#274381=CARTESIAN_POINT('Ctrl Pts',(-10.0160238186115,12.2,-5.24415555162838));
#274382=CARTESIAN_POINT('Ctrl Pts',(-10.0182388956476,12.2,-5.24694578014271));
#274383=CARTESIAN_POINT('Ctrl Pts',(-10.0204550622336,12.2,-5.24974408087327));
#274384=CARTESIAN_POINT('Ctrl Pts',(-10.0226712292222,12.2,-5.25254238211218));
#274385=CARTESIAN_POINT('Ctrl Pts',(-10.0248884846278,12.2,-5.25534875565338));
#274386=CARTESIAN_POINT('Ctrl Pts',(-10.027106784742,12.2,-5.25816319135518));
#274387=CARTESIAN_POINT('Ctrl Pts',(-10.0293250844532,12.2,-5.26097762654569));
#274388=CARTESIAN_POINT('Ctrl Pts',(-10.031544430856,12.2,-5.26380012362741));
#274389=CARTESIAN_POINT('Ctrl Pts',(-10.0337647804838,12.2,-5.26663067331696));
#274390=CARTESIAN_POINT('Ctrl Pts',(-10.0359851301115,12.2,-5.26946122300651));
#274391=CARTESIAN_POINT('Ctrl Pts',(-10.0382064823394,12.2,-5.27229982469302));
#274392=CARTESIAN_POINT('Ctrl Pts',(-10.0404287964771,12.2,-5.27514646747755));
#274393=CARTESIAN_POINT('Ctrl Pts',(-10.0433918818594,12.2,-5.27894199101787));
#274394=CARTESIAN_POINT('Ctrl Pts',(-10.046356677641,12.2,-5.28275181269434));
#274395=CARTESIAN_POINT('Ctrl Pts',(-10.0493230837317,12.2,-5.28657590615806));
#274396=CARTESIAN_POINT('Ctrl Pts',(-10.0515478888049,12.2,-5.28944397690714));
#274397=CARTESIAN_POINT('Ctrl Pts',(-10.0537735996117,12.2,-5.29232007617512));
#274398=CARTESIAN_POINT('Ctrl Pts',(-10.0560001747271,12.2,-5.29520419388704));
#274399=CARTESIAN_POINT('Ctrl Pts',(-10.058226749438,12.2,-5.29808831107501));
#274400=CARTESIAN_POINT('Ctrl Pts',(-10.0604541895072,12.2,-5.30098044610422));
#274401=CARTESIAN_POINT('Ctrl Pts',(-10.0626824527179,12.2,-5.30388058883287));
#274402=CARTESIAN_POINT('Ctrl Pts',(-10.0649107159287,12.2,-5.30678073156153));
#274403=CARTESIAN_POINT('Ctrl Pts',(-10.0671398030063,12.2,-5.30968888177863));
#274404=CARTESIAN_POINT('Ctrl Pts',(-10.0693696727271,12.2,-5.31260503043594));
#274405=CARTESIAN_POINT('Ctrl Pts',(-10.0715995424479,12.2,-5.31552117909327));
#274406=CARTESIAN_POINT('Ctrl Pts',(-10.073830195969,12.2,-5.31844532509055));
#274407=CARTESIAN_POINT('Ctrl Pts',(-10.0760615897314,12.2,-5.3213774582473));
#274408=CARTESIAN_POINT('Ctrl Pts',(-10.0782929834937,12.2,-5.32430959140405));
#274409=CARTESIAN_POINT('Ctrl Pts',(-10.0805251200545,12.2,-5.32724971180322));
#274410=CARTESIAN_POINT('Ctrl Pts',(-10.0827579573067,12.2,-5.33019780894542));
#274411=CARTESIAN_POINT('Ctrl Pts',(-10.0849907945588,12.2,-5.33314590608762));
#274412=CARTESIAN_POINT('Ctrl Pts',(-10.0872243338109,12.2,-5.33610197912926));
#274413=CARTESIAN_POINT('Ctrl Pts',(-10.0894585349797,12.2,-5.33906601889547));
#274414=CARTESIAN_POINT('Ctrl Pts',(-10.0916927365543,12.2,-5.34203005920015));
#274415=CARTESIAN_POINT('Ctrl Pts',(-10.0939276000624,12.2,-5.34500206704876));
#274416=CARTESIAN_POINT('Ctrl Pts',(-10.0961630855541,12.2,-5.34798202985793));
#274417=CARTESIAN_POINT('Ctrl Pts',(-10.0991437321994,12.2,-5.35195531270122));
#274418=CARTESIAN_POINT('Ctrl Pts',(-10.1021254821311,12.2,-5.355942739759));
#274419=CARTESIAN_POINT('Ctrl Pts',(-10.1051082402897,12.2,-5.35994428450557));
#274420=CARTESIAN_POINT('Ctrl Pts',(-10.1073453090102,12.2,-5.3629454432018));
#274421=CARTESIAN_POINT('Ctrl Pts',(-10.1095829447208,12.2,-5.36595454263154));
#274422=CARTESIAN_POINT('Ctrl Pts',(-10.1118211114728,12.2,-5.36897157389624));
#274423=CARTESIAN_POINT('Ctrl Pts',(-10.1140592782247,12.2,-5.37198860516093));
#274424=CARTESIAN_POINT('Ctrl Pts',(-10.1162979764433,12.2,-5.37501356935007));
#274425=CARTESIAN_POINT('Ctrl Pts',(-10.1185371685286,12.2,-5.37804645357213));
#274426=CARTESIAN_POINT('Ctrl Pts',(-10.1207763610206,12.2,-5.38107933834517));
#274427=CARTESIAN_POINT('Ctrl Pts',(-10.1230160464794,12.2,-5.3841201444871));
#274428=CARTESIAN_POINT('Ctrl Pts',(-10.1252561779717,12.2,-5.38716885968126));
#274429=CARTESIAN_POINT('Ctrl Pts',(-10.1274963090571,12.2,-5.39021757432157));
#274430=CARTESIAN_POINT('Ctrl Pts',(-10.1297368853697,12.2,-5.3932741973836));
#274431=CARTESIAN_POINT('Ctrl Pts',(-10.131977863942,12.2,-5.39633871684295));
#274432=CARTESIAN_POINT('Ctrl Pts',(-10.1342188425142,12.2,-5.3994032363023));
#274433=CARTESIAN_POINT('Ctrl Pts',(-10.1364602251632,12.2,-5.40247565238601));
#274434=CARTESIAN_POINT('Ctrl Pts',(-10.1387019915142,12.2,-5.40555595924693));
#274435=CARTESIAN_POINT('Ctrl Pts',(-10.1409437578652,12.2,-5.40863626610785));
#274436=CARTESIAN_POINT('Ctrl Pts',(-10.1431859115927,12.2,-5.41172446343756));
#274437=CARTESIAN_POINT('Ctrl Pts',(-10.1454284470001,12.2,-5.41482055400001));
#274438=CARTESIAN_POINT('Ctrl Pts',(-9.95917514600006,15.2,-5.75020264100001));
#274439=CARTESIAN_POINT('Ctrl Pts',(-9.95917514600006,11.6,-5.75020264100001));
#274440=CARTESIAN_POINT('Ctrl Pts',(-9.95841243100006,15.2,-5.75014921000002));
#274441=CARTESIAN_POINT('Ctrl Pts',(-9.95841243100006,11.6,-5.75014921000002));
#274442=CARTESIAN_POINT('Ctrl Pts',(-9.95688746000006,15.2,-5.75004209300002));
#274443=CARTESIAN_POINT('Ctrl Pts',(-9.95688746000006,11.6,-5.75004209300002));
#274444=CARTESIAN_POINT('Ctrl Pts',(-9.95460138500006,15.2,-5.74988064700002));
#274445=CARTESIAN_POINT('Ctrl Pts',(-9.95460138500006,11.6,-5.74988064700002));
#274446=CARTESIAN_POINT('Ctrl Pts',(-9.95155604400006,15.2,-5.74966384900002));
#274447=CARTESIAN_POINT('Ctrl Pts',(-9.95155604400006,11.6,-5.74966384900002));
#274448=CARTESIAN_POINT('Ctrl Pts',(-9.94775397000006,15.2,-5.74939029000002));
#274449=CARTESIAN_POINT('Ctrl Pts',(-9.94775397000006,11.6,-5.74939029000002));
#274450=CARTESIAN_POINT('Ctrl Pts',(-9.94395649900006,15.2,-5.74911416700001));
#274451=CARTESIAN_POINT('Ctrl Pts',(-9.94395649900006,11.6,-5.74911416700001));
#274452=CARTESIAN_POINT('Ctrl Pts',(-9.94016363100006,15.2,-5.74883548400001));
#274453=CARTESIAN_POINT('Ctrl Pts',(-9.94016363100006,11.6,-5.74883548400001));
#274454=CARTESIAN_POINT('Ctrl Pts',(-9.93637537100006,15.2,-5.74855424400001));
#274455=CARTESIAN_POINT('Ctrl Pts',(-9.93637537100006,11.6,-5.74855424400001));
#274456=CARTESIAN_POINT('Ctrl Pts',(-9.93259172200006,15.2,-5.74827044900001));
#274457=CARTESIAN_POINT('Ctrl Pts',(-9.93259172200006,11.6,-5.74827044900001));
#274458=CARTESIAN_POINT('Ctrl Pts',(-9.92881269100006,15.2,-5.74798410500001));
#274459=CARTESIAN_POINT('Ctrl Pts',(-9.92881269100006,11.6,-5.74798410500001));
#274460=CARTESIAN_POINT('Ctrl Pts',(-9.92503828400006,15.2,-5.74769522000001));
#274461=CARTESIAN_POINT('Ctrl Pts',(-9.92503828400006,11.6,-5.74769522000001));
#274462=CARTESIAN_POINT('Ctrl Pts',(-9.92126851000006,15.2,-5.74740380100002));
#274463=CARTESIAN_POINT('Ctrl Pts',(-9.92126851000006,11.6,-5.74740380100002));
#274464=CARTESIAN_POINT('Ctrl Pts',(-9.91750337600006,15.2,-5.74710985300002));
#274465=CARTESIAN_POINT('Ctrl Pts',(-9.91750337600006,11.6,-5.74710985300002));
#274466=CARTESIAN_POINT('Ctrl Pts',(-9.91374289200006,15.2,-5.74681338700002));
#274467=CARTESIAN_POINT('Ctrl Pts',(-9.91374289200006,11.6,-5.74681338700002));
#274468=CARTESIAN_POINT('Ctrl Pts',(-9.90998706400006,15.2,-5.74651440900002));
#274469=CARTESIAN_POINT('Ctrl Pts',(-9.90998706400006,11.6,-5.74651440900002));
#274470=CARTESIAN_POINT('Ctrl Pts',(-9.90623590000006,15.2,-5.74621292500002));
#274471=CARTESIAN_POINT('Ctrl Pts',(-9.90623590000006,11.6,-5.74621292500002));
#274472=CARTESIAN_POINT('Ctrl Pts',(-9.90248940500006,15.2,-5.74590894100002));
#274473=CARTESIAN_POINT('Ctrl Pts',(-9.90248940500006,11.6,-5.74590894100002));
#274474=CARTESIAN_POINT('Ctrl Pts',(-9.89874758700006,15.2,-5.74560246200001));
#274475=CARTESIAN_POINT('Ctrl Pts',(-9.89874758700006,11.6,-5.74560246200001));
#274476=CARTESIAN_POINT('Ctrl Pts',(-9.89501045000006,15.2,-5.74529349400001));
#274477=CARTESIAN_POINT('Ctrl Pts',(-9.89501045000006,11.6,-5.74529349400001));
#274478=CARTESIAN_POINT('Ctrl Pts',(-9.89127800100006,15.2,-5.74498204400002));
#274479=CARTESIAN_POINT('Ctrl Pts',(-9.89127800100006,11.6,-5.74498204400002));
#274480=CARTESIAN_POINT('Ctrl Pts',(-9.88755024700006,15.2,-5.74466811600002));
#274481=CARTESIAN_POINT('Ctrl Pts',(-9.88755024700006,11.6,-5.74466811600002));
#274482=CARTESIAN_POINT('Ctrl Pts',(-9.88382719300006,15.2,-5.74435171600002));
#274483=CARTESIAN_POINT('Ctrl Pts',(-9.88382719300006,11.6,-5.74435171600002));
#274484=CARTESIAN_POINT('Ctrl Pts',(-9.88010884700006,15.2,-5.74403285200002));
#274485=CARTESIAN_POINT('Ctrl Pts',(-9.88010884700006,11.6,-5.74403285200002));
#274486=CARTESIAN_POINT('Ctrl Pts',(-9.87639521400006,15.2,-5.74371152900002));
#274487=CARTESIAN_POINT('Ctrl Pts',(-9.87639521400006,11.6,-5.74371152900002));
#274488=CARTESIAN_POINT('Ctrl Pts',(-9.87268630300006,15.2,-5.74338775400002));
#274489=CARTESIAN_POINT('Ctrl Pts',(-9.87268630300006,11.6,-5.74338775400002));
#274490=CARTESIAN_POINT('Ctrl Pts',(-9.86898212000006,15.2,-5.74306153500002));
#274491=CARTESIAN_POINT('Ctrl Pts',(-9.86898212000006,11.6,-5.74306153500002));
#274492=CARTESIAN_POINT('Ctrl Pts',(-9.86528267300006,15.2,-5.74273287600001));
#274493=CARTESIAN_POINT('Ctrl Pts',(-9.86528267300006,11.6,-5.74273287600001));
#274494=CARTESIAN_POINT('Ctrl Pts',(-9.86158796700006,15.2,-5.74240178400002));
#274495=CARTESIAN_POINT('Ctrl Pts',(-9.86158796700006,11.6,-5.74240178400002));
#274496=CARTESIAN_POINT('Ctrl Pts',(-9.85789800900006,15.2,-5.74206826700002));
#274497=CARTESIAN_POINT('Ctrl Pts',(-9.85789800900006,11.6,-5.74206826700002));
#274498=CARTESIAN_POINT('Ctrl Pts',(-9.85421280700006,15.2,-5.74173232900002));
#274499=CARTESIAN_POINT('Ctrl Pts',(-9.85421280700006,11.6,-5.74173232900002));
#274500=CARTESIAN_POINT('Ctrl Pts',(-9.85053236600006,15.2,-5.74139397800002));
#274501=CARTESIAN_POINT('Ctrl Pts',(-9.85053236600006,11.6,-5.74139397800002));
#274502=CARTESIAN_POINT('Ctrl Pts',(-9.84685669200006,15.2,-5.74105321800002));
#274503=CARTESIAN_POINT('Ctrl Pts',(-9.84685669200006,11.6,-5.74105321800002));
#274504=CARTESIAN_POINT('Ctrl Pts',(-9.84318579500006,15.2,-5.74071005800001));
#274505=CARTESIAN_POINT('Ctrl Pts',(-9.84318579500006,11.6,-5.74071005800001));
#274506=CARTESIAN_POINT('Ctrl Pts',(-9.83951967700006,15.2,-5.74036450400002));
#274507=CARTESIAN_POINT('Ctrl Pts',(-9.83951967700006,11.6,-5.74036450400002));
#274508=CARTESIAN_POINT('Ctrl Pts',(-9.83585834900006,15.2,-5.74001656000001));
#274509=CARTESIAN_POINT('Ctrl Pts',(-9.83585834900006,11.6,-5.74001656000001));
#274510=CARTESIAN_POINT('Ctrl Pts',(-9.83220181500006,15.2,-5.73966623600001));
#274511=CARTESIAN_POINT('Ctrl Pts',(-9.83220181500006,11.6,-5.73966623600001));
#274512=CARTESIAN_POINT('Ctrl Pts',(-9.82855008400006,15.2,-5.73931353600001));
#274513=CARTESIAN_POINT('Ctrl Pts',(-9.82855008400006,11.6,-5.73931353600001));
#274514=CARTESIAN_POINT('Ctrl Pts',(-9.82490316100006,15.2,-5.73895846600001));
#274515=CARTESIAN_POINT('Ctrl Pts',(-9.82490316100006,11.6,-5.73895846600001));
#274516=CARTESIAN_POINT('Ctrl Pts',(-9.82126105300006,15.2,-5.73860103500002));
#274517=CARTESIAN_POINT('Ctrl Pts',(-9.82126105300006,11.6,-5.73860103500002));
#274518=CARTESIAN_POINT('Ctrl Pts',(-9.81762376700006,15.2,-5.73824124900002));
#274519=CARTESIAN_POINT('Ctrl Pts',(-9.81762376700006,11.6,-5.73824124900002));
#274520=CARTESIAN_POINT('Ctrl Pts',(-9.81399131100006,15.2,-5.73787911300002));
#274521=CARTESIAN_POINT('Ctrl Pts',(-9.81399131100006,11.6,-5.73787911300002));
#274522=CARTESIAN_POINT('Ctrl Pts',(-9.81036369000006,15.2,-5.73751463500002));
#274523=CARTESIAN_POINT('Ctrl Pts',(-9.81036369000006,11.6,-5.73751463500002));
#274524=CARTESIAN_POINT('Ctrl Pts',(-9.80674091100006,15.2,-5.73714781900001));
#274525=CARTESIAN_POINT('Ctrl Pts',(-9.80674091100006,11.6,-5.73714781900001));
#274526=CARTESIAN_POINT('Ctrl Pts',(-9.80312298100005,15.2,-5.73677867600002));
#274527=CARTESIAN_POINT('Ctrl Pts',(-9.80312298100005,11.6,-5.73677867600002));
#274528=CARTESIAN_POINT('Ctrl Pts',(-9.79950990800005,15.2,-5.73640720800002));
#274529=CARTESIAN_POINT('Ctrl Pts',(-9.79950990800005,11.6,-5.73640720800002));
#274530=CARTESIAN_POINT('Ctrl Pts',(-9.79590169600005,15.2,-5.73603342500002));
#274531=CARTESIAN_POINT('Ctrl Pts',(-9.79590169600005,11.6,-5.73603342500002));
#274532=CARTESIAN_POINT('Ctrl Pts',(-9.79229835500006,15.2,-5.73565733100001));
#274533=CARTESIAN_POINT('Ctrl Pts',(-9.79229835500006,11.6,-5.73565733100001));
#274534=CARTESIAN_POINT('Ctrl Pts',(-9.78869989000006,15.2,-5.73527893500002));
#274535=CARTESIAN_POINT('Ctrl Pts',(-9.78869989000006,11.6,-5.73527893500002));
#274536=CARTESIAN_POINT('Ctrl Pts',(-9.78510630800006,15.2,-5.73489824300002));
#274537=CARTESIAN_POINT('Ctrl Pts',(-9.78510630800006,11.6,-5.73489824300002));
#274538=CARTESIAN_POINT('Ctrl Pts',(-9.78151761600006,15.2,-5.73451526100002));
#274539=CARTESIAN_POINT('Ctrl Pts',(-9.78151761600006,11.6,-5.73451526100002));
#274540=CARTESIAN_POINT('Ctrl Pts',(-9.77793382100005,15.2,-5.73412999600002));
#274541=CARTESIAN_POINT('Ctrl Pts',(-9.77793382100005,11.6,-5.73412999600002));
#274542=CARTESIAN_POINT('Ctrl Pts',(-9.77435492900005,15.2,-5.73374245400001));
#274543=CARTESIAN_POINT('Ctrl Pts',(-9.77435492900005,11.6,-5.73374245400001));
#274544=CARTESIAN_POINT('Ctrl Pts',(-9.77078094800006,15.2,-5.73335264400002));
#274545=CARTESIAN_POINT('Ctrl Pts',(-9.77078094800006,11.6,-5.73335264400002));
#274546=CARTESIAN_POINT('Ctrl Pts',(-9.76721188400006,15.2,-5.73296057000002));
#274547=CARTESIAN_POINT('Ctrl Pts',(-9.76721188400006,11.6,-5.73296057000002));
#274548=CARTESIAN_POINT('Ctrl Pts',(-9.76364774500006,15.2,-5.73256624100001));
#274549=CARTESIAN_POINT('Ctrl Pts',(-9.76364774500006,11.6,-5.73256624100001));
#274550=CARTESIAN_POINT('Ctrl Pts',(-9.76008853600005,15.2,-5.73216966200001));
#274551=CARTESIAN_POINT('Ctrl Pts',(-9.76008853600005,11.6,-5.73216966200001));
#274552=CARTESIAN_POINT('Ctrl Pts',(-9.75653426500006,15.2,-5.73177084100001));
#274553=CARTESIAN_POINT('Ctrl Pts',(-9.75653426500006,11.6,-5.73177084100001));
#274554=CARTESIAN_POINT('Ctrl Pts',(-9.75298493900006,15.2,-5.73136978400001));
#274555=CARTESIAN_POINT('Ctrl Pts',(-9.75298493900006,11.6,-5.73136978400001));
#274556=CARTESIAN_POINT('Ctrl Pts',(-9.74944056500006,15.2,-5.73096650000001));
#274557=CARTESIAN_POINT('Ctrl Pts',(-9.74944056500006,11.6,-5.73096650000001));
#274558=CARTESIAN_POINT('Ctrl Pts',(-9.74590115000005,15.2,-5.73056099200001));
#274559=CARTESIAN_POINT('Ctrl Pts',(-9.74590115000005,11.6,-5.73056099200001));
#274560=CARTESIAN_POINT('Ctrl Pts',(-9.74236669900005,15.2,-5.73015327100002));
#274561=CARTESIAN_POINT('Ctrl Pts',(-9.74236669900005,11.6,-5.73015327100002));
#274562=CARTESIAN_POINT('Ctrl Pts',(-9.73883722100006,15.2,-5.72974334100002));
#274563=CARTESIAN_POINT('Ctrl Pts',(-9.73883722100006,11.6,-5.72974334100002));
#274564=CARTESIAN_POINT('Ctrl Pts',(-9.73531272200006,15.2,-5.72933121000001));
#274565=CARTESIAN_POINT('Ctrl Pts',(-9.73531272200006,11.6,-5.72933121000001));
#274566=CARTESIAN_POINT('Ctrl Pts',(-9.73179320900006,15.2,-5.72891688500002));
#274567=CARTESIAN_POINT('Ctrl Pts',(-9.73179320900006,11.6,-5.72891688500002));
#274568=CARTESIAN_POINT('Ctrl Pts',(-9.72827869000006,15.2,-5.72850037300002));
#274569=CARTESIAN_POINT('Ctrl Pts',(-9.72827869000006,11.6,-5.72850037300002));
#274570=CARTESIAN_POINT('Ctrl Pts',(-9.72476917000006,15.2,-5.72808168000002));
#274571=CARTESIAN_POINT('Ctrl Pts',(-9.72476917000006,11.6,-5.72808168000002));
#274572=CARTESIAN_POINT('Ctrl Pts',(-9.72126465700006,15.2,-5.72766081300002));
#274573=CARTESIAN_POINT('Ctrl Pts',(-9.72126465700006,11.6,-5.72766081300002));
#274574=CARTESIAN_POINT('Ctrl Pts',(-9.71776515900006,15.2,-5.72723778200002));
#274575=CARTESIAN_POINT('Ctrl Pts',(-9.71776515900006,11.6,-5.72723778200002));
#274576=CARTESIAN_POINT('Ctrl Pts',(-9.71427068100006,15.2,-5.72681259100002));
#274577=CARTESIAN_POINT('Ctrl Pts',(-9.71427068100006,11.6,-5.72681259100002));
#274578=CARTESIAN_POINT('Ctrl Pts',(-9.71078123000006,15.2,-5.72638524700002));
#274579=CARTESIAN_POINT('Ctrl Pts',(-9.71078123000006,11.6,-5.72638524700002));
#274580=CARTESIAN_POINT('Ctrl Pts',(-9.70729681500006,15.2,-5.72595575900002));
#274581=CARTESIAN_POINT('Ctrl Pts',(-9.70729681500006,11.6,-5.72595575900002));
#274582=CARTESIAN_POINT('Ctrl Pts',(-9.70381744100006,15.2,-5.72552413200001));
#274583=CARTESIAN_POINT('Ctrl Pts',(-9.70381744100006,11.6,-5.72552413200001));
#274584=CARTESIAN_POINT('Ctrl Pts',(-9.70034311500006,15.2,-5.72509037400001));
#274585=CARTESIAN_POINT('Ctrl Pts',(-9.70034311500006,11.6,-5.72509037400001));
#274586=CARTESIAN_POINT('Ctrl Pts',(-9.69687384600006,15.2,-5.72465449300001));
#274587=CARTESIAN_POINT('Ctrl Pts',(-9.69687384600006,11.6,-5.72465449300001));
#274588=CARTESIAN_POINT('Ctrl Pts',(-9.69340963900006,15.2,-5.72421649500002));
#274589=CARTESIAN_POINT('Ctrl Pts',(-9.69340963900006,11.6,-5.72421649500002));
#274590=CARTESIAN_POINT('Ctrl Pts',(-9.68995050200006,15.2,-5.72377638700001));
#274591=CARTESIAN_POINT('Ctrl Pts',(-9.68995050200006,11.6,-5.72377638700001));
#274592=CARTESIAN_POINT('Ctrl Pts',(-9.68649644100006,15.2,-5.72333417800002));
#274593=CARTESIAN_POINT('Ctrl Pts',(-9.68649644100006,11.6,-5.72333417800002));
#274594=CARTESIAN_POINT('Ctrl Pts',(-9.68304746500005,15.2,-5.72288987300002));
#274595=CARTESIAN_POINT('Ctrl Pts',(-9.68304746500005,11.6,-5.72288987300002));
#274596=CARTESIAN_POINT('Ctrl Pts',(-9.67960357800006,15.2,-5.72244348100002));
#274597=CARTESIAN_POINT('Ctrl Pts',(-9.67960357800006,11.6,-5.72244348100002));
#274598=CARTESIAN_POINT('Ctrl Pts',(-9.67616479000006,15.2,-5.72199500700002));
#274599=CARTESIAN_POINT('Ctrl Pts',(-9.67616479000006,11.6,-5.72199500700002));
#274600=CARTESIAN_POINT('Ctrl Pts',(-9.67273110700006,15.2,-5.72154446000001));
#274601=CARTESIAN_POINT('Ctrl Pts',(-9.67273110700006,11.6,-5.72154446000001));
#274602=CARTESIAN_POINT('Ctrl Pts',(-9.66930253400006,15.2,-5.72109184700002));
#274603=CARTESIAN_POINT('Ctrl Pts',(-9.66930253400006,11.6,-5.72109184700002));
#274604=CARTESIAN_POINT('Ctrl Pts',(-9.66587908100006,15.2,-5.72063717600001));
#274605=CARTESIAN_POINT('Ctrl Pts',(-9.66587908100006,11.6,-5.72063717600001));
#274606=CARTESIAN_POINT('Ctrl Pts',(-9.66246075400005,15.2,-5.72018045200001));
#274607=CARTESIAN_POINT('Ctrl Pts',(-9.66246075400005,11.6,-5.72018045200001));
#274608=CARTESIAN_POINT('Ctrl Pts',(-9.65904756000005,15.2,-5.71972168500002));
#274609=CARTESIAN_POINT('Ctrl Pts',(-9.65904756000005,11.6,-5.71972168500002));
#274610=CARTESIAN_POINT('Ctrl Pts',(-9.65563950500006,15.2,-5.71926088000002));
#274611=CARTESIAN_POINT('Ctrl Pts',(-9.65563950500006,11.6,-5.71926088000002));
#274612=CARTESIAN_POINT('Ctrl Pts',(-9.65223659800006,15.2,-5.71879804700002));
#274613=CARTESIAN_POINT('Ctrl Pts',(-9.65223659800006,11.6,-5.71879804700002));
#274614=CARTESIAN_POINT('Ctrl Pts',(-9.64883884500006,15.2,-5.71833319000002));
#274615=CARTESIAN_POINT('Ctrl Pts',(-9.64883884500006,11.6,-5.71833319000002));
#274616=CARTESIAN_POINT('Ctrl Pts',(-9.64544625400006,15.2,-5.71786632000002));
#274617=CARTESIAN_POINT('Ctrl Pts',(-9.64544625400006,11.6,-5.71786632000002));
#274618=CARTESIAN_POINT('Ctrl Pts',(-9.64205883100006,15.2,-5.71739744100002));
#274619=CARTESIAN_POINT('Ctrl Pts',(-9.64205883100006,11.6,-5.71739744100002));
#274620=CARTESIAN_POINT('Ctrl Pts',(-9.63867658300006,15.2,-5.71692656400002));
#274621=CARTESIAN_POINT('Ctrl Pts',(-9.63867658300006,11.6,-5.71692656400002));
#274622=CARTESIAN_POINT('Ctrl Pts',(-9.63529951700006,15.2,-5.71645369400001));
#274623=CARTESIAN_POINT('Ctrl Pts',(-9.63529951700006,11.6,-5.71645369400001));
#274624=CARTESIAN_POINT('Ctrl Pts',(-9.63192764200006,15.2,-5.71597884000001));
#274625=CARTESIAN_POINT('Ctrl Pts',(-9.63192764200006,11.6,-5.71597884000001));
#274626=CARTESIAN_POINT('Ctrl Pts',(-9.62856096400006,15.2,-5.71550200700001));
#274627=CARTESIAN_POINT('Ctrl Pts',(-9.62856096400006,11.6,-5.71550200700001));
#274628=CARTESIAN_POINT('Ctrl Pts',(-9.62519948900006,15.2,-5.71502320500001));
#274629=CARTESIAN_POINT('Ctrl Pts',(-9.62519948900006,11.6,-5.71502320500001));
#274630=CARTESIAN_POINT('Ctrl Pts',(-9.62184322600006,15.2,-5.71454244100002));
#274631=CARTESIAN_POINT('Ctrl Pts',(-9.62184322600006,11.6,-5.71454244100002));
#274632=CARTESIAN_POINT('Ctrl Pts',(-9.61849218000006,15.2,-5.71405972200001));
#274633=CARTESIAN_POINT('Ctrl Pts',(-9.61849218000006,11.6,-5.71405972200001));
#274634=CARTESIAN_POINT('Ctrl Pts',(-9.61514636100006,15.2,-5.71357505700002));
#274635=CARTESIAN_POINT('Ctrl Pts',(-9.61514636100006,11.6,-5.71357505700002));
#274636=CARTESIAN_POINT('Ctrl Pts',(-9.61180577400006,15.2,-5.71308845100001));
#274637=CARTESIAN_POINT('Ctrl Pts',(-9.61180577400006,11.6,-5.71308845100001));
#274638=CARTESIAN_POINT('Ctrl Pts',(-9.60847042700006,15.2,-5.71259991300002));
#274639=CARTESIAN_POINT('Ctrl Pts',(-9.60847042700006,11.6,-5.71259991300002));
#274640=CARTESIAN_POINT('Ctrl Pts',(-9.60514032600006,15.2,-5.71210945300002));
#274641=CARTESIAN_POINT('Ctrl Pts',(-9.60514032600006,11.6,-5.71210945300002));
#274642=CARTESIAN_POINT('Ctrl Pts',(-9.60181548000006,15.2,-5.71161707400002));
#274643=CARTESIAN_POINT('Ctrl Pts',(-9.60181548000006,11.6,-5.71161707400002));
#274644=CARTESIAN_POINT('Ctrl Pts',(-9.59849589600006,15.2,-5.71112278700002));
#274645=CARTESIAN_POINT('Ctrl Pts',(-9.59849589600006,11.6,-5.71112278700002));
#274646=CARTESIAN_POINT('Ctrl Pts',(-9.59518158000006,15.2,-5.71062660000001));
#274647=CARTESIAN_POINT('Ctrl Pts',(-9.59518158000006,11.6,-5.71062660000001));
#274648=CARTESIAN_POINT('Ctrl Pts',(-9.59187253900006,15.2,-5.71012851800001));
#274649=CARTESIAN_POINT('Ctrl Pts',(-9.59187253900006,11.6,-5.71012851800001));
#274650=CARTESIAN_POINT('Ctrl Pts',(-9.58856878200006,15.2,-5.70962855200002));
#274651=CARTESIAN_POINT('Ctrl Pts',(-9.58856878200006,11.6,-5.70962855200002));
#274652=CARTESIAN_POINT('Ctrl Pts',(-9.58527031500006,15.2,-5.70912670700002));
#274653=CARTESIAN_POINT('Ctrl Pts',(-9.58527031500006,11.6,-5.70912670700002));
#274654=CARTESIAN_POINT('Ctrl Pts',(-9.58197714700006,15.2,-5.70862299200002));
#274655=CARTESIAN_POINT('Ctrl Pts',(-9.58197714700006,11.6,-5.70862299200002));
#274656=CARTESIAN_POINT('Ctrl Pts',(-9.57868928200006,15.2,-5.70811741500002));
#274657=CARTESIAN_POINT('Ctrl Pts',(-9.57868928200006,11.6,-5.70811741500002));
#274658=CARTESIAN_POINT('Ctrl Pts',(-9.57540672900006,15.2,-5.70760998400001));
#274659=CARTESIAN_POINT('Ctrl Pts',(-9.57540672900006,11.6,-5.70760998400001));
#274660=CARTESIAN_POINT('Ctrl Pts',(-9.57212949600006,15.2,-5.70710070600001));
#274661=CARTESIAN_POINT('Ctrl Pts',(-9.57212949600006,11.6,-5.70710070600001));
#274662=CARTESIAN_POINT('Ctrl Pts',(-9.56885759000006,15.2,-5.70658959000002));
#274663=CARTESIAN_POINT('Ctrl Pts',(-9.56885759000006,11.6,-5.70658959000002));
#274664=CARTESIAN_POINT('Ctrl Pts',(-9.56559101700006,15.2,-5.70607664300002));
#274665=CARTESIAN_POINT('Ctrl Pts',(-9.56559101700006,11.6,-5.70607664300002));
#274666=CARTESIAN_POINT('Ctrl Pts',(-9.56232978500006,15.2,-5.70556187300002));
#274667=CARTESIAN_POINT('Ctrl Pts',(-9.56232978500006,11.6,-5.70556187300002));
#274668=CARTESIAN_POINT('Ctrl Pts',(-9.55907390200006,15.2,-5.70504528800001));
#274669=CARTESIAN_POINT('Ctrl Pts',(-9.55907390200006,11.6,-5.70504528800001));
#274670=CARTESIAN_POINT('Ctrl Pts',(-9.55582337400006,15.2,-5.70452689600002));
#274671=CARTESIAN_POINT('Ctrl Pts',(-9.55582337400006,11.6,-5.70452689600002));
#274672=CARTESIAN_POINT('Ctrl Pts',(-9.55257821000006,15.2,-5.70400670700002));
#274673=CARTESIAN_POINT('Ctrl Pts',(-9.55257821000006,11.6,-5.70400670700002));
#274674=CARTESIAN_POINT('Ctrl Pts',(-9.54933841600005,15.2,-5.70348472500001));
#274675=CARTESIAN_POINT('Ctrl Pts',(-9.54933841600005,11.6,-5.70348472500001));
#274676=CARTESIAN_POINT('Ctrl Pts',(-9.54610400000006,15.2,-5.70296096100002));
#274677=CARTESIAN_POINT('Ctrl Pts',(-9.54610400000006,11.6,-5.70296096100002));
#274678=CARTESIAN_POINT('Ctrl Pts',(-9.54287496800006,15.2,-5.70243542200001));
#274679=CARTESIAN_POINT('Ctrl Pts',(-9.54287496800006,11.6,-5.70243542200001));
#274680=CARTESIAN_POINT('Ctrl Pts',(-9.53965133000005,15.2,-5.70190811700002));
#274681=CARTESIAN_POINT('Ctrl Pts',(-9.53965133000005,11.6,-5.70190811700002));
#274682=CARTESIAN_POINT('Ctrl Pts',(-9.53643309000006,15.2,-5.70137905200002));
#274683=CARTESIAN_POINT('Ctrl Pts',(-9.53643309000006,11.6,-5.70137905200002));
#274684=CARTESIAN_POINT('Ctrl Pts',(-9.53322025900006,15.2,-5.70084823700002));
#274685=CARTESIAN_POINT('Ctrl Pts',(-9.53322025900006,11.6,-5.70084823700002));
#274686=CARTESIAN_POINT('Ctrl Pts',(-9.53001284100005,15.2,-5.70031568100001));
#274687=CARTESIAN_POINT('Ctrl Pts',(-9.53001284100005,11.6,-5.70031568100001));
#274688=CARTESIAN_POINT('Ctrl Pts',(-9.52681084500006,15.2,-5.69978139000002));
#274689=CARTESIAN_POINT('Ctrl Pts',(-9.52681084500006,11.6,-5.69978139000002));
#274690=CARTESIAN_POINT('Ctrl Pts',(-9.52361428000006,15.2,-5.69924537200002));
#274691=CARTESIAN_POINT('Ctrl Pts',(-9.52361428000006,11.6,-5.69924537200002));
#274692=CARTESIAN_POINT('Ctrl Pts',(-9.52042315000006,15.2,-5.69870763800001));
#274693=CARTESIAN_POINT('Ctrl Pts',(-9.52042315000006,11.6,-5.69870763800001));
#274694=CARTESIAN_POINT('Ctrl Pts',(-9.51723746400006,15.2,-5.69816819400002));
#274695=CARTESIAN_POINT('Ctrl Pts',(-9.51723746400006,11.6,-5.69816819400002));
#274696=CARTESIAN_POINT('Ctrl Pts',(-9.51405723100006,15.2,-5.69762704800001));
#274697=CARTESIAN_POINT('Ctrl Pts',(-9.51405723100006,11.6,-5.69762704800001));
#274698=CARTESIAN_POINT('Ctrl Pts',(-9.51088245600006,15.2,-5.69708421000002));
#274699=CARTESIAN_POINT('Ctrl Pts',(-9.51088245600006,11.6,-5.69708421000002));
#274700=CARTESIAN_POINT('Ctrl Pts',(-9.50771314700006,15.2,-5.69653968700001));
#274701=CARTESIAN_POINT('Ctrl Pts',(-9.50771314700006,11.6,-5.69653968700001));
#274702=CARTESIAN_POINT('Ctrl Pts',(-9.50454931300006,15.2,-5.69599348800002));
#274703=CARTESIAN_POINT('Ctrl Pts',(-9.50454931300006,11.6,-5.69599348800002));
#274704=CARTESIAN_POINT('Ctrl Pts',(-9.50139095800006,15.2,-5.69544562100001));
#274705=CARTESIAN_POINT('Ctrl Pts',(-9.50139095800006,11.6,-5.69544562100001));
#274706=CARTESIAN_POINT('Ctrl Pts',(-9.49823809300005,15.2,-5.69489609400001));
#274707=CARTESIAN_POINT('Ctrl Pts',(-9.49823809300005,11.6,-5.69489609400001));
#274708=CARTESIAN_POINT('Ctrl Pts',(-9.49509072500006,15.2,-5.69434491500001));
#274709=CARTESIAN_POINT('Ctrl Pts',(-9.49509072500006,11.6,-5.69434491500001));
#274710=CARTESIAN_POINT('Ctrl Pts',(-9.49194886000006,15.2,-5.69379209500001));
#274711=CARTESIAN_POINT('Ctrl Pts',(-9.49194886000006,11.6,-5.69379209500001));
#274712=CARTESIAN_POINT('Ctrl Pts',(-9.48881250600006,15.2,-5.69323764000002));
#274713=CARTESIAN_POINT('Ctrl Pts',(-9.48881250600006,11.6,-5.69323764000002));
#274714=CARTESIAN_POINT('Ctrl Pts',(-9.48568167200006,15.2,-5.69268155900001));
#274715=CARTESIAN_POINT('Ctrl Pts',(-9.48568167200006,11.6,-5.69268155900001));
#274716=CARTESIAN_POINT('Ctrl Pts',(-9.48255636300006,15.2,-5.69212386100002));
#274717=CARTESIAN_POINT('Ctrl Pts',(-9.48255636300006,11.6,-5.69212386100002));
#274718=CARTESIAN_POINT('Ctrl Pts',(-9.47943658800006,15.2,-5.69156455400002));
#274719=CARTESIAN_POINT('Ctrl Pts',(-9.47943658800006,11.6,-5.69156455400002));
#274720=CARTESIAN_POINT('Ctrl Pts',(-9.47632235400006,15.2,-5.69100364700001));
#274721=CARTESIAN_POINT('Ctrl Pts',(-9.47632235400006,11.6,-5.69100364700001));
#274722=CARTESIAN_POINT('Ctrl Pts',(-9.47321366800006,15.2,-5.69044114700001));
#274723=CARTESIAN_POINT('Ctrl Pts',(-9.47321366800006,11.6,-5.69044114700001));
#274724=CARTESIAN_POINT('Ctrl Pts',(-9.47011053900006,15.2,-5.68987706500002));
#274725=CARTESIAN_POINT('Ctrl Pts',(-9.47011053900006,11.6,-5.68987706500002));
#274726=CARTESIAN_POINT('Ctrl Pts',(-9.46701297400006,15.2,-5.68931140800002));
#274727=CARTESIAN_POINT('Ctrl Pts',(-9.46701297400006,11.6,-5.68931140800002));
#274728=CARTESIAN_POINT('Ctrl Pts',(-9.46392098000005,15.2,-5.68874418700001));
#274729=CARTESIAN_POINT('Ctrl Pts',(-9.46392098000005,11.6,-5.68874418700001));
#274730=CARTESIAN_POINT('Ctrl Pts',(-9.46083456600006,15.2,-5.68817540700002));
#274731=CARTESIAN_POINT('Ctrl Pts',(-9.46083456600006,11.6,-5.68817540700002));
#274732=CARTESIAN_POINT('Ctrl Pts',(-9.45775373800006,15.2,-5.68760507900001));
#274733=CARTESIAN_POINT('Ctrl Pts',(-9.45775373800006,11.6,-5.68760507900001));
#274734=CARTESIAN_POINT('Ctrl Pts',(-9.45467850400006,15.2,-5.68703321000001));
#274735=CARTESIAN_POINT('Ctrl Pts',(-9.45467850400006,11.6,-5.68703321000001));
#274736=CARTESIAN_POINT('Ctrl Pts',(-9.45160887200006,15.2,-5.68645981100002));
#274737=CARTESIAN_POINT('Ctrl Pts',(-9.45160887200006,11.6,-5.68645981100002));
#274738=CARTESIAN_POINT('Ctrl Pts',(-9.44854485000005,15.2,-5.68588488900001));
#274739=CARTESIAN_POINT('Ctrl Pts',(-9.44854485000005,11.6,-5.68588488900001));
#274740=CARTESIAN_POINT('Ctrl Pts',(-9.44548644300006,15.2,-5.68530845500002));
#274741=CARTESIAN_POINT('Ctrl Pts',(-9.44548644300006,11.6,-5.68530845500002));
#274742=CARTESIAN_POINT('Ctrl Pts',(-9.44243366200006,15.2,-5.68473051500002));
#274743=CARTESIAN_POINT('Ctrl Pts',(-9.44243366200006,11.6,-5.68473051500002));
#274744=CARTESIAN_POINT('Ctrl Pts',(-9.43938651300006,15.2,-5.68415107900002));
#274745=CARTESIAN_POINT('Ctrl Pts',(-9.43938651300006,11.6,-5.68415107900002));
#274746=CARTESIAN_POINT('Ctrl Pts',(-9.43634500500006,15.2,-5.68357015700002));
#274747=CARTESIAN_POINT('Ctrl Pts',(-9.43634500500006,11.6,-5.68357015700002));
#274748=CARTESIAN_POINT('Ctrl Pts',(-9.43330914300006,15.2,-5.68298775600002));
#274749=CARTESIAN_POINT('Ctrl Pts',(-9.43330914300006,11.6,-5.68298775600002));
#274750=CARTESIAN_POINT('Ctrl Pts',(-9.43027893700006,15.2,-5.68240388600002));
#274751=CARTESIAN_POINT('Ctrl Pts',(-9.43027893700006,11.6,-5.68240388600002));
#274752=CARTESIAN_POINT('Ctrl Pts',(-9.42725439400006,15.2,-5.68181855600002));
#274753=CARTESIAN_POINT('Ctrl Pts',(-9.42725439400006,11.6,-5.68181855600002));
#274754=CARTESIAN_POINT('Ctrl Pts',(-9.42423552100006,15.2,-5.68123177400001));
#274755=CARTESIAN_POINT('Ctrl Pts',(-9.42423552100006,11.6,-5.68123177400001));
#274756=CARTESIAN_POINT('Ctrl Pts',(-9.42122232700006,15.2,-5.68064355000002));
#274757=CARTESIAN_POINT('Ctrl Pts',(-9.42122232700006,11.6,-5.68064355000002));
#274758=CARTESIAN_POINT('Ctrl Pts',(-9.41821481900006,15.2,-5.68005389300002));
#274759=CARTESIAN_POINT('Ctrl Pts',(-9.41821481900006,11.6,-5.68005389300002));
#274760=CARTESIAN_POINT('Ctrl Pts',(-9.41521300400006,15.2,-5.67946281100002));
#274761=CARTESIAN_POINT('Ctrl Pts',(-9.41521300400006,11.6,-5.67946281100002));
#274762=CARTESIAN_POINT('Ctrl Pts',(-9.41221689100006,15.2,-5.67887031500002));
#274763=CARTESIAN_POINT('Ctrl Pts',(-9.41221689100006,11.6,-5.67887031500002));
#274764=CARTESIAN_POINT('Ctrl Pts',(-9.40922648700005,15.2,-5.67827641200001));
#274765=CARTESIAN_POINT('Ctrl Pts',(-9.40922648700005,11.6,-5.67827641200001));
#274766=CARTESIAN_POINT('Ctrl Pts',(-9.40624180100006,15.2,-5.67768111200002));
#274767=CARTESIAN_POINT('Ctrl Pts',(-9.40624180100006,11.6,-5.67768111200002));
#274768=CARTESIAN_POINT('Ctrl Pts',(-9.40326283700006,15.2,-5.67708442400002));
#274769=CARTESIAN_POINT('Ctrl Pts',(-9.40326283700006,11.6,-5.67708442400002));
#274770=CARTESIAN_POINT('Ctrl Pts',(-9.40028960800005,15.2,-5.67648635800002));
#274771=CARTESIAN_POINT('Ctrl Pts',(-9.40028960800005,11.6,-5.67648635800002));
#274772=CARTESIAN_POINT('Ctrl Pts',(-9.39732211800006,15.2,-5.67588692100002));
#274773=CARTESIAN_POINT('Ctrl Pts',(-9.39732211800006,11.6,-5.67588692100002));
#274774=CARTESIAN_POINT('Ctrl Pts',(-9.39436037700006,15.2,-5.67528612600002));
#274775=CARTESIAN_POINT('Ctrl Pts',(-9.39436037700006,11.6,-5.67528612600002));
#274776=CARTESIAN_POINT('Ctrl Pts',(-9.39140439200006,15.2,-5.67468397800001));
#274777=CARTESIAN_POINT('Ctrl Pts',(-9.39140439200006,11.6,-5.67468397800001));
#274778=CARTESIAN_POINT('Ctrl Pts',(-9.38845417000006,15.2,-5.67408048900001));
#274779=CARTESIAN_POINT('Ctrl Pts',(-9.38845417000006,11.6,-5.67408048900001));
#274780=CARTESIAN_POINT('Ctrl Pts',(-9.38550971900005,15.2,-5.67347566700001));
#274781=CARTESIAN_POINT('Ctrl Pts',(-9.38550971900005,11.6,-5.67347566700001));
#274782=CARTESIAN_POINT('Ctrl Pts',(-9.38257104800006,15.2,-5.67286952400002));
#274783=CARTESIAN_POINT('Ctrl Pts',(-9.38257104800006,11.6,-5.67286952400002));
#274784=CARTESIAN_POINT('Ctrl Pts',(-9.37963816300006,15.2,-5.67226206500001));
#274785=CARTESIAN_POINT('Ctrl Pts',(-9.37963816300006,11.6,-5.67226206500001));
#274786=CARTESIAN_POINT('Ctrl Pts',(-9.37671107500006,15.2,-5.67165330200002));
#274787=CARTESIAN_POINT('Ctrl Pts',(-9.37671107500006,11.6,-5.67165330200002));
#274788=CARTESIAN_POINT('Ctrl Pts',(-9.37378978800006,15.2,-5.67104324400002));
#274789=CARTESIAN_POINT('Ctrl Pts',(-9.37378978800006,11.6,-5.67104324400002));
#274790=CARTESIAN_POINT('Ctrl Pts',(-9.37087431300006,15.2,-5.67043190100001));
#274791=CARTESIAN_POINT('Ctrl Pts',(-9.37087431300006,11.6,-5.67043190100001));
#274792=CARTESIAN_POINT('Ctrl Pts',(-9.36796465500005,15.2,-5.66981928200001));
#274793=CARTESIAN_POINT('Ctrl Pts',(-9.36796465500005,11.6,-5.66981928200001));
#274794=CARTESIAN_POINT('Ctrl Pts',(-9.36506082600006,15.2,-5.66920539600002));
#274795=CARTESIAN_POINT('Ctrl Pts',(-9.36506082600006,11.6,-5.66920539600002));
#274796=CARTESIAN_POINT('Ctrl Pts',(-9.36216282900006,15.2,-5.66859025300002));
#274797=CARTESIAN_POINT('Ctrl Pts',(-9.36216282900006,11.6,-5.66859025300002));
#274798=CARTESIAN_POINT('Ctrl Pts',(-9.35927067600005,15.2,-5.66797386300002));
#274799=CARTESIAN_POINT('Ctrl Pts',(-9.35927067600005,11.6,-5.66797386300002));
#274800=CARTESIAN_POINT('Ctrl Pts',(-9.35638437300006,15.2,-5.66735623400002));
#274801=CARTESIAN_POINT('Ctrl Pts',(-9.35638437300006,11.6,-5.66735623400002));
#274802=CARTESIAN_POINT('Ctrl Pts',(-9.35350392700006,15.2,-5.66673737800001));
#274803=CARTESIAN_POINT('Ctrl Pts',(-9.35350392700006,11.6,-5.66673737800001));
#274804=CARTESIAN_POINT('Ctrl Pts',(-9.35062934800006,15.2,-5.66611730200002));
#274805=CARTESIAN_POINT('Ctrl Pts',(-9.35062934800006,11.6,-5.66611730200002));
#274806=CARTESIAN_POINT('Ctrl Pts',(-9.34776064400006,15.2,-5.66549601900002));
#274807=CARTESIAN_POINT('Ctrl Pts',(-9.34776064400006,11.6,-5.66549601900002));
#274808=CARTESIAN_POINT('Ctrl Pts',(-9.34489782000006,15.2,-5.66487353500002));
#274809=CARTESIAN_POINT('Ctrl Pts',(-9.34489782000006,11.6,-5.66487353500002));
#274810=CARTESIAN_POINT('Ctrl Pts',(-9.34204088800006,15.2,-5.66424986100002));
#274811=CARTESIAN_POINT('Ctrl Pts',(-9.34204088800006,11.6,-5.66424986100002));
#274812=CARTESIAN_POINT('Ctrl Pts',(-9.33918985300006,15.2,-5.66362500900001));
#274813=CARTESIAN_POINT('Ctrl Pts',(-9.33918985300006,11.6,-5.66362500900001));
#274814=CARTESIAN_POINT('Ctrl Pts',(-9.33634472400006,15.2,-5.66299898600001));
#274815=CARTESIAN_POINT('Ctrl Pts',(-9.33634472400006,11.6,-5.66299898600001));
#274816=CARTESIAN_POINT('Ctrl Pts',(-9.33350550900006,15.2,-5.66237180200002));
#274817=CARTESIAN_POINT('Ctrl Pts',(-9.33350550900006,11.6,-5.66237180200002));
#274818=CARTESIAN_POINT('Ctrl Pts',(-9.33067221700006,15.2,-5.66174346800001));
#274819=CARTESIAN_POINT('Ctrl Pts',(-9.33067221700006,11.6,-5.66174346800001));
#274820=CARTESIAN_POINT('Ctrl Pts',(-9.32784485500006,15.2,-5.66111399300001));
#274821=CARTESIAN_POINT('Ctrl Pts',(-9.32784485500006,11.6,-5.66111399300001));
#274822=CARTESIAN_POINT('Ctrl Pts',(-9.32502343100006,15.2,-5.66048338800002));
#274823=CARTESIAN_POINT('Ctrl Pts',(-9.32502343100006,11.6,-5.66048338800002));
#274824=CARTESIAN_POINT('Ctrl Pts',(-9.32220795200006,15.2,-5.65985166300001));
#274825=CARTESIAN_POINT('Ctrl Pts',(-9.32220795200006,11.6,-5.65985166300001));
#274826=CARTESIAN_POINT('Ctrl Pts',(-9.31939842900006,15.2,-5.65921882600002));
#274827=CARTESIAN_POINT('Ctrl Pts',(-9.31939842900006,11.6,-5.65921882600002));
#274828=CARTESIAN_POINT('Ctrl Pts',(-9.31659486700006,15.2,-5.65858488800002));
#274829=CARTESIAN_POINT('Ctrl Pts',(-9.31659486700006,11.6,-5.65858488800002));
#274830=CARTESIAN_POINT('Ctrl Pts',(-9.31379727700006,15.2,-5.65794986000002));
#274831=CARTESIAN_POINT('Ctrl Pts',(-9.31379727700006,11.6,-5.65794986000002));
#274832=CARTESIAN_POINT('Ctrl Pts',(-9.31100566500006,15.2,-5.65731375100002));
#274833=CARTESIAN_POINT('Ctrl Pts',(-9.31100566500006,11.6,-5.65731375100002));
#274834=CARTESIAN_POINT('Ctrl Pts',(-9.30822003900006,15.2,-5.65667657100001));
#274835=CARTESIAN_POINT('Ctrl Pts',(-9.30822003900006,11.6,-5.65667657100001));
#274836=CARTESIAN_POINT('Ctrl Pts',(-9.30544040900006,15.2,-5.65603833100001));
#274837=CARTESIAN_POINT('Ctrl Pts',(-9.30544040900006,11.6,-5.65603833100001));
#274838=CARTESIAN_POINT('Ctrl Pts',(-9.30266678100006,15.2,-5.65539904000002));
#274839=CARTESIAN_POINT('Ctrl Pts',(-9.30266678100006,11.6,-5.65539904000002));
#274840=CARTESIAN_POINT('Ctrl Pts',(-9.29989916500006,15.2,-5.65475871000002));
#274841=CARTESIAN_POINT('Ctrl Pts',(-9.29989916500006,11.6,-5.65475871000002));
#274842=CARTESIAN_POINT('Ctrl Pts',(-9.29713756800006,15.2,-5.65411734800002));
#274843=CARTESIAN_POINT('Ctrl Pts',(-9.29713756800006,11.6,-5.65411734800002));
#274844=CARTESIAN_POINT('Ctrl Pts',(-9.29438199800006,15.2,-5.65347496700002));
#274845=CARTESIAN_POINT('Ctrl Pts',(-9.29438199800006,11.6,-5.65347496700002));
#274846=CARTESIAN_POINT('Ctrl Pts',(-9.29163246500006,15.2,-5.65283157600001));
#274847=CARTESIAN_POINT('Ctrl Pts',(-9.29163246500006,11.6,-5.65283157600001));
#274848=CARTESIAN_POINT('Ctrl Pts',(-9.28888897500006,15.2,-5.65218718600002));
#274849=CARTESIAN_POINT('Ctrl Pts',(-9.28888897500006,11.6,-5.65218718600002));
#274850=CARTESIAN_POINT('Ctrl Pts',(-9.28615153700006,15.2,-5.65154180700001));
#274851=CARTESIAN_POINT('Ctrl Pts',(-9.28615153700006,11.6,-5.65154180700001));
#274852=CARTESIAN_POINT('Ctrl Pts',(-9.28342015900006,15.2,-5.65089545000002));
#274853=CARTESIAN_POINT('Ctrl Pts',(-9.28342015900006,11.6,-5.65089545000002));
#274854=CARTESIAN_POINT('Ctrl Pts',(-9.28069485100006,15.2,-5.65024812400001));
#274855=CARTESIAN_POINT('Ctrl Pts',(-9.28069485100006,11.6,-5.65024812400001));
#274856=CARTESIAN_POINT('Ctrl Pts',(-9.27797561900006,15.2,-5.64959984000001));
#274857=CARTESIAN_POINT('Ctrl Pts',(-9.27797561900006,11.6,-5.64959984000001));
#274858=CARTESIAN_POINT('Ctrl Pts',(-9.27526247200005,15.2,-5.64895060900001));
#274859=CARTESIAN_POINT('Ctrl Pts',(-9.27526247200005,11.6,-5.64895060900001));
#274860=CARTESIAN_POINT('Ctrl Pts',(-9.27255541900006,15.2,-5.64830044000002));
#274861=CARTESIAN_POINT('Ctrl Pts',(-9.27255541900006,11.6,-5.64830044000002));
#274862=CARTESIAN_POINT('Ctrl Pts',(-9.26985446700006,15.2,-5.64764934600001));
#274863=CARTESIAN_POINT('Ctrl Pts',(-9.26985446700006,11.6,-5.64764934600001));
#274864=CARTESIAN_POINT('Ctrl Pts',(-9.26715962600005,15.2,-5.64699733600001));
#274865=CARTESIAN_POINT('Ctrl Pts',(-9.26715962600005,11.6,-5.64699733600001));
#274866=CARTESIAN_POINT('Ctrl Pts',(-9.26447090200006,15.2,-5.64634441900001));
#274867=CARTESIAN_POINT('Ctrl Pts',(-9.26447090200006,11.6,-5.64634441900001));
#274868=CARTESIAN_POINT('Ctrl Pts',(-9.26178830500006,15.2,-5.64569061000002));
#274869=CARTESIAN_POINT('Ctrl Pts',(-9.26178830500006,11.6,-5.64569061000002));
#274870=CARTESIAN_POINT('Ctrl Pts',(-9.25911184300006,15.2,-5.64503591500001));
#274871=CARTESIAN_POINT('Ctrl Pts',(-9.25911184300006,11.6,-5.64503591500001));
#274872=CARTESIAN_POINT('Ctrl Pts',(-9.25644152500006,15.2,-5.64438034700002));
#274873=CARTESIAN_POINT('Ctrl Pts',(-9.25644152500006,11.6,-5.64438034700002));
#274874=CARTESIAN_POINT('Ctrl Pts',(-9.25377735900006,15.2,-5.64372391600001));
#274875=CARTESIAN_POINT('Ctrl Pts',(-9.25377735900006,11.6,-5.64372391600001));
#274876=CARTESIAN_POINT('Ctrl Pts',(-9.25111935200006,15.2,-5.64306663200002));
#274877=CARTESIAN_POINT('Ctrl Pts',(-9.25111935200006,11.6,-5.64306663200002));
#274878=CARTESIAN_POINT('Ctrl Pts',(-9.24846751400005,15.2,-5.64240850900001));
#274879=CARTESIAN_POINT('Ctrl Pts',(-9.24846751400005,11.6,-5.64240850900001));
#274880=CARTESIAN_POINT('Ctrl Pts',(-9.24582185200006,15.2,-5.64174955400001));
#274881=CARTESIAN_POINT('Ctrl Pts',(-9.24582185200006,11.6,-5.64174955400001));
#274882=CARTESIAN_POINT('Ctrl Pts',(-9.24318237700006,15.2,-5.64108978000001));
#274883=CARTESIAN_POINT('Ctrl Pts',(-9.24318237700006,11.6,-5.64108978000001));
#274884=CARTESIAN_POINT('Ctrl Pts',(-9.24054909400006,15.2,-5.64042919800002));
#274885=CARTESIAN_POINT('Ctrl Pts',(-9.24054909400006,11.6,-5.64042919800002));
#274886=CARTESIAN_POINT('Ctrl Pts',(-9.23792201400006,15.2,-5.63976781700001));
#274887=CARTESIAN_POINT('Ctrl Pts',(-9.23792201400006,11.6,-5.63976781700001));
#274888=CARTESIAN_POINT('Ctrl Pts',(-9.23530114500006,15.2,-5.63910565000001));
#274889=CARTESIAN_POINT('Ctrl Pts',(-9.23530114500006,11.6,-5.63910565000001));
#274890=CARTESIAN_POINT('Ctrl Pts',(-9.23268649500006,15.2,-5.63844270600002));
#274891=CARTESIAN_POINT('Ctrl Pts',(-9.23268649500006,11.6,-5.63844270600002));
#274892=CARTESIAN_POINT('Ctrl Pts',(-9.23007807100005,15.2,-5.63777899800002));
#274893=CARTESIAN_POINT('Ctrl Pts',(-9.23007807100005,11.6,-5.63777899800002));
#274894=CARTESIAN_POINT('Ctrl Pts',(-9.22747588600006,15.2,-5.63711453700002));
#274895=CARTESIAN_POINT('Ctrl Pts',(-9.22747588600006,11.6,-5.63711453700002));
#274896=CARTESIAN_POINT('Ctrl Pts',(-9.22487994400005,15.2,-5.63644933100001));
#274897=CARTESIAN_POINT('Ctrl Pts',(-9.22487994400005,11.6,-5.63644933100001));
#274898=CARTESIAN_POINT('Ctrl Pts',(-9.22229025500006,15.2,-5.63578339500001));
#274899=CARTESIAN_POINT('Ctrl Pts',(-9.22229025500006,11.6,-5.63578339500001));
#274900=CARTESIAN_POINT('Ctrl Pts',(-9.21970682800006,15.2,-5.63511673800001));
#274901=CARTESIAN_POINT('Ctrl Pts',(-9.21970682800006,11.6,-5.63511673800001));
#274902=CARTESIAN_POINT('Ctrl Pts',(-9.21712967100006,15.2,-5.63444937200002));
#274903=CARTESIAN_POINT('Ctrl Pts',(-9.21712967100006,11.6,-5.63444937200002));
#274904=CARTESIAN_POINT('Ctrl Pts',(-9.21455879300006,15.2,-5.63378130700002));
#274905=CARTESIAN_POINT('Ctrl Pts',(-9.21455879300006,11.6,-5.63378130700002));
#274906=CARTESIAN_POINT('Ctrl Pts',(-9.21199420300006,15.2,-5.63311255500002));
#274907=CARTESIAN_POINT('Ctrl Pts',(-9.21199420300006,11.6,-5.63311255500002));
#274908=CARTESIAN_POINT('Ctrl Pts',(-9.20943590900006,15.2,-5.63244312900002));
#274909=CARTESIAN_POINT('Ctrl Pts',(-9.20943590900006,11.6,-5.63244312900002));
#274910=CARTESIAN_POINT('Ctrl Pts',(-9.20688391900006,15.2,-5.63177303700002));
#274911=CARTESIAN_POINT('Ctrl Pts',(-9.20688391900006,11.6,-5.63177303700002));
#274912=CARTESIAN_POINT('Ctrl Pts',(-9.20433824200006,15.2,-5.63110229300001));
#274913=CARTESIAN_POINT('Ctrl Pts',(-9.20433824200006,11.6,-5.63110229300001));
#274914=CARTESIAN_POINT('Ctrl Pts',(-9.20179888700006,15.2,-5.63043090700001));
#274915=CARTESIAN_POINT('Ctrl Pts',(-9.20179888700006,11.6,-5.63043090700001));
#274916=CARTESIAN_POINT('Ctrl Pts',(-9.19926586300006,15.2,-5.62975889100001));
#274917=CARTESIAN_POINT('Ctrl Pts',(-9.19926586300006,11.6,-5.62975889100001));
#274918=CARTESIAN_POINT('Ctrl Pts',(-9.19673917800005,15.2,-5.62908625600001));
#274919=CARTESIAN_POINT('Ctrl Pts',(-9.19673917800005,11.6,-5.62908625600001));
#274920=CARTESIAN_POINT('Ctrl Pts',(-9.19421884100006,15.2,-5.62841301400002));
#274921=CARTESIAN_POINT('Ctrl Pts',(-9.19421884100006,11.6,-5.62841301400002));
#274922=CARTESIAN_POINT('Ctrl Pts',(-9.19170486100005,15.2,-5.62773917700001));
#274923=CARTESIAN_POINT('Ctrl Pts',(-9.19170486100005,11.6,-5.62773917700001));
#274924=CARTESIAN_POINT('Ctrl Pts',(-9.18919724600006,15.2,-5.62706475600002));
#274925=CARTESIAN_POINT('Ctrl Pts',(-9.18919724600006,11.6,-5.62706475600002));
#274926=CARTESIAN_POINT('Ctrl Pts',(-9.18669600500006,15.2,-5.62638976200001));
#274927=CARTESIAN_POINT('Ctrl Pts',(-9.18669600500006,11.6,-5.62638976200001));
#274928=CARTESIAN_POINT('Ctrl Pts',(-9.18420114700006,15.2,-5.62571420700001));
#274929=CARTESIAN_POINT('Ctrl Pts',(-9.18420114700006,11.6,-5.62571420700001));
#274930=CARTESIAN_POINT('Ctrl Pts',(-9.18171268000006,15.2,-5.62503810300001));
#274931=CARTESIAN_POINT('Ctrl Pts',(-9.18171268000006,11.6,-5.62503810300001));
#274932=CARTESIAN_POINT('Ctrl Pts',(-9.17923061300005,15.2,-5.62436146200001));
#274933=CARTESIAN_POINT('Ctrl Pts',(-9.17923061300005,11.6,-5.62436146200001));
#274934=CARTESIAN_POINT('Ctrl Pts',(-9.17675495600006,15.2,-5.62368429500001));
#274935=CARTESIAN_POINT('Ctrl Pts',(-9.17675495600006,11.6,-5.62368429500001));
#274936=CARTESIAN_POINT('Ctrl Pts',(-9.17428571800006,15.2,-5.62300661500001));
#274937=CARTESIAN_POINT('Ctrl Pts',(-9.17428571800006,11.6,-5.62300661500001));
#274938=CARTESIAN_POINT('Ctrl Pts',(-9.17182290500006,15.2,-5.62232843300002));
#274939=CARTESIAN_POINT('Ctrl Pts',(-9.17182290500006,11.6,-5.62232843300002));
#274940=CARTESIAN_POINT('Ctrl Pts',(-9.16936652800005,15.2,-5.62164975900002));
#274941=CARTESIAN_POINT('Ctrl Pts',(-9.16936652800005,11.6,-5.62164975900002));
#274942=CARTESIAN_POINT('Ctrl Pts',(-9.16691659500006,15.2,-5.62097060900001));
#274943=CARTESIAN_POINT('Ctrl Pts',(-9.16691659500006,11.6,-5.62097060900001));
#274944=CARTESIAN_POINT('Ctrl Pts',(-9.16447311600006,15.2,-5.62029099200001));
#274945=CARTESIAN_POINT('Ctrl Pts',(-9.16447311600006,11.6,-5.62029099200001));
#274946=CARTESIAN_POINT('Ctrl Pts',(-9.16203609900006,15.2,-5.61961092000002));
#274947=CARTESIAN_POINT('Ctrl Pts',(-9.16203609900006,11.6,-5.61961092000002));
#274948=CARTESIAN_POINT('Ctrl Pts',(-9.15960555200006,15.2,-5.61893040700001));
#274949=CARTESIAN_POINT('Ctrl Pts',(-9.15960555200006,11.6,-5.61893040700001));
#274950=CARTESIAN_POINT('Ctrl Pts',(-9.15718148700006,15.2,-5.61824946300002));
#274951=CARTESIAN_POINT('Ctrl Pts',(-9.15718148700006,11.6,-5.61824946300002));
#274952=CARTESIAN_POINT('Ctrl Pts',(-9.15476390900006,15.2,-5.61756810200002));
#274953=CARTESIAN_POINT('Ctrl Pts',(-9.15476390900006,11.6,-5.61756810200002));
#274954=CARTESIAN_POINT('Ctrl Pts',(-9.15235283000005,15.2,-5.61688633300002));
#274955=CARTESIAN_POINT('Ctrl Pts',(-9.15235283000005,11.6,-5.61688633300002));
#274956=CARTESIAN_POINT('Ctrl Pts',(-9.14994825800006,15.2,-5.61620417200002));
#274957=CARTESIAN_POINT('Ctrl Pts',(-9.14994825800006,11.6,-5.61620417200002));
#274958=CARTESIAN_POINT('Ctrl Pts',(-9.14755020200005,15.2,-5.61552162900002));
#274959=CARTESIAN_POINT('Ctrl Pts',(-9.14755020200005,11.6,-5.61552162900002));
#274960=CARTESIAN_POINT('Ctrl Pts',(-9.14515866900006,15.2,-5.61483871700001));
#274961=CARTESIAN_POINT('Ctrl Pts',(-9.14515866900006,11.6,-5.61483871700001));
#274962=CARTESIAN_POINT('Ctrl Pts',(-9.14277367200006,15.2,-5.61415544800001));
#274963=CARTESIAN_POINT('Ctrl Pts',(-9.14277367200006,11.6,-5.61415544800001));
#274964=CARTESIAN_POINT('Ctrl Pts',(-9.14039521600006,15.2,-5.61347183400001));
#274965=CARTESIAN_POINT('Ctrl Pts',(-9.14039521600006,11.6,-5.61347183400001));
#274966=CARTESIAN_POINT('Ctrl Pts',(-9.13802331300005,15.2,-5.61278788800001));
#274967=CARTESIAN_POINT('Ctrl Pts',(-9.13802331300005,11.6,-5.61278788800001));
#274968=CARTESIAN_POINT('Ctrl Pts',(-9.13565797000006,15.2,-5.61210362300002));
#274969=CARTESIAN_POINT('Ctrl Pts',(-9.13565797000006,11.6,-5.61210362300002));
#274970=CARTESIAN_POINT('Ctrl Pts',(-9.13329919900006,15.2,-5.61141905000001));
#274971=CARTESIAN_POINT('Ctrl Pts',(-9.13329919900006,11.6,-5.61141905000001));
#274972=CARTESIAN_POINT('Ctrl Pts',(-9.13094700500006,15.2,-5.61073418300001));
#274973=CARTESIAN_POINT('Ctrl Pts',(-9.13094700500006,11.6,-5.61073418300001));
#274974=CARTESIAN_POINT('Ctrl Pts',(-9.12860140000006,15.2,-5.61004903300002));
#274975=CARTESIAN_POINT('Ctrl Pts',(-9.12860140000006,11.6,-5.61004903300002));
#274976=CARTESIAN_POINT('Ctrl Pts',(-9.12626239200005,15.2,-5.60936361300001));
#274977=CARTESIAN_POINT('Ctrl Pts',(-9.12626239200005,11.6,-5.60936361300001));
#274978=CARTESIAN_POINT('Ctrl Pts',(-9.12392999100006,15.2,-5.60867793700002));
#274979=CARTESIAN_POINT('Ctrl Pts',(-9.12392999100006,11.6,-5.60867793700002));
#274980=CARTESIAN_POINT('Ctrl Pts',(-9.12160420500006,15.2,-5.60799201600001));
#274981=CARTESIAN_POINT('Ctrl Pts',(-9.12160420500006,11.6,-5.60799201600001));
#274982=CARTESIAN_POINT('Ctrl Pts',(-9.11928504400005,15.2,-5.60730586400001));
#274983=CARTESIAN_POINT('Ctrl Pts',(-9.11928504400005,11.6,-5.60730586400001));
#274984=CARTESIAN_POINT('Ctrl Pts',(-9.11697251700006,15.2,-5.60661949300002));
#274985=CARTESIAN_POINT('Ctrl Pts',(-9.11697251700006,11.6,-5.60661949300002));
#274986=CARTESIAN_POINT('Ctrl Pts',(-9.11466663400006,15.2,-5.60593291600001));
#274987=CARTESIAN_POINT('Ctrl Pts',(-9.11466663400006,11.6,-5.60593291600001));
#274988=CARTESIAN_POINT('Ctrl Pts',(-9.11236740200006,15.2,-5.60524614600002));
#274989=CARTESIAN_POINT('Ctrl Pts',(-9.11236740200006,11.6,-5.60524614600002));
#274990=CARTESIAN_POINT('Ctrl Pts',(-9.11007483200006,15.2,-5.60455919500002));
#274991=CARTESIAN_POINT('Ctrl Pts',(-9.11007483200006,11.6,-5.60455919500002));
#274992=CARTESIAN_POINT('Ctrl Pts',(-9.10778893400006,15.2,-5.60387207800002));
#274993=CARTESIAN_POINT('Ctrl Pts',(-9.10778893400006,11.6,-5.60387207800002));
#274994=CARTESIAN_POINT('Ctrl Pts',(-9.10550971500006,15.2,-5.60318480500001));
#274995=CARTESIAN_POINT('Ctrl Pts',(-9.10550971500006,11.6,-5.60318480500001));
#274996=CARTESIAN_POINT('Ctrl Pts',(-9.10323718600005,15.2,-5.60249739200001));
#274997=CARTESIAN_POINT('Ctrl Pts',(-9.10323718600005,11.6,-5.60249739200001));
#274998=CARTESIAN_POINT('Ctrl Pts',(-9.10097135600006,15.2,-5.60180985000001));
#274999=CARTESIAN_POINT('Ctrl Pts',(-9.10097135600006,11.6,-5.60180985000001));
#275000=CARTESIAN_POINT('Ctrl Pts',(-9.09871223500006,15.2,-5.60112219300001));
#275001=CARTESIAN_POINT('Ctrl Pts',(-9.09871223500006,11.6,-5.60112219300001));
#275002=CARTESIAN_POINT('Ctrl Pts',(-9.09645983100006,15.2,-5.60043443500001));
#275003=CARTESIAN_POINT('Ctrl Pts',(-9.09645983100006,11.6,-5.60043443500001));
#275004=CARTESIAN_POINT('Ctrl Pts',(-9.09421415200006,15.2,-5.59974658700002));
#275005=CARTESIAN_POINT('Ctrl Pts',(-9.09421415200006,11.6,-5.59974658700002));
#275006=CARTESIAN_POINT('Ctrl Pts',(-9.09197521100005,15.2,-5.59905866400001));
#275007=CARTESIAN_POINT('Ctrl Pts',(-9.09197521100005,11.6,-5.59905866400001));
#275008=CARTESIAN_POINT('Ctrl Pts',(-9.08974301600006,15.2,-5.59837067900002));
#275009=CARTESIAN_POINT('Ctrl Pts',(-9.08974301600006,11.6,-5.59837067900002));
#275010=CARTESIAN_POINT('Ctrl Pts',(-9.08751757500006,15.2,-5.59768264400001));
#275011=CARTESIAN_POINT('Ctrl Pts',(-9.08751757500006,11.6,-5.59768264400001));
#275012=CARTESIAN_POINT('Ctrl Pts',(-9.08529889900005,15.2,-5.59699457500002));
#275013=CARTESIAN_POINT('Ctrl Pts',(-9.08529889900005,11.6,-5.59699457500002));
#275014=CARTESIAN_POINT('Ctrl Pts',(-9.08308699800006,15.2,-5.59630648300002));
#275015=CARTESIAN_POINT('Ctrl Pts',(-9.08308699800006,11.6,-5.59630648300002));
#275016=CARTESIAN_POINT('Ctrl Pts',(-9.08088188000006,15.2,-5.59561838200001));
#275017=CARTESIAN_POINT('Ctrl Pts',(-9.08088188000006,11.6,-5.59561838200001));
#275018=CARTESIAN_POINT('Ctrl Pts',(-9.07868355400005,15.2,-5.59493028700001));
#275019=CARTESIAN_POINT('Ctrl Pts',(-9.07868355400005,11.6,-5.59493028700001));
#275020=CARTESIAN_POINT('Ctrl Pts',(-9.07649203200006,15.2,-5.59424221100001));
#275021=CARTESIAN_POINT('Ctrl Pts',(-9.07649203200006,11.6,-5.59424221100001));
#275022=CARTESIAN_POINT('Ctrl Pts',(-9.07430732100006,15.2,-5.59355416500001));
#275023=CARTESIAN_POINT('Ctrl Pts',(-9.07430732100006,11.6,-5.59355416500001));
#275024=CARTESIAN_POINT('Ctrl Pts',(-9.07212943200006,15.2,-5.59286616700001));
#275025=CARTESIAN_POINT('Ctrl Pts',(-9.07212943200006,11.6,-5.59286616700001));
#275026=CARTESIAN_POINT('Ctrl Pts',(-9.06995837500006,15.2,-5.59217822700001));
#275027=CARTESIAN_POINT('Ctrl Pts',(-9.06995837500006,11.6,-5.59217822700001));
#275028=CARTESIAN_POINT('Ctrl Pts',(-9.06779415800005,15.2,-5.59149036100001));
#275029=CARTESIAN_POINT('Ctrl Pts',(-9.06779415800005,11.6,-5.59149036100001));
#275030=CARTESIAN_POINT('Ctrl Pts',(-9.06563679200006,15.2,-5.59080258200002));
#275031=CARTESIAN_POINT('Ctrl Pts',(-9.06563679200006,11.6,-5.59080258200002));
#275032=CARTESIAN_POINT('Ctrl Pts',(-9.06348628500006,15.2,-5.59011490300001));
#275033=CARTESIAN_POINT('Ctrl Pts',(-9.06348628500006,11.6,-5.59011490300001));
#275034=CARTESIAN_POINT('Ctrl Pts',(-9.06134264800006,15.2,-5.58942734000002));
#275035=CARTESIAN_POINT('Ctrl Pts',(-9.06134264800006,11.6,-5.58942734000002));
#275036=CARTESIAN_POINT('Ctrl Pts',(-9.05920589100005,15.2,-5.58873990500001));
#275037=CARTESIAN_POINT('Ctrl Pts',(-9.05920589100005,11.6,-5.58873990500001));
#275038=CARTESIAN_POINT('Ctrl Pts',(-9.05707602300006,15.2,-5.58805261300002));
#275039=CARTESIAN_POINT('Ctrl Pts',(-9.05707602300006,11.6,-5.58805261300002));
#275040=CARTESIAN_POINT('Ctrl Pts',(-9.05495305400006,15.2,-5.58736547900001));
#275041=CARTESIAN_POINT('Ctrl Pts',(-9.05495305400006,11.6,-5.58736547900001));
#275042=CARTESIAN_POINT('Ctrl Pts',(-9.05283699300006,15.2,-5.58667851400001));
#275043=CARTESIAN_POINT('Ctrl Pts',(-9.05283699300006,11.6,-5.58667851400001));
#275044=CARTESIAN_POINT('Ctrl Pts',(-9.05072785100005,15.2,-5.58599173500001));
#275045=CARTESIAN_POINT('Ctrl Pts',(-9.05072785100005,11.6,-5.58599173500001));
#275046=CARTESIAN_POINT('Ctrl Pts',(-9.04862563600006,15.2,-5.58530515500001));
#275047=CARTESIAN_POINT('Ctrl Pts',(-9.04862563600006,11.6,-5.58530515500001));
#275048=CARTESIAN_POINT('Ctrl Pts',(-9.04653036000006,15.2,-5.58461878900002));
#275049=CARTESIAN_POINT('Ctrl Pts',(-9.04653036000006,11.6,-5.58461878900002));
#275050=CARTESIAN_POINT('Ctrl Pts',(-9.04444203100006,15.2,-5.58393265000001));
#275051=CARTESIAN_POINT('Ctrl Pts',(-9.04444203100006,11.6,-5.58393265000001));
#275052=CARTESIAN_POINT('Ctrl Pts',(-9.04236066000006,15.2,-5.58324675400002));
#275053=CARTESIAN_POINT('Ctrl Pts',(-9.04236066000006,11.6,-5.58324675400002));
#275054=CARTESIAN_POINT('Ctrl Pts',(-9.04028625700006,15.2,-5.58256111400001));
#275055=CARTESIAN_POINT('Ctrl Pts',(-9.04028625700006,11.6,-5.58256111400001));
#275056=CARTESIAN_POINT('Ctrl Pts',(-9.03821883100006,15.2,-5.58187574600002));
#275057=CARTESIAN_POINT('Ctrl Pts',(-9.03821883100006,11.6,-5.58187574600002));
#275058=CARTESIAN_POINT('Ctrl Pts',(-9.03615839200006,15.2,-5.58119066200002));
#275059=CARTESIAN_POINT('Ctrl Pts',(-9.03615839200006,11.6,-5.58119066200002));
#275060=CARTESIAN_POINT('Ctrl Pts',(-9.03410494900006,15.2,-5.58050587900001));
#275061=CARTESIAN_POINT('Ctrl Pts',(-9.03410494900006,11.6,-5.58050587900001));
#275062=CARTESIAN_POINT('Ctrl Pts',(-9.03205851500006,15.2,-5.57982141200001));
#275063=CARTESIAN_POINT('Ctrl Pts',(-9.03205851500006,11.6,-5.57982141200001));
#275064=CARTESIAN_POINT('Ctrl Pts',(-9.03001909700006,15.2,-5.57913727300001));
#275065=CARTESIAN_POINT('Ctrl Pts',(-9.03001909700006,11.6,-5.57913727300001));
#275066=CARTESIAN_POINT('Ctrl Pts',(-9.02798670700006,15.2,-5.57845347800002));
#275067=CARTESIAN_POINT('Ctrl Pts',(-9.02798670700006,11.6,-5.57845347800002));
#275068=CARTESIAN_POINT('Ctrl Pts',(-9.02596135300006,15.2,-5.57777004200001));
#275069=CARTESIAN_POINT('Ctrl Pts',(-9.02596135300006,11.6,-5.57777004200001));
#275070=CARTESIAN_POINT('Ctrl Pts',(-9.02394304700006,15.2,-5.57708698000001));
#275071=CARTESIAN_POINT('Ctrl Pts',(-9.02394304700006,11.6,-5.57708698000001));
#275072=CARTESIAN_POINT('Ctrl Pts',(-9.02193179700006,15.2,-5.57640430700001));
#275073=CARTESIAN_POINT('Ctrl Pts',(-9.02193179700006,11.6,-5.57640430700001));
#275074=CARTESIAN_POINT('Ctrl Pts',(-9.01992761500006,15.2,-5.57572203700001));
#275075=CARTESIAN_POINT('Ctrl Pts',(-9.01992761500006,11.6,-5.57572203700001));
#275076=CARTESIAN_POINT('Ctrl Pts',(-9.01793051100006,15.2,-5.57504018600001));
#275077=CARTESIAN_POINT('Ctrl Pts',(-9.01793051100006,11.6,-5.57504018600001));
#275078=CARTESIAN_POINT('Ctrl Pts',(-9.01594049400006,15.2,-5.57435876800001));
#275079=CARTESIAN_POINT('Ctrl Pts',(-9.01594049400006,11.6,-5.57435876800001));
#275080=CARTESIAN_POINT('Ctrl Pts',(-9.01395757400006,15.2,-5.57367779900002));
#275081=CARTESIAN_POINT('Ctrl Pts',(-9.01395757400006,11.6,-5.57367779900002));
#275082=CARTESIAN_POINT('Ctrl Pts',(-9.01198176300005,15.2,-5.57299729300002));
#275083=CARTESIAN_POINT('Ctrl Pts',(-9.01198176300005,11.6,-5.57299729300002));
#275084=CARTESIAN_POINT('Ctrl Pts',(-9.01001306900006,15.2,-5.57231726600001));
#275085=CARTESIAN_POINT('Ctrl Pts',(-9.01001306900006,11.6,-5.57231726600001));
#275086=CARTESIAN_POINT('Ctrl Pts',(-9.00805150400006,15.2,-5.57163773500001));
#275087=CARTESIAN_POINT('Ctrl Pts',(-9.00805150400006,11.6,-5.57163773500001));
#275088=CARTESIAN_POINT('Ctrl Pts',(-9.00609707700006,15.2,-5.57095871100001));
#275089=CARTESIAN_POINT('Ctrl Pts',(-9.00609707700006,11.6,-5.57095871100001));
#275090=CARTESIAN_POINT('Ctrl Pts',(-9.00414979900006,15.2,-5.57028021300002));
#275091=CARTESIAN_POINT('Ctrl Pts',(-9.00414979900006,11.6,-5.57028021300002));
#275092=CARTESIAN_POINT('Ctrl Pts',(-9.00220967900006,15.2,-5.56960225700001));
#275093=CARTESIAN_POINT('Ctrl Pts',(-9.00220967900006,11.6,-5.56960225700001));
#275094=CARTESIAN_POINT('Ctrl Pts',(-9.00027673000006,15.2,-5.56892485600001));
#275095=CARTESIAN_POINT('Ctrl Pts',(-9.00027673000006,11.6,-5.56892485600001));
#275096=CARTESIAN_POINT('Ctrl Pts',(-8.99835095900006,15.2,-5.56824802500001));
#275097=CARTESIAN_POINT('Ctrl Pts',(-8.99835095900006,11.6,-5.56824802500001));
#275098=CARTESIAN_POINT('Ctrl Pts',(-8.99643237900005,15.2,-5.56757178200002));
#275099=CARTESIAN_POINT('Ctrl Pts',(-8.99643237900005,11.6,-5.56757178200002));
#275100=CARTESIAN_POINT('Ctrl Pts',(-8.99452100000006,15.2,-5.56689614200002));
#275101=CARTESIAN_POINT('Ctrl Pts',(-8.99452100000006,11.6,-5.56689614200002));
#275102=CARTESIAN_POINT('Ctrl Pts',(-8.99261683100006,15.2,-5.56622112000001));
#275103=CARTESIAN_POINT('Ctrl Pts',(-8.99261683100006,11.6,-5.56622112000001));
#275104=CARTESIAN_POINT('Ctrl Pts',(-8.99071988300006,15.2,-5.56554673300001));
#275105=CARTESIAN_POINT('Ctrl Pts',(-8.99071988300006,11.6,-5.56554673300001));
#275106=CARTESIAN_POINT('Ctrl Pts',(-8.98883016700006,15.2,-5.56487299500001));
#275107=CARTESIAN_POINT('Ctrl Pts',(-8.98883016700006,11.6,-5.56487299500001));
#275108=CARTESIAN_POINT('Ctrl Pts',(-8.98694769300005,15.2,-5.56419992300001));
#275109=CARTESIAN_POINT('Ctrl Pts',(-8.98694769300005,11.6,-5.56419992300001));
#275110=CARTESIAN_POINT('Ctrl Pts',(-8.98507247200006,15.2,-5.56352753400001));
#275111=CARTESIAN_POINT('Ctrl Pts',(-8.98507247200006,11.6,-5.56352753400001));
#275112=CARTESIAN_POINT('Ctrl Pts',(-8.98320451500006,15.2,-5.56285584200001));
#275113=CARTESIAN_POINT('Ctrl Pts',(-8.98320451500006,11.6,-5.56285584200001));
#275114=CARTESIAN_POINT('Ctrl Pts',(-8.98134383200006,15.2,-5.56218486400001));
#275115=CARTESIAN_POINT('Ctrl Pts',(-8.98134383200006,11.6,-5.56218486400001));
#275116=CARTESIAN_POINT('Ctrl Pts',(-8.97949043200006,15.2,-5.56151461700002));
#275117=CARTESIAN_POINT('Ctrl Pts',(-8.97949043200006,11.6,-5.56151461700002));
#275118=CARTESIAN_POINT('Ctrl Pts',(-8.97764432800006,15.2,-5.56084511500002));
#275119=CARTESIAN_POINT('Ctrl Pts',(-8.97764432800006,11.6,-5.56084511500002));
#275120=CARTESIAN_POINT('Ctrl Pts',(-8.97580552900006,15.2,-5.56017637700001));
#275121=CARTESIAN_POINT('Ctrl Pts',(-8.97580552900006,11.6,-5.56017637700001));
#275122=CARTESIAN_POINT('Ctrl Pts',(-8.97397404700006,15.2,-5.55950841800001));
#275123=CARTESIAN_POINT('Ctrl Pts',(-8.97397404700006,11.6,-5.55950841800001));
#275124=CARTESIAN_POINT('Ctrl Pts',(-8.97214989200006,15.2,-5.55884125300001));
#275125=CARTESIAN_POINT('Ctrl Pts',(-8.97214989200006,11.6,-5.55884125300001));
#275126=CARTESIAN_POINT('Ctrl Pts',(-8.97033307400006,15.2,-5.55817490100001));
#275127=CARTESIAN_POINT('Ctrl Pts',(-8.97033307400006,11.6,-5.55817490100001));
#275128=CARTESIAN_POINT('Ctrl Pts',(-8.96852360500005,15.2,-5.55750937700001));
#275129=CARTESIAN_POINT('Ctrl Pts',(-8.96852360500005,11.6,-5.55750937700001));
#275130=CARTESIAN_POINT('Ctrl Pts',(-8.96672149500005,15.2,-5.55684469700001));
#275131=CARTESIAN_POINT('Ctrl Pts',(-8.96672149500005,11.6,-5.55684469700001));
#275132=CARTESIAN_POINT('Ctrl Pts',(-8.96492675600006,15.2,-5.55618088000001));
#275133=CARTESIAN_POINT('Ctrl Pts',(-8.96492675600006,11.6,-5.55618088000001));
#275134=CARTESIAN_POINT('Ctrl Pts',(-8.96313939700006,15.2,-5.55551794000001));
#275135=CARTESIAN_POINT('Ctrl Pts',(-8.96313939700006,11.6,-5.55551794000001));
#275136=CARTESIAN_POINT('Ctrl Pts',(-8.96135943000005,15.2,-5.55485589600002));
#275137=CARTESIAN_POINT('Ctrl Pts',(-8.96135943000005,11.6,-5.55485589600002));
#275138=CARTESIAN_POINT('Ctrl Pts',(-8.95958686500006,15.2,-5.55419476300001));
#275139=CARTESIAN_POINT('Ctrl Pts',(-8.95958686500006,11.6,-5.55419476300001));
#275140=CARTESIAN_POINT('Ctrl Pts',(-8.95782171400005,15.2,-5.55353456000002));
#275141=CARTESIAN_POINT('Ctrl Pts',(-8.95782171400005,11.6,-5.55353456000002));
#275142=CARTESIAN_POINT('Ctrl Pts',(-8.95606398700006,15.2,-5.55287530100002));
#275143=CARTESIAN_POINT('Ctrl Pts',(-8.95606398700006,11.6,-5.55287530100002));
#275144=CARTESIAN_POINT('Ctrl Pts',(-8.95431369600006,15.2,-5.55221700600002));
#275145=CARTESIAN_POINT('Ctrl Pts',(-8.95431369600006,11.6,-5.55221700600002));
#275146=CARTESIAN_POINT('Ctrl Pts',(-8.95257085100006,15.2,-5.55155969100001));
#275147=CARTESIAN_POINT('Ctrl Pts',(-8.95257085100006,11.6,-5.55155969100001));
#275148=CARTESIAN_POINT('Ctrl Pts',(-8.95083546400006,15.2,-5.55090337200001));
#275149=CARTESIAN_POINT('Ctrl Pts',(-8.95083546400006,11.6,-5.55090337200001));
#275150=CARTESIAN_POINT('Ctrl Pts',(-8.94910754500006,15.2,-5.55024806800001));
#275151=CARTESIAN_POINT('Ctrl Pts',(-8.94910754500006,11.6,-5.55024806800001));
#275152=CARTESIAN_POINT('Ctrl Pts',(-8.94738710500006,15.2,-5.54959379500001));
#275153=CARTESIAN_POINT('Ctrl Pts',(-8.94738710500006,11.6,-5.54959379500001));
#275154=CARTESIAN_POINT('Ctrl Pts',(-8.94567415700006,15.2,-5.54894057200002));
#275155=CARTESIAN_POINT('Ctrl Pts',(-8.94567415700006,11.6,-5.54894057200002));
#275156=CARTESIAN_POINT('Ctrl Pts',(-8.94396871000006,15.2,-5.54828841500001));
#275157=CARTESIAN_POINT('Ctrl Pts',(-8.94396871000006,11.6,-5.54828841500001));
#275158=CARTESIAN_POINT('Ctrl Pts',(-8.94227077600006,15.2,-5.54763734200002));
#275159=CARTESIAN_POINT('Ctrl Pts',(-8.94227077600006,11.6,-5.54763734200002));
#275160=CARTESIAN_POINT('Ctrl Pts',(-8.94058036500006,15.2,-5.54698737000002));
#275161=CARTESIAN_POINT('Ctrl Pts',(-8.94058036500006,11.6,-5.54698737000002));
#275162=CARTESIAN_POINT('Ctrl Pts',(-8.93889749100006,15.2,-5.54633851800002));
#275163=CARTESIAN_POINT('Ctrl Pts',(-8.93889749100006,11.6,-5.54633851800002));
#275164=CARTESIAN_POINT('Ctrl Pts',(-8.93722216300005,15.2,-5.54569080200002));
#275165=CARTESIAN_POINT('Ctrl Pts',(-8.93722216300005,11.6,-5.54569080200002));
#275166=CARTESIAN_POINT('Ctrl Pts',(-8.93555439300006,15.2,-5.54504424100001));
#275167=CARTESIAN_POINT('Ctrl Pts',(-8.93555439300006,11.6,-5.54504424100001));
#275168=CARTESIAN_POINT('Ctrl Pts',(-8.93389419300006,15.2,-5.54439885300001));
#275169=CARTESIAN_POINT('Ctrl Pts',(-8.93389419300006,11.6,-5.54439885300001));
#275170=CARTESIAN_POINT('Ctrl Pts',(-8.93224157200006,15.2,-5.54375465500001));
#275171=CARTESIAN_POINT('Ctrl Pts',(-8.93224157200006,11.6,-5.54375465500001));
#275172=CARTESIAN_POINT('Ctrl Pts',(-8.93059654400006,15.2,-5.54311166500002));
#275173=CARTESIAN_POINT('Ctrl Pts',(-8.93059654400006,11.6,-5.54311166500002));
#275174=CARTESIAN_POINT('Ctrl Pts',(-8.92895911900006,15.2,-5.54246990200001));
#275175=CARTESIAN_POINT('Ctrl Pts',(-8.92895911900006,11.6,-5.54246990200001));
#275176=CARTESIAN_POINT('Ctrl Pts',(-8.92732930900005,15.2,-5.54182938400002));
#275177=CARTESIAN_POINT('Ctrl Pts',(-8.92732930900005,11.6,-5.54182938400002));
#275178=CARTESIAN_POINT('Ctrl Pts',(-8.92570712400006,15.2,-5.54119012900002));
#275179=CARTESIAN_POINT('Ctrl Pts',(-8.92570712400006,11.6,-5.54119012900002));
#275180=CARTESIAN_POINT('Ctrl Pts',(-8.92409257800006,15.2,-5.54055215500001));
#275181=CARTESIAN_POINT('Ctrl Pts',(-8.92409257800006,11.6,-5.54055215500001));
#275182=CARTESIAN_POINT('Ctrl Pts',(-8.92248568200005,15.2,-5.53991548100001));
#275183=CARTESIAN_POINT('Ctrl Pts',(-8.92248568200005,11.6,-5.53991548100001));
#275184=CARTESIAN_POINT('Ctrl Pts',(-8.92088644600006,15.2,-5.53928012400001));
#275185=CARTESIAN_POINT('Ctrl Pts',(-8.92088644600006,11.6,-5.53928012400001));
#275186=CARTESIAN_POINT('Ctrl Pts',(-8.91929488200006,15.2,-5.53864610500002));
#275187=CARTESIAN_POINT('Ctrl Pts',(-8.91929488200006,11.6,-5.53864610500002));
#275188=CARTESIAN_POINT('Ctrl Pts',(-8.91771100300006,15.2,-5.53801344000002));
#275189=CARTESIAN_POINT('Ctrl Pts',(-8.91771100300006,11.6,-5.53801344000002));
#275190=CARTESIAN_POINT('Ctrl Pts',(-8.91613481900006,15.2,-5.53738215000001));
#275191=CARTESIAN_POINT('Ctrl Pts',(-8.91613481900006,11.6,-5.53738215000001));
#275192=CARTESIAN_POINT('Ctrl Pts',(-8.91456634200006,15.2,-5.53675225200001));
#275193=CARTESIAN_POINT('Ctrl Pts',(-8.91456634200006,11.6,-5.53675225200001));
#275194=CARTESIAN_POINT('Ctrl Pts',(-8.91300558500006,15.2,-5.53612376600002));
#275195=CARTESIAN_POINT('Ctrl Pts',(-8.91300558500006,11.6,-5.53612376600002));
#275196=CARTESIAN_POINT('Ctrl Pts',(-8.91145255900006,15.2,-5.53549671000001));
#275197=CARTESIAN_POINT('Ctrl Pts',(-8.91145255900006,11.6,-5.53549671000001));
#275198=CARTESIAN_POINT('Ctrl Pts',(-8.90990727500006,15.2,-5.53487110500001));
#275199=CARTESIAN_POINT('Ctrl Pts',(-8.90990727500006,11.6,-5.53487110500001));
#275200=CARTESIAN_POINT('Ctrl Pts',(-8.90836974600006,15.2,-5.53424696600001));
#275201=CARTESIAN_POINT('Ctrl Pts',(-8.90836974600006,11.6,-5.53424696600001));
#275202=CARTESIAN_POINT('Ctrl Pts',(-8.90683998400006,15.2,-5.53362431600001));
#275203=CARTESIAN_POINT('Ctrl Pts',(-8.90683998400006,11.6,-5.53362431600001));
#275204=CARTESIAN_POINT('Ctrl Pts',(-8.90531800000005,15.2,-5.53300317300002));
#275205=CARTESIAN_POINT('Ctrl Pts',(-8.90531800000005,11.6,-5.53300317300002));
#275206=CARTESIAN_POINT('Ctrl Pts',(-8.90380380500006,15.2,-5.53238355600001));
#275207=CARTESIAN_POINT('Ctrl Pts',(-8.90380380500006,11.6,-5.53238355600001));
#275208=CARTESIAN_POINT('Ctrl Pts',(-8.90229741300006,15.2,-5.53176548500002));
#275209=CARTESIAN_POINT('Ctrl Pts',(-8.90229741300006,11.6,-5.53176548500002));
#275210=CARTESIAN_POINT('Ctrl Pts',(-8.90079883600006,15.2,-5.53114897800001));
#275211=CARTESIAN_POINT('Ctrl Pts',(-8.90079883600006,11.6,-5.53114897800001));
#275212=CARTESIAN_POINT('Ctrl Pts',(-8.89930808500005,15.2,-5.53053405700001));
#275213=CARTESIAN_POINT('Ctrl Pts',(-8.89930808500005,11.6,-5.53053405700001));
#275214=CARTESIAN_POINT('Ctrl Pts',(-8.89782517200005,15.2,-5.52992073900001));
#275215=CARTESIAN_POINT('Ctrl Pts',(-8.89782517200005,11.6,-5.52992073900001));
#275216=CARTESIAN_POINT('Ctrl Pts',(-8.89635011000006,15.2,-5.52930904500001));
#275217=CARTESIAN_POINT('Ctrl Pts',(-8.89635011000006,11.6,-5.52930904500001));
#275218=CARTESIAN_POINT('Ctrl Pts',(-8.89488291000006,15.2,-5.52869899600001));
#275219=CARTESIAN_POINT('Ctrl Pts',(-8.89488291000006,11.6,-5.52869899600001));
#275220=CARTESIAN_POINT('Ctrl Pts',(-8.89342358400006,15.2,-5.52809061000001));
#275221=CARTESIAN_POINT('Ctrl Pts',(-8.89342358400006,11.6,-5.52809061000001));
#275222=CARTESIAN_POINT('Ctrl Pts',(-8.89197214600006,15.2,-5.52748390800001));
#275223=CARTESIAN_POINT('Ctrl Pts',(-8.89197214600006,11.6,-5.52748390800001));
#275224=CARTESIAN_POINT('Ctrl Pts',(-8.89052860700006,15.2,-5.52687890900001));
#275225=CARTESIAN_POINT('Ctrl Pts',(-8.89052860700006,11.6,-5.52687890900001));
#275226=CARTESIAN_POINT('Ctrl Pts',(-8.88909298100005,15.2,-5.52627563500002));
#275227=CARTESIAN_POINT('Ctrl Pts',(-8.88909298100005,11.6,-5.52627563500002));
#275228=CARTESIAN_POINT('Ctrl Pts',(-8.88766527700006,15.2,-5.52567410500002));
#275229=CARTESIAN_POINT('Ctrl Pts',(-8.88766527700006,11.6,-5.52567410500002));
#275230=CARTESIAN_POINT('Ctrl Pts',(-8.88624550900006,15.2,-5.52507434000002));
#275231=CARTESIAN_POINT('Ctrl Pts',(-8.88624550900006,11.6,-5.52507434000002));
#275232=CARTESIAN_POINT('Ctrl Pts',(-8.88483369100006,15.2,-5.52447635900001));
#275233=CARTESIAN_POINT('Ctrl Pts',(-8.88483369100006,11.6,-5.52447635900001));
#275234=CARTESIAN_POINT('Ctrl Pts',(-8.88342983400005,15.2,-5.52388018300002));
#275235=CARTESIAN_POINT('Ctrl Pts',(-8.88342983400005,11.6,-5.52388018300002));
#275236=CARTESIAN_POINT('Ctrl Pts',(-8.88203395000006,15.2,-5.52328583400001));
#275237=CARTESIAN_POINT('Ctrl Pts',(-8.88203395000006,11.6,-5.52328583400001));
#275238=CARTESIAN_POINT('Ctrl Pts',(-8.88064605300006,15.2,-5.52269333100002));
#275239=CARTESIAN_POINT('Ctrl Pts',(-8.88064605300006,11.6,-5.52269333100002));
#275240=CARTESIAN_POINT('Ctrl Pts',(-8.87926615400006,15.2,-5.52210269500002));
#275241=CARTESIAN_POINT('Ctrl Pts',(-8.87926615400006,11.6,-5.52210269500002));
#275242=CARTESIAN_POINT('Ctrl Pts',(-8.87789426600006,15.2,-5.52151394800001));
#275243=CARTESIAN_POINT('Ctrl Pts',(-8.87789426600006,11.6,-5.52151394800001));
#275244=CARTESIAN_POINT('Ctrl Pts',(-8.87653040200006,15.2,-5.52092711100002));
#275245=CARTESIAN_POINT('Ctrl Pts',(-8.87653040200006,11.6,-5.52092711100002));
#275246=CARTESIAN_POINT('Ctrl Pts',(-8.87517457600006,15.2,-5.52034220400001));
#275247=CARTESIAN_POINT('Ctrl Pts',(-8.87517457600006,11.6,-5.52034220400001));
#275248=CARTESIAN_POINT('Ctrl Pts',(-8.87382679800006,15.2,-5.51975924800002));
#275249=CARTESIAN_POINT('Ctrl Pts',(-8.87382679800006,11.6,-5.51975924800002));
#275250=CARTESIAN_POINT('Ctrl Pts',(-8.87248708300006,15.2,-5.51917826500001));
#275251=CARTESIAN_POINT('Ctrl Pts',(-8.87248708300006,11.6,-5.51917826500001));
#275252=CARTESIAN_POINT('Ctrl Pts',(-8.87115544200006,15.2,-5.51859927600002));
#275253=CARTESIAN_POINT('Ctrl Pts',(-8.87115544200006,11.6,-5.51859927600002));
#275254=CARTESIAN_POINT('Ctrl Pts',(-8.86983189000006,15.2,-5.51802230200002));
#275255=CARTESIAN_POINT('Ctrl Pts',(-8.86983189000006,11.6,-5.51802230200002));
#275256=CARTESIAN_POINT('Ctrl Pts',(-8.86851643800006,15.2,-5.51744736600002));
#275257=CARTESIAN_POINT('Ctrl Pts',(-8.86851643800006,11.6,-5.51744736600002));
#275258=CARTESIAN_POINT('Ctrl Pts',(-8.86720910000006,15.2,-5.51687448900001));
#275259=CARTESIAN_POINT('Ctrl Pts',(-8.86720910000006,11.6,-5.51687448900001));
#275260=CARTESIAN_POINT('Ctrl Pts',(-8.86590988800006,15.2,-5.51630369100002));
#275261=CARTESIAN_POINT('Ctrl Pts',(-8.86590988800006,11.6,-5.51630369100002));
#275262=CARTESIAN_POINT('Ctrl Pts',(-8.86461881500006,15.2,-5.51573499500002));
#275263=CARTESIAN_POINT('Ctrl Pts',(-8.86461881500006,11.6,-5.51573499500002));
#275264=CARTESIAN_POINT('Ctrl Pts',(-8.86333589600006,15.2,-5.51516842500002));
#275265=CARTESIAN_POINT('Ctrl Pts',(-8.86333589600006,11.6,-5.51516842500002));
#275266=CARTESIAN_POINT('Ctrl Pts',(-8.86206114200006,15.2,-5.51460399900002));
#275267=CARTESIAN_POINT('Ctrl Pts',(-8.86206114200006,11.6,-5.51460399900002));
#275268=CARTESIAN_POINT('Ctrl Pts',(-8.86079456700006,15.2,-5.51404174200002));
#275269=CARTESIAN_POINT('Ctrl Pts',(-8.86079456700006,11.6,-5.51404174200002));
#275270=CARTESIAN_POINT('Ctrl Pts',(-8.85953618500006,15.2,-5.51348167500001));
#275271=CARTESIAN_POINT('Ctrl Pts',(-8.85953618500006,11.6,-5.51348167500001));
#275272=CARTESIAN_POINT('Ctrl Pts',(-8.85828600800006,15.2,-5.51292382200002));
#275273=CARTESIAN_POINT('Ctrl Pts',(-8.85828600800006,11.6,-5.51292382200002));
#275274=CARTESIAN_POINT('Ctrl Pts',(-8.85704404900006,15.2,-5.51236820300002));
#275275=CARTESIAN_POINT('Ctrl Pts',(-8.85704404900006,11.6,-5.51236820300002));
#275276=CARTESIAN_POINT('Ctrl Pts',(-8.85581032300006,15.2,-5.51181484300002));
#275277=CARTESIAN_POINT('Ctrl Pts',(-8.85581032300006,11.6,-5.51181484300002));
#275278=CARTESIAN_POINT('Ctrl Pts',(-8.85458484100005,15.2,-5.51126376300001));
#275279=CARTESIAN_POINT('Ctrl Pts',(-8.85458484100005,11.6,-5.51126376300001));
#275280=CARTESIAN_POINT('Ctrl Pts',(-8.85336761800006,15.2,-5.51071498500002));
#275281=CARTESIAN_POINT('Ctrl Pts',(-8.85336761800006,11.6,-5.51071498500002));
#275282=CARTESIAN_POINT('Ctrl Pts',(-8.85215866800005,15.2,-5.51016853300001));
#275283=CARTESIAN_POINT('Ctrl Pts',(-8.85215866800005,11.6,-5.51016853300001));
#275284=CARTESIAN_POINT('Ctrl Pts',(-8.85095800400006,15.2,-5.50962443100001));
#275285=CARTESIAN_POINT('Ctrl Pts',(-8.85095800400006,11.6,-5.50962443100001));
#275286=CARTESIAN_POINT('Ctrl Pts',(-8.84976563900005,15.2,-5.50908269900001));
#275287=CARTESIAN_POINT('Ctrl Pts',(-8.84976563900005,11.6,-5.50908269900001));
#275288=CARTESIAN_POINT('Ctrl Pts',(-8.84858158700006,15.2,-5.50854336400001));
#275289=CARTESIAN_POINT('Ctrl Pts',(-8.84858158700006,11.6,-5.50854336400001));
#275290=CARTESIAN_POINT('Ctrl Pts',(-8.84740586100006,15.2,-5.50800644600002));
#275291=CARTESIAN_POINT('Ctrl Pts',(-8.84740586100006,11.6,-5.50800644600002));
#275292=CARTESIAN_POINT('Ctrl Pts',(-8.84623847600006,15.2,-5.50747197000002));
#275293=CARTESIAN_POINT('Ctrl Pts',(-8.84623847600006,11.6,-5.50747197000002));
#275294=CARTESIAN_POINT('Ctrl Pts',(-8.84507944500006,15.2,-5.50693996000001));
#275295=CARTESIAN_POINT('Ctrl Pts',(-8.84507944500006,11.6,-5.50693996000001));
#275296=CARTESIAN_POINT('Ctrl Pts',(-8.84392878100006,15.2,-5.50641043700002));
#275297=CARTESIAN_POINT('Ctrl Pts',(-8.84392878100006,11.6,-5.50641043700002));
#275298=CARTESIAN_POINT('Ctrl Pts',(-8.84278650000006,15.2,-5.50588342700001));
#275299=CARTESIAN_POINT('Ctrl Pts',(-8.84278650000006,11.6,-5.50588342700001));
#275300=CARTESIAN_POINT('Ctrl Pts',(-8.84165261400006,15.2,-5.50535895400001));
#275301=CARTESIAN_POINT('Ctrl Pts',(-8.84165261400006,11.6,-5.50535895400001));
#275302=CARTESIAN_POINT('Ctrl Pts',(-8.84052713700006,15.2,-5.50483704100001));
#275303=CARTESIAN_POINT('Ctrl Pts',(-8.84052713700006,11.6,-5.50483704100001));
#275304=CARTESIAN_POINT('Ctrl Pts',(-8.83941008400006,15.2,-5.50431771200001));
#275305=CARTESIAN_POINT('Ctrl Pts',(-8.83941008400006,11.6,-5.50431771200001));
#275306=CARTESIAN_POINT('Ctrl Pts',(-8.83830146800006,15.2,-5.50380099200002));
#275307=CARTESIAN_POINT('Ctrl Pts',(-8.83830146800006,11.6,-5.50380099200002));
#275308=CARTESIAN_POINT('Ctrl Pts',(-8.83720130500006,15.2,-5.50328690400002));
#275309=CARTESIAN_POINT('Ctrl Pts',(-8.83720130500006,11.6,-5.50328690400002));
#275310=CARTESIAN_POINT('Ctrl Pts',(-8.83610960700006,15.2,-5.50277547300002));
#275311=CARTESIAN_POINT('Ctrl Pts',(-8.83610960700006,11.6,-5.50277547300002));
#275312=CARTESIAN_POINT('Ctrl Pts',(-8.83502638900006,15.2,-5.50226672400001));
#275313=CARTESIAN_POINT('Ctrl Pts',(-8.83502638900006,11.6,-5.50226672400001));
#275314=CARTESIAN_POINT('Ctrl Pts',(-8.83395166600006,15.2,-5.50176068100001));
#275315=CARTESIAN_POINT('Ctrl Pts',(-8.83395166600006,11.6,-5.50176068100001));
#275316=CARTESIAN_POINT('Ctrl Pts',(-8.83288545200006,15.2,-5.50125736900001));
#275317=CARTESIAN_POINT('Ctrl Pts',(-8.83288545200006,11.6,-5.50125736900001));
#275318=CARTESIAN_POINT('Ctrl Pts',(-8.83182776000006,15.2,-5.50075681300001));
#275319=CARTESIAN_POINT('Ctrl Pts',(-8.83182776000006,11.6,-5.50075681300001));
#275320=CARTESIAN_POINT('Ctrl Pts',(-8.83077860600006,15.2,-5.50025903800002));
#275321=CARTESIAN_POINT('Ctrl Pts',(-8.83077860600006,11.6,-5.50025903800002));
#275322=CARTESIAN_POINT('Ctrl Pts',(-8.82973800300006,15.2,-5.49976406800001));
#275323=CARTESIAN_POINT('Ctrl Pts',(-8.82973800300006,11.6,-5.49976406800001));
#275324=CARTESIAN_POINT('Ctrl Pts',(-8.82870596800006,15.2,-5.49927193100002));
#275325=CARTESIAN_POINT('Ctrl Pts',(-8.82870596800006,11.6,-5.49927193100002));
#275326=CARTESIAN_POINT('Ctrl Pts',(-8.82768251300006,15.2,-5.49878264900002));
#275327=CARTESIAN_POINT('Ctrl Pts',(-8.82768251300006,11.6,-5.49878264900002));
#275328=CARTESIAN_POINT('Ctrl Pts',(-8.82666765400005,15.2,-5.49829625000001));
#275329=CARTESIAN_POINT('Ctrl Pts',(-8.82666765400005,11.6,-5.49829625000001));
#275330=CARTESIAN_POINT('Ctrl Pts',(-8.82566140500006,15.2,-5.49781275800001));
#275331=CARTESIAN_POINT('Ctrl Pts',(-8.82566140500006,11.6,-5.49781275800001));
#275332=CARTESIAN_POINT('Ctrl Pts',(-8.82466378100006,15.2,-5.49733219900002));
#275333=CARTESIAN_POINT('Ctrl Pts',(-8.82466378100006,11.6,-5.49733219900002));
#275334=CARTESIAN_POINT('Ctrl Pts',(-8.82367479800006,15.2,-5.49685460000001));
#275335=CARTESIAN_POINT('Ctrl Pts',(-8.82367479800006,11.6,-5.49685460000001));
#275336=CARTESIAN_POINT('Ctrl Pts',(-8.82269446900006,15.2,-5.49637998700002));
#275337=CARTESIAN_POINT('Ctrl Pts',(-8.82269446900006,11.6,-5.49637998700002));
#275338=CARTESIAN_POINT('Ctrl Pts',(-8.82172281000006,15.2,-5.49590838500002));
#275339=CARTESIAN_POINT('Ctrl Pts',(-8.82172281000006,11.6,-5.49590838500002));
#275340=CARTESIAN_POINT('Ctrl Pts',(-8.82075983700006,15.2,-5.49543981900001));
#275341=CARTESIAN_POINT('Ctrl Pts',(-8.82075983700006,11.6,-5.49543981900001));
#275342=CARTESIAN_POINT('Ctrl Pts',(-8.81980556200006,15.2,-5.49497431900001));
#275343=CARTESIAN_POINT('Ctrl Pts',(-8.81980556200006,11.6,-5.49497431900001));
#275344=CARTESIAN_POINT('Ctrl Pts',(-8.81886000300005,15.2,-5.49451190900001));
#275345=CARTESIAN_POINT('Ctrl Pts',(-8.81886000300005,11.6,-5.49451190900001));
#275346=CARTESIAN_POINT('Ctrl Pts',(-8.81792317400006,15.2,-5.49405261600001));
#275347=CARTESIAN_POINT('Ctrl Pts',(-8.81792317400006,11.6,-5.49405261600001));
#275348=CARTESIAN_POINT('Ctrl Pts',(-8.81699508900006,15.2,-5.49359646700001));
#275349=CARTESIAN_POINT('Ctrl Pts',(-8.81699508900006,11.6,-5.49359646700001));
#275350=CARTESIAN_POINT('Ctrl Pts',(-8.81607576700006,15.2,-5.49314348900001));
#275351=CARTESIAN_POINT('Ctrl Pts',(-8.81607576700006,11.6,-5.49314348900001));
#275352=CARTESIAN_POINT('Ctrl Pts',(-8.81516521900006,15.2,-5.49269371000001));
#275353=CARTESIAN_POINT('Ctrl Pts',(-8.81516521900006,11.6,-5.49269371000001));
#275354=CARTESIAN_POINT('Ctrl Pts',(-8.81426346300006,15.2,-5.49224715500001));
#275355=CARTESIAN_POINT('Ctrl Pts',(-8.81426346300006,11.6,-5.49224715500001));
#275356=CARTESIAN_POINT('Ctrl Pts',(-8.81337051400006,15.2,-5.49180385500001));
#275357=CARTESIAN_POINT('Ctrl Pts',(-8.81337051400006,11.6,-5.49180385500001));
#275358=CARTESIAN_POINT('Ctrl Pts',(-8.81248638700006,15.2,-5.49136383300001));
#275359=CARTESIAN_POINT('Ctrl Pts',(-8.81248638700006,11.6,-5.49136383300001));
#275360=CARTESIAN_POINT('Ctrl Pts',(-8.81161109900006,15.2,-5.49092711900002));
#275361=CARTESIAN_POINT('Ctrl Pts',(-8.81161109900006,11.6,-5.49092711900002));
#275362=CARTESIAN_POINT('Ctrl Pts',(-8.81074466500005,15.2,-5.49049374100001));
#275363=CARTESIAN_POINT('Ctrl Pts',(-8.81074466500005,11.6,-5.49049374100001));
#275364=CARTESIAN_POINT('Ctrl Pts',(-8.80988709900006,15.2,-5.49006372600001));
#275365=CARTESIAN_POINT('Ctrl Pts',(-8.80988709900006,11.6,-5.49006372600001));
#275366=CARTESIAN_POINT('Ctrl Pts',(-8.80903841900006,15.2,-5.48963710300002));
#275367=CARTESIAN_POINT('Ctrl Pts',(-8.80903841900006,11.6,-5.48963710300002));
#275368=CARTESIAN_POINT('Ctrl Pts',(-8.80819864000006,15.2,-5.48921389900002));
#275369=CARTESIAN_POINT('Ctrl Pts',(-8.80819864000006,11.6,-5.48921389900002));
#275370=CARTESIAN_POINT('Ctrl Pts',(-8.80736777900006,15.2,-5.48879414400002));
#275371=CARTESIAN_POINT('Ctrl Pts',(-8.80736777900006,11.6,-5.48879414400002));
#275372=CARTESIAN_POINT('Ctrl Pts',(-8.80655058300006,15.2,-5.48838026300002));
#275373=CARTESIAN_POINT('Ctrl Pts',(-8.80655058300006,11.6,-5.48838026300002));
#275374=CARTESIAN_POINT('Ctrl Pts',(-8.80590483100006,15.2,-5.48805240200001));
#275375=CARTESIAN_POINT('Ctrl Pts',(-8.80590483100006,11.6,-5.48805240200001));
#275376=CARTESIAN_POINT('Ctrl Pts',(-8.80542564400006,15.2,-5.48780866000001));
#275377=CARTESIAN_POINT('Ctrl Pts',(-8.80542564400006,11.6,-5.48780866000001));
#275378=CARTESIAN_POINT('Ctrl Pts',(-8.80510947800006,15.2,-5.48764764400001));
#275379=CARTESIAN_POINT('Ctrl Pts',(-8.80510947800006,11.6,-5.48764764400001));
#275380=CARTESIAN_POINT('Ctrl Pts',(-8.80495412800006,15.2,-5.48756848000002));
#275381=CARTESIAN_POINT('Ctrl Pts',(-8.80495412800006,11.6,-5.48756848000002));
#275382=CARTESIAN_POINT('',(-8.80495412746579,12.2,-5.48756847941587));
#275383=CARTESIAN_POINT('',(-8.80495412746579,15.2,-5.48756847941587));
#275384=CARTESIAN_POINT('',(-8.80495412700006,12.2,-5.48756847900002));
#275385=CARTESIAN_POINT('Ctrl Pts',(-9.95917514600006,12.2,-5.75020264100001));
#275386=CARTESIAN_POINT('Ctrl Pts',(-9.95409037794778,12.2,-5.74984643423629));
#275387=CARTESIAN_POINT('Ctrl Pts',(-9.94901787496109,12.2,-5.74948339722987));
#275388=CARTESIAN_POINT('Ctrl Pts',(-9.94395764896434,12.2,-5.74911352693123));
#275389=CARTESIAN_POINT('Ctrl Pts',(-9.9401624798115,12.2,-5.74883612423245));
#275390=CARTESIAN_POINT('Ctrl Pts',(-9.93637421526921,12.2,-5.74855488063251));
#275391=CARTESIAN_POINT('Ctrl Pts',(-9.93259287576015,12.2,-5.74826981171152));
#275392=CARTESIAN_POINT('Ctrl Pts',(-9.92881153625109,12.2,-5.74798474279053));
#275393=CARTESIAN_POINT('Ctrl Pts',(-9.92503712276863,12.2,-5.7476958515911));
#275394=CARTESIAN_POINT('Ctrl Pts',(-9.92126966961447,12.2,-5.74740316876808));
#275395=CARTESIAN_POINT('Ctrl Pts',(-9.91750221646032,12.2,-5.74711048594505));
#275396=CARTESIAN_POINT('Ctrl Pts',(-9.91374172529696,12.2,-5.74681401298914));
#275397=CARTESIAN_POINT('Ctrl Pts',(-9.909988229975,12.2,-5.74651378250004));
#275398=CARTESIAN_POINT('Ctrl Pts',(-9.90623473465304,12.2,-5.74621355201095));
#275399=CARTESIAN_POINT('Ctrl Pts',(-9.90248823458913,12.2,-5.74590956273868));
#275400=CARTESIAN_POINT('Ctrl Pts',(-9.89874875768272,12.2,-5.74560183979185));
#275401=CARTESIAN_POINT('Ctrl Pts',(-9.89500928077632,12.2,-5.74529411684502));
#275402=CARTESIAN_POINT('Ctrl Pts',(-9.89127682625575,12.2,-5.74498266149818));
#275403=CARTESIAN_POINT('Ctrl Pts',(-9.88755142274585,12.2,-5.74466749807765));
#275404=CARTESIAN_POINT('Ctrl Pts',(-9.88382601923595,12.2,-5.74435233465712));
#275405=CARTESIAN_POINT('Ctrl Pts',(-9.88010766652519,12.2,-5.74403346444147));
#275406=CARTESIAN_POINT('Ctrl Pts',(-9.87639639528407,12.2,-5.74371091607869));
#275407=CARTESIAN_POINT('Ctrl Pts',(-9.87268512336873,12.2,-5.74338836765731));
#275408=CARTESIAN_POINT('Ctrl Pts',(-9.86898093399704,12.2,-5.7430621426099));
#275409=CARTESIAN_POINT('Ctrl Pts',(-9.86528385746071,12.2,-5.74273226768646));
#275410=CARTESIAN_POINT('Ctrl Pts',(-9.86158678159601,12.2,-5.74240239282295));
#275411=CARTESIAN_POINT('Ctrl Pts',(-9.85789681776428,12.2,-5.74206886966797));
#275412=CARTESIAN_POINT('Ctrl Pts',(-9.85421399685703,12.2,-5.7417317256799));
#275413=CARTESIAN_POINT('Ctrl Pts',(-9.85053117594978,12.2,-5.74139458169183));
#275414=CARTESIAN_POINT('Ctrl Pts',(-9.84685549666336,12.2,-5.74105381605546));
#275415=CARTESIAN_POINT('Ctrl Pts',(-9.84318698982168,12.2,-5.74070945948306));
#275416=CARTESIAN_POINT('Ctrl Pts',(-9.83829564758826,12.2,-5.74025031740737));
#275417=CARTESIAN_POINT('Ctrl Pts',(-9.83341705508244,12.2,-5.73978478939629));
#275418=CARTESIAN_POINT('Ctrl Pts',(-9.82855128681223,12.2,-5.73931294360218));
#275419=CARTESIAN_POINT('Ctrl Pts',(-9.82490195978086,12.2,-5.73895905917623));
#275420=CARTESIAN_POINT('Ctrl Pts',(-9.82125984466824,12.2,-5.73860162195762));
#275421=CARTESIAN_POINT('Ctrl Pts',(-9.81762497368261,12.2,-5.73824066144635));
#275422=CARTESIAN_POINT('Ctrl Pts',(-9.81399010335732,12.2,-5.73787970100065));
#275423=CARTESIAN_POINT('Ctrl Pts',(-9.81036247660667,12.2,-5.73751521608014));
#275424=CARTESIAN_POINT('Ctrl Pts',(-9.80674212286384,12.2,-5.73714723713487));
#275425=CARTESIAN_POINT('Ctrl Pts',(-9.80312176912101,12.2,-5.73677925818961));
#275426=CARTESIAN_POINT('Ctrl Pts',(-9.79950868946539,12.2,-5.73640778523779));
#275427=CARTESIAN_POINT('Ctrl Pts',(-9.79590291370507,12.2,-5.73603284729136));
#275428=CARTESIAN_POINT('Ctrl Pts',(-9.79229713794475,12.2,-5.73565790934494));
#275429=CARTESIAN_POINT('Ctrl Pts',(-9.7886986668058,12.2,-5.7352795069549));
#275430=CARTESIAN_POINT('Ctrl Pts',(-9.78510753050327,12.2,-5.73489767050872));
#275431=CARTESIAN_POINT('Ctrl Pts',(-9.78151639420074,12.2,-5.73451583406254));
#275432=CARTESIAN_POINT('Ctrl Pts',(-9.77793259291067,12.2,-5.7341305624446));
#275433=CARTESIAN_POINT('Ctrl Pts',(-9.77435615712329,12.2,-5.73374188700068));
#275434=CARTESIAN_POINT('Ctrl Pts',(-9.76958757564029,12.2,-5.73322365302838));
#275435=CARTESIAN_POINT('Ctrl Pts',(-9.76483208952837,12.2,-5.73269936735814));
#275436=CARTESIAN_POINT('Ctrl Pts',(-9.76008977010411,12.2,-5.73216910143996));
#275437=CARTESIAN_POINT('Ctrl Pts',(-9.75653303085899,12.2,-5.73177140203746));
#275438=CARTESIAN_POINT('Ctrl Pts',(-9.75298369860466,12.2,-5.73137033946868));
#275439=CARTESIAN_POINT('Ctrl Pts',(-9.74944180473333,12.2,-5.73096594406671));
#275440=CARTESIAN_POINT('Ctrl Pts',(-9.745899910862,12.2,-5.73056154866473));
#275441=CARTESIAN_POINT('Ctrl Pts',(-9.74236545397374,12.2,-5.73015382064624));
#275442=CARTESIAN_POINT('Ctrl Pts',(-9.73883846614291,12.2,-5.72974279078645));
#275443=CARTESIAN_POINT('Ctrl Pts',(-9.73531147831207,12.2,-5.72933176092667));
#275444=CARTESIAN_POINT('Ctrl Pts',(-9.73179195946162,12.2,-5.72891742980278));
#275445=CARTESIAN_POINT('Ctrl Pts',(-9.72827994045456,12.2,-5.72849982783914));
#275446=CARTESIAN_POINT('Ctrl Pts',(-9.72476792144751,12.2,-5.72808222587549));
#275447=CARTESIAN_POINT('Ctrl Pts',(-9.72126340215299,12.2,-5.72766135264331));
#275448=CARTESIAN_POINT('Ctrl Pts',(-9.71776641477902,12.2,-5.72723724211749));
#275449=CARTESIAN_POINT('Ctrl Pts',(-9.71426942676977,12.2,-5.72681313151463));
#275450=CARTESIAN_POINT('Ctrl Pts',(-9.71077996901264,12.2,-5.72638578120253));
#275451=CARTESIAN_POINT('Ctrl Pts',(-9.70729807450762,12.2,-5.72595522418117));
#275452=CARTESIAN_POINT('Ctrl Pts',(-9.70381618063515,12.2,-5.72552466723804));
#275453=CARTESIAN_POINT('Ctrl Pts',(-9.70034184847897,12.2,-5.72509090265343));
#275454=CARTESIAN_POINT('Ctrl Pts',(-9.69687511114725,12.2,-5.72465396371069));
#275455=CARTESIAN_POINT('Ctrl Pts',(-9.69340837381553,12.2,-5.72421702476795));
#275456=CARTESIAN_POINT('Ctrl Pts',(-9.68994923005378,12.2,-5.72377691043556));
#275457=CARTESIAN_POINT('Ctrl Pts',(-9.68649771220521,12.2,-5.72333365403297));
#275458=CARTESIAN_POINT('Ctrl Pts',(-9.68304619435663,12.2,-5.72289039763038));
#275459=CARTESIAN_POINT('Ctrl Pts',(-9.67960230117726,12.2,-5.72244399855281));
#275460=CARTESIAN_POINT('Ctrl Pts',(-9.67616606624479,12.2,-5.72199448873378));
#275461=CARTESIAN_POINT('Ctrl Pts',(-9.67272983131232,12.2,-5.72154497891475));
#275462=CARTESIAN_POINT('Ctrl Pts',(-9.66930125221604,12.2,-5.7210923596995));
#275463=CARTESIAN_POINT('Ctrl Pts',(-9.66588036288134,12.2,-5.72063666284132));
#275464=CARTESIAN_POINT('Ctrl Pts',(-9.66245947354664,12.2,-5.72018096598314));
#275465=CARTESIAN_POINT('Ctrl Pts',(-9.65904627296974,12.2,-5.71972219145018));
#275466=CARTESIAN_POINT('Ctrl Pts',(-9.6556407927174,12.2,-5.71926037305071));
#275467=CARTESIAN_POINT('Ctrl Pts',(-9.65223531184641,12.2,-5.71879855456734));
#275468=CARTESIAN_POINT('Ctrl Pts',(-9.64883755221928,12.2,-5.71833369164978));
#275469=CARTESIAN_POINT('Ctrl Pts',(-9.64544754526932,12.2,-5.71786581770637));
#275470=CARTESIAN_POINT('Ctrl Pts',(-9.64205753893523,12.2,-5.71739794384796));
#275471=CARTESIAN_POINT('Ctrl Pts',(-9.63867528399229,12.2,-5.71692705929846));
#275472=CARTESIAN_POINT('Ctrl Pts',(-9.63530081407221,12.2,-5.71645319787499));
#275473=CARTESIAN_POINT('Ctrl Pts',(-9.63192634415214,12.2,-5.71597933645153));
#275474=CARTESIAN_POINT('Ctrl Pts',(-9.62855965989462,12.2,-5.71550249684718));
#275475=CARTESIAN_POINT('Ctrl Pts',(-9.62520079160068,12.2,-5.71502271444769));
#275476=CARTESIAN_POINT('Ctrl Pts',(-9.62184192330675,12.2,-5.7145429320482));
#275477=CARTESIAN_POINT('Ctrl Pts',(-9.61849087136186,12.2,-5.71406020668239));
#275478=CARTESIAN_POINT('Ctrl Pts',(-9.615147669025,12.2,-5.71357457178337));
#275479=CARTESIAN_POINT('Ctrl Pts',(-9.61180446668813,12.2,-5.71308893688435));
#275480=CARTESIAN_POINT('Ctrl Pts',(-9.60846911280929,12.2,-5.71260039226878));
#275481=CARTESIAN_POINT('Ctrl Pts',(-9.60514164009616,12.2,-5.71210897337022));
#275482=CARTESIAN_POINT('Ctrl Pts',(-9.60181416738304,12.2,-5.71161755447166));
#275483=CARTESIAN_POINT('Ctrl Pts',(-9.59849457728684,12.2,-5.71112326023597));
#275484=CARTESIAN_POINT('Ctrl Pts',(-9.59518289940747,12.2,-5.71062612639619));
#275485=CARTESIAN_POINT('Ctrl Pts',(-9.5918712215281,12.2,-5.71012899255641));
#275486=CARTESIAN_POINT('Ctrl Pts',(-9.5885674572665,12.2,-5.70962901887432));
#275487=CARTESIAN_POINT('Ctrl Pts',(-9.58527164042683,12.2,-5.70912623960131));
#275488=CARTESIAN_POINT('Ctrl Pts',(-9.58087721757477,12.2,-5.70845586717639));
#275489=CARTESIAN_POINT('Ctrl Pts',(-9.57649691992405,12.2,-5.70778050829822));
#275490=CARTESIAN_POINT('Ctrl Pts',(-9.57213082774167,12.2,-5.70710024648337));
#275491=CARTESIAN_POINT('Ctrl Pts',(-9.56776473555929,12.2,-5.70641998466852));
#275492=CARTESIAN_POINT('Ctrl Pts',(-9.56341284680075,12.2,-5.70573481985865));
#275493=CARTESIAN_POINT('Ctrl Pts',(-9.55907524006581,12.2,-5.70504483615388));
#275494=CARTESIAN_POINT('Ctrl Pts',(-9.55256883055439,12.2,-5.70400986069076));
#275495=CARTESIAN_POINT('Ctrl Pts',(-9.54609455572192,12.2,-5.70296404560449));
#275496=CARTESIAN_POINT('Ctrl Pts',(-9.53965267920738,12.2,-5.70190767697575));
#275497=CARTESIAN_POINT('Ctrl Pts',(-9.5353580950594,12.2,-5.70120343125523));
#275498=CARTESIAN_POINT('Ctrl Pts',(-9.53107790966964,12.2,-5.70049449661066));
#275499=CARTESIAN_POINT('Ctrl Pts',(-9.52681220340578,12.2,-5.69978095839169));
#275500=CARTESIAN_POINT('Ctrl Pts',(-9.52254649656072,12.2,-5.6990674200755));
#275501=CARTESIAN_POINT('Ctrl Pts',(-9.51829526704999,12.2,-5.69834928007278));
#275502=CARTESIAN_POINT('Ctrl Pts',(-9.51405859552212,12.2,-5.69762662497454));
#275503=CARTESIAN_POINT('Ctrl Pts',(-9.5098219245715,12.2,-5.69690396997476));
#275504=CARTESIAN_POINT('Ctrl Pts',(-9.50559980981213,12.2,-5.69617680117049));
#275505=CARTESIAN_POINT('Ctrl Pts',(-9.50139233115459,12.2,-5.69544520611965));
#275506=CARTESIAN_POINT('Ctrl Pts',(-9.4971848519238,12.2,-5.69471361096912));
#275507=CARTESIAN_POINT('Ctrl Pts',(-9.49299201074995,12.2,-5.69397758987372));
#275508=CARTESIAN_POINT('Ctrl Pts',(-9.48881388596666,12.2,-5.69323723350003));
#275509=CARTESIAN_POINT('Ctrl Pts',(-9.48463576118336,12.2,-5.69249687712634));
#275510=CARTESIAN_POINT('Ctrl Pts',(-9.48047235300741,12.2,-5.69175218570216));
#275511=CARTESIAN_POINT('Ctrl Pts',(-9.47632374033838,12.2,-5.69100324866091));
#275512=CARTESIAN_POINT('Ctrl Pts',(-9.47217512823461,12.2,-5.6902543117217));
#275513=CARTESIAN_POINT('Ctrl Pts',(-9.46804131249317,12.2,-5.68950113035317));
#275514=CARTESIAN_POINT('Ctrl Pts',(-9.46392237497781,12.2,-5.68874379730055));
#275515=CARTESIAN_POINT('Ctrl Pts',(-9.45980343690124,12.2,-5.68798646414473));
#275516=CARTESIAN_POINT('Ctrl Pts',(-9.45569937597219,12.2,-5.68722497653366));
#275517=CARTESIAN_POINT('Ctrl Pts',(-9.45161027380643,12.2,-5.6864594301582));
#275518=CARTESIAN_POINT('Ctrl Pts',(-9.44752117219781,12.2,-5.68569388388704));
#275519=CARTESIAN_POINT('Ctrl Pts',(-9.44344702710667,12.2,-5.68492427853029));
#275520=CARTESIAN_POINT('Ctrl Pts',(-9.43938792354864,12.2,-5.68415070753823));
#275521=CARTESIAN_POINT('Ctrl Pts',(-9.43329926793507,12.2,-5.68299035099745));
#275522=CARTESIAN_POINT('Ctrl Pts',(-9.42724444977319,12.2,-5.68182107141003));
#275523=CARTESIAN_POINT('Ctrl Pts',(-9.42122374915626,12.2,-5.68064319187008));
#275524=CARTESIAN_POINT('Ctrl Pts',(-9.41720994838038,12.2,-5.67985793877212));
#275525=CARTESIAN_POINT('Ctrl Pts',(-9.41321130928653,12.2,-5.67906886372935));
#275526=CARTESIAN_POINT('Ctrl Pts',(-9.40922791645832,12.2,-5.6782760627417));
#275527=CARTESIAN_POINT('Ctrl Pts',(-9.40524452363011,12.2,-5.67748326175405));
#275528=CARTESIAN_POINT('Ctrl Pts',(-9.4012763745148,12.2,-5.67668673501318));
#275529=CARTESIAN_POINT('Ctrl Pts',(-9.39732355457872,12.2,-5.67588658130254));
#275530=CARTESIAN_POINT('Ctrl Pts',(-9.39337073518123,12.2,-5.67508642770091));
#275531=CARTESIAN_POINT('Ctrl Pts',(-9.38943324447615,12.2,-5.67428264574698));
#275532=CARTESIAN_POINT('Ctrl Pts',(-9.38551116429577,12.2,-5.67347533675766));
#275533=CARTESIAN_POINT('Ctrl Pts',(-9.38158908358101,12.2,-5.67266802765834));
#275534=CARTESIAN_POINT('Ctrl Pts',(-9.37768241456836,12.2,-5.67185718898666));
#275535=CARTESIAN_POINT('Ctrl Pts',(-9.37379124038544,12.2,-5.67104292262352));
#275536=CARTESIAN_POINT('Ctrl Pts',(-9.36892727292189,12.2,-5.67002508972507));
#275537=CARTESIAN_POINT('Ctrl Pts',(-9.36408751697371,12.2,-5.66900190092705));
#275538=CARTESIAN_POINT('Ctrl Pts',(-9.35927213787848,12.2,-5.66797355314885));
#275539=CARTESIAN_POINT('Ctrl Pts',(-9.35541983491722,12.2,-5.66715087499355));
#275540=CARTESIAN_POINT('Ctrl Pts',(-9.35158313178172,12.2,-5.66632489584701));
#275541=CARTESIAN_POINT('Ctrl Pts',(-9.34776211437084,12.2,-5.66549571885945));
#275542=CARTESIAN_POINT('Ctrl Pts',(-9.34394109643936,12.2,-5.66466654175891));
#275543=CARTESIAN_POINT('Ctrl Pts',(-9.34013576407524,12.2,-5.66383416589132));
#275544=CARTESIAN_POINT('Ctrl Pts',(-9.33634620195853,12.2,-5.66299869563711));
#275545=CARTESIAN_POINT('Ctrl Pts',(-9.33255664035815,12.2,-5.66216322549674));
#275546=CARTESIAN_POINT('Ctrl Pts',(-9.32878285161785,12.2,-5.66132466031647));
#275547=CARTESIAN_POINT('Ctrl Pts',(-9.32502491759068,12.2,-5.66048310805213));
#275548=CARTESIAN_POINT('Ctrl Pts',(-9.3212669830515,12.2,-5.65964155567312));
#275549=CARTESIAN_POINT('Ctrl Pts',(-9.31752490530313,12.2,-5.65879701334654));
#275550=CARTESIAN_POINT('Ctrl Pts',(-9.3137987712122,12.2,-5.65794958968906));
#275551=CARTESIAN_POINT('Ctrl Pts',(-9.31007263762896,12.2,-5.65710216614704));
#275552=CARTESIAN_POINT('Ctrl Pts',(-9.30636244611732,12.2,-5.65625185991588));
#275553=CARTESIAN_POINT('Ctrl Pts',(-9.30266828451113,12.2,-5.65539878033213));
#275554=CARTESIAN_POINT('Ctrl Pts',(-9.29897412240161,12.2,-5.65454570063215));
#275555=CARTESIAN_POINT('Ctrl Pts',(-9.2952959901743,12.2,-5.65368984571845));
#275556=CARTESIAN_POINT('Ctrl Pts',(-9.29163397547577,12.2,-5.65283132617148));
#275557=CARTESIAN_POINT('Ctrl Pts',(-9.2879719612762,12.2,-5.65197280674148));
#275558=CARTESIAN_POINT('Ctrl Pts',(-9.28432606282339,12.2,-5.65111162334815));
#275559=CARTESIAN_POINT('Ctrl Pts',(-9.28069637061846,12.2,-5.65024788464124));
#275560=CARTESIAN_POINT('Ctrl Pts',(-9.27706667791898,12.2,-5.64938414581665));
#275561=CARTESIAN_POINT('Ctrl Pts',(-9.273453189371,12.2,-5.64851785205074));
#275562=CARTESIAN_POINT('Ctrl Pts',(-9.26985599471421,12.2,-5.64764911699943));
#275563=CARTESIAN_POINT('Ctrl Pts',(-9.26625880054753,12.2,-5.64678038206649));
#275564=CARTESIAN_POINT('Ctrl Pts',(-9.26267789834029,12.2,-5.64590920418508));
#275565=CARTESIAN_POINT('Ctrl Pts',(-9.25911337957447,12.2,-5.64503569686784));
#275566=CARTESIAN_POINT('Ctrl Pts',(-9.25554886032297,12.2,-5.64416218943158));
#275567=CARTESIAN_POINT('Ctrl Pts',(-9.25200072389246,12.2,-5.64328635198677));
#275568=CARTESIAN_POINT('Ctrl Pts',(-9.24846905803332,12.2,-5.64240830105002));
#275569=CARTESIAN_POINT('Ctrl Pts',(-9.24493739217417,12.2,-5.64153025011328));
#275570=CARTESIAN_POINT('Ctrl Pts',(-9.24142219814474,12.2,-5.64064998448184));
#275571=CARTESIAN_POINT('Ctrl Pts',(-9.23792356617797,12.2,-5.63976762032242));
#275572=CARTESIAN_POINT('Ctrl Pts',(-9.23442493468789,12.2,-5.63888525628323));
#275573=CARTESIAN_POINT('Ctrl Pts',(-9.23094286375706,12.2,-5.6380007941294));
#275574=CARTESIAN_POINT('Ctrl Pts',(-9.22747744680235,12.2,-5.63711435080896));
#275575=CARTESIAN_POINT('Ctrl Pts',(-9.22401202937549,12.2,-5.63622790736773));
#275576=CARTESIAN_POINT('Ctrl Pts',(-9.22056326270751,12.2,-5.63533948328094));
#275577=CARTESIAN_POINT('Ctrl Pts',(-9.21713124018886,12.2,-5.63444919712112));
#275578=CARTESIAN_POINT('Ctrl Pts',(-9.21369921813782,12.2,-5.63355891108261));
#275579=CARTESIAN_POINT('Ctrl Pts',(-9.2102839409179,12.2,-5.63266676329989));
#275580=CARTESIAN_POINT('Ctrl Pts',(-9.20688549752797,12.2,-5.63177287403975));
#275581=CARTESIAN_POINT('Ctrl Pts',(-9.20348705367501,12.2,-5.63087898465782));
#275582=CARTESIAN_POINT('Ctrl Pts',(-9.20010544519518,12.2,-5.62998335421368));
#275583=CARTESIAN_POINT('Ctrl Pts',(-9.19674076451184,12.2,-5.62908610411981));
#275584=CARTESIAN_POINT('Ctrl Pts',(-9.19337608428694,12.2,-5.6281888541482));
#275585=CARTESIAN_POINT('Ctrl Pts',(-9.19002833246516,12.2,-5.62728998641658));
#275586=CARTESIAN_POINT('Ctrl Pts',(-9.1866976010141,12.2,-5.62638962182361));
#275587=CARTESIAN_POINT('Ctrl Pts',(-9.18336686910923,12.2,-5.62548925710797));
#275588=CARTESIAN_POINT('Ctrl Pts',(-9.18005315646755,12.2,-5.62458739670882));
#275589=CARTESIAN_POINT('Ctrl Pts',(-9.17675656045565,12.2,-5.6236841666595));
#275590=CARTESIAN_POINT('Ctrl Pts',(-9.17345996489292,12.2,-5.62278093673325));
#275591=CARTESIAN_POINT('Ctrl Pts',(-9.17018048252125,12.2,-5.62187633587755));
#275592=CARTESIAN_POINT('Ctrl Pts',(-9.16691820895679,12.2,-5.62097049240645));
#275593=CARTESIAN_POINT('Ctrl Pts',(-9.16365593494787,12.2,-5.62006464881194));
#275594=CARTESIAN_POINT('Ctrl Pts',(-9.16041086977495,12.2,-5.61915756073922));
#275595=CARTESIAN_POINT('Ctrl Pts',(-9.15718310854462,12.2,-5.6182493586341));
#275596=CARTESIAN_POINT('Ctrl Pts',(-9.15395534775407,12.2,-5.61734115665272));
#275597=CARTESIAN_POINT('Ctrl Pts',(-9.15074489128502,12.2,-5.61643183876044));
#275598=CARTESIAN_POINT('Ctrl Pts',(-9.14755183332206,12.2,-5.61552153689052));
#275599=CARTESIAN_POINT('Ctrl Pts',(-9.14356051054207,12.2,-5.61438365946009));
#275600=CARTESIAN_POINT('Ctrl Pts',(-9.13959637408344,12.2,-5.61324424281155));
#275601=CARTESIAN_POINT('Ctrl Pts',(-9.13565961339875,12.2,-5.61210354615743));
#275602=CARTESIAN_POINT('Ctrl Pts',(-9.13172285271406,12.2,-5.6109628495033));
#275603=CARTESIAN_POINT('Ctrl Pts',(-9.12781346627214,12.2,-5.6098208716136));
#275604=CARTESIAN_POINT('Ctrl Pts',(-9.12393164502069,12.2,-5.60867787584976));
#275605=CARTESIAN_POINT('Ctrl Pts',(-9.12004982376924,12.2,-5.60753488008593));
#275606=CARTESIAN_POINT('Ctrl Pts',(-9.11619556795187,12.2,-5.60639086647484));
#275607=CARTESIAN_POINT('Ctrl Pts',(-9.11236906774208,12.2,-5.60524610084988));
#275608=CARTESIAN_POINT('Ctrl Pts',(-9.1085425675323,12.2,-5.60410133522491));
#275609=CARTESIAN_POINT('Ctrl Pts',(-9.10474382473154,12.2,-5.60295581854716));
#275610=CARTESIAN_POINT('Ctrl Pts',(-9.10097303348009,12.2,-5.60180982132496));
#275611=CARTESIAN_POINT('Ctrl Pts',(-9.09720224222865,12.2,-5.60066382410277));
#275612=CARTESIAN_POINT('Ctrl Pts',(-9.09345939989119,12.2,-5.59951734792806));
#275613=CARTESIAN_POINT('Ctrl Pts',(-9.08974470452701,12.2,-5.59837066653397));
#275614=CARTESIAN_POINT('Ctrl Pts',(-9.08603000916283,12.2,-5.59722398513988));
#275615=CARTESIAN_POINT('Ctrl Pts',(-9.08234346030553,12.2,-5.59607709923335));
#275616=CARTESIAN_POINT('Ctrl Pts',(-9.07868525495831,12.2,-5.59493029173335));
#275617=CARTESIAN_POINT('Ctrl Pts',(-9.07502704961108,12.2,-5.59378348423334));
#275618=CARTESIAN_POINT('Ctrl Pts',(-9.07139718858651,12.2,-5.59263675178237));
#275619=CARTESIAN_POINT('Ctrl Pts',(-9.06779587072302,12.2,-5.59149038274939));
#275620=CARTESIAN_POINT('Ctrl Pts',(-9.06419455285953,12.2,-5.59034401371641));
#275621=CARTESIAN_POINT('Ctrl Pts',(-9.06062177702242,12.2,-5.58919800558618));
#275622=CARTESIAN_POINT('Ctrl Pts',(-9.05707774751005,12.2,-5.58805265239178));
#275623=CARTESIAN_POINT('Ctrl Pts',(-9.05353371799768,12.2,-5.58690729919738));
#275624=CARTESIAN_POINT('Ctrl Pts',(-9.05001843272618,12.2,-5.58576259785294));
#275625=CARTESIAN_POINT('Ctrl Pts',(-9.04653209654715,12.2,-5.58461884570022));
#275626=CARTESIAN_POINT('Ctrl Pts',(-9.04304576036813,12.2,-5.5834750935475));
#275627=CARTESIAN_POINT('Ctrl Pts',(-9.03958837427692,12.2,-5.58233229076888));
#275628=CARTESIAN_POINT('Ctrl Pts',(-9.03616014063545,12.2,-5.58119073710083));
#275629=CARTESIAN_POINT('Ctrl Pts',(-9.03273190699398,12.2,-5.58004918343277));
#275630=CARTESIAN_POINT('Ctrl Pts',(-9.02933282980129,12.2,-5.57890888160094));
#275631=CARTESIAN_POINT('Ctrl Pts',(-9.0259631145259,12.2,-5.57777013535106));
#275632=CARTESIAN_POINT('Ctrl Pts',(-9.02259339925052,12.2,-5.57663138910119));
#275633=CARTESIAN_POINT('Ctrl Pts',(-9.01925304713674,12.2,-5.57549420050135));
#275634=CARTESIAN_POINT('Ctrl Pts',(-9.0159422678336,12.2,-5.57435888008484));
#275635=CARTESIAN_POINT('Ctrl Pts',(-9.01263148889134,12.2,-5.57322355979209));
#275636=CARTESIAN_POINT('Ctrl Pts',(-9.00935028375105,12.2,-5.57209010840261));
#275637=CARTESIAN_POINT('Ctrl Pts',(-9.0060988646586,12.2,-5.57095884262298));
#275638=CARTESIAN_POINT('Ctrl Pts',(-9.00284744521174,12.2,-5.56982757672003));
#275639=CARTESIAN_POINT('Ctrl Pts',(-8.99962581084212,12.2,-5.5686984999809));
#275640=CARTESIAN_POINT('Ctrl Pts',(-8.99643417965913,12.2,-5.56757193289736));
#275641=CARTESIAN_POINT('Ctrl Pts',(-8.99324254847613,12.2,-5.56644536581384));
#275642=CARTESIAN_POINT('Ctrl Pts',(-8.99008091774436,12.2,-5.56532130925861));
#275643=CARTESIAN_POINT('Ctrl Pts',(-8.9869495066136,12.2,-5.56420009385517));
#275644=CARTESIAN_POINT('Ctrl Pts',(-8.98319181305189,12.2,-5.56285463529771));
#275645=CARTESIAN_POINT('Ctrl Pts',(-8.97947763719697,12.2,-5.56151326617684));
#275646=CARTESIAN_POINT('Ctrl Pts',(-8.97580735783326,12.2,-5.56017657160431));
#275647=CARTESIAN_POINT('Ctrl Pts',(-8.97213707880293,12.2,-5.55883987715319));
#275648=CARTESIAN_POINT('Ctrl Pts',(-8.9685106971594,12.2,-5.55750785349889));
#275649=CARTESIAN_POINT('Ctrl Pts',(-8.96492860102335,12.2,-5.55618109929107));
#275650=CARTESIAN_POINT('Ctrl Pts',(-8.96134650488731,12.2,-5.55485434508325));
#275651=CARTESIAN_POINT('Ctrl Pts',(-8.95780869174889,12.2,-5.55353285835752));
#275652=CARTESIAN_POINT('Ctrl Pts',(-8.95431555770721,12.2,-5.55221725107173));
#275653=CARTESIAN_POINT('Ctrl Pts',(-8.95082242334824,12.2,-5.55090164366644));
#275654=CARTESIAN_POINT('Ctrl Pts',(-8.94737396721143,12.2,-5.54959191300355));
#275655=CARTESIAN_POINT('Ctrl Pts',(-8.94397058786236,12.2,-5.54828868584962));
#275656=CARTESIAN_POINT('Ctrl Pts',(-8.94056720882241,12.2,-5.54698545881408));
#275657=CARTESIAN_POINT('Ctrl Pts',(-8.93720890657228,12.2,-5.54568873347425));
#275658=CARTESIAN_POINT('Ctrl Pts',(-8.93389608761129,12.2,-5.54439915043808));
#275659=CARTESIAN_POINT('Ctrl Pts',(-8.9305832686503,12.2,-5.54310956740191));
#275660=CARTESIAN_POINT('Ctrl Pts',(-8.92731593080235,12.2,-5.54182712500687));
#275661=CARTESIAN_POINT('Ctrl Pts',(-8.92409449066741,12.2,-5.54055248005283));
#275662=CARTESIAN_POINT('Ctrl Pts',(-8.92087305053247,12.2,-5.53927783509881));
#275663=CARTESIAN_POINT('Ctrl Pts',(-8.9176975042139,12.2,-5.5380109859087));
#275664=CARTESIAN_POINT('Ctrl Pts',(-8.91456827232441,12.2,-5.5367526051205));
#275665=CARTESIAN_POINT('Ctrl Pts',(-8.91143904015069,12.2,-5.53549422421799));
#275666=CARTESIAN_POINT('Ctrl Pts',(-8.90835612418982,12.2,-5.53424431125798));
#275667=CARTESIAN_POINT('Ctrl Pts',(-8.90531994710969,12.2,-5.53300355444075));
#275668=CARTESIAN_POINT('Ctrl Pts',(-8.90228377030535,12.2,-5.53176279773622));
#275669=CARTESIAN_POINT('Ctrl Pts',(-8.89929433564735,12.2,-5.53053119599766));
#275670=CARTESIAN_POINT('Ctrl Pts',(-8.89635207566886,12.2,-5.52930945629162));
#275671=CARTESIAN_POINT('Ctrl Pts',(-8.89340981569037,12.2,-5.52808771658559));
#275672=CARTESIAN_POINT('Ctrl Pts',(-8.89051473087686,12.2,-5.52687583798803));
#275673=CARTESIAN_POINT('Ctrl Pts',(-8.88766726131037,12.2,-5.52567454636428));
#275674=CARTESIAN_POINT('Ctrl Pts',(-8.88481979148523,12.2,-5.5244732546314));
#275675=CARTESIAN_POINT('Ctrl Pts',(-8.88201994158144,12.2,-5.52328254665789));
#275676=CARTESIAN_POINT('Ctrl Pts',(-8.87926815660021,12.2,-5.52210316717744));
#275677=CARTESIAN_POINT('Ctrl Pts',(-8.87651637186895,12.2,-5.52092378780412));
#275678=CARTESIAN_POINT('Ctrl Pts',(-8.87381265496687,12.2,-5.51975573906379));
#275679=CARTESIAN_POINT('Ctrl Pts',(-8.87115746421785,12.2,-5.51859977976719));
#275680=CARTESIAN_POINT('Ctrl Pts',(-8.86850227346883,12.2,-5.51744382047058));
#275681=CARTESIAN_POINT('Ctrl Pts',(-8.86589560838085,12.2,-5.51629995355806));
#275682=CARTESIAN_POINT('Ctrl Pts',(-8.86333793755377,12.2,-5.51516896118161));
#275683=CARTESIAN_POINT('Ctrl Pts',(-8.86078026649437,12.2,-5.51403796870243));
#275684=CARTESIAN_POINT('Ctrl Pts',(-8.8582715898829,12.2,-5.51291984943276));
#275685=CARTESIAN_POINT('Ctrl Pts',(-8.85581238379553,12.2,-5.51181541290152));
#275686=CARTESIAN_POINT('Ctrl Pts',(-8.85335317793155,12.2,-5.51071097647061));
#275687=CARTESIAN_POINT('Ctrl Pts',(-8.85094344409755,12.2,-5.50962021750255));
#275688=CARTESIAN_POINT('Ctrl Pts',(-8.84858366851663,12.2,-5.50854396829165));
#275689=CARTESIAN_POINT('Ctrl Pts',(-8.8462238929357,12.2,-5.50746771908076));
#275690=CARTESIAN_POINT('Ctrl Pts',(-8.84391407709403,12.2,-5.50640597620805));
#275691=CARTESIAN_POINT('Ctrl Pts',(-8.84165471647699,12.2,-5.50535959410958));
#275692=CARTESIAN_POINT('Ctrl Pts',(-8.83939535565472,12.2,-5.50431321191606));
#275693=CARTESIAN_POINT('Ctrl Pts',(-8.83718645120391,12.2,-5.50328218836858));
#275694=CARTESIAN_POINT('Ctrl Pts',(-8.83502851250643,12.2,-5.50226740039771));
#275695=CARTESIAN_POINT('Ctrl Pts',(-8.83287057400498,12.2,-5.50125261251901));
#275696=CARTESIAN_POINT('Ctrl Pts',(-8.83076360063357,12.2,-5.50025405960163));
#275697=CARTESIAN_POINT('Ctrl Pts',(-8.82870811303237,12.2,-5.49927264479954));
#275698=CARTESIAN_POINT('Ctrl Pts',(-8.82665262543117,12.2,-5.49829122999746));
#275699=CARTESIAN_POINT('Ctrl Pts',(-8.82464862187126,12.2,-5.49732695060138));
#275700=CARTESIAN_POINT('Ctrl Pts',(-8.82269663660656,12.2,-5.49638073980162));
#275701=CARTESIAN_POINT('Ctrl Pts',(-8.82074465116457,12.2,-5.49543452891593));
#275702=CARTESIAN_POINT('Ctrl Pts',(-8.81884468407904,12.2,-5.49450638212414));
#275703=CARTESIAN_POINT('Ctrl Pts',(-8.81699727948194,12.2,-5.49359725965922));
#275704=CARTESIAN_POINT('Ctrl Pts',(-8.81514987505265,12.2,-5.49268813727688));
#275705=CARTESIAN_POINT('Ctrl Pts',(-8.81335503191469,12.2,-5.4917980403285));
#275706=CARTESIAN_POINT('Ctrl Pts',(-8.81161331239693,12.2,-5.49092795294431));
#275707=CARTESIAN_POINT('Ctrl Pts',(-8.80929937863631,12.2,-5.48977201219011));
#275708=CARTESIAN_POINT('Ctrl Pts',(-8.80707920106142,12.2,-5.48865138494897));
#275709=CARTESIAN_POINT('Ctrl Pts',(-8.80495412800006,12.2,-5.48756848000002));
#275710=CARTESIAN_POINT('Ctrl Pts',(-8.80495412800006,15.2,-5.48756848000002));
#275711=CARTESIAN_POINT('Ctrl Pts',(-8.80654601357685,15.2,-5.48837968070677));
#275712=CARTESIAN_POINT('Ctrl Pts',(-8.80819126582659,15.2,-5.48921205180374));
#275713=CARTESIAN_POINT('Ctrl Pts',(-8.809889320289,15.2,-5.49006457388994));
#275714=CARTESIAN_POINT('Ctrl Pts',(-8.81159556362836,15.2,-5.49092120726858));
#275715=CARTESIAN_POINT('Ctrl Pts',(-8.81335511570803,15.2,-5.49179818670865));
#275716=CARTESIAN_POINT('Ctrl Pts',(-8.81516741715041,15.2,-5.49269451613673));
#275717=CARTESIAN_POINT('Ctrl Pts',(-8.81697971842817,15.2,-5.49359084548341));
#275718=CARTESIAN_POINT('Ctrl Pts',(-8.81884476611964,15.2,-5.49450652398393));
#275719=CARTESIAN_POINT('Ctrl Pts',(-8.82076201154996,15.2,-5.49544058544998));
#275720=CARTESIAN_POINT('Ctrl Pts',(-8.82267925698027,15.2,-5.49637464691604));
#275721=CARTESIAN_POINT('Ctrl Pts',(-8.824648700705,15.2,-5.49732708982732));
#275722=CARTESIAN_POINT('Ctrl Pts',(-8.82666980631291,15.2,-5.49829697667287));
#275723=CARTESIAN_POINT('Ctrl Pts',(-8.8286909121044,15.2,-5.49926686360652));
#275724=CARTESIAN_POINT('Ctrl Pts',(-8.8307636790539,15.2,-5.50025419422024));
#275725=CARTESIAN_POINT('Ctrl Pts',(-8.83288758275648,15.2,-5.50125805810941));
#275726=CARTESIAN_POINT('Ctrl Pts',(-8.83501148626615,15.2,-5.5022619219074));
#275727=CARTESIAN_POINT('Ctrl Pts',(-8.83718652676331,15.2,-5.5032823192667));
#275728=CARTESIAN_POINT('Ctrl Pts',(-8.83941219327598,15.2,-5.50431836423379));
#275729=CARTESIAN_POINT('Ctrl Pts',(-8.84163785978865,15.2,-5.50535440920089));
#275730=CARTESIAN_POINT('Ctrl Pts',(-8.84391415062677,15.2,-5.50640610420631));
#275731=CARTESIAN_POINT('Ctrl Pts',(-8.84624056437339,15.2,-5.50747258641693));
#275732=CARTESIAN_POINT('Ctrl Pts',(-8.84856697833133,15.2,-5.50853906872442));
#275733=CARTESIAN_POINT('Ctrl Pts',(-8.85094351562051,15.2,-5.50962034055873));
#275734=CARTESIAN_POINT('Ctrl Pts',(-8.85336968650611,15.2,-5.51071556661937));
#275735=CARTESIAN_POINT('Ctrl Pts',(-8.85579585717132,15.2,-5.51181079258052));
#275736=CARTESIAN_POINT('Ctrl Pts',(-8.85827166062738,15.2,-5.51291996937641));
#275737=CARTESIAN_POINT('Ctrl Pts',(-8.86079661537112,15.2,-5.51404228958621));
#275738=CARTESIAN_POINT('Ctrl Pts',(-8.86332157011486,15.2,-5.51516460979602));
#275739=CARTESIAN_POINT('Ctrl Pts',(-8.86589567860466,15.2,-5.51630007113808));
#275740=CARTESIAN_POINT('Ctrl Pts',(-8.86851846634056,15.2,-5.51744788067916));
#275741=CARTESIAN_POINT('Ctrl Pts',(-8.87114125407647,15.2,-5.51859569022025));
#275742=CARTESIAN_POINT('Ctrl Pts',(-8.87381272327231,15.2,-5.51975585284065));
#275743=CARTESIAN_POINT('Ctrl Pts',(-8.87653241117021,15.2,-5.52092759338061));
#275744=CARTESIAN_POINT('Ctrl Pts',(-8.87925209931515,15.2,-5.52209933402701));
#275745=CARTESIAN_POINT('Ctrl Pts',(-8.88202000817308,15.2,-5.52328265684124));
#275746=CARTESIAN_POINT('Ctrl Pts',(-8.88483568141196,15.2,-5.52447681032346));
#275747=CARTESIAN_POINT('Ctrl Pts',(-8.88765135439507,15.2,-5.5256709636972));
#275748=CARTESIAN_POINT('Ctrl Pts',(-8.89051479414961,15.2,-5.52687594635476));
#275749=CARTESIAN_POINT('Ctrl Pts',(-8.89342555597366,15.2,-5.52809103098278));
#275750=CARTESIAN_POINT('Ctrl Pts',(-8.8963363177977,15.2,-5.52930611561081));
#275751=CARTESIAN_POINT('Ctrl Pts',(-8.89929439944313,15.2,-5.53053130127758));
#275752=CARTESIAN_POINT('Ctrl Pts',(-8.90229936641411,15.2,-5.53176587589877));
#275753=CARTESIAN_POINT('Ctrl Pts',(-8.90530433365805,15.2,-5.53300045063209));
#275754=CARTESIAN_POINT('Ctrl Pts',(-8.90835618651481,15.2,-5.53424441469965));
#275755=CARTESIAN_POINT('Ctrl Pts',(-8.9114544946857,15.2,-5.53549707276831));
#275756=CARTESIAN_POINT('Ctrl Pts',(-8.91455280257515,15.2,-5.53674973072317));
#275757=CARTESIAN_POINT('Ctrl Pts',(-8.91769756619174,15.2,-5.53801108558147));
#275758=CARTESIAN_POINT('Ctrl Pts',(-8.92088836400686,15.2,-5.53928045845776));
#275759=CARTESIAN_POINT('Ctrl Pts',(-8.92407916182198,15.2,-5.54054983133406));
#275760=CARTESIAN_POINT('Ctrl Pts',(-8.92731599336455,15.2,-5.54182722173214));
#275761=CARTESIAN_POINT('Ctrl Pts',(-8.93059844440887,15.2,-5.54311197160163));
#275762=CARTESIAN_POINT('Ctrl Pts',(-8.93388089575133,15.2,-5.54439672158783));
#275763=CARTESIAN_POINT('Ctrl Pts',(-8.93720896609641,15.2,-5.54568882888127));
#275764=CARTESIAN_POINT('Ctrl Pts',(-8.94058224953474,15.2,-5.54698765010066));
#275765=CARTESIAN_POINT('Ctrl Pts',(-8.94395553266667,15.2,-5.54828647120208));
#275766=CARTESIAN_POINT('Ctrl Pts',(-8.94737402688413,15.2,-5.54959200568932));
#275767=CARTESIAN_POINT('Ctrl Pts',(-8.95083733100831,15.2,-5.550903625725));
#275768=CARTESIAN_POINT('Ctrl Pts',(-8.95430063513249,15.2,-5.55221524576068));
#275769=CARTESIAN_POINT('Ctrl Pts',(-8.95780874996059,15.2,-5.55353294947097));
#275770=CARTESIAN_POINT('Ctrl Pts',(-8.96136128017309,15.2,-5.55485612365535));
#275771=CARTESIAN_POINT('Ctrl Pts',(-8.96491381070828,15.2,-5.55617929795992));
#275772=CARTESIAN_POINT('Ctrl Pts',(-8.96851075529544,15.2,-5.55750794212235));
#275773=CARTESIAN_POINT('Ctrl Pts',(-8.97215172666352,15.2,-5.55884145636203));
#275774=CARTESIAN_POINT('Ctrl Pts',(-8.97579269770089,15.2,-5.56017497048057));
#275775=CARTESIAN_POINT('Ctrl Pts',(-8.9794776951951,15.2,-5.56151335337662));
#275776=CARTESIAN_POINT('Ctrl Pts',(-8.98320633349334,15.2,-5.56285602050061));
#275777=CARTESIAN_POINT('Ctrl Pts',(-8.98693497179157,15.2,-5.56419868762461));
#275778=CARTESIAN_POINT('Ctrl Pts',(-8.99070725611604,15.2,-5.56554563715898));
#275779=CARTESIAN_POINT('Ctrl Pts',(-8.99452280230889,15.2,-5.56689629644308));
#275780=CARTESIAN_POINT('Ctrl Pts',(-8.99770242425178,15.2,-5.5680218458874));
#275781=CARTESIAN_POINT('Ctrl Pts',(-9.00091209151763,15.2,-5.56914997208176));
#275782=CARTESIAN_POINT('Ctrl Pts',(-9.00415158832164,15.2,-5.5702803484011));
#275783=CARTESIAN_POINT('Ctrl Pts',(-9.00739108512563,15.2,-5.57141072472042));
#275784=CARTESIAN_POINT('Ctrl Pts',(-9.01066041008883,15.2,-5.57254335434425));
#275785=CARTESIAN_POINT('Ctrl Pts',(-9.01395935121486,15.2,-5.57367791476606));
#275786=CARTESIAN_POINT('Ctrl Pts',(-9.01725829234089,15.2,-5.57481247518789));
#275787=CARTESIAN_POINT('Ctrl Pts',(-9.02058684908886,15.2,-5.57594896675556));
#275788=CARTESIAN_POINT('Ctrl Pts',(-9.02394481103331,15.2,-5.57708707724167));
#275789=CARTESIAN_POINT('Ctrl Pts',(-9.02730277297776,15.2,-5.57822518772779));
#275790=CARTESIAN_POINT('Ctrl Pts',(-9.03069013840847,15.2,-5.57936491817877));
#275791=CARTESIAN_POINT('Ctrl Pts',(-9.03410670120185,15.2,-5.58050595797563));
#275792=CARTESIAN_POINT('Ctrl Pts',(-9.03752326399521,15.2,-5.58164699777248));
#275793=CARTESIAN_POINT('Ctrl Pts',(-9.0409690221759,15.2,-5.58278935031363));
#275794=CARTESIAN_POINT('Ctrl Pts',(-9.04444377071907,15.2,-5.58393271079979));
#275795=CARTESIAN_POINT('Ctrl Pts',(-9.04791851926226,15.2,-5.58507607128596));
#275796=CARTESIAN_POINT('Ctrl Pts',(-9.05142225763523,15.2,-5.58622044081932));
#275797=CARTESIAN_POINT('Ctrl Pts',(-9.05495478124785,15.2,-5.58736552137491));
#275798=CARTESIAN_POINT('Ctrl Pts',(-9.05848730486047,15.2,-5.5885106019305));
#275799=CARTESIAN_POINT('Ctrl Pts',(-9.06204861416326,15.2,-5.58965639411467));
#275800=CARTESIAN_POINT('Ctrl Pts',(-9.06563850719182,15.2,-5.59080260715807));
#275801=CARTESIAN_POINT('Ctrl Pts',(-9.06922840022036,15.2,-5.59194882020148));
#275802=CARTESIAN_POINT('Ctrl Pts',(-9.07284687567467,15.2,-5.5930954523889));
#275803=CARTESIAN_POINT('Ctrl Pts',(-9.07649373526034,15.2,-5.59424221870834));
#275804=CARTESIAN_POINT('Ctrl Pts',(-9.080140594846,15.2,-5.5953889850278));
#275805=CARTESIAN_POINT('Ctrl Pts',(-9.08381583734878,15.2,-5.59653588415004));
#275806=CARTESIAN_POINT('Ctrl Pts',(-9.08751926672607,15.2,-5.59768263560834));
#275807=CARTESIAN_POINT('Ctrl Pts',(-9.0912226956997,15.2,-5.59882938694166));
#275808=CARTESIAN_POINT('Ctrl Pts',(-9.09495431111479,15.2,-5.59997599026944));
#275809=CARTESIAN_POINT('Ctrl Pts',(-9.09871391375824,15.2,-5.60112216757509));
#275810=CARTESIAN_POINT('Ctrl Pts',(-9.10247351681149,15.2,-5.60226834500568));
#275811=CARTESIAN_POINT('Ctrl Pts',(-9.10626111065876,15.2,-5.60341409837796));
#275812=CARTESIAN_POINT('Ctrl Pts',(-9.11007649947594,15.2,-5.60455915330858));
#275813=CARTESIAN_POINT('Ctrl Pts',(-9.11389188829312,15.2,-5.60570420823918));
#275814=CARTESIAN_POINT('Ctrl Pts',(-9.11773507289039,15.2,-5.6068485657226));
#275815=CARTESIAN_POINT('Ctrl Pts',(-9.12160586073537,15.2,-5.6079919580838));
#275816=CARTESIAN_POINT('Ctrl Pts',(-9.12547664858033,15.2,-5.60913535044498));
#275817=CARTESIAN_POINT('Ctrl Pts',(-9.12937503967234,15.2,-5.61027777802153));
#275818=CARTESIAN_POINT('Ctrl Pts',(-9.13330084285269,15.2,-5.61141897634254));
#275819=CARTESIAN_POINT('Ctrl Pts',(-9.13722664603305,15.2,-5.61256017466353));
#275820=CARTESIAN_POINT('Ctrl Pts',(-9.14117986225791,15.2,-5.61370014517547));
#275821=CARTESIAN_POINT('Ctrl Pts',(-9.14516030267316,15.2,-5.61483862767555));
#275822=CARTESIAN_POINT('Ctrl Pts',(-9.14914074308841,15.2,-5.61597711017563));
#275823=CARTESIAN_POINT('Ctrl Pts',(-9.15314840722661,15.2,-5.61711410606457));
#275824=CARTESIAN_POINT('Ctrl Pts',(-9.15718310854461,15.2,-5.6182493586341));
#275825=CARTESIAN_POINT('Ctrl Pts',(-9.1612178098626,15.2,-5.61938461120361));
#275826=CARTESIAN_POINT('Ctrl Pts',(-9.16527954857928,15.2,-5.62051812167203));
#275827=CARTESIAN_POINT('Ctrl Pts',(-9.16936813901443,15.2,-5.62164963994107));
#275828=CARTESIAN_POINT('Ctrl Pts',(-9.17345672944959,15.2,-5.6227811582101));
#275829=CARTESIAN_POINT('Ctrl Pts',(-9.17757216966108,15.2,-5.62391068283891));
#275830=CARTESIAN_POINT('Ctrl Pts',(-9.18171428000832,15.2,-5.62503796874169));
#275831=CARTESIAN_POINT('Ctrl Pts',(-9.18502796846671,15.2,-5.62593979751306));
#275832=CARTESIAN_POINT('Ctrl Pts',(-9.18835872356594,15.2,-5.62684019365371));
#275833=CARTESIAN_POINT('Ctrl Pts',(-9.19170645280569,15.2,-5.62773903114698));
#275834=CARTESIAN_POINT('Ctrl Pts',(-9.1950541815893,15.2,-5.62863786851779));
#275835=CARTESIAN_POINT('Ctrl Pts',(-9.19841888494494,15.2,-5.62953514950466));
#275836=CARTESIAN_POINT('Ctrl Pts',(-9.20180046973936,15.2,-5.63043074949108));
#275837=CARTESIAN_POINT('Ctrl Pts',(-9.2051820549945,15.2,-5.63132634959952));
#275838=CARTESIAN_POINT('Ctrl Pts',(-9.20858052225944,15.2,-5.63222026905579));
#275839=CARTESIAN_POINT('Ctrl Pts',(-9.21199577755839,15.2,-5.63311238660422));
#275840=CARTESIAN_POINT('Ctrl Pts',(-9.21541103239202,15.2,-5.6340045040311));
#275841=CARTESIAN_POINT('Ctrl Pts',(-9.21884307743735,15.2,-5.63489482060821));
#275842=CARTESIAN_POINT('Ctrl Pts',(-9.22229182020988,15.2,-5.63578321470237));
#275843=CARTESIAN_POINT('Ctrl Pts',(-9.2257405634523,15.2,-5.63667160891759));
#275844=CARTESIAN_POINT('Ctrl Pts',(-9.22920600346796,15.2,-5.63755808168615));
#275845=CARTESIAN_POINT('Ctrl Pts',(-9.23268805205535,15.2,-5.63844251511168));
#275846=CARTESIAN_POINT('Ctrl Pts',(-9.23617010016832,15.2,-5.63932694841672));
#275847=CARTESIAN_POINT('Ctrl Pts',(-9.23966875394013,15.2,-5.64020934176098));
#275848=CARTESIAN_POINT('Ctrl Pts',(-9.24318392476279,15.2,-5.64108957791138));
#275849=CARTESIAN_POINT('Ctrl Pts',(-9.24669909606439,15.2,-5.64196981418171));
#275850=CARTESIAN_POINT('Ctrl Pts',(-9.25023078448187,15.2,-5.64284789414069));
#275851=CARTESIAN_POINT('Ctrl Pts',(-9.25377889906521,15.2,-5.64372370285493));
#275852=CARTESIAN_POINT('Ctrl Pts',(-9.2573270131651,15.2,-5.64459951144985));
#275853=CARTESIAN_POINT('Ctrl Pts',(-9.2608915536624,15.2,-5.64547304632609));
#275854=CARTESIAN_POINT('Ctrl Pts',(-9.26447243321381,15.2,-5.6463441957986));
#275855=CARTESIAN_POINT('Ctrl Pts',(-9.26805331325311,15.2,-5.64721534538981));
#275856=CARTESIAN_POINT('Ctrl Pts',(-9.2716505298031,15.2,-5.64808410911266));
#275857=CARTESIAN_POINT('Ctrl Pts',(-9.27526399577888,15.2,-5.64895037460415));
#275858=CARTESIAN_POINT('Ctrl Pts',(-9.27887746126233,15.2,-5.64981663997761));
#275859=CARTESIAN_POINT('Ctrl Pts',(-9.28250717538693,15.2,-5.65068040619046));
#275860=CARTESIAN_POINT('Ctrl Pts',(-9.28615305142057,15.2,-5.65154156234256));
#275861=CARTESIAN_POINT('Ctrl Pts',(-9.28979892795095,15.2,-5.65240271861198));
#275862=CARTESIAN_POINT('Ctrl Pts',(-9.29346096421862,15.2,-5.65326126572231));
#275863=CARTESIAN_POINT('Ctrl Pts',(-9.29713907476917,15.2,-5.65411709321728));
#275864=CARTESIAN_POINT('Ctrl Pts',(-9.30081718481857,15.2,-5.65497292059564));
#275865=CARTESIAN_POINT('Ctrl Pts',(-9.30451136788721,15.2,-5.65582602702467));
#275866=CARTESIAN_POINT('Ctrl Pts',(-9.30822153736005,15.2,-5.65667630584434));
#275867=CARTESIAN_POINT('Ctrl Pts',(-9.3119317073384,15.2,-5.65752658477986));
#275868=CARTESIAN_POINT('Ctrl Pts',(-9.31565786331827,15.2,-5.65837403525957));
#275869=CARTESIAN_POINT('Ctrl Pts',(-9.31939991929999,15.2,-5.65921855075003));
#275870=CARTESIAN_POINT('Ctrl Pts',(-9.3231419752817,15.2,-5.6600630662405));
#275871=CARTESIAN_POINT('Ctrl Pts',(-9.32689993141806,15.2,-5.66090464463618));
#275872=CARTESIAN_POINT('Ctrl Pts',(-9.33067370012535,15.2,-5.66174318290379));
#275873=CARTESIAN_POINT('Ctrl Pts',(-9.33444746831846,15.2,-5.66258172105715));
#275874=CARTESIAN_POINT('Ctrl Pts',(-9.33823705201902,15.2,-5.66341721691093));
#275875=CARTESIAN_POINT('Ctrl Pts',(-9.34204236228074,15.2,-5.66424956645779));
#275876=CARTESIAN_POINT('Ctrl Pts',(-9.34584767306092,15.2,-5.66508191611807));
#275877=CARTESIAN_POINT('Ctrl Pts',(-9.34966871181662,15.2,-5.66591111958483));
#275878=CARTESIAN_POINT('Ctrl Pts',(-9.35350539436063,15.2,-5.66673707318507));
#275879=CARTESIAN_POINT('Ctrl Pts',(-9.3573420763819,15.2,-5.66756302667276));
#275880=CARTESIAN_POINT('Ctrl Pts',(-9.36119440090951,15.2,-5.66838573019423));
#275881=CARTESIAN_POINT('Ctrl Pts',(-9.36506228375894,15.2,-5.66920508168302));
#275882=CARTESIAN_POINT('Ctrl Pts',(-9.36893016713539,15.2,-5.67002443328345));
#275883=CARTESIAN_POINT('Ctrl Pts',(-9.37281360963223,15.2,-5.6708404320139));
#275884=CARTESIAN_POINT('Ctrl Pts',(-9.37671252587417,15.2,-5.67165297837625));
#275885=CARTESIAN_POINT('Ctrl Pts',(-9.3806114415849,15.2,-5.67246552462789));
#275886=CARTESIAN_POINT('Ctrl Pts',(-9.38452583170395,15.2,-5.67327461622755));
#275887=CARTESIAN_POINT('Ctrl Pts',(-9.38845561243721,15.2,-5.67408015571747));
#275888=CARTESIAN_POINT('Ctrl Pts',(-9.3923853937059,15.2,-5.67488569531716));
#275889=CARTESIAN_POINT('Ctrl Pts',(-9.3963305643515,15.2,-5.67568768109977));
#275890=CARTESIAN_POINT('Ctrl Pts',(-9.40029104312391,15.2,-5.67648601536526));
#275891=CARTESIAN_POINT('Ctrl Pts',(-9.4042515213567,15.2,-5.67728434952198));
#275892=CARTESIAN_POINT('Ctrl Pts',(-9.4082273074975,15.2,-5.67807903148776));
#275893=CARTESIAN_POINT('Ctrl Pts',(-9.41221831761414,15.2,-5.67886996314571));
#275894=CARTESIAN_POINT('Ctrl Pts',(-9.41620932827454,15.2,-5.67966089491143));
#275895=CARTESIAN_POINT('Ctrl Pts',(-9.42021556338748,15.2,-5.68044807716821));
#275896=CARTESIAN_POINT('Ctrl Pts',(-9.42423694073607,15.2,-5.68123141349223));
#275897=CARTESIAN_POINT('Ctrl Pts',(-9.42825831753676,15.2,-5.68201474970952));
#275898=CARTESIAN_POINT('Ctrl Pts',(-9.43229483704532,15.2,-5.682794239489));
#275899=CARTESIAN_POINT('Ctrl Pts',(-9.43634641587924,15.2,-5.68356978714823));
#275900=CARTESIAN_POINT('Ctrl Pts',(-9.44039799526518,15.2,-5.68434533491312));
#275901=CARTESIAN_POINT('Ctrl Pts',(-9.4444646351331,15.2,-5.68511694119431));
#275902=CARTESIAN_POINT('Ctrl Pts',(-9.44854625379999,15.2,-5.68588451095837));
#275903=CARTESIAN_POINT('Ctrl Pts',(-9.45364827685554,15.2,-5.68684397311115));
#275904=CARTESIAN_POINT('Ctrl Pts',(-9.4587737026627,15.2,-5.68779713090737));
#275905=CARTESIAN_POINT('Ctrl Pts',(-9.46392237497781,15.2,-5.68874379730055));
#275906=CARTESIAN_POINT('Ctrl Pts',(-9.46804131249317,15.2,-5.68950113035317));
#275907=CARTESIAN_POINT('Ctrl Pts',(-9.47217512823459,15.2,-5.6902543117217));
#275908=CARTESIAN_POINT('Ctrl Pts',(-9.47632374033837,15.2,-5.69100324866091));
#275909=CARTESIAN_POINT('Ctrl Pts',(-9.48047235300741,15.2,-5.69175218570217));
#275910=CARTESIAN_POINT('Ctrl Pts',(-9.48463576118337,15.2,-5.69249687712635));
#275911=CARTESIAN_POINT('Ctrl Pts',(-9.48881388596666,15.2,-5.69323723350004));
#275912=CARTESIAN_POINT('Ctrl Pts',(-9.49299201074995,15.2,-5.69397758987372));
#275913=CARTESIAN_POINT('Ctrl Pts',(-9.49718485192381,15.2,-5.69471361096912));
#275914=CARTESIAN_POINT('Ctrl Pts',(-9.50139233115459,15.2,-5.69544520611965));
#275915=CARTESIAN_POINT('Ctrl Pts',(-9.50559980981211,15.2,-5.69617680117049));
#275916=CARTESIAN_POINT('Ctrl Pts',(-9.50982192457151,15.2,-5.69690396997477));
#275917=CARTESIAN_POINT('Ctrl Pts',(-9.51405859552212,15.2,-5.69762662497454));
#275918=CARTESIAN_POINT('Ctrl Pts',(-9.51829526704998,15.2,-5.69834928007278));
#275919=CARTESIAN_POINT('Ctrl Pts',(-9.52254649656072,15.2,-5.6990674200755));
#275920=CARTESIAN_POINT('Ctrl Pts',(-9.52681220340578,15.2,-5.69978095839169));
#275921=CARTESIAN_POINT('Ctrl Pts',(-9.53107790966964,15.2,-5.70049449661066));
#275922=CARTESIAN_POINT('Ctrl Pts',(-9.53535809505942,15.2,-5.70120343125524));
#275923=CARTESIAN_POINT('Ctrl Pts',(-9.53965267920739,15.2,-5.70190767697575));
#275924=CARTESIAN_POINT('Ctrl Pts',(-9.54394726394048,15.2,-5.70261192279221));
#275925=CARTESIAN_POINT('Ctrl Pts',(-9.5482562481357,15.2,-5.70331147900367));
#275926=CARTESIAN_POINT('Ctrl Pts',(-9.55257955314409,15.2,-5.70400625890916));
#275927=CARTESIAN_POINT('Ctrl Pts',(-9.55690285756343,15.2,-5.70470103871999));
#275928=CARTESIAN_POINT('Ctrl Pts',(-9.56124048313994,15.2,-5.70539104347189));
#275929=CARTESIAN_POINT('Ctrl Pts',(-9.56559235189437,15.2,-5.70607618719398));
#275930=CARTESIAN_POINT('Ctrl Pts',(-9.57103218828209,15.2,-5.7069326169166));
#275931=CARTESIAN_POINT('Ctrl Pts',(-9.57649427917041,15.2,-5.70778145088903));
#275932=CARTESIAN_POINT('Ctrl Pts',(-9.58197847243313,15.2,-5.70862252644498));
#275933=CARTESIAN_POINT('Ctrl Pts',(-9.58636582728242,15.2,-5.70929538692643));
#275934=CARTESIAN_POINT('Ctrl Pts',(-9.59076732850055,15.2,-5.70996328121627));
#275935=CARTESIAN_POINT('Ctrl Pts',(-9.59518289940747,15.2,-5.71062612639619));
#275936=CARTESIAN_POINT('Ctrl Pts',(-9.59849457728686,15.2,-5.71112326023597));
#275937=CARTESIAN_POINT('Ctrl Pts',(-9.60181416738305,15.2,-5.71161755447166));
#275938=CARTESIAN_POINT('Ctrl Pts',(-9.60514164009616,15.2,-5.71210897337022));
#275939=CARTESIAN_POINT('Ctrl Pts',(-9.60846911280928,15.2,-5.71260039226878));
#275940=CARTESIAN_POINT('Ctrl Pts',(-9.61180446668815,15.2,-5.71308893688435));
#275941=CARTESIAN_POINT('Ctrl Pts',(-9.615147669025,15.2,-5.71357457178337));
#275942=CARTESIAN_POINT('Ctrl Pts',(-9.61849087136186,15.2,-5.71406020668239));
#275943=CARTESIAN_POINT('Ctrl Pts',(-9.62184192330674,15.2,-5.7145429320482));
#275944=CARTESIAN_POINT('Ctrl Pts',(-9.62520079160068,15.2,-5.71502271444769));
#275945=CARTESIAN_POINT('Ctrl Pts',(-9.62855965989462,15.2,-5.71550249684718));
#275946=CARTESIAN_POINT('Ctrl Pts',(-9.63192634415213,15.2,-5.71597933645152));
#275947=CARTESIAN_POINT('Ctrl Pts',(-9.63530081407221,15.2,-5.71645319787499));
#275948=CARTESIAN_POINT('Ctrl Pts',(-9.63867528399228,15.2,-5.71692705929846));
#275949=CARTESIAN_POINT('Ctrl Pts',(-9.64205753893522,15.2,-5.71739794384796));
#275950=CARTESIAN_POINT('Ctrl Pts',(-9.64544754526932,15.2,-5.71786581770637));
#275951=CARTESIAN_POINT('Ctrl Pts',(-9.64883755221928,15.2,-5.71833369164978));
#275952=CARTESIAN_POINT('Ctrl Pts',(-9.65223531184643,15.2,-5.71879855456734));
#275953=CARTESIAN_POINT('Ctrl Pts',(-9.65564079271741,15.2,-5.71926037305071));
#275954=CARTESIAN_POINT('Ctrl Pts',(-9.65904627296972,15.2,-5.71972219145018));
#275955=CARTESIAN_POINT('Ctrl Pts',(-9.66245947354663,15.2,-5.72018096598314));
#275956=CARTESIAN_POINT('Ctrl Pts',(-9.66588036288134,15.2,-5.72063666284132));
#275957=CARTESIAN_POINT('Ctrl Pts',(-9.66930125221606,15.2,-5.7210923596995));
#275958=CARTESIAN_POINT('Ctrl Pts',(-9.67272983131233,15.2,-5.72154497891475));
#275959=CARTESIAN_POINT('Ctrl Pts',(-9.67616606624479,15.2,-5.72199448873378));
#275960=CARTESIAN_POINT('Ctrl Pts',(-9.67960230117725,15.2,-5.72244399855281));
#275961=CARTESIAN_POINT('Ctrl Pts',(-9.68304619435662,15.2,-5.72289039763038));
#275962=CARTESIAN_POINT('Ctrl Pts',(-9.68649771220521,15.2,-5.72333365403297));
#275963=CARTESIAN_POINT('Ctrl Pts',(-9.68994923005379,15.2,-5.72377691043556));
#275964=CARTESIAN_POINT('Ctrl Pts',(-9.69340837381555,15.2,-5.72421702476796));
#275965=CARTESIAN_POINT('Ctrl Pts',(-9.69687511114726,15.2,-5.72465396371069));
#275966=CARTESIAN_POINT('Ctrl Pts',(-9.70034184847896,15.2,-5.72509090265342));
#275967=CARTESIAN_POINT('Ctrl Pts',(-9.70381618063514,15.2,-5.72552466723804));
#275968=CARTESIAN_POINT('Ctrl Pts',(-9.70729807450762,15.2,-5.72595522418117));
#275969=CARTESIAN_POINT('Ctrl Pts',(-9.71077996901264,15.2,-5.72638578120253));
#275970=CARTESIAN_POINT('Ctrl Pts',(-9.71426942676977,15.2,-5.72681313151463));
#275971=CARTESIAN_POINT('Ctrl Pts',(-9.71776641477902,15.2,-5.72723724211749));
#275972=CARTESIAN_POINT('Ctrl Pts',(-9.72242906439922,15.2,-5.7278027227929));
#275973=CARTESIAN_POINT('Ctrl Pts',(-9.72710510388947,15.2,-5.72836244767296));
#275974=CARTESIAN_POINT('Ctrl Pts',(-9.73179445747181,15.2,-5.72891633824133));
#275975=CARTESIAN_POINT('Ctrl Pts',(-9.73531147281829,15.2,-5.72933175618647));
#275976=CARTESIAN_POINT('Ctrl Pts',(-9.73883597809413,15.2,-5.72974389375332));
#275977=CARTESIAN_POINT('Ctrl Pts',(-9.74236794184014,15.2,-5.73015271873875));
#275978=CARTESIAN_POINT('Ctrl Pts',(-9.74589990558615,15.2,-5.73056154372418));
#275979=CARTESIAN_POINT('Ctrl Pts',(-9.74943932694002,15.2,-5.73096705712652));
#275980=CARTESIAN_POINT('Ctrl Pts',(-9.7529861762268,15.2,-5.73136922711236));
#275981=CARTESIAN_POINT('Ctrl Pts',(-9.75653302615793,15.2,-5.73177139717127));
#275982=CARTESIAN_POINT('Ctrl Pts',(-9.76008730432449,15.2,-5.73217022509589));
#275983=CARTESIAN_POINT('Ctrl Pts',(-9.76364897830146,15.2,-5.73256567861124));
#275984=CARTESIAN_POINT('Ctrl Pts',(-9.76839787585902,15.2,-5.7330929498453));
#275985=CARTESIAN_POINT('Ctrl Pts',(-9.77315992287876,15.2,-5.73361422294126));
#275986=CARTESIAN_POINT('Ctrl Pts',(-9.77793504637643,15.2,-5.73412942673287));
#275987=CARTESIAN_POINT('Ctrl Pts',(-9.78151638916232,15.2,-5.73451582959412));
#275988=CARTESIAN_POINT('Ctrl Pts',(-9.78510508708951,15.2,-5.734898817421));
#275989=CARTESIAN_POINT('Ctrl Pts',(-9.78870111005434,15.2,-5.73527836092658));
#275990=CARTESIAN_POINT('Ctrl Pts',(-9.79229713301916,15.2,-5.73565790443214));
#275991=CARTESIAN_POINT('Ctrl Pts',(-9.7959004807284,15.2,-5.7360340042152));
#275992=CARTESIAN_POINT('Ctrl Pts',(-9.79951112251289,15.2,-5.73640662911881));
#275993=CARTESIAN_POINT('Ctrl Pts',(-9.80432531199617,15.2,-5.73690346236873));
#275994=CARTESIAN_POINT('Ctrl Pts',(-9.8091524688362,15.2,-5.73739411877364));
#275995=CARTESIAN_POINT('Ctrl Pts',(-9.81399251976667,15.2,-5.73787852746671));
#275996=CARTESIAN_POINT('Ctrl Pts',(-9.81762255763479,15.2,-5.73824183395351));
#275997=CARTESIAN_POINT('Ctrl Pts',(-9.82125984956925,15.2,-5.73860162582378));
#275998=CARTESIAN_POINT('Ctrl Pts',(-9.82490436435288,15.2,-5.73895787568615));
#275999=CARTESIAN_POINT('Ctrl Pts',(-9.8285488791365,15.2,-5.73931412554851));
#276000=CARTESIAN_POINT('Ctrl Pts',(-9.83220061632649,15.2,-5.73966683146062));
#276001=CARTESIAN_POINT('Ctrl Pts',(-9.83585954683383,15.2,-5.74001596488246));
#276002=CARTESIAN_POINT('Ctrl Pts',(-9.83951847734118,15.2,-5.7403650983043));
#276003=CARTESIAN_POINT('Ctrl Pts',(-9.84318460051701,15.2,-5.74071065853743));
#276004=CARTESIAN_POINT('Ctrl Pts',(-9.84685788538257,15.2,-5.74105261790049));
#276005=CARTESIAN_POINT('Ctrl Pts',(-9.85053117091544,15.2,-5.74139457732568));
#276006=CARTESIAN_POINT('Ctrl Pts',(-9.85421161878367,15.2,-5.74173293480819));
#276007=CARTESIAN_POINT('Ctrl Pts',(-9.8578991987789,15.2,-5.74206766185634));
#276008=CARTESIAN_POINT('Ctrl Pts',(-9.86281597098936,15.2,-5.74251396448586));
#276009=CARTESIAN_POINT('Ctrl Pts',(-9.86774542312871,15.2,-5.74295381429955));
#276010=CARTESIAN_POINT('Ctrl Pts',(-9.87268748461278,15.2,-5.74338714293122));
#276011=CARTESIAN_POINT('Ctrl Pts',(-9.87639403089416,15.2,-5.74371213941973));
#276012=CARTESIAN_POINT('Ctrl Pts',(-9.88010766974699,15.2,-5.74403346845046));
#276013=CARTESIAN_POINT('Ctrl Pts',(-9.88382836925522,15.2,-5.74435109991355));
#276014=CARTESIAN_POINT('Ctrl Pts',(-9.88754906876343,15.2,-5.74466873137664));
#276015=CARTESIAN_POINT('Ctrl Pts',(-9.89127682890582,15.2,-5.74498266487651));
#276016=CARTESIAN_POINT('Ctrl Pts',(-9.89501162118583,15.2,-5.74529287340741));
#276017=CARTESIAN_POINT('Ctrl Pts',(-9.89874641414433,15.2,-5.74560308199467));
#276018=CARTESIAN_POINT('Ctrl Pts',(-9.90248823858813,15.2,-5.74590956647255));
#276019=CARTESIAN_POINT('Ctrl Pts',(-9.90623706809226,15.2,-5.7462123000577));
#276020=CARTESIAN_POINT('Ctrl Pts',(-9.90998589691535,15.2,-5.74651503358786));
#276021=CARTESIAN_POINT('Ctrl Pts',(-9.91374173067972,15.2,-5.74681401720988));
#276022=CARTESIAN_POINT('Ctrl Pts',(-9.91750453887694,15.2,-5.74710922349049));
#276023=CARTESIAN_POINT('Ctrl Pts',(-9.92126734707416,15.2,-5.7474044297711));
#276024=CARTESIAN_POINT('Ctrl Pts',(-9.92503712877347,15.2,-5.74769585587613));
#276025=CARTESIAN_POINT('Ctrl Pts',(-9.92881384702844,15.2,-5.74798346974197));
#276026=CARTESIAN_POINT('Ctrl Pts',(-9.9325905652834,15.2,-5.74827108360781));
#276027=CARTESIAN_POINT('Ctrl Pts',(-9.93637421943378,15.2,-5.74855488345867));
#276028=CARTESIAN_POINT('Ctrl Pts',(-9.9401647829799,15.2,-5.74883484474145));
#276029=CARTESIAN_POINT('Ctrl Pts',(-9.94648238911965,15.2,-5.74930144689638));
#276030=CARTESIAN_POINT('Ctrl Pts',(-9.95281918628111,15.2,-5.74975738256963));
#276031=CARTESIAN_POINT('Ctrl Pts',(-9.95917514600006,15.2,-5.75020264100001));
#276032=CARTESIAN_POINT('Origin',(-5.66257110645729E-14,15.2,-1.77635683940025E-14));
#276033=CARTESIAN_POINT('',(-8.56667970938041,15.2,-5.85257411403214));
#276034=CARTESIAN_POINT('',(-8.56667970938041,12.2,-5.85257411403214));
#276035=CARTESIAN_POINT('',(-8.56667970900006,15.2,-5.85257411400002));
#276036=CARTESIAN_POINT('Origin',(-5.66257110645729E-14,12.2,-1.77635683940025E-14));
#276037=CARTESIAN_POINT('Origin',(-5.66257110645729E-14,15.2,-1.77635683940025E-14));
#276038=CARTESIAN_POINT('Origin',(-5.66257110645729E-14,15.2,-1.77635683940025E-14));
#276039=CARTESIAN_POINT('',(-9.27155330300005,15.2,-6.80355049700001));
#276040=CARTESIAN_POINT('',(-9.03946594400006,15.2,-7.10901226900001));
#276041=CARTESIAN_POINT('Origin',(-5.66257110645729E-14,15.2,-1.77635683940025E-14));
#276042=CARTESIAN_POINT('',(-9.03946594400006,12.2,-7.10901226900001));
#276043=CARTESIAN_POINT('',(-9.03946594400006,15.2,-7.10901226900001));
#276044=CARTESIAN_POINT('',(-9.27155330300005,12.2,-6.80355049700001));
#276045=CARTESIAN_POINT('Origin',(-5.66257110645729E-14,12.2,-1.77635683940025E-14));
#276046=CARTESIAN_POINT('',(-9.27155330200006,15.2,-6.80355049700001));
#276047=CARTESIAN_POINT('Ctrl Pts',(-9.03946594400006,15.2,-7.10901226900001));
#276048=CARTESIAN_POINT('Ctrl Pts',(-9.03946594400006,11.6,-7.10901226900001));
#276049=CARTESIAN_POINT('Ctrl Pts',(-9.03871859600006,15.2,-7.10885083600001));
#276050=CARTESIAN_POINT('Ctrl Pts',(-9.03871859600006,11.6,-7.10885083600001));
#276051=CARTESIAN_POINT('Ctrl Pts',(-9.03722439200006,15.2,-7.10852778400002));
#276052=CARTESIAN_POINT('Ctrl Pts',(-9.03722439200006,11.6,-7.10852778400002));
#276053=CARTESIAN_POINT('Ctrl Pts',(-9.03498456200006,15.2,-7.10804263900001));
#276054=CARTESIAN_POINT('Ctrl Pts',(-9.03498456200006,11.6,-7.10804263900001));
#276055=CARTESIAN_POINT('Ctrl Pts',(-9.03200107200006,15.2,-7.10739465100002));
#276056=CARTESIAN_POINT('Ctrl Pts',(-9.03200107200006,11.6,-7.10739465100002));
#276057=CARTESIAN_POINT('Ctrl Pts',(-9.02827662900006,15.2,-7.10658278400001));
#276058=CARTESIAN_POINT('Ctrl Pts',(-9.02827662900006,11.6,-7.10658278400001));
#276059=CARTESIAN_POINT('Ctrl Pts',(-9.02455710700006,15.2,-7.10576903500002));
#276060=CARTESIAN_POINT('Ctrl Pts',(-9.02455710700006,11.6,-7.10576903500002));
#276061=CARTESIAN_POINT('Ctrl Pts',(-9.02084250600005,15.2,-7.10495340800002));
#276062=CARTESIAN_POINT('Ctrl Pts',(-9.02084250600005,11.6,-7.10495340800002));
#276063=CARTESIAN_POINT('Ctrl Pts',(-9.01713282900005,15.2,-7.10413590400002));
#276064=CARTESIAN_POINT('Ctrl Pts',(-9.01713282900005,11.6,-7.10413590400002));
#276065=CARTESIAN_POINT('Ctrl Pts',(-9.01342808000006,15.2,-7.10331652800001));
#276066=CARTESIAN_POINT('Ctrl Pts',(-9.01342808000006,11.6,-7.10331652800001));
#276067=CARTESIAN_POINT('Ctrl Pts',(-9.00972826500006,15.2,-7.10249528800002));
#276068=CARTESIAN_POINT('Ctrl Pts',(-9.00972826500006,11.6,-7.10249528800002));
#276069=CARTESIAN_POINT('Ctrl Pts',(-9.00603338900006,15.2,-7.10167218900001));
#276070=CARTESIAN_POINT('Ctrl Pts',(-9.00603338900006,11.6,-7.10167218900001));
#276071=CARTESIAN_POINT('Ctrl Pts',(-9.00234345900006,15.2,-7.10084724000002));
#276072=CARTESIAN_POINT('Ctrl Pts',(-9.00234345900006,11.6,-7.10084724000002));
#276073=CARTESIAN_POINT('Ctrl Pts',(-8.99865848200006,15.2,-7.10002045100002));
#276074=CARTESIAN_POINT('Ctrl Pts',(-8.99865848200006,11.6,-7.10002045100002));
#276075=CARTESIAN_POINT('Ctrl Pts',(-8.99497846500006,15.2,-7.09919182900002));
#276076=CARTESIAN_POINT('Ctrl Pts',(-8.99497846500006,11.6,-7.09919182900002));
#276077=CARTESIAN_POINT('Ctrl Pts',(-8.99130341600006,15.2,-7.09836138400001));
#276078=CARTESIAN_POINT('Ctrl Pts',(-8.99130341600006,11.6,-7.09836138400001));
#276079=CARTESIAN_POINT('Ctrl Pts',(-8.98763333900006,15.2,-7.09752912300001));
#276080=CARTESIAN_POINT('Ctrl Pts',(-8.98763333900006,11.6,-7.09752912300001));
#276081=CARTESIAN_POINT('Ctrl Pts',(-8.98396824000006,15.2,-7.09669505000001));
#276082=CARTESIAN_POINT('Ctrl Pts',(-8.98396824000006,11.6,-7.09669505000001));
#276083=CARTESIAN_POINT('Ctrl Pts',(-8.98030812400006,15.2,-7.09585917500001));
#276084=CARTESIAN_POINT('Ctrl Pts',(-8.98030812400006,11.6,-7.09585917500001));
#276085=CARTESIAN_POINT('Ctrl Pts',(-8.97665299700006,15.2,-7.09502150300001));
#276086=CARTESIAN_POINT('Ctrl Pts',(-8.97665299700006,11.6,-7.09502150300001));
#276087=CARTESIAN_POINT('Ctrl Pts',(-8.97300286400006,15.2,-7.09418203900002));
#276088=CARTESIAN_POINT('Ctrl Pts',(-8.97300286400006,11.6,-7.09418203900002));
#276089=CARTESIAN_POINT('Ctrl Pts',(-8.96935772900006,15.2,-7.09334079100002));
#276090=CARTESIAN_POINT('Ctrl Pts',(-8.96935772900006,11.6,-7.09334079100002));
#276091=CARTESIAN_POINT('Ctrl Pts',(-8.96571759800005,15.2,-7.09249776700001));
#276092=CARTESIAN_POINT('Ctrl Pts',(-8.96571759800005,11.6,-7.09249776700001));
#276093=CARTESIAN_POINT('Ctrl Pts',(-8.96208247800006,15.2,-7.09165297200002));
#276094=CARTESIAN_POINT('Ctrl Pts',(-8.96208247800006,11.6,-7.09165297200002));
#276095=CARTESIAN_POINT('Ctrl Pts',(-8.95845237400006,15.2,-7.09080641500002));
#276096=CARTESIAN_POINT('Ctrl Pts',(-8.95845237400006,11.6,-7.09080641500002));
#276097=CARTESIAN_POINT('Ctrl Pts',(-8.95482729200006,15.2,-7.08995810200002));
#276098=CARTESIAN_POINT('Ctrl Pts',(-8.95482729200006,11.6,-7.08995810200002));
#276099=CARTESIAN_POINT('Ctrl Pts',(-8.95120723800006,15.2,-7.08910804300002));
#276100=CARTESIAN_POINT('Ctrl Pts',(-8.95120723800006,11.6,-7.08910804300002));
#276101=CARTESIAN_POINT('Ctrl Pts',(-8.94759221900006,15.2,-7.08825624300002));
#276102=CARTESIAN_POINT('Ctrl Pts',(-8.94759221900006,11.6,-7.08825624300002));
#276103=CARTESIAN_POINT('Ctrl Pts',(-8.94398223900006,15.2,-7.08740271100002));
#276104=CARTESIAN_POINT('Ctrl Pts',(-8.94398223900006,11.6,-7.08740271100002));
#276105=CARTESIAN_POINT('Ctrl Pts',(-8.94037730400006,15.2,-7.08654745200001));
#276106=CARTESIAN_POINT('Ctrl Pts',(-8.94037730400006,11.6,-7.08654745200001));
#276107=CARTESIAN_POINT('Ctrl Pts',(-8.93677742100006,15.2,-7.08569047400001));
#276108=CARTESIAN_POINT('Ctrl Pts',(-8.93677742100006,11.6,-7.08569047400001));
#276109=CARTESIAN_POINT('Ctrl Pts',(-8.93318259400005,15.2,-7.08483178600002));
#276110=CARTESIAN_POINT('Ctrl Pts',(-8.93318259400005,11.6,-7.08483178600002));
#276111=CARTESIAN_POINT('Ctrl Pts',(-8.92959282900006,15.2,-7.08397139300001));
#276112=CARTESIAN_POINT('Ctrl Pts',(-8.92959282900006,11.6,-7.08397139300001));
#276113=CARTESIAN_POINT('Ctrl Pts',(-8.92600813200006,15.2,-7.08310930200001));
#276114=CARTESIAN_POINT('Ctrl Pts',(-8.92600813200006,11.6,-7.08310930200001));
#276115=CARTESIAN_POINT('Ctrl Pts',(-8.92242850800006,15.2,-7.08224552100001));
#276116=CARTESIAN_POINT('Ctrl Pts',(-8.92242850800006,11.6,-7.08224552100001));
#276117=CARTESIAN_POINT('Ctrl Pts',(-8.91885396500006,15.2,-7.08138005800001));
#276118=CARTESIAN_POINT('Ctrl Pts',(-8.91885396500006,11.6,-7.08138005800001));
#276119=CARTESIAN_POINT('Ctrl Pts',(-8.91528450600006,15.2,-7.08051292100001));
#276120=CARTESIAN_POINT('Ctrl Pts',(-8.91528450600006,11.6,-7.08051292100001));
#276121=CARTESIAN_POINT('Ctrl Pts',(-8.91172013800006,15.2,-7.07964411500001));
#276122=CARTESIAN_POINT('Ctrl Pts',(-8.91172013800006,11.6,-7.07964411500001));
#276123=CARTESIAN_POINT('Ctrl Pts',(-8.90816086700006,15.2,-7.07877364900002));
#276124=CARTESIAN_POINT('Ctrl Pts',(-8.90816086700006,11.6,-7.07877364900002));
#276125=CARTESIAN_POINT('Ctrl Pts',(-8.90460669800006,15.2,-7.07790152900002));
#276126=CARTESIAN_POINT('Ctrl Pts',(-8.90460669800006,11.6,-7.07790152900002));
#276127=CARTESIAN_POINT('Ctrl Pts',(-8.90105763800005,15.2,-7.07702776600001));
#276128=CARTESIAN_POINT('Ctrl Pts',(-8.90105763800005,11.6,-7.07702776600001));
#276129=CARTESIAN_POINT('Ctrl Pts',(-8.89751369200006,15.2,-7.07615236300001));
#276130=CARTESIAN_POINT('Ctrl Pts',(-8.89751369200006,11.6,-7.07615236300001));
#276131=CARTESIAN_POINT('Ctrl Pts',(-8.89397486600006,15.2,-7.07527533000002));
#276132=CARTESIAN_POINT('Ctrl Pts',(-8.89397486600006,11.6,-7.07527533000002));
#276133=CARTESIAN_POINT('Ctrl Pts',(-8.89044116400006,15.2,-7.07439667400001));
#276134=CARTESIAN_POINT('Ctrl Pts',(-8.89044116400006,11.6,-7.07439667400001));
#276135=CARTESIAN_POINT('Ctrl Pts',(-8.88691259400006,15.2,-7.07351640200002));
#276136=CARTESIAN_POINT('Ctrl Pts',(-8.88691259400006,11.6,-7.07351640200002));
#276137=CARTESIAN_POINT('Ctrl Pts',(-8.88338916200006,15.2,-7.07263452100002));
#276138=CARTESIAN_POINT('Ctrl Pts',(-8.88338916200006,11.6,-7.07263452100002));
#276139=CARTESIAN_POINT('Ctrl Pts',(-8.87987087300005,15.2,-7.07175104100001));
#276140=CARTESIAN_POINT('Ctrl Pts',(-8.87987087300005,11.6,-7.07175104100001));
#276141=CARTESIAN_POINT('Ctrl Pts',(-8.87635773200006,15.2,-7.07086596600002));
#276142=CARTESIAN_POINT('Ctrl Pts',(-8.87635773200006,11.6,-7.07086596600002));
#276143=CARTESIAN_POINT('Ctrl Pts',(-8.87284974500006,15.2,-7.06997930700001));
#276144=CARTESIAN_POINT('Ctrl Pts',(-8.87284974500006,11.6,-7.06997930700001));
#276145=CARTESIAN_POINT('Ctrl Pts',(-8.86934691800005,15.2,-7.06909107000002));
#276146=CARTESIAN_POINT('Ctrl Pts',(-8.86934691800005,11.6,-7.06909107000002));
#276147=CARTESIAN_POINT('Ctrl Pts',(-8.86584925900006,15.2,-7.06820126200002));
#276148=CARTESIAN_POINT('Ctrl Pts',(-8.86584925900006,11.6,-7.06820126200002));
#276149=CARTESIAN_POINT('Ctrl Pts',(-8.86235677000006,15.2,-7.06730989100001));
#276150=CARTESIAN_POINT('Ctrl Pts',(-8.86235677000006,11.6,-7.06730989100001));
#276151=CARTESIAN_POINT('Ctrl Pts',(-8.85886945900005,15.2,-7.06641696400002));
#276152=CARTESIAN_POINT('Ctrl Pts',(-8.85886945900005,11.6,-7.06641696400002));
#276153=CARTESIAN_POINT('Ctrl Pts',(-8.85538733200006,15.2,-7.06552249100002));
#276154=CARTESIAN_POINT('Ctrl Pts',(-8.85538733200006,11.6,-7.06552249100002));
#276155=CARTESIAN_POINT('Ctrl Pts',(-8.85191039400006,15.2,-7.06462647700001));
#276156=CARTESIAN_POINT('Ctrl Pts',(-8.85191039400006,11.6,-7.06462647700001));
#276157=CARTESIAN_POINT('Ctrl Pts',(-8.84843865100006,15.2,-7.06372893100002));
#276158=CARTESIAN_POINT('Ctrl Pts',(-8.84843865100006,11.6,-7.06372893100002));
#276159=CARTESIAN_POINT('Ctrl Pts',(-8.84497210900006,15.2,-7.06282986200002));
#276160=CARTESIAN_POINT('Ctrl Pts',(-8.84497210900006,11.6,-7.06282986200002));
#276161=CARTESIAN_POINT('Ctrl Pts',(-8.84151077400006,15.2,-7.06192927400001));
#276162=CARTESIAN_POINT('Ctrl Pts',(-8.84151077400006,11.6,-7.06192927400001));
#276163=CARTESIAN_POINT('Ctrl Pts',(-8.83805465100006,15.2,-7.06102717900002));
#276164=CARTESIAN_POINT('Ctrl Pts',(-8.83805465100006,11.6,-7.06102717900002));
#276165=CARTESIAN_POINT('Ctrl Pts',(-8.83460374700006,15.2,-7.06012358200002));
#276166=CARTESIAN_POINT('Ctrl Pts',(-8.83460374700006,11.6,-7.06012358200002));
#276167=CARTESIAN_POINT('Ctrl Pts',(-8.83115806700006,15.2,-7.05921849000001));
#276168=CARTESIAN_POINT('Ctrl Pts',(-8.83115806700006,11.6,-7.05921849000001));
#276169=CARTESIAN_POINT('Ctrl Pts',(-8.82771761700005,15.2,-7.05831191300001));
#276170=CARTESIAN_POINT('Ctrl Pts',(-8.82771761700005,11.6,-7.05831191300001));
#276171=CARTESIAN_POINT('Ctrl Pts',(-8.82428240300005,15.2,-7.05740385900001));
#276172=CARTESIAN_POINT('Ctrl Pts',(-8.82428240300005,11.6,-7.05740385900001));
#276173=CARTESIAN_POINT('Ctrl Pts',(-8.82085243100006,15.2,-7.05649433500002));
#276174=CARTESIAN_POINT('Ctrl Pts',(-8.82085243100006,11.6,-7.05649433500002));
#276175=CARTESIAN_POINT('Ctrl Pts',(-8.81742770700006,15.2,-7.05558334800001));
#276176=CARTESIAN_POINT('Ctrl Pts',(-8.81742770700006,11.6,-7.05558334800001));
#276177=CARTESIAN_POINT('Ctrl Pts',(-8.81400823600006,15.2,-7.05467090600001));
#276178=CARTESIAN_POINT('Ctrl Pts',(-8.81400823600006,11.6,-7.05467090600001));
#276179=CARTESIAN_POINT('Ctrl Pts',(-8.81059402400006,15.2,-7.05375701900002));
#276180=CARTESIAN_POINT('Ctrl Pts',(-8.81059402400006,11.6,-7.05375701900002));
#276181=CARTESIAN_POINT('Ctrl Pts',(-8.80718507800006,15.2,-7.05284169300001));
#276182=CARTESIAN_POINT('Ctrl Pts',(-8.80718507800006,11.6,-7.05284169300001));
#276183=CARTESIAN_POINT('Ctrl Pts',(-8.80378140200006,15.2,-7.05192493600002));
#276184=CARTESIAN_POINT('Ctrl Pts',(-8.80378140200006,11.6,-7.05192493600002));
#276185=CARTESIAN_POINT('Ctrl Pts',(-8.80038300400006,15.2,-7.05100675600002));
#276186=CARTESIAN_POINT('Ctrl Pts',(-8.80038300400006,11.6,-7.05100675600002));
#276187=CARTESIAN_POINT('Ctrl Pts',(-8.79698988900006,15.2,-7.05008716200001));
#276188=CARTESIAN_POINT('Ctrl Pts',(-8.79698988900006,11.6,-7.05008716200001));
#276189=CARTESIAN_POINT('Ctrl Pts',(-8.79360206200005,15.2,-7.04916616100002));
#276190=CARTESIAN_POINT('Ctrl Pts',(-8.79360206200005,11.6,-7.04916616100002));
#276191=CARTESIAN_POINT('Ctrl Pts',(-8.79021953000005,15.2,-7.04824376100002));
#276192=CARTESIAN_POINT('Ctrl Pts',(-8.79021953000005,11.6,-7.04824376100002));
#276193=CARTESIAN_POINT('Ctrl Pts',(-8.78684229800006,15.2,-7.04731997100002));
#276194=CARTESIAN_POINT('Ctrl Pts',(-8.78684229800006,11.6,-7.04731997100002));
#276195=CARTESIAN_POINT('Ctrl Pts',(-8.78347037400006,15.2,-7.04639479800001));
#276196=CARTESIAN_POINT('Ctrl Pts',(-8.78347037400006,11.6,-7.04639479800001));
#276197=CARTESIAN_POINT('Ctrl Pts',(-8.78010376100006,15.2,-7.04546825000002));
#276198=CARTESIAN_POINT('Ctrl Pts',(-8.78010376100006,11.6,-7.04546825000002));
#276199=CARTESIAN_POINT('Ctrl Pts',(-8.77674246700006,15.2,-7.04454033500002));
#276200=CARTESIAN_POINT('Ctrl Pts',(-8.77674246700006,11.6,-7.04454033500002));
#276201=CARTESIAN_POINT('Ctrl Pts',(-8.77338649600006,15.2,-7.04361106300002));
#276202=CARTESIAN_POINT('Ctrl Pts',(-8.77338649600006,11.6,-7.04361106300002));
#276203=CARTESIAN_POINT('Ctrl Pts',(-8.77003585700006,15.2,-7.04268044000001));
#276204=CARTESIAN_POINT('Ctrl Pts',(-8.77003585700006,11.6,-7.04268044000001));
#276205=CARTESIAN_POINT('Ctrl Pts',(-8.76669055200006,15.2,-7.04174847400001));
#276206=CARTESIAN_POINT('Ctrl Pts',(-8.76669055200006,11.6,-7.04174847400001));
#276207=CARTESIAN_POINT('Ctrl Pts',(-8.76335059000006,15.2,-7.04081517500001));
#276208=CARTESIAN_POINT('Ctrl Pts',(-8.76335059000006,11.6,-7.04081517500001));
#276209=CARTESIAN_POINT('Ctrl Pts',(-8.76001597600006,15.2,-7.03988055000002));
#276210=CARTESIAN_POINT('Ctrl Pts',(-8.76001597600006,11.6,-7.03988055000002));
#276211=CARTESIAN_POINT('Ctrl Pts',(-8.75668671600006,15.2,-7.03894460800001));
#276212=CARTESIAN_POINT('Ctrl Pts',(-8.75668671600006,11.6,-7.03894460800001));
#276213=CARTESIAN_POINT('Ctrl Pts',(-8.75336281400006,15.2,-7.03800735500002));
#276214=CARTESIAN_POINT('Ctrl Pts',(-8.75336281400006,11.6,-7.03800735500002));
#276215=CARTESIAN_POINT('Ctrl Pts',(-8.75004427900006,15.2,-7.03706880200002));
#276216=CARTESIAN_POINT('Ctrl Pts',(-8.75004427900006,11.6,-7.03706880200002));
#276217=CARTESIAN_POINT('Ctrl Pts',(-8.74673111600006,15.2,-7.03612895700001));
#276218=CARTESIAN_POINT('Ctrl Pts',(-8.74673111600006,11.6,-7.03612895700001));
#276219=CARTESIAN_POINT('Ctrl Pts',(-8.74342333000006,15.2,-7.03518782500002));
#276220=CARTESIAN_POINT('Ctrl Pts',(-8.74342333000006,11.6,-7.03518782500002));
#276221=CARTESIAN_POINT('Ctrl Pts',(-8.74012092800006,15.2,-7.03424541800001));
#276222=CARTESIAN_POINT('Ctrl Pts',(-8.74012092800006,11.6,-7.03424541800001));
#276223=CARTESIAN_POINT('Ctrl Pts',(-8.73682391500006,15.2,-7.03330174300002));
#276224=CARTESIAN_POINT('Ctrl Pts',(-8.73682391500006,11.6,-7.03330174300002));
#276225=CARTESIAN_POINT('Ctrl Pts',(-8.73353229800006,15.2,-7.03235680900002));
#276226=CARTESIAN_POINT('Ctrl Pts',(-8.73353229800006,11.6,-7.03235680900002));
#276227=CARTESIAN_POINT('Ctrl Pts',(-8.73024608200006,15.2,-7.03141062300002));
#276228=CARTESIAN_POINT('Ctrl Pts',(-8.73024608200006,11.6,-7.03141062300002));
#276229=CARTESIAN_POINT('Ctrl Pts',(-8.72696527300005,15.2,-7.03046319400002));
#276230=CARTESIAN_POINT('Ctrl Pts',(-8.72696527300005,11.6,-7.03046319400002));
#276231=CARTESIAN_POINT('Ctrl Pts',(-8.72368987800006,15.2,-7.02951453100002));
#276232=CARTESIAN_POINT('Ctrl Pts',(-8.72368987800006,11.6,-7.02951453100002));
#276233=CARTESIAN_POINT('Ctrl Pts',(-8.72041990300006,15.2,-7.02856464100002));
#276234=CARTESIAN_POINT('Ctrl Pts',(-8.72041990300006,11.6,-7.02856464100002));
#276235=CARTESIAN_POINT('Ctrl Pts',(-8.71715535200006,15.2,-7.02761353400001));
#276236=CARTESIAN_POINT('Ctrl Pts',(-8.71715535200006,11.6,-7.02761353400001));
#276237=CARTESIAN_POINT('Ctrl Pts',(-8.71389623400006,15.2,-7.02666121800001));
#276238=CARTESIAN_POINT('Ctrl Pts',(-8.71389623400006,11.6,-7.02666121800001));
#276239=CARTESIAN_POINT('Ctrl Pts',(-8.71064255200006,15.2,-7.02570770100002));
#276240=CARTESIAN_POINT('Ctrl Pts',(-8.71064255200006,11.6,-7.02570770100002));
#276241=CARTESIAN_POINT('Ctrl Pts',(-8.70739431400006,15.2,-7.02475299200002));
#276242=CARTESIAN_POINT('Ctrl Pts',(-8.70739431400006,11.6,-7.02475299200002));
#276243=CARTESIAN_POINT('Ctrl Pts',(-8.70415152500006,15.2,-7.02379710000002));
#276244=CARTESIAN_POINT('Ctrl Pts',(-8.70415152500006,11.6,-7.02379710000002));
#276245=CARTESIAN_POINT('Ctrl Pts',(-8.70091419100006,15.2,-7.02284003200001));
#276246=CARTESIAN_POINT('Ctrl Pts',(-8.70091419100006,11.6,-7.02284003200001));
#276247=CARTESIAN_POINT('Ctrl Pts',(-8.69768231900006,15.2,-7.02188179800002));
#276248=CARTESIAN_POINT('Ctrl Pts',(-8.69768231900006,11.6,-7.02188179800002));
#276249=CARTESIAN_POINT('Ctrl Pts',(-8.69445591400006,15.2,-7.02092240600001));
#276250=CARTESIAN_POINT('Ctrl Pts',(-8.69445591400006,11.6,-7.02092240600001));
#276251=CARTESIAN_POINT('Ctrl Pts',(-8.69123498300005,15.2,-7.01996186500002));
#276252=CARTESIAN_POINT('Ctrl Pts',(-8.69123498300005,11.6,-7.01996186500002));
#276253=CARTESIAN_POINT('Ctrl Pts',(-8.68801953200006,15.2,-7.01900018400002));
#276254=CARTESIAN_POINT('Ctrl Pts',(-8.68801953200006,11.6,-7.01900018400002));
#276255=CARTESIAN_POINT('Ctrl Pts',(-8.68480956600006,15.2,-7.01803737000001));
#276256=CARTESIAN_POINT('Ctrl Pts',(-8.68480956600006,11.6,-7.01803737000001));
#276257=CARTESIAN_POINT('Ctrl Pts',(-8.68160509100005,15.2,-7.01707343300002));
#276258=CARTESIAN_POINT('Ctrl Pts',(-8.68160509100005,11.6,-7.01707343300002));
#276259=CARTESIAN_POINT('Ctrl Pts',(-8.67840611400006,15.2,-7.01610838100001));
#276260=CARTESIAN_POINT('Ctrl Pts',(-8.67840611400006,11.6,-7.01610838100001));
#276261=CARTESIAN_POINT('Ctrl Pts',(-8.67521264100005,15.2,-7.01514222400001));
#276262=CARTESIAN_POINT('Ctrl Pts',(-8.67521264100005,11.6,-7.01514222400001));
#276263=CARTESIAN_POINT('Ctrl Pts',(-8.67202467700006,15.2,-7.01417496900002));
#276264=CARTESIAN_POINT('Ctrl Pts',(-8.67202467700006,11.6,-7.01417496900002));
#276265=CARTESIAN_POINT('Ctrl Pts',(-8.66884222900006,15.2,-7.01320662700001));
#276266=CARTESIAN_POINT('Ctrl Pts',(-8.66884222900006,11.6,-7.01320662700001));
#276267=CARTESIAN_POINT('Ctrl Pts',(-8.66566530400006,15.2,-7.01223720400002));
#276268=CARTESIAN_POINT('Ctrl Pts',(-8.66566530400006,11.6,-7.01223720400002));
#276269=CARTESIAN_POINT('Ctrl Pts',(-8.66249390600006,15.2,-7.01126671100001));
#276270=CARTESIAN_POINT('Ctrl Pts',(-8.66249390600006,11.6,-7.01126671100001));
#276271=CARTESIAN_POINT('Ctrl Pts',(-8.65932804200006,15.2,-7.01029515700001));
#276272=CARTESIAN_POINT('Ctrl Pts',(-8.65932804200006,11.6,-7.01029515700001));
#276273=CARTESIAN_POINT('Ctrl Pts',(-8.65616771800006,15.2,-7.00932254900002));
#276274=CARTESIAN_POINT('Ctrl Pts',(-8.65616771800006,11.6,-7.00932254900002));
#276275=CARTESIAN_POINT('Ctrl Pts',(-8.65301294000006,15.2,-7.00834889700002));
#276276=CARTESIAN_POINT('Ctrl Pts',(-8.65301294000006,11.6,-7.00834889700002));
#276277=CARTESIAN_POINT('Ctrl Pts',(-8.64986371500006,15.2,-7.00737421000002));
#276278=CARTESIAN_POINT('Ctrl Pts',(-8.64986371500006,11.6,-7.00737421000002));
#276279=CARTESIAN_POINT('Ctrl Pts',(-8.64672004800006,15.2,-7.00639849700002));
#276280=CARTESIAN_POINT('Ctrl Pts',(-8.64672004800006,11.6,-7.00639849700002));
#276281=CARTESIAN_POINT('Ctrl Pts',(-8.64358194600005,15.2,-7.00542176600001));
#276282=CARTESIAN_POINT('Ctrl Pts',(-8.64358194600005,11.6,-7.00542176600001));
#276283=CARTESIAN_POINT('Ctrl Pts',(-8.64044941400006,15.2,-7.00444402600001));
#276284=CARTESIAN_POINT('Ctrl Pts',(-8.64044941400006,11.6,-7.00444402600001));
#276285=CARTESIAN_POINT('Ctrl Pts',(-8.63732245800006,15.2,-7.00346528800001));
#276286=CARTESIAN_POINT('Ctrl Pts',(-8.63732245800006,11.6,-7.00346528800001));
#276287=CARTESIAN_POINT('Ctrl Pts',(-8.63420108600006,15.2,-7.00248556000002));
#276288=CARTESIAN_POINT('Ctrl Pts',(-8.63420108600006,11.6,-7.00248556000002));
#276289=CARTESIAN_POINT('Ctrl Pts',(-8.63108530200006,15.2,-7.00150485000002));
#276290=CARTESIAN_POINT('Ctrl Pts',(-8.63108530200006,11.6,-7.00150485000002));
#276291=CARTESIAN_POINT('Ctrl Pts',(-8.62797511400006,15.2,-7.00052316700001));
#276292=CARTESIAN_POINT('Ctrl Pts',(-8.62797511400006,11.6,-7.00052316700001));
#276293=CARTESIAN_POINT('Ctrl Pts',(-8.62487052700006,15.2,-6.99954052200002));
#276294=CARTESIAN_POINT('Ctrl Pts',(-8.62487052700006,11.6,-6.99954052200002));
#276295=CARTESIAN_POINT('Ctrl Pts',(-8.62177154800005,15.2,-6.99855692200002));
#276296=CARTESIAN_POINT('Ctrl Pts',(-8.62177154800005,11.6,-6.99855692200002));
#276297=CARTESIAN_POINT('Ctrl Pts',(-8.61867818200006,15.2,-6.99757237900001));
#276298=CARTESIAN_POINT('Ctrl Pts',(-8.61867818200006,11.6,-6.99757237900001));
#276299=CARTESIAN_POINT('Ctrl Pts',(-8.61559043500005,15.2,-6.99658689800001));
#276300=CARTESIAN_POINT('Ctrl Pts',(-8.61559043500005,11.6,-6.99658689800001));
#276301=CARTESIAN_POINT('Ctrl Pts',(-8.61250831400006,15.2,-6.99560049200001));
#276302=CARTESIAN_POINT('Ctrl Pts',(-8.61250831400006,11.6,-6.99560049200001));
#276303=CARTESIAN_POINT('Ctrl Pts',(-8.60943182500005,15.2,-6.99461316800001));
#276304=CARTESIAN_POINT('Ctrl Pts',(-8.60943182500005,11.6,-6.99461316800001));
#276305=CARTESIAN_POINT('Ctrl Pts',(-8.60636097400005,15.2,-6.99362493600002));
#276306=CARTESIAN_POINT('Ctrl Pts',(-8.60636097400005,11.6,-6.99362493600002));
#276307=CARTESIAN_POINT('Ctrl Pts',(-8.60329576800006,15.2,-6.99263580600002));
#276308=CARTESIAN_POINT('Ctrl Pts',(-8.60329576800006,11.6,-6.99263580600002));
#276309=CARTESIAN_POINT('Ctrl Pts',(-8.60023621200006,15.2,-6.99164578600002));
#276310=CARTESIAN_POINT('Ctrl Pts',(-8.60023621200006,11.6,-6.99164578600002));
#276311=CARTESIAN_POINT('Ctrl Pts',(-8.59718231200005,15.2,-6.99065488500001));
#276312=CARTESIAN_POINT('Ctrl Pts',(-8.59718231200005,11.6,-6.99065488500001));
#276313=CARTESIAN_POINT('Ctrl Pts',(-8.59413407600006,15.2,-6.98966311400002));
#276314=CARTESIAN_POINT('Ctrl Pts',(-8.59413407600006,11.6,-6.98966311400002));
#276315=CARTESIAN_POINT('Ctrl Pts',(-8.59109150900006,15.2,-6.98867048200002));
#276316=CARTESIAN_POINT('Ctrl Pts',(-8.59109150900006,11.6,-6.98867048200002));
#276317=CARTESIAN_POINT('Ctrl Pts',(-8.58805461700006,15.2,-6.98767699600002));
#276318=CARTESIAN_POINT('Ctrl Pts',(-8.58805461700006,11.6,-6.98767699600002));
#276319=CARTESIAN_POINT('Ctrl Pts',(-8.58502340600005,15.2,-6.98668266800002));
#276320=CARTESIAN_POINT('Ctrl Pts',(-8.58502340600005,11.6,-6.98668266800002));
#276321=CARTESIAN_POINT('Ctrl Pts',(-8.58199788300006,15.2,-6.98568750700002));
#276322=CARTESIAN_POINT('Ctrl Pts',(-8.58199788300006,11.6,-6.98568750700002));
#276323=CARTESIAN_POINT('Ctrl Pts',(-8.57897805400006,15.2,-6.98469152300002));
#276324=CARTESIAN_POINT('Ctrl Pts',(-8.57897805400006,11.6,-6.98469152300002));
#276325=CARTESIAN_POINT('Ctrl Pts',(-8.57596392500006,15.2,-6.98369472200002));
#276326=CARTESIAN_POINT('Ctrl Pts',(-8.57596392500006,11.6,-6.98369472200002));
#276327=CARTESIAN_POINT('Ctrl Pts',(-8.57295550200006,15.2,-6.98269711800001));
#276328=CARTESIAN_POINT('Ctrl Pts',(-8.57295550200006,11.6,-6.98269711800001));
#276329=CARTESIAN_POINT('Ctrl Pts',(-8.56995279100006,15.2,-6.98169871900002));
#276330=CARTESIAN_POINT('Ctrl Pts',(-8.56995279100006,11.6,-6.98169871900002));
#276331=CARTESIAN_POINT('Ctrl Pts',(-8.56695580000006,15.2,-6.98069953300001));
#276332=CARTESIAN_POINT('Ctrl Pts',(-8.56695580000006,11.6,-6.98069953300001));
#276333=CARTESIAN_POINT('Ctrl Pts',(-8.56396453400006,15.2,-6.97969957100002));
#276334=CARTESIAN_POINT('Ctrl Pts',(-8.56396453400006,11.6,-6.97969957100002));
#276335=CARTESIAN_POINT('Ctrl Pts',(-8.56097900000006,15.2,-6.97869884300002));
#276336=CARTESIAN_POINT('Ctrl Pts',(-8.56097900000006,11.6,-6.97869884300002));
#276337=CARTESIAN_POINT('Ctrl Pts',(-8.55799920200005,15.2,-6.97769735700002));
#276338=CARTESIAN_POINT('Ctrl Pts',(-8.55799920200005,11.6,-6.97769735700002));
#276339=CARTESIAN_POINT('Ctrl Pts',(-8.55502514900006,15.2,-6.97669512400001));
#276340=CARTESIAN_POINT('Ctrl Pts',(-8.55502514900006,11.6,-6.97669512400001));
#276341=CARTESIAN_POINT('Ctrl Pts',(-8.55205684500006,15.2,-6.97569215300001));
#276342=CARTESIAN_POINT('Ctrl Pts',(-8.55205684500006,11.6,-6.97569215300001));
#276343=CARTESIAN_POINT('Ctrl Pts',(-8.54909429800006,15.2,-6.97468845400002));
#276344=CARTESIAN_POINT('Ctrl Pts',(-8.54909429800006,11.6,-6.97468845400002));
#276345=CARTESIAN_POINT('Ctrl Pts',(-8.54613751300005,15.2,-6.97368403700001));
#276346=CARTESIAN_POINT('Ctrl Pts',(-8.54613751300005,11.6,-6.97368403700001));
#276347=CARTESIAN_POINT('Ctrl Pts',(-8.54318649800006,15.2,-6.97267891200001));
#276348=CARTESIAN_POINT('Ctrl Pts',(-8.54318649800006,11.6,-6.97267891200001));
#276349=CARTESIAN_POINT('Ctrl Pts',(-8.54024125700005,15.2,-6.97167308800001));
#276350=CARTESIAN_POINT('Ctrl Pts',(-8.54024125700005,11.6,-6.97167308800001));
#276351=CARTESIAN_POINT('Ctrl Pts',(-8.53730179800005,15.2,-6.97066657500002));
#276352=CARTESIAN_POINT('Ctrl Pts',(-8.53730179800005,11.6,-6.97066657500002));
#276353=CARTESIAN_POINT('Ctrl Pts',(-8.53436812700006,15.2,-6.96965938200002));
#276354=CARTESIAN_POINT('Ctrl Pts',(-8.53436812700006,11.6,-6.96965938200002));
#276355=CARTESIAN_POINT('Ctrl Pts',(-8.53144025100006,15.2,-6.96865152100001));
#276356=CARTESIAN_POINT('Ctrl Pts',(-8.53144025100006,11.6,-6.96865152100001));
#276357=CARTESIAN_POINT('Ctrl Pts',(-8.52851817400006,15.2,-6.96764300000002));
#276358=CARTESIAN_POINT('Ctrl Pts',(-8.52851817400006,11.6,-6.96764300000002));
#276359=CARTESIAN_POINT('Ctrl Pts',(-8.52560190400006,15.2,-6.96663382900002));
#276360=CARTESIAN_POINT('Ctrl Pts',(-8.52560190400006,11.6,-6.96663382900002));
#276361=CARTESIAN_POINT('Ctrl Pts',(-8.52269144900006,15.2,-6.96562402000002));
#276362=CARTESIAN_POINT('Ctrl Pts',(-8.52269144900006,11.6,-6.96562402000002));
#276363=CARTESIAN_POINT('Ctrl Pts',(-8.51978681100006,15.2,-6.96461358000001));
#276364=CARTESIAN_POINT('Ctrl Pts',(-8.51978681100006,11.6,-6.96461358000001));
#276365=CARTESIAN_POINT('Ctrl Pts',(-8.51688800000005,15.2,-6.96360252200002));
#276366=CARTESIAN_POINT('Ctrl Pts',(-8.51688800000005,11.6,-6.96360252200002));
#276367=CARTESIAN_POINT('Ctrl Pts',(-8.51399502100006,15.2,-6.96259085300002));
#276368=CARTESIAN_POINT('Ctrl Pts',(-8.51399502100006,11.6,-6.96259085300002));
#276369=CARTESIAN_POINT('Ctrl Pts',(-8.51110788000006,15.2,-6.96157858500002));
#276370=CARTESIAN_POINT('Ctrl Pts',(-8.51110788000006,11.6,-6.96157858500002));
#276371=CARTESIAN_POINT('Ctrl Pts',(-8.50822658400006,15.2,-6.96056572800002));
#276372=CARTESIAN_POINT('Ctrl Pts',(-8.50822658400006,11.6,-6.96056572800002));
#276373=CARTESIAN_POINT('Ctrl Pts',(-8.50535113900006,15.2,-6.95955229100001));
#276374=CARTESIAN_POINT('Ctrl Pts',(-8.50535113900006,11.6,-6.95955229100001));
#276375=CARTESIAN_POINT('Ctrl Pts',(-8.50248155100006,15.2,-6.95853828600002));
#276376=CARTESIAN_POINT('Ctrl Pts',(-8.50248155100006,11.6,-6.95853828600002));
#276377=CARTESIAN_POINT('Ctrl Pts',(-8.49961782900006,15.2,-6.95752372000002));
#276378=CARTESIAN_POINT('Ctrl Pts',(-8.49961782900006,11.6,-6.95752372000002));
#276379=CARTESIAN_POINT('Ctrl Pts',(-8.49675997600006,15.2,-6.95650860700002));
#276380=CARTESIAN_POINT('Ctrl Pts',(-8.49675997600006,11.6,-6.95650860700002));
#276381=CARTESIAN_POINT('Ctrl Pts',(-8.49390800000006,15.2,-6.95549295400002));
#276382=CARTESIAN_POINT('Ctrl Pts',(-8.49390800000006,11.6,-6.95549295400002));
#276383=CARTESIAN_POINT('Ctrl Pts',(-8.49106190600006,15.2,-6.95447677400002));
#276384=CARTESIAN_POINT('Ctrl Pts',(-8.49106190600006,11.6,-6.95447677400002));
#276385=CARTESIAN_POINT('Ctrl Pts',(-8.48822170400006,15.2,-6.95346007500002));
#276386=CARTESIAN_POINT('Ctrl Pts',(-8.48822170400006,11.6,-6.95346007500002));
#276387=CARTESIAN_POINT('Ctrl Pts',(-8.48538739600006,15.2,-6.95244286800002));
#276388=CARTESIAN_POINT('Ctrl Pts',(-8.48538739600006,11.6,-6.95244286800002));
#276389=CARTESIAN_POINT('Ctrl Pts',(-8.48255899100005,15.2,-6.95142516400002));
#276390=CARTESIAN_POINT('Ctrl Pts',(-8.48255899100005,11.6,-6.95142516400002));
#276391=CARTESIAN_POINT('Ctrl Pts',(-8.47973649400006,15.2,-6.95040697300002));
#276392=CARTESIAN_POINT('Ctrl Pts',(-8.47973649400006,11.6,-6.95040697300002));
#276393=CARTESIAN_POINT('Ctrl Pts',(-8.47691991300006,15.2,-6.94938830400002));
#276394=CARTESIAN_POINT('Ctrl Pts',(-8.47691991300006,11.6,-6.94938830400002));
#276395=CARTESIAN_POINT('Ctrl Pts',(-8.47410925300006,15.2,-6.94836916900002));
#276396=CARTESIAN_POINT('Ctrl Pts',(-8.47410925300006,11.6,-6.94836916900002));
#276397=CARTESIAN_POINT('Ctrl Pts',(-8.47130452200006,15.2,-6.94734957900002));
#276398=CARTESIAN_POINT('Ctrl Pts',(-8.47130452200006,11.6,-6.94734957900002));
#276399=CARTESIAN_POINT('Ctrl Pts',(-8.46850572600006,15.2,-6.94632954200002));
#276400=CARTESIAN_POINT('Ctrl Pts',(-8.46850572600006,11.6,-6.94632954200002));
#276401=CARTESIAN_POINT('Ctrl Pts',(-8.46571286900006,15.2,-6.94530907100001));
#276402=CARTESIAN_POINT('Ctrl Pts',(-8.46571286900006,11.6,-6.94530907100001));
#276403=CARTESIAN_POINT('Ctrl Pts',(-8.46292596100006,15.2,-6.94428817600001));
#276404=CARTESIAN_POINT('Ctrl Pts',(-8.46292596100006,11.6,-6.94428817600001));
#276405=CARTESIAN_POINT('Ctrl Pts',(-8.46014500600005,15.2,-6.94326686700002));
#276406=CARTESIAN_POINT('Ctrl Pts',(-8.46014500600005,11.6,-6.94326686700002));
#276407=CARTESIAN_POINT('Ctrl Pts',(-8.45737001200006,15.2,-6.94224515400002));
#276408=CARTESIAN_POINT('Ctrl Pts',(-8.45737001200006,11.6,-6.94224515400002));
#276409=CARTESIAN_POINT('Ctrl Pts',(-8.45460098500006,15.2,-6.94122304900001));
#276410=CARTESIAN_POINT('Ctrl Pts',(-8.45460098500006,11.6,-6.94122304900001));
#276411=CARTESIAN_POINT('Ctrl Pts',(-8.45183793100006,15.2,-6.94020056100002));
#276412=CARTESIAN_POINT('Ctrl Pts',(-8.45183793100006,11.6,-6.94020056100002));
#276413=CARTESIAN_POINT('Ctrl Pts',(-8.44908085600006,15.2,-6.93917770200001));
#276414=CARTESIAN_POINT('Ctrl Pts',(-8.44908085600006,11.6,-6.93917770200001));
#276415=CARTESIAN_POINT('Ctrl Pts',(-8.44632976900006,15.2,-6.93815448200001));
#276416=CARTESIAN_POINT('Ctrl Pts',(-8.44632976900006,11.6,-6.93815448200001));
#276417=CARTESIAN_POINT('Ctrl Pts',(-8.44358467400006,15.2,-6.93713091300002));
#276418=CARTESIAN_POINT('Ctrl Pts',(-8.44358467400006,11.6,-6.93713091300002));
#276419=CARTESIAN_POINT('Ctrl Pts',(-8.44084557900005,15.2,-6.93610700400002));
#276420=CARTESIAN_POINT('Ctrl Pts',(-8.44084557900005,11.6,-6.93610700400002));
#276421=CARTESIAN_POINT('Ctrl Pts',(-8.43811248900005,15.2,-6.93508276600002));
#276422=CARTESIAN_POINT('Ctrl Pts',(-8.43811248900005,11.6,-6.93508276600002));
#276423=CARTESIAN_POINT('Ctrl Pts',(-8.43538541200006,15.2,-6.93405821000002));
#276424=CARTESIAN_POINT('Ctrl Pts',(-8.43538541200006,11.6,-6.93405821000002));
#276425=CARTESIAN_POINT('Ctrl Pts',(-8.43266435300006,15.2,-6.93303334900002));
#276426=CARTESIAN_POINT('Ctrl Pts',(-8.43266435300006,11.6,-6.93303334900002));
#276427=CARTESIAN_POINT('Ctrl Pts',(-8.42994932200006,15.2,-6.93200819000002));
#276428=CARTESIAN_POINT('Ctrl Pts',(-8.42994932200006,11.6,-6.93200819000002));
#276429=CARTESIAN_POINT('Ctrl Pts',(-8.42724032100006,15.2,-6.93098274800001));
#276430=CARTESIAN_POINT('Ctrl Pts',(-8.42724032100006,11.6,-6.93098274800001));
#276431=CARTESIAN_POINT('Ctrl Pts',(-8.42453736000006,15.2,-6.92995703000002));
#276432=CARTESIAN_POINT('Ctrl Pts',(-8.42453736000006,11.6,-6.92995703000002));
#276433=CARTESIAN_POINT('Ctrl Pts',(-8.42184044300006,15.2,-6.92893105000002));
#276434=CARTESIAN_POINT('Ctrl Pts',(-8.42184044300006,11.6,-6.92893105000002));
#276435=CARTESIAN_POINT('Ctrl Pts',(-8.41914957900006,15.2,-6.92790481800002));
#276436=CARTESIAN_POINT('Ctrl Pts',(-8.41914957900006,11.6,-6.92790481800002));
#276437=CARTESIAN_POINT('Ctrl Pts',(-8.41646477200005,15.2,-6.92687834500001));
#276438=CARTESIAN_POINT('Ctrl Pts',(-8.41646477200005,11.6,-6.92687834500001));
#276439=CARTESIAN_POINT('Ctrl Pts',(-8.41378603100006,15.2,-6.92585164200001));
#276440=CARTESIAN_POINT('Ctrl Pts',(-8.41378603100006,11.6,-6.92585164200001));
#276441=CARTESIAN_POINT('Ctrl Pts',(-8.41111336100006,15.2,-6.92482472000002));
#276442=CARTESIAN_POINT('Ctrl Pts',(-8.41111336100006,11.6,-6.92482472000002));
#276443=CARTESIAN_POINT('Ctrl Pts',(-8.40844676900005,15.2,-6.92379758900002));
#276444=CARTESIAN_POINT('Ctrl Pts',(-8.40844676900005,11.6,-6.92379758900002));
#276445=CARTESIAN_POINT('Ctrl Pts',(-8.40578626200006,15.2,-6.92277026300002));
#276446=CARTESIAN_POINT('Ctrl Pts',(-8.40578626200006,11.6,-6.92277026300002));
#276447=CARTESIAN_POINT('Ctrl Pts',(-8.40313184700006,15.2,-6.92174275100002));
#276448=CARTESIAN_POINT('Ctrl Pts',(-8.40313184700006,11.6,-6.92174275100002));
#276449=CARTESIAN_POINT('Ctrl Pts',(-8.40048352900006,15.2,-6.92071506500002));
#276450=CARTESIAN_POINT('Ctrl Pts',(-8.40048352900006,11.6,-6.92071506500002));
#276451=CARTESIAN_POINT('Ctrl Pts',(-8.39784131700006,15.2,-6.91968721500002));
#276452=CARTESIAN_POINT('Ctrl Pts',(-8.39784131700006,11.6,-6.91968721500002));
#276453=CARTESIAN_POINT('Ctrl Pts',(-8.39520521500006,15.2,-6.91865921400002));
#276454=CARTESIAN_POINT('Ctrl Pts',(-8.39520521500006,11.6,-6.91865921400002));
#276455=CARTESIAN_POINT('Ctrl Pts',(-8.39257523200006,15.2,-6.91763107400002));
#276456=CARTESIAN_POINT('Ctrl Pts',(-8.39257523200006,11.6,-6.91763107400002));
#276457=CARTESIAN_POINT('Ctrl Pts',(-8.38995137300006,15.2,-6.91660280300002));
#276458=CARTESIAN_POINT('Ctrl Pts',(-8.38995137300006,11.6,-6.91660280300002));
#276459=CARTESIAN_POINT('Ctrl Pts',(-8.38733364500006,15.2,-6.91557441500001));
#276460=CARTESIAN_POINT('Ctrl Pts',(-8.38733364500006,11.6,-6.91557441500001));
#276461=CARTESIAN_POINT('Ctrl Pts',(-8.38472205600005,15.2,-6.91454592100002));
#276462=CARTESIAN_POINT('Ctrl Pts',(-8.38472205600005,11.6,-6.91454592100002));
#276463=CARTESIAN_POINT('Ctrl Pts',(-8.38211661100006,15.2,-6.91351733200002));
#276464=CARTESIAN_POINT('Ctrl Pts',(-8.38211661100006,11.6,-6.91351733200002));
#276465=CARTESIAN_POINT('Ctrl Pts',(-8.37951731800005,15.2,-6.91248865900001));
#276466=CARTESIAN_POINT('Ctrl Pts',(-8.37951731800005,11.6,-6.91248865900001));
#276467=CARTESIAN_POINT('Ctrl Pts',(-8.37692418100006,15.2,-6.91145991600001));
#276468=CARTESIAN_POINT('Ctrl Pts',(-8.37692418100006,11.6,-6.91145991600001));
#276469=CARTESIAN_POINT('Ctrl Pts',(-8.37433721100006,15.2,-6.91043111100001));
#276470=CARTESIAN_POINT('Ctrl Pts',(-8.37433721100006,11.6,-6.91043111100001));
#276471=CARTESIAN_POINT('Ctrl Pts',(-8.37175641100006,15.2,-6.90940225800002));
#276472=CARTESIAN_POINT('Ctrl Pts',(-8.37175641100006,11.6,-6.90940225800002));
#276473=CARTESIAN_POINT('Ctrl Pts',(-8.36918179000006,15.2,-6.90837336800002));
#276474=CARTESIAN_POINT('Ctrl Pts',(-8.36918179000006,11.6,-6.90837336800002));
#276475=CARTESIAN_POINT('Ctrl Pts',(-8.36661335300006,15.2,-6.90734445300001));
#276476=CARTESIAN_POINT('Ctrl Pts',(-8.36661335300006,11.6,-6.90734445300001));
#276477=CARTESIAN_POINT('Ctrl Pts',(-8.36405110900006,15.2,-6.90631552400002));
#276478=CARTESIAN_POINT('Ctrl Pts',(-8.36405110900006,11.6,-6.90631552400002));
#276479=CARTESIAN_POINT('Ctrl Pts',(-8.36149506200006,15.2,-6.90528659300002));
#276480=CARTESIAN_POINT('Ctrl Pts',(-8.36149506200006,11.6,-6.90528659300002));
#276481=CARTESIAN_POINT('Ctrl Pts',(-8.35894522100006,15.2,-6.90425767200002));
#276482=CARTESIAN_POINT('Ctrl Pts',(-8.35894522100006,11.6,-6.90425767200002));
#276483=CARTESIAN_POINT('Ctrl Pts',(-8.35640159200006,15.2,-6.90322877200002));
#276484=CARTESIAN_POINT('Ctrl Pts',(-8.35640159200006,11.6,-6.90322877200002));
#276485=CARTESIAN_POINT('Ctrl Pts',(-8.35386418000006,15.2,-6.90219990600001));
#276486=CARTESIAN_POINT('Ctrl Pts',(-8.35386418000006,11.6,-6.90219990600001));
#276487=CARTESIAN_POINT('Ctrl Pts',(-8.35133299600006,15.2,-6.90117108400001));
#276488=CARTESIAN_POINT('Ctrl Pts',(-8.35133299600006,11.6,-6.90117108400001));
#276489=CARTESIAN_POINT('Ctrl Pts',(-8.34880804200005,15.2,-6.90014232000002));
#276490=CARTESIAN_POINT('Ctrl Pts',(-8.34880804200005,11.6,-6.90014232000002));
#276491=CARTESIAN_POINT('Ctrl Pts',(-8.34628932800005,15.2,-6.89911362500002));
#276492=CARTESIAN_POINT('Ctrl Pts',(-8.34628932800005,11.6,-6.89911362500002));
#276493=CARTESIAN_POINT('Ctrl Pts',(-8.34377685900006,15.2,-6.89808501100002));
#276494=CARTESIAN_POINT('Ctrl Pts',(-8.34377685900006,11.6,-6.89808501100002));
#276495=CARTESIAN_POINT('Ctrl Pts',(-8.34127064400005,15.2,-6.89705649000001));
#276496=CARTESIAN_POINT('Ctrl Pts',(-8.34127064400005,11.6,-6.89705649000001));
#276497=CARTESIAN_POINT('Ctrl Pts',(-8.33877068700006,15.2,-6.89602807400002));
#276498=CARTESIAN_POINT('Ctrl Pts',(-8.33877068700006,11.6,-6.89602807400002));
#276499=CARTESIAN_POINT('Ctrl Pts',(-8.33627699700006,15.2,-6.89499977500001));
#276500=CARTESIAN_POINT('Ctrl Pts',(-8.33627699700006,11.6,-6.89499977500001));
#276501=CARTESIAN_POINT('Ctrl Pts',(-8.33378957900005,15.2,-6.89397160500001));
#276502=CARTESIAN_POINT('Ctrl Pts',(-8.33378957900005,11.6,-6.89397160500001));
#276503=CARTESIAN_POINT('Ctrl Pts',(-8.33130844300005,15.2,-6.89294357600001));
#276504=CARTESIAN_POINT('Ctrl Pts',(-8.33130844300005,11.6,-6.89294357600001));
#276505=CARTESIAN_POINT('Ctrl Pts',(-8.32883359200006,15.2,-6.89191570100002));
#276506=CARTESIAN_POINT('Ctrl Pts',(-8.32883359200006,11.6,-6.89191570100002));
#276507=CARTESIAN_POINT('Ctrl Pts',(-8.32636503500006,15.2,-6.89088799200002));
#276508=CARTESIAN_POINT('Ctrl Pts',(-8.32636503500006,11.6,-6.89088799200002));
#276509=CARTESIAN_POINT('Ctrl Pts',(-8.32390277900006,15.2,-6.88986046100001));
#276510=CARTESIAN_POINT('Ctrl Pts',(-8.32390277900006,11.6,-6.88986046100001));
#276511=CARTESIAN_POINT('Ctrl Pts',(-8.32144683000006,15.2,-6.88883311900002));
#276512=CARTESIAN_POINT('Ctrl Pts',(-8.32144683000006,11.6,-6.88883311900002));
#276513=CARTESIAN_POINT('Ctrl Pts',(-8.31899719600005,15.2,-6.88780598100001));
#276514=CARTESIAN_POINT('Ctrl Pts',(-8.31899719600005,11.6,-6.88780598100001));
#276515=CARTESIAN_POINT('Ctrl Pts',(-8.31655388200006,15.2,-6.88677905700001));
#276516=CARTESIAN_POINT('Ctrl Pts',(-8.31655388200006,11.6,-6.88677905700001));
#276517=CARTESIAN_POINT('Ctrl Pts',(-8.31411689600005,15.2,-6.88575236100001));
#276518=CARTESIAN_POINT('Ctrl Pts',(-8.31411689600005,11.6,-6.88575236100001));
#276519=CARTESIAN_POINT('Ctrl Pts',(-8.31168624600006,15.2,-6.88472590400002));
#276520=CARTESIAN_POINT('Ctrl Pts',(-8.31168624600006,11.6,-6.88472590400002));
#276521=CARTESIAN_POINT('Ctrl Pts',(-8.30926193800006,15.2,-6.88369969900001));
#276522=CARTESIAN_POINT('Ctrl Pts',(-8.30926193800006,11.6,-6.88369969900001));
#276523=CARTESIAN_POINT('Ctrl Pts',(-8.30684397800006,15.2,-6.88267375900002));
#276524=CARTESIAN_POINT('Ctrl Pts',(-8.30684397800006,11.6,-6.88267375900002));
#276525=CARTESIAN_POINT('Ctrl Pts',(-8.30443237500005,15.2,-6.88164809600002));
#276526=CARTESIAN_POINT('Ctrl Pts',(-8.30443237500005,11.6,-6.88164809600002));
#276527=CARTESIAN_POINT('Ctrl Pts',(-8.30202713400006,15.2,-6.88062272300002));
#276528=CARTESIAN_POINT('Ctrl Pts',(-8.30202713400006,11.6,-6.88062272300002));
#276529=CARTESIAN_POINT('Ctrl Pts',(-8.29962826300006,15.2,-6.87959765300001));
#276530=CARTESIAN_POINT('Ctrl Pts',(-8.29962826300006,11.6,-6.87959765300001));
#276531=CARTESIAN_POINT('Ctrl Pts',(-8.29723576800006,15.2,-6.87857289700001));
#276532=CARTESIAN_POINT('Ctrl Pts',(-8.29723576800006,11.6,-6.87857289700001));
#276533=CARTESIAN_POINT('Ctrl Pts',(-8.29484965700006,15.2,-6.87754847000001));
#276534=CARTESIAN_POINT('Ctrl Pts',(-8.29484965700006,11.6,-6.87754847000001));
#276535=CARTESIAN_POINT('Ctrl Pts',(-8.29246993600006,15.2,-6.87652438300002));
#276536=CARTESIAN_POINT('Ctrl Pts',(-8.29246993600006,11.6,-6.87652438300002));
#276537=CARTESIAN_POINT('Ctrl Pts',(-8.29009661400006,15.2,-6.87550064900002));
#276538=CARTESIAN_POINT('Ctrl Pts',(-8.29009661400006,11.6,-6.87550064900002));
#276539=CARTESIAN_POINT('Ctrl Pts',(-8.28772969600006,15.2,-6.87447728100001));
#276540=CARTESIAN_POINT('Ctrl Pts',(-8.28772969600006,11.6,-6.87447728100001));
#276541=CARTESIAN_POINT('Ctrl Pts',(-8.28536918900006,15.2,-6.87345429300001));
#276542=CARTESIAN_POINT('Ctrl Pts',(-8.28536918900006,11.6,-6.87345429300001));
#276543=CARTESIAN_POINT('Ctrl Pts',(-8.28301510100006,15.2,-6.87243169500002));
#276544=CARTESIAN_POINT('Ctrl Pts',(-8.28301510100006,11.6,-6.87243169500002));
#276545=CARTESIAN_POINT('Ctrl Pts',(-8.28066743900006,15.2,-6.87140950400002));
#276546=CARTESIAN_POINT('Ctrl Pts',(-8.28066743900006,11.6,-6.87140950400002));
#276547=CARTESIAN_POINT('Ctrl Pts',(-8.27832621000006,15.2,-6.87038772900002));
#276548=CARTESIAN_POINT('Ctrl Pts',(-8.27832621000006,11.6,-6.87038772900002));
#276549=CARTESIAN_POINT('Ctrl Pts',(-8.27599142100006,15.2,-6.86936638500002));
#276550=CARTESIAN_POINT('Ctrl Pts',(-8.27599142100006,11.6,-6.86936638500002));
#276551=CARTESIAN_POINT('Ctrl Pts',(-8.27366307900006,15.2,-6.86834548500002));
#276552=CARTESIAN_POINT('Ctrl Pts',(-8.27366307900006,11.6,-6.86834548500002));
#276553=CARTESIAN_POINT('Ctrl Pts',(-8.27134119000006,15.2,-6.86732504200001));
#276554=CARTESIAN_POINT('Ctrl Pts',(-8.27134119000006,11.6,-6.86732504200001));
#276555=CARTESIAN_POINT('Ctrl Pts',(-8.26902576200006,15.2,-6.86630507000002));
#276556=CARTESIAN_POINT('Ctrl Pts',(-8.26902576200006,11.6,-6.86630507000002));
#276557=CARTESIAN_POINT('Ctrl Pts',(-8.26671680300005,15.2,-6.86528558000001));
#276558=CARTESIAN_POINT('Ctrl Pts',(-8.26671680300005,11.6,-6.86528558000001));
#276559=CARTESIAN_POINT('Ctrl Pts',(-8.26441431900006,15.2,-6.86426658600002));
#276560=CARTESIAN_POINT('Ctrl Pts',(-8.26441431900006,11.6,-6.86426658600002));
#276561=CARTESIAN_POINT('Ctrl Pts',(-8.26211831700006,15.2,-6.86324810400002));
#276562=CARTESIAN_POINT('Ctrl Pts',(-8.26211831700006,11.6,-6.86324810400002));
#276563=CARTESIAN_POINT('Ctrl Pts',(-8.25982880500005,15.2,-6.86223014300002));
#276564=CARTESIAN_POINT('Ctrl Pts',(-8.25982880500005,11.6,-6.86223014300002));
#276565=CARTESIAN_POINT('Ctrl Pts',(-8.25754578900005,15.2,-6.86121271800002));
#276566=CARTESIAN_POINT('Ctrl Pts',(-8.25754578900005,11.6,-6.86121271800002));
#276567=CARTESIAN_POINT('Ctrl Pts',(-8.25526927700006,15.2,-6.86019584300002));
#276568=CARTESIAN_POINT('Ctrl Pts',(-8.25526927700006,11.6,-6.86019584300002));
#276569=CARTESIAN_POINT('Ctrl Pts',(-8.25299927600006,15.2,-6.85917953200001));
#276570=CARTESIAN_POINT('Ctrl Pts',(-8.25299927600006,11.6,-6.85917953200001));
#276571=CARTESIAN_POINT('Ctrl Pts',(-8.25073579400006,15.2,-6.85816379700002));
#276572=CARTESIAN_POINT('Ctrl Pts',(-8.25073579400006,11.6,-6.85816379700002));
#276573=CARTESIAN_POINT('Ctrl Pts',(-8.24847883600006,15.2,-6.85714865200002));
#276574=CARTESIAN_POINT('Ctrl Pts',(-8.24847883600006,11.6,-6.85714865200002));
#276575=CARTESIAN_POINT('Ctrl Pts',(-8.24622841100006,15.2,-6.85613411000002));
#276576=CARTESIAN_POINT('Ctrl Pts',(-8.24622841100006,11.6,-6.85613411000002));
#276577=CARTESIAN_POINT('Ctrl Pts',(-8.24398452500006,15.2,-6.85512018700001));
#276578=CARTESIAN_POINT('Ctrl Pts',(-8.24398452500006,11.6,-6.85512018700001));
#276579=CARTESIAN_POINT('Ctrl Pts',(-8.24174718700006,15.2,-6.85410689300002));
#276580=CARTESIAN_POINT('Ctrl Pts',(-8.24174718700006,11.6,-6.85410689300002));
#276581=CARTESIAN_POINT('Ctrl Pts',(-8.23951640200006,15.2,-6.85309424500002));
#276582=CARTESIAN_POINT('Ctrl Pts',(-8.23951640200006,11.6,-6.85309424500002));
#276583=CARTESIAN_POINT('Ctrl Pts',(-8.23729218000006,15.2,-6.85208225400002));
#276584=CARTESIAN_POINT('Ctrl Pts',(-8.23729218000006,11.6,-6.85208225400002));
#276585=CARTESIAN_POINT('Ctrl Pts',(-8.23507452500005,15.2,-6.85107093700001));
#276586=CARTESIAN_POINT('Ctrl Pts',(-8.23507452500005,11.6,-6.85107093700001));
#276587=CARTESIAN_POINT('Ctrl Pts',(-8.23286344500006,15.2,-6.85006030300002));
#276588=CARTESIAN_POINT('Ctrl Pts',(-8.23286344500006,11.6,-6.85006030300002));
#276589=CARTESIAN_POINT('Ctrl Pts',(-8.23065894900006,15.2,-6.84905037100001));
#276590=CARTESIAN_POINT('Ctrl Pts',(-8.23065894900006,11.6,-6.84905037100001));
#276591=CARTESIAN_POINT('Ctrl Pts',(-8.22846104400006,15.2,-6.84804115200001));
#276592=CARTESIAN_POINT('Ctrl Pts',(-8.22846104400006,11.6,-6.84804115200001));
#276593=CARTESIAN_POINT('Ctrl Pts',(-8.22626973600006,15.2,-6.84703266000002));
#276594=CARTESIAN_POINT('Ctrl Pts',(-8.22626973600006,11.6,-6.84703266000002));
#276595=CARTESIAN_POINT('Ctrl Pts',(-8.22408503300006,15.2,-6.84602491000001));
#276596=CARTESIAN_POINT('Ctrl Pts',(-8.22408503300006,11.6,-6.84602491000001));
#276597=CARTESIAN_POINT('Ctrl Pts',(-8.22190694200006,15.2,-6.84501791600002));
#276598=CARTESIAN_POINT('Ctrl Pts',(-8.22190694200006,11.6,-6.84501791600002));
#276599=CARTESIAN_POINT('Ctrl Pts',(-8.21973547100006,15.2,-6.84401169100001));
#276600=CARTESIAN_POINT('Ctrl Pts',(-8.21973547100006,11.6,-6.84401169100001));
#276601=CARTESIAN_POINT('Ctrl Pts',(-8.21757062600006,15.2,-6.84300624900001));
#276602=CARTESIAN_POINT('Ctrl Pts',(-8.21757062600006,11.6,-6.84300624900001));
#276603=CARTESIAN_POINT('Ctrl Pts',(-8.21541241600006,15.2,-6.84200160600002));
#276604=CARTESIAN_POINT('Ctrl Pts',(-8.21541241600006,11.6,-6.84200160600002));
#276605=CARTESIAN_POINT('Ctrl Pts',(-8.21326084700006,15.2,-6.84099777500002));
#276606=CARTESIAN_POINT('Ctrl Pts',(-8.21326084700006,11.6,-6.84099777500002));
#276607=CARTESIAN_POINT('Ctrl Pts',(-8.21111592700005,15.2,-6.83999477000001));
#276608=CARTESIAN_POINT('Ctrl Pts',(-8.21111592700005,11.6,-6.83999477000001));
#276609=CARTESIAN_POINT('Ctrl Pts',(-8.20897766400006,15.2,-6.83899260600001));
#276610=CARTESIAN_POINT('Ctrl Pts',(-8.20897766400006,11.6,-6.83899260600001));
#276611=CARTESIAN_POINT('Ctrl Pts',(-8.20684606400006,15.2,-6.83799129700001));
#276612=CARTESIAN_POINT('Ctrl Pts',(-8.20684606400006,11.6,-6.83799129700001));
#276613=CARTESIAN_POINT('Ctrl Pts',(-8.20472113500006,15.2,-6.83699085700002));
#276614=CARTESIAN_POINT('Ctrl Pts',(-8.20472113500006,11.6,-6.83699085700002));
#276615=CARTESIAN_POINT('Ctrl Pts',(-8.20260288500006,15.2,-6.83599130200002));
#276616=CARTESIAN_POINT('Ctrl Pts',(-8.20260288500006,11.6,-6.83599130200002));
#276617=CARTESIAN_POINT('Ctrl Pts',(-8.20049132100005,15.2,-6.83499264500002));
#276618=CARTESIAN_POINT('Ctrl Pts',(-8.20049132100005,11.6,-6.83499264500002));
#276619=CARTESIAN_POINT('Ctrl Pts',(-8.19838644900006,15.2,-6.83399490000002));
#276620=CARTESIAN_POINT('Ctrl Pts',(-8.19838644900006,11.6,-6.83399490000002));
#276621=CARTESIAN_POINT('Ctrl Pts',(-8.19628827900006,15.2,-6.83299808400001));
#276622=CARTESIAN_POINT('Ctrl Pts',(-8.19628827900006,11.6,-6.83299808400001));
#276623=CARTESIAN_POINT('Ctrl Pts',(-8.19419681700005,15.2,-6.83200220900002));
#276624=CARTESIAN_POINT('Ctrl Pts',(-8.19419681700005,11.6,-6.83200220900002));
#276625=CARTESIAN_POINT('Ctrl Pts',(-8.19211207000006,15.2,-6.83100729200002));
#276626=CARTESIAN_POINT('Ctrl Pts',(-8.19211207000006,11.6,-6.83100729200002));
#276627=CARTESIAN_POINT('Ctrl Pts',(-8.19003404800006,15.2,-6.83001334600001));
#276628=CARTESIAN_POINT('Ctrl Pts',(-8.19003404800006,11.6,-6.83001334600001));
#276629=CARTESIAN_POINT('Ctrl Pts',(-8.18796275500006,15.2,-6.82902038700002));
#276630=CARTESIAN_POINT('Ctrl Pts',(-8.18796275500006,11.6,-6.82902038700002));
#276631=CARTESIAN_POINT('Ctrl Pts',(-8.18589820000006,15.2,-6.82802842800001));
#276632=CARTESIAN_POINT('Ctrl Pts',(-8.18589820000006,11.6,-6.82802842800001));
#276633=CARTESIAN_POINT('Ctrl Pts',(-8.18384039200006,15.2,-6.82703748600002));
#276634=CARTESIAN_POINT('Ctrl Pts',(-8.18384039200006,11.6,-6.82703748600002));
#276635=CARTESIAN_POINT('Ctrl Pts',(-8.18178933600005,15.2,-6.82604757600001));
#276636=CARTESIAN_POINT('Ctrl Pts',(-8.18178933600005,11.6,-6.82604757600001));
#276637=CARTESIAN_POINT('Ctrl Pts',(-8.17974504200006,15.2,-6.82505871000001));
#276638=CARTESIAN_POINT('Ctrl Pts',(-8.17974504200006,11.6,-6.82505871000001));
#276639=CARTESIAN_POINT('Ctrl Pts',(-8.17770751500005,15.2,-6.82407090600002));
#276640=CARTESIAN_POINT('Ctrl Pts',(-8.17770751500005,11.6,-6.82407090600002));
#276641=CARTESIAN_POINT('Ctrl Pts',(-8.17567676400006,15.2,-6.82308417800002));
#276642=CARTESIAN_POINT('Ctrl Pts',(-8.17567676400006,11.6,-6.82308417800002));
#276643=CARTESIAN_POINT('Ctrl Pts',(-8.17365279800006,15.2,-6.82209854300002));
#276644=CARTESIAN_POINT('Ctrl Pts',(-8.17365279800006,11.6,-6.82209854300002));
#276645=CARTESIAN_POINT('Ctrl Pts',(-8.17163562200006,15.2,-6.82111401300002));
#276646=CARTESIAN_POINT('Ctrl Pts',(-8.17163562200006,11.6,-6.82111401300002));
#276647=CARTESIAN_POINT('Ctrl Pts',(-8.16962524500006,15.2,-6.82013060400001));
#276648=CARTESIAN_POINT('Ctrl Pts',(-8.16962524500006,11.6,-6.82013060400001));
#276649=CARTESIAN_POINT('Ctrl Pts',(-8.16762167300006,15.2,-6.81914833300001));
#276650=CARTESIAN_POINT('Ctrl Pts',(-8.16762167300006,11.6,-6.81914833300001));
#276651=CARTESIAN_POINT('Ctrl Pts',(-8.16562491600006,15.2,-6.81816721500001));
#276652=CARTESIAN_POINT('Ctrl Pts',(-8.16562491600006,11.6,-6.81816721500001));
#276653=CARTESIAN_POINT('Ctrl Pts',(-8.16363498100005,15.2,-6.81718726300002));
#276654=CARTESIAN_POINT('Ctrl Pts',(-8.16363498100005,11.6,-6.81718726300002));
#276655=CARTESIAN_POINT('Ctrl Pts',(-8.16165187500006,15.2,-6.81620849600002));
#276656=CARTESIAN_POINT('Ctrl Pts',(-8.16165187500006,11.6,-6.81620849600002));
#276657=CARTESIAN_POINT('Ctrl Pts',(-8.15967560600006,15.2,-6.81523092700001));
#276658=CARTESIAN_POINT('Ctrl Pts',(-8.15967560600006,11.6,-6.81523092700001));
#276659=CARTESIAN_POINT('Ctrl Pts',(-8.15770618100006,15.2,-6.81425457200002));
#276660=CARTESIAN_POINT('Ctrl Pts',(-8.15770618100006,11.6,-6.81425457200002));
#276661=CARTESIAN_POINT('Ctrl Pts',(-8.15574360800005,15.2,-6.81327944800002));
#276662=CARTESIAN_POINT('Ctrl Pts',(-8.15574360800005,11.6,-6.81327944800002));
#276663=CARTESIAN_POINT('Ctrl Pts',(-8.15378789600006,15.2,-6.81230556900001));
#276664=CARTESIAN_POINT('Ctrl Pts',(-8.15378789600006,11.6,-6.81230556900001));
#276665=CARTESIAN_POINT('Ctrl Pts',(-8.15183905100006,15.2,-6.81133295000001));
#276666=CARTESIAN_POINT('Ctrl Pts',(-8.15183905100006,11.6,-6.81133295000001));
#276667=CARTESIAN_POINT('Ctrl Pts',(-8.14989708100006,15.2,-6.81036160900002));
#276668=CARTESIAN_POINT('Ctrl Pts',(-8.14989708100006,11.6,-6.81036160900002));
#276669=CARTESIAN_POINT('Ctrl Pts',(-8.14796199500006,15.2,-6.80939156100001));
#276670=CARTESIAN_POINT('Ctrl Pts',(-8.14796199500006,11.6,-6.80939156100001));
#276671=CARTESIAN_POINT('Ctrl Pts',(-8.14603380000005,15.2,-6.80842282100001));
#276672=CARTESIAN_POINT('Ctrl Pts',(-8.14603380000005,11.6,-6.80842282100001));
#276673=CARTESIAN_POINT('Ctrl Pts',(-8.14411250400006,15.2,-6.80745540700002));
#276674=CARTESIAN_POINT('Ctrl Pts',(-8.14411250400006,11.6,-6.80745540700002));
#276675=CARTESIAN_POINT('Ctrl Pts',(-8.14219811500006,15.2,-6.80648933300001));
#276676=CARTESIAN_POINT('Ctrl Pts',(-8.14219811500006,11.6,-6.80648933300001));
#276677=CARTESIAN_POINT('Ctrl Pts',(-8.14029063900006,15.2,-6.80552461600002));
#276678=CARTESIAN_POINT('Ctrl Pts',(-8.14029063900006,11.6,-6.80552461600002));
#276679=CARTESIAN_POINT('Ctrl Pts',(-8.13839008600005,15.2,-6.80456127100002));
#276680=CARTESIAN_POINT('Ctrl Pts',(-8.13839008600005,11.6,-6.80456127100002));
#276681=CARTESIAN_POINT('Ctrl Pts',(-8.13649646400006,15.2,-6.80359931600002));
#276682=CARTESIAN_POINT('Ctrl Pts',(-8.13649646400006,11.6,-6.80359931600002));
#276683=CARTESIAN_POINT('Ctrl Pts',(-8.13460977800006,15.2,-6.80263876500002));
#276684=CARTESIAN_POINT('Ctrl Pts',(-8.13460977800006,11.6,-6.80263876500002));
#276685=CARTESIAN_POINT('Ctrl Pts',(-8.13273003800006,15.2,-6.80167963700002));
#276686=CARTESIAN_POINT('Ctrl Pts',(-8.13273003800006,11.6,-6.80167963700002));
#276687=CARTESIAN_POINT('Ctrl Pts',(-8.13085725300006,15.2,-6.80072194600001));
#276688=CARTESIAN_POINT('Ctrl Pts',(-8.13085725300006,11.6,-6.80072194600001));
#276689=CARTESIAN_POINT('Ctrl Pts',(-8.12899142800006,15.2,-6.79976570900001));
#276690=CARTESIAN_POINT('Ctrl Pts',(-8.12899142800006,11.6,-6.79976570900001));
#276691=CARTESIAN_POINT('Ctrl Pts',(-8.12713257400006,15.2,-6.79881094300002));
#276692=CARTESIAN_POINT('Ctrl Pts',(-8.12713257400006,11.6,-6.79881094300002));
#276693=CARTESIAN_POINT('Ctrl Pts',(-8.12528069700006,15.2,-6.79785766400002));
#276694=CARTESIAN_POINT('Ctrl Pts',(-8.12528069700006,11.6,-6.79785766400002));
#276695=CARTESIAN_POINT('Ctrl Pts',(-8.12343580400006,15.2,-6.79690588900002));
#276696=CARTESIAN_POINT('Ctrl Pts',(-8.12343580400006,11.6,-6.79690588900002));
#276697=CARTESIAN_POINT('Ctrl Pts',(-8.12159790600005,15.2,-6.79595563300002));
#276698=CARTESIAN_POINT('Ctrl Pts',(-8.12159790600005,11.6,-6.79595563300002));
#276699=CARTESIAN_POINT('Ctrl Pts',(-8.11976700800006,15.2,-6.79500691500002));
#276700=CARTESIAN_POINT('Ctrl Pts',(-8.11976700800006,11.6,-6.79500691500002));
#276701=CARTESIAN_POINT('Ctrl Pts',(-8.11794312000006,15.2,-6.79405975100002));
#276702=CARTESIAN_POINT('Ctrl Pts',(-8.11794312000006,11.6,-6.79405975100002));
#276703=CARTESIAN_POINT('Ctrl Pts',(-8.11612624900006,15.2,-6.79311415700001));
#276704=CARTESIAN_POINT('Ctrl Pts',(-8.11612624900006,11.6,-6.79311415700001));
#276705=CARTESIAN_POINT('Ctrl Pts',(-8.11431640400006,15.2,-6.79217015000001));
#276706=CARTESIAN_POINT('Ctrl Pts',(-8.11431640400006,11.6,-6.79217015000001));
#276707=CARTESIAN_POINT('Ctrl Pts',(-8.11251359200006,15.2,-6.79122774800001));
#276708=CARTESIAN_POINT('Ctrl Pts',(-8.11251359200006,11.6,-6.79122774800001));
#276709=CARTESIAN_POINT('Ctrl Pts',(-8.11071782100005,15.2,-6.79028696700002));
#276710=CARTESIAN_POINT('Ctrl Pts',(-8.11071782100005,11.6,-6.79028696700002));
#276711=CARTESIAN_POINT('Ctrl Pts',(-8.10892909900006,15.2,-6.78934782500002));
#276712=CARTESIAN_POINT('Ctrl Pts',(-8.10892909900006,11.6,-6.78934782500002));
#276713=CARTESIAN_POINT('Ctrl Pts',(-8.10714743500006,15.2,-6.78841033800002));
#276714=CARTESIAN_POINT('Ctrl Pts',(-8.10714743500006,11.6,-6.78841033800002));
#276715=CARTESIAN_POINT('Ctrl Pts',(-8.10537283700006,15.2,-6.78747452400002));
#276716=CARTESIAN_POINT('Ctrl Pts',(-8.10537283700006,11.6,-6.78747452400002));
#276717=CARTESIAN_POINT('Ctrl Pts',(-8.10360531200006,15.2,-6.78654039900002));
#276718=CARTESIAN_POINT('Ctrl Pts',(-8.10360531200006,11.6,-6.78654039900002));
#276719=CARTESIAN_POINT('Ctrl Pts',(-8.10184486900006,15.2,-6.78560798200002));
#276720=CARTESIAN_POINT('Ctrl Pts',(-8.10184486900006,11.6,-6.78560798200002));
#276721=CARTESIAN_POINT('Ctrl Pts',(-8.10009151600006,15.2,-6.78467728800002));
#276722=CARTESIAN_POINT('Ctrl Pts',(-8.10009151600006,11.6,-6.78467728800002));
#276723=CARTESIAN_POINT('Ctrl Pts',(-8.09834526200006,15.2,-6.78374833700002));
#276724=CARTESIAN_POINT('Ctrl Pts',(-8.09834526200006,11.6,-6.78374833700002));
#276725=CARTESIAN_POINT('Ctrl Pts',(-8.09660611400006,15.2,-6.78282114600002));
#276726=CARTESIAN_POINT('Ctrl Pts',(-8.09660611400006,11.6,-6.78282114600002));
#276727=CARTESIAN_POINT('Ctrl Pts',(-8.09487408000006,15.2,-6.78189573100001));
#276728=CARTESIAN_POINT('Ctrl Pts',(-8.09487408000006,11.6,-6.78189573100001));
#276729=CARTESIAN_POINT('Ctrl Pts',(-8.09314916900006,15.2,-6.78097211100001));
#276730=CARTESIAN_POINT('Ctrl Pts',(-8.09314916900006,11.6,-6.78097211100001));
#276731=CARTESIAN_POINT('Ctrl Pts',(-8.09143138900006,15.2,-6.78005030300002));
#276732=CARTESIAN_POINT('Ctrl Pts',(-8.09143138900006,11.6,-6.78005030300002));
#276733=CARTESIAN_POINT('Ctrl Pts',(-8.08972074900005,15.2,-6.77913032500002));
#276734=CARTESIAN_POINT('Ctrl Pts',(-8.08972074900005,11.6,-6.77913032500002));
#276735=CARTESIAN_POINT('Ctrl Pts',(-8.08801725500006,15.2,-6.77821219500002));
#276736=CARTESIAN_POINT('Ctrl Pts',(-8.08801725500006,11.6,-6.77821219500002));
#276737=CARTESIAN_POINT('Ctrl Pts',(-8.08632091900006,15.2,-6.77729593100001));
#276738=CARTESIAN_POINT('Ctrl Pts',(-8.08632091900006,11.6,-6.77729593100001));
#276739=CARTESIAN_POINT('Ctrl Pts',(-8.08463174500006,15.2,-6.77638154900002));
#276740=CARTESIAN_POINT('Ctrl Pts',(-8.08463174500006,11.6,-6.77638154900002));
#276741=CARTESIAN_POINT('Ctrl Pts',(-8.08294974400006,15.2,-6.77546907100002));
#276742=CARTESIAN_POINT('Ctrl Pts',(-8.08294974400006,11.6,-6.77546907100002));
#276743=CARTESIAN_POINT('Ctrl Pts',(-8.08127492400006,15.2,-6.77455851200002));
#276744=CARTESIAN_POINT('Ctrl Pts',(-8.08127492400006,11.6,-6.77455851200002));
#276745=CARTESIAN_POINT('Ctrl Pts',(-8.07960729300006,15.2,-6.77364988900001));
#276746=CARTESIAN_POINT('Ctrl Pts',(-8.07960729300006,11.6,-6.77364988900001));
#276747=CARTESIAN_POINT('Ctrl Pts',(-8.07794685900006,15.2,-6.77274322400002));
#276748=CARTESIAN_POINT('Ctrl Pts',(-8.07794685900006,11.6,-6.77274322400002));
#276749=CARTESIAN_POINT('Ctrl Pts',(-8.07629363200006,15.2,-6.77183853400001));
#276750=CARTESIAN_POINT('Ctrl Pts',(-8.07629363200006,11.6,-6.77183853400001));
#276751=CARTESIAN_POINT('Ctrl Pts',(-8.07464761900006,15.2,-6.77093583600002));
#276752=CARTESIAN_POINT('Ctrl Pts',(-8.07464761900006,11.6,-6.77093583600002));
#276753=CARTESIAN_POINT('Ctrl Pts',(-8.07300882800006,15.2,-6.77003514800001));
#276754=CARTESIAN_POINT('Ctrl Pts',(-8.07300882800006,11.6,-6.77003514800001));
#276755=CARTESIAN_POINT('Ctrl Pts',(-8.07137726900006,15.2,-6.76913649000002));
#276756=CARTESIAN_POINT('Ctrl Pts',(-8.07137726900006,11.6,-6.76913649000002));
#276757=CARTESIAN_POINT('Ctrl Pts',(-8.06975294900005,15.2,-6.76823988100002));
#276758=CARTESIAN_POINT('Ctrl Pts',(-8.06975294900005,11.6,-6.76823988100002));
#276759=CARTESIAN_POINT('Ctrl Pts',(-8.06813587700006,15.2,-6.76734533800002));
#276760=CARTESIAN_POINT('Ctrl Pts',(-8.06813587700006,11.6,-6.76734533800002));
#276761=CARTESIAN_POINT('Ctrl Pts',(-8.06652606200006,15.2,-6.76645288100002));
#276762=CARTESIAN_POINT('Ctrl Pts',(-8.06652606200006,11.6,-6.76645288100002));
#276763=CARTESIAN_POINT('Ctrl Pts',(-8.06492351200006,15.2,-6.76556252900002));
#276764=CARTESIAN_POINT('Ctrl Pts',(-8.06492351200006,11.6,-6.76556252900002));
#276765=CARTESIAN_POINT('Ctrl Pts',(-8.06332823500006,15.2,-6.76467429900002));
#276766=CARTESIAN_POINT('Ctrl Pts',(-8.06332823500006,11.6,-6.76467429900002));
#276767=CARTESIAN_POINT('Ctrl Pts',(-8.06174024100006,15.2,-6.76378821200001));
#276768=CARTESIAN_POINT('Ctrl Pts',(-8.06174024100006,11.6,-6.76378821200001));
#276769=CARTESIAN_POINT('Ctrl Pts',(-8.06015953800006,15.2,-6.76290428500002));
#276770=CARTESIAN_POINT('Ctrl Pts',(-8.06015953800006,11.6,-6.76290428500002));
#276771=CARTESIAN_POINT('Ctrl Pts',(-8.05858613400006,15.2,-6.76202254000002));
#276772=CARTESIAN_POINT('Ctrl Pts',(-8.05858613400006,11.6,-6.76202254000002));
#276773=CARTESIAN_POINT('Ctrl Pts',(-8.05702003900005,15.2,-6.76114299200002));
#276774=CARTESIAN_POINT('Ctrl Pts',(-8.05702003900005,11.6,-6.76114299200002));
#276775=CARTESIAN_POINT('Ctrl Pts',(-8.05546126000005,15.2,-6.76026566400001));
#276776=CARTESIAN_POINT('Ctrl Pts',(-8.05546126000005,11.6,-6.76026566400001));
#276777=CARTESIAN_POINT('Ctrl Pts',(-8.05390980500006,15.2,-6.75939057400001));
#276778=CARTESIAN_POINT('Ctrl Pts',(-8.05390980500006,11.6,-6.75939057400001));
#276779=CARTESIAN_POINT('Ctrl Pts',(-8.05236568500005,15.2,-6.75851774000002));
#276780=CARTESIAN_POINT('Ctrl Pts',(-8.05236568500005,11.6,-6.75851774000002));
#276781=CARTESIAN_POINT('Ctrl Pts',(-8.05082890800006,15.2,-6.75764718400002));
#276782=CARTESIAN_POINT('Ctrl Pts',(-8.05082890800006,11.6,-6.75764718400002));
#276783=CARTESIAN_POINT('Ctrl Pts',(-8.04929948200006,15.2,-6.75677892300002));
#276784=CARTESIAN_POINT('Ctrl Pts',(-8.04929948200006,11.6,-6.75677892300002));
#276785=CARTESIAN_POINT('Ctrl Pts',(-8.04777741600006,15.2,-6.75591297900001));
#276786=CARTESIAN_POINT('Ctrl Pts',(-8.04777741600006,11.6,-6.75591297900001));
#276787=CARTESIAN_POINT('Ctrl Pts',(-8.04626271900006,15.2,-6.75504936900002));
#276788=CARTESIAN_POINT('Ctrl Pts',(-8.04626271900006,11.6,-6.75504936900002));
#276789=CARTESIAN_POINT('Ctrl Pts',(-8.04475540000006,15.2,-6.75418811400001));
#276790=CARTESIAN_POINT('Ctrl Pts',(-8.04475540000006,11.6,-6.75418811400001));
#276791=CARTESIAN_POINT('Ctrl Pts',(-8.04325546700005,15.2,-6.75332923500001));
#276792=CARTESIAN_POINT('Ctrl Pts',(-8.04325546700005,11.6,-6.75332923500001));
#276793=CARTESIAN_POINT('Ctrl Pts',(-8.04176292900006,15.2,-6.75247275100002));
#276794=CARTESIAN_POINT('Ctrl Pts',(-8.04176292900006,11.6,-6.75247275100002));
#276795=CARTESIAN_POINT('Ctrl Pts',(-8.04027779600006,15.2,-6.75161868200002));
#276796=CARTESIAN_POINT('Ctrl Pts',(-8.04027779600006,11.6,-6.75161868200002));
#276797=CARTESIAN_POINT('Ctrl Pts',(-8.03880007500006,15.2,-6.75076704800002));
#276798=CARTESIAN_POINT('Ctrl Pts',(-8.03880007500006,11.6,-6.75076704800002));
#276799=CARTESIAN_POINT('Ctrl Pts',(-8.03732977700006,15.2,-6.74991786800001));
#276800=CARTESIAN_POINT('Ctrl Pts',(-8.03732977700006,11.6,-6.74991786800001));
#276801=CARTESIAN_POINT('Ctrl Pts',(-8.03586690900006,15.2,-6.74907116500002));
#276802=CARTESIAN_POINT('Ctrl Pts',(-8.03586690900006,11.6,-6.74907116500002));
#276803=CARTESIAN_POINT('Ctrl Pts',(-8.03441148100006,15.2,-6.74822695700002));
#276804=CARTESIAN_POINT('Ctrl Pts',(-8.03441148100006,11.6,-6.74822695700002));
#276805=CARTESIAN_POINT('Ctrl Pts',(-8.03296350200006,15.2,-6.74738526600001));
#276806=CARTESIAN_POINT('Ctrl Pts',(-8.03296350200006,11.6,-6.74738526600001));
#276807=CARTESIAN_POINT('Ctrl Pts',(-8.03152298000006,15.2,-6.74654611000002));
#276808=CARTESIAN_POINT('Ctrl Pts',(-8.03152298000006,11.6,-6.74654611000002));
#276809=CARTESIAN_POINT('Ctrl Pts',(-8.03008992500006,15.2,-6.74570951200002));
#276810=CARTESIAN_POINT('Ctrl Pts',(-8.03008992500006,11.6,-6.74570951200002));
#276811=CARTESIAN_POINT('Ctrl Pts',(-8.02866434500006,15.2,-6.74487549200002));
#276812=CARTESIAN_POINT('Ctrl Pts',(-8.02866434500006,11.6,-6.74487549200002));
#276813=CARTESIAN_POINT('Ctrl Pts',(-8.02724625000005,15.2,-6.74404407000001));
#276814=CARTESIAN_POINT('Ctrl Pts',(-8.02724625000005,11.6,-6.74404407000001));
#276815=CARTESIAN_POINT('Ctrl Pts',(-8.02583565000005,15.2,-6.74321526700002));
#276816=CARTESIAN_POINT('Ctrl Pts',(-8.02583565000005,11.6,-6.74321526700002));
#276817=CARTESIAN_POINT('Ctrl Pts',(-8.02443255200006,15.2,-6.74238910500002));
#276818=CARTESIAN_POINT('Ctrl Pts',(-8.02443255200006,11.6,-6.74238910500002));
#276819=CARTESIAN_POINT('Ctrl Pts',(-8.02303696600006,15.2,-6.74156560400001));
#276820=CARTESIAN_POINT('Ctrl Pts',(-8.02303696600006,11.6,-6.74156560400001));
#276821=CARTESIAN_POINT('Ctrl Pts',(-8.02164890100006,15.2,-6.74074478500001));
#276822=CARTESIAN_POINT('Ctrl Pts',(-8.02164890100006,11.6,-6.74074478500001));
#276823=CARTESIAN_POINT('Ctrl Pts',(-8.02026836500006,15.2,-6.73992667000002));
#276824=CARTESIAN_POINT('Ctrl Pts',(-8.02026836500006,11.6,-6.73992667000002));
#276825=CARTESIAN_POINT('Ctrl Pts',(-8.01889537100006,15.2,-6.73911127900002));
#276826=CARTESIAN_POINT('Ctrl Pts',(-8.01889537100006,11.6,-6.73911127900002));
#276827=CARTESIAN_POINT('Ctrl Pts',(-8.01752992300005,15.2,-6.73829863500002));
#276828=CARTESIAN_POINT('Ctrl Pts',(-8.01752992300005,11.6,-6.73829863500002));
#276829=CARTESIAN_POINT('Ctrl Pts',(-8.01617203400006,15.2,-6.73748875800002));
#276830=CARTESIAN_POINT('Ctrl Pts',(-8.01617203400006,11.6,-6.73748875800002));
#276831=CARTESIAN_POINT('Ctrl Pts',(-8.01482171200006,15.2,-6.73668166900002));
#276832=CARTESIAN_POINT('Ctrl Pts',(-8.01482171200006,11.6,-6.73668166900002));
#276833=CARTESIAN_POINT('Ctrl Pts',(-8.01347896700005,15.2,-6.73587739300002));
#276834=CARTESIAN_POINT('Ctrl Pts',(-8.01347896700005,11.6,-6.73587739300002));
#276835=CARTESIAN_POINT('Ctrl Pts',(-8.01214380700005,15.2,-6.73507594700002));
#276836=CARTESIAN_POINT('Ctrl Pts',(-8.01214380700005,11.6,-6.73507594700002));
#276837=CARTESIAN_POINT('Ctrl Pts',(-8.01081624200006,15.2,-6.73427735600002));
#276838=CARTESIAN_POINT('Ctrl Pts',(-8.01081624200006,11.6,-6.73427735600002));
#276839=CARTESIAN_POINT('Ctrl Pts',(-8.00949628200006,15.2,-6.73348164200001));
#276840=CARTESIAN_POINT('Ctrl Pts',(-8.00949628200006,11.6,-6.73348164200001));
#276841=CARTESIAN_POINT('Ctrl Pts',(-8.00818393600006,15.2,-6.73268882500001));
#276842=CARTESIAN_POINT('Ctrl Pts',(-8.00818393600006,11.6,-6.73268882500001));
#276843=CARTESIAN_POINT('Ctrl Pts',(-8.00687921200005,15.2,-6.73189892800002));
#276844=CARTESIAN_POINT('Ctrl Pts',(-8.00687921200005,11.6,-6.73189892800002));
#276845=CARTESIAN_POINT('Ctrl Pts',(-8.00558212100006,15.2,-6.73111197200001));
#276846=CARTESIAN_POINT('Ctrl Pts',(-8.00558212100006,11.6,-6.73111197200001));
#276847=CARTESIAN_POINT('Ctrl Pts',(-8.00429267200006,15.2,-6.73032798200002));
#276848=CARTESIAN_POINT('Ctrl Pts',(-8.00429267200006,11.6,-6.73032798200002));
#276849=CARTESIAN_POINT('Ctrl Pts',(-8.00301087500005,15.2,-6.72954697800002));
#276850=CARTESIAN_POINT('Ctrl Pts',(-8.00301087500005,11.6,-6.72954697800002));
#276851=CARTESIAN_POINT('Ctrl Pts',(-8.00173673800006,15.2,-6.72876898400002));
#276852=CARTESIAN_POINT('Ctrl Pts',(-8.00173673800006,11.6,-6.72876898400002));
#276853=CARTESIAN_POINT('Ctrl Pts',(-8.00047027300005,15.2,-6.72799402200001));
#276854=CARTESIAN_POINT('Ctrl Pts',(-8.00047027300005,11.6,-6.72799402200001));
#276855=CARTESIAN_POINT('Ctrl Pts',(-7.99921148700006,15.2,-6.72722211400002));
#276856=CARTESIAN_POINT('Ctrl Pts',(-7.99921148700006,11.6,-6.72722211400002));
#276857=CARTESIAN_POINT('Ctrl Pts',(-7.99796039100006,15.2,-6.72645328300002));
#276858=CARTESIAN_POINT('Ctrl Pts',(-7.99796039100006,11.6,-6.72645328300002));
#276859=CARTESIAN_POINT('Ctrl Pts',(-7.99671699500006,15.2,-6.72568755200002));
#276860=CARTESIAN_POINT('Ctrl Pts',(-7.99671699500006,11.6,-6.72568755200002));
#276861=CARTESIAN_POINT('Ctrl Pts',(-7.99548130800006,15.2,-6.72492494400001));
#276862=CARTESIAN_POINT('Ctrl Pts',(-7.99548130800006,11.6,-6.72492494400001));
#276863=CARTESIAN_POINT('Ctrl Pts',(-7.99425333800006,15.2,-6.72416548300002));
#276864=CARTESIAN_POINT('Ctrl Pts',(-7.99425333800006,11.6,-6.72416548300002));
#276865=CARTESIAN_POINT('Ctrl Pts',(-7.99303309800005,15.2,-6.72340919000002));
#276866=CARTESIAN_POINT('Ctrl Pts',(-7.99303309800005,11.6,-6.72340919000002));
#276867=CARTESIAN_POINT('Ctrl Pts',(-7.99182059500006,15.2,-6.72265608900001));
#276868=CARTESIAN_POINT('Ctrl Pts',(-7.99182059500006,11.6,-6.72265608900001));
#276869=CARTESIAN_POINT('Ctrl Pts',(-7.99061584100006,15.2,-6.72190620500002));
#276870=CARTESIAN_POINT('Ctrl Pts',(-7.99061584100006,11.6,-6.72190620500002));
#276871=CARTESIAN_POINT('Ctrl Pts',(-7.98941884300006,15.2,-6.72115955900002));
#276872=CARTESIAN_POINT('Ctrl Pts',(-7.98941884300006,11.6,-6.72115955900002));
#276873=CARTESIAN_POINT('Ctrl Pts',(-7.98822961400005,15.2,-6.72041617700001));
#276874=CARTESIAN_POINT('Ctrl Pts',(-7.98822961400005,11.6,-6.72041617700001));
#276875=CARTESIAN_POINT('Ctrl Pts',(-7.98704816100006,15.2,-6.71967608000001));
#276876=CARTESIAN_POINT('Ctrl Pts',(-7.98704816100006,11.6,-6.71967608000001));
#276877=CARTESIAN_POINT('Ctrl Pts',(-7.98587449600006,15.2,-6.71893929400002));
#276878=CARTESIAN_POINT('Ctrl Pts',(-7.98587449600006,11.6,-6.71893929400002));
#276879=CARTESIAN_POINT('Ctrl Pts',(-7.98470862800006,15.2,-6.71820584100002));
#276880=CARTESIAN_POINT('Ctrl Pts',(-7.98470862800006,11.6,-6.71820584100002));
#276881=CARTESIAN_POINT('Ctrl Pts',(-7.98355056700006,15.2,-6.71747574700002));
#276882=CARTESIAN_POINT('Ctrl Pts',(-7.98355056700006,11.6,-6.71747574700002));
#276883=CARTESIAN_POINT('Ctrl Pts',(-7.98240032200006,15.2,-6.71674903500002));
#276884=CARTESIAN_POINT('Ctrl Pts',(-7.98240032200006,11.6,-6.71674903500002));
#276885=CARTESIAN_POINT('Ctrl Pts',(-7.98125790500006,15.2,-6.71602572900002));
#276886=CARTESIAN_POINT('Ctrl Pts',(-7.98125790500006,11.6,-6.71602572900002));
#276887=CARTESIAN_POINT('Ctrl Pts',(-7.98012332400006,15.2,-6.71530585300002));
#276888=CARTESIAN_POINT('Ctrl Pts',(-7.98012332400006,11.6,-6.71530585300002));
#276889=CARTESIAN_POINT('Ctrl Pts',(-7.97899659000005,15.2,-6.71458943300002));
#276890=CARTESIAN_POINT('Ctrl Pts',(-7.97899659000005,11.6,-6.71458943300002));
#276891=CARTESIAN_POINT('Ctrl Pts',(-7.97787771400006,15.2,-6.71387649200001));
#276892=CARTESIAN_POINT('Ctrl Pts',(-7.97787771400006,11.6,-6.71387649200001));
#276893=CARTESIAN_POINT('Ctrl Pts',(-7.97676670400006,15.2,-6.71316705500002));
#276894=CARTESIAN_POINT('Ctrl Pts',(-7.97676670400006,11.6,-6.71316705500002));
#276895=CARTESIAN_POINT('Ctrl Pts',(-7.97566357200005,15.2,-6.71246114600001));
#276896=CARTESIAN_POINT('Ctrl Pts',(-7.97566357200005,11.6,-6.71246114600001));
#276897=CARTESIAN_POINT('Ctrl Pts',(-7.97456832700006,15.2,-6.71175879200002));
#276898=CARTESIAN_POINT('Ctrl Pts',(-7.97456832700006,11.6,-6.71175879200002));
#276899=CARTESIAN_POINT('Ctrl Pts',(-7.97348098000005,15.2,-6.71106001600001));
#276900=CARTESIAN_POINT('Ctrl Pts',(-7.97348098000005,11.6,-6.71106001600001));
#276901=CARTESIAN_POINT('Ctrl Pts',(-7.97240154100006,15.2,-6.71036484500001));
#276902=CARTESIAN_POINT('Ctrl Pts',(-7.97240154100006,11.6,-6.71036484500001));
#276903=CARTESIAN_POINT('Ctrl Pts',(-7.97133002000006,15.2,-6.70967330200002));
#276904=CARTESIAN_POINT('Ctrl Pts',(-7.97133002000006,11.6,-6.70967330200002));
#276905=CARTESIAN_POINT('Ctrl Pts',(-7.97026642700006,15.2,-6.70898541300001));
#276906=CARTESIAN_POINT('Ctrl Pts',(-7.97026642700006,11.6,-6.70898541300001));
#276907=CARTESIAN_POINT('Ctrl Pts',(-7.96921077400006,15.2,-6.70830120300002));
#276908=CARTESIAN_POINT('Ctrl Pts',(-7.96921077400006,11.6,-6.70830120300002));
#276909=CARTESIAN_POINT('Ctrl Pts',(-7.96816307000006,15.2,-6.70762070000002));
#276910=CARTESIAN_POINT('Ctrl Pts',(-7.96816307000006,11.6,-6.70762070000002));
#276911=CARTESIAN_POINT('Ctrl Pts',(-7.96712332500006,15.2,-6.70694392700002));
#276912=CARTESIAN_POINT('Ctrl Pts',(-7.96712332500006,11.6,-6.70694392700002));
#276913=CARTESIAN_POINT('Ctrl Pts',(-7.96609155000005,15.2,-6.70627091100001));
#276914=CARTESIAN_POINT('Ctrl Pts',(-7.96609155000005,11.6,-6.70627091100001));
#276915=CARTESIAN_POINT('Ctrl Pts',(-7.96506775600006,15.2,-6.70560167700001));
#276916=CARTESIAN_POINT('Ctrl Pts',(-7.96506775600006,11.6,-6.70560167700001));
#276917=CARTESIAN_POINT('Ctrl Pts',(-7.96405195200006,15.2,-6.70493625300002));
#276918=CARTESIAN_POINT('Ctrl Pts',(-7.96405195200006,11.6,-6.70493625300002));
#276919=CARTESIAN_POINT('Ctrl Pts',(-7.96304415000006,15.2,-6.70427466300002));
#276920=CARTESIAN_POINT('Ctrl Pts',(-7.96304415000006,11.6,-6.70427466300002));
#276921=CARTESIAN_POINT('Ctrl Pts',(-7.96204436100006,15.2,-6.70361693500002));
#276922=CARTESIAN_POINT('Ctrl Pts',(-7.96204436100006,11.6,-6.70361693500002));
#276923=CARTESIAN_POINT('Ctrl Pts',(-7.96105259400005,15.2,-6.70296309300002));
#276924=CARTESIAN_POINT('Ctrl Pts',(-7.96105259400005,11.6,-6.70296309300002));
#276925=CARTESIAN_POINT('Ctrl Pts',(-7.96006886100006,15.2,-6.70231316600002));
#276926=CARTESIAN_POINT('Ctrl Pts',(-7.96006886100006,11.6,-6.70231316600002));
#276927=CARTESIAN_POINT('Ctrl Pts',(-7.95909317200006,15.2,-6.70166718000001));
#276928=CARTESIAN_POINT('Ctrl Pts',(-7.95909317200006,11.6,-6.70166718000001));
#276929=CARTESIAN_POINT('Ctrl Pts',(-7.95812553700006,15.2,-6.70102516100001));
#276930=CARTESIAN_POINT('Ctrl Pts',(-7.95812553700006,11.6,-6.70102516100001));
#276931=CARTESIAN_POINT('Ctrl Pts',(-7.95716596800006,15.2,-6.70038713600002));
#276932=CARTESIAN_POINT('Ctrl Pts',(-7.95716596800006,11.6,-6.70038713600002));
#276933=CARTESIAN_POINT('Ctrl Pts',(-7.95621447600006,15.2,-6.69975313400001));
#276934=CARTESIAN_POINT('Ctrl Pts',(-7.95621447600006,11.6,-6.69975313400001));
#276935=CARTESIAN_POINT('Ctrl Pts',(-7.95527107000006,15.2,-6.69912317900001));
#276936=CARTESIAN_POINT('Ctrl Pts',(-7.95527107000006,11.6,-6.69912317900001));
#276937=CARTESIAN_POINT('Ctrl Pts',(-7.95433576200006,15.2,-6.69849730100001));
#276938=CARTESIAN_POINT('Ctrl Pts',(-7.95433576200006,11.6,-6.69849730100001));
#276939=CARTESIAN_POINT('Ctrl Pts',(-7.95340856400006,15.2,-6.69787552700001));
#276940=CARTESIAN_POINT('Ctrl Pts',(-7.95340856400006,11.6,-6.69787552700001));
#276941=CARTESIAN_POINT('Ctrl Pts',(-7.95248948500006,15.2,-6.69725788300001));
#276942=CARTESIAN_POINT('Ctrl Pts',(-7.95248948500006,11.6,-6.69725788300001));
#276943=CARTESIAN_POINT('Ctrl Pts',(-7.95157853800006,15.2,-6.69664439800002));
#276944=CARTESIAN_POINT('Ctrl Pts',(-7.95157853800006,11.6,-6.69664439800002));
#276945=CARTESIAN_POINT('Ctrl Pts',(-7.95067573200006,15.2,-6.69603510000002));
#276946=CARTESIAN_POINT('Ctrl Pts',(-7.95067573200006,11.6,-6.69603510000002));
#276947=CARTESIAN_POINT('Ctrl Pts',(-7.94978107900006,15.2,-6.69543001700001));
#276948=CARTESIAN_POINT('Ctrl Pts',(-7.94978107900006,11.6,-6.69543001700001));
#276949=CARTESIAN_POINT('Ctrl Pts',(-7.94889459000006,15.2,-6.69482917500002));
#276950=CARTESIAN_POINT('Ctrl Pts',(-7.94889459000006,11.6,-6.69482917500002));
#276951=CARTESIAN_POINT('Ctrl Pts',(-7.94801627800006,15.2,-6.69423260500002));
#276952=CARTESIAN_POINT('Ctrl Pts',(-7.94801627800006,11.6,-6.69423260500002));
#276953=CARTESIAN_POINT('Ctrl Pts',(-7.94714615000006,15.2,-6.69364033500001));
#276954=CARTESIAN_POINT('Ctrl Pts',(-7.94714615000006,11.6,-6.69364033500001));
#276955=CARTESIAN_POINT('Ctrl Pts',(-7.94628422000006,15.2,-6.69305239200002));
#276956=CARTESIAN_POINT('Ctrl Pts',(-7.94628422000006,11.6,-6.69305239200002));
#276957=CARTESIAN_POINT('Ctrl Pts',(-7.94543050000006,15.2,-6.69246880700002));
#276958=CARTESIAN_POINT('Ctrl Pts',(-7.94543050000006,11.6,-6.69246880700002));
#276959=CARTESIAN_POINT('Ctrl Pts',(-7.94458499900006,15.2,-6.69188960600002));
#276960=CARTESIAN_POINT('Ctrl Pts',(-7.94458499900006,11.6,-6.69188960600002));
#276961=CARTESIAN_POINT('Ctrl Pts',(-7.94374773100006,15.2,-6.69131482000001));
#276962=CARTESIAN_POINT('Ctrl Pts',(-7.94374773100006,11.6,-6.69131482000001));
#276963=CARTESIAN_POINT('Ctrl Pts',(-7.94291870400006,15.2,-6.69074447800002));
#276964=CARTESIAN_POINT('Ctrl Pts',(-7.94291870400006,11.6,-6.69074447800002));
#276965=CARTESIAN_POINT('Ctrl Pts',(-7.94209793300006,15.2,-6.69017860900002));
#276966=CARTESIAN_POINT('Ctrl Pts',(-7.94209793300006,11.6,-6.69017860900002));
#276967=CARTESIAN_POINT('Ctrl Pts',(-7.94128542700006,15.2,-6.68961724100001));
#276968=CARTESIAN_POINT('Ctrl Pts',(-7.94128542700006,11.6,-6.68961724100001));
#276969=CARTESIAN_POINT('Ctrl Pts',(-7.94048119900006,15.2,-6.68906040700002));
#276970=CARTESIAN_POINT('Ctrl Pts',(-7.94048119900006,11.6,-6.68906040700002));
#276971=CARTESIAN_POINT('Ctrl Pts',(-7.93968525900006,15.2,-6.68850813300002));
#276972=CARTESIAN_POINT('Ctrl Pts',(-7.93968525900006,11.6,-6.68850813300002));
#276973=CARTESIAN_POINT('Ctrl Pts',(-7.93889762000005,15.2,-6.68796045200001));
#276974=CARTESIAN_POINT('Ctrl Pts',(-7.93889762000005,11.6,-6.68796045200001));
#276975=CARTESIAN_POINT('Ctrl Pts',(-7.93811829300005,15.2,-6.68741739000002));
#276976=CARTESIAN_POINT('Ctrl Pts',(-7.93811829300005,11.6,-6.68741739000002));
#276977=CARTESIAN_POINT('Ctrl Pts',(-7.93734729000006,15.2,-6.68687898200002));
#276978=CARTESIAN_POINT('Ctrl Pts',(-7.93734729000006,11.6,-6.68687898200002));
#276979=CARTESIAN_POINT('Ctrl Pts',(-7.93658462200005,15.2,-6.68634525500002));
#276980=CARTESIAN_POINT('Ctrl Pts',(-7.93658462200005,11.6,-6.68634525500002));
#276981=CARTESIAN_POINT('Ctrl Pts',(-7.93583464600006,15.2,-6.68581928800001));
#276982=CARTESIAN_POINT('Ctrl Pts',(-7.93583464600006,11.6,-6.68581928800001));
#276983=CARTESIAN_POINT('Ctrl Pts',(-7.93524212700006,15.2,-6.68540286400002));
#276984=CARTESIAN_POINT('Ctrl Pts',(-7.93524212700006,11.6,-6.68540286400002));
#276985=CARTESIAN_POINT('Ctrl Pts',(-7.93480250500006,15.2,-6.68509340800002));
#276986=CARTESIAN_POINT('Ctrl Pts',(-7.93480250500006,11.6,-6.68509340800002));
#276987=CARTESIAN_POINT('Ctrl Pts',(-7.93451247300006,15.2,-6.68488903500001));
#276988=CARTESIAN_POINT('Ctrl Pts',(-7.93451247300006,11.6,-6.68488903500001));
#276989=CARTESIAN_POINT('Ctrl Pts',(-7.93436997000006,15.2,-6.68478856700002));
#276990=CARTESIAN_POINT('Ctrl Pts',(-7.93436997000006,11.6,-6.68478856700002));
#276991=CARTESIAN_POINT('',(-7.93436997000006,12.2,-6.68478856700002));
#276992=CARTESIAN_POINT('',(-7.93436997000006,15.2,-6.68478856700002));
#276993=CARTESIAN_POINT('',(-7.93436997000006,12.2,-6.68478856700002));
#276994=CARTESIAN_POINT('Ctrl Pts',(-9.03946594400006,12.2,-7.10901226900001));
#276995=CARTESIAN_POINT('Ctrl Pts',(-9.03871859600006,12.2,-7.10885083600001));
#276996=CARTESIAN_POINT('Ctrl Pts',(-9.03722439200006,12.2,-7.10852778400002));
#276997=CARTESIAN_POINT('Ctrl Pts',(-9.03498456200006,12.2,-7.10804263900001));
#276998=CARTESIAN_POINT('Ctrl Pts',(-9.03200107200006,12.2,-7.10739465100002));
#276999=CARTESIAN_POINT('Ctrl Pts',(-9.02827662900006,12.2,-7.10658278400001));
#277000=CARTESIAN_POINT('Ctrl Pts',(-9.02455710700006,12.2,-7.10576903500002));
#277001=CARTESIAN_POINT('Ctrl Pts',(-9.02084250600005,12.2,-7.10495340800002));
#277002=CARTESIAN_POINT('Ctrl Pts',(-9.01713282900005,12.2,-7.10413590400002));
#277003=CARTESIAN_POINT('Ctrl Pts',(-9.01342808000006,12.2,-7.10331652800001));
#277004=CARTESIAN_POINT('Ctrl Pts',(-9.00972826500006,12.2,-7.10249528800002));
#277005=CARTESIAN_POINT('Ctrl Pts',(-9.00603338900006,12.2,-7.10167218900001));
#277006=CARTESIAN_POINT('Ctrl Pts',(-9.00234345900006,12.2,-7.10084724000002));
#277007=CARTESIAN_POINT('Ctrl Pts',(-8.99865848200006,12.2,-7.10002045100002));
#277008=CARTESIAN_POINT('Ctrl Pts',(-8.99497846500006,12.2,-7.09919182900002));
#277009=CARTESIAN_POINT('Ctrl Pts',(-8.99130341600006,12.2,-7.09836138400001));
#277010=CARTESIAN_POINT('Ctrl Pts',(-8.98763333900006,12.2,-7.09752912300001));
#277011=CARTESIAN_POINT('Ctrl Pts',(-8.98396824000006,12.2,-7.09669505000001));
#277012=CARTESIAN_POINT('Ctrl Pts',(-8.98030812400006,12.2,-7.09585917500001));
#277013=CARTESIAN_POINT('Ctrl Pts',(-8.97665299700006,12.2,-7.09502150300001));
#277014=CARTESIAN_POINT('Ctrl Pts',(-8.97300286400006,12.2,-7.09418203900002));
#277015=CARTESIAN_POINT('Ctrl Pts',(-8.96935772900006,12.2,-7.09334079100002));
#277016=CARTESIAN_POINT('Ctrl Pts',(-8.96571759800005,12.2,-7.09249776700001));
#277017=CARTESIAN_POINT('Ctrl Pts',(-8.96208247800006,12.2,-7.09165297200002));
#277018=CARTESIAN_POINT('Ctrl Pts',(-8.95845237400006,12.2,-7.09080641500002));
#277019=CARTESIAN_POINT('Ctrl Pts',(-8.95482729200006,12.2,-7.08995810200002));
#277020=CARTESIAN_POINT('Ctrl Pts',(-8.95120723800006,12.2,-7.08910804300002));
#277021=CARTESIAN_POINT('Ctrl Pts',(-8.94759221900006,12.2,-7.08825624300002));
#277022=CARTESIAN_POINT('Ctrl Pts',(-8.94398223900006,12.2,-7.08740271100002));
#277023=CARTESIAN_POINT('Ctrl Pts',(-8.94037730400006,12.2,-7.08654745200001));
#277024=CARTESIAN_POINT('Ctrl Pts',(-8.93677742100006,12.2,-7.08569047400001));
#277025=CARTESIAN_POINT('Ctrl Pts',(-8.93318259400005,12.2,-7.08483178600002));
#277026=CARTESIAN_POINT('Ctrl Pts',(-8.92959282900006,12.2,-7.08397139300001));
#277027=CARTESIAN_POINT('Ctrl Pts',(-8.92600813200006,12.2,-7.08310930200001));
#277028=CARTESIAN_POINT('Ctrl Pts',(-8.92242850800006,12.2,-7.08224552100001));
#277029=CARTESIAN_POINT('Ctrl Pts',(-8.91885396500006,12.2,-7.08138005800001));
#277030=CARTESIAN_POINT('Ctrl Pts',(-8.91528450600006,12.2,-7.08051292100001));
#277031=CARTESIAN_POINT('Ctrl Pts',(-8.91172013800006,12.2,-7.07964411500001));
#277032=CARTESIAN_POINT('Ctrl Pts',(-8.90816086700006,12.2,-7.07877364900002));
#277033=CARTESIAN_POINT('Ctrl Pts',(-8.90460669800006,12.2,-7.07790152900002));
#277034=CARTESIAN_POINT('Ctrl Pts',(-8.90105763800005,12.2,-7.07702776600001));
#277035=CARTESIAN_POINT('Ctrl Pts',(-8.89751369200006,12.2,-7.07615236300001));
#277036=CARTESIAN_POINT('Ctrl Pts',(-8.89397486600006,12.2,-7.07527533000002));
#277037=CARTESIAN_POINT('Ctrl Pts',(-8.89044116400006,12.2,-7.07439667400001));
#277038=CARTESIAN_POINT('Ctrl Pts',(-8.88691259400006,12.2,-7.07351640200002));
#277039=CARTESIAN_POINT('Ctrl Pts',(-8.88338916200006,12.2,-7.07263452100002));
#277040=CARTESIAN_POINT('Ctrl Pts',(-8.87987087300005,12.2,-7.07175104100001));
#277041=CARTESIAN_POINT('Ctrl Pts',(-8.87635773200006,12.2,-7.07086596600002));
#277042=CARTESIAN_POINT('Ctrl Pts',(-8.87284974500006,12.2,-7.06997930700001));
#277043=CARTESIAN_POINT('Ctrl Pts',(-8.86934691800005,12.2,-7.06909107000002));
#277044=CARTESIAN_POINT('Ctrl Pts',(-8.86584925900006,12.2,-7.06820126200002));
#277045=CARTESIAN_POINT('Ctrl Pts',(-8.86235677000006,12.2,-7.06730989100001));
#277046=CARTESIAN_POINT('Ctrl Pts',(-8.85886945900005,12.2,-7.06641696400002));
#277047=CARTESIAN_POINT('Ctrl Pts',(-8.85538733200006,12.2,-7.06552249100002));
#277048=CARTESIAN_POINT('Ctrl Pts',(-8.85191039400006,12.2,-7.06462647700001));
#277049=CARTESIAN_POINT('Ctrl Pts',(-8.84843865100006,12.2,-7.06372893100002));
#277050=CARTESIAN_POINT('Ctrl Pts',(-8.84497210900006,12.2,-7.06282986200002));
#277051=CARTESIAN_POINT('Ctrl Pts',(-8.84151077400006,12.2,-7.06192927400001));
#277052=CARTESIAN_POINT('Ctrl Pts',(-8.83805465100006,12.2,-7.06102717900002));
#277053=CARTESIAN_POINT('Ctrl Pts',(-8.83391356635052,12.2,-7.05994286263941));
#277054=CARTESIAN_POINT('Ctrl Pts',(-8.82978031732483,12.2,-7.05885630368031));
#277055=CARTESIAN_POINT('Ctrl Pts',(-8.82565491667528,12.2,-7.05776752231972));
#277056=CARTESIAN_POINT('Ctrl Pts',(-8.82153737602361,12.2,-7.05667653245971));
#277057=CARTESIAN_POINT('Ctrl Pts',(-8.81742770700006,12.2,-7.05558334800001));
#277058=CARTESIAN_POINT('Ctrl Pts',(-8.81400823600006,12.2,-7.05467090600001));
#277059=CARTESIAN_POINT('Ctrl Pts',(-8.81059402400006,12.2,-7.05375701900002));
#277060=CARTESIAN_POINT('Ctrl Pts',(-8.80718507800006,12.2,-7.05284169300001));
#277061=CARTESIAN_POINT('Ctrl Pts',(-8.80378140200006,12.2,-7.05192493600002));
#277062=CARTESIAN_POINT('Ctrl Pts',(-8.80038300400006,12.2,-7.05100675600002));
#277063=CARTESIAN_POINT('Ctrl Pts',(-8.79698988900006,12.2,-7.05008716200001));
#277064=CARTESIAN_POINT('Ctrl Pts',(-8.79360206200005,12.2,-7.04916616100002));
#277065=CARTESIAN_POINT('Ctrl Pts',(-8.79021953000005,12.2,-7.04824376100002));
#277066=CARTESIAN_POINT('Ctrl Pts',(-8.78684229800006,12.2,-7.04731997100002));
#277067=CARTESIAN_POINT('Ctrl Pts',(-8.78347037400006,12.2,-7.04639479800001));
#277068=CARTESIAN_POINT('Ctrl Pts',(-8.78010376100006,12.2,-7.04546825000002));
#277069=CARTESIAN_POINT('Ctrl Pts',(-8.77674246700006,12.2,-7.04454033500002));
#277070=CARTESIAN_POINT('Ctrl Pts',(-8.77338649600006,12.2,-7.04361106300002));
#277071=CARTESIAN_POINT('Ctrl Pts',(-8.77003585700006,12.2,-7.04268044000001));
#277072=CARTESIAN_POINT('Ctrl Pts',(-8.76669055200006,12.2,-7.04174847400001));
#277073=CARTESIAN_POINT('Ctrl Pts',(-8.76335059000006,12.2,-7.04081517500001));
#277074=CARTESIAN_POINT('Ctrl Pts',(-8.76001597600006,12.2,-7.03988055000002));
#277075=CARTESIAN_POINT('Ctrl Pts',(-8.75668671600006,12.2,-7.03894460800001));
#277076=CARTESIAN_POINT('Ctrl Pts',(-8.75336281400006,12.2,-7.03800735500002));
#277077=CARTESIAN_POINT('Ctrl Pts',(-8.75004427900006,12.2,-7.03706880200002));
#277078=CARTESIAN_POINT('Ctrl Pts',(-8.74673111600006,12.2,-7.03612895700001));
#277079=CARTESIAN_POINT('Ctrl Pts',(-8.74342333000006,12.2,-7.03518782500002));
#277080=CARTESIAN_POINT('Ctrl Pts',(-8.74012092800006,12.2,-7.03424541800001));
#277081=CARTESIAN_POINT('Ctrl Pts',(-8.73682391500006,12.2,-7.03330174300002));
#277082=CARTESIAN_POINT('Ctrl Pts',(-8.73353229800006,12.2,-7.03235680900002));
#277083=CARTESIAN_POINT('Ctrl Pts',(-8.73024608200006,12.2,-7.03141062300002));
#277084=CARTESIAN_POINT('Ctrl Pts',(-8.72696527300005,12.2,-7.03046319400002));
#277085=CARTESIAN_POINT('Ctrl Pts',(-8.72368987800006,12.2,-7.02951453100002));
#277086=CARTESIAN_POINT('Ctrl Pts',(-8.72041990300006,12.2,-7.02856464100002));
#277087=CARTESIAN_POINT('Ctrl Pts',(-8.71715535200006,12.2,-7.02761353400001));
#277088=CARTESIAN_POINT('Ctrl Pts',(-8.71389623400006,12.2,-7.02666121800001));
#277089=CARTESIAN_POINT('Ctrl Pts',(-8.71064255200006,12.2,-7.02570770100002));
#277090=CARTESIAN_POINT('Ctrl Pts',(-8.70739431400006,12.2,-7.02475299200002));
#277091=CARTESIAN_POINT('Ctrl Pts',(-8.70415152500006,12.2,-7.02379710000002));
#277092=CARTESIAN_POINT('Ctrl Pts',(-8.70091419100006,12.2,-7.02284003200001));
#277093=CARTESIAN_POINT('Ctrl Pts',(-8.69768231900006,12.2,-7.02188179800002));
#277094=CARTESIAN_POINT('Ctrl Pts',(-8.69445591400006,12.2,-7.02092240600001));
#277095=CARTESIAN_POINT('Ctrl Pts',(-8.69123498300005,12.2,-7.01996186500002));
#277096=CARTESIAN_POINT('Ctrl Pts',(-8.68801953200006,12.2,-7.01900018400002));
#277097=CARTESIAN_POINT('Ctrl Pts',(-8.68480956600006,12.2,-7.01803737000001));
#277098=CARTESIAN_POINT('Ctrl Pts',(-8.68160509100005,12.2,-7.01707343300002));
#277099=CARTESIAN_POINT('Ctrl Pts',(-8.67840611400006,12.2,-7.01610838100001));
#277100=CARTESIAN_POINT('Ctrl Pts',(-8.67521264100005,12.2,-7.01514222400001));
#277101=CARTESIAN_POINT('Ctrl Pts',(-8.67202467700006,12.2,-7.01417496900002));
#277102=CARTESIAN_POINT('Ctrl Pts',(-8.66884222900006,12.2,-7.01320662700001));
#277103=CARTESIAN_POINT('Ctrl Pts',(-8.66566530400006,12.2,-7.01223720400002));
#277104=CARTESIAN_POINT('Ctrl Pts',(-8.66249390600006,12.2,-7.01126671100001));
#277105=CARTESIAN_POINT('Ctrl Pts',(-8.65932804200006,12.2,-7.01029515700001));
#277106=CARTESIAN_POINT('Ctrl Pts',(-8.65616771800006,12.2,-7.00932254900002));
#277107=CARTESIAN_POINT('Ctrl Pts',(-8.65301294000006,12.2,-7.00834889700002));
#277108=CARTESIAN_POINT('Ctrl Pts',(-8.64986371500006,12.2,-7.00737421000002));
#277109=CARTESIAN_POINT('Ctrl Pts',(-8.64672004800006,12.2,-7.00639849700002));
#277110=CARTESIAN_POINT('Ctrl Pts',(-8.64358194600005,12.2,-7.00542176600001));
#277111=CARTESIAN_POINT('Ctrl Pts',(-8.64044941400006,12.2,-7.00444402600001));
#277112=CARTESIAN_POINT('Ctrl Pts',(-8.63732245800006,12.2,-7.00346528800001));
#277113=CARTESIAN_POINT('Ctrl Pts',(-8.63420108600006,12.2,-7.00248556000002));
#277114=CARTESIAN_POINT('Ctrl Pts',(-8.63108530200006,12.2,-7.00150485000002));
#277115=CARTESIAN_POINT('Ctrl Pts',(-8.62797511400006,12.2,-7.00052316700001));
#277116=CARTESIAN_POINT('Ctrl Pts',(-8.62487052700006,12.2,-6.99954052200002));
#277117=CARTESIAN_POINT('Ctrl Pts',(-8.62177154800005,12.2,-6.99855692200002));
#277118=CARTESIAN_POINT('Ctrl Pts',(-8.61867818200006,12.2,-6.99757237900001));
#277119=CARTESIAN_POINT('Ctrl Pts',(-8.61559043500005,12.2,-6.99658689800001));
#277120=CARTESIAN_POINT('Ctrl Pts',(-8.61250831400006,12.2,-6.99560049200001));
#277121=CARTESIAN_POINT('Ctrl Pts',(-8.60943182500005,12.2,-6.99461316800001));
#277122=CARTESIAN_POINT('Ctrl Pts',(-8.60636097400005,12.2,-6.99362493600002));
#277123=CARTESIAN_POINT('Ctrl Pts',(-8.60329576800006,12.2,-6.99263580600002));
#277124=CARTESIAN_POINT('Ctrl Pts',(-8.60023621200006,12.2,-6.99164578600002));
#277125=CARTESIAN_POINT('Ctrl Pts',(-8.59718231200005,12.2,-6.99065488500001));
#277126=CARTESIAN_POINT('Ctrl Pts',(-8.59413407600006,12.2,-6.98966311400002));
#277127=CARTESIAN_POINT('Ctrl Pts',(-8.59109150900006,12.2,-6.98867048200002));
#277128=CARTESIAN_POINT('Ctrl Pts',(-8.58805461700006,12.2,-6.98767699600002));
#277129=CARTESIAN_POINT('Ctrl Pts',(-8.58502340600005,12.2,-6.98668266800002));
#277130=CARTESIAN_POINT('Ctrl Pts',(-8.58199788300006,12.2,-6.98568750700002));
#277131=CARTESIAN_POINT('Ctrl Pts',(-8.57897805400006,12.2,-6.98469152300002));
#277132=CARTESIAN_POINT('Ctrl Pts',(-8.57596392500006,12.2,-6.98369472200002));
#277133=CARTESIAN_POINT('Ctrl Pts',(-8.57295550200006,12.2,-6.98269711800001));
#277134=CARTESIAN_POINT('Ctrl Pts',(-8.56995279100006,12.2,-6.98169871900002));
#277135=CARTESIAN_POINT('Ctrl Pts',(-8.56695580000006,12.2,-6.98069953300001));
#277136=CARTESIAN_POINT('Ctrl Pts',(-8.56396453400006,12.2,-6.97969957100002));
#277137=CARTESIAN_POINT('Ctrl Pts',(-8.56097900000006,12.2,-6.97869884300002));
#277138=CARTESIAN_POINT('Ctrl Pts',(-8.55799920200005,12.2,-6.97769735700002));
#277139=CARTESIAN_POINT('Ctrl Pts',(-8.55502514900006,12.2,-6.97669512400001));
#277140=CARTESIAN_POINT('Ctrl Pts',(-8.55205684500006,12.2,-6.97569215300001));
#277141=CARTESIAN_POINT('Ctrl Pts',(-8.54909429800006,12.2,-6.97468845400002));
#277142=CARTESIAN_POINT('Ctrl Pts',(-8.54613751300005,12.2,-6.97368403700001));
#277143=CARTESIAN_POINT('Ctrl Pts',(-8.54318649800006,12.2,-6.97267891200001));
#277144=CARTESIAN_POINT('Ctrl Pts',(-8.54024125700005,12.2,-6.97167308800001));
#277145=CARTESIAN_POINT('Ctrl Pts',(-8.53730179800005,12.2,-6.97066657500002));
#277146=CARTESIAN_POINT('Ctrl Pts',(-8.53436812700006,12.2,-6.96965938200002));
#277147=CARTESIAN_POINT('Ctrl Pts',(-8.53144025100006,12.2,-6.96865152100001));
#277148=CARTESIAN_POINT('Ctrl Pts',(-8.52851817400006,12.2,-6.96764300000002));
#277149=CARTESIAN_POINT('Ctrl Pts',(-8.52560190400006,12.2,-6.96663382900002));
#277150=CARTESIAN_POINT('Ctrl Pts',(-8.52269144900006,12.2,-6.96562402000002));
#277151=CARTESIAN_POINT('Ctrl Pts',(-8.51978681100006,12.2,-6.96461358000001));
#277152=CARTESIAN_POINT('Ctrl Pts',(-8.51688800000005,12.2,-6.96360252200002));
#277153=CARTESIAN_POINT('Ctrl Pts',(-8.51399502100006,12.2,-6.96259085300002));
#277154=CARTESIAN_POINT('Ctrl Pts',(-8.51110788000006,12.2,-6.96157858500002));
#277155=CARTESIAN_POINT('Ctrl Pts',(-8.50822658400006,12.2,-6.96056572800002));
#277156=CARTESIAN_POINT('Ctrl Pts',(-8.50535113900006,12.2,-6.95955229100001));
#277157=CARTESIAN_POINT('Ctrl Pts',(-8.50248155100006,12.2,-6.95853828600002));
#277158=CARTESIAN_POINT('Ctrl Pts',(-8.49961782900006,12.2,-6.95752372000002));
#277159=CARTESIAN_POINT('Ctrl Pts',(-8.49675997600006,12.2,-6.95650860700002));
#277160=CARTESIAN_POINT('Ctrl Pts',(-8.49390800000006,12.2,-6.95549295400002));
#277161=CARTESIAN_POINT('Ctrl Pts',(-8.49106190600006,12.2,-6.95447677400002));
#277162=CARTESIAN_POINT('Ctrl Pts',(-8.48822170400006,12.2,-6.95346007500002));
#277163=CARTESIAN_POINT('Ctrl Pts',(-8.48538739600006,12.2,-6.95244286800002));
#277164=CARTESIAN_POINT('Ctrl Pts',(-8.48255899100005,12.2,-6.95142516400002));
#277165=CARTESIAN_POINT('Ctrl Pts',(-8.47973649400006,12.2,-6.95040697300002));
#277166=CARTESIAN_POINT('Ctrl Pts',(-8.47691991300006,12.2,-6.94938830400002));
#277167=CARTESIAN_POINT('Ctrl Pts',(-8.47410925300006,12.2,-6.94836916900002));
#277168=CARTESIAN_POINT('Ctrl Pts',(-8.47130452200006,12.2,-6.94734957900002));
#277169=CARTESIAN_POINT('Ctrl Pts',(-8.46850572600006,12.2,-6.94632954200002));
#277170=CARTESIAN_POINT('Ctrl Pts',(-8.46571286900006,12.2,-6.94530907100001));
#277171=CARTESIAN_POINT('Ctrl Pts',(-8.46292596100006,12.2,-6.94428817600001));
#277172=CARTESIAN_POINT('Ctrl Pts',(-8.46014500600005,12.2,-6.94326686700002));
#277173=CARTESIAN_POINT('Ctrl Pts',(-8.45737001200006,12.2,-6.94224515400002));
#277174=CARTESIAN_POINT('Ctrl Pts',(-8.45460098500006,12.2,-6.94122304900001));
#277175=CARTESIAN_POINT('Ctrl Pts',(-8.45183793100006,12.2,-6.94020056100002));
#277176=CARTESIAN_POINT('Ctrl Pts',(-8.44908085600006,12.2,-6.93917770200001));
#277177=CARTESIAN_POINT('Ctrl Pts',(-8.44632976900006,12.2,-6.93815448200001));
#277178=CARTESIAN_POINT('Ctrl Pts',(-8.44358467400006,12.2,-6.93713091300002));
#277179=CARTESIAN_POINT('Ctrl Pts',(-8.44084557900005,12.2,-6.93610700400002));
#277180=CARTESIAN_POINT('Ctrl Pts',(-8.43811248900005,12.2,-6.93508276600002));
#277181=CARTESIAN_POINT('Ctrl Pts',(-8.43538541200006,12.2,-6.93405821000002));
#277182=CARTESIAN_POINT('Ctrl Pts',(-8.43266435300006,12.2,-6.93303334900002));
#277183=CARTESIAN_POINT('Ctrl Pts',(-8.42994932200006,12.2,-6.93200819000002));
#277184=CARTESIAN_POINT('Ctrl Pts',(-8.42724032100006,12.2,-6.93098274800001));
#277185=CARTESIAN_POINT('Ctrl Pts',(-8.42453736000006,12.2,-6.92995703000002));
#277186=CARTESIAN_POINT('Ctrl Pts',(-8.42184044300006,12.2,-6.92893105000002));
#277187=CARTESIAN_POINT('Ctrl Pts',(-8.41914957900006,12.2,-6.92790481800002));
#277188=CARTESIAN_POINT('Ctrl Pts',(-8.41646477200005,12.2,-6.92687834500001));
#277189=CARTESIAN_POINT('Ctrl Pts',(-8.41378603100006,12.2,-6.92585164200001));
#277190=CARTESIAN_POINT('Ctrl Pts',(-8.41111336100006,12.2,-6.92482472000002));
#277191=CARTESIAN_POINT('Ctrl Pts',(-8.40844676900005,12.2,-6.92379758900002));
#277192=CARTESIAN_POINT('Ctrl Pts',(-8.40578626200006,12.2,-6.92277026300002));
#277193=CARTESIAN_POINT('Ctrl Pts',(-8.40313184700006,12.2,-6.92174275100002));
#277194=CARTESIAN_POINT('Ctrl Pts',(-8.40048352900006,12.2,-6.92071506500002));
#277195=CARTESIAN_POINT('Ctrl Pts',(-8.39784131700006,12.2,-6.91968721500002));
#277196=CARTESIAN_POINT('Ctrl Pts',(-8.39520521500006,12.2,-6.91865921400002));
#277197=CARTESIAN_POINT('Ctrl Pts',(-8.39257523200006,12.2,-6.91763107400002));
#277198=CARTESIAN_POINT('Ctrl Pts',(-8.38995137300006,12.2,-6.91660280300002));
#277199=CARTESIAN_POINT('Ctrl Pts',(-8.38733364500006,12.2,-6.91557441500001));
#277200=CARTESIAN_POINT('Ctrl Pts',(-8.38472205600005,12.2,-6.91454592100002));
#277201=CARTESIAN_POINT('Ctrl Pts',(-8.38211661100006,12.2,-6.91351733200002));
#277202=CARTESIAN_POINT('Ctrl Pts',(-8.37951731800005,12.2,-6.91248865900001));
#277203=CARTESIAN_POINT('Ctrl Pts',(-8.37692418100006,12.2,-6.91145991600001));
#277204=CARTESIAN_POINT('Ctrl Pts',(-8.37433721100006,12.2,-6.91043111100001));
#277205=CARTESIAN_POINT('Ctrl Pts',(-8.37175641100006,12.2,-6.90940225800002));
#277206=CARTESIAN_POINT('Ctrl Pts',(-8.36918179000006,12.2,-6.90837336800002));
#277207=CARTESIAN_POINT('Ctrl Pts',(-8.36661335300006,12.2,-6.90734445300001));
#277208=CARTESIAN_POINT('Ctrl Pts',(-8.36405110900006,12.2,-6.90631552400002));
#277209=CARTESIAN_POINT('Ctrl Pts',(-8.36149506200006,12.2,-6.90528659300002));
#277210=CARTESIAN_POINT('Ctrl Pts',(-8.35894522100006,12.2,-6.90425767200002));
#277211=CARTESIAN_POINT('Ctrl Pts',(-8.35640159200006,12.2,-6.90322877200002));
#277212=CARTESIAN_POINT('Ctrl Pts',(-8.35386418000006,12.2,-6.90219990600001));
#277213=CARTESIAN_POINT('Ctrl Pts',(-8.35133299600006,12.2,-6.90117108400001));
#277214=CARTESIAN_POINT('Ctrl Pts',(-8.34880804200005,12.2,-6.90014232000002));
#277215=CARTESIAN_POINT('Ctrl Pts',(-8.34628932800005,12.2,-6.89911362500002));
#277216=CARTESIAN_POINT('Ctrl Pts',(-8.34377685900006,12.2,-6.89808501100002));
#277217=CARTESIAN_POINT('Ctrl Pts',(-8.34127064400005,12.2,-6.89705649000001));
#277218=CARTESIAN_POINT('Ctrl Pts',(-8.33877068700006,12.2,-6.89602807400002));
#277219=CARTESIAN_POINT('Ctrl Pts',(-8.33627699700006,12.2,-6.89499977500001));
#277220=CARTESIAN_POINT('Ctrl Pts',(-8.33378957900005,12.2,-6.89397160500001));
#277221=CARTESIAN_POINT('Ctrl Pts',(-8.33130844300005,12.2,-6.89294357600001));
#277222=CARTESIAN_POINT('Ctrl Pts',(-8.32883359200006,12.2,-6.89191570100002));
#277223=CARTESIAN_POINT('Ctrl Pts',(-8.32636503500006,12.2,-6.89088799200002));
#277224=CARTESIAN_POINT('Ctrl Pts',(-8.32390277900006,12.2,-6.88986046100001));
#277225=CARTESIAN_POINT('Ctrl Pts',(-8.32144683000006,12.2,-6.88883311900002));
#277226=CARTESIAN_POINT('Ctrl Pts',(-8.31899719600005,12.2,-6.88780598100001));
#277227=CARTESIAN_POINT('Ctrl Pts',(-8.31655388200006,12.2,-6.88677905700001));
#277228=CARTESIAN_POINT('Ctrl Pts',(-8.31411689600005,12.2,-6.88575236100001));
#277229=CARTESIAN_POINT('Ctrl Pts',(-8.31168624600006,12.2,-6.88472590400002));
#277230=CARTESIAN_POINT('Ctrl Pts',(-8.30926193800006,12.2,-6.88369969900001));
#277231=CARTESIAN_POINT('Ctrl Pts',(-8.30684397800006,12.2,-6.88267375900002));
#277232=CARTESIAN_POINT('Ctrl Pts',(-8.30443237500005,12.2,-6.88164809600002));
#277233=CARTESIAN_POINT('Ctrl Pts',(-8.30202713400006,12.2,-6.88062272300002));
#277234=CARTESIAN_POINT('Ctrl Pts',(-8.29962826300006,12.2,-6.87959765300001));
#277235=CARTESIAN_POINT('Ctrl Pts',(-8.29723576800006,12.2,-6.87857289700001));
#277236=CARTESIAN_POINT('Ctrl Pts',(-8.29484965700006,12.2,-6.87754847000001));
#277237=CARTESIAN_POINT('Ctrl Pts',(-8.29246993600006,12.2,-6.87652438300002));
#277238=CARTESIAN_POINT('Ctrl Pts',(-8.29009661400006,12.2,-6.87550064900002));
#277239=CARTESIAN_POINT('Ctrl Pts',(-8.28772969600006,12.2,-6.87447728100001));
#277240=CARTESIAN_POINT('Ctrl Pts',(-8.28536918900006,12.2,-6.87345429300001));
#277241=CARTESIAN_POINT('Ctrl Pts',(-8.28301510100006,12.2,-6.87243169500002));
#277242=CARTESIAN_POINT('Ctrl Pts',(-8.28066743900006,12.2,-6.87140950400002));
#277243=CARTESIAN_POINT('Ctrl Pts',(-8.27832621000006,12.2,-6.87038772900002));
#277244=CARTESIAN_POINT('Ctrl Pts',(-8.27599142100006,12.2,-6.86936638500002));
#277245=CARTESIAN_POINT('Ctrl Pts',(-8.27366307900006,12.2,-6.86834548500002));
#277246=CARTESIAN_POINT('Ctrl Pts',(-8.27134119000006,12.2,-6.86732504200001));
#277247=CARTESIAN_POINT('Ctrl Pts',(-8.26902576200006,12.2,-6.86630507000002));
#277248=CARTESIAN_POINT('Ctrl Pts',(-8.26671680300005,12.2,-6.86528558000001));
#277249=CARTESIAN_POINT('Ctrl Pts',(-8.26441431900006,12.2,-6.86426658600002));
#277250=CARTESIAN_POINT('Ctrl Pts',(-8.26211831700006,12.2,-6.86324810400002));
#277251=CARTESIAN_POINT('Ctrl Pts',(-8.25982880500005,12.2,-6.86223014300002));
#277252=CARTESIAN_POINT('Ctrl Pts',(-8.25754578900005,12.2,-6.86121271800002));
#277253=CARTESIAN_POINT('Ctrl Pts',(-8.25526927700006,12.2,-6.86019584300002));
#277254=CARTESIAN_POINT('Ctrl Pts',(-8.25299927600006,12.2,-6.85917953200001));
#277255=CARTESIAN_POINT('Ctrl Pts',(-8.25073579400006,12.2,-6.85816379700002));
#277256=CARTESIAN_POINT('Ctrl Pts',(-8.24847883600006,12.2,-6.85714865200002));
#277257=CARTESIAN_POINT('Ctrl Pts',(-8.24622841100006,12.2,-6.85613411000002));
#277258=CARTESIAN_POINT('Ctrl Pts',(-8.24398452500006,12.2,-6.85512018700001));
#277259=CARTESIAN_POINT('Ctrl Pts',(-8.24174718700006,12.2,-6.85410689300002));
#277260=CARTESIAN_POINT('Ctrl Pts',(-8.23951640200006,12.2,-6.85309424500002));
#277261=CARTESIAN_POINT('Ctrl Pts',(-8.23729218000006,12.2,-6.85208225400002));
#277262=CARTESIAN_POINT('Ctrl Pts',(-8.23507452500005,12.2,-6.85107093700001));
#277263=CARTESIAN_POINT('Ctrl Pts',(-8.23286344500006,12.2,-6.85006030300002));
#277264=CARTESIAN_POINT('Ctrl Pts',(-8.23065894900006,12.2,-6.84905037100001));
#277265=CARTESIAN_POINT('Ctrl Pts',(-8.22846104400006,12.2,-6.84804115200001));
#277266=CARTESIAN_POINT('Ctrl Pts',(-8.22626973600006,12.2,-6.84703266000002));
#277267=CARTESIAN_POINT('Ctrl Pts',(-8.22408503300006,12.2,-6.84602491000001));
#277268=CARTESIAN_POINT('Ctrl Pts',(-8.22190694200006,12.2,-6.84501791600002));
#277269=CARTESIAN_POINT('Ctrl Pts',(-8.21973547100006,12.2,-6.84401169100001));
#277270=CARTESIAN_POINT('Ctrl Pts',(-8.21757062600006,12.2,-6.84300624900001));
#277271=CARTESIAN_POINT('Ctrl Pts',(-8.21541241600006,12.2,-6.84200160600002));
#277272=CARTESIAN_POINT('Ctrl Pts',(-8.21326084700006,12.2,-6.84099777500002));
#277273=CARTESIAN_POINT('Ctrl Pts',(-8.21111592700005,12.2,-6.83999477000001));
#277274=CARTESIAN_POINT('Ctrl Pts',(-8.20897766400006,12.2,-6.83899260600001));
#277275=CARTESIAN_POINT('Ctrl Pts',(-8.20684606400006,12.2,-6.83799129700001));
#277276=CARTESIAN_POINT('Ctrl Pts',(-8.20472113500006,12.2,-6.83699085700002));
#277277=CARTESIAN_POINT('Ctrl Pts',(-8.20260288500006,12.2,-6.83599130200002));
#277278=CARTESIAN_POINT('Ctrl Pts',(-8.20049132100005,12.2,-6.83499264500002));
#277279=CARTESIAN_POINT('Ctrl Pts',(-8.19838644900006,12.2,-6.83399490000002));
#277280=CARTESIAN_POINT('Ctrl Pts',(-8.19628827900006,12.2,-6.83299808400001));
#277281=CARTESIAN_POINT('Ctrl Pts',(-8.19419681700005,12.2,-6.83200220900002));
#277282=CARTESIAN_POINT('Ctrl Pts',(-8.19211207000006,12.2,-6.83100729200002));
#277283=CARTESIAN_POINT('Ctrl Pts',(-8.19003404800006,12.2,-6.83001334600001));
#277284=CARTESIAN_POINT('Ctrl Pts',(-8.18796275500006,12.2,-6.82902038700002));
#277285=CARTESIAN_POINT('Ctrl Pts',(-8.18589820000006,12.2,-6.82802842800001));
#277286=CARTESIAN_POINT('Ctrl Pts',(-8.18384039200006,12.2,-6.82703748600002));
#277287=CARTESIAN_POINT('Ctrl Pts',(-8.18178933600005,12.2,-6.82604757600001));
#277288=CARTESIAN_POINT('Ctrl Pts',(-8.17974504200006,12.2,-6.82505871000001));
#277289=CARTESIAN_POINT('Ctrl Pts',(-8.17770751500005,12.2,-6.82407090600002));
#277290=CARTESIAN_POINT('Ctrl Pts',(-8.17567676400006,12.2,-6.82308417800002));
#277291=CARTESIAN_POINT('Ctrl Pts',(-8.17365279800006,12.2,-6.82209854300002));
#277292=CARTESIAN_POINT('Ctrl Pts',(-8.17163562200006,12.2,-6.82111401300002));
#277293=CARTESIAN_POINT('Ctrl Pts',(-8.16962524500006,12.2,-6.82013060400001));
#277294=CARTESIAN_POINT('Ctrl Pts',(-8.16762167300006,12.2,-6.81914833300001));
#277295=CARTESIAN_POINT('Ctrl Pts',(-8.16562491600006,12.2,-6.81816721500001));
#277296=CARTESIAN_POINT('Ctrl Pts',(-8.16363498100005,12.2,-6.81718726300002));
#277297=CARTESIAN_POINT('Ctrl Pts',(-8.16165187500006,12.2,-6.81620849600002));
#277298=CARTESIAN_POINT('Ctrl Pts',(-8.15967560600006,12.2,-6.81523092700001));
#277299=CARTESIAN_POINT('Ctrl Pts',(-8.15770618100006,12.2,-6.81425457200002));
#277300=CARTESIAN_POINT('Ctrl Pts',(-8.15574360800005,12.2,-6.81327944800002));
#277301=CARTESIAN_POINT('Ctrl Pts',(-8.15378789600006,12.2,-6.81230556900001));
#277302=CARTESIAN_POINT('Ctrl Pts',(-8.15183905100006,12.2,-6.81133295000001));
#277303=CARTESIAN_POINT('Ctrl Pts',(-8.14989708100006,12.2,-6.81036160900002));
#277304=CARTESIAN_POINT('Ctrl Pts',(-8.14796199500006,12.2,-6.80939156100001));
#277305=CARTESIAN_POINT('Ctrl Pts',(-8.14603380000005,12.2,-6.80842282100001));
#277306=CARTESIAN_POINT('Ctrl Pts',(-8.14411250400006,12.2,-6.80745540700002));
#277307=CARTESIAN_POINT('Ctrl Pts',(-8.14219811500006,12.2,-6.80648933300001));
#277308=CARTESIAN_POINT('Ctrl Pts',(-8.14029063900006,12.2,-6.80552461600002));
#277309=CARTESIAN_POINT('Ctrl Pts',(-8.13839008600005,12.2,-6.80456127100002));
#277310=CARTESIAN_POINT('Ctrl Pts',(-8.13649646400006,12.2,-6.80359931600002));
#277311=CARTESIAN_POINT('Ctrl Pts',(-8.13460977800006,12.2,-6.80263876500002));
#277312=CARTESIAN_POINT('Ctrl Pts',(-8.13273003800006,12.2,-6.80167963700002));
#277313=CARTESIAN_POINT('Ctrl Pts',(-8.13085725300006,12.2,-6.80072194600001));
#277314=CARTESIAN_POINT('Ctrl Pts',(-8.12899142800006,12.2,-6.79976570900001));
#277315=CARTESIAN_POINT('Ctrl Pts',(-8.12713257400006,12.2,-6.79881094300002));
#277316=CARTESIAN_POINT('Ctrl Pts',(-8.12528069700006,12.2,-6.79785766400002));
#277317=CARTESIAN_POINT('Ctrl Pts',(-8.12343580400006,12.2,-6.79690588900002));
#277318=CARTESIAN_POINT('Ctrl Pts',(-8.12159790600005,12.2,-6.79595563300002));
#277319=CARTESIAN_POINT('Ctrl Pts',(-8.11976700800006,12.2,-6.79500691500002));
#277320=CARTESIAN_POINT('Ctrl Pts',(-8.11794312000006,12.2,-6.79405975100002));
#277321=CARTESIAN_POINT('Ctrl Pts',(-8.11612624900006,12.2,-6.79311415700001));
#277322=CARTESIAN_POINT('Ctrl Pts',(-8.11431640400006,12.2,-6.79217015000001));
#277323=CARTESIAN_POINT('Ctrl Pts',(-8.11251359200006,12.2,-6.79122774800001));
#277324=CARTESIAN_POINT('Ctrl Pts',(-8.11071782100005,12.2,-6.79028696700002));
#277325=CARTESIAN_POINT('Ctrl Pts',(-8.10892909900006,12.2,-6.78934782500002));
#277326=CARTESIAN_POINT('Ctrl Pts',(-8.10714743500006,12.2,-6.78841033800002));
#277327=CARTESIAN_POINT('Ctrl Pts',(-8.10537283700006,12.2,-6.78747452400002));
#277328=CARTESIAN_POINT('Ctrl Pts',(-8.10360531200006,12.2,-6.78654039900002));
#277329=CARTESIAN_POINT('Ctrl Pts',(-8.10184486900006,12.2,-6.78560798200002));
#277330=CARTESIAN_POINT('Ctrl Pts',(-8.10009151600006,12.2,-6.78467728800002));
#277331=CARTESIAN_POINT('Ctrl Pts',(-8.09834526200006,12.2,-6.78374833700002));
#277332=CARTESIAN_POINT('Ctrl Pts',(-8.09660611400006,12.2,-6.78282114600002));
#277333=CARTESIAN_POINT('Ctrl Pts',(-8.09487408000006,12.2,-6.78189573100001));
#277334=CARTESIAN_POINT('Ctrl Pts',(-8.09314916900006,12.2,-6.78097211100001));
#277335=CARTESIAN_POINT('Ctrl Pts',(-8.09143138900006,12.2,-6.78005030300002));
#277336=CARTESIAN_POINT('Ctrl Pts',(-8.08972074900005,12.2,-6.77913032500002));
#277337=CARTESIAN_POINT('Ctrl Pts',(-8.08801725500006,12.2,-6.77821219500002));
#277338=CARTESIAN_POINT('Ctrl Pts',(-8.08632091900006,12.2,-6.77729593100001));
#277339=CARTESIAN_POINT('Ctrl Pts',(-8.08463174500006,12.2,-6.77638154900002));
#277340=CARTESIAN_POINT('Ctrl Pts',(-8.08294974400006,12.2,-6.77546907100002));
#277341=CARTESIAN_POINT('Ctrl Pts',(-8.08127492400006,12.2,-6.77455851200002));
#277342=CARTESIAN_POINT('Ctrl Pts',(-8.07960729300006,12.2,-6.77364988900001));
#277343=CARTESIAN_POINT('Ctrl Pts',(-8.07794685900006,12.2,-6.77274322400002));
#277344=CARTESIAN_POINT('Ctrl Pts',(-8.07629363200006,12.2,-6.77183853400001));
#277345=CARTESIAN_POINT('Ctrl Pts',(-8.07464761900006,12.2,-6.77093583600002));
#277346=CARTESIAN_POINT('Ctrl Pts',(-8.07300882800006,12.2,-6.77003514800001));
#277347=CARTESIAN_POINT('Ctrl Pts',(-8.07137726900006,12.2,-6.76913649000002));
#277348=CARTESIAN_POINT('Ctrl Pts',(-8.06975294900005,12.2,-6.76823988100002));
#277349=CARTESIAN_POINT('Ctrl Pts',(-8.06813587700006,12.2,-6.76734533800002));
#277350=CARTESIAN_POINT('Ctrl Pts',(-8.06652606200006,12.2,-6.76645288100002));
#277351=CARTESIAN_POINT('Ctrl Pts',(-8.06492351200006,12.2,-6.76556252900002));
#277352=CARTESIAN_POINT('Ctrl Pts',(-8.06332823500006,12.2,-6.76467429900002));
#277353=CARTESIAN_POINT('Ctrl Pts',(-8.06174024100006,12.2,-6.76378821200001));
#277354=CARTESIAN_POINT('Ctrl Pts',(-8.06015953800006,12.2,-6.76290428500002));
#277355=CARTESIAN_POINT('Ctrl Pts',(-8.05858613400006,12.2,-6.76202254000002));
#277356=CARTESIAN_POINT('Ctrl Pts',(-8.05702003900005,12.2,-6.76114299200002));
#277357=CARTESIAN_POINT('Ctrl Pts',(-8.05546126000005,12.2,-6.76026566400001));
#277358=CARTESIAN_POINT('Ctrl Pts',(-8.05390980500006,12.2,-6.75939057400001));
#277359=CARTESIAN_POINT('Ctrl Pts',(-8.05236568500005,12.2,-6.75851774000002));
#277360=CARTESIAN_POINT('Ctrl Pts',(-8.05082890800006,12.2,-6.75764718400002));
#277361=CARTESIAN_POINT('Ctrl Pts',(-8.04929948200006,12.2,-6.75677892300002));
#277362=CARTESIAN_POINT('Ctrl Pts',(-8.04777741600006,12.2,-6.75591297900001));
#277363=CARTESIAN_POINT('Ctrl Pts',(-8.04626271900006,12.2,-6.75504936900002));
#277364=CARTESIAN_POINT('Ctrl Pts',(-8.04475540000006,12.2,-6.75418811400001));
#277365=CARTESIAN_POINT('Ctrl Pts',(-8.04325546700005,12.2,-6.75332923500001));
#277366=CARTESIAN_POINT('Ctrl Pts',(-8.04176292900006,12.2,-6.75247275100002));
#277367=CARTESIAN_POINT('Ctrl Pts',(-8.04027779600006,12.2,-6.75161868200002));
#277368=CARTESIAN_POINT('Ctrl Pts',(-8.03880007500006,12.2,-6.75076704800002));
#277369=CARTESIAN_POINT('Ctrl Pts',(-8.03732977700006,12.2,-6.74991786800001));
#277370=CARTESIAN_POINT('Ctrl Pts',(-8.03586690900006,12.2,-6.74907116500002));
#277371=CARTESIAN_POINT('Ctrl Pts',(-8.03441148100006,12.2,-6.74822695700002));
#277372=CARTESIAN_POINT('Ctrl Pts',(-8.03296350200006,12.2,-6.74738526600001));
#277373=CARTESIAN_POINT('Ctrl Pts',(-8.03152298000006,12.2,-6.74654611000002));
#277374=CARTESIAN_POINT('Ctrl Pts',(-8.03008992500006,12.2,-6.74570951200002));
#277375=CARTESIAN_POINT('Ctrl Pts',(-8.02866434500006,12.2,-6.74487549200002));
#277376=CARTESIAN_POINT('Ctrl Pts',(-8.02724625000005,12.2,-6.74404407000001));
#277377=CARTESIAN_POINT('Ctrl Pts',(-8.02583565000005,12.2,-6.74321526700002));
#277378=CARTESIAN_POINT('Ctrl Pts',(-8.02443255200006,12.2,-6.74238910500002));
#277379=CARTESIAN_POINT('Ctrl Pts',(-8.02303696600006,12.2,-6.74156560400001));
#277380=CARTESIAN_POINT('Ctrl Pts',(-8.02164890100006,12.2,-6.74074478500001));
#277381=CARTESIAN_POINT('Ctrl Pts',(-8.02026836500006,12.2,-6.73992667000002));
#277382=CARTESIAN_POINT('Ctrl Pts',(-8.01889537100006,12.2,-6.73911127900002));
#277383=CARTESIAN_POINT('Ctrl Pts',(-8.01752992300005,12.2,-6.73829863500002));
#277384=CARTESIAN_POINT('Ctrl Pts',(-8.01617203400006,12.2,-6.73748875800002));
#277385=CARTESIAN_POINT('Ctrl Pts',(-8.01482171200006,12.2,-6.73668166900002));
#277386=CARTESIAN_POINT('Ctrl Pts',(-8.01347896700005,12.2,-6.73587739300002));
#277387=CARTESIAN_POINT('Ctrl Pts',(-8.01214380700005,12.2,-6.73507594700002));
#277388=CARTESIAN_POINT('Ctrl Pts',(-8.01081624200006,12.2,-6.73427735600002));
#277389=CARTESIAN_POINT('Ctrl Pts',(-8.00949628200006,12.2,-6.73348164200001));
#277390=CARTESIAN_POINT('Ctrl Pts',(-8.00818393600006,12.2,-6.73268882500001));
#277391=CARTESIAN_POINT('Ctrl Pts',(-8.00687921200005,12.2,-6.73189892800002));
#277392=CARTESIAN_POINT('Ctrl Pts',(-8.00558212100006,12.2,-6.73111197200001));
#277393=CARTESIAN_POINT('Ctrl Pts',(-8.00429267200006,12.2,-6.73032798200002));
#277394=CARTESIAN_POINT('Ctrl Pts',(-8.00301087500005,12.2,-6.72954697800002));
#277395=CARTESIAN_POINT('Ctrl Pts',(-8.00173673800006,12.2,-6.72876898400002));
#277396=CARTESIAN_POINT('Ctrl Pts',(-8.00047027300005,12.2,-6.72799402200001));
#277397=CARTESIAN_POINT('Ctrl Pts',(-7.99921148700006,12.2,-6.72722211400002));
#277398=CARTESIAN_POINT('Ctrl Pts',(-7.99796039100006,12.2,-6.72645328300002));
#277399=CARTESIAN_POINT('Ctrl Pts',(-7.99671699500006,12.2,-6.72568755200002));
#277400=CARTESIAN_POINT('Ctrl Pts',(-7.99548130800006,12.2,-6.72492494400001));
#277401=CARTESIAN_POINT('Ctrl Pts',(-7.99425333800006,12.2,-6.72416548300002));
#277402=CARTESIAN_POINT('Ctrl Pts',(-7.99303309800005,12.2,-6.72340919000002));
#277403=CARTESIAN_POINT('Ctrl Pts',(-7.99182059500006,12.2,-6.72265608900001));
#277404=CARTESIAN_POINT('Ctrl Pts',(-7.99061584100006,12.2,-6.72190620500002));
#277405=CARTESIAN_POINT('Ctrl Pts',(-7.98941884300006,12.2,-6.72115955900002));
#277406=CARTESIAN_POINT('Ctrl Pts',(-7.98822961400005,12.2,-6.72041617700001));
#277407=CARTESIAN_POINT('Ctrl Pts',(-7.98704816100006,12.2,-6.71967608000001));
#277408=CARTESIAN_POINT('Ctrl Pts',(-7.98587449600006,12.2,-6.71893929400002));
#277409=CARTESIAN_POINT('Ctrl Pts',(-7.98470862800006,12.2,-6.71820584100002));
#277410=CARTESIAN_POINT('Ctrl Pts',(-7.98355056700006,12.2,-6.71747574700002));
#277411=CARTESIAN_POINT('Ctrl Pts',(-7.98240032200006,12.2,-6.71674903500002));
#277412=CARTESIAN_POINT('Ctrl Pts',(-7.98125790500006,12.2,-6.71602572900002));
#277413=CARTESIAN_POINT('Ctrl Pts',(-7.98012332400006,12.2,-6.71530585300002));
#277414=CARTESIAN_POINT('Ctrl Pts',(-7.97899659000005,12.2,-6.71458943300002));
#277415=CARTESIAN_POINT('Ctrl Pts',(-7.97787771400006,12.2,-6.71387649200001));
#277416=CARTESIAN_POINT('Ctrl Pts',(-7.97676670400006,12.2,-6.71316705500002));
#277417=CARTESIAN_POINT('Ctrl Pts',(-7.97566357200005,12.2,-6.71246114600001));
#277418=CARTESIAN_POINT('Ctrl Pts',(-7.97456832700006,12.2,-6.71175879200002));
#277419=CARTESIAN_POINT('Ctrl Pts',(-7.97348098000005,12.2,-6.71106001600001));
#277420=CARTESIAN_POINT('Ctrl Pts',(-7.97240154100006,12.2,-6.71036484500001));
#277421=CARTESIAN_POINT('Ctrl Pts',(-7.97133002000006,12.2,-6.70967330200002));
#277422=CARTESIAN_POINT('Ctrl Pts',(-7.97026642700006,12.2,-6.70898541300001));
#277423=CARTESIAN_POINT('Ctrl Pts',(-7.96921077400006,12.2,-6.70830120300002));
#277424=CARTESIAN_POINT('Ctrl Pts',(-7.96816307000006,12.2,-6.70762070000002));
#277425=CARTESIAN_POINT('Ctrl Pts',(-7.96712332500006,12.2,-6.70694392700002));
#277426=CARTESIAN_POINT('Ctrl Pts',(-7.96609155000005,12.2,-6.70627091100001));
#277427=CARTESIAN_POINT('Ctrl Pts',(-7.96506775600006,12.2,-6.70560167700001));
#277428=CARTESIAN_POINT('Ctrl Pts',(-7.96405195200006,12.2,-6.70493625300002));
#277429=CARTESIAN_POINT('Ctrl Pts',(-7.96304415000006,12.2,-6.70427466300002));
#277430=CARTESIAN_POINT('Ctrl Pts',(-7.96204436100006,12.2,-6.70361693500002));
#277431=CARTESIAN_POINT('Ctrl Pts',(-7.96105259400005,12.2,-6.70296309300002));
#277432=CARTESIAN_POINT('Ctrl Pts',(-7.96006886100006,12.2,-6.70231316600002));
#277433=CARTESIAN_POINT('Ctrl Pts',(-7.95909317200006,12.2,-6.70166718000001));
#277434=CARTESIAN_POINT('Ctrl Pts',(-7.95812553700006,12.2,-6.70102516100001));
#277435=CARTESIAN_POINT('Ctrl Pts',(-7.95716596800006,12.2,-6.70038713600002));
#277436=CARTESIAN_POINT('Ctrl Pts',(-7.95621447600006,12.2,-6.69975313400001));
#277437=CARTESIAN_POINT('Ctrl Pts',(-7.95527107000006,12.2,-6.69912317900001));
#277438=CARTESIAN_POINT('Ctrl Pts',(-7.95433576200006,12.2,-6.69849730100001));
#277439=CARTESIAN_POINT('Ctrl Pts',(-7.95340856400006,12.2,-6.69787552700001));
#277440=CARTESIAN_POINT('Ctrl Pts',(-7.95248948500006,12.2,-6.69725788300001));
#277441=CARTESIAN_POINT('Ctrl Pts',(-7.95157853800006,12.2,-6.69664439800002));
#277442=CARTESIAN_POINT('Ctrl Pts',(-7.95067573200006,12.2,-6.69603510000002));
#277443=CARTESIAN_POINT('Ctrl Pts',(-7.94978107900006,12.2,-6.69543001700001));
#277444=CARTESIAN_POINT('Ctrl Pts',(-7.94889459000006,12.2,-6.69482917500002));
#277445=CARTESIAN_POINT('Ctrl Pts',(-7.94801627800006,12.2,-6.69423260500002));
#277446=CARTESIAN_POINT('Ctrl Pts',(-7.94714615000006,12.2,-6.69364033500001));
#277447=CARTESIAN_POINT('Ctrl Pts',(-7.94628422000006,12.2,-6.69305239200002));
#277448=CARTESIAN_POINT('Ctrl Pts',(-7.94543050000006,12.2,-6.69246880700002));
#277449=CARTESIAN_POINT('Ctrl Pts',(-7.94458499900006,12.2,-6.69188960600002));
#277450=CARTESIAN_POINT('Ctrl Pts',(-7.94374773100006,12.2,-6.69131482000001));
#277451=CARTESIAN_POINT('Ctrl Pts',(-7.94291870400006,12.2,-6.69074447800002));
#277452=CARTESIAN_POINT('Ctrl Pts',(-7.94209793300006,12.2,-6.69017860900002));
#277453=CARTESIAN_POINT('Ctrl Pts',(-7.94128542700006,12.2,-6.68961724100001));
#277454=CARTESIAN_POINT('Ctrl Pts',(-7.94048119900006,12.2,-6.68906040700002));
#277455=CARTESIAN_POINT('Ctrl Pts',(-7.93968525900006,12.2,-6.68850813300002));
#277456=CARTESIAN_POINT('Ctrl Pts',(-7.93889762000005,12.2,-6.68796045200001));
#277457=CARTESIAN_POINT('Ctrl Pts',(-7.93811829300005,12.2,-6.68741739000002));
#277458=CARTESIAN_POINT('Ctrl Pts',(-7.93734729000006,12.2,-6.68687898200002));
#277459=CARTESIAN_POINT('Ctrl Pts',(-7.93658462200005,12.2,-6.68634525500002));
#277460=CARTESIAN_POINT('Ctrl Pts',(-7.93583464600006,12.2,-6.68581928800001));
#277461=CARTESIAN_POINT('Ctrl Pts',(-7.93524212700006,12.2,-6.68540286400002));
#277462=CARTESIAN_POINT('Ctrl Pts',(-7.93480250600006,12.2,-6.68509340700002));
#277463=CARTESIAN_POINT('Ctrl Pts',(-7.93451247200006,12.2,-6.68488903400001));
#277464=CARTESIAN_POINT('Ctrl Pts',(-7.93436997000006,12.2,-6.68478856700002));
#277465=CARTESIAN_POINT('Ctrl Pts',(-7.93436997000006,15.2,-6.68478856700002));
#277466=CARTESIAN_POINT('Ctrl Pts',(-7.93451247200006,15.2,-6.68488903400001));
#277467=CARTESIAN_POINT('Ctrl Pts',(-7.93480250600006,15.2,-6.68509340700002));
#277468=CARTESIAN_POINT('Ctrl Pts',(-7.93524212700006,15.2,-6.68540286400002));
#277469=CARTESIAN_POINT('Ctrl Pts',(-7.93583464600006,15.2,-6.68581928800001));
#277470=CARTESIAN_POINT('Ctrl Pts',(-7.93658462200005,15.2,-6.68634525500002));
#277471=CARTESIAN_POINT('Ctrl Pts',(-7.93734729000006,15.2,-6.68687898200002));
#277472=CARTESIAN_POINT('Ctrl Pts',(-7.93811829300005,15.2,-6.68741739000002));
#277473=CARTESIAN_POINT('Ctrl Pts',(-7.93889762000005,15.2,-6.68796045200001));
#277474=CARTESIAN_POINT('Ctrl Pts',(-7.93968525900006,15.2,-6.68850813300002));
#277475=CARTESIAN_POINT('Ctrl Pts',(-7.94048119900006,15.2,-6.68906040700002));
#277476=CARTESIAN_POINT('Ctrl Pts',(-7.94128542700006,15.2,-6.68961724100001));
#277477=CARTESIAN_POINT('Ctrl Pts',(-7.94209793300006,15.2,-6.69017860900002));
#277478=CARTESIAN_POINT('Ctrl Pts',(-7.94291870400006,15.2,-6.69074447800002));
#277479=CARTESIAN_POINT('Ctrl Pts',(-7.94374773100006,15.2,-6.69131482000001));
#277480=CARTESIAN_POINT('Ctrl Pts',(-7.94458499900006,15.2,-6.69188960600002));
#277481=CARTESIAN_POINT('Ctrl Pts',(-7.94543050000006,15.2,-6.69246880700002));
#277482=CARTESIAN_POINT('Ctrl Pts',(-7.94628422000006,15.2,-6.69305239200002));
#277483=CARTESIAN_POINT('Ctrl Pts',(-7.94714615000006,15.2,-6.69364033500001));
#277484=CARTESIAN_POINT('Ctrl Pts',(-7.94801627800006,15.2,-6.69423260500002));
#277485=CARTESIAN_POINT('Ctrl Pts',(-7.94889459000006,15.2,-6.69482917500002));
#277486=CARTESIAN_POINT('Ctrl Pts',(-7.94978107900006,15.2,-6.69543001700001));
#277487=CARTESIAN_POINT('Ctrl Pts',(-7.95067573200006,15.2,-6.69603510000002));
#277488=CARTESIAN_POINT('Ctrl Pts',(-7.95157853800006,15.2,-6.69664439800002));
#277489=CARTESIAN_POINT('Ctrl Pts',(-7.95248948500006,15.2,-6.69725788300001));
#277490=CARTESIAN_POINT('Ctrl Pts',(-7.95340856400006,15.2,-6.69787552700001));
#277491=CARTESIAN_POINT('Ctrl Pts',(-7.95433576200006,15.2,-6.69849730100001));
#277492=CARTESIAN_POINT('Ctrl Pts',(-7.95527107000006,15.2,-6.69912317900001));
#277493=CARTESIAN_POINT('Ctrl Pts',(-7.95621447600006,15.2,-6.69975313400001));
#277494=CARTESIAN_POINT('Ctrl Pts',(-7.95716596800006,15.2,-6.70038713600002));
#277495=CARTESIAN_POINT('Ctrl Pts',(-7.95812553700006,15.2,-6.70102516100001));
#277496=CARTESIAN_POINT('Ctrl Pts',(-7.95909317200006,15.2,-6.70166718000001));
#277497=CARTESIAN_POINT('Ctrl Pts',(-7.96006886100006,15.2,-6.70231316600002));
#277498=CARTESIAN_POINT('Ctrl Pts',(-7.96105259400005,15.2,-6.70296309300002));
#277499=CARTESIAN_POINT('Ctrl Pts',(-7.96204436100006,15.2,-6.70361693500002));
#277500=CARTESIAN_POINT('Ctrl Pts',(-7.96304415000006,15.2,-6.70427466300002));
#277501=CARTESIAN_POINT('Ctrl Pts',(-7.96405195200006,15.2,-6.70493625300002));
#277502=CARTESIAN_POINT('Ctrl Pts',(-7.96506775600006,15.2,-6.70560167700001));
#277503=CARTESIAN_POINT('Ctrl Pts',(-7.96609155000005,15.2,-6.70627091100001));
#277504=CARTESIAN_POINT('Ctrl Pts',(-7.96712332500006,15.2,-6.70694392700002));
#277505=CARTESIAN_POINT('Ctrl Pts',(-7.96816307000006,15.2,-6.70762070000002));
#277506=CARTESIAN_POINT('Ctrl Pts',(-7.96921077400006,15.2,-6.70830120300002));
#277507=CARTESIAN_POINT('Ctrl Pts',(-7.97026642700006,15.2,-6.70898541300001));
#277508=CARTESIAN_POINT('Ctrl Pts',(-7.97133002000006,15.2,-6.70967330200002));
#277509=CARTESIAN_POINT('Ctrl Pts',(-7.97240154100006,15.2,-6.71036484500001));
#277510=CARTESIAN_POINT('Ctrl Pts',(-7.97348098000005,15.2,-6.71106001600001));
#277511=CARTESIAN_POINT('Ctrl Pts',(-7.97456832700006,15.2,-6.71175879200002));
#277512=CARTESIAN_POINT('Ctrl Pts',(-7.97566357200005,15.2,-6.71246114600001));
#277513=CARTESIAN_POINT('Ctrl Pts',(-7.97676670400006,15.2,-6.71316705500002));
#277514=CARTESIAN_POINT('Ctrl Pts',(-7.97787771400006,15.2,-6.71387649200001));
#277515=CARTESIAN_POINT('Ctrl Pts',(-7.97899659000005,15.2,-6.71458943300002));
#277516=CARTESIAN_POINT('Ctrl Pts',(-7.98012332400006,15.2,-6.71530585300002));
#277517=CARTESIAN_POINT('Ctrl Pts',(-7.98125790500006,15.2,-6.71602572900002));
#277518=CARTESIAN_POINT('Ctrl Pts',(-7.98240032200006,15.2,-6.71674903500002));
#277519=CARTESIAN_POINT('Ctrl Pts',(-7.98355056700006,15.2,-6.71747574700002));
#277520=CARTESIAN_POINT('Ctrl Pts',(-7.98470862800006,15.2,-6.71820584100002));
#277521=CARTESIAN_POINT('Ctrl Pts',(-7.98587449600006,15.2,-6.71893929400002));
#277522=CARTESIAN_POINT('Ctrl Pts',(-7.98704816100006,15.2,-6.71967608000001));
#277523=CARTESIAN_POINT('Ctrl Pts',(-7.98822961400005,15.2,-6.72041617700001));
#277524=CARTESIAN_POINT('Ctrl Pts',(-7.98941884300006,15.2,-6.72115955900002));
#277525=CARTESIAN_POINT('Ctrl Pts',(-7.99061584100006,15.2,-6.72190620500002));
#277526=CARTESIAN_POINT('Ctrl Pts',(-7.99182059500006,15.2,-6.72265608900001));
#277527=CARTESIAN_POINT('Ctrl Pts',(-7.99303309800005,15.2,-6.72340919000002));
#277528=CARTESIAN_POINT('Ctrl Pts',(-7.99425333800006,15.2,-6.72416548300002));
#277529=CARTESIAN_POINT('Ctrl Pts',(-7.99548130800006,15.2,-6.72492494400001));
#277530=CARTESIAN_POINT('Ctrl Pts',(-7.99671699500006,15.2,-6.72568755200002));
#277531=CARTESIAN_POINT('Ctrl Pts',(-7.99796039100006,15.2,-6.72645328300002));
#277532=CARTESIAN_POINT('Ctrl Pts',(-7.99921148700006,15.2,-6.72722211400002));
#277533=CARTESIAN_POINT('Ctrl Pts',(-8.00047027300005,15.2,-6.72799402200001));
#277534=CARTESIAN_POINT('Ctrl Pts',(-8.00173673800006,15.2,-6.72876898400002));
#277535=CARTESIAN_POINT('Ctrl Pts',(-8.00301087500005,15.2,-6.72954697800002));
#277536=CARTESIAN_POINT('Ctrl Pts',(-8.00429267200006,15.2,-6.73032798200002));
#277537=CARTESIAN_POINT('Ctrl Pts',(-8.00558212100006,15.2,-6.73111197200001));
#277538=CARTESIAN_POINT('Ctrl Pts',(-8.00687921200005,15.2,-6.73189892800002));
#277539=CARTESIAN_POINT('Ctrl Pts',(-8.00818393600006,15.2,-6.73268882500001));
#277540=CARTESIAN_POINT('Ctrl Pts',(-8.00949628200006,15.2,-6.73348164200001));
#277541=CARTESIAN_POINT('Ctrl Pts',(-8.01081624200006,15.2,-6.73427735600002));
#277542=CARTESIAN_POINT('Ctrl Pts',(-8.01214380700005,15.2,-6.73507594700002));
#277543=CARTESIAN_POINT('Ctrl Pts',(-8.01347896700005,15.2,-6.73587739300002));
#277544=CARTESIAN_POINT('Ctrl Pts',(-8.01482171200006,15.2,-6.73668166900002));
#277545=CARTESIAN_POINT('Ctrl Pts',(-8.01617203400006,15.2,-6.73748875800002));
#277546=CARTESIAN_POINT('Ctrl Pts',(-8.01752992300005,15.2,-6.73829863500002));
#277547=CARTESIAN_POINT('Ctrl Pts',(-8.01889537100006,15.2,-6.73911127900002));
#277548=CARTESIAN_POINT('Ctrl Pts',(-8.02026836500006,15.2,-6.73992667000002));
#277549=CARTESIAN_POINT('Ctrl Pts',(-8.02164890100006,15.2,-6.74074478500001));
#277550=CARTESIAN_POINT('Ctrl Pts',(-8.02303696600006,15.2,-6.74156560400001));
#277551=CARTESIAN_POINT('Ctrl Pts',(-8.02443255200006,15.2,-6.74238910500002));
#277552=CARTESIAN_POINT('Ctrl Pts',(-8.02583565000005,15.2,-6.74321526700002));
#277553=CARTESIAN_POINT('Ctrl Pts',(-8.02724625000005,15.2,-6.74404407000001));
#277554=CARTESIAN_POINT('Ctrl Pts',(-8.02866434500006,15.2,-6.74487549200002));
#277555=CARTESIAN_POINT('Ctrl Pts',(-8.03008992500006,15.2,-6.74570951200002));
#277556=CARTESIAN_POINT('Ctrl Pts',(-8.03152298000006,15.2,-6.74654611000002));
#277557=CARTESIAN_POINT('Ctrl Pts',(-8.03296350200006,15.2,-6.74738526600001));
#277558=CARTESIAN_POINT('Ctrl Pts',(-8.03441148100006,15.2,-6.74822695700002));
#277559=CARTESIAN_POINT('Ctrl Pts',(-8.03586690900006,15.2,-6.74907116500002));
#277560=CARTESIAN_POINT('Ctrl Pts',(-8.03732977700006,15.2,-6.74991786800001));
#277561=CARTESIAN_POINT('Ctrl Pts',(-8.03880007500006,15.2,-6.75076704800002));
#277562=CARTESIAN_POINT('Ctrl Pts',(-8.04027779600006,15.2,-6.75161868200002));
#277563=CARTESIAN_POINT('Ctrl Pts',(-8.04176292900006,15.2,-6.75247275100002));
#277564=CARTESIAN_POINT('Ctrl Pts',(-8.04325546700005,15.2,-6.75332923500001));
#277565=CARTESIAN_POINT('Ctrl Pts',(-8.04475540000006,15.2,-6.75418811400001));
#277566=CARTESIAN_POINT('Ctrl Pts',(-8.04626271900006,15.2,-6.75504936900002));
#277567=CARTESIAN_POINT('Ctrl Pts',(-8.04777741600006,15.2,-6.75591297900001));
#277568=CARTESIAN_POINT('Ctrl Pts',(-8.04929948200006,15.2,-6.75677892300002));
#277569=CARTESIAN_POINT('Ctrl Pts',(-8.05082890800006,15.2,-6.75764718400002));
#277570=CARTESIAN_POINT('Ctrl Pts',(-8.05236568500005,15.2,-6.75851774000002));
#277571=CARTESIAN_POINT('Ctrl Pts',(-8.05390980500006,15.2,-6.75939057400001));
#277572=CARTESIAN_POINT('Ctrl Pts',(-8.05546126000005,15.2,-6.76026566400001));
#277573=CARTESIAN_POINT('Ctrl Pts',(-8.05702003900005,15.2,-6.76114299200002));
#277574=CARTESIAN_POINT('Ctrl Pts',(-8.05858613400006,15.2,-6.76202254000002));
#277575=CARTESIAN_POINT('Ctrl Pts',(-8.06015953800006,15.2,-6.76290428500002));
#277576=CARTESIAN_POINT('Ctrl Pts',(-8.06174024100006,15.2,-6.76378821200001));
#277577=CARTESIAN_POINT('Ctrl Pts',(-8.06332823500006,15.2,-6.76467429900002));
#277578=CARTESIAN_POINT('Ctrl Pts',(-8.06492351200006,15.2,-6.76556252900002));
#277579=CARTESIAN_POINT('Ctrl Pts',(-8.06652606200006,15.2,-6.76645288100002));
#277580=CARTESIAN_POINT('Ctrl Pts',(-8.06813587700006,15.2,-6.76734533800002));
#277581=CARTESIAN_POINT('Ctrl Pts',(-8.06975294900005,15.2,-6.76823988100002));
#277582=CARTESIAN_POINT('Ctrl Pts',(-8.07137726900006,15.2,-6.76913649000002));
#277583=CARTESIAN_POINT('Ctrl Pts',(-8.07300882800006,15.2,-6.77003514800001));
#277584=CARTESIAN_POINT('Ctrl Pts',(-8.07464761900006,15.2,-6.77093583600002));
#277585=CARTESIAN_POINT('Ctrl Pts',(-8.07629363200006,15.2,-6.77183853400001));
#277586=CARTESIAN_POINT('Ctrl Pts',(-8.07794685900006,15.2,-6.77274322400002));
#277587=CARTESIAN_POINT('Ctrl Pts',(-8.07960729300006,15.2,-6.77364988900001));
#277588=CARTESIAN_POINT('Ctrl Pts',(-8.08127492400006,15.2,-6.77455851200002));
#277589=CARTESIAN_POINT('Ctrl Pts',(-8.08294974400006,15.2,-6.77546907100002));
#277590=CARTESIAN_POINT('Ctrl Pts',(-8.08463174500006,15.2,-6.77638154900002));
#277591=CARTESIAN_POINT('Ctrl Pts',(-8.08632091900006,15.2,-6.77729593100001));
#277592=CARTESIAN_POINT('Ctrl Pts',(-8.08801725500006,15.2,-6.77821219500002));
#277593=CARTESIAN_POINT('Ctrl Pts',(-8.08972074900005,15.2,-6.77913032500002));
#277594=CARTESIAN_POINT('Ctrl Pts',(-8.09143138900006,15.2,-6.78005030300002));
#277595=CARTESIAN_POINT('Ctrl Pts',(-8.09314916900006,15.2,-6.78097211100001));
#277596=CARTESIAN_POINT('Ctrl Pts',(-8.09487408000006,15.2,-6.78189573100001));
#277597=CARTESIAN_POINT('Ctrl Pts',(-8.09660611400006,15.2,-6.78282114600002));
#277598=CARTESIAN_POINT('Ctrl Pts',(-8.09834526200006,15.2,-6.78374833700002));
#277599=CARTESIAN_POINT('Ctrl Pts',(-8.10009151600006,15.2,-6.78467728800002));
#277600=CARTESIAN_POINT('Ctrl Pts',(-8.10184486900006,15.2,-6.78560798200002));
#277601=CARTESIAN_POINT('Ctrl Pts',(-8.10360531200006,15.2,-6.78654039900002));
#277602=CARTESIAN_POINT('Ctrl Pts',(-8.10537283700006,15.2,-6.78747452400002));
#277603=CARTESIAN_POINT('Ctrl Pts',(-8.10714743500006,15.2,-6.78841033800002));
#277604=CARTESIAN_POINT('Ctrl Pts',(-8.10892909900006,15.2,-6.78934782500002));
#277605=CARTESIAN_POINT('Ctrl Pts',(-8.11071782100005,15.2,-6.79028696700002));
#277606=CARTESIAN_POINT('Ctrl Pts',(-8.11251359200006,15.2,-6.79122774800001));
#277607=CARTESIAN_POINT('Ctrl Pts',(-8.11431640400006,15.2,-6.79217015000001));
#277608=CARTESIAN_POINT('Ctrl Pts',(-8.11612624900006,15.2,-6.79311415700001));
#277609=CARTESIAN_POINT('Ctrl Pts',(-8.11794312000006,15.2,-6.79405975100002));
#277610=CARTESIAN_POINT('Ctrl Pts',(-8.11976700800006,15.2,-6.79500691500002));
#277611=CARTESIAN_POINT('Ctrl Pts',(-8.12159790600005,15.2,-6.79595563300002));
#277612=CARTESIAN_POINT('Ctrl Pts',(-8.12343580400006,15.2,-6.79690588900002));
#277613=CARTESIAN_POINT('Ctrl Pts',(-8.12528069700006,15.2,-6.79785766400002));
#277614=CARTESIAN_POINT('Ctrl Pts',(-8.12713257400006,15.2,-6.79881094300002));
#277615=CARTESIAN_POINT('Ctrl Pts',(-8.12899142800006,15.2,-6.79976570900001));
#277616=CARTESIAN_POINT('Ctrl Pts',(-8.13085725300006,15.2,-6.80072194600001));
#277617=CARTESIAN_POINT('Ctrl Pts',(-8.13273003800006,15.2,-6.80167963700002));
#277618=CARTESIAN_POINT('Ctrl Pts',(-8.13460977800006,15.2,-6.80263876500002));
#277619=CARTESIAN_POINT('Ctrl Pts',(-8.13649646400006,15.2,-6.80359931600002));
#277620=CARTESIAN_POINT('Ctrl Pts',(-8.13839008600005,15.2,-6.80456127100002));
#277621=CARTESIAN_POINT('Ctrl Pts',(-8.14029063900006,15.2,-6.80552461600002));
#277622=CARTESIAN_POINT('Ctrl Pts',(-8.14219811500006,15.2,-6.80648933300001));
#277623=CARTESIAN_POINT('Ctrl Pts',(-8.14411250400006,15.2,-6.80745540700002));
#277624=CARTESIAN_POINT('Ctrl Pts',(-8.14603380000005,15.2,-6.80842282100001));
#277625=CARTESIAN_POINT('Ctrl Pts',(-8.14796199500006,15.2,-6.80939156100001));
#277626=CARTESIAN_POINT('Ctrl Pts',(-8.14989708100006,15.2,-6.81036160900002));
#277627=CARTESIAN_POINT('Ctrl Pts',(-8.15183905100006,15.2,-6.81133295000001));
#277628=CARTESIAN_POINT('Ctrl Pts',(-8.15378789600006,15.2,-6.81230556900001));
#277629=CARTESIAN_POINT('Ctrl Pts',(-8.15574360800005,15.2,-6.81327944800002));
#277630=CARTESIAN_POINT('Ctrl Pts',(-8.15770618100006,15.2,-6.81425457200002));
#277631=CARTESIAN_POINT('Ctrl Pts',(-8.15967560600006,15.2,-6.81523092700001));
#277632=CARTESIAN_POINT('Ctrl Pts',(-8.16165187500006,15.2,-6.81620849600002));
#277633=CARTESIAN_POINT('Ctrl Pts',(-8.16363498100005,15.2,-6.81718726300002));
#277634=CARTESIAN_POINT('Ctrl Pts',(-8.16562491600006,15.2,-6.81816721500001));
#277635=CARTESIAN_POINT('Ctrl Pts',(-8.16762167300006,15.2,-6.81914833300001));
#277636=CARTESIAN_POINT('Ctrl Pts',(-8.16962524500006,15.2,-6.82013060400001));
#277637=CARTESIAN_POINT('Ctrl Pts',(-8.17163562200006,15.2,-6.82111401300002));
#277638=CARTESIAN_POINT('Ctrl Pts',(-8.17365279800006,15.2,-6.82209854300002));
#277639=CARTESIAN_POINT('Ctrl Pts',(-8.17567676400006,15.2,-6.82308417800002));
#277640=CARTESIAN_POINT('Ctrl Pts',(-8.17770751500005,15.2,-6.82407090600002));
#277641=CARTESIAN_POINT('Ctrl Pts',(-8.17974504200006,15.2,-6.82505871000001));
#277642=CARTESIAN_POINT('Ctrl Pts',(-8.18178933600005,15.2,-6.82604757600001));
#277643=CARTESIAN_POINT('Ctrl Pts',(-8.18384039200006,15.2,-6.82703748600002));
#277644=CARTESIAN_POINT('Ctrl Pts',(-8.18589820000006,15.2,-6.82802842800001));
#277645=CARTESIAN_POINT('Ctrl Pts',(-8.18796275500006,15.2,-6.82902038700002));
#277646=CARTESIAN_POINT('Ctrl Pts',(-8.19003404800006,15.2,-6.83001334600001));
#277647=CARTESIAN_POINT('Ctrl Pts',(-8.19211207000006,15.2,-6.83100729200002));
#277648=CARTESIAN_POINT('Ctrl Pts',(-8.19419681700005,15.2,-6.83200220900002));
#277649=CARTESIAN_POINT('Ctrl Pts',(-8.19628827900006,15.2,-6.83299808400001));
#277650=CARTESIAN_POINT('Ctrl Pts',(-8.19838644900006,15.2,-6.83399490000002));
#277651=CARTESIAN_POINT('Ctrl Pts',(-8.20049132100005,15.2,-6.83499264500002));
#277652=CARTESIAN_POINT('Ctrl Pts',(-8.20260288500006,15.2,-6.83599130200002));
#277653=CARTESIAN_POINT('Ctrl Pts',(-8.20472113500006,15.2,-6.83699085700002));
#277654=CARTESIAN_POINT('Ctrl Pts',(-8.20684606400006,15.2,-6.83799129700001));
#277655=CARTESIAN_POINT('Ctrl Pts',(-8.20897766400006,15.2,-6.83899260600001));
#277656=CARTESIAN_POINT('Ctrl Pts',(-8.21111592700005,15.2,-6.83999477000001));
#277657=CARTESIAN_POINT('Ctrl Pts',(-8.21326084700006,15.2,-6.84099777500002));
#277658=CARTESIAN_POINT('Ctrl Pts',(-8.21541241600006,15.2,-6.84200160600002));
#277659=CARTESIAN_POINT('Ctrl Pts',(-8.21757062600006,15.2,-6.84300624900001));
#277660=CARTESIAN_POINT('Ctrl Pts',(-8.21973547100006,15.2,-6.84401169100001));
#277661=CARTESIAN_POINT('Ctrl Pts',(-8.22190694200006,15.2,-6.84501791600002));
#277662=CARTESIAN_POINT('Ctrl Pts',(-8.22408503300006,15.2,-6.84602491000001));
#277663=CARTESIAN_POINT('Ctrl Pts',(-8.22626973600006,15.2,-6.84703266000002));
#277664=CARTESIAN_POINT('Ctrl Pts',(-8.22846104400006,15.2,-6.84804115200001));
#277665=CARTESIAN_POINT('Ctrl Pts',(-8.23065894900006,15.2,-6.84905037100001));
#277666=CARTESIAN_POINT('Ctrl Pts',(-8.23286344500006,15.2,-6.85006030300002));
#277667=CARTESIAN_POINT('Ctrl Pts',(-8.23507452500005,15.2,-6.85107093700001));
#277668=CARTESIAN_POINT('Ctrl Pts',(-8.23729218000006,15.2,-6.85208225400002));
#277669=CARTESIAN_POINT('Ctrl Pts',(-8.23951640200006,15.2,-6.85309424500002));
#277670=CARTESIAN_POINT('Ctrl Pts',(-8.24174718700006,15.2,-6.85410689300002));
#277671=CARTESIAN_POINT('Ctrl Pts',(-8.24398452500006,15.2,-6.85512018700001));
#277672=CARTESIAN_POINT('Ctrl Pts',(-8.24622841100006,15.2,-6.85613411000002));
#277673=CARTESIAN_POINT('Ctrl Pts',(-8.24847883600006,15.2,-6.85714865200002));
#277674=CARTESIAN_POINT('Ctrl Pts',(-8.25073579400006,15.2,-6.85816379700002));
#277675=CARTESIAN_POINT('Ctrl Pts',(-8.25299927600006,15.2,-6.85917953200001));
#277676=CARTESIAN_POINT('Ctrl Pts',(-8.25526927700006,15.2,-6.86019584300002));
#277677=CARTESIAN_POINT('Ctrl Pts',(-8.25754578900005,15.2,-6.86121271800002));
#277678=CARTESIAN_POINT('Ctrl Pts',(-8.25982880500005,15.2,-6.86223014300002));
#277679=CARTESIAN_POINT('Ctrl Pts',(-8.26211831700006,15.2,-6.86324810400002));
#277680=CARTESIAN_POINT('Ctrl Pts',(-8.26441431900006,15.2,-6.86426658600002));
#277681=CARTESIAN_POINT('Ctrl Pts',(-8.26671680300005,15.2,-6.86528558000001));
#277682=CARTESIAN_POINT('Ctrl Pts',(-8.26902576200006,15.2,-6.86630507000002));
#277683=CARTESIAN_POINT('Ctrl Pts',(-8.27134119000006,15.2,-6.86732504200001));
#277684=CARTESIAN_POINT('Ctrl Pts',(-8.27366307900006,15.2,-6.86834548500002));
#277685=CARTESIAN_POINT('Ctrl Pts',(-8.27599142100006,15.2,-6.86936638500002));
#277686=CARTESIAN_POINT('Ctrl Pts',(-8.27832621000006,15.2,-6.87038772900002));
#277687=CARTESIAN_POINT('Ctrl Pts',(-8.28066743900006,15.2,-6.87140950400002));
#277688=CARTESIAN_POINT('Ctrl Pts',(-8.28301510100006,15.2,-6.87243169500002));
#277689=CARTESIAN_POINT('Ctrl Pts',(-8.28536918900006,15.2,-6.87345429300001));
#277690=CARTESIAN_POINT('Ctrl Pts',(-8.28772969600006,15.2,-6.87447728100001));
#277691=CARTESIAN_POINT('Ctrl Pts',(-8.29009661400006,15.2,-6.87550064900002));
#277692=CARTESIAN_POINT('Ctrl Pts',(-8.29246993600006,15.2,-6.87652438300002));
#277693=CARTESIAN_POINT('Ctrl Pts',(-8.29484965700006,15.2,-6.87754847000001));
#277694=CARTESIAN_POINT('Ctrl Pts',(-8.29723576800006,15.2,-6.87857289700001));
#277695=CARTESIAN_POINT('Ctrl Pts',(-8.29962826300006,15.2,-6.87959765300001));
#277696=CARTESIAN_POINT('Ctrl Pts',(-8.30202713400006,15.2,-6.88062272300002));
#277697=CARTESIAN_POINT('Ctrl Pts',(-8.30443237500005,15.2,-6.88164809600002));
#277698=CARTESIAN_POINT('Ctrl Pts',(-8.30684397800006,15.2,-6.88267375900002));
#277699=CARTESIAN_POINT('Ctrl Pts',(-8.30926193800006,15.2,-6.88369969900001));
#277700=CARTESIAN_POINT('Ctrl Pts',(-8.31168624600006,15.2,-6.88472590400002));
#277701=CARTESIAN_POINT('Ctrl Pts',(-8.31411689600005,15.2,-6.88575236100001));
#277702=CARTESIAN_POINT('Ctrl Pts',(-8.31655388200006,15.2,-6.88677905700001));
#277703=CARTESIAN_POINT('Ctrl Pts',(-8.31899719600005,15.2,-6.88780598100001));
#277704=CARTESIAN_POINT('Ctrl Pts',(-8.32144683000006,15.2,-6.88883311900002));
#277705=CARTESIAN_POINT('Ctrl Pts',(-8.32390277900006,15.2,-6.88986046100001));
#277706=CARTESIAN_POINT('Ctrl Pts',(-8.32636503500006,15.2,-6.89088799200002));
#277707=CARTESIAN_POINT('Ctrl Pts',(-8.32883359200006,15.2,-6.89191570100002));
#277708=CARTESIAN_POINT('Ctrl Pts',(-8.33130844300005,15.2,-6.89294357600001));
#277709=CARTESIAN_POINT('Ctrl Pts',(-8.33378957900005,15.2,-6.89397160500001));
#277710=CARTESIAN_POINT('Ctrl Pts',(-8.33627699700006,15.2,-6.89499977500001));
#277711=CARTESIAN_POINT('Ctrl Pts',(-8.33877068700006,15.2,-6.89602807400002));
#277712=CARTESIAN_POINT('Ctrl Pts',(-8.34127064400005,15.2,-6.89705649000001));
#277713=CARTESIAN_POINT('Ctrl Pts',(-8.34377685900006,15.2,-6.89808501100002));
#277714=CARTESIAN_POINT('Ctrl Pts',(-8.34628932800005,15.2,-6.89911362500002));
#277715=CARTESIAN_POINT('Ctrl Pts',(-8.34880804200005,15.2,-6.90014232000002));
#277716=CARTESIAN_POINT('Ctrl Pts',(-8.35133299600006,15.2,-6.90117108400001));
#277717=CARTESIAN_POINT('Ctrl Pts',(-8.35386418000006,15.2,-6.90219990600001));
#277718=CARTESIAN_POINT('Ctrl Pts',(-8.35640159200006,15.2,-6.90322877200002));
#277719=CARTESIAN_POINT('Ctrl Pts',(-8.35894522100006,15.2,-6.90425767200002));
#277720=CARTESIAN_POINT('Ctrl Pts',(-8.36149506200006,15.2,-6.90528659300002));
#277721=CARTESIAN_POINT('Ctrl Pts',(-8.36405110900006,15.2,-6.90631552400002));
#277722=CARTESIAN_POINT('Ctrl Pts',(-8.36661335300006,15.2,-6.90734445300001));
#277723=CARTESIAN_POINT('Ctrl Pts',(-8.36918179000006,15.2,-6.90837336800002));
#277724=CARTESIAN_POINT('Ctrl Pts',(-8.37175641100006,15.2,-6.90940225800002));
#277725=CARTESIAN_POINT('Ctrl Pts',(-8.37433721100006,15.2,-6.91043111100001));
#277726=CARTESIAN_POINT('Ctrl Pts',(-8.37692418100006,15.2,-6.91145991600001));
#277727=CARTESIAN_POINT('Ctrl Pts',(-8.37951731800005,15.2,-6.91248865900001));
#277728=CARTESIAN_POINT('Ctrl Pts',(-8.38211661100006,15.2,-6.91351733200002));
#277729=CARTESIAN_POINT('Ctrl Pts',(-8.38472205600005,15.2,-6.91454592100002));
#277730=CARTESIAN_POINT('Ctrl Pts',(-8.38733364500006,15.2,-6.91557441500001));
#277731=CARTESIAN_POINT('Ctrl Pts',(-8.38995137300006,15.2,-6.91660280300002));
#277732=CARTESIAN_POINT('Ctrl Pts',(-8.39257523200006,15.2,-6.91763107400002));
#277733=CARTESIAN_POINT('Ctrl Pts',(-8.39520521500006,15.2,-6.91865921400002));
#277734=CARTESIAN_POINT('Ctrl Pts',(-8.39784131700006,15.2,-6.91968721500002));
#277735=CARTESIAN_POINT('Ctrl Pts',(-8.40048352900006,15.2,-6.92071506500002));
#277736=CARTESIAN_POINT('Ctrl Pts',(-8.40313184700006,15.2,-6.92174275100002));
#277737=CARTESIAN_POINT('Ctrl Pts',(-8.40578626200006,15.2,-6.92277026300002));
#277738=CARTESIAN_POINT('Ctrl Pts',(-8.40844676900005,15.2,-6.92379758900002));
#277739=CARTESIAN_POINT('Ctrl Pts',(-8.41111336100006,15.2,-6.92482472000002));
#277740=CARTESIAN_POINT('Ctrl Pts',(-8.41378603100006,15.2,-6.92585164200001));
#277741=CARTESIAN_POINT('Ctrl Pts',(-8.41646477200005,15.2,-6.92687834500001));
#277742=CARTESIAN_POINT('Ctrl Pts',(-8.41914957900006,15.2,-6.92790481800002));
#277743=CARTESIAN_POINT('Ctrl Pts',(-8.42184044300006,15.2,-6.92893105000002));
#277744=CARTESIAN_POINT('Ctrl Pts',(-8.42453736000006,15.2,-6.92995703000002));
#277745=CARTESIAN_POINT('Ctrl Pts',(-8.42724032100006,15.2,-6.93098274800001));
#277746=CARTESIAN_POINT('Ctrl Pts',(-8.42994932200006,15.2,-6.93200819000002));
#277747=CARTESIAN_POINT('Ctrl Pts',(-8.43266435300006,15.2,-6.93303334900002));
#277748=CARTESIAN_POINT('Ctrl Pts',(-8.43538541200006,15.2,-6.93405821000002));
#277749=CARTESIAN_POINT('Ctrl Pts',(-8.43811248900005,15.2,-6.93508276600002));
#277750=CARTESIAN_POINT('Ctrl Pts',(-8.44084557900005,15.2,-6.93610700400002));
#277751=CARTESIAN_POINT('Ctrl Pts',(-8.44358467400006,15.2,-6.93713091300002));
#277752=CARTESIAN_POINT('Ctrl Pts',(-8.44632976900006,15.2,-6.93815448200001));
#277753=CARTESIAN_POINT('Ctrl Pts',(-8.44908085600006,15.2,-6.93917770200001));
#277754=CARTESIAN_POINT('Ctrl Pts',(-8.45183793100006,15.2,-6.94020056100002));
#277755=CARTESIAN_POINT('Ctrl Pts',(-8.45460098500006,15.2,-6.94122304900001));
#277756=CARTESIAN_POINT('Ctrl Pts',(-8.45737001200006,15.2,-6.94224515400002));
#277757=CARTESIAN_POINT('Ctrl Pts',(-8.46014500600005,15.2,-6.94326686700002));
#277758=CARTESIAN_POINT('Ctrl Pts',(-8.46292596100006,15.2,-6.94428817600001));
#277759=CARTESIAN_POINT('Ctrl Pts',(-8.46571286900006,15.2,-6.94530907100001));
#277760=CARTESIAN_POINT('Ctrl Pts',(-8.46850572600006,15.2,-6.94632954200002));
#277761=CARTESIAN_POINT('Ctrl Pts',(-8.47130452200006,15.2,-6.94734957900002));
#277762=CARTESIAN_POINT('Ctrl Pts',(-8.47410925300006,15.2,-6.94836916900002));
#277763=CARTESIAN_POINT('Ctrl Pts',(-8.47691991300006,15.2,-6.94938830400002));
#277764=CARTESIAN_POINT('Ctrl Pts',(-8.47973649400006,15.2,-6.95040697300002));
#277765=CARTESIAN_POINT('Ctrl Pts',(-8.48255899100005,15.2,-6.95142516400002));
#277766=CARTESIAN_POINT('Ctrl Pts',(-8.48538739600006,15.2,-6.95244286800002));
#277767=CARTESIAN_POINT('Ctrl Pts',(-8.48822170400006,15.2,-6.95346007500002));
#277768=CARTESIAN_POINT('Ctrl Pts',(-8.49106190600006,15.2,-6.95447677400002));
#277769=CARTESIAN_POINT('Ctrl Pts',(-8.49390800000006,15.2,-6.95549295400002));
#277770=CARTESIAN_POINT('Ctrl Pts',(-8.49675997600006,15.2,-6.95650860700002));
#277771=CARTESIAN_POINT('Ctrl Pts',(-8.49961782900006,15.2,-6.95752372000002));
#277772=CARTESIAN_POINT('Ctrl Pts',(-8.50248155100006,15.2,-6.95853828600002));
#277773=CARTESIAN_POINT('Ctrl Pts',(-8.50535113900006,15.2,-6.95955229100001));
#277774=CARTESIAN_POINT('Ctrl Pts',(-8.50822658400006,15.2,-6.96056572800002));
#277775=CARTESIAN_POINT('Ctrl Pts',(-8.51110788000006,15.2,-6.96157858500002));
#277776=CARTESIAN_POINT('Ctrl Pts',(-8.51399502100006,15.2,-6.96259085300002));
#277777=CARTESIAN_POINT('Ctrl Pts',(-8.51688800000005,15.2,-6.96360252200002));
#277778=CARTESIAN_POINT('Ctrl Pts',(-8.51978681100006,15.2,-6.96461358000001));
#277779=CARTESIAN_POINT('Ctrl Pts',(-8.52269144900006,15.2,-6.96562402000002));
#277780=CARTESIAN_POINT('Ctrl Pts',(-8.52560190400006,15.2,-6.96663382900002));
#277781=CARTESIAN_POINT('Ctrl Pts',(-8.52851817400006,15.2,-6.96764300000002));
#277782=CARTESIAN_POINT('Ctrl Pts',(-8.53144025100006,15.2,-6.96865152100001));
#277783=CARTESIAN_POINT('Ctrl Pts',(-8.53436812700006,15.2,-6.96965938200002));
#277784=CARTESIAN_POINT('Ctrl Pts',(-8.53730179800005,15.2,-6.97066657500002));
#277785=CARTESIAN_POINT('Ctrl Pts',(-8.54024125700005,15.2,-6.97167308800001));
#277786=CARTESIAN_POINT('Ctrl Pts',(-8.54318649800006,15.2,-6.97267891200001));
#277787=CARTESIAN_POINT('Ctrl Pts',(-8.54613751300005,15.2,-6.97368403700001));
#277788=CARTESIAN_POINT('Ctrl Pts',(-8.54909429800006,15.2,-6.97468845400002));
#277789=CARTESIAN_POINT('Ctrl Pts',(-8.55205684500006,15.2,-6.97569215300001));
#277790=CARTESIAN_POINT('Ctrl Pts',(-8.55502514900006,15.2,-6.97669512400001));
#277791=CARTESIAN_POINT('Ctrl Pts',(-8.55799920200005,15.2,-6.97769735700002));
#277792=CARTESIAN_POINT('Ctrl Pts',(-8.56097900000006,15.2,-6.97869884300002));
#277793=CARTESIAN_POINT('Ctrl Pts',(-8.56396453400006,15.2,-6.97969957100002));
#277794=CARTESIAN_POINT('Ctrl Pts',(-8.56695580000006,15.2,-6.98069953300001));
#277795=CARTESIAN_POINT('Ctrl Pts',(-8.56995279100006,15.2,-6.98169871900002));
#277796=CARTESIAN_POINT('Ctrl Pts',(-8.57295550200006,15.2,-6.98269711800001));
#277797=CARTESIAN_POINT('Ctrl Pts',(-8.57596392500006,15.2,-6.98369472200002));
#277798=CARTESIAN_POINT('Ctrl Pts',(-8.57897805400006,15.2,-6.98469152300002));
#277799=CARTESIAN_POINT('Ctrl Pts',(-8.58199788300006,15.2,-6.98568750700002));
#277800=CARTESIAN_POINT('Ctrl Pts',(-8.58502340600005,15.2,-6.98668266800002));
#277801=CARTESIAN_POINT('Ctrl Pts',(-8.58805461700006,15.2,-6.98767699600002));
#277802=CARTESIAN_POINT('Ctrl Pts',(-8.59109150900006,15.2,-6.98867048200002));
#277803=CARTESIAN_POINT('Ctrl Pts',(-8.59413407600006,15.2,-6.98966311400002));
#277804=CARTESIAN_POINT('Ctrl Pts',(-8.59718231200005,15.2,-6.99065488500001));
#277805=CARTESIAN_POINT('Ctrl Pts',(-8.60023621200006,15.2,-6.99164578600002));
#277806=CARTESIAN_POINT('Ctrl Pts',(-8.60329576800006,15.2,-6.99263580600002));
#277807=CARTESIAN_POINT('Ctrl Pts',(-8.60636097400005,15.2,-6.99362493600002));
#277808=CARTESIAN_POINT('Ctrl Pts',(-8.60943182500005,15.2,-6.99461316800001));
#277809=CARTESIAN_POINT('Ctrl Pts',(-8.61250831400006,15.2,-6.99560049200001));
#277810=CARTESIAN_POINT('Ctrl Pts',(-8.61559043500005,15.2,-6.99658689800001));
#277811=CARTESIAN_POINT('Ctrl Pts',(-8.61867818200006,15.2,-6.99757237900001));
#277812=CARTESIAN_POINT('Ctrl Pts',(-8.62177154800005,15.2,-6.99855692200002));
#277813=CARTESIAN_POINT('Ctrl Pts',(-8.62487052700006,15.2,-6.99954052200002));
#277814=CARTESIAN_POINT('Ctrl Pts',(-8.62797511400006,15.2,-7.00052316700001));
#277815=CARTESIAN_POINT('Ctrl Pts',(-8.63108530200006,15.2,-7.00150485000002));
#277816=CARTESIAN_POINT('Ctrl Pts',(-8.63420108600006,15.2,-7.00248556000002));
#277817=CARTESIAN_POINT('Ctrl Pts',(-8.63732245800006,15.2,-7.00346528800001));
#277818=CARTESIAN_POINT('Ctrl Pts',(-8.64044941400006,15.2,-7.00444402600001));
#277819=CARTESIAN_POINT('Ctrl Pts',(-8.64358194600005,15.2,-7.00542176600001));
#277820=CARTESIAN_POINT('Ctrl Pts',(-8.64672004800006,15.2,-7.00639849700002));
#277821=CARTESIAN_POINT('Ctrl Pts',(-8.64986371500006,15.2,-7.00737421000002));
#277822=CARTESIAN_POINT('Ctrl Pts',(-8.65301294000006,15.2,-7.00834889700002));
#277823=CARTESIAN_POINT('Ctrl Pts',(-8.65616771800006,15.2,-7.00932254900002));
#277824=CARTESIAN_POINT('Ctrl Pts',(-8.65932804200006,15.2,-7.01029515700001));
#277825=CARTESIAN_POINT('Ctrl Pts',(-8.66249390600006,15.2,-7.01126671100001));
#277826=CARTESIAN_POINT('Ctrl Pts',(-8.66566530400006,15.2,-7.01223720400002));
#277827=CARTESIAN_POINT('Ctrl Pts',(-8.66884222900006,15.2,-7.01320662700001));
#277828=CARTESIAN_POINT('Ctrl Pts',(-8.67202467700006,15.2,-7.01417496900002));
#277829=CARTESIAN_POINT('Ctrl Pts',(-8.67521264100005,15.2,-7.01514222400001));
#277830=CARTESIAN_POINT('Ctrl Pts',(-8.67840611400006,15.2,-7.01610838100001));
#277831=CARTESIAN_POINT('Ctrl Pts',(-8.68160509100005,15.2,-7.01707343300002));
#277832=CARTESIAN_POINT('Ctrl Pts',(-8.68480956600006,15.2,-7.01803737000001));
#277833=CARTESIAN_POINT('Ctrl Pts',(-8.68801953200006,15.2,-7.01900018400002));
#277834=CARTESIAN_POINT('Ctrl Pts',(-8.69123498300005,15.2,-7.01996186500002));
#277835=CARTESIAN_POINT('Ctrl Pts',(-8.69445591400006,15.2,-7.02092240600001));
#277836=CARTESIAN_POINT('Ctrl Pts',(-8.69768231900006,15.2,-7.02188179800002));
#277837=CARTESIAN_POINT('Ctrl Pts',(-8.70091419100006,15.2,-7.02284003200001));
#277838=CARTESIAN_POINT('Ctrl Pts',(-8.70415152500006,15.2,-7.02379710000002));
#277839=CARTESIAN_POINT('Ctrl Pts',(-8.70739431400006,15.2,-7.02475299200002));
#277840=CARTESIAN_POINT('Ctrl Pts',(-8.71064255200006,15.2,-7.02570770100002));
#277841=CARTESIAN_POINT('Ctrl Pts',(-8.71389623400006,15.2,-7.02666121800001));
#277842=CARTESIAN_POINT('Ctrl Pts',(-8.71715535200006,15.2,-7.02761353400001));
#277843=CARTESIAN_POINT('Ctrl Pts',(-8.72041990300006,15.2,-7.02856464100002));
#277844=CARTESIAN_POINT('Ctrl Pts',(-8.72368987800006,15.2,-7.02951453100002));
#277845=CARTESIAN_POINT('Ctrl Pts',(-8.72696527300005,15.2,-7.03046319400002));
#277846=CARTESIAN_POINT('Ctrl Pts',(-8.73024608200006,15.2,-7.03141062300002));
#277847=CARTESIAN_POINT('Ctrl Pts',(-8.73353229800006,15.2,-7.03235680900002));
#277848=CARTESIAN_POINT('Ctrl Pts',(-8.73682391500006,15.2,-7.03330174300002));
#277849=CARTESIAN_POINT('Ctrl Pts',(-8.74012092800006,15.2,-7.03424541800001));
#277850=CARTESIAN_POINT('Ctrl Pts',(-8.74342333000006,15.2,-7.03518782500002));
#277851=CARTESIAN_POINT('Ctrl Pts',(-8.74673111600006,15.2,-7.03612895700001));
#277852=CARTESIAN_POINT('Ctrl Pts',(-8.75004427900006,15.2,-7.03706880200002));
#277853=CARTESIAN_POINT('Ctrl Pts',(-8.75336281400006,15.2,-7.03800735500002));
#277854=CARTESIAN_POINT('Ctrl Pts',(-8.75668671600006,15.2,-7.03894460800001));
#277855=CARTESIAN_POINT('Ctrl Pts',(-8.76001597600006,15.2,-7.03988055000002));
#277856=CARTESIAN_POINT('Ctrl Pts',(-8.76335059000006,15.2,-7.04081517500001));
#277857=CARTESIAN_POINT('Ctrl Pts',(-8.76669055200006,15.2,-7.04174847400001));
#277858=CARTESIAN_POINT('Ctrl Pts',(-8.77003585700006,15.2,-7.04268044000001));
#277859=CARTESIAN_POINT('Ctrl Pts',(-8.77338649600006,15.2,-7.04361106300002));
#277860=CARTESIAN_POINT('Ctrl Pts',(-8.77674246700006,15.2,-7.04454033500002));
#277861=CARTESIAN_POINT('Ctrl Pts',(-8.78010376100006,15.2,-7.04546825000002));
#277862=CARTESIAN_POINT('Ctrl Pts',(-8.78347037400006,15.2,-7.04639479800001));
#277863=CARTESIAN_POINT('Ctrl Pts',(-8.78684229800006,15.2,-7.04731997100002));
#277864=CARTESIAN_POINT('Ctrl Pts',(-8.79021953000005,15.2,-7.04824376100002));
#277865=CARTESIAN_POINT('Ctrl Pts',(-8.79360206200005,15.2,-7.04916616100002));
#277866=CARTESIAN_POINT('Ctrl Pts',(-8.79698988900006,15.2,-7.05008716200001));
#277867=CARTESIAN_POINT('Ctrl Pts',(-8.80038300400006,15.2,-7.05100675600002));
#277868=CARTESIAN_POINT('Ctrl Pts',(-8.80378140200006,15.2,-7.05192493600002));
#277869=CARTESIAN_POINT('Ctrl Pts',(-8.80718507800006,15.2,-7.05284169300001));
#277870=CARTESIAN_POINT('Ctrl Pts',(-8.81059402400006,15.2,-7.05375701900002));
#277871=CARTESIAN_POINT('Ctrl Pts',(-8.81400823600006,15.2,-7.05467090600001));
#277872=CARTESIAN_POINT('Ctrl Pts',(-8.81742770700006,15.2,-7.05558334800001));
#277873=CARTESIAN_POINT('Ctrl Pts',(-8.82153737602403,15.2,-7.0566765324596));
#277874=CARTESIAN_POINT('Ctrl Pts',(-8.82565491667507,15.2,-7.05776752231977));
#277875=CARTESIAN_POINT('Ctrl Pts',(-8.82978031732504,15.2,-7.05885630368026));
#277876=CARTESIAN_POINT('Ctrl Pts',(-8.8339135663501,15.2,-7.05994286263952));
#277877=CARTESIAN_POINT('Ctrl Pts',(-8.83805465100006,15.2,-7.06102717900002));
#277878=CARTESIAN_POINT('Ctrl Pts',(-8.84151077400006,15.2,-7.06192927400001));
#277879=CARTESIAN_POINT('Ctrl Pts',(-8.84497210900006,15.2,-7.06282986200002));
#277880=CARTESIAN_POINT('Ctrl Pts',(-8.84843865100006,15.2,-7.06372893100002));
#277881=CARTESIAN_POINT('Ctrl Pts',(-8.85191039400006,15.2,-7.06462647700001));
#277882=CARTESIAN_POINT('Ctrl Pts',(-8.85538733200006,15.2,-7.06552249100002));
#277883=CARTESIAN_POINT('Ctrl Pts',(-8.85886945900005,15.2,-7.06641696400002));
#277884=CARTESIAN_POINT('Ctrl Pts',(-8.86235677000006,15.2,-7.06730989100001));
#277885=CARTESIAN_POINT('Ctrl Pts',(-8.86584925900006,15.2,-7.06820126200002));
#277886=CARTESIAN_POINT('Ctrl Pts',(-8.86934691800005,15.2,-7.06909107000002));
#277887=CARTESIAN_POINT('Ctrl Pts',(-8.87284974500006,15.2,-7.06997930700001));
#277888=CARTESIAN_POINT('Ctrl Pts',(-8.87635773200006,15.2,-7.07086596600002));
#277889=CARTESIAN_POINT('Ctrl Pts',(-8.87987087300005,15.2,-7.07175104100001));
#277890=CARTESIAN_POINT('Ctrl Pts',(-8.88338916200006,15.2,-7.07263452100002));
#277891=CARTESIAN_POINT('Ctrl Pts',(-8.88691259400006,15.2,-7.07351640200002));
#277892=CARTESIAN_POINT('Ctrl Pts',(-8.89044116400006,15.2,-7.07439667400001));
#277893=CARTESIAN_POINT('Ctrl Pts',(-8.89397486600006,15.2,-7.07527533000002));
#277894=CARTESIAN_POINT('Ctrl Pts',(-8.89751369200006,15.2,-7.07615236300001));
#277895=CARTESIAN_POINT('Ctrl Pts',(-8.90105763800005,15.2,-7.07702776600001));
#277896=CARTESIAN_POINT('Ctrl Pts',(-8.90460669800006,15.2,-7.07790152900002));
#277897=CARTESIAN_POINT('Ctrl Pts',(-8.90816086700006,15.2,-7.07877364900002));
#277898=CARTESIAN_POINT('Ctrl Pts',(-8.91172013800006,15.2,-7.07964411500001));
#277899=CARTESIAN_POINT('Ctrl Pts',(-8.91528450600006,15.2,-7.08051292100001));
#277900=CARTESIAN_POINT('Ctrl Pts',(-8.91885396500006,15.2,-7.08138005800001));
#277901=CARTESIAN_POINT('Ctrl Pts',(-8.92242850800006,15.2,-7.08224552100001));
#277902=CARTESIAN_POINT('Ctrl Pts',(-8.92600813200006,15.2,-7.08310930200001));
#277903=CARTESIAN_POINT('Ctrl Pts',(-8.92959282900006,15.2,-7.08397139300001));
#277904=CARTESIAN_POINT('Ctrl Pts',(-8.93318259400005,15.2,-7.08483178600002));
#277905=CARTESIAN_POINT('Ctrl Pts',(-8.93677742100006,15.2,-7.08569047400001));
#277906=CARTESIAN_POINT('Ctrl Pts',(-8.94037730400006,15.2,-7.08654745200001));
#277907=CARTESIAN_POINT('Ctrl Pts',(-8.94398223900006,15.2,-7.08740271100002));
#277908=CARTESIAN_POINT('Ctrl Pts',(-8.94759221900006,15.2,-7.08825624300002));
#277909=CARTESIAN_POINT('Ctrl Pts',(-8.95120723800006,15.2,-7.08910804300002));
#277910=CARTESIAN_POINT('Ctrl Pts',(-8.95482729200006,15.2,-7.08995810200002));
#277911=CARTESIAN_POINT('Ctrl Pts',(-8.95845237400006,15.2,-7.09080641500002));
#277912=CARTESIAN_POINT('Ctrl Pts',(-8.96208247800006,15.2,-7.09165297200002));
#277913=CARTESIAN_POINT('Ctrl Pts',(-8.96571759800005,15.2,-7.09249776700001));
#277914=CARTESIAN_POINT('Ctrl Pts',(-8.96935772900006,15.2,-7.09334079100002));
#277915=CARTESIAN_POINT('Ctrl Pts',(-8.97300286400006,15.2,-7.09418203900002));
#277916=CARTESIAN_POINT('Ctrl Pts',(-8.97665299700006,15.2,-7.09502150300001));
#277917=CARTESIAN_POINT('Ctrl Pts',(-8.98030812400006,15.2,-7.09585917500001));
#277918=CARTESIAN_POINT('Ctrl Pts',(-8.98396824000006,15.2,-7.09669505000001));
#277919=CARTESIAN_POINT('Ctrl Pts',(-8.98763333900006,15.2,-7.09752912300001));
#277920=CARTESIAN_POINT('Ctrl Pts',(-8.99130341600006,15.2,-7.09836138400001));
#277921=CARTESIAN_POINT('Ctrl Pts',(-8.99497846500006,15.2,-7.09919182900002));
#277922=CARTESIAN_POINT('Ctrl Pts',(-8.99865848200006,15.2,-7.10002045100002));
#277923=CARTESIAN_POINT('Ctrl Pts',(-9.00234345900006,15.2,-7.10084724000002));
#277924=CARTESIAN_POINT('Ctrl Pts',(-9.00603338900006,15.2,-7.10167218900001));
#277925=CARTESIAN_POINT('Ctrl Pts',(-9.00972826500006,15.2,-7.10249528800002));
#277926=CARTESIAN_POINT('Ctrl Pts',(-9.01342808000006,15.2,-7.10331652800001));
#277927=CARTESIAN_POINT('Ctrl Pts',(-9.01713282900005,15.2,-7.10413590400002));
#277928=CARTESIAN_POINT('Ctrl Pts',(-9.02084250600005,15.2,-7.10495340800002));
#277929=CARTESIAN_POINT('Ctrl Pts',(-9.02455710700006,15.2,-7.10576903500002));
#277930=CARTESIAN_POINT('Ctrl Pts',(-9.02827662900006,15.2,-7.10658278400001));
#277931=CARTESIAN_POINT('Ctrl Pts',(-9.03200107200006,15.2,-7.10739465100002));
#277932=CARTESIAN_POINT('Ctrl Pts',(-9.03498456200006,15.2,-7.10804263900001));
#277933=CARTESIAN_POINT('Ctrl Pts',(-9.03722439200006,15.2,-7.10852778400002));
#277934=CARTESIAN_POINT('Ctrl Pts',(-9.03871859600006,15.2,-7.10885083600001));
#277935=CARTESIAN_POINT('Ctrl Pts',(-9.03946594400006,15.2,-7.10901226900001));
#277936=CARTESIAN_POINT('Ctrl Pts',(-8.56667971000006,15.2,-5.85257411400002));
#277937=CARTESIAN_POINT('Ctrl Pts',(-8.56667971000006,11.6,-5.85257411400002));
#277938=CARTESIAN_POINT('Ctrl Pts',(-8.56681469200005,15.2,-5.85268447900001));
#277939=CARTESIAN_POINT('Ctrl Pts',(-8.56681469200005,11.6,-5.85268447900001));
#277940=CARTESIAN_POINT('Ctrl Pts',(-8.56708931800006,15.2,-5.85290912800002));
#277941=CARTESIAN_POINT('Ctrl Pts',(-8.56708931800006,11.6,-5.85290912800002));
#277942=CARTESIAN_POINT('Ctrl Pts',(-8.56750527400006,15.2,-5.85324973300001));
#277943=CARTESIAN_POINT('Ctrl Pts',(-8.56750527400006,11.6,-5.85324973300001));
#277944=CARTESIAN_POINT('Ctrl Pts',(-8.56806526200005,15.2,-5.85370897400002));
#277945=CARTESIAN_POINT('Ctrl Pts',(-8.56806526200005,11.6,-5.85370897400002));
#277946=CARTESIAN_POINT('Ctrl Pts',(-8.56877298400006,15.2,-5.85429055400001));
#277947=CARTESIAN_POINT('Ctrl Pts',(-8.56877298400006,11.6,-5.85429055400001));
#277948=CARTESIAN_POINT('Ctrl Pts',(-8.56949158200005,15.2,-5.85488228200001));
#277949=CARTESIAN_POINT('Ctrl Pts',(-8.56949158200005,11.6,-5.85488228200001));
#277950=CARTESIAN_POINT('Ctrl Pts',(-8.57021692700006,15.2,-5.85548078500001));
#277951=CARTESIAN_POINT('Ctrl Pts',(-8.57021692700006,11.6,-5.85548078500001));
#277952=CARTESIAN_POINT('Ctrl Pts',(-8.57094898300006,15.2,-5.85608606100001));
#277953=CARTESIAN_POINT('Ctrl Pts',(-8.57094898300006,11.6,-5.85608606100001));
#277954=CARTESIAN_POINT('Ctrl Pts',(-8.57168771900006,15.2,-5.85669810600002));
#277955=CARTESIAN_POINT('Ctrl Pts',(-8.57168771900006,11.6,-5.85669810600002));
#277956=CARTESIAN_POINT('Ctrl Pts',(-8.57243310300005,15.2,-5.85731691800002));
#277957=CARTESIAN_POINT('Ctrl Pts',(-8.57243310300005,11.6,-5.85731691800002));
#277958=CARTESIAN_POINT('Ctrl Pts',(-8.57318510400006,15.2,-5.85794249300001));
#277959=CARTESIAN_POINT('Ctrl Pts',(-8.57318510400006,11.6,-5.85794249300001));
#277960=CARTESIAN_POINT('Ctrl Pts',(-8.57394368900006,15.2,-5.85857482800002));
#277961=CARTESIAN_POINT('Ctrl Pts',(-8.57394368900006,11.6,-5.85857482800002));
#277962=CARTESIAN_POINT('Ctrl Pts',(-8.57470882600006,15.2,-5.85921392000002));
#277963=CARTESIAN_POINT('Ctrl Pts',(-8.57470882600006,11.6,-5.85921392000002));
#277964=CARTESIAN_POINT('Ctrl Pts',(-8.57548048600006,15.2,-5.85985976500002));
#277965=CARTESIAN_POINT('Ctrl Pts',(-8.57548048600006,11.6,-5.85985976500002));
#277966=CARTESIAN_POINT('Ctrl Pts',(-8.57625863500006,15.2,-5.86051236100002));
#277967=CARTESIAN_POINT('Ctrl Pts',(-8.57625863500006,11.6,-5.86051236100002));
#277968=CARTESIAN_POINT('Ctrl Pts',(-8.57704324400006,15.2,-5.86117170400002));
#277969=CARTESIAN_POINT('Ctrl Pts',(-8.57704324400006,11.6,-5.86117170400002));
#277970=CARTESIAN_POINT('Ctrl Pts',(-8.57783428100005,15.2,-5.86183779100002));
#277971=CARTESIAN_POINT('Ctrl Pts',(-8.57783428100005,11.6,-5.86183779100002));
#277972=CARTESIAN_POINT('Ctrl Pts',(-8.57863171500006,15.2,-5.86251061900001));
#277973=CARTESIAN_POINT('Ctrl Pts',(-8.57863171500006,11.6,-5.86251061900001));
#277974=CARTESIAN_POINT('Ctrl Pts',(-8.57943551500006,15.2,-5.86319018600002));
#277975=CARTESIAN_POINT('Ctrl Pts',(-8.57943551500006,11.6,-5.86319018600002));
#277976=CARTESIAN_POINT('Ctrl Pts',(-8.58024565200006,15.2,-5.86387648600001));
#277977=CARTESIAN_POINT('Ctrl Pts',(-8.58024565200006,11.6,-5.86387648600001));
#277978=CARTESIAN_POINT('Ctrl Pts',(-8.58106209400006,15.2,-5.86456951900002));
#277979=CARTESIAN_POINT('Ctrl Pts',(-8.58106209400006,11.6,-5.86456951900002));
#277980=CARTESIAN_POINT('Ctrl Pts',(-8.58188481200006,15.2,-5.86526928000002));
#277981=CARTESIAN_POINT('Ctrl Pts',(-8.58188481200006,11.6,-5.86526928000002));
#277982=CARTESIAN_POINT('Ctrl Pts',(-8.58271377600006,15.2,-5.86597576500001));
#277983=CARTESIAN_POINT('Ctrl Pts',(-8.58271377600006,11.6,-5.86597576500001));
#277984=CARTESIAN_POINT('Ctrl Pts',(-8.58354895500005,15.2,-5.86668897300001));
#277985=CARTESIAN_POINT('Ctrl Pts',(-8.58354895500005,11.6,-5.86668897300001));
#277986=CARTESIAN_POINT('Ctrl Pts',(-8.58439032000006,15.2,-5.86740890000002));
#277987=CARTESIAN_POINT('Ctrl Pts',(-8.58439032000006,11.6,-5.86740890000002));
#277988=CARTESIAN_POINT('Ctrl Pts',(-8.58523784000005,15.2,-5.86813554200001));
#277989=CARTESIAN_POINT('Ctrl Pts',(-8.58523784000005,11.6,-5.86813554200001));
#277990=CARTESIAN_POINT('Ctrl Pts',(-8.58609148800005,15.2,-5.86886889800001));
#277991=CARTESIAN_POINT('Ctrl Pts',(-8.58609148800005,11.6,-5.86886889800001));
#277992=CARTESIAN_POINT('Ctrl Pts',(-8.58695123200006,15.2,-5.86960896200001));
#277993=CARTESIAN_POINT('Ctrl Pts',(-8.58695123200006,11.6,-5.86960896200001));
#277994=CARTESIAN_POINT('Ctrl Pts',(-8.58781704400006,15.2,-5.87035573200002));
#277995=CARTESIAN_POINT('Ctrl Pts',(-8.58781704400006,11.6,-5.87035573200002));
#277996=CARTESIAN_POINT('Ctrl Pts',(-8.58868889600006,15.2,-5.87110920600002));
#277997=CARTESIAN_POINT('Ctrl Pts',(-8.58868889600006,11.6,-5.87110920600002));
#277998=CARTESIAN_POINT('Ctrl Pts',(-8.58956675800006,15.2,-5.87186938100002));
#277999=CARTESIAN_POINT('Ctrl Pts',(-8.58956675800006,11.6,-5.87186938100002));
#278000=CARTESIAN_POINT('Ctrl Pts',(-8.59045060000006,15.2,-5.87263625100002));
#278001=CARTESIAN_POINT('Ctrl Pts',(-8.59045060000006,11.6,-5.87263625100002));
#278002=CARTESIAN_POINT('Ctrl Pts',(-8.59134039400006,15.2,-5.87340981600001));
#278003=CARTESIAN_POINT('Ctrl Pts',(-8.59134039400006,11.6,-5.87340981600001));
#278004=CARTESIAN_POINT('Ctrl Pts',(-8.59223611300006,15.2,-5.87419007000002));
#278005=CARTESIAN_POINT('Ctrl Pts',(-8.59223611300006,11.6,-5.87419007000002));
#278006=CARTESIAN_POINT('Ctrl Pts',(-8.59313772800006,15.2,-5.87497701200002));
#278007=CARTESIAN_POINT('Ctrl Pts',(-8.59313772800006,11.6,-5.87497701200002));
#278008=CARTESIAN_POINT('Ctrl Pts',(-8.59404520800006,15.2,-5.87577063900002));
#278009=CARTESIAN_POINT('Ctrl Pts',(-8.59404520800006,11.6,-5.87577063900002));
#278010=CARTESIAN_POINT('Ctrl Pts',(-8.59495852900006,15.2,-5.87657094700001));
#278011=CARTESIAN_POINT('Ctrl Pts',(-8.59495852900006,11.6,-5.87657094700001));
#278012=CARTESIAN_POINT('Ctrl Pts',(-8.59587766000006,15.2,-5.87737793200001));
#278013=CARTESIAN_POINT('Ctrl Pts',(-8.59587766000006,11.6,-5.87737793200001));
#278014=CARTESIAN_POINT('Ctrl Pts',(-8.59680257500005,15.2,-5.87819159300001));
#278015=CARTESIAN_POINT('Ctrl Pts',(-8.59680257500005,11.6,-5.87819159300001));
#278016=CARTESIAN_POINT('Ctrl Pts',(-8.59773324400006,15.2,-5.87901192500001));
#278017=CARTESIAN_POINT('Ctrl Pts',(-8.59773324400006,11.6,-5.87901192500001));
#278018=CARTESIAN_POINT('Ctrl Pts',(-8.59866964200006,15.2,-5.87983892500001));
#278019=CARTESIAN_POINT('Ctrl Pts',(-8.59866964200006,11.6,-5.87983892500001));
#278020=CARTESIAN_POINT('Ctrl Pts',(-8.59961174000006,15.2,-5.88067259100002));
#278021=CARTESIAN_POINT('Ctrl Pts',(-8.59961174000006,11.6,-5.88067259100002));
#278022=CARTESIAN_POINT('Ctrl Pts',(-8.60055950900006,15.2,-5.88151292000001));
#278023=CARTESIAN_POINT('Ctrl Pts',(-8.60055950900006,11.6,-5.88151292000001));
#278024=CARTESIAN_POINT('Ctrl Pts',(-8.60151292500005,15.2,-5.88235990700002));
#278025=CARTESIAN_POINT('Ctrl Pts',(-8.60151292500005,11.6,-5.88235990700002));
#278026=CARTESIAN_POINT('Ctrl Pts',(-8.60247195900006,15.2,-5.88321355000001));
#278027=CARTESIAN_POINT('Ctrl Pts',(-8.60247195900006,11.6,-5.88321355000001));
#278028=CARTESIAN_POINT('Ctrl Pts',(-8.60343658500006,15.2,-5.88407384600002));
#278029=CARTESIAN_POINT('Ctrl Pts',(-8.60343658500006,11.6,-5.88407384600002));
#278030=CARTESIAN_POINT('Ctrl Pts',(-8.60440677400006,15.2,-5.88494079200002));
#278031=CARTESIAN_POINT('Ctrl Pts',(-8.60440677400006,11.6,-5.88494079200002));
#278032=CARTESIAN_POINT('Ctrl Pts',(-8.60538250200005,15.2,-5.88581438400002));
#278033=CARTESIAN_POINT('Ctrl Pts',(-8.60538250200005,11.6,-5.88581438400002));
#278034=CARTESIAN_POINT('Ctrl Pts',(-8.60636373900006,15.2,-5.88669461900002));
#278035=CARTESIAN_POINT('Ctrl Pts',(-8.60636373900006,11.6,-5.88669461900002));
#278036=CARTESIAN_POINT('Ctrl Pts',(-8.60735046200006,15.2,-5.88758149500002));
#278037=CARTESIAN_POINT('Ctrl Pts',(-8.60735046200006,11.6,-5.88758149500002));
#278038=CARTESIAN_POINT('Ctrl Pts',(-8.60834264200006,15.2,-5.88847500800001));
#278039=CARTESIAN_POINT('Ctrl Pts',(-8.60834264200006,11.6,-5.88847500800001));
#278040=CARTESIAN_POINT('Ctrl Pts',(-8.60934025400006,15.2,-5.88937515500002));
#278041=CARTESIAN_POINT('Ctrl Pts',(-8.60934025400006,11.6,-5.88937515500002));
#278042=CARTESIAN_POINT('Ctrl Pts',(-8.61034327100005,15.2,-5.89028193300001));
#278043=CARTESIAN_POINT('Ctrl Pts',(-8.61034327100005,11.6,-5.89028193300001));
#278044=CARTESIAN_POINT('Ctrl Pts',(-8.61135166800005,15.2,-5.89119533800002));
#278045=CARTESIAN_POINT('Ctrl Pts',(-8.61135166800005,11.6,-5.89119533800002));
#278046=CARTESIAN_POINT('Ctrl Pts',(-8.61236541700006,15.2,-5.89211536900001));
#278047=CARTESIAN_POINT('Ctrl Pts',(-8.61236541700006,11.6,-5.89211536900001));
#278048=CARTESIAN_POINT('Ctrl Pts',(-8.61338449500006,15.2,-5.89304202000001));
#278049=CARTESIAN_POINT('Ctrl Pts',(-8.61338449500006,11.6,-5.89304202000001));
#278050=CARTESIAN_POINT('Ctrl Pts',(-8.61440887300006,15.2,-5.89397529000002));
#278051=CARTESIAN_POINT('Ctrl Pts',(-8.61440887300006,11.6,-5.89397529000002));
#278052=CARTESIAN_POINT('Ctrl Pts',(-8.61543852900006,15.2,-5.89491517500001));
#278053=CARTESIAN_POINT('Ctrl Pts',(-8.61543852900006,11.6,-5.89491517500001));
#278054=CARTESIAN_POINT('Ctrl Pts',(-8.61647343400006,15.2,-5.89586167100002));
#278055=CARTESIAN_POINT('Ctrl Pts',(-8.61647343400006,11.6,-5.89586167100002));
#278056=CARTESIAN_POINT('Ctrl Pts',(-8.61751356400006,15.2,-5.89681477700001));
#278057=CARTESIAN_POINT('Ctrl Pts',(-8.61751356400006,11.6,-5.89681477700001));
#278058=CARTESIAN_POINT('Ctrl Pts',(-8.61855889400006,15.2,-5.89777448800002));
#278059=CARTESIAN_POINT('Ctrl Pts',(-8.61855889400006,11.6,-5.89777448800002));
#278060=CARTESIAN_POINT('Ctrl Pts',(-8.61960939900005,15.2,-5.89874080200002));
#278061=CARTESIAN_POINT('Ctrl Pts',(-8.61960939900005,11.6,-5.89874080200002));
#278062=CARTESIAN_POINT('Ctrl Pts',(-8.62066505300006,15.2,-5.89971371600001));
#278063=CARTESIAN_POINT('Ctrl Pts',(-8.62066505300006,11.6,-5.89971371600001));
#278064=CARTESIAN_POINT('Ctrl Pts',(-8.62172583200006,15.2,-5.90069322500002));
#278065=CARTESIAN_POINT('Ctrl Pts',(-8.62172583200006,11.6,-5.90069322500002));
#278066=CARTESIAN_POINT('Ctrl Pts',(-8.62279170900005,15.2,-5.90167932800002));
#278067=CARTESIAN_POINT('Ctrl Pts',(-8.62279170900005,11.6,-5.90167932800002));
#278068=CARTESIAN_POINT('Ctrl Pts',(-8.62386266200006,15.2,-5.90267202100001));
#278069=CARTESIAN_POINT('Ctrl Pts',(-8.62386266200006,11.6,-5.90267202100001));
#278070=CARTESIAN_POINT('Ctrl Pts',(-8.62493866400006,15.2,-5.90367130100002));
#278071=CARTESIAN_POINT('Ctrl Pts',(-8.62493866400006,11.6,-5.90367130100002));
#278072=CARTESIAN_POINT('Ctrl Pts',(-8.62601969300006,15.2,-5.90467716400001));
#278073=CARTESIAN_POINT('Ctrl Pts',(-8.62601969300006,11.6,-5.90467716400001));
#278074=CARTESIAN_POINT('Ctrl Pts',(-8.62710572200006,15.2,-5.90568960800002));
#278075=CARTESIAN_POINT('Ctrl Pts',(-8.62710572200006,11.6,-5.90568960800002));
#278076=CARTESIAN_POINT('Ctrl Pts',(-8.62819672800006,15.2,-5.90670862900001));
#278077=CARTESIAN_POINT('Ctrl Pts',(-8.62819672800006,11.6,-5.90670862900001));
#278078=CARTESIAN_POINT('Ctrl Pts',(-8.62929268600006,15.2,-5.90773422500002));
#278079=CARTESIAN_POINT('Ctrl Pts',(-8.62929268600006,11.6,-5.90773422500002));
#278080=CARTESIAN_POINT('Ctrl Pts',(-8.63039357300006,15.2,-5.90876639200002));
#278081=CARTESIAN_POINT('Ctrl Pts',(-8.63039357300006,11.6,-5.90876639200002));
#278082=CARTESIAN_POINT('Ctrl Pts',(-8.63149936300006,15.2,-5.90980512700002));
#278083=CARTESIAN_POINT('Ctrl Pts',(-8.63149936300006,11.6,-5.90980512700002));
#278084=CARTESIAN_POINT('Ctrl Pts',(-8.63261003400006,15.2,-5.91085042600002));
#278085=CARTESIAN_POINT('Ctrl Pts',(-8.63261003400006,11.6,-5.91085042600002));
#278086=CARTESIAN_POINT('Ctrl Pts',(-8.63372556100006,15.2,-5.91190228700002));
#278087=CARTESIAN_POINT('Ctrl Pts',(-8.63372556100006,11.6,-5.91190228700002));
#278088=CARTESIAN_POINT('Ctrl Pts',(-8.63484592000006,15.2,-5.91296070700002));
#278089=CARTESIAN_POINT('Ctrl Pts',(-8.63484592000006,11.6,-5.91296070700002));
#278090=CARTESIAN_POINT('Ctrl Pts',(-8.63597108800005,15.2,-5.91402568300002));
#278091=CARTESIAN_POINT('Ctrl Pts',(-8.63597108800005,11.6,-5.91402568300002));
#278092=CARTESIAN_POINT('Ctrl Pts',(-8.63710104100005,15.2,-5.91509721000002));
#278093=CARTESIAN_POINT('Ctrl Pts',(-8.63710104100005,11.6,-5.91509721000002));
#278094=CARTESIAN_POINT('Ctrl Pts',(-8.63823575600006,15.2,-5.91617528700001));
#278095=CARTESIAN_POINT('Ctrl Pts',(-8.63823575600006,11.6,-5.91617528700001));
#278096=CARTESIAN_POINT('Ctrl Pts',(-8.63937520800006,15.2,-5.91725991000001));
#278097=CARTESIAN_POINT('Ctrl Pts',(-8.63937520800006,11.6,-5.91725991000001));
#278098=CARTESIAN_POINT('Ctrl Pts',(-8.64051937700006,15.2,-5.91835107600001));
#278099=CARTESIAN_POINT('Ctrl Pts',(-8.64051937700006,11.6,-5.91835107600001));
#278100=CARTESIAN_POINT('Ctrl Pts',(-8.64166823700005,15.2,-5.91944878100002));
#278101=CARTESIAN_POINT('Ctrl Pts',(-8.64166823700005,11.6,-5.91944878100002));
#278102=CARTESIAN_POINT('Ctrl Pts',(-8.64282176500006,15.2,-5.92055302300002));
#278103=CARTESIAN_POINT('Ctrl Pts',(-8.64282176500006,11.6,-5.92055302300002));
#278104=CARTESIAN_POINT('Ctrl Pts',(-8.64397994000005,15.2,-5.92166379800001));
#278105=CARTESIAN_POINT('Ctrl Pts',(-8.64397994000005,11.6,-5.92166379800001));
#278106=CARTESIAN_POINT('Ctrl Pts',(-8.64514273700006,15.2,-5.92278110300001));
#278107=CARTESIAN_POINT('Ctrl Pts',(-8.64514273700006,11.6,-5.92278110300001));
#278108=CARTESIAN_POINT('Ctrl Pts',(-8.64631013400006,15.2,-5.92390493600002));
#278109=CARTESIAN_POINT('Ctrl Pts',(-8.64631013400006,11.6,-5.92390493600002));
#278110=CARTESIAN_POINT('Ctrl Pts',(-8.64748210800006,15.2,-5.92503529300001));
#278111=CARTESIAN_POINT('Ctrl Pts',(-8.64748210800006,11.6,-5.92503529300001));
#278112=CARTESIAN_POINT('Ctrl Pts',(-8.64865863600006,15.2,-5.92617216900001));
#278113=CARTESIAN_POINT('Ctrl Pts',(-8.64865863600006,11.6,-5.92617216900001));
#278114=CARTESIAN_POINT('Ctrl Pts',(-8.64983969600006,15.2,-5.92731556500001));
#278115=CARTESIAN_POINT('Ctrl Pts',(-8.64983969600006,11.6,-5.92731556500001));
#278116=CARTESIAN_POINT('Ctrl Pts',(-8.65102526500005,15.2,-5.92846547300002));
#278117=CARTESIAN_POINT('Ctrl Pts',(-8.65102526500005,11.6,-5.92846547300002));
#278118=CARTESIAN_POINT('Ctrl Pts',(-8.65221532200006,15.2,-5.92962189400002));
#278119=CARTESIAN_POINT('Ctrl Pts',(-8.65221532200006,11.6,-5.92962189400002));
#278120=CARTESIAN_POINT('Ctrl Pts',(-8.65340984400006,15.2,-5.93078482300001));
#278121=CARTESIAN_POINT('Ctrl Pts',(-8.65340984400006,11.6,-5.93078482300001));
#278122=CARTESIAN_POINT('Ctrl Pts',(-8.65460880700006,15.2,-5.93195425700002));
#278123=CARTESIAN_POINT('Ctrl Pts',(-8.65460880700006,11.6,-5.93195425700002));
#278124=CARTESIAN_POINT('Ctrl Pts',(-8.65581219200006,15.2,-5.93313019200002));
#278125=CARTESIAN_POINT('Ctrl Pts',(-8.65581219200006,11.6,-5.93313019200002));
#278126=CARTESIAN_POINT('Ctrl Pts',(-8.65701997300006,15.2,-5.93431262700002));
#278127=CARTESIAN_POINT('Ctrl Pts',(-8.65701997300006,11.6,-5.93431262700002));
#278128=CARTESIAN_POINT('Ctrl Pts',(-8.65823213200006,15.2,-5.93550155700001));
#278129=CARTESIAN_POINT('Ctrl Pts',(-8.65823213200006,11.6,-5.93550155700001));
#278130=CARTESIAN_POINT('Ctrl Pts',(-8.65944864600005,15.2,-5.93669697900002));
#278131=CARTESIAN_POINT('Ctrl Pts',(-8.65944864600005,11.6,-5.93669697900002));
#278132=CARTESIAN_POINT('Ctrl Pts',(-8.66066949100006,15.2,-5.93789889000002));
#278133=CARTESIAN_POINT('Ctrl Pts',(-8.66066949100006,11.6,-5.93789889000002));
#278134=CARTESIAN_POINT('Ctrl Pts',(-8.66189464700006,15.2,-5.93910728900001));
#278135=CARTESIAN_POINT('Ctrl Pts',(-8.66189464700006,11.6,-5.93910728900001));
#278136=CARTESIAN_POINT('Ctrl Pts',(-8.66312409300006,15.2,-5.94032216900001));
#278137=CARTESIAN_POINT('Ctrl Pts',(-8.66312409300006,11.6,-5.94032216900001));
#278138=CARTESIAN_POINT('Ctrl Pts',(-8.66435780700006,15.2,-5.94154352900001));
#278139=CARTESIAN_POINT('Ctrl Pts',(-8.66435780700006,11.6,-5.94154352900001));
#278140=CARTESIAN_POINT('Ctrl Pts',(-8.66559576700006,15.2,-5.94277136600001));
#278141=CARTESIAN_POINT('Ctrl Pts',(-8.66559576700006,11.6,-5.94277136600001));
#278142=CARTESIAN_POINT('Ctrl Pts',(-8.66683795200006,15.2,-5.94400567600001));
#278143=CARTESIAN_POINT('Ctrl Pts',(-8.66683795200006,11.6,-5.94400567600001));
#278144=CARTESIAN_POINT('Ctrl Pts',(-8.66808434000006,15.2,-5.94524645700002));
#278145=CARTESIAN_POINT('Ctrl Pts',(-8.66808434000006,11.6,-5.94524645700002));
#278146=CARTESIAN_POINT('Ctrl Pts',(-8.66933491100006,15.2,-5.94649370400001));
#278147=CARTESIAN_POINT('Ctrl Pts',(-8.66933491100006,11.6,-5.94649370400001));
#278148=CARTESIAN_POINT('Ctrl Pts',(-8.67058964300006,15.2,-5.94774741600002));
#278149=CARTESIAN_POINT('Ctrl Pts',(-8.67058964300006,11.6,-5.94774741600002));
#278150=CARTESIAN_POINT('Ctrl Pts',(-8.67184851500006,15.2,-5.94900758800001));
#278151=CARTESIAN_POINT('Ctrl Pts',(-8.67184851500006,11.6,-5.94900758800001));
#278152=CARTESIAN_POINT('Ctrl Pts',(-8.67311150600005,15.2,-5.95027421800002));
#278153=CARTESIAN_POINT('Ctrl Pts',(-8.67311150600005,11.6,-5.95027421800002));
#278154=CARTESIAN_POINT('Ctrl Pts',(-8.67437859500006,15.2,-5.95154730200001));
#278155=CARTESIAN_POINT('Ctrl Pts',(-8.67437859500006,11.6,-5.95154730200001));
#278156=CARTESIAN_POINT('Ctrl Pts',(-8.67564976200006,15.2,-5.95282683700002));
#278157=CARTESIAN_POINT('Ctrl Pts',(-8.67564976200006,11.6,-5.95282683700002));
#278158=CARTESIAN_POINT('Ctrl Pts',(-8.67692498600006,15.2,-5.95411282200002));
#278159=CARTESIAN_POINT('Ctrl Pts',(-8.67692498600006,11.6,-5.95411282200002));
#278160=CARTESIAN_POINT('Ctrl Pts',(-8.67820424500006,15.2,-5.95540525000001));
#278161=CARTESIAN_POINT('Ctrl Pts',(-8.67820424500006,11.6,-5.95540525000001));
#278162=CARTESIAN_POINT('Ctrl Pts',(-8.67948752100006,15.2,-5.95670412000001));
#278163=CARTESIAN_POINT('Ctrl Pts',(-8.67948752100006,11.6,-5.95670412000001));
#278164=CARTESIAN_POINT('Ctrl Pts',(-8.68077479100006,15.2,-5.95800942900001));
#278165=CARTESIAN_POINT('Ctrl Pts',(-8.68077479100006,11.6,-5.95800942900001));
#278166=CARTESIAN_POINT('Ctrl Pts',(-8.68206603400006,15.2,-5.95932117300002));
#278167=CARTESIAN_POINT('Ctrl Pts',(-8.68206603400006,11.6,-5.95932117300002));
#278168=CARTESIAN_POINT('Ctrl Pts',(-8.68336123200006,15.2,-5.96063934900001));
#278169=CARTESIAN_POINT('Ctrl Pts',(-8.68336123200006,11.6,-5.96063934900001));
#278170=CARTESIAN_POINT('Ctrl Pts',(-8.68466036500006,15.2,-5.96196395400002));
#278171=CARTESIAN_POINT('Ctrl Pts',(-8.68466036500006,11.6,-5.96196395400002));
#278172=CARTESIAN_POINT('Ctrl Pts',(-8.68596340900006,15.2,-5.96329498600002));
#278173=CARTESIAN_POINT('Ctrl Pts',(-8.68596340900006,11.6,-5.96329498600002));
#278174=CARTESIAN_POINT('Ctrl Pts',(-8.68727034800006,15.2,-5.96463244000002));
#278175=CARTESIAN_POINT('Ctrl Pts',(-8.68727034800006,11.6,-5.96463244000002));
#278176=CARTESIAN_POINT('Ctrl Pts',(-8.68858116100006,15.2,-5.96597631400002));
#278177=CARTESIAN_POINT('Ctrl Pts',(-8.68858116100006,11.6,-5.96597631400002));
#278178=CARTESIAN_POINT('Ctrl Pts',(-8.68989582600006,15.2,-5.96732660300002));
#278179=CARTESIAN_POINT('Ctrl Pts',(-8.68989582600006,11.6,-5.96732660300002));
#278180=CARTESIAN_POINT('Ctrl Pts',(-8.69121432400006,15.2,-5.96868330600002));
#278181=CARTESIAN_POINT('Ctrl Pts',(-8.69121432400006,11.6,-5.96868330600002));
#278182=CARTESIAN_POINT('Ctrl Pts',(-8.69253663700006,15.2,-5.97004641800002));
#278183=CARTESIAN_POINT('Ctrl Pts',(-8.69253663700006,11.6,-5.97004641800002));
#278184=CARTESIAN_POINT('Ctrl Pts',(-8.69386274300006,15.2,-5.97141593800002));
#278185=CARTESIAN_POINT('Ctrl Pts',(-8.69386274300006,11.6,-5.97141593800002));
#278186=CARTESIAN_POINT('Ctrl Pts',(-8.69519262200006,15.2,-5.97279186100002));
#278187=CARTESIAN_POINT('Ctrl Pts',(-8.69519262200006,11.6,-5.97279186100002));
#278188=CARTESIAN_POINT('Ctrl Pts',(-8.69652625700006,15.2,-5.97417418400001));
#278189=CARTESIAN_POINT('Ctrl Pts',(-8.69652625700006,11.6,-5.97417418400001));
#278190=CARTESIAN_POINT('Ctrl Pts',(-8.69786362600006,15.2,-5.97556290600001));
#278191=CARTESIAN_POINT('Ctrl Pts',(-8.69786362600006,11.6,-5.97556290600001));
#278192=CARTESIAN_POINT('Ctrl Pts',(-8.69920471000006,15.2,-5.97695802000001));
#278193=CARTESIAN_POINT('Ctrl Pts',(-8.69920471000006,11.6,-5.97695802000001));
#278194=CARTESIAN_POINT('Ctrl Pts',(-8.70054949000006,15.2,-5.97835952600001));
#278195=CARTESIAN_POINT('Ctrl Pts',(-8.70054949000006,11.6,-5.97835952600001));
#278196=CARTESIAN_POINT('Ctrl Pts',(-8.70189794500006,15.2,-5.97976741900001));
#278197=CARTESIAN_POINT('Ctrl Pts',(-8.70189794500006,11.6,-5.97976741900001));
#278198=CARTESIAN_POINT('Ctrl Pts',(-8.70325005900006,15.2,-5.98118169700002));
#278199=CARTESIAN_POINT('Ctrl Pts',(-8.70325005900006,11.6,-5.98118169700002));
#278200=CARTESIAN_POINT('Ctrl Pts',(-8.70460581000006,15.2,-5.98260235600002));
#278201=CARTESIAN_POINT('Ctrl Pts',(-8.70460581000006,11.6,-5.98260235600002));
#278202=CARTESIAN_POINT('Ctrl Pts',(-8.70596518000006,15.2,-5.98402939300002));
#278203=CARTESIAN_POINT('Ctrl Pts',(-8.70596518000006,11.6,-5.98402939300002));
#278204=CARTESIAN_POINT('Ctrl Pts',(-8.70732814900006,15.2,-5.98546280500001));
#278205=CARTESIAN_POINT('Ctrl Pts',(-8.70732814900006,11.6,-5.98546280500001));
#278206=CARTESIAN_POINT('Ctrl Pts',(-8.70869469900006,15.2,-5.98690258900002));
#278207=CARTESIAN_POINT('Ctrl Pts',(-8.70869469900006,11.6,-5.98690258900002));
#278208=CARTESIAN_POINT('Ctrl Pts',(-8.71006481000006,15.2,-5.98834874100002));
#278209=CARTESIAN_POINT('Ctrl Pts',(-8.71006481000006,11.6,-5.98834874100002));
#278210=CARTESIAN_POINT('Ctrl Pts',(-8.71143846400006,15.2,-5.98980125800002));
#278211=CARTESIAN_POINT('Ctrl Pts',(-8.71143846400006,11.6,-5.98980125800002));
#278212=CARTESIAN_POINT('Ctrl Pts',(-8.71281564200006,15.2,-5.99126013700002));
#278213=CARTESIAN_POINT('Ctrl Pts',(-8.71281564200006,11.6,-5.99126013700002));
#278214=CARTESIAN_POINT('Ctrl Pts',(-8.71419632600006,15.2,-5.99272537600001));
#278215=CARTESIAN_POINT('Ctrl Pts',(-8.71419632600006,11.6,-5.99272537600001));
#278216=CARTESIAN_POINT('Ctrl Pts',(-8.71558049500005,15.2,-5.99419696900001));
#278217=CARTESIAN_POINT('Ctrl Pts',(-8.71558049500005,11.6,-5.99419696900001));
#278218=CARTESIAN_POINT('Ctrl Pts',(-8.71696813200005,15.2,-5.99567491600002));
#278219=CARTESIAN_POINT('Ctrl Pts',(-8.71696813200005,11.6,-5.99567491600002));
#278220=CARTESIAN_POINT('Ctrl Pts',(-8.71835921700006,15.2,-5.99715921100002));
#278221=CARTESIAN_POINT('Ctrl Pts',(-8.71835921700006,11.6,-5.99715921100002));
#278222=CARTESIAN_POINT('Ctrl Pts',(-8.71975373500005,15.2,-5.99864985300002));
#278223=CARTESIAN_POINT('Ctrl Pts',(-8.71975373500005,11.6,-5.99864985300002));
#278224=CARTESIAN_POINT('Ctrl Pts',(-8.72115166300006,15.2,-6.00014683800002));
#278225=CARTESIAN_POINT('Ctrl Pts',(-8.72115166300006,11.6,-6.00014683800002));
#278226=CARTESIAN_POINT('Ctrl Pts',(-8.72255298500006,15.2,-6.00165016200001));
#278227=CARTESIAN_POINT('Ctrl Pts',(-8.72255298500006,11.6,-6.00165016200001));
#278228=CARTESIAN_POINT('Ctrl Pts',(-8.72395768300006,15.2,-6.00315982300001));
#278229=CARTESIAN_POINT('Ctrl Pts',(-8.72395768300006,11.6,-6.00315982300001));
#278230=CARTESIAN_POINT('Ctrl Pts',(-8.72536573800006,15.2,-6.00467581600002));
#278231=CARTESIAN_POINT('Ctrl Pts',(-8.72536573800006,11.6,-6.00467581600002));
#278232=CARTESIAN_POINT('Ctrl Pts',(-8.72677713200006,15.2,-6.00619814100002));
#278233=CARTESIAN_POINT('Ctrl Pts',(-8.72677713200006,11.6,-6.00619814100002));
#278234=CARTESIAN_POINT('Ctrl Pts',(-8.72819184600005,15.2,-6.00772679200002));
#278235=CARTESIAN_POINT('Ctrl Pts',(-8.72819184600005,11.6,-6.00772679200002));
#278236=CARTESIAN_POINT('Ctrl Pts',(-8.72960986400006,15.2,-6.00926176600002));
#278237=CARTESIAN_POINT('Ctrl Pts',(-8.72960986400006,11.6,-6.00926176600002));
#278238=CARTESIAN_POINT('Ctrl Pts',(-8.73103116600005,15.2,-6.01080306100001));
#278239=CARTESIAN_POINT('Ctrl Pts',(-8.73103116600005,11.6,-6.01080306100001));
#278240=CARTESIAN_POINT('Ctrl Pts',(-8.73245573500006,15.2,-6.01235067300002));
#278241=CARTESIAN_POINT('Ctrl Pts',(-8.73245573500006,11.6,-6.01235067300002));
#278242=CARTESIAN_POINT('Ctrl Pts',(-8.73388355200006,15.2,-6.01390459800001));
#278243=CARTESIAN_POINT('Ctrl Pts',(-8.73388355200006,11.6,-6.01390459800001));
#278244=CARTESIAN_POINT('Ctrl Pts',(-8.73531460000006,15.2,-6.01546483500002));
#278245=CARTESIAN_POINT('Ctrl Pts',(-8.73531460000006,11.6,-6.01546483500002));
#278246=CARTESIAN_POINT('Ctrl Pts',(-8.73674886200006,15.2,-6.01703137900002));
#278247=CARTESIAN_POINT('Ctrl Pts',(-8.73674886200006,11.6,-6.01703137900002));
#278248=CARTESIAN_POINT('Ctrl Pts',(-8.73818631900006,15.2,-6.01860422700002));
#278249=CARTESIAN_POINT('Ctrl Pts',(-8.73818631900006,11.6,-6.01860422700002));
#278250=CARTESIAN_POINT('Ctrl Pts',(-8.73962695400006,15.2,-6.02018337700001));
#278251=CARTESIAN_POINT('Ctrl Pts',(-8.73962695400006,11.6,-6.02018337700001));
#278252=CARTESIAN_POINT('Ctrl Pts',(-8.74107074900006,15.2,-6.02176882400002));
#278253=CARTESIAN_POINT('Ctrl Pts',(-8.74107074900006,11.6,-6.02176882400002));
#278254=CARTESIAN_POINT('Ctrl Pts',(-8.74251768700006,15.2,-6.02336056500001));
#278255=CARTESIAN_POINT('Ctrl Pts',(-8.74251768700006,11.6,-6.02336056500001));
#278256=CARTESIAN_POINT('Ctrl Pts',(-8.74396774900006,15.2,-6.02495859900002));
#278257=CARTESIAN_POINT('Ctrl Pts',(-8.74396774900006,11.6,-6.02495859900002));
#278258=CARTESIAN_POINT('Ctrl Pts',(-8.74542091900006,15.2,-6.02656292000002));
#278259=CARTESIAN_POINT('Ctrl Pts',(-8.74542091900006,11.6,-6.02656292000002));
#278260=CARTESIAN_POINT('Ctrl Pts',(-8.74687718000006,15.2,-6.02817352700002));
#278261=CARTESIAN_POINT('Ctrl Pts',(-8.74687718000006,11.6,-6.02817352700002));
#278262=CARTESIAN_POINT('Ctrl Pts',(-8.74833651400006,15.2,-6.02979041500002));
#278263=CARTESIAN_POINT('Ctrl Pts',(-8.74833651400006,11.6,-6.02979041500002));
#278264=CARTESIAN_POINT('Ctrl Pts',(-8.74979890300006,15.2,-6.03141358100002));
#278265=CARTESIAN_POINT('Ctrl Pts',(-8.74979890300006,11.6,-6.03141358100002));
#278266=CARTESIAN_POINT('Ctrl Pts',(-8.75126433000006,15.2,-6.03304302300002));
#278267=CARTESIAN_POINT('Ctrl Pts',(-8.75126433000006,11.6,-6.03304302300002));
#278268=CARTESIAN_POINT('Ctrl Pts',(-8.75273277900006,15.2,-6.03467873700002));
#278269=CARTESIAN_POINT('Ctrl Pts',(-8.75273277900006,11.6,-6.03467873700002));
#278270=CARTESIAN_POINT('Ctrl Pts',(-8.75420423300006,15.2,-6.03632072000002));
#278271=CARTESIAN_POINT('Ctrl Pts',(-8.75420423300006,11.6,-6.03632072000002));
#278272=CARTESIAN_POINT('Ctrl Pts',(-8.75567867300006,15.2,-6.03796896800001));
#278273=CARTESIAN_POINT('Ctrl Pts',(-8.75567867300006,11.6,-6.03796896800001));
#278274=CARTESIAN_POINT('Ctrl Pts',(-8.75715608400006,15.2,-6.03962347800002));
#278275=CARTESIAN_POINT('Ctrl Pts',(-8.75715608400006,11.6,-6.03962347800002));
#278276=CARTESIAN_POINT('Ctrl Pts',(-8.75863644800006,15.2,-6.04128424800002));
#278277=CARTESIAN_POINT('Ctrl Pts',(-8.75863644800006,11.6,-6.04128424800002));
#278278=CARTESIAN_POINT('Ctrl Pts',(-8.76011974800005,15.2,-6.04295127200002));
#278279=CARTESIAN_POINT('Ctrl Pts',(-8.76011974800005,11.6,-6.04295127200002));
#278280=CARTESIAN_POINT('Ctrl Pts',(-8.76160596900006,15.2,-6.04462455100002));
#278281=CARTESIAN_POINT('Ctrl Pts',(-8.76160596900006,11.6,-6.04462455100002));
#278282=CARTESIAN_POINT('Ctrl Pts',(-8.76309509200006,15.2,-6.04630407800002));
#278283=CARTESIAN_POINT('Ctrl Pts',(-8.76309509200006,11.6,-6.04630407800002));
#278284=CARTESIAN_POINT('Ctrl Pts',(-8.76458710000006,15.2,-6.04798985100001));
#278285=CARTESIAN_POINT('Ctrl Pts',(-8.76458710000006,11.6,-6.04798985100001));
#278286=CARTESIAN_POINT('Ctrl Pts',(-8.76608197800006,15.2,-6.04968186700001));
#278287=CARTESIAN_POINT('Ctrl Pts',(-8.76608197800006,11.6,-6.04968186700001));
#278288=CARTESIAN_POINT('Ctrl Pts',(-8.76757970900006,15.2,-6.05138012300002));
#278289=CARTESIAN_POINT('Ctrl Pts',(-8.76757970900006,11.6,-6.05138012300002));
#278290=CARTESIAN_POINT('Ctrl Pts',(-8.76908027600006,15.2,-6.05308461500002));
#278291=CARTESIAN_POINT('Ctrl Pts',(-8.76908027600006,11.6,-6.05308461500002));
#278292=CARTESIAN_POINT('Ctrl Pts',(-8.77058366300006,15.2,-6.05479534100001));
#278293=CARTESIAN_POINT('Ctrl Pts',(-8.77058366300006,11.6,-6.05479534100001));
#278294=CARTESIAN_POINT('Ctrl Pts',(-8.77208985300006,15.2,-6.05651229500002));
#278295=CARTESIAN_POINT('Ctrl Pts',(-8.77208985300006,11.6,-6.05651229500002));
#278296=CARTESIAN_POINT('Ctrl Pts',(-8.77359883000006,15.2,-6.05823547700002));
#278297=CARTESIAN_POINT('Ctrl Pts',(-8.77359883000006,11.6,-6.05823547700002));
#278298=CARTESIAN_POINT('Ctrl Pts',(-8.77511057700006,15.2,-6.05996488200002));
#278299=CARTESIAN_POINT('Ctrl Pts',(-8.77511057700006,11.6,-6.05996488200002));
#278300=CARTESIAN_POINT('Ctrl Pts',(-8.77662507900006,15.2,-6.06170050700002));
#278301=CARTESIAN_POINT('Ctrl Pts',(-8.77662507900006,11.6,-6.06170050700002));
#278302=CARTESIAN_POINT('Ctrl Pts',(-8.77814231800006,15.2,-6.06344234800002));
#278303=CARTESIAN_POINT('Ctrl Pts',(-8.77814231800006,11.6,-6.06344234800002));
#278304=CARTESIAN_POINT('Ctrl Pts',(-8.77966227900006,15.2,-6.06519040400002));
#278305=CARTESIAN_POINT('Ctrl Pts',(-8.77966227900006,11.6,-6.06519040400002));
#278306=CARTESIAN_POINT('Ctrl Pts',(-8.78118494600006,15.2,-6.06694467000001));
#278307=CARTESIAN_POINT('Ctrl Pts',(-8.78118494600006,11.6,-6.06694467000001));
#278308=CARTESIAN_POINT('Ctrl Pts',(-8.78271030200005,15.2,-6.06870514200001));
#278309=CARTESIAN_POINT('Ctrl Pts',(-8.78271030200005,11.6,-6.06870514200001));
#278310=CARTESIAN_POINT('Ctrl Pts',(-8.78423833200005,15.2,-6.07047181900001));
#278311=CARTESIAN_POINT('Ctrl Pts',(-8.78423833200005,11.6,-6.07047181900001));
#278312=CARTESIAN_POINT('Ctrl Pts',(-8.78576901900006,15.2,-6.07224469600002));
#278313=CARTESIAN_POINT('Ctrl Pts',(-8.78576901900006,11.6,-6.07224469600002));
#278314=CARTESIAN_POINT('Ctrl Pts',(-8.78730234600006,15.2,-6.07402377000002));
#278315=CARTESIAN_POINT('Ctrl Pts',(-8.78730234600006,11.6,-6.07402377000002));
#278316=CARTESIAN_POINT('Ctrl Pts',(-8.78883830100006,15.2,-6.07580903900002));
#278317=CARTESIAN_POINT('Ctrl Pts',(-8.78883830100006,11.6,-6.07580903900002));
#278318=CARTESIAN_POINT('Ctrl Pts',(-8.79037686400006,15.2,-6.07760049900002));
#278319=CARTESIAN_POINT('Ctrl Pts',(-8.79037686400006,11.6,-6.07760049900002));
#278320=CARTESIAN_POINT('Ctrl Pts',(-8.79191802100006,15.2,-6.07939814500002));
#278321=CARTESIAN_POINT('Ctrl Pts',(-8.79191802100006,11.6,-6.07939814500002));
#278322=CARTESIAN_POINT('Ctrl Pts',(-8.79346175700006,15.2,-6.08120197500002));
#278323=CARTESIAN_POINT('Ctrl Pts',(-8.79346175700006,11.6,-6.08120197500002));
#278324=CARTESIAN_POINT('Ctrl Pts',(-8.79500805500006,15.2,-6.08301198800002));
#278325=CARTESIAN_POINT('Ctrl Pts',(-8.79500805500006,11.6,-6.08301198800002));
#278326=CARTESIAN_POINT('Ctrl Pts',(-8.79655690000006,15.2,-6.08482817600001));
#278327=CARTESIAN_POINT('Ctrl Pts',(-8.79655690000006,11.6,-6.08482817600001));
#278328=CARTESIAN_POINT('Ctrl Pts',(-8.79810827500006,15.2,-6.08665054000002));
#278329=CARTESIAN_POINT('Ctrl Pts',(-8.79810827500006,11.6,-6.08665054000002));
#278330=CARTESIAN_POINT('Ctrl Pts',(-8.79966216600006,15.2,-6.08847907500002));
#278331=CARTESIAN_POINT('Ctrl Pts',(-8.79966216600006,11.6,-6.08847907500002));
#278332=CARTESIAN_POINT('Ctrl Pts',(-8.80121855800006,15.2,-6.09031377800001));
#278333=CARTESIAN_POINT('Ctrl Pts',(-8.80121855800006,11.6,-6.09031377800001));
#278334=CARTESIAN_POINT('Ctrl Pts',(-8.80277743400006,15.2,-6.09215464600001));
#278335=CARTESIAN_POINT('Ctrl Pts',(-8.80277743400006,11.6,-6.09215464600001));
#278336=CARTESIAN_POINT('Ctrl Pts',(-8.80433877800006,15.2,-6.09400167400001));
#278337=CARTESIAN_POINT('Ctrl Pts',(-8.80433877800006,11.6,-6.09400167400001));
#278338=CARTESIAN_POINT('Ctrl Pts',(-8.80590257700005,15.2,-6.09585486100002));
#278339=CARTESIAN_POINT('Ctrl Pts',(-8.80590257700005,11.6,-6.09585486100002));
#278340=CARTESIAN_POINT('Ctrl Pts',(-8.80746881400006,15.2,-6.09771420100002));
#278341=CARTESIAN_POINT('Ctrl Pts',(-8.80746881400006,11.6,-6.09771420100002));
#278342=CARTESIAN_POINT('Ctrl Pts',(-8.80903747400006,15.2,-6.09957969500002));
#278343=CARTESIAN_POINT('Ctrl Pts',(-8.80903747400006,11.6,-6.09957969500002));
#278344=CARTESIAN_POINT('Ctrl Pts',(-8.81060854200006,15.2,-6.10145133500002));
#278345=CARTESIAN_POINT('Ctrl Pts',(-8.81060854200006,11.6,-6.10145133500002));
#278346=CARTESIAN_POINT('Ctrl Pts',(-8.81218200200006,15.2,-6.10332912100001));
#278347=CARTESIAN_POINT('Ctrl Pts',(-8.81218200200006,11.6,-6.10332912100001));
#278348=CARTESIAN_POINT('Ctrl Pts',(-8.81375784100005,15.2,-6.10521304800002));
#278349=CARTESIAN_POINT('Ctrl Pts',(-8.81375784100005,11.6,-6.10521304800002));
#278350=CARTESIAN_POINT('Ctrl Pts',(-8.81533604000006,15.2,-6.10710311400001));
#278351=CARTESIAN_POINT('Ctrl Pts',(-8.81533604000006,11.6,-6.10710311400001));
#278352=CARTESIAN_POINT('Ctrl Pts',(-8.81691658800005,15.2,-6.10899931400001));
#278353=CARTESIAN_POINT('Ctrl Pts',(-8.81691658800005,11.6,-6.10899931400001));
#278354=CARTESIAN_POINT('Ctrl Pts',(-8.81849946900006,15.2,-6.11090164700002));
#278355=CARTESIAN_POINT('Ctrl Pts',(-8.81849946900006,11.6,-6.11090164700002));
#278356=CARTESIAN_POINT('Ctrl Pts',(-8.82008466600006,15.2,-6.11281010700001));
#278357=CARTESIAN_POINT('Ctrl Pts',(-8.82008466600006,11.6,-6.11281010700001));
#278358=CARTESIAN_POINT('Ctrl Pts',(-8.82167216500006,15.2,-6.11472469300002));
#278359=CARTESIAN_POINT('Ctrl Pts',(-8.82167216500006,11.6,-6.11472469300002));
#278360=CARTESIAN_POINT('Ctrl Pts',(-8.82326195200006,15.2,-6.11664540100002));
#278361=CARTESIAN_POINT('Ctrl Pts',(-8.82326195200006,11.6,-6.11664540100002));
#278362=CARTESIAN_POINT('Ctrl Pts',(-8.82485401100006,15.2,-6.11857222700002));
#278363=CARTESIAN_POINT('Ctrl Pts',(-8.82485401100006,11.6,-6.11857222700002));
#278364=CARTESIAN_POINT('Ctrl Pts',(-8.82644832900005,15.2,-6.12050516800001));
#278365=CARTESIAN_POINT('Ctrl Pts',(-8.82644832900005,11.6,-6.12050516800001));
#278366=CARTESIAN_POINT('Ctrl Pts',(-8.82804488900006,15.2,-6.12244422100002));
#278367=CARTESIAN_POINT('Ctrl Pts',(-8.82804488900006,11.6,-6.12244422100002));
#278368=CARTESIAN_POINT('Ctrl Pts',(-8.82964367800006,15.2,-6.12438938300001));
#278369=CARTESIAN_POINT('Ctrl Pts',(-8.82964367800006,11.6,-6.12438938300001));
#278370=CARTESIAN_POINT('Ctrl Pts',(-8.83124468100006,15.2,-6.12634065100002));
#278371=CARTESIAN_POINT('Ctrl Pts',(-8.83124468100006,11.6,-6.12634065100002));
#278372=CARTESIAN_POINT('Ctrl Pts',(-8.83284788200006,15.2,-6.12829802000002));
#278373=CARTESIAN_POINT('Ctrl Pts',(-8.83284788200006,11.6,-6.12829802000002));
#278374=CARTESIAN_POINT('Ctrl Pts',(-8.83445326800006,15.2,-6.13026148800002));
#278375=CARTESIAN_POINT('Ctrl Pts',(-8.83445326800006,11.6,-6.13026148800002));
#278376=CARTESIAN_POINT('Ctrl Pts',(-8.83606082300006,15.2,-6.13223105100002));
#278377=CARTESIAN_POINT('Ctrl Pts',(-8.83606082300006,11.6,-6.13223105100002));
#278378=CARTESIAN_POINT('Ctrl Pts',(-8.83767053400006,15.2,-6.13420670600001));
#278379=CARTESIAN_POINT('Ctrl Pts',(-8.83767053400006,11.6,-6.13420670600001));
#278380=CARTESIAN_POINT('Ctrl Pts',(-8.83928238600006,15.2,-6.13618845100002));
#278381=CARTESIAN_POINT('Ctrl Pts',(-8.83928238600006,11.6,-6.13618845100002));
#278382=CARTESIAN_POINT('Ctrl Pts',(-8.84089636400006,15.2,-6.13817628100002));
#278383=CARTESIAN_POINT('Ctrl Pts',(-8.84089636400006,11.6,-6.13817628100002));
#278384=CARTESIAN_POINT('Ctrl Pts',(-8.84251245500005,15.2,-6.14017019300002));
#278385=CARTESIAN_POINT('Ctrl Pts',(-8.84251245500005,11.6,-6.14017019300002));
#278386=CARTESIAN_POINT('Ctrl Pts',(-8.84413064300006,15.2,-6.14217018300002));
#278387=CARTESIAN_POINT('Ctrl Pts',(-8.84413064300006,11.6,-6.14217018300002));
#278388=CARTESIAN_POINT('Ctrl Pts',(-8.84575091500006,15.2,-6.14417625000002));
#278389=CARTESIAN_POINT('Ctrl Pts',(-8.84575091500006,11.6,-6.14417625000002));
#278390=CARTESIAN_POINT('Ctrl Pts',(-8.84737325600006,15.2,-6.14618838800002));
#278391=CARTESIAN_POINT('Ctrl Pts',(-8.84737325600006,11.6,-6.14618838800002));
#278392=CARTESIAN_POINT('Ctrl Pts',(-8.84899765200006,15.2,-6.14820659600002));
#278393=CARTESIAN_POINT('Ctrl Pts',(-8.84899765200006,11.6,-6.14820659600002));
#278394=CARTESIAN_POINT('Ctrl Pts',(-8.85062408800006,15.2,-6.15023087000001));
#278395=CARTESIAN_POINT('Ctrl Pts',(-8.85062408800006,11.6,-6.15023087000001));
#278396=CARTESIAN_POINT('Ctrl Pts',(-8.85225255100006,15.2,-6.15226120500001));
#278397=CARTESIAN_POINT('Ctrl Pts',(-8.85225255100006,11.6,-6.15226120500001));
#278398=CARTESIAN_POINT('Ctrl Pts',(-8.85388302600006,15.2,-6.15429759900002));
#278399=CARTESIAN_POINT('Ctrl Pts',(-8.85388302600006,11.6,-6.15429759900002));
#278400=CARTESIAN_POINT('Ctrl Pts',(-8.85551550100006,15.2,-6.15634004900001));
#278401=CARTESIAN_POINT('Ctrl Pts',(-8.85551550100006,11.6,-6.15634004900001));
#278402=CARTESIAN_POINT('Ctrl Pts',(-8.85714995900006,15.2,-6.15838855200002));
#278403=CARTESIAN_POINT('Ctrl Pts',(-8.85714995900006,11.6,-6.15838855200002));
#278404=CARTESIAN_POINT('Ctrl Pts',(-8.85878638800006,15.2,-6.16044310300002));
#278405=CARTESIAN_POINT('Ctrl Pts',(-8.85878638800006,11.6,-6.16044310300002));
#278406=CARTESIAN_POINT('Ctrl Pts',(-8.86042477400006,15.2,-6.16250370000002));
#278407=CARTESIAN_POINT('Ctrl Pts',(-8.86042477400006,11.6,-6.16250370000002));
#278408=CARTESIAN_POINT('Ctrl Pts',(-8.86206510200006,15.2,-6.16457033900002));
#278409=CARTESIAN_POINT('Ctrl Pts',(-8.86206510200006,11.6,-6.16457033900002));
#278410=CARTESIAN_POINT('Ctrl Pts',(-8.86370735900006,15.2,-6.16664301800002));
#278411=CARTESIAN_POINT('Ctrl Pts',(-8.86370735900006,11.6,-6.16664301800002));
#278412=CARTESIAN_POINT('Ctrl Pts',(-8.86535153100006,15.2,-6.16872173200001));
#278413=CARTESIAN_POINT('Ctrl Pts',(-8.86535153100006,11.6,-6.16872173200001));
#278414=CARTESIAN_POINT('Ctrl Pts',(-8.86699760400005,15.2,-6.17080647800002));
#278415=CARTESIAN_POINT('Ctrl Pts',(-8.86699760400005,11.6,-6.17080647800002));
#278416=CARTESIAN_POINT('Ctrl Pts',(-8.86864556400005,15.2,-6.17289725400001));
#278417=CARTESIAN_POINT('Ctrl Pts',(-8.86864556400005,11.6,-6.17289725400001));
#278418=CARTESIAN_POINT('Ctrl Pts',(-8.87029539800006,15.2,-6.17499405500002));
#278419=CARTESIAN_POINT('Ctrl Pts',(-8.87029539800006,11.6,-6.17499405500002));
#278420=CARTESIAN_POINT('Ctrl Pts',(-8.87194709200006,15.2,-6.17709687800001));
#278421=CARTESIAN_POINT('Ctrl Pts',(-8.87194709200006,11.6,-6.17709687800001));
#278422=CARTESIAN_POINT('Ctrl Pts',(-8.87360063200006,15.2,-6.17920572000001));
#278423=CARTESIAN_POINT('Ctrl Pts',(-8.87360063200006,11.6,-6.17920572000001));
#278424=CARTESIAN_POINT('Ctrl Pts',(-8.87525600500006,15.2,-6.18132057900001));
#278425=CARTESIAN_POINT('Ctrl Pts',(-8.87525600500006,11.6,-6.18132057900001));
#278426=CARTESIAN_POINT('Ctrl Pts',(-8.87691319700006,15.2,-6.18344144900002));
#278427=CARTESIAN_POINT('Ctrl Pts',(-8.87691319700006,11.6,-6.18344144900002));
#278428=CARTESIAN_POINT('Ctrl Pts',(-8.87857219500006,15.2,-6.18556832800002));
#278429=CARTESIAN_POINT('Ctrl Pts',(-8.87857219500006,11.6,-6.18556832800002));
#278430=CARTESIAN_POINT('Ctrl Pts',(-8.88023298500006,15.2,-6.18770121300001));
#278431=CARTESIAN_POINT('Ctrl Pts',(-8.88023298500006,11.6,-6.18770121300001));
#278432=CARTESIAN_POINT('Ctrl Pts',(-8.88189555400006,15.2,-6.18984010100001));
#278433=CARTESIAN_POINT('Ctrl Pts',(-8.88189555400006,11.6,-6.18984010100001));
#278434=CARTESIAN_POINT('Ctrl Pts',(-8.88355988700006,15.2,-6.19198498700002));
#278435=CARTESIAN_POINT('Ctrl Pts',(-8.88355988700006,11.6,-6.19198498700002));
#278436=CARTESIAN_POINT('Ctrl Pts',(-8.88522597300006,15.2,-6.19413586900002));
#278437=CARTESIAN_POINT('Ctrl Pts',(-8.88522597300006,11.6,-6.19413586900002));
#278438=CARTESIAN_POINT('Ctrl Pts',(-8.88689379800006,15.2,-6.19629274300002));
#278439=CARTESIAN_POINT('Ctrl Pts',(-8.88689379800006,11.6,-6.19629274300002));
#278440=CARTESIAN_POINT('Ctrl Pts',(-8.88856334800005,15.2,-6.19845560600002));
#278441=CARTESIAN_POINT('Ctrl Pts',(-8.88856334800005,11.6,-6.19845560600002));
#278442=CARTESIAN_POINT('Ctrl Pts',(-8.89023460900006,15.2,-6.20062445500002));
#278443=CARTESIAN_POINT('Ctrl Pts',(-8.89023460900006,11.6,-6.20062445500002));
#278444=CARTESIAN_POINT('Ctrl Pts',(-8.89190757000006,15.2,-6.20279928600001));
#278445=CARTESIAN_POINT('Ctrl Pts',(-8.89190757000006,11.6,-6.20279928600001));
#278446=CARTESIAN_POINT('Ctrl Pts',(-8.89358221600006,15.2,-6.20498009500002));
#278447=CARTESIAN_POINT('Ctrl Pts',(-8.89358221600006,11.6,-6.20498009500002));
#278448=CARTESIAN_POINT('Ctrl Pts',(-8.89525853400006,15.2,-6.20716688000002));
#278449=CARTESIAN_POINT('Ctrl Pts',(-8.89525853400006,11.6,-6.20716688000002));
#278450=CARTESIAN_POINT('Ctrl Pts',(-8.89693651200006,15.2,-6.20935963800001));
#278451=CARTESIAN_POINT('Ctrl Pts',(-8.89693651200006,11.6,-6.20935963800001));
#278452=CARTESIAN_POINT('Ctrl Pts',(-8.89861613600005,15.2,-6.21155836400002));
#278453=CARTESIAN_POINT('Ctrl Pts',(-8.89861613600005,11.6,-6.21155836400002));
#278454=CARTESIAN_POINT('Ctrl Pts',(-8.90029739200006,15.2,-6.21376305500001));
#278455=CARTESIAN_POINT('Ctrl Pts',(-8.90029739200006,11.6,-6.21376305500001));
#278456=CARTESIAN_POINT('Ctrl Pts',(-8.90198026900006,15.2,-6.21597370900002));
#278457=CARTESIAN_POINT('Ctrl Pts',(-8.90198026900006,11.6,-6.21597370900002));
#278458=CARTESIAN_POINT('Ctrl Pts',(-8.90366475400005,15.2,-6.21819032100002));
#278459=CARTESIAN_POINT('Ctrl Pts',(-8.90366475400005,11.6,-6.21819032100002));
#278460=CARTESIAN_POINT('Ctrl Pts',(-8.90535083200006,15.2,-6.22041288900002));
#278461=CARTESIAN_POINT('Ctrl Pts',(-8.90535083200006,11.6,-6.22041288900002));
#278462=CARTESIAN_POINT('Ctrl Pts',(-8.90703849000005,15.2,-6.22264140900001));
#278463=CARTESIAN_POINT('Ctrl Pts',(-8.90703849000005,11.6,-6.22264140900001));
#278464=CARTESIAN_POINT('Ctrl Pts',(-8.90872771800005,15.2,-6.22487587700002));
#278465=CARTESIAN_POINT('Ctrl Pts',(-8.90872771800005,11.6,-6.22487587700002));
#278466=CARTESIAN_POINT('Ctrl Pts',(-8.91041850200006,15.2,-6.22711629000002));
#278467=CARTESIAN_POINT('Ctrl Pts',(-8.91041850200006,11.6,-6.22711629000002));
#278468=CARTESIAN_POINT('Ctrl Pts',(-8.91211082800006,15.2,-6.22936264500002));
#278469=CARTESIAN_POINT('Ctrl Pts',(-8.91211082800006,11.6,-6.22936264500002));
#278470=CARTESIAN_POINT('Ctrl Pts',(-8.91380468400006,15.2,-6.23161493900002));
#278471=CARTESIAN_POINT('Ctrl Pts',(-8.91380468400006,11.6,-6.23161493900002));
#278472=CARTESIAN_POINT('Ctrl Pts',(-8.91550005600006,15.2,-6.23387316900001));
#278473=CARTESIAN_POINT('Ctrl Pts',(-8.91550005600006,11.6,-6.23387316900001));
#278474=CARTESIAN_POINT('Ctrl Pts',(-8.91719693400006,15.2,-6.23613733000001));
#278475=CARTESIAN_POINT('Ctrl Pts',(-8.91719693400006,11.6,-6.23613733000001));
#278476=CARTESIAN_POINT('Ctrl Pts',(-8.91889530300006,15.2,-6.23840741900001));
#278477=CARTESIAN_POINT('Ctrl Pts',(-8.91889530300006,11.6,-6.23840741900001));
#278478=CARTESIAN_POINT('Ctrl Pts',(-8.92059515000006,15.2,-6.24068343300002));
#278479=CARTESIAN_POINT('Ctrl Pts',(-8.92059515000006,11.6,-6.24068343300002));
#278480=CARTESIAN_POINT('Ctrl Pts',(-8.92229646500006,15.2,-6.24296536900002));
#278481=CARTESIAN_POINT('Ctrl Pts',(-8.92229646500006,11.6,-6.24296536900002));
#278482=CARTESIAN_POINT('Ctrl Pts',(-8.92399923400006,15.2,-6.24525322300002));
#278483=CARTESIAN_POINT('Ctrl Pts',(-8.92399923400006,11.6,-6.24525322300002));
#278484=CARTESIAN_POINT('Ctrl Pts',(-8.92570344300006,15.2,-6.24754699200002));
#278485=CARTESIAN_POINT('Ctrl Pts',(-8.92570344300006,11.6,-6.24754699200002));
#278486=CARTESIAN_POINT('Ctrl Pts',(-8.92740908100006,15.2,-6.24984667200001));
#278487=CARTESIAN_POINT('Ctrl Pts',(-8.92740908100006,11.6,-6.24984667200001));
#278488=CARTESIAN_POINT('Ctrl Pts',(-8.92911613500005,15.2,-6.25215226100002));
#278489=CARTESIAN_POINT('Ctrl Pts',(-8.92911613500005,11.6,-6.25215226100002));
#278490=CARTESIAN_POINT('Ctrl Pts',(-8.93082459500006,15.2,-6.25446375500001));
#278491=CARTESIAN_POINT('Ctrl Pts',(-8.93082459500006,11.6,-6.25446375500001));
#278492=CARTESIAN_POINT('Ctrl Pts',(-8.93253444400005,15.2,-6.25678115000002));
#278493=CARTESIAN_POINT('Ctrl Pts',(-8.93253444400005,11.6,-6.25678115000002));
#278494=CARTESIAN_POINT('Ctrl Pts',(-8.93424567300006,15.2,-6.25910444200001));
#278495=CARTESIAN_POINT('Ctrl Pts',(-8.93424567300006,11.6,-6.25910444200001));
#278496=CARTESIAN_POINT('Ctrl Pts',(-8.93595826900006,15.2,-6.26143363000002));
#278497=CARTESIAN_POINT('Ctrl Pts',(-8.93595826900006,11.6,-6.26143363000002));
#278498=CARTESIAN_POINT('Ctrl Pts',(-8.93767221800006,15.2,-6.26376870800001));
#278499=CARTESIAN_POINT('Ctrl Pts',(-8.93767221800006,11.6,-6.26376870800001));
#278500=CARTESIAN_POINT('Ctrl Pts',(-8.93938751100006,15.2,-6.26610967500002));
#278501=CARTESIAN_POINT('Ctrl Pts',(-8.93938751100006,11.6,-6.26610967500002));
#278502=CARTESIAN_POINT('Ctrl Pts',(-8.94110413200006,15.2,-6.26845652500001));
#278503=CARTESIAN_POINT('Ctrl Pts',(-8.94110413200006,11.6,-6.26845652500001));
#278504=CARTESIAN_POINT('Ctrl Pts',(-8.94282207100006,15.2,-6.27080925700002));
#278505=CARTESIAN_POINT('Ctrl Pts',(-8.94282207100006,11.6,-6.27080925700002));
#278506=CARTESIAN_POINT('Ctrl Pts',(-8.94454131600006,15.2,-6.27316786700002));
#278507=CARTESIAN_POINT('Ctrl Pts',(-8.94454131600006,11.6,-6.27316786700002));
#278508=CARTESIAN_POINT('Ctrl Pts',(-8.94626185300006,15.2,-6.27553235000001));
#278509=CARTESIAN_POINT('Ctrl Pts',(-8.94626185300006,11.6,-6.27553235000001));
#278510=CARTESIAN_POINT('Ctrl Pts',(-8.94798367300006,15.2,-6.27790270500002));
#278511=CARTESIAN_POINT('Ctrl Pts',(-8.94798367300006,11.6,-6.27790270500002));
#278512=CARTESIAN_POINT('Ctrl Pts',(-8.94970676000005,15.2,-6.28027892700001));
#278513=CARTESIAN_POINT('Ctrl Pts',(-8.94970676000005,11.6,-6.28027892700001));
#278514=CARTESIAN_POINT('Ctrl Pts',(-8.95143110500005,15.2,-6.28266101300002));
#278515=CARTESIAN_POINT('Ctrl Pts',(-8.95143110500005,11.6,-6.28266101300002));
#278516=CARTESIAN_POINT('Ctrl Pts',(-8.95315669400006,15.2,-6.28504896000001));
#278517=CARTESIAN_POINT('Ctrl Pts',(-8.95315669400006,11.6,-6.28504896000001));
#278518=CARTESIAN_POINT('Ctrl Pts',(-8.95488351600006,15.2,-6.28744276400001));
#278519=CARTESIAN_POINT('Ctrl Pts',(-8.95488351600006,11.6,-6.28744276400001));
#278520=CARTESIAN_POINT('Ctrl Pts',(-8.95661155800006,15.2,-6.28984242200002));
#278521=CARTESIAN_POINT('Ctrl Pts',(-8.95661155800006,11.6,-6.28984242200002));
#278522=CARTESIAN_POINT('Ctrl Pts',(-8.95834081000006,15.2,-6.29224793100001));
#278523=CARTESIAN_POINT('Ctrl Pts',(-8.95834081000006,11.6,-6.29224793100001));
#278524=CARTESIAN_POINT('Ctrl Pts',(-8.96007125900006,15.2,-6.29465928600002));
#278525=CARTESIAN_POINT('Ctrl Pts',(-8.96007125900006,11.6,-6.29465928600002));
#278526=CARTESIAN_POINT('Ctrl Pts',(-8.96180289200006,15.2,-6.29707648500001));
#278527=CARTESIAN_POINT('Ctrl Pts',(-8.96180289200006,11.6,-6.29707648500001));
#278528=CARTESIAN_POINT('Ctrl Pts',(-8.96353569900005,15.2,-6.29949952400001));
#278529=CARTESIAN_POINT('Ctrl Pts',(-8.96353569900005,11.6,-6.29949952400001));
#278530=CARTESIAN_POINT('Ctrl Pts',(-8.96526966700005,15.2,-6.30192840000002));
#278531=CARTESIAN_POINT('Ctrl Pts',(-8.96526966700005,11.6,-6.30192840000002));
#278532=CARTESIAN_POINT('Ctrl Pts',(-8.96700478400006,15.2,-6.30436311000001));
#278533=CARTESIAN_POINT('Ctrl Pts',(-8.96700478400006,11.6,-6.30436311000001));
#278534=CARTESIAN_POINT('Ctrl Pts',(-8.96874103900006,15.2,-6.30680364900002));
#278535=CARTESIAN_POINT('Ctrl Pts',(-8.96874103900006,11.6,-6.30680364900002));
#278536=CARTESIAN_POINT('Ctrl Pts',(-8.97047842000006,15.2,-6.30925001600002));
#278537=CARTESIAN_POINT('Ctrl Pts',(-8.97047842000006,11.6,-6.30925001600002));
#278538=CARTESIAN_POINT('Ctrl Pts',(-8.97221691500006,15.2,-6.31170220500002));
#278539=CARTESIAN_POINT('Ctrl Pts',(-8.97221691500006,11.6,-6.31170220500002));
#278540=CARTESIAN_POINT('Ctrl Pts',(-8.97395651200006,15.2,-6.31416021300002));
#278541=CARTESIAN_POINT('Ctrl Pts',(-8.97395651200006,11.6,-6.31416021300002));
#278542=CARTESIAN_POINT('Ctrl Pts',(-8.97569720200006,15.2,-6.31662403900001));
#278543=CARTESIAN_POINT('Ctrl Pts',(-8.97569720200006,11.6,-6.31662403900001));
#278544=CARTESIAN_POINT('Ctrl Pts',(-8.97743896900005,15.2,-6.31909367700001));
#278545=CARTESIAN_POINT('Ctrl Pts',(-8.97743896900005,11.6,-6.31909367700001));
#278546=CARTESIAN_POINT('Ctrl Pts',(-8.97918180500006,15.2,-6.32156912600002));
#278547=CARTESIAN_POINT('Ctrl Pts',(-8.97918180500006,11.6,-6.32156912600002));
#278548=CARTESIAN_POINT('Ctrl Pts',(-8.98092569500006,15.2,-6.32405038000002));
#278549=CARTESIAN_POINT('Ctrl Pts',(-8.98092569500006,11.6,-6.32405038000002));
#278550=CARTESIAN_POINT('Ctrl Pts',(-8.98267063200005,15.2,-6.32653743600001));
#278551=CARTESIAN_POINT('Ctrl Pts',(-8.98267063200005,11.6,-6.32653743600001));
#278552=CARTESIAN_POINT('Ctrl Pts',(-8.98441660000006,15.2,-6.32903029200002));
#278553=CARTESIAN_POINT('Ctrl Pts',(-8.98441660000006,11.6,-6.32903029200002));
#278554=CARTESIAN_POINT('Ctrl Pts',(-8.98616359200006,15.2,-6.33152894400002));
#278555=CARTESIAN_POINT('Ctrl Pts',(-8.98616359200006,11.6,-6.33152894400002));
#278556=CARTESIAN_POINT('Ctrl Pts',(-8.98791159200006,15.2,-6.33403338800001));
#278557=CARTESIAN_POINT('Ctrl Pts',(-8.98791159200006,11.6,-6.33403338800001));
#278558=CARTESIAN_POINT('Ctrl Pts',(-8.98966059100006,15.2,-6.33654362100001));
#278559=CARTESIAN_POINT('Ctrl Pts',(-8.98966059100006,11.6,-6.33654362100001));
#278560=CARTESIAN_POINT('Ctrl Pts',(-8.99141057700006,15.2,-6.33905964000002));
#278561=CARTESIAN_POINT('Ctrl Pts',(-8.99141057700006,11.6,-6.33905964000002));
#278562=CARTESIAN_POINT('Ctrl Pts',(-8.99316153900006,15.2,-6.34158144100001));
#278563=CARTESIAN_POINT('Ctrl Pts',(-8.99316153900006,11.6,-6.34158144100001));
#278564=CARTESIAN_POINT('Ctrl Pts',(-8.99491346500006,15.2,-6.34410902000001));
#278565=CARTESIAN_POINT('Ctrl Pts',(-8.99491346500006,11.6,-6.34410902000001));
#278566=CARTESIAN_POINT('Ctrl Pts',(-8.99666634400005,15.2,-6.34664237500001));
#278567=CARTESIAN_POINT('Ctrl Pts',(-8.99666634400005,11.6,-6.34664237500001));
#278568=CARTESIAN_POINT('Ctrl Pts',(-8.99842016600006,15.2,-6.34918150200001));
#278569=CARTESIAN_POINT('Ctrl Pts',(-8.99842016600006,11.6,-6.34918150200001));
#278570=CARTESIAN_POINT('Ctrl Pts',(-9.00017491800006,15.2,-6.35172639700002));
#278571=CARTESIAN_POINT('Ctrl Pts',(-9.00017491800006,11.6,-6.35172639700002));
#278572=CARTESIAN_POINT('Ctrl Pts',(-9.00193058900006,15.2,-6.35427705700002));
#278573=CARTESIAN_POINT('Ctrl Pts',(-9.00193058900006,11.6,-6.35427705700002));
#278574=CARTESIAN_POINT('Ctrl Pts',(-9.00368716800006,15.2,-6.35683347800001));
#278575=CARTESIAN_POINT('Ctrl Pts',(-9.00368716800006,11.6,-6.35683347800001));
#278576=CARTESIAN_POINT('Ctrl Pts',(-9.00544464500006,15.2,-6.35939565800002));
#278577=CARTESIAN_POINT('Ctrl Pts',(-9.00544464500006,11.6,-6.35939565800002));
#278578=CARTESIAN_POINT('Ctrl Pts',(-9.00720300700005,15.2,-6.36196359300002));
#278579=CARTESIAN_POINT('Ctrl Pts',(-9.00720300700005,11.6,-6.36196359300002));
#278580=CARTESIAN_POINT('Ctrl Pts',(-9.00896224300006,15.2,-6.36453727700002));
#278581=CARTESIAN_POINT('Ctrl Pts',(-9.00896224300006,11.6,-6.36453727700002));
#278582=CARTESIAN_POINT('Ctrl Pts',(-9.01072234200005,15.2,-6.36711671100001));
#278583=CARTESIAN_POINT('Ctrl Pts',(-9.01072234200005,11.6,-6.36711671100001));
#278584=CARTESIAN_POINT('Ctrl Pts',(-9.01248329500006,15.2,-6.36970188800002));
#278585=CARTESIAN_POINT('Ctrl Pts',(-9.01248329500006,11.6,-6.36970188800002));
#278586=CARTESIAN_POINT('Ctrl Pts',(-9.01424508900006,15.2,-6.37229280700002));
#278587=CARTESIAN_POINT('Ctrl Pts',(-9.01424508900006,11.6,-6.37229280700002));
#278588=CARTESIAN_POINT('Ctrl Pts',(-9.01600771300006,15.2,-6.37488946300002));
#278589=CARTESIAN_POINT('Ctrl Pts',(-9.01600771300006,11.6,-6.37488946300002));
#278590=CARTESIAN_POINT('Ctrl Pts',(-9.01777115600006,15.2,-6.37749185300001));
#278591=CARTESIAN_POINT('Ctrl Pts',(-9.01777115600006,11.6,-6.37749185300001));
#278592=CARTESIAN_POINT('Ctrl Pts',(-9.01953540800006,15.2,-6.38009997300002));
#278593=CARTESIAN_POINT('Ctrl Pts',(-9.01953540800006,11.6,-6.38009997300002));
#278594=CARTESIAN_POINT('Ctrl Pts',(-9.02130045700006,15.2,-6.38271382100001));
#278595=CARTESIAN_POINT('Ctrl Pts',(-9.02130045700006,11.6,-6.38271382100001));
#278596=CARTESIAN_POINT('Ctrl Pts',(-9.02306629300006,15.2,-6.38533339200002));
#278597=CARTESIAN_POINT('Ctrl Pts',(-9.02306629300006,11.6,-6.38533339200002));
#278598=CARTESIAN_POINT('Ctrl Pts',(-9.02483290400006,15.2,-6.38795868400001));
#278599=CARTESIAN_POINT('Ctrl Pts',(-9.02483290400006,11.6,-6.38795868400001));
#278600=CARTESIAN_POINT('Ctrl Pts',(-9.02660028000006,15.2,-6.39058969200001));
#278601=CARTESIAN_POINT('Ctrl Pts',(-9.02660028000006,11.6,-6.39058969200001));
#278602=CARTESIAN_POINT('Ctrl Pts',(-9.02836840900006,15.2,-6.39322641400002));
#278603=CARTESIAN_POINT('Ctrl Pts',(-9.02836840900006,11.6,-6.39322641400002));
#278604=CARTESIAN_POINT('Ctrl Pts',(-9.03013728200006,15.2,-6.39586884500002));
#278605=CARTESIAN_POINT('Ctrl Pts',(-9.03013728200006,11.6,-6.39586884500002));
#278606=CARTESIAN_POINT('Ctrl Pts',(-9.03190688600005,15.2,-6.39851698200002));
#278607=CARTESIAN_POINT('Ctrl Pts',(-9.03190688600005,11.6,-6.39851698200002));
#278608=CARTESIAN_POINT('Ctrl Pts',(-9.03367721300006,15.2,-6.40117082400002));
#278609=CARTESIAN_POINT('Ctrl Pts',(-9.03367721300006,11.6,-6.40117082400002));
#278610=CARTESIAN_POINT('Ctrl Pts',(-9.03544825000006,15.2,-6.40383036400002));
#278611=CARTESIAN_POINT('Ctrl Pts',(-9.03544825000006,11.6,-6.40383036400002));
#278612=CARTESIAN_POINT('Ctrl Pts',(-9.03721998600006,15.2,-6.40649560000002));
#278613=CARTESIAN_POINT('Ctrl Pts',(-9.03721998600006,11.6,-6.40649560000002));
#278614=CARTESIAN_POINT('Ctrl Pts',(-9.03899241400006,15.2,-6.40916652900002));
#278615=CARTESIAN_POINT('Ctrl Pts',(-9.03899241400006,11.6,-6.40916652900002));
#278616=CARTESIAN_POINT('Ctrl Pts',(-9.04076551800006,15.2,-6.41184314700002));
#278617=CARTESIAN_POINT('Ctrl Pts',(-9.04076551800006,11.6,-6.41184314700002));
#278618=CARTESIAN_POINT('Ctrl Pts',(-9.04253929100006,15.2,-6.41452545100002));
#278619=CARTESIAN_POINT('Ctrl Pts',(-9.04253929100006,11.6,-6.41452545100002));
#278620=CARTESIAN_POINT('Ctrl Pts',(-9.04431372100006,15.2,-6.41721343600001));
#278621=CARTESIAN_POINT('Ctrl Pts',(-9.04431372100006,11.6,-6.41721343600001));
#278622=CARTESIAN_POINT('Ctrl Pts',(-9.04608879800006,15.2,-6.41990710100002));
#278623=CARTESIAN_POINT('Ctrl Pts',(-9.04608879800006,11.6,-6.41990710100002));
#278624=CARTESIAN_POINT('Ctrl Pts',(-9.04786451100006,15.2,-6.42260644100002));
#278625=CARTESIAN_POINT('Ctrl Pts',(-9.04786451100006,11.6,-6.42260644100002));
#278626=CARTESIAN_POINT('Ctrl Pts',(-9.04964085000006,15.2,-6.42531145100002));
#278627=CARTESIAN_POINT('Ctrl Pts',(-9.04964085000006,11.6,-6.42531145100002));
#278628=CARTESIAN_POINT('Ctrl Pts',(-9.05141780400006,15.2,-6.42802213200002));
#278629=CARTESIAN_POINT('Ctrl Pts',(-9.05141780400006,11.6,-6.42802213200002));
#278630=CARTESIAN_POINT('Ctrl Pts',(-9.05319536300006,15.2,-6.43073847600002));
#278631=CARTESIAN_POINT('Ctrl Pts',(-9.05319536300006,11.6,-6.43073847600002));
#278632=CARTESIAN_POINT('Ctrl Pts',(-9.05497351500006,15.2,-6.43346048200002));
#278633=CARTESIAN_POINT('Ctrl Pts',(-9.05497351500006,11.6,-6.43346048200002));
#278634=CARTESIAN_POINT('Ctrl Pts',(-9.05675225100006,15.2,-6.43618814600002));
#278635=CARTESIAN_POINT('Ctrl Pts',(-9.05675225100006,11.6,-6.43618814600002));
#278636=CARTESIAN_POINT('Ctrl Pts',(-9.05853156100006,15.2,-6.43892146500002));
#278637=CARTESIAN_POINT('Ctrl Pts',(-9.05853156100006,11.6,-6.43892146500002));
#278638=CARTESIAN_POINT('Ctrl Pts',(-9.06031143300006,15.2,-6.44166043400002));
#278639=CARTESIAN_POINT('Ctrl Pts',(-9.06031143300006,11.6,-6.44166043400002));
#278640=CARTESIAN_POINT('Ctrl Pts',(-9.06209185800006,15.2,-6.44440505100001));
#278641=CARTESIAN_POINT('Ctrl Pts',(-9.06209185800006,11.6,-6.44440505100001));
#278642=CARTESIAN_POINT('Ctrl Pts',(-9.06387282500006,15.2,-6.44715531100001));
#278643=CARTESIAN_POINT('Ctrl Pts',(-9.06387282500006,11.6,-6.44715531100001));
#278644=CARTESIAN_POINT('Ctrl Pts',(-9.06565432400006,15.2,-6.44991121200002));
#278645=CARTESIAN_POINT('Ctrl Pts',(-9.06565432400006,11.6,-6.44991121200002));
#278646=CARTESIAN_POINT('Ctrl Pts',(-9.06743634400006,15.2,-6.45267275100001));
#278647=CARTESIAN_POINT('Ctrl Pts',(-9.06743634400006,11.6,-6.45267275100001));
#278648=CARTESIAN_POINT('Ctrl Pts',(-9.06921887500006,15.2,-6.45543992300002));
#278649=CARTESIAN_POINT('Ctrl Pts',(-9.06921887500006,11.6,-6.45543992300002));
#278650=CARTESIAN_POINT('Ctrl Pts',(-9.07100190700006,15.2,-6.45821272500001));
#278651=CARTESIAN_POINT('Ctrl Pts',(-9.07100190700006,11.6,-6.45821272500001));
#278652=CARTESIAN_POINT('Ctrl Pts',(-9.07278543000006,15.2,-6.46099115300002));
#278653=CARTESIAN_POINT('Ctrl Pts',(-9.07278543000006,11.6,-6.46099115300002));
#278654=CARTESIAN_POINT('Ctrl Pts',(-9.07456943400006,15.2,-6.46377520400002));
#278655=CARTESIAN_POINT('Ctrl Pts',(-9.07456943400006,11.6,-6.46377520400002));
#278656=CARTESIAN_POINT('Ctrl Pts',(-9.07635390800005,15.2,-6.46656487600002));
#278657=CARTESIAN_POINT('Ctrl Pts',(-9.07635390800005,11.6,-6.46656487600002));
#278658=CARTESIAN_POINT('Ctrl Pts',(-9.07813884200005,15.2,-6.46936016400002));
#278659=CARTESIAN_POINT('Ctrl Pts',(-9.07813884200005,11.6,-6.46936016400002));
#278660=CARTESIAN_POINT('Ctrl Pts',(-9.07992422600006,15.2,-6.47216106300001));
#278661=CARTESIAN_POINT('Ctrl Pts',(-9.07992422600006,11.6,-6.47216106300001));
#278662=CARTESIAN_POINT('Ctrl Pts',(-9.08171005000005,15.2,-6.47496757300001));
#278663=CARTESIAN_POINT('Ctrl Pts',(-9.08171005000005,11.6,-6.47496757300001));
#278664=CARTESIAN_POINT('Ctrl Pts',(-9.08349630400006,15.2,-6.47777968800002));
#278665=CARTESIAN_POINT('Ctrl Pts',(-9.08349630400006,11.6,-6.47777968800002));
#278666=CARTESIAN_POINT('Ctrl Pts',(-9.08528297600006,15.2,-6.48059740600001));
#278667=CARTESIAN_POINT('Ctrl Pts',(-9.08528297600006,11.6,-6.48059740600001));
#278668=CARTESIAN_POINT('Ctrl Pts',(-9.08707006000006,15.2,-6.48342072200002));
#278669=CARTESIAN_POINT('Ctrl Pts',(-9.08707006000006,11.6,-6.48342072200002));
#278670=CARTESIAN_POINT('Ctrl Pts',(-9.08885754100006,15.2,-6.48624963300002));
#278671=CARTESIAN_POINT('Ctrl Pts',(-9.08885754100006,11.6,-6.48624963300002));
#278672=CARTESIAN_POINT('Ctrl Pts',(-9.09064541400006,15.2,-6.48908413600001));
#278673=CARTESIAN_POINT('Ctrl Pts',(-9.09064541400006,11.6,-6.48908413600001));
#278674=CARTESIAN_POINT('Ctrl Pts',(-9.09243366600006,15.2,-6.49192422600001));
#278675=CARTESIAN_POINT('Ctrl Pts',(-9.09243366600006,11.6,-6.49192422600001));
#278676=CARTESIAN_POINT('Ctrl Pts',(-9.09422228600006,15.2,-6.49476990200001));
#278677=CARTESIAN_POINT('Ctrl Pts',(-9.09422228600006,11.6,-6.49476990200001));
#278678=CARTESIAN_POINT('Ctrl Pts',(-9.09601126800006,15.2,-6.49762115900002));
#278679=CARTESIAN_POINT('Ctrl Pts',(-9.09601126800006,11.6,-6.49762115900002));
#278680=CARTESIAN_POINT('Ctrl Pts',(-9.09780059900006,15.2,-6.50047799400002));
#278681=CARTESIAN_POINT('Ctrl Pts',(-9.09780059900006,11.6,-6.50047799400002));
#278682=CARTESIAN_POINT('Ctrl Pts',(-9.09959026900006,15.2,-6.50334040300002));
#278683=CARTESIAN_POINT('Ctrl Pts',(-9.09959026900006,11.6,-6.50334040300002));
#278684=CARTESIAN_POINT('Ctrl Pts',(-9.10138027000006,15.2,-6.50620838300001));
#278685=CARTESIAN_POINT('Ctrl Pts',(-9.10138027000006,11.6,-6.50620838300001));
#278686=CARTESIAN_POINT('Ctrl Pts',(-9.10317059000005,15.2,-6.50908193000002));
#278687=CARTESIAN_POINT('Ctrl Pts',(-9.10317059000005,11.6,-6.50908193000002));
#278688=CARTESIAN_POINT('Ctrl Pts',(-9.10496122200006,15.2,-6.51196104000002));
#278689=CARTESIAN_POINT('Ctrl Pts',(-9.10496122200006,11.6,-6.51196104000002));
#278690=CARTESIAN_POINT('Ctrl Pts',(-9.10675215200006,15.2,-6.51484571200001));
#278691=CARTESIAN_POINT('Ctrl Pts',(-9.10675215200006,11.6,-6.51484571200001));
#278692=CARTESIAN_POINT('Ctrl Pts',(-9.10854337500006,15.2,-6.51773593900002));
#278693=CARTESIAN_POINT('Ctrl Pts',(-9.10854337500006,11.6,-6.51773593900002));
#278694=CARTESIAN_POINT('Ctrl Pts',(-9.11033487900006,15.2,-6.52063172000001));
#278695=CARTESIAN_POINT('Ctrl Pts',(-9.11033487900006,11.6,-6.52063172000001));
#278696=CARTESIAN_POINT('Ctrl Pts',(-9.11212665300006,15.2,-6.52353305100001));
#278697=CARTESIAN_POINT('Ctrl Pts',(-9.11212665300006,11.6,-6.52353305100001));
#278698=CARTESIAN_POINT('Ctrl Pts',(-9.11391868900006,15.2,-6.52643992700002));
#278699=CARTESIAN_POINT('Ctrl Pts',(-9.11391868900006,11.6,-6.52643992700002));
#278700=CARTESIAN_POINT('Ctrl Pts',(-9.11571097600006,15.2,-6.52935234700001));
#278701=CARTESIAN_POINT('Ctrl Pts',(-9.11571097600006,11.6,-6.52935234700001));
#278702=CARTESIAN_POINT('Ctrl Pts',(-9.11750350600006,15.2,-6.53227030600001));
#278703=CARTESIAN_POINT('Ctrl Pts',(-9.11750350600006,11.6,-6.53227030600001));
#278704=CARTESIAN_POINT('Ctrl Pts',(-9.11929626800006,15.2,-6.53519380000001));
#278705=CARTESIAN_POINT('Ctrl Pts',(-9.11929626800006,11.6,-6.53519380000001));
#278706=CARTESIAN_POINT('Ctrl Pts',(-9.12108925300006,15.2,-6.53812282700001));
#278707=CARTESIAN_POINT('Ctrl Pts',(-9.12108925300006,11.6,-6.53812282700001));
#278708=CARTESIAN_POINT('Ctrl Pts',(-9.12288245100006,15.2,-6.54105738200002));
#278709=CARTESIAN_POINT('Ctrl Pts',(-9.12288245100006,11.6,-6.54105738200002));
#278710=CARTESIAN_POINT('Ctrl Pts',(-9.12467585400006,15.2,-6.54399746200002));
#278711=CARTESIAN_POINT('Ctrl Pts',(-9.12467585400006,11.6,-6.54399746200002));
#278712=CARTESIAN_POINT('Ctrl Pts',(-9.12646945000006,15.2,-6.54694306500001));
#278713=CARTESIAN_POINT('Ctrl Pts',(-9.12646945000006,11.6,-6.54694306500001));
#278714=CARTESIAN_POINT('Ctrl Pts',(-9.12826322900005,15.2,-6.54989418500002));
#278715=CARTESIAN_POINT('Ctrl Pts',(-9.12826322900005,11.6,-6.54989418500002));
#278716=CARTESIAN_POINT('Ctrl Pts',(-9.13005718400006,15.2,-6.55285082000002));
#278717=CARTESIAN_POINT('Ctrl Pts',(-9.13005718400006,11.6,-6.55285082000002));
#278718=CARTESIAN_POINT('Ctrl Pts',(-9.13185130600005,15.2,-6.55581296500002));
#278719=CARTESIAN_POINT('Ctrl Pts',(-9.13185130600005,11.6,-6.55581296500002));
#278720=CARTESIAN_POINT('Ctrl Pts',(-9.13364558200006,15.2,-6.55878061800002));
#278721=CARTESIAN_POINT('Ctrl Pts',(-9.13364558200006,11.6,-6.55878061800002));
#278722=CARTESIAN_POINT('Ctrl Pts',(-9.13544000500006,15.2,-6.56175377700002));
#278723=CARTESIAN_POINT('Ctrl Pts',(-9.13544000500006,11.6,-6.56175377700002));
#278724=CARTESIAN_POINT('Ctrl Pts',(-9.13723456500006,15.2,-6.56473243400002));
#278725=CARTESIAN_POINT('Ctrl Pts',(-9.13723456500006,11.6,-6.56473243400002));
#278726=CARTESIAN_POINT('Ctrl Pts',(-9.13902925300006,15.2,-6.56771658900002));
#278727=CARTESIAN_POINT('Ctrl Pts',(-9.13902925300006,11.6,-6.56771658900002));
#278728=CARTESIAN_POINT('Ctrl Pts',(-9.14082405800006,15.2,-6.57070623800001));
#278729=CARTESIAN_POINT('Ctrl Pts',(-9.14082405800006,11.6,-6.57070623800001));
#278730=CARTESIAN_POINT('Ctrl Pts',(-9.14261897300005,15.2,-6.57370137600001));
#278731=CARTESIAN_POINT('Ctrl Pts',(-9.14261897300005,11.6,-6.57370137600001));
#278732=CARTESIAN_POINT('Ctrl Pts',(-9.14441398600006,15.2,-6.57670200000001));
#278733=CARTESIAN_POINT('Ctrl Pts',(-9.14441398600006,11.6,-6.57670200000001));
#278734=CARTESIAN_POINT('Ctrl Pts',(-9.14620909000006,15.2,-6.57970810800002));
#278735=CARTESIAN_POINT('Ctrl Pts',(-9.14620909000006,11.6,-6.57970810800002));
#278736=CARTESIAN_POINT('Ctrl Pts',(-9.14800427400005,15.2,-6.58271969500002));
#278737=CARTESIAN_POINT('Ctrl Pts',(-9.14800427400005,11.6,-6.58271969500002));
#278738=CARTESIAN_POINT('Ctrl Pts',(-9.14979953000006,15.2,-6.58573675700002));
#278739=CARTESIAN_POINT('Ctrl Pts',(-9.14979953000006,11.6,-6.58573675700002));
#278740=CARTESIAN_POINT('Ctrl Pts',(-9.15159484800006,15.2,-6.58875929200001));
#278741=CARTESIAN_POINT('Ctrl Pts',(-9.15159484800006,11.6,-6.58875929200001));
#278742=CARTESIAN_POINT('Ctrl Pts',(-9.15339022000006,15.2,-6.59178729700002));
#278743=CARTESIAN_POINT('Ctrl Pts',(-9.15339022000006,11.6,-6.59178729700002));
#278744=CARTESIAN_POINT('Ctrl Pts',(-9.15518563400006,15.2,-6.59482076600002));
#278745=CARTESIAN_POINT('Ctrl Pts',(-9.15518563400006,11.6,-6.59482076600002));
#278746=CARTESIAN_POINT('Ctrl Pts',(-9.15698108400005,15.2,-6.59785969700001));
#278747=CARTESIAN_POINT('Ctrl Pts',(-9.15698108400005,11.6,-6.59785969700001));
#278748=CARTESIAN_POINT('Ctrl Pts',(-9.15877655800006,15.2,-6.60090408500002));
#278749=CARTESIAN_POINT('Ctrl Pts',(-9.15877655800006,11.6,-6.60090408500002));
#278750=CARTESIAN_POINT('Ctrl Pts',(-9.16057204800006,15.2,-6.60395392900002));
#278751=CARTESIAN_POINT('Ctrl Pts',(-9.16057204800006,11.6,-6.60395392900002));
#278752=CARTESIAN_POINT('Ctrl Pts',(-9.16236754400006,15.2,-6.60700922400002));
#278753=CARTESIAN_POINT('Ctrl Pts',(-9.16236754400006,11.6,-6.60700922400002));
#278754=CARTESIAN_POINT('Ctrl Pts',(-9.16416303800006,15.2,-6.61006996600002));
#278755=CARTESIAN_POINT('Ctrl Pts',(-9.16416303800006,11.6,-6.61006996600002));
#278756=CARTESIAN_POINT('Ctrl Pts',(-9.16595852200006,15.2,-6.61313615300001));
#278757=CARTESIAN_POINT('Ctrl Pts',(-9.16595852200006,11.6,-6.61313615300001));
#278758=CARTESIAN_POINT('Ctrl Pts',(-9.16775398400006,15.2,-6.61620778000002));
#278759=CARTESIAN_POINT('Ctrl Pts',(-9.16775398400006,11.6,-6.61620778000002));
#278760=CARTESIAN_POINT('Ctrl Pts',(-9.16954941700006,15.2,-6.61928484400002));
#278761=CARTESIAN_POINT('Ctrl Pts',(-9.16954941700006,11.6,-6.61928484400002));
#278762=CARTESIAN_POINT('Ctrl Pts',(-9.17134481000006,15.2,-6.62236734100001));
#278763=CARTESIAN_POINT('Ctrl Pts',(-9.17134481000006,11.6,-6.62236734100001));
#278764=CARTESIAN_POINT('Ctrl Pts',(-9.17314015700006,15.2,-6.62545526700002));
#278765=CARTESIAN_POINT('Ctrl Pts',(-9.17314015700006,11.6,-6.62545526700002));
#278766=CARTESIAN_POINT('Ctrl Pts',(-9.17493544600006,15.2,-6.62854862000002));
#278767=CARTESIAN_POINT('Ctrl Pts',(-9.17493544600006,11.6,-6.62854862000002));
#278768=CARTESIAN_POINT('Ctrl Pts',(-9.17673066900005,15.2,-6.63164739700001));
#278769=CARTESIAN_POINT('Ctrl Pts',(-9.17673066900005,11.6,-6.63164739700001));
#278770=CARTESIAN_POINT('Ctrl Pts',(-9.17852581900006,15.2,-6.63475159300001));
#278771=CARTESIAN_POINT('Ctrl Pts',(-9.17852581900006,11.6,-6.63475159300001));
#278772=CARTESIAN_POINT('Ctrl Pts',(-9.18032088300006,15.2,-6.63786120300002));
#278773=CARTESIAN_POINT('Ctrl Pts',(-9.18032088300006,11.6,-6.63786120300002));
#278774=CARTESIAN_POINT('Ctrl Pts',(-9.18211585500006,15.2,-6.64097622700002));
#278775=CARTESIAN_POINT('Ctrl Pts',(-9.18211585500006,11.6,-6.64097622700002));
#278776=CARTESIAN_POINT('Ctrl Pts',(-9.18391072400006,15.2,-6.64409665900001));
#278777=CARTESIAN_POINT('Ctrl Pts',(-9.18391072400006,11.6,-6.64409665900001));
#278778=CARTESIAN_POINT('Ctrl Pts',(-9.18570548500006,15.2,-6.64722249500001));
#278779=CARTESIAN_POINT('Ctrl Pts',(-9.18570548500006,11.6,-6.64722249500001));
#278780=CARTESIAN_POINT('Ctrl Pts',(-9.18750012400006,15.2,-6.65035373300002));
#278781=CARTESIAN_POINT('Ctrl Pts',(-9.18750012400006,11.6,-6.65035373300002));
#278782=CARTESIAN_POINT('Ctrl Pts',(-9.18929463600006,15.2,-6.65349037000002));
#278783=CARTESIAN_POINT('Ctrl Pts',(-9.18929463600006,11.6,-6.65349037000002));
#278784=CARTESIAN_POINT('Ctrl Pts',(-9.19108901000006,15.2,-6.65663240000002));
#278785=CARTESIAN_POINT('Ctrl Pts',(-9.19108901000006,11.6,-6.65663240000002));
#278786=CARTESIAN_POINT('Ctrl Pts',(-9.19288323700006,15.2,-6.65977982200002));
#278787=CARTESIAN_POINT('Ctrl Pts',(-9.19288323700006,11.6,-6.65977982200002));
#278788=CARTESIAN_POINT('Ctrl Pts',(-9.19467731000006,15.2,-6.66293263100001));
#278789=CARTESIAN_POINT('Ctrl Pts',(-9.19467731000006,11.6,-6.66293263100001));
#278790=CARTESIAN_POINT('Ctrl Pts',(-9.19647122000006,15.2,-6.66609082300001));
#278791=CARTESIAN_POINT('Ctrl Pts',(-9.19647122000006,11.6,-6.66609082300001));
#278792=CARTESIAN_POINT('Ctrl Pts',(-9.19826495500006,15.2,-6.66925439600002));
#278793=CARTESIAN_POINT('Ctrl Pts',(-9.19826495500006,11.6,-6.66925439600002));
#278794=CARTESIAN_POINT('Ctrl Pts',(-9.20005851100006,15.2,-6.67242334500001));
#278795=CARTESIAN_POINT('Ctrl Pts',(-9.20005851100006,11.6,-6.67242334500001));
#278796=CARTESIAN_POINT('Ctrl Pts',(-9.20185187600006,15.2,-6.67559766700002));
#278797=CARTESIAN_POINT('Ctrl Pts',(-9.20185187600006,11.6,-6.67559766700002));
#278798=CARTESIAN_POINT('Ctrl Pts',(-9.20364504200006,15.2,-6.67877735900002));
#278799=CARTESIAN_POINT('Ctrl Pts',(-9.20364504200006,11.6,-6.67877735900002));
#278800=CARTESIAN_POINT('Ctrl Pts',(-9.20543800000006,15.2,-6.68196241700001));
#278801=CARTESIAN_POINT('Ctrl Pts',(-9.20543800000006,11.6,-6.68196241700001));
#278802=CARTESIAN_POINT('Ctrl Pts',(-9.20723074300006,15.2,-6.68515283700001));
#278803=CARTESIAN_POINT('Ctrl Pts',(-9.20723074300006,11.6,-6.68515283700001));
#278804=CARTESIAN_POINT('Ctrl Pts',(-9.20902326000006,15.2,-6.68834861600001));
#278805=CARTESIAN_POINT('Ctrl Pts',(-9.20902326000006,11.6,-6.68834861600001));
#278806=CARTESIAN_POINT('Ctrl Pts',(-9.21081554300006,15.2,-6.69154975000002));
#278807=CARTESIAN_POINT('Ctrl Pts',(-9.21081554300006,11.6,-6.69154975000002));
#278808=CARTESIAN_POINT('Ctrl Pts',(-9.21260758500006,15.2,-6.69475623600002));
#278809=CARTESIAN_POINT('Ctrl Pts',(-9.21260758500006,11.6,-6.69475623600002));
#278810=CARTESIAN_POINT('Ctrl Pts',(-9.21439937500006,15.2,-6.69796807000001));
#278811=CARTESIAN_POINT('Ctrl Pts',(-9.21439937500006,11.6,-6.69796807000001));
#278812=CARTESIAN_POINT('Ctrl Pts',(-9.21619090600006,15.2,-6.70118524900002));
#278813=CARTESIAN_POINT('Ctrl Pts',(-9.21619090600006,11.6,-6.70118524900002));
#278814=CARTESIAN_POINT('Ctrl Pts',(-9.21798216800006,15.2,-6.70440776900002));
#278815=CARTESIAN_POINT('Ctrl Pts',(-9.21798216800006,11.6,-6.70440776900002));
#278816=CARTESIAN_POINT('Ctrl Pts',(-9.21977315400006,15.2,-6.70763562500002));
#278817=CARTESIAN_POINT('Ctrl Pts',(-9.21977315400006,11.6,-6.70763562500002));
#278818=CARTESIAN_POINT('Ctrl Pts',(-9.22156385400006,15.2,-6.71086881600001));
#278819=CARTESIAN_POINT('Ctrl Pts',(-9.22156385400006,11.6,-6.71086881600001));
#278820=CARTESIAN_POINT('Ctrl Pts',(-9.22335426000006,15.2,-6.71410733700001));
#278821=CARTESIAN_POINT('Ctrl Pts',(-9.22335426000006,11.6,-6.71410733700001));
#278822=CARTESIAN_POINT('Ctrl Pts',(-9.22514436500006,15.2,-6.71735118500001));
#278823=CARTESIAN_POINT('Ctrl Pts',(-9.22514436500006,11.6,-6.71735118500001));
#278824=CARTESIAN_POINT('Ctrl Pts',(-9.22693415700006,15.2,-6.72060035600002));
#278825=CARTESIAN_POINT('Ctrl Pts',(-9.22693415700006,11.6,-6.72060035600002));
#278826=CARTESIAN_POINT('Ctrl Pts',(-9.22872363300005,15.2,-6.72385484600002));
#278827=CARTESIAN_POINT('Ctrl Pts',(-9.22872363300005,11.6,-6.72385484600002));
#278828=CARTESIAN_POINT('Ctrl Pts',(-9.23051278000005,15.2,-6.72711465300001));
#278829=CARTESIAN_POINT('Ctrl Pts',(-9.23051278000005,11.6,-6.72711465300001));
#278830=CARTESIAN_POINT('Ctrl Pts',(-9.23230159100006,15.2,-6.73037977300002));
#278831=CARTESIAN_POINT('Ctrl Pts',(-9.23230159100006,11.6,-6.73037977300002));
#278832=CARTESIAN_POINT('Ctrl Pts',(-9.23409005700006,15.2,-6.73365020100002));
#278833=CARTESIAN_POINT('Ctrl Pts',(-9.23409005700006,11.6,-6.73365020100002));
#278834=CARTESIAN_POINT('Ctrl Pts',(-9.23587817000006,15.2,-6.73692593400002));
#278835=CARTESIAN_POINT('Ctrl Pts',(-9.23587817000006,11.6,-6.73692593400002));
#278836=CARTESIAN_POINT('Ctrl Pts',(-9.23766592000005,15.2,-6.74020696900002));
#278837=CARTESIAN_POINT('Ctrl Pts',(-9.23766592000005,11.6,-6.74020696900002));
#278838=CARTESIAN_POINT('Ctrl Pts',(-9.23945330000006,15.2,-6.74349330100001));
#278839=CARTESIAN_POINT('Ctrl Pts',(-9.23945330000006,11.6,-6.74349330100001));
#278840=CARTESIAN_POINT('Ctrl Pts',(-9.24124030000005,15.2,-6.74678492800002));
#278841=CARTESIAN_POINT('Ctrl Pts',(-9.24124030000005,11.6,-6.74678492800002));
#278842=CARTESIAN_POINT('Ctrl Pts',(-9.24302691300005,15.2,-6.75008184600002));
#278843=CARTESIAN_POINT('Ctrl Pts',(-9.24302691300005,11.6,-6.75008184600002));
#278844=CARTESIAN_POINT('Ctrl Pts',(-9.24481313200006,15.2,-6.75338405000002));
#278845=CARTESIAN_POINT('Ctrl Pts',(-9.24481313200006,11.6,-6.75338405000002));
#278846=CARTESIAN_POINT('Ctrl Pts',(-9.24659894900006,15.2,-6.75669153900002));
#278847=CARTESIAN_POINT('Ctrl Pts',(-9.24659894900006,11.6,-6.75669153900002));
#278848=CARTESIAN_POINT('Ctrl Pts',(-9.24838435600006,15.2,-6.76000431000002));
#278849=CARTESIAN_POINT('Ctrl Pts',(-9.24838435600006,11.6,-6.76000431000002));
#278850=CARTESIAN_POINT('Ctrl Pts',(-9.25016934500006,15.2,-6.76332235800002));
#278851=CARTESIAN_POINT('Ctrl Pts',(-9.25016934500006,11.6,-6.76332235800002));
#278852=CARTESIAN_POINT('Ctrl Pts',(-9.25195390900006,15.2,-6.76664567900002));
#278853=CARTESIAN_POINT('Ctrl Pts',(-9.25195390900006,11.6,-6.76664567900002));
#278854=CARTESIAN_POINT('Ctrl Pts',(-9.25373803600005,15.2,-6.76997427200002));
#278855=CARTESIAN_POINT('Ctrl Pts',(-9.25373803600005,11.6,-6.76997427200002));
#278856=CARTESIAN_POINT('Ctrl Pts',(-9.25552171800006,15.2,-6.77330812800002));
#278857=CARTESIAN_POINT('Ctrl Pts',(-9.25552171800006,11.6,-6.77330812800002));
#278858=CARTESIAN_POINT('Ctrl Pts',(-9.25730494300005,15.2,-6.77664724600002));
#278859=CARTESIAN_POINT('Ctrl Pts',(-9.25730494300005,11.6,-6.77664724600002));
#278860=CARTESIAN_POINT('Ctrl Pts',(-9.25908770300006,15.2,-6.77999162000001));
#278861=CARTESIAN_POINT('Ctrl Pts',(-9.25908770300006,11.6,-6.77999162000001));
#278862=CARTESIAN_POINT('Ctrl Pts',(-9.26086998700006,15.2,-6.78334124800001));
#278863=CARTESIAN_POINT('Ctrl Pts',(-9.26086998700006,11.6,-6.78334124800001));
#278864=CARTESIAN_POINT('Ctrl Pts',(-9.26265178900006,15.2,-6.78669612500002));
#278865=CARTESIAN_POINT('Ctrl Pts',(-9.26265178900006,11.6,-6.78669612500002));
#278866=CARTESIAN_POINT('Ctrl Pts',(-9.26443310200005,15.2,-6.79005624800002));
#278867=CARTESIAN_POINT('Ctrl Pts',(-9.26443310200005,11.6,-6.79005624800002));
#278868=CARTESIAN_POINT('Ctrl Pts',(-9.26621392500006,15.2,-6.79342161700002));
#278869=CARTESIAN_POINT('Ctrl Pts',(-9.26621392500006,11.6,-6.79342161700002));
#278870=CARTESIAN_POINT('Ctrl Pts',(-9.26799425300005,15.2,-6.79679223000001));
#278871=CARTESIAN_POINT('Ctrl Pts',(-9.26799425300005,11.6,-6.79679223000001));
#278872=CARTESIAN_POINT('Ctrl Pts',(-9.26941812100005,15.2,-6.79949291400002));
#278873=CARTESIAN_POINT('Ctrl Pts',(-9.26941812100005,11.6,-6.79949291400002));
#278874=CARTESIAN_POINT('Ctrl Pts',(-9.27048579800006,15.2,-6.80152078800001));
#278875=CARTESIAN_POINT('Ctrl Pts',(-9.27048579800006,11.6,-6.80152078800001));
#278876=CARTESIAN_POINT('Ctrl Pts',(-9.27119748500006,15.2,-6.80287375200002));
#278877=CARTESIAN_POINT('Ctrl Pts',(-9.27119748500006,11.6,-6.80287375200002));
#278878=CARTESIAN_POINT('Ctrl Pts',(-9.27155330300005,15.2,-6.80355049700001));
#278879=CARTESIAN_POINT('Ctrl Pts',(-9.27155330300005,11.6,-6.80355049700001));
#278880=CARTESIAN_POINT('Ctrl Pts',(-8.56667971000006,15.2,-5.85257411400002));
#278881=CARTESIAN_POINT('Ctrl Pts',(-8.56806288384934,15.2,-5.85370503502559));
#278882=CARTESIAN_POINT('Ctrl Pts',(-8.56948692484017,15.2,-5.85487627493062));
#278883=CARTESIAN_POINT('Ctrl Pts',(-8.57095065283135,15.2,-5.85608775313393));
#278884=CARTESIAN_POINT('Ctrl Pts',(-8.57242143965877,15.2,-5.85730507369751));
#278885=CARTESIAN_POINT('Ctrl Pts',(-8.57393230452754,15.2,-5.85856301222101));
#278886=CARTESIAN_POINT('Ctrl Pts',(-8.57548210844168,15.2,-5.85986145285899));
#278887=CARTESIAN_POINT('Ctrl Pts',(-8.57703191221504,15.2,-5.86115989337901));
#278888=CARTESIAN_POINT('Ctrl Pts',(-8.57862065441741,15.2,-5.86249883667505));
#278889=CARTESIAN_POINT('Ctrl Pts',(-8.58024722827499,15.2,-5.86387816920827));
#278890=CARTESIAN_POINT('Ctrl Pts',(-8.58187380213257,15.2,-5.8652575017415));
#278891=CARTESIAN_POINT('Ctrl Pts',(-8.58353820868947,15.1999999999999,
-5.86667722288291));
#278892=CARTESIAN_POINT('Ctrl Pts',(-8.58523937179385,15.2,-5.86813722031714));
#278893=CARTESIAN_POINT('Ctrl Pts',(-8.58694053505276,15.2,-5.86959721788399));
#278894=CARTESIAN_POINT('Ctrl Pts',(-8.58867845668591,15.2,-5.87109749028118));
#278895=CARTESIAN_POINT('Ctrl Pts',(-8.59045208820166,15.2,-5.87263792486786));
#278896=CARTESIAN_POINT('Ctrl Pts',(-8.59222571955631,15.2,-5.87417835931461));
#278897=CARTESIAN_POINT('Ctrl Pts',(-8.59403506469271,15.2,-5.87575895551878));
#278898=CARTESIAN_POINT('Ctrl Pts',(-8.5958791059675,15.2,-5.87737960096735));
#278899=CARTESIAN_POINT('Ctrl Pts',(-8.59772314724229,15.2,-5.87900024641592));
#278900=CARTESIAN_POINT('Ctrl Pts',(-8.59960188407517,15.2,-5.88066094137928));
#278901=CARTESIAN_POINT('Ctrl Pts',(-8.60151432942091,15.2,-5.8823615708991));
#278902=CARTESIAN_POINT('Ctrl Pts',(-8.60342677494035,15.2,-5.88406220057339));
#278903=CARTESIAN_POINT('Ctrl Pts',(-8.60537292788893,15.2,-5.88580276593591));
#278904=CARTESIAN_POINT('Ctrl Pts',(-8.60735182649905,15.2,-5.88758315445236));
#278905=CARTESIAN_POINT('Ctrl Pts',(-8.6093307249294,15.2,-5.88936354280707));
#278906=CARTESIAN_POINT('Ctrl Pts',(-8.61134236849269,15.2,-5.89118375430898));
#278907=CARTESIAN_POINT('Ctrl Pts',(-8.61338582016984,15.2,-5.89304367482648));
#278908=CARTESIAN_POINT('Ctrl Pts',(-8.615429271847,15.2,-5.89490359534398));
#278909=CARTESIAN_POINT('Ctrl Pts',(-8.61750453139654,15.2,-5.89680322461661));
#278910=CARTESIAN_POINT('Ctrl Pts',(-8.61961068615201,15.2,-5.89874245187776));
#278911=CARTESIAN_POINT('Ctrl Pts',(-8.62171684090748,15.2,-5.90068167913891));
#278912=CARTESIAN_POINT('Ctrl Pts',(-8.62385388904458,15.2,-5.90266050258931));
#278913=CARTESIAN_POINT('Ctrl Pts',(-8.62602094279714,15.2,-5.9046788090133));
#278914=CARTESIAN_POINT('Ctrl Pts',(-8.62818799674654,15.2,-5.90669711562061));
#278915=CARTESIAN_POINT('Ctrl Pts',(-8.63038505409052,15.2,-5.90875490690673));
#278916=CARTESIAN_POINT('Ctrl Pts',(-8.63261124812979,15.2,-5.91085206660608));
#278917=CARTESIAN_POINT('Ctrl Pts',(-8.63483744196683,15.2,-5.91294922611493));
#278918=CARTESIAN_POINT('Ctrl Pts',(-8.63709277010499,15.2,-5.91508575739324));
#278919=CARTESIAN_POINT('Ctrl Pts',(-8.63937638719897,15.2,-5.91726154574063));
#278920=CARTESIAN_POINT('Ctrl Pts',(-8.64166000429297,15.2,-5.91943733408802));
#278921=CARTESIAN_POINT('Ctrl Pts',(-8.64397191091524,15.2,-5.9216523775805));
#278922=CARTESIAN_POINT('Ctrl Pts',(-8.64631127799502,15.2,-5.92390656674592));
#278923=CARTESIAN_POINT('Ctrl Pts',(-8.6486506452873,15.2,-5.92616075611608));
#278924=CARTESIAN_POINT('Ctrl Pts',(-8.65101747287396,15.2,-5.92845408682341));
#278925=CARTESIAN_POINT('Ctrl Pts',(-8.65341095442223,15.2,-5.93078644936889));
#278926=CARTESIAN_POINT('Ctrl Pts',(-8.6558044357531,15.2,-5.93311881170251));
#278927=CARTESIAN_POINT('Ctrl Pts',(-8.65822457123507,15.2,-5.93549020269225));
#278928=CARTESIAN_POINT('Ctrl Pts',(-8.66067056874057,15.2,-5.93790051194886));
#278929=CARTESIAN_POINT('Ctrl Pts',(-8.66311656624608,15.2,-5.94031082120545));
#278930=CARTESIAN_POINT('Ctrl Pts',(-8.66558843005363,15.2,-5.94276004585515));
#278931=CARTESIAN_POINT('Ctrl Pts',(-8.66808538546118,15.2,-5.94524807326209));
#278932=CARTESIAN_POINT('Ctrl Pts',(-8.67058234109555,15.2,-5.94773610089503));
#278933=CARTESIAN_POINT('Ctrl Pts',(-8.67310438880402,15.2,-5.95026293009468));
#278934=CARTESIAN_POINT('Ctrl Pts',(-8.67565077648807,15.2,-5.95282844969823));
#278935=CARTESIAN_POINT('Ctrl Pts',(-8.67819716394084,15.2,-5.95539396906875));
#278936=CARTESIAN_POINT('Ctrl Pts',(-8.68076788847761,15.2,-5.95799817577096));
#278937=CARTESIAN_POINT('Ctrl Pts',(-8.68336221571668,15.2,-5.96064095625828));
#278938=CARTESIAN_POINT('Ctrl Pts',(-8.68595654295576,15.2,-5.96328373674558));
#278939=CARTESIAN_POINT('Ctrl Pts',(-8.68857446975996,15.2,-5.96596509348544));
#278940=CARTESIAN_POINT('Ctrl Pts',(-8.69121527746127,15.2,-5.96868490802027));
#278941=CARTESIAN_POINT('Ctrl Pts',(-8.69385608540248,15.2,-5.97140472280214));
#278942=CARTESIAN_POINT('Ctrl Pts',(-8.69651977346154,15.2,-5.97416299852474));
#278943=CARTESIAN_POINT('Ctrl Pts',(-8.69920563427612,15.2,-5.97695961826312));
#278944=CARTESIAN_POINT('Ctrl Pts',(-8.70189149484673,15.2,-5.97975623774748));
#278945=CARTESIAN_POINT('Ctrl Pts',(-8.70459952848798,15.2,-5.98259120266751));
#278946=CARTESIAN_POINT('Ctrl Pts',(-8.70732904423459,15.2,-5.98546439799293));
#278947=CARTESIAN_POINT('Ctrl Pts',(-8.71005855998121,15.2,-5.98833759331834));
#278948=CARTESIAN_POINT('Ctrl Pts',(-8.712809559009,15.2,-5.99124901789818));
#278949=CARTESIAN_POINT('Ctrl Pts',(-8.71558136182404,15.2,-5.99419855728936));
#278950=CARTESIAN_POINT('Ctrl Pts',(-8.71789119758718,15.2,-5.99665650687132));
#278951=CARTESIAN_POINT('Ctrl Pts',(-8.72021548140903,15.2,-5.99914092571506));
#278952=CARTESIAN_POINT('Ctrl Pts',(-8.72255382883885,15.2,-6.0016517460609));
#278953=CARTESIAN_POINT('Ctrl Pts',(-8.72489217626867,15.2,-6.00416256640674));
#278954=CARTESIAN_POINT('Ctrl Pts',(-8.72724458758246,15.2,-6.00669978913697));
#278955=CARTESIAN_POINT('Ctrl Pts',(-8.72961068502373,15.2,-6.00926334623189));
#278956=CARTESIAN_POINT('Ctrl Pts',(-8.731976782465,15.2,-6.0118269033268));
#278957=CARTESIAN_POINT('Ctrl Pts',(-8.73435656410001,15.2,-6.0144167953555));
#278958=CARTESIAN_POINT('Ctrl Pts',(-8.73674966076669,15.2,-6.01703295500828));
#278959=CARTESIAN_POINT('Ctrl Pts',(-8.73914275743336,15.2,-6.01964911466105));
#278960=CARTESIAN_POINT('Ctrl Pts',(-8.74154916827364,15.2,-6.02229154210031));
#278961=CARTESIAN_POINT('Ctrl Pts',(-8.74396852599302,15.2,-6.02496017079308));
#278962=CARTESIAN_POINT('Ctrl Pts',(-8.74638788371239,15.2,-6.02762879948585));
#278963=CARTESIAN_POINT('Ctrl Pts',(-8.74882019127601,15.2,-6.0303236283378));
#278964=CARTESIAN_POINT('Ctrl Pts',(-8.75126508565167,15.2,-6.0330445911864));
#278965=CARTESIAN_POINT('Ctrl Pts',(-8.75370998002734,15.2,-6.03576555403501));
#278966=CARTESIAN_POINT('Ctrl Pts',(-8.75616746439987,15.2,-6.038512650419));
#278967=CARTESIAN_POINT('Ctrl Pts',(-8.75863718217829,15.2,-6.04128581173981));
#278968=CARTESIAN_POINT('Ctrl Pts',(-8.7611068999567,15.2,-6.0440589730606));
#278969=CARTESIAN_POINT('Ctrl Pts',(-8.76358885294193,15.2,-6.04685820099616));
#278970=CARTESIAN_POINT('Ctrl Pts',(-8.76608269153957,15.2,-6.04968342731967));
#278971=CARTESIAN_POINT('Ctrl Pts',(-8.7685765301372,15.2,-6.05250865364318));
#278972=CARTESIAN_POINT('Ctrl Pts',(-8.77108225506726,15.2,-6.05535987786309));
#278973=CARTESIAN_POINT('Ctrl Pts',(-8.77359952284596,15.2,-6.05823703314296));
#278974=CARTESIAN_POINT('Ctrl Pts',(-8.77611679062466,15.2,-6.06111418842282));
#278975=CARTESIAN_POINT('Ctrl Pts',(-8.77864560165358,15.2,-6.06401727391984));
#278976=CARTESIAN_POINT('Ctrl Pts',(-8.78118561859893,15.2,-6.06694622190807));
#278977=CARTESIAN_POINT('Ctrl Pts',(-8.78372563526744,15.2,-6.06987516957704));
#278978=CARTESIAN_POINT('Ctrl Pts',(-8.78627685702285,15.2,-6.07282997980375));
#278979=CARTESIAN_POINT('Ctrl Pts',(-8.78883895271491,15.2,-6.07581058635177));
#278980=CARTESIAN_POINT('Ctrl Pts',(-8.79140104868625,15.2,-6.07879119322466));
#278981=CARTESIAN_POINT('Ctrl Pts',(-8.79397401767406,15.2,-6.08179759316655));
#278982=CARTESIAN_POINT('Ctrl Pts',(-8.79655753218712,15.2,-6.08482971955336));
#278983=CARTESIAN_POINT('Ctrl Pts',(-8.79914104670016,15.2,-6.08786184594017));
#278984=CARTESIAN_POINT('Ctrl Pts',(-8.80173510762689,15.2,-6.09091970129317));
#278985=CARTESIAN_POINT('Ctrl Pts',(-8.80433939137606,15.2,-6.09400321330497));
#278986=CARTESIAN_POINT('Ctrl Pts',(-8.80694367512524,15.2,-6.09708672531678));
#278987=CARTESIAN_POINT('Ctrl Pts',(-8.80955818265387,15.2,-6.1001958954091));
#278988=CARTESIAN_POINT('Ctrl Pts',(-8.81218259639541,15.2,-6.10333065591114));
#278989=CARTESIAN_POINT('Ctrl Pts',(-8.81480701013694,15.2,-6.10646541641319));
#278990=CARTESIAN_POINT('Ctrl Pts',(-8.81744132993878,15.2,-6.10962576694863));
#278991=CARTESIAN_POINT('Ctrl Pts',(-8.82008524132718,15.2,-6.11281163826675));
#278992=CARTESIAN_POINT('Ctrl Pts',(-8.82272915271557,15.2,-6.11599750958487));
#278993=CARTESIAN_POINT('Ctrl Pts',(-8.82538265717086,15.2,-6.11920890262307));
#278994=CARTESIAN_POINT('Ctrl Pts',(-8.82804544605928,15.2,-6.12244574803842));
#278995=CARTESIAN_POINT('Ctrl Pts',(-8.8301756772861,15.2,-6.12503522451181));
#278996=CARTESIAN_POINT('Ctrl Pts',(-8.83231185130607,15.2,-6.12764099158576));
#278997=CARTESIAN_POINT('Ctrl Pts',(-8.83445381058588,15.2,-6.13026301213885));
#278998=CARTESIAN_POINT('Ctrl Pts',(-8.83659576957385,15.2,-6.13288503233469));
#278999=CARTESIAN_POINT('Ctrl Pts',(-8.83874351450323,15.2,-6.13552330721506));
#279000=CARTESIAN_POINT('Ctrl Pts',(-8.84089689204905,15.2,-6.13817780127477));
#279001=CARTESIAN_POINT('Ctrl Pts',(-8.84305026988826,15.2,-6.14083229569616));
#279002=CARTESIAN_POINT('Ctrl Pts',(-8.84520928007816,15.2,-6.14350300849172));
#279003=CARTESIAN_POINT('Ctrl Pts',(-8.8473737699187,15.2,-6.14618990569476));
#279004=CARTESIAN_POINT('Ctrl Pts',(-8.84953825946433,15.2,-6.14887680253172));
#279005=CARTESIAN_POINT('Ctrl Pts',(-8.85170822732348,15.2,-6.15157988369332));
#279006=CARTESIAN_POINT('Ctrl Pts',(-8.85388352564275,15.2,-6.15429911260547));
#279007=CARTESIAN_POINT('Ctrl Pts',(-8.8560588242584,15.2,-6.15701834188811));
#279008=CARTESIAN_POINT('Ctrl Pts',(-8.85823945179819,15.2,-6.15975372025736));
#279009=CARTESIAN_POINT('Ctrl Pts',(-8.86042525969545,15.2,-6.16250521074171));
#279010=CARTESIAN_POINT('Ctrl Pts',(-8.86261106729488,15.2,-6.16525670085117));
#279011=CARTESIAN_POINT('Ctrl Pts',(-8.86480205507935,15.2,-6.16802430430459));
#279012=CARTESIAN_POINT('Ctrl Pts',(-8.86699807539933,15.2,-6.17080798501983));
#279013=CARTESIAN_POINT('Ctrl Pts',(-8.86919409601849,15.2,-6.17359166611435));
#279014=CARTESIAN_POINT('Ctrl Pts',(-8.87139514961294,15.2,-6.17639142383001));
#279015=CARTESIAN_POINT('Ctrl Pts',(-8.87360109024321,15.2,-6.17920722421854));
#279016=CARTESIAN_POINT('Ctrl Pts',(-8.87580703057293,15.2,-6.18202302422343));
#279017=CARTESIAN_POINT('Ctrl Pts',(-8.87801785844163,15.2,-6.1848548652799));
#279018=CARTESIAN_POINT('Ctrl Pts',(-8.88023342937113,15.2,-6.18770271326767));
#279019=CARTESIAN_POINT('Ctrl Pts',(-8.8824490006025,15.2,-6.19055056164345));
#279020=CARTESIAN_POINT('Ctrl Pts',(-8.88466931401767,15.2,-6.19341441575966));
#279021=CARTESIAN_POINT('Ctrl Pts',(-8.88689422925004,15.2,-6.19629424024995));
#279022=CARTESIAN_POINT('Ctrl Pts',(-8.88911914448241,15.2,-6.19917406474024));
#279023=CARTESIAN_POINT('Ctrl Pts',(-8.89134865964033,15.2,-6.20206986025183));
#279024=CARTESIAN_POINT('Ctrl Pts',(-8.89358263437363,15.2,-6.20498158946769));
#279025=CARTESIAN_POINT('Ctrl Pts',(-8.89581660880255,15.2,-6.20789331828683));
#279026=CARTESIAN_POINT('Ctrl Pts',(-8.898055043405,15.2,-6.21082098300581));
#279027=CARTESIAN_POINT('Ctrl Pts',(-8.90029779723184,15.2,-6.21376454572295));
#279028=CARTESIAN_POINT('Ctrl Pts',(-8.90254055136426,15.2,-6.21670810884115));
#279029=CARTESIAN_POINT('Ctrl Pts',(-8.90478762671167,15.2,-6.21966757138653));
#279030=CARTESIAN_POINT('Ctrl Pts',(-8.90703888283479,15.2,-6.22264289649476));
#279031=CARTESIAN_POINT('Ctrl Pts',(-8.90985295283532,15.2,-6.22636205267735));
#279032=CARTESIAN_POINT('Ctrl Pts',(-8.91267355956372,15.2,-6.23010599364642));
#279033=CARTESIAN_POINT('Ctrl Pts',(-8.91550043282813,15.2,-6.23387465225957));
#279034=CARTESIAN_POINT('Ctrl Pts',(-8.91776193125479,15.2,-6.23688957890362));
#279035=CARTESIAN_POINT('Ctrl Pts',(-8.92002744089597,15.2,-6.23992032246372));
#279036=CARTESIAN_POINT('Ctrl Pts',(-8.9222968284985,15.2,-6.24296684850622));
#279037=CARTESIAN_POINT('Ctrl Pts',(-8.92456621641023,15.2,-6.24601337496379));
#279038=CARTESIAN_POINT('Ctrl Pts',(-8.92683947885619,15.2,-6.24907568269497));
#279039=CARTESIAN_POINT('Ctrl Pts',(-8.929116486814,15.2,-6.25215373775323));
#279040=CARTESIAN_POINT('Ctrl Pts',(-8.93196274660615,15.2,-6.25600130636636));
#279041=CARTESIAN_POINT('Ctrl Pts',(-8.9348148543845,15.2,-6.25987347703545));
#279042=CARTESIAN_POINT('Ctrl Pts',(-8.93767255431549,15.2,-6.26377018071798));
#279043=CARTESIAN_POINT('Ctrl Pts',(-8.93995871407339,15.2,-6.26688754340916));
#279044=CARTESIAN_POINT('Ctrl Pts',(-8.94224845249498,15.2,-6.27002060719097));
#279045=CARTESIAN_POINT('Ctrl Pts',(-8.94454163904014,15.2,-6.27316933528114));
#279046=CARTESIAN_POINT('Ctrl Pts',(-8.94683482589775,15.2,-6.27631806380033));
#279047=CARTESIAN_POINT('Ctrl Pts',(-8.94913146166429,15.2,-6.27948245697554));
#279048=CARTESIAN_POINT('Ctrl Pts',(-8.95143141640109,15.2,-6.28266247876156));
#279049=CARTESIAN_POINT('Ctrl Pts',(-8.95373137082452,15.2,-6.28584250011431));
#279050=CARTESIAN_POINT('Ctrl Pts',(-8.9560346433614,15.2,-6.28903815024836));
#279051=CARTESIAN_POINT('Ctrl Pts',(-8.95834110906152,15.2,-6.29224939226258));
#279052=CARTESIAN_POINT('Ctrl Pts',(-8.96064757507589,15.2,-6.29546063471434));
#279053=CARTESIAN_POINT('Ctrl Pts',(-8.96295723229657,15.2,-6.29868746839159));
#279054=CARTESIAN_POINT('Ctrl Pts',(-8.96526995459398,15.2,-6.30192985895386));
#279055=CARTESIAN_POINT('Ctrl Pts',(-8.96758267657627,15.2,-6.30517224907435));
#279056=CARTESIAN_POINT('Ctrl Pts',(-8.96989846369191,15.2,-6.30843019532333));
#279057=CARTESIAN_POINT('Ctrl Pts',(-8.97221719033552,15.2,-6.31170365949917));
#279058=CARTESIAN_POINT('Ctrl Pts',(-8.97453591729504,15.2,-6.31497712412101));
#279059=CARTESIAN_POINT('Ctrl Pts',(-8.97685758585211,15.2,-6.31826610919745));
#279060=CARTESIAN_POINT('Ctrl Pts',(-8.97918206875676,15.2,-6.32157057754524));
#279061=CARTESIAN_POINT('Ctrl Pts',(-8.98208767222923,15.2,-6.32570116275486));
#279062=CARTESIAN_POINT('Ctrl Pts',(-8.98499767754044,15.2,-6.3298559384388));
#279063=CARTESIAN_POINT('Ctrl Pts',(-8.98791184191566,15.2,-6.3340348355234));
#279064=CARTESIAN_POINT('Ctrl Pts',(-8.99024317322525,15.2,-6.33737795291779));
#279065=CARTESIAN_POINT('Ctrl Pts',(-8.99257716749385,15.2,-6.34073650793572));
#279066=CARTESIAN_POINT('Ctrl Pts',(-8.99491370291935,15.2,-6.34411046349379));
#279067=CARTESIAN_POINT('Ctrl Pts',(-8.9972502386632,15.2,-6.34748441951156));
#279068=CARTESIAN_POINT('Ctrl Pts',(-8.99958931723872,15.2,-6.35087377702523));
#279069=CARTESIAN_POINT('Ctrl Pts',(-9.00193081619982,15.2,-6.3542784975451));
#279070=CARTESIAN_POINT('Ctrl Pts',(-9.00427231484188,15.2,-6.35768321760108));
#279071=CARTESIAN_POINT('Ctrl Pts',(-9.0066162363529,15.2,-6.36110330248731));
#279072=CARTESIAN_POINT('Ctrl Pts',(-9.00896245838311,15.2,-6.3645387138716));
#279073=CARTESIAN_POINT('Ctrl Pts',(-9.01130868073298,15.2,-6.36797412572396));
#279074=CARTESIAN_POINT('Ctrl Pts',(-9.01365720745451,15.2,-6.3714248660115));
#279075=CARTESIAN_POINT('Ctrl Pts',(-9.01600791775998,15.2,-6.37489089649399));
#279076=CARTESIAN_POINT('Ctrl Pts',(-9.01894630548169,15.2,-6.37922343436098));
#279077=CARTESIAN_POINT('Ctrl Pts',(-9.02188810778695,15.2,-6.38357986379644));
#279078=CARTESIAN_POINT('Ctrl Pts',(-9.024833095426,15.2,-6.38796011331156));
#279079=CARTESIAN_POINT('Ctrl Pts',(-9.02718908534464,15.2,-6.3914643126372));
#279080=CARTESIAN_POINT('Ctrl Pts',(-9.02954711368232,15.2,-6.39498375569034));
#279081=CARTESIAN_POINT('Ctrl Pts',(-9.03190706632253,15.2,-6.39851840762205));
#279082=CARTESIAN_POINT('Ctrl Pts',(-9.03426701928429,15.2,-6.40205306003535));
#279083=CARTESIAN_POINT('Ctrl Pts',(-9.03662889621487,15.2,-6.40560292010574));
#279084=CARTESIAN_POINT('Ctrl Pts',(-9.03899258307666,15.2,-6.40916795126072));
#279085=CARTESIAN_POINT('Ctrl Pts',(-9.0413562696164,15.2,-6.41273298192997));
#279086=CARTESIAN_POINT('Ctrl Pts',(-9.04372176464837,15.2,-6.41631318334646));
#279087=CARTESIAN_POINT('Ctrl Pts',(-9.04608895662135,15.2,-6.41990851916213));
#279088=CARTESIAN_POINT('Ctrl Pts',(-9.04845614891687,15.2,-6.42350385546766));
#279089=CARTESIAN_POINT('Ctrl Pts',(-9.05082503831251,15.2,-6.42711432488845));
#279090=CARTESIAN_POINT('Ctrl Pts',(-9.05319551127505,15.2,-6.43073989147495));
#279091=CARTESIAN_POINT('Ctrl Pts',(-9.05556598423759,15.2,-6.43436545806145));
#279092=CARTESIAN_POINT('Ctrl Pts',(-9.05793804126972,15.2,-6.43800612276077));
#279093=CARTESIAN_POINT('Ctrl Pts',(-9.06031157162145,15.2,-6.44166184657267));
#279094=CARTESIAN_POINT('Ctrl Pts',(-9.0626851016498,15.2,-6.44531756988648));
#279095=CARTESIAN_POINT('Ctrl Pts',(-9.06506010570969,15.2,-6.44898835265985));
#279096=CARTESIAN_POINT('Ctrl Pts',(-9.06743647174844,15.2,-6.45267415926412));
#279097=CARTESIAN_POINT('Ctrl Pts',(-9.06981283811096,15.2,-6.45635996637058));
#279098=CARTESIAN_POINT('Ctrl Pts',(-9.0721905676009,15.2,-6.46006079468401));
#279099=CARTESIAN_POINT('Ctrl Pts',(-9.07456955189735,15.2,-6.4637766098325));
#279100=CARTESIAN_POINT('Ctrl Pts',(-9.07694853586966,15.2,-6.46749242447471));
#279101=CARTESIAN_POINT('Ctrl Pts',(-9.07932877337237,15.2,-6.47122322472885));
#279102=CARTESIAN_POINT('Ctrl Pts',(-9.08171015728871,15.2,-6.47496897397721));
#279103=CARTESIAN_POINT('Ctrl Pts',(-9.0834961953071,15.2,-6.47777828604108));
#279104=CARTESIAN_POINT('Ctrl Pts',(-9.08528287729666,15.2,-6.48059600691573));
#279105=CARTESIAN_POINT('Ctrl Pts',(-9.0870701589876,15.2,-6.48342212020326));
#279106=CARTESIAN_POINT('Ctrl Pts',(-9.08885744067855,15.2,-6.4862482334908));
#279107=CARTESIAN_POINT('Ctrl Pts',(-9.09064532242522,15.2,-6.4890827392013));
#279108=CARTESIAN_POINT('Ctrl Pts',(-9.09243375765184,15.2,-6.49192562184689));
#279109=CARTESIAN_POINT('Ctrl Pts',(-9.09422219320335,15.2,-6.49476850500892));
#279110=CARTESIAN_POINT('Ctrl Pts',(-9.09601118414669,15.2,-6.49761976600662));
#279111=CARTESIAN_POINT('Ctrl Pts',(-9.09780068415683,15.2,-6.50047938813169));
#279112=CARTESIAN_POINT('Ctrl Pts',(-9.09959018384188,15.2,-6.50333900973727));
#279113=CARTESIAN_POINT('Ctrl Pts',(-9.1013801930769,15.2,-6.50620699290073));
#279114=CARTESIAN_POINT('Ctrl Pts',(-9.10317066813689,15.2,-6.50908332108862));
#279115=CARTESIAN_POINT('Ctrl Pts',(-9.10496114319688,15.2,-6.51195964927651));
#279116=CARTESIAN_POINT('Ctrl Pts',(-9.1067520827753,15.2,-6.51484432377786));
#279117=CARTESIAN_POINT('Ctrl Pts',(-9.10854344526001,15.2,-6.51773732747758));
#279118=CARTESIAN_POINT('Ctrl Pts',(-9.11093192846448,15.2,-6.52159466556869));
#279119=CARTESIAN_POINT('Ctrl Pts',(-9.11332115958528,15.2,-6.5254668126087));
#279120=CARTESIAN_POINT('Ctrl Pts',(-9.11571103633431,15.2,-6.52935373112279));
#279121=CARTESIAN_POINT('Ctrl Pts',(-9.11750344430311,15.2,-6.53226892067035));
#279122=CARTESIAN_POINT('Ctrl Pts',(-9.11929621564698,15.2,-6.53519241856187));
#279123=CARTESIAN_POINT('Ctrl Pts',(-9.12108930665761,15.2,-6.53812420965575));
#279124=CARTESIAN_POINT('Ctrl Pts',(-9.12288239734251,15.2,-6.54105600021703));
#279125=CARTESIAN_POINT('Ctrl Pts',(-9.12467580924405,15.2,-6.54399608354453));
#279126=CARTESIAN_POINT('Ctrl Pts',(-9.12646949597057,15.2,-6.5469444446048));
#279127=CARTESIAN_POINT('Ctrl Pts',(-9.12826318269709,15.2,-6.54989280566507));
#279128=CARTESIAN_POINT('Ctrl Pts',(-9.13005714644206,15.2,-6.55284944326355));
#279129=CARTESIAN_POINT('Ctrl Pts',(-9.13185134455168,15.2,-6.55581434200265));
#279130=CARTESIAN_POINT('Ctrl Pts',(-9.13364554266131,15.2,-6.55877924074175));
#279131=CARTESIAN_POINT('Ctrl Pts',(-9.13543997387214,15.2,-6.5617524027254));
#279132=CARTESIAN_POINT('Ctrl Pts',(-9.13723459698176,15.2,-6.56473380846392));
#279133=CARTESIAN_POINT('Ctrl Pts',(-9.13902922009137,15.2,-6.56771521420243));
#279134=CARTESIAN_POINT('Ctrl Pts',(-9.14082403420296,15.2,-6.57070486649963));
#279135=CARTESIAN_POINT('Ctrl Pts',(-9.14261899734608,15.2,-6.57370274718166));
#279136=CARTESIAN_POINT('Ctrl Pts',(-9.14441396048919,15.2,-6.5767006278637));
#279137=CARTESIAN_POINT('Ctrl Pts',(-9.14620907240727,15.2,-6.57970673897014));
#279138=CARTESIAN_POINT('Ctrl Pts',(-9.14800429159204,15.2,-6.58272106310952));
#279139=CARTESIAN_POINT('Ctrl Pts',(-9.14979951110294,15.2,-6.5857353877965));
#279140=CARTESIAN_POINT('Ctrl Pts',(-9.15159483843051,15.2,-6.58875792658575));
#279141=CARTESIAN_POINT('Ctrl Pts',(-9.15339023094145,15.2,-6.591788663694));
#279142=CARTESIAN_POINT('Ctrl Pts',(-9.15518562312623,15.2,-6.59481940025167));
#279143=CARTESIAN_POINT('Ctrl Pts',(-9.1569810810563,15.2,-6.59785833376379));
#279144=CARTESIAN_POINT('Ctrl Pts',(-9.15877656233077,15.2,-6.60090544955625));
#279145=CARTESIAN_POINT('Ctrl Pts',(-9.16057204360524,15.2,-6.60395256534871));
#279146=CARTESIAN_POINT('Ctrl Pts',(-9.16236754756099,15.2,-6.60700786346127));
#279147=CARTESIAN_POINT('Ctrl Pts',(-9.16416303566243,15.2,-6.61007132755902));
#279148=CARTESIAN_POINT('Ctrl Pts',(-9.16595852376386,15.2,-6.61313479165675));
#279149=CARTESIAN_POINT('Ctrl Pts',(-9.16775399481528,15.2,-6.61620642219517));
#279150=CARTESIAN_POINT('Ctrl Pts',(-9.16954940704173,15.2,-6.61928620224996));
#279151=CARTESIAN_POINT('Ctrl Pts',(-9.17194329022776,15.2,-6.62339257602934));
#279152=CARTESIAN_POINT('Ctrl Pts',(-9.1743370700721,15.2,-6.62751343742149));
#279153=CARTESIAN_POINT('Ctrl Pts',(-9.1767306510914,15.2,-6.63164875242608));
#279154=CARTESIAN_POINT('Ctrl Pts',(-9.17852583669283,15.2,-6.63475023839782));
#279155=CARTESIAN_POINT('Ctrl Pts',(-9.18032090972761,15.2,-6.63785985188584));
#279156=CARTESIAN_POINT('Ctrl Pts',(-9.1821158294957,15.2,-6.64097757935659));
#279157=CARTESIAN_POINT('Ctrl Pts',(-9.1839107492638,15.2,-6.64409530682733));
#279158=CARTESIAN_POINT('Ctrl Pts',(-9.18570551742541,15.2,-6.6472211457024));
#279159=CARTESIAN_POINT('Ctrl Pts',(-9.18750009220169,15.2,-6.65035508272781));
#279160=CARTESIAN_POINT('Ctrl Pts',(-9.18929466697797,15.2,-6.65348901975321));
#279161=CARTESIAN_POINT('Ctrl Pts',(-9.19108904920546,15.2,-6.65663105373061));
#279162=CARTESIAN_POINT('Ctrl Pts',(-9.19288319848176,15.2,-6.65978116875544));
#279163=CARTESIAN_POINT('Ctrl Pts',(-9.19587344738425,15.2,-6.66503136065424));
#279164=CARTESIAN_POINT('Ctrl Pts',(-9.19886305158896,15.2,-6.67030399831107));
#279165=CARTESIAN_POINT('Ctrl Pts',(-9.20185182624172,15.2,-6.67559900949162));
#279166=CARTESIAN_POINT('Ctrl Pts',(-9.20424284609425,15.2,-6.67983501866692));
#279167=CARTESIAN_POINT('Ctrl Pts',(-9.20663333593562,15.2,-6.6840853469439));
#279168=CARTESIAN_POINT('Ctrl Pts',(-9.20902320189913,15.2,-6.68834995545556));
#279169=CARTESIAN_POINT('Ctrl Pts',(-9.21081560120895,15.2,-6.69154841154878));
#279170=CARTESIAN_POINT('Ctrl Pts',(-9.21260765075567,15.2,-6.69475490061058));
#279171=CARTESIAN_POINT('Ctrl Pts',(-9.2143993105717,15.2,-6.69796940686363));
#279172=CARTESIAN_POINT('Ctrl Pts',(-9.21619097038772,15.2,-6.70118391311667));
#279173=CARTESIAN_POINT('Ctrl Pts',(-9.21798224052702,15.2,-6.70440643593556));
#279174=CARTESIAN_POINT('Ctrl Pts',(-9.21977308271192,15.2,-6.70763695906889));
#279175=CARTESIAN_POINT('Ctrl Pts',(-9.22156392489683,15.2,-6.71086748220223));
#279176=CARTESIAN_POINT('Ctrl Pts',(-9.22335433901509,15.2,-6.71410600670124));
#279177=CARTESIAN_POINT('Ctrl Pts',(-9.22514428682506,15.2,-6.71735251574996));
#279178=CARTESIAN_POINT('Ctrl Pts',(-9.22753088412179,15.2,-6.72168119487477));
#279179=CARTESIAN_POINT('Ctrl Pts',(-9.22991665462957,15.2,-6.72602406893459));
#279180=CARTESIAN_POINT('Ctrl Pts',(-9.23230150514831,15.2,-6.730381100729));
#279181=CARTESIAN_POINT('Ctrl Pts',(-9.23468635534212,15.2,-6.73473813192977));
#279182=CARTESIAN_POINT('Ctrl Pts',(-9.23707028615185,15.2,-6.73910931940226));
#279183=CARTESIAN_POINT('Ctrl Pts',(-9.23945320502344,15.2,-6.74349462473031));
#279184=CARTESIAN_POINT('Ctrl Pts',(-9.24124039425829,15.2,-6.74678360387572));
#279185=CARTESIAN_POINT('Ctrl Pts',(-9.24302701403688,15.2,-6.75008052466064));
#279186=CARTESIAN_POINT('Ctrl Pts',(-9.24481303130537,15.2,-6.7533853708732));
#279187=CARTESIAN_POINT('Ctrl Pts',(-9.24659904857387,15.2,-6.75669021708576));
#279188=CARTESIAN_POINT('Ctrl Pts',(-9.24838446267574,15.2,-6.76000299138112));
#279189=CARTESIAN_POINT('Ctrl Pts',(-9.25016923831931,15.2,-6.76332367555106));
#279190=CARTESIAN_POINT('Ctrl Pts',(-9.25195401428712,15.2,-6.76664436032426));
#279191=CARTESIAN_POINT('Ctrl Pts',(-9.25373815124641,15.2,-6.76997295699134));
#279192=CARTESIAN_POINT('Ctrl Pts',(-9.25552160417219,15.2,-6.77330944418565));
#279193=CARTESIAN_POINT('Ctrl Pts',(-9.25730505677395,15.2,-6.77664593077383));
#279194=CARTESIAN_POINT('Ctrl Pts',(-9.25908782435398,15.2,-6.77999030870202));
#279195=CARTESIAN_POINT('Ctrl Pts',(-9.2608698668365,15.2,-6.78334256091528));
#279196=CARTESIAN_POINT('Ctrl Pts',(-9.26265190931903,15.2,-6.78669481312853));
#279197=CARTESIAN_POINT('Ctrl Pts',(-9.26443322619546,15.2,-6.7900549376617));
#279198=CARTESIAN_POINT('Ctrl Pts',(-9.26621380150165,15.2,-6.79342292836566));
#279199=CARTESIAN_POINT('Ctrl Pts',(-9.26799437680784,15.2,-6.79679091906962));
#279200=CARTESIAN_POINT('Ctrl Pts',(-9.26977421267685,15.2,-6.80016677138531));
#279201=CARTESIAN_POINT('Ctrl Pts',(-9.27155330300005,15.2,-6.80355049700001));
#279202=CARTESIAN_POINT('Ctrl Pts',(-8.56667971000006,12.2,-5.85257411400002));
#279203=CARTESIAN_POINT('Ctrl Pts',(-8.56806288384934,12.2,-5.85370503502559));
#279204=CARTESIAN_POINT('Ctrl Pts',(-8.56948692484017,12.2,-5.85487627493062));
#279205=CARTESIAN_POINT('Ctrl Pts',(-8.57095065283135,12.2,-5.85608775313393));
#279206=CARTESIAN_POINT('Ctrl Pts',(-8.57242143965877,12.2,-5.85730507369751));
#279207=CARTESIAN_POINT('Ctrl Pts',(-8.57393230452754,12.2,-5.85856301222101));
#279208=CARTESIAN_POINT('Ctrl Pts',(-8.57548210844168,12.2,-5.85986145285899));
#279209=CARTESIAN_POINT('Ctrl Pts',(-8.57703191221504,12.2,-5.86115989337901));
#279210=CARTESIAN_POINT('Ctrl Pts',(-8.57862065441741,12.2,-5.86249883667505));
#279211=CARTESIAN_POINT('Ctrl Pts',(-8.58024722827499,12.2,-5.86387816920827));
#279212=CARTESIAN_POINT('Ctrl Pts',(-8.58187380213257,12.2,-5.8652575017415));
#279213=CARTESIAN_POINT('Ctrl Pts',(-8.58353820868947,12.2,-5.86667722288291));
#279214=CARTESIAN_POINT('Ctrl Pts',(-8.58523937179385,12.2,-5.86813722031714));
#279215=CARTESIAN_POINT('Ctrl Pts',(-8.58694053505276,12.2,-5.86959721788399));
#279216=CARTESIAN_POINT('Ctrl Pts',(-8.58867845668591,12.2,-5.87109749028118));
#279217=CARTESIAN_POINT('Ctrl Pts',(-8.59045208820166,12.2,-5.87263792486786));
#279218=CARTESIAN_POINT('Ctrl Pts',(-8.59222571955631,12.2,-5.87417835931461));
#279219=CARTESIAN_POINT('Ctrl Pts',(-8.59403506469271,12.2,-5.87575895551878));
#279220=CARTESIAN_POINT('Ctrl Pts',(-8.5958791059675,12.2,-5.87737960096735));
#279221=CARTESIAN_POINT('Ctrl Pts',(-8.59772314724229,12.2,-5.87900024641592));
#279222=CARTESIAN_POINT('Ctrl Pts',(-8.59960188407517,12.2,-5.88066094137928));
#279223=CARTESIAN_POINT('Ctrl Pts',(-8.60151432942091,12.2,-5.8823615708991));
#279224=CARTESIAN_POINT('Ctrl Pts',(-8.60342677494035,12.2,-5.88406220057339));
#279225=CARTESIAN_POINT('Ctrl Pts',(-8.60537292788893,12.2,-5.88580276593591));
#279226=CARTESIAN_POINT('Ctrl Pts',(-8.60735182649905,12.2,-5.88758315445236));
#279227=CARTESIAN_POINT('Ctrl Pts',(-8.6093307249294,12.2,-5.88936354280707));
#279228=CARTESIAN_POINT('Ctrl Pts',(-8.61134236849269,12.2,-5.89118375430898));
#279229=CARTESIAN_POINT('Ctrl Pts',(-8.61338582016984,12.2,-5.89304367482648));
#279230=CARTESIAN_POINT('Ctrl Pts',(-8.615429271847,12.2,-5.89490359534398));
#279231=CARTESIAN_POINT('Ctrl Pts',(-8.61750453139654,12.2,-5.89680322461661));
#279232=CARTESIAN_POINT('Ctrl Pts',(-8.61961068615201,12.2,-5.89874245187776));
#279233=CARTESIAN_POINT('Ctrl Pts',(-8.62171684090748,12.2,-5.90068167913891));
#279234=CARTESIAN_POINT('Ctrl Pts',(-8.62385388904457,12.2,-5.90266050258931));
#279235=CARTESIAN_POINT('Ctrl Pts',(-8.62602094279714,12.2,-5.9046788090133));
#279236=CARTESIAN_POINT('Ctrl Pts',(-8.62818799674654,12.2,-5.90669711562061));
#279237=CARTESIAN_POINT('Ctrl Pts',(-8.63038505409052,12.2,-5.90875490690673));
#279238=CARTESIAN_POINT('Ctrl Pts',(-8.63261124812979,12.2,-5.91085206660607));
#279239=CARTESIAN_POINT('Ctrl Pts',(-8.63483744196683,12.2,-5.91294922611493));
#279240=CARTESIAN_POINT('Ctrl Pts',(-8.63709277010497,12.2,-5.91508575739323));
#279241=CARTESIAN_POINT('Ctrl Pts',(-8.63937638719896,12.2,-5.91726154574061));
#279242=CARTESIAN_POINT('Ctrl Pts',(-8.64166000429295,12.2,-5.919437334088));
#279243=CARTESIAN_POINT('Ctrl Pts',(-8.64397191091524,12.2,-5.9216523775805));
#279244=CARTESIAN_POINT('Ctrl Pts',(-8.64631127799502,12.2,-5.92390656674592));
#279245=CARTESIAN_POINT('Ctrl Pts',(-8.6486506452873,12.2,-5.92616075611608));
#279246=CARTESIAN_POINT('Ctrl Pts',(-8.65101747287396,12.2,-5.92845408682341));
#279247=CARTESIAN_POINT('Ctrl Pts',(-8.65341095442223,12.2,-5.93078644936889));
#279248=CARTESIAN_POINT('Ctrl Pts',(-8.6558044357531,12.2,-5.93311881170251));
#279249=CARTESIAN_POINT('Ctrl Pts',(-8.65822457123506,12.2,-5.93549020269223));
#279250=CARTESIAN_POINT('Ctrl Pts',(-8.66067056874055,12.2,-5.93790051194884));
#279251=CARTESIAN_POINT('Ctrl Pts',(-8.66311656624606,12.2,-5.94031082120544));
#279252=CARTESIAN_POINT('Ctrl Pts',(-8.66558843005363,12.2,-5.94276004585516));
#279253=CARTESIAN_POINT('Ctrl Pts',(-8.66808538546118,12.2,-5.94524807326209));
#279254=CARTESIAN_POINT('Ctrl Pts',(-8.67058234109555,12.2,-5.94773610089504));
#279255=CARTESIAN_POINT('Ctrl Pts',(-8.67310438880401,12.2,-5.95026293009466));
#279256=CARTESIAN_POINT('Ctrl Pts',(-8.67565077648806,12.2,-5.95282844969821));
#279257=CARTESIAN_POINT('Ctrl Pts',(-8.67819716394083,12.2,-5.95539396906874));
#279258=CARTESIAN_POINT('Ctrl Pts',(-8.68076788847761,12.2,-5.95799817577096));
#279259=CARTESIAN_POINT('Ctrl Pts',(-8.68336221571668,12.2,-5.96064095625827));
#279260=CARTESIAN_POINT('Ctrl Pts',(-8.68595654295576,12.2,-5.96328373674558));
#279261=CARTESIAN_POINT('Ctrl Pts',(-8.68857446975996,12.2,-5.96596509348544));
#279262=CARTESIAN_POINT('Ctrl Pts',(-8.69121527746127,12.2,-5.96868490802027));
#279263=CARTESIAN_POINT('Ctrl Pts',(-8.69385608540248,12.2,-5.97140472280214));
#279264=CARTESIAN_POINT('Ctrl Pts',(-8.69651977346155,12.2,-5.97416299852475));
#279265=CARTESIAN_POINT('Ctrl Pts',(-8.69920563427613,12.2,-5.97695961826314));
#279266=CARTESIAN_POINT('Ctrl Pts',(-8.70189149484674,12.2,-5.9797562377475));
#279267=CARTESIAN_POINT('Ctrl Pts',(-8.70459952848798,12.2,-5.98259120266751));
#279268=CARTESIAN_POINT('Ctrl Pts',(-8.70732904423459,12.2,-5.98546439799293));
#279269=CARTESIAN_POINT('Ctrl Pts',(-8.71005855998121,12.2,-5.98833759331834));
#279270=CARTESIAN_POINT('Ctrl Pts',(-8.712809559009,12.2,-5.99124901789818));
#279271=CARTESIAN_POINT('Ctrl Pts',(-8.71558136182404,12.2,-5.99419855728936));
#279272=CARTESIAN_POINT('Ctrl Pts',(-8.71789119758718,12.2,-5.99665650687131));
#279273=CARTESIAN_POINT('Ctrl Pts',(-8.72021548140903,12.2,-5.99914092571506));
#279274=CARTESIAN_POINT('Ctrl Pts',(-8.72255382883885,12.2,-6.0016517460609));
#279275=CARTESIAN_POINT('Ctrl Pts',(-8.72489217626867,12.2,-6.00416256640674));
#279276=CARTESIAN_POINT('Ctrl Pts',(-8.72724458758245,12.2,-6.00669978913697));
#279277=CARTESIAN_POINT('Ctrl Pts',(-8.72961068502373,12.2,-6.00926334623188));
#279278=CARTESIAN_POINT('Ctrl Pts',(-8.731976782465,12.2,-6.0118269033268));
#279279=CARTESIAN_POINT('Ctrl Pts',(-8.73435656410001,12.2,-6.0144167953555));
#279280=CARTESIAN_POINT('Ctrl Pts',(-8.73674966076669,12.2,-6.01703295500828));
#279281=CARTESIAN_POINT('Ctrl Pts',(-8.73914275743336,12.2,-6.01964911466105));
#279282=CARTESIAN_POINT('Ctrl Pts',(-8.74154916827364,12.2,-6.02229154210031));
#279283=CARTESIAN_POINT('Ctrl Pts',(-8.74396852599302,12.2,-6.02496017079308));
#279284=CARTESIAN_POINT('Ctrl Pts',(-8.74638788371239,12.2,-6.02762879948585));
#279285=CARTESIAN_POINT('Ctrl Pts',(-8.74882019127601,12.2,-6.0303236283378));
#279286=CARTESIAN_POINT('Ctrl Pts',(-8.75126508565167,12.2,-6.0330445911864));
#279287=CARTESIAN_POINT('Ctrl Pts',(-8.75370998002734,12.2,-6.03576555403501));
#279288=CARTESIAN_POINT('Ctrl Pts',(-8.75616746439987,12.2,-6.038512650419));
#279289=CARTESIAN_POINT('Ctrl Pts',(-8.75863718217829,12.2,-6.04128581173981));
#279290=CARTESIAN_POINT('Ctrl Pts',(-8.7611068999567,12.2,-6.0440589730606));
#279291=CARTESIAN_POINT('Ctrl Pts',(-8.76358885294193,12.2,-6.04685820099616));
#279292=CARTESIAN_POINT('Ctrl Pts',(-8.76608269153956,12.2,-6.04968342731967));
#279293=CARTESIAN_POINT('Ctrl Pts',(-8.76857653013719,12.2,-6.05250865364318));
#279294=CARTESIAN_POINT('Ctrl Pts',(-8.77108225506726,12.2,-6.05535987786309));
#279295=CARTESIAN_POINT('Ctrl Pts',(-8.77359952284596,12.2,-6.05823703314296));
#279296=CARTESIAN_POINT('Ctrl Pts',(-8.77611679062466,12.2,-6.06111418842282));
#279297=CARTESIAN_POINT('Ctrl Pts',(-8.77864560165358,12.2,-6.06401727391984));
#279298=CARTESIAN_POINT('Ctrl Pts',(-8.78118561859893,12.2,-6.06694622190807));
#279299=CARTESIAN_POINT('Ctrl Pts',(-8.78372563526744,12.2,-6.06987516957704));
#279300=CARTESIAN_POINT('Ctrl Pts',(-8.78627685702285,12.2,-6.07282997980376));
#279301=CARTESIAN_POINT('Ctrl Pts',(-8.78883895271491,12.2,-6.07581058635177));
#279302=CARTESIAN_POINT('Ctrl Pts',(-8.79140104868625,12.2,-6.07879119322467));
#279303=CARTESIAN_POINT('Ctrl Pts',(-8.79397401767406,12.2,-6.08179759316655));
#279304=CARTESIAN_POINT('Ctrl Pts',(-8.79655753218712,12.2,-6.08482971955336));
#279305=CARTESIAN_POINT('Ctrl Pts',(-8.79914104670016,12.2,-6.08786184594017));
#279306=CARTESIAN_POINT('Ctrl Pts',(-8.80173510762689,12.2,-6.09091970129317));
#279307=CARTESIAN_POINT('Ctrl Pts',(-8.80433939137607,12.2,-6.09400321330498));
#279308=CARTESIAN_POINT('Ctrl Pts',(-8.80694367512525,12.2,-6.09708672531679));
#279309=CARTESIAN_POINT('Ctrl Pts',(-8.80955818265387,12.2,-6.1001958954091));
#279310=CARTESIAN_POINT('Ctrl Pts',(-8.81218259639541,12.2,-6.10333065591114));
#279311=CARTESIAN_POINT('Ctrl Pts',(-8.81480701013694,12.2,-6.10646541641319));
#279312=CARTESIAN_POINT('Ctrl Pts',(-8.81744132993878,12.2,-6.10962576694863));
#279313=CARTESIAN_POINT('Ctrl Pts',(-8.82008524132718,12.2,-6.11281163826675));
#279314=CARTESIAN_POINT('Ctrl Pts',(-8.82272915271557,12.2,-6.11599750958487));
#279315=CARTESIAN_POINT('Ctrl Pts',(-8.82538265717086,12.2,-6.11920890262307));
#279316=CARTESIAN_POINT('Ctrl Pts',(-8.82804544605928,12.2,-6.12244574803842));
#279317=CARTESIAN_POINT('Ctrl Pts',(-8.8301756772861,12.2,-6.12503522451181));
#279318=CARTESIAN_POINT('Ctrl Pts',(-8.83231185130607,12.2,-6.12764099158576));
#279319=CARTESIAN_POINT('Ctrl Pts',(-8.83445381058588,12.2,-6.13026301213885));
#279320=CARTESIAN_POINT('Ctrl Pts',(-8.83659576957385,12.2,-6.13288503233469));
#279321=CARTESIAN_POINT('Ctrl Pts',(-8.83874351450323,12.2,-6.13552330721506));
#279322=CARTESIAN_POINT('Ctrl Pts',(-8.84089689204905,12.2,-6.13817780127477));
#279323=CARTESIAN_POINT('Ctrl Pts',(-8.84305026988826,12.2,-6.14083229569616));
#279324=CARTESIAN_POINT('Ctrl Pts',(-8.84520928007816,12.2,-6.14350300849172));
#279325=CARTESIAN_POINT('Ctrl Pts',(-8.8473737699187,12.2,-6.14618990569475));
#279326=CARTESIAN_POINT('Ctrl Pts',(-8.84953825946433,12.2,-6.14887680253171));
#279327=CARTESIAN_POINT('Ctrl Pts',(-8.85170822732348,12.2,-6.15157988369332));
#279328=CARTESIAN_POINT('Ctrl Pts',(-8.85388352564275,12.2,-6.15429911260547));
#279329=CARTESIAN_POINT('Ctrl Pts',(-8.8560588242584,12.2,-6.15701834188811));
#279330=CARTESIAN_POINT('Ctrl Pts',(-8.85823945179819,12.2,-6.15975372025736));
#279331=CARTESIAN_POINT('Ctrl Pts',(-8.86042525969545,12.2,-6.16250521074171));
#279332=CARTESIAN_POINT('Ctrl Pts',(-8.8631575194181,12.2,-6.1659445736597));
#279333=CARTESIAN_POINT('Ctrl Pts',(-8.8658978728794,12.2,-6.16940911354923));
#279334=CARTESIAN_POINT('Ctrl Pts',(-8.86864603267148,12.2,-6.172898760495));
#279335=CARTESIAN_POINT('Ctrl Pts',(-8.87084456032542,12.2,-6.17569047782338));
#279336=CARTESIAN_POINT('Ctrl Pts',(-8.87304808434192,12.2,-6.17849826257591));
#279337=CARTESIAN_POINT('Ctrl Pts',(-8.87525645943795,12.2,-6.18132208137362));
#279338=CARTESIAN_POINT('Ctrl Pts',(-8.87746483483486,12.2,-6.18414590055607));
#279339=CARTESIAN_POINT('Ctrl Pts',(-8.87967806187132,12.2,-6.18698575165742));
#279340=CARTESIAN_POINT('Ctrl Pts',(-8.88189599521473,12.2,-6.18984160075857));
#279341=CARTESIAN_POINT('Ctrl Pts',(-8.88411392825596,12.2,-6.19269744947061));
#279342=CARTESIAN_POINT('Ctrl Pts',(-8.88633656964897,12.2,-6.19556929464607));
#279343=CARTESIAN_POINT('Ctrl Pts',(-8.8885637754109,12.2,-6.19845710201947));
#279344=CARTESIAN_POINT('Ctrl Pts',(-8.89079098147626,12.2,-6.20134490978636));
#279345=CARTESIAN_POINT('Ctrl Pts',(-8.89302275296397,12.2,-6.20424867817396));
#279346=CARTESIAN_POINT('Ctrl Pts',(-8.8952589489849,12.2,-6.20716837323528));
#279347=CARTESIAN_POINT('Ctrl Pts',(-8.89749514470114,12.2,-6.21008806789879));
#279348=CARTESIAN_POINT('Ctrl Pts',(-8.89973576435583,12.2,-6.21302368800751));
#279349=CARTESIAN_POINT('Ctrl Pts',(-8.90198067061634,12.2,-6.2159751980424));
#279350=CARTESIAN_POINT('Ctrl Pts',(-8.9042255771827,12.2,-6.21892670847943));
#279351=CARTESIAN_POINT('Ctrl Pts',(-8.90647476709946,12.2,-6.22189410942071));
#279352=CARTESIAN_POINT('Ctrl Pts',(-8.90872810700003,12.2,-6.22487736324994));
#279353=CARTESIAN_POINT('Ctrl Pts',(-8.91098144690061,12.2,-6.22786061707918));
#279354=CARTESIAN_POINT('Ctrl Pts',(-8.91323893409335,12.2,-6.23085972520474));
#279355=CARTESIAN_POINT('Ctrl Pts',(-8.91550043282813,12.2,-6.23387465225957));
#279356=CARTESIAN_POINT('Ctrl Pts',(-8.91776193125479,12.2,-6.23688957890362));
#279357=CARTESIAN_POINT('Ctrl Pts',(-8.92002744089597,12.2,-6.23992032246372));
#279358=CARTESIAN_POINT('Ctrl Pts',(-8.9222968284985,12.2,-6.24296684850622));
#279359=CARTESIAN_POINT('Ctrl Pts',(-8.92456621641023,12.2,-6.2460133749638));
#279360=CARTESIAN_POINT('Ctrl Pts',(-8.92683947885618,12.2,-6.24907568269497));
#279361=CARTESIAN_POINT('Ctrl Pts',(-8.929116486814,12.2,-6.25215373775322));
#279362=CARTESIAN_POINT('Ctrl Pts',(-8.93139349446158,12.2,-6.2552317923921));
#279363=CARTESIAN_POINT('Ctrl Pts',(-8.93367424523641,12.2,-6.258325592265));
#279364=CARTESIAN_POINT('Ctrl Pts',(-8.935958607105,12.2,-6.26143510228757));
#279365=CARTESIAN_POINT('Ctrl Pts',(-8.93938515006349,12.2,-6.26609936753325));
#279366=CARTESIAN_POINT('Ctrl Pts',(-8.9428198185254,12.2,-6.27079898012494));
#279367=CARTESIAN_POINT('Ctrl Pts',(-8.94626217331649,12.2,-6.27553381745053));
#279368=CARTESIAN_POINT('Ctrl Pts',(-8.94855707671901,12.2,-6.27869037595431));
#279369=CARTESIAN_POINT('Ctrl Pts',(-8.95085539610796,12.2,-6.28186259047346));
#279370=CARTESIAN_POINT('Ctrl Pts',(-8.95315700223339,12.2,-6.28505042425829));
#279371=CARTESIAN_POINT('Ctrl Pts',(-8.95545860835881,12.2,-6.28823825804313));
#279372=CARTESIAN_POINT('Ctrl Pts',(-8.95776350188742,12.2,-6.29144171166591));
#279373=CARTESIAN_POINT('Ctrl Pts',(-8.96007155540241,12.2,-6.2946607475096));
#279374=CARTESIAN_POINT('Ctrl Pts',(-8.96237960860292,12.2,-6.2978797829147));
#279375=CARTESIAN_POINT('Ctrl Pts',(-8.9646908219466,12.2,-6.3011144018654));
#279376=CARTESIAN_POINT('Ctrl Pts',(-8.96700506849013,12.2,-6.30436456728108));
#279377=CARTESIAN_POINT('Ctrl Pts',(-8.96931931534898,12.2,-6.30761473313958));
#279378=CARTESIAN_POINT('Ctrl Pts',(-8.97163659549987,12.2,-6.31088044553658));
#279379=CARTESIAN_POINT('Ctrl Pts',(-8.97395678557107,12.2,-6.31416166799478));
#279380=CARTESIAN_POINT('Ctrl Pts',(-8.97627697532613,12.2,-6.3174428900059));
#279381=CARTESIAN_POINT('Ctrl Pts',(-8.97860007328637,12.2,-6.32073962412056));
#279382=CARTESIAN_POINT('Ctrl Pts',(-8.98092595648493,12.2,-6.32405183023766));
#279383=CARTESIAN_POINT('Ctrl Pts',(-8.98325184000039,12.2,-6.32736403680605));
#279384=CARTESIAN_POINT('Ctrl Pts',(-8.98558051028843,12.2,-6.33069171767352));
#279385=CARTESIAN_POINT('Ctrl Pts',(-8.98791184191566,12.2,-6.3340348355234));
#279386=CARTESIAN_POINT('Ctrl Pts',(-8.99024317322525,12.2,-6.33737795291779));
#279387=CARTESIAN_POINT('Ctrl Pts',(-8.99257716749385,12.2,-6.34073650793572));
#279388=CARTESIAN_POINT('Ctrl Pts',(-8.99491370291935,12.2,-6.34411046349379));
#279389=CARTESIAN_POINT('Ctrl Pts',(-8.9972502386632,12.2,-6.34748441951156));
#279390=CARTESIAN_POINT('Ctrl Pts',(-8.99958931723872,12.2,-6.35087377702523));
#279391=CARTESIAN_POINT('Ctrl Pts',(-9.00193081619982,12.2,-6.3542784975451));
#279392=CARTESIAN_POINT('Ctrl Pts',(-9.00427231484188,12.2,-6.35768321760108));
#279393=CARTESIAN_POINT('Ctrl Pts',(-9.0066162363529,12.2,-6.36110330248731));
#279394=CARTESIAN_POINT('Ctrl Pts',(-9.00896245838311,12.2,-6.3645387138716));
#279395=CARTESIAN_POINT('Ctrl Pts',(-9.01130868073298,12.2,-6.36797412572396));
#279396=CARTESIAN_POINT('Ctrl Pts',(-9.01365720745451,12.2,-6.3714248660115));
#279397=CARTESIAN_POINT('Ctrl Pts',(-9.01600791775998,12.2,-6.37489089649399));
#279398=CARTESIAN_POINT('Ctrl Pts',(-9.01835862774518,12.2,-6.37835692650424));
#279399=CARTESIAN_POINT('Ctrl Pts',(-9.02071152312996,12.2,-6.38183824699623));
#279400=CARTESIAN_POINT('Ctrl Pts',(-9.02306648638168,12.2,-6.38533482165327));
#279401=CARTESIAN_POINT('Ctrl Pts',(-9.02542144995427,12.2,-6.38883139678672));
#279402=CARTESIAN_POINT('Ctrl Pts',(-9.02777848116317,12.2,-6.3923432262133));
#279403=CARTESIAN_POINT('Ctrl Pts',(-9.03013746479171,12.2,-6.39587027151661));
#279404=CARTESIAN_POINT('Ctrl Pts',(-9.03249644842025,12.2,-6.39939731681992));
#279405=CARTESIAN_POINT('Ctrl Pts',(-9.03485738446018,12.2,-6.40293958068339));
#279406=CARTESIAN_POINT('Ctrl Pts',(-9.03722015931136,12.2,-6.40649702382327));
#279407=CARTESIAN_POINT('Ctrl Pts',(-9.03958293384062,12.2,-6.41005446647846));
#279408=CARTESIAN_POINT('Ctrl Pts',(-9.04194754608948,12.2,-6.41362708990791));
#279409=CARTESIAN_POINT('Ctrl Pts',(-9.0443138827401,12.2,-6.41721485596418));
#279410=CARTESIAN_POINT('Ctrl Pts',(-9.04668021971314,12.2,-6.42080262250928));
#279411=CARTESIAN_POINT('Ctrl Pts',(-9.0490482813804,12.2,-6.42440553203445));
#279412=CARTESIAN_POINT('Ctrl Pts',(-9.05141795562083,12.2,-6.42802354839985));
#279413=CARTESIAN_POINT('Ctrl Pts',(-9.05378762953839,12.2,-6.43164156427229));
#279414=CARTESIAN_POINT('Ctrl Pts',(-9.05615891469182,12.2,-6.43527468591496));
#279415=CARTESIAN_POINT('Ctrl Pts',(-9.05853170133109,12.2,-6.43892287722686));
#279416=CARTESIAN_POINT('Ctrl Pts',(-9.06090448829365,12.2,-6.44257106903582));
#279417=CARTESIAN_POINT('Ctrl Pts',(-9.06327877618818,12.2,-6.4462343287427));
#279418=CARTESIAN_POINT('Ctrl Pts',(-9.06565445460312,12.2,-6.44991262201711));
#279419=CARTESIAN_POINT('Ctrl Pts',(-9.06803013269437,12.2,-6.45359091479036));
#279420=CARTESIAN_POINT('Ctrl Pts',(-9.07040720007513,12.2,-6.45728423970382));
#279421=CARTESIAN_POINT('Ctrl Pts',(-9.07278555004731,12.2,-6.46099255845528));
#279422=CARTESIAN_POINT('Ctrl Pts',(-9.07516390034354,12.2,-6.46470087771199));
#279423=CARTESIAN_POINT('Ctrl Pts',(-9.07754353184263,12.2,-6.46842419346764));
#279424=CARTESIAN_POINT('Ctrl Pts',(-9.07992433619469,12.2,-6.4721624660057));
#279425=CARTESIAN_POINT('Ctrl Pts',(-9.08230514022236,12.2,-6.47590073803442));
#279426=CARTESIAN_POINT('Ctrl Pts',(-9.08468711684124,12.2,-6.47965396932436));
#279427=CARTESIAN_POINT('Ctrl Pts',(-9.0870701589876,12.2,-6.48342212020326));
#279428=CARTESIAN_POINT('Ctrl Pts',(-9.08885744067855,12.2,-6.48624823349079));
#279429=CARTESIAN_POINT('Ctrl Pts',(-9.09064532242522,12.2,-6.4890827392013));
#279430=CARTESIAN_POINT('Ctrl Pts',(-9.09243375765184,12.2,-6.49192562184688));
#279431=CARTESIAN_POINT('Ctrl Pts',(-9.09422219320335,12.2,-6.49476850500892));
#279432=CARTESIAN_POINT('Ctrl Pts',(-9.09601118414669,12.2,-6.49761976600661));
#279433=CARTESIAN_POINT('Ctrl Pts',(-9.09780068415682,12.2,-6.50047938813169));
#279434=CARTESIAN_POINT('Ctrl Pts',(-9.09959018384188,12.2,-6.50333900973726));
#279435=CARTESIAN_POINT('Ctrl Pts',(-9.1013801930769,12.2,-6.50620699290073));
#279436=CARTESIAN_POINT('Ctrl Pts',(-9.10317066813689,12.2,-6.50908332108862));
#279437=CARTESIAN_POINT('Ctrl Pts',(-9.10496114319688,12.2,-6.51195964927651));
#279438=CARTESIAN_POINT('Ctrl Pts',(-9.1067520827753,12.2,-6.51484432377786));
#279439=CARTESIAN_POINT('Ctrl Pts',(-9.10854344526001,12.2,-6.51773732747758));
#279440=CARTESIAN_POINT('Ctrl Pts',(-9.11033480774472,12.2,-6.5206303311773));
#279441=CARTESIAN_POINT('Ctrl Pts',(-9.11212659112207,12.2,-6.52353166530653));
#279442=CARTESIAN_POINT('Ctrl Pts',(-9.11391875177342,12.2,-6.52644131296398));
#279443=CARTESIAN_POINT('Ctrl Pts',(-9.11571091242477,12.2,-6.52935096062143));
#279444=CARTESIAN_POINT('Ctrl Pts',(-9.11750345090314,12.2,-6.53226892280484));
#279445=CARTESIAN_POINT('Ctrl Pts',(-9.1192963235463,12.2,-6.53519518290613));
#279446=CARTESIAN_POINT('Ctrl Pts',(-9.12108919618947,12.2,-6.53812144300742));
#279447=CARTESIAN_POINT('Ctrl Pts',(-9.12288240335759,12.2,-6.54105600101645));
#279448=CARTESIAN_POINT('Ctrl Pts',(-9.12467590187574,12.2,-6.54399884207509));
#279449=CARTESIAN_POINT('Ctrl Pts',(-9.1264694007197,12.2,-6.54694168366835));
#279450=CARTESIAN_POINT('Ctrl Pts',(-9.12826318826373,12.2,-6.54989280803055));
#279451=CARTESIAN_POINT('Ctrl Pts',(-9.13005722610782,12.2,-6.55285219817011));
#279452=CARTESIAN_POINT('Ctrl Pts',(-9.131851263626,12.2,-6.55581158777205));
#279453=CARTESIAN_POINT('Ctrl Pts',(-9.13364554887279,12.2,-6.55877924443433));
#279454=CARTESIAN_POINT('Ctrl Pts',(-9.13544003960558,12.2,-6.56175515214246));
#279455=CARTESIAN_POINT('Ctrl Pts',(-9.13723453033836,12.2,-6.5647310598506));
#279456=CARTESIAN_POINT('Ctrl Pts',(-9.13902922651089,12.2,-6.56771521753427));
#279457=CARTESIAN_POINT('Ctrl Pts',(-9.14082408565403,12.2,-6.57070761059293));
#279458=CARTESIAN_POINT('Ctrl Pts',(-9.14261894479717,12.2,-6.5737000036516));
#279459=CARTESIAN_POINT('Ctrl Pts',(-9.14441396688194,12.2,-6.5767006307426));
#279460=CARTESIAN_POINT('Ctrl Pts',(-9.14620911002505,12.2,-6.57970947775828));
#279461=CARTESIAN_POINT('Ctrl Pts',(-9.14800425316816,12.2,-6.58271832477397));
#279462=CARTESIAN_POINT('Ctrl Pts',(-9.14979951716959,12.2,-6.58573538963095));
#279463=CARTESIAN_POINT('Ctrl Pts',(-9.15159486127103,12.2,-6.58876065914535));
#279464=CARTESIAN_POINT('Ctrl Pts',(-9.15339020537247,12.2,-6.59178592865973));
#279465=CARTESIAN_POINT('Ctrl Pts',(-9.15518562849488,12.2,-6.5948194014044));
#279466=CARTESIAN_POINT('Ctrl Pts',(-9.15698108968601,12.2,-6.59786106069489));
#279467=CARTESIAN_POINT('Ctrl Pts',(-9.15937503815829,12.2,-6.60191660678392));
#279468=CARTESIAN_POINT('Ctrl Pts',(-9.16176905130973,12.2,-6.605986708391));
#279469=CARTESIAN_POINT('Ctrl Pts',(-9.16416303566243,12.2,-6.61007132755901));
#279470=CARTESIAN_POINT('Ctrl Pts',(-9.16595852376386,12.2,-6.61313479165675));
#279471=CARTESIAN_POINT('Ctrl Pts',(-9.16775399481528,12.2,-6.61620642219517));
#279472=CARTESIAN_POINT('Ctrl Pts',(-9.16954940704172,12.2,-6.61928620224996));
#279473=CARTESIAN_POINT('Ctrl Pts',(-9.17194329022776,12.2,-6.62339257602934));
#279474=CARTESIAN_POINT('Ctrl Pts',(-9.1743370700721,12.2,-6.62751343742149));
#279475=CARTESIAN_POINT('Ctrl Pts',(-9.1767306510914,12.2,-6.63164875242609));
#279476=CARTESIAN_POINT('Ctrl Pts',(-9.17852583669283,12.2,-6.63475023839782));
#279477=CARTESIAN_POINT('Ctrl Pts',(-9.18032090972761,12.2,-6.63785985188584));
#279478=CARTESIAN_POINT('Ctrl Pts',(-9.1821158294957,12.2,-6.64097757935659));
#279479=CARTESIAN_POINT('Ctrl Pts',(-9.1839107492638,12.2,-6.64409530682733));
#279480=CARTESIAN_POINT('Ctrl Pts',(-9.18570551742541,12.2,-6.6472211457024));
#279481=CARTESIAN_POINT('Ctrl Pts',(-9.18750009220169,12.2,-6.65035508272781));
#279482=CARTESIAN_POINT('Ctrl Pts',(-9.18929466697797,12.2,-6.65348901975322));
#279483=CARTESIAN_POINT('Ctrl Pts',(-9.19108904920546,12.2,-6.65663105373061));
#279484=CARTESIAN_POINT('Ctrl Pts',(-9.19288319848176,12.2,-6.65978116875544));
#279485=CARTESIAN_POINT('Ctrl Pts',(-9.19467734775807,12.2,-6.66293128378026));
#279486=CARTESIAN_POINT('Ctrl Pts',(-9.19647126521969,12.2,-6.66608947912071));
#279487=CARTESIAN_POINT('Ctrl Pts',(-9.19826490998788,12.2,-6.66925573967164));
#279488=CARTESIAN_POINT('Ctrl Pts',(-9.20005855475607,12.2,-6.67242200022257));
#279489=CARTESIAN_POINT('Ctrl Pts',(-9.2018519283576,12.2,-6.67559632525625));
#279490=CARTESIAN_POINT('Ctrl Pts',(-9.20364498962584,12.2,-6.67877869980621));
#279491=CARTESIAN_POINT('Ctrl Pts',(-9.20543805121982,12.2,-6.6819610749343));
#279492=CARTESIAN_POINT('Ctrl Pts',(-9.20723080226369,12.2,-6.68515149878128));
#279493=CARTESIAN_POINT('Ctrl Pts',(-9.20902320189913,12.2,-6.68834995545555));
#279494=CARTESIAN_POINT('Ctrl Pts',(-9.21081560120895,12.2,-6.69154841154877));
#279495=CARTESIAN_POINT('Ctrl Pts',(-9.21260765075567,12.2,-6.69475490061058));
#279496=CARTESIAN_POINT('Ctrl Pts',(-9.21439931057169,12.2,-6.69796940686362));
#279497=CARTESIAN_POINT('Ctrl Pts',(-9.21619097038772,12.2,-6.70118391311667));
#279498=CARTESIAN_POINT('Ctrl Pts',(-9.21798224052702,12.2,-6.70440643593556));
#279499=CARTESIAN_POINT('Ctrl Pts',(-9.21977308271192,12.2,-6.70763695906889));
#279500=CARTESIAN_POINT('Ctrl Pts',(-9.22156392489683,12.2,-6.71086748220222));
#279501=CARTESIAN_POINT('Ctrl Pts',(-9.22335433901509,12.2,-6.71410600670123));
#279502=CARTESIAN_POINT('Ctrl Pts',(-9.22514428682506,12.2,-6.71735251574995));
#279503=CARTESIAN_POINT('Ctrl Pts',(-9.22693423463502,12.2,-6.72059902479868));
#279504=CARTESIAN_POINT('Ctrl Pts',(-9.22872371752001,12.2,-6.72385351788039));
#279505=CARTESIAN_POINT('Ctrl Pts',(-9.23051269578838,12.2,-6.72711598088615));
#279506=CARTESIAN_POINT('Ctrl Pts',(-9.233494326344,12.2,-6.73255341942663));
#279507=CARTESIAN_POINT('Ctrl Pts',(-9.23647455619045,12.2,-6.73801299262213));
#279508=CARTESIAN_POINT('Ctrl Pts',(-9.23945320502344,12.2,-6.74349462473031));
#279509=CARTESIAN_POINT('Ctrl Pts',(-9.2412403942583,12.2,-6.74678360387573));
#279510=CARTESIAN_POINT('Ctrl Pts',(-9.24302701403688,12.2,-6.75008052466064));
#279511=CARTESIAN_POINT('Ctrl Pts',(-9.24481303130537,12.2,-6.7533853708732));
#279512=CARTESIAN_POINT('Ctrl Pts',(-9.24659904857387,12.2,-6.75669021708576));
#279513=CARTESIAN_POINT('Ctrl Pts',(-9.24838446267574,12.2,-6.76000299138112));
#279514=CARTESIAN_POINT('Ctrl Pts',(-9.25016923831931,12.2,-6.76332367555106));
#279515=CARTESIAN_POINT('Ctrl Pts',(-9.25195401428712,12.2,-6.76664436032426));
#279516=CARTESIAN_POINT('Ctrl Pts',(-9.25373815124641,12.2,-6.76997295699134));
#279517=CARTESIAN_POINT('Ctrl Pts',(-9.25552160417219,12.2,-6.77330944418565));
#279518=CARTESIAN_POINT('Ctrl Pts',(-9.25730505677395,12.2,-6.77664593077383));
#279519=CARTESIAN_POINT('Ctrl Pts',(-9.25908782435398,12.2,-6.77999030870202));
#279520=CARTESIAN_POINT('Ctrl Pts',(-9.2608698668365,12.2,-6.78334256091528));
#279521=CARTESIAN_POINT('Ctrl Pts',(-9.26265190931903,12.2,-6.78669481312853));
#279522=CARTESIAN_POINT('Ctrl Pts',(-9.26443322619546,12.2,-6.7900549376617));
#279523=CARTESIAN_POINT('Ctrl Pts',(-9.26621380150165,12.2,-6.79342292836566));
#279524=CARTESIAN_POINT('Ctrl Pts',(-9.26799437680784,12.2,-6.79679091906963));
#279525=CARTESIAN_POINT('Ctrl Pts',(-9.26977421267685,12.2,-6.80016677138531));
#279526=CARTESIAN_POINT('Ctrl Pts',(-9.27155330300005,12.2,-6.80355049700001));
#279527=CARTESIAN_POINT('Origin',(-5.66257110645729E-14,15.2,-1.77635683940025E-14));
#279528=CARTESIAN_POINT('',(-7.64657512344065,15.2,-7.01216898588537));
#279529=CARTESIAN_POINT('',(-7.64657512344065,12.2,-7.01216898588537));
#279530=CARTESIAN_POINT('',(-7.64657512300006,15.2,-7.01216898500002));
#279531=CARTESIAN_POINT('Origin',(-5.66257110645729E-14,12.2,-1.77635683940025E-14));
#279532=CARTESIAN_POINT('Origin',(-5.66257110645729E-14,15.2,-1.77635683940025E-14));
#279533=CARTESIAN_POINT('Origin',(-5.66257110645729E-14,15.2,-1.77635683940025E-14));
#279534=CARTESIAN_POINT('',(-8.20893607000006,15.2,-8.05377977100001));
#279535=CARTESIAN_POINT('',(-7.93573928331785,15.2,-8.32310290898372));
#279536=CARTESIAN_POINT('Origin',(-5.66257110645729E-14,15.2,-1.77635683940025E-14));
#279537=CARTESIAN_POINT('',(-7.93573928331785,12.2,-8.32310290898372));
#279538=CARTESIAN_POINT('',(-7.93573928300006,15.2,-8.32310290900002));
#279539=CARTESIAN_POINT('',(-8.20893607000006,12.2,-8.05377977100001));
#279540=CARTESIAN_POINT('Origin',(-5.66257110645729E-14,12.2,-1.77635683940025E-14));
#279541=CARTESIAN_POINT('',(-8.20893607000006,15.2,-8.05377977100001));
#279542=CARTESIAN_POINT('Ctrl Pts',(-7.64657512400006,15.2,-7.01216898700002));
#279543=CARTESIAN_POINT('Ctrl Pts',(-7.64657512400006,11.6,-7.01216898700002));
#279544=CARTESIAN_POINT('Ctrl Pts',(-7.64669302700005,15.2,-7.01229743700001));
#279545=CARTESIAN_POINT('Ctrl Pts',(-7.64669302700005,11.6,-7.01229743700001));
#279546=CARTESIAN_POINT('Ctrl Pts',(-7.64693288600006,15.2,-7.01255888400001));
#279547=CARTESIAN_POINT('Ctrl Pts',(-7.64693288600006,11.6,-7.01255888400001));
#279548=CARTESIAN_POINT('Ctrl Pts',(-7.64729613400006,15.2,-7.01295521700001));
#279549=CARTESIAN_POINT('Ctrl Pts',(-7.64729613400006,11.6,-7.01295521700001));
#279550=CARTESIAN_POINT('Ctrl Pts',(-7.64778506600006,15.2,-7.01348948000001));
#279551=CARTESIAN_POINT('Ctrl Pts',(-7.64778506600006,11.6,-7.01348948000001));
#279552=CARTESIAN_POINT('Ctrl Pts',(-7.64840281700006,15.2,-7.01416585800001));
#279553=CARTESIAN_POINT('Ctrl Pts',(-7.64840281700006,11.6,-7.01416585800001));
#279554=CARTESIAN_POINT('Ctrl Pts',(-7.64902989000006,15.2,-7.01485383100002));
#279555=CARTESIAN_POINT('Ctrl Pts',(-7.64902989000006,11.6,-7.01485383100002));
#279556=CARTESIAN_POINT('Ctrl Pts',(-7.64966267500006,15.2,-7.01554946900002));
#279557=CARTESIAN_POINT('Ctrl Pts',(-7.64966267500006,11.6,-7.01554946900002));
#279558=CARTESIAN_POINT('Ctrl Pts',(-7.65030113900006,15.2,-7.01625276700002));
#279559=CARTESIAN_POINT('Ctrl Pts',(-7.65030113900006,11.6,-7.01625276700002));
#279560=CARTESIAN_POINT('Ctrl Pts',(-7.65094525300006,15.2,-7.01696371500002));
#279561=CARTESIAN_POINT('Ctrl Pts',(-7.65094525300006,11.6,-7.01696371500002));
#279562=CARTESIAN_POINT('Ctrl Pts',(-7.65159498500006,15.2,-7.01768230800001));
#279563=CARTESIAN_POINT('Ctrl Pts',(-7.65159498500006,11.6,-7.01768230800001));
#279564=CARTESIAN_POINT('Ctrl Pts',(-7.65225030200006,15.2,-7.01840853700002));
#279565=CARTESIAN_POINT('Ctrl Pts',(-7.65225030200006,11.6,-7.01840853700002));
#279566=CARTESIAN_POINT('Ctrl Pts',(-7.65291117500006,15.2,-7.01914239300002));
#279567=CARTESIAN_POINT('Ctrl Pts',(-7.65291117500006,11.6,-7.01914239300002));
#279568=CARTESIAN_POINT('Ctrl Pts',(-7.65357757300006,15.2,-7.01988387000001));
#279569=CARTESIAN_POINT('Ctrl Pts',(-7.65357757300006,11.6,-7.01988387000001));
#279570=CARTESIAN_POINT('Ctrl Pts',(-7.65424946500006,15.2,-7.02063296100001));
#279571=CARTESIAN_POINT('Ctrl Pts',(-7.65424946500006,11.6,-7.02063296100001));
#279572=CARTESIAN_POINT('Ctrl Pts',(-7.65492682000006,15.2,-7.02138965600002));
#279573=CARTESIAN_POINT('Ctrl Pts',(-7.65492682000006,11.6,-7.02138965600002));
#279574=CARTESIAN_POINT('Ctrl Pts',(-7.65560960800006,15.2,-7.02215394900002));
#279575=CARTESIAN_POINT('Ctrl Pts',(-7.65560960800006,11.6,-7.02215394900002));
#279576=CARTESIAN_POINT('Ctrl Pts',(-7.65629779900006,15.2,-7.02292583300002));
#279577=CARTESIAN_POINT('Ctrl Pts',(-7.65629779900006,11.6,-7.02292583300002));
#279578=CARTESIAN_POINT('Ctrl Pts',(-7.65699136200006,15.2,-7.02370530000002));
#279579=CARTESIAN_POINT('Ctrl Pts',(-7.65699136200006,11.6,-7.02370530000002));
#279580=CARTESIAN_POINT('Ctrl Pts',(-7.65769027000006,15.2,-7.02449234200002));
#279581=CARTESIAN_POINT('Ctrl Pts',(-7.65769027000006,11.6,-7.02449234200002));
#279582=CARTESIAN_POINT('Ctrl Pts',(-7.65839449000006,15.2,-7.02528695200002));
#279583=CARTESIAN_POINT('Ctrl Pts',(-7.65839449000006,11.6,-7.02528695200002));
#279584=CARTESIAN_POINT('Ctrl Pts',(-7.65910399300005,15.2,-7.02608912100001));
#279585=CARTESIAN_POINT('Ctrl Pts',(-7.65910399300005,11.6,-7.02608912100001));
#279586=CARTESIAN_POINT('Ctrl Pts',(-7.65981875000006,15.2,-7.02689884500002));
#279587=CARTESIAN_POINT('Ctrl Pts',(-7.65981875000006,11.6,-7.02689884500002));
#279588=CARTESIAN_POINT('Ctrl Pts',(-7.66053873200006,15.2,-7.02771611300002));
#279589=CARTESIAN_POINT('Ctrl Pts',(-7.66053873200006,11.6,-7.02771611300002));
#279590=CARTESIAN_POINT('Ctrl Pts',(-7.66126391000006,15.2,-7.02854092000001));
#279591=CARTESIAN_POINT('Ctrl Pts',(-7.66126391000006,11.6,-7.02854092000001));
#279592=CARTESIAN_POINT('Ctrl Pts',(-7.66199425500006,15.2,-7.02937325800002));
#279593=CARTESIAN_POINT('Ctrl Pts',(-7.66199425500006,11.6,-7.02937325800002));
#279594=CARTESIAN_POINT('Ctrl Pts',(-7.66272973800006,15.2,-7.03021311800001));
#279595=CARTESIAN_POINT('Ctrl Pts',(-7.66272973800006,11.6,-7.03021311800001));
#279596=CARTESIAN_POINT('Ctrl Pts',(-7.66347032900006,15.2,-7.03106049500001));
#279597=CARTESIAN_POINT('Ctrl Pts',(-7.66347032900006,11.6,-7.03106049500001));
#279598=CARTESIAN_POINT('Ctrl Pts',(-7.66421600000006,15.2,-7.03191538200001));
#279599=CARTESIAN_POINT('Ctrl Pts',(-7.66421600000006,11.6,-7.03191538200001));
#279600=CARTESIAN_POINT('Ctrl Pts',(-7.66496672300006,15.2,-7.03277777000002));
#279601=CARTESIAN_POINT('Ctrl Pts',(-7.66496672300006,11.6,-7.03277777000002));
#279602=CARTESIAN_POINT('Ctrl Pts',(-7.66572246900005,15.2,-7.03364765100002));
#279603=CARTESIAN_POINT('Ctrl Pts',(-7.66572246900005,11.6,-7.03364765100002));
#279604=CARTESIAN_POINT('Ctrl Pts',(-7.66648321200006,15.2,-7.03452502000002));
#279605=CARTESIAN_POINT('Ctrl Pts',(-7.66648321200006,11.6,-7.03452502000002));
#279606=CARTESIAN_POINT('Ctrl Pts',(-7.66724892000005,15.2,-7.03540986900002));
#279607=CARTESIAN_POINT('Ctrl Pts',(-7.66724892000005,11.6,-7.03540986900002));
#279608=CARTESIAN_POINT('Ctrl Pts',(-7.66801956900006,15.2,-7.03630219100001));
#279609=CARTESIAN_POINT('Ctrl Pts',(-7.66801956900006,11.6,-7.03630219100001));
#279610=CARTESIAN_POINT('Ctrl Pts',(-7.66879512900006,15.2,-7.03720197800001));
#279611=CARTESIAN_POINT('Ctrl Pts',(-7.66879512900006,11.6,-7.03720197800001));
#279612=CARTESIAN_POINT('Ctrl Pts',(-7.66957557200006,15.2,-7.03810922400002));
#279613=CARTESIAN_POINT('Ctrl Pts',(-7.66957557200006,11.6,-7.03810922400002));
#279614=CARTESIAN_POINT('Ctrl Pts',(-7.67036087200006,15.2,-7.03902392000002));
#279615=CARTESIAN_POINT('Ctrl Pts',(-7.67036087200006,11.6,-7.03902392000002));
#279616=CARTESIAN_POINT('Ctrl Pts',(-7.67115100100006,15.2,-7.03994606100002));
#279617=CARTESIAN_POINT('Ctrl Pts',(-7.67115100100006,11.6,-7.03994606100002));
#279618=CARTESIAN_POINT('Ctrl Pts',(-7.67194593100006,15.2,-7.04087563800002));
#279619=CARTESIAN_POINT('Ctrl Pts',(-7.67194593100006,11.6,-7.04087563800002));
#279620=CARTESIAN_POINT('Ctrl Pts',(-7.67274563400005,15.2,-7.04181264600001));
#279621=CARTESIAN_POINT('Ctrl Pts',(-7.67274563400005,11.6,-7.04181264600001));
#279622=CARTESIAN_POINT('Ctrl Pts',(-7.67355008500005,15.2,-7.04275707600001));
#279623=CARTESIAN_POINT('Ctrl Pts',(-7.67355008500005,11.6,-7.04275707600001));
#279624=CARTESIAN_POINT('Ctrl Pts',(-7.67435925800006,15.2,-7.04370892300001));
#279625=CARTESIAN_POINT('Ctrl Pts',(-7.67435925800006,11.6,-7.04370892300001));
#279626=CARTESIAN_POINT('Ctrl Pts',(-7.67517312200006,15.2,-7.04466817700002));
#279627=CARTESIAN_POINT('Ctrl Pts',(-7.67517312200006,11.6,-7.04466817700002));
#279628=CARTESIAN_POINT('Ctrl Pts',(-7.67599165500006,15.2,-7.04563483400002));
#279629=CARTESIAN_POINT('Ctrl Pts',(-7.67599165500006,11.6,-7.04563483400002));
#279630=CARTESIAN_POINT('Ctrl Pts',(-7.67681482700005,15.2,-7.04660888500002));
#279631=CARTESIAN_POINT('Ctrl Pts',(-7.67681482700005,11.6,-7.04660888500002));
#279632=CARTESIAN_POINT('Ctrl Pts',(-7.67764261400006,15.2,-7.04759032400001));
#279633=CARTESIAN_POINT('Ctrl Pts',(-7.67764261400006,11.6,-7.04759032400001));
#279634=CARTESIAN_POINT('Ctrl Pts',(-7.67847498800006,15.2,-7.04857914500002));
#279635=CARTESIAN_POINT('Ctrl Pts',(-7.67847498800006,11.6,-7.04857914500002));
#279636=CARTESIAN_POINT('Ctrl Pts',(-7.67931192300006,15.2,-7.04957533800001));
#279637=CARTESIAN_POINT('Ctrl Pts',(-7.67931192300006,11.6,-7.04957533800001));
#279638=CARTESIAN_POINT('Ctrl Pts',(-7.68015339400005,15.2,-7.05057889900001));
#279639=CARTESIAN_POINT('Ctrl Pts',(-7.68015339400005,11.6,-7.05057889900001));
#279640=CARTESIAN_POINT('Ctrl Pts',(-7.68099937300006,15.2,-7.05158981900002));
#279641=CARTESIAN_POINT('Ctrl Pts',(-7.68099937300006,11.6,-7.05158981900002));
#279642=CARTESIAN_POINT('Ctrl Pts',(-7.68184983600006,15.2,-7.05260809300002));
#279643=CARTESIAN_POINT('Ctrl Pts',(-7.68184983600006,11.6,-7.05260809300002));
#279644=CARTESIAN_POINT('Ctrl Pts',(-7.68270475700006,15.2,-7.05363371400002));
#279645=CARTESIAN_POINT('Ctrl Pts',(-7.68270475700006,11.6,-7.05363371400002));
#279646=CARTESIAN_POINT('Ctrl Pts',(-7.68356411100005,15.2,-7.05466667300002));
#279647=CARTESIAN_POINT('Ctrl Pts',(-7.68356411100005,11.6,-7.05466667300002));
#279648=CARTESIAN_POINT('Ctrl Pts',(-7.68442787100006,15.2,-7.05570696600001));
#279649=CARTESIAN_POINT('Ctrl Pts',(-7.68442787100006,11.6,-7.05570696600001));
#279650=CARTESIAN_POINT('Ctrl Pts',(-7.68529601300005,15.2,-7.05675458400002));
#279651=CARTESIAN_POINT('Ctrl Pts',(-7.68529601300005,11.6,-7.05675458400002));
#279652=CARTESIAN_POINT('Ctrl Pts',(-7.68616851000005,15.2,-7.05780952100002));
#279653=CARTESIAN_POINT('Ctrl Pts',(-7.68616851000005,11.6,-7.05780952100002));
#279654=CARTESIAN_POINT('Ctrl Pts',(-7.68704533800006,15.2,-7.05887177000001));
#279655=CARTESIAN_POINT('Ctrl Pts',(-7.68704533800006,11.6,-7.05887177000001));
#279656=CARTESIAN_POINT('Ctrl Pts',(-7.68792647200006,15.2,-7.05994132500001));
#279657=CARTESIAN_POINT('Ctrl Pts',(-7.68792647200006,11.6,-7.05994132500001));
#279658=CARTESIAN_POINT('Ctrl Pts',(-7.68881188700006,15.2,-7.06101817800001));
#279659=CARTESIAN_POINT('Ctrl Pts',(-7.68881188700006,11.6,-7.06101817800001));
#279660=CARTESIAN_POINT('Ctrl Pts',(-7.68970155800006,15.2,-7.06210232300001));
#279661=CARTESIAN_POINT('Ctrl Pts',(-7.68970155800006,11.6,-7.06210232300001));
#279662=CARTESIAN_POINT('Ctrl Pts',(-7.69059546000006,15.2,-7.06319375400002));
#279663=CARTESIAN_POINT('Ctrl Pts',(-7.69059546000006,11.6,-7.06319375400002));
#279664=CARTESIAN_POINT('Ctrl Pts',(-7.69149356900006,15.2,-7.06429246300001));
#279665=CARTESIAN_POINT('Ctrl Pts',(-7.69149356900006,11.6,-7.06429246300001));
#279666=CARTESIAN_POINT('Ctrl Pts',(-7.69239586000006,15.2,-7.06539844300002));
#279667=CARTESIAN_POINT('Ctrl Pts',(-7.69239586000006,11.6,-7.06539844300002));
#279668=CARTESIAN_POINT('Ctrl Pts',(-7.69330230900006,15.2,-7.06651168900001));
#279669=CARTESIAN_POINT('Ctrl Pts',(-7.69330230900006,11.6,-7.06651168900001));
#279670=CARTESIAN_POINT('Ctrl Pts',(-7.69421289200006,15.2,-7.06763219300001));
#279671=CARTESIAN_POINT('Ctrl Pts',(-7.69421289200006,11.6,-7.06763219300001));
#279672=CARTESIAN_POINT('Ctrl Pts',(-7.69512758300006,15.2,-7.06875994900001));
#279673=CARTESIAN_POINT('Ctrl Pts',(-7.69512758300006,11.6,-7.06875994900001));
#279674=CARTESIAN_POINT('Ctrl Pts',(-7.69604636100006,15.2,-7.06989495100002));
#279675=CARTESIAN_POINT('Ctrl Pts',(-7.69604636100006,11.6,-7.06989495100002));
#279676=CARTESIAN_POINT('Ctrl Pts',(-7.69696919900006,15.2,-7.07103719000001));
#279677=CARTESIAN_POINT('Ctrl Pts',(-7.69696919900006,11.6,-7.07103719000001));
#279678=CARTESIAN_POINT('Ctrl Pts',(-7.69789607400006,15.2,-7.07218666200002));
#279679=CARTESIAN_POINT('Ctrl Pts',(-7.69789607400006,11.6,-7.07218666200002));
#279680=CARTESIAN_POINT('Ctrl Pts',(-7.69882696400006,15.2,-7.07334335800001));
#279681=CARTESIAN_POINT('Ctrl Pts',(-7.69882696400006,11.6,-7.07334335800001));
#279682=CARTESIAN_POINT('Ctrl Pts',(-7.69976184300005,15.2,-7.07450727300002));
#279683=CARTESIAN_POINT('Ctrl Pts',(-7.69976184300005,11.6,-7.07450727300002));
#279684=CARTESIAN_POINT('Ctrl Pts',(-7.70070068900005,15.2,-7.07567840100002));
#279685=CARTESIAN_POINT('Ctrl Pts',(-7.70070068900005,11.6,-7.07567840100002));
#279686=CARTESIAN_POINT('Ctrl Pts',(-7.70164347700005,15.2,-7.07685673500002));
#279687=CARTESIAN_POINT('Ctrl Pts',(-7.70164347700005,11.6,-7.07685673500002));
#279688=CARTESIAN_POINT('Ctrl Pts',(-7.70259018400005,15.2,-7.07804226800001));
#279689=CARTESIAN_POINT('Ctrl Pts',(-7.70259018400005,11.6,-7.07804226800001));
#279690=CARTESIAN_POINT('Ctrl Pts',(-7.70354078800005,15.2,-7.07923499200002));
#279691=CARTESIAN_POINT('Ctrl Pts',(-7.70354078800005,11.6,-7.07923499200002));
#279692=CARTESIAN_POINT('Ctrl Pts',(-7.70449526500006,15.2,-7.08043490300001));
#279693=CARTESIAN_POINT('Ctrl Pts',(-7.70449526500006,11.6,-7.08043490300001));
#279694=CARTESIAN_POINT('Ctrl Pts',(-7.70545359200005,15.2,-7.08164199400001));
#279695=CARTESIAN_POINT('Ctrl Pts',(-7.70545359200005,11.6,-7.08164199400001));
#279696=CARTESIAN_POINT('Ctrl Pts',(-7.70641574500005,15.2,-7.08285625800002));
#279697=CARTESIAN_POINT('Ctrl Pts',(-7.70641574500005,11.6,-7.08285625800002));
#279698=CARTESIAN_POINT('Ctrl Pts',(-7.70738170300006,15.2,-7.08407768800001));
#279699=CARTESIAN_POINT('Ctrl Pts',(-7.70738170300006,11.6,-7.08407768800001));
#279700=CARTESIAN_POINT('Ctrl Pts',(-7.70835144200006,15.2,-7.08530627800001));
#279701=CARTESIAN_POINT('Ctrl Pts',(-7.70835144200006,11.6,-7.08530627800001));
#279702=CARTESIAN_POINT('Ctrl Pts',(-7.70932493900006,15.2,-7.08654202100002));
#279703=CARTESIAN_POINT('Ctrl Pts',(-7.70932493900006,11.6,-7.08654202100002));
#279704=CARTESIAN_POINT('Ctrl Pts',(-7.71030217200006,15.2,-7.08778491300002));
#279705=CARTESIAN_POINT('Ctrl Pts',(-7.71030217200006,11.6,-7.08778491300002));
#279706=CARTESIAN_POINT('Ctrl Pts',(-7.71128311900006,15.2,-7.08903494500002));
#279707=CARTESIAN_POINT('Ctrl Pts',(-7.71128311900006,11.6,-7.08903494500002));
#279708=CARTESIAN_POINT('Ctrl Pts',(-7.71226775600006,15.2,-7.09029211100002));
#279709=CARTESIAN_POINT('Ctrl Pts',(-7.71226775600006,11.6,-7.09029211100002));
#279710=CARTESIAN_POINT('Ctrl Pts',(-7.71325606200006,15.2,-7.09155640600001));
#279711=CARTESIAN_POINT('Ctrl Pts',(-7.71325606200006,11.6,-7.09155640600001));
#279712=CARTESIAN_POINT('Ctrl Pts',(-7.71424801400006,15.2,-7.09282782200002));
#279713=CARTESIAN_POINT('Ctrl Pts',(-7.71424801400006,11.6,-7.09282782200002));
#279714=CARTESIAN_POINT('Ctrl Pts',(-7.71524359000006,15.2,-7.09410635300002));
#279715=CARTESIAN_POINT('Ctrl Pts',(-7.71524359000006,11.6,-7.09410635300002));
#279716=CARTESIAN_POINT('Ctrl Pts',(-7.71624276900006,15.2,-7.09539199400002));
#279717=CARTESIAN_POINT('Ctrl Pts',(-7.71624276900006,11.6,-7.09539199400002));
#279718=CARTESIAN_POINT('Ctrl Pts',(-7.71724552800006,15.2,-7.09668473700001));
#279719=CARTESIAN_POINT('Ctrl Pts',(-7.71724552800006,11.6,-7.09668473700001));
#279720=CARTESIAN_POINT('Ctrl Pts',(-7.71825184400006,15.2,-7.09798457600002));
#279721=CARTESIAN_POINT('Ctrl Pts',(-7.71825184400006,11.6,-7.09798457600002));
#279722=CARTESIAN_POINT('Ctrl Pts',(-7.71926169800006,15.2,-7.09929150500002));
#279723=CARTESIAN_POINT('Ctrl Pts',(-7.71926169800006,11.6,-7.09929150500002));
#279724=CARTESIAN_POINT('Ctrl Pts',(-7.72027506500006,15.2,-7.10060551700002));
#279725=CARTESIAN_POINT('Ctrl Pts',(-7.72027506500006,11.6,-7.10060551700002));
#279726=CARTESIAN_POINT('Ctrl Pts',(-7.72129192600006,15.2,-7.10192660800002));
#279727=CARTESIAN_POINT('Ctrl Pts',(-7.72129192600006,11.6,-7.10192660800002));
#279728=CARTESIAN_POINT('Ctrl Pts',(-7.72231225800006,15.2,-7.10325476900002));
#279729=CARTESIAN_POINT('Ctrl Pts',(-7.72231225800006,11.6,-7.10325476900002));
#279730=CARTESIAN_POINT('Ctrl Pts',(-7.72333604000006,15.2,-7.10458999400001));
#279731=CARTESIAN_POINT('Ctrl Pts',(-7.72333604000006,11.6,-7.10458999400001));
#279732=CARTESIAN_POINT('Ctrl Pts',(-7.72436325100006,15.2,-7.10593227900001));
#279733=CARTESIAN_POINT('Ctrl Pts',(-7.72436325100006,11.6,-7.10593227900001));
#279734=CARTESIAN_POINT('Ctrl Pts',(-7.72539386900006,15.2,-7.10728161400001));
#279735=CARTESIAN_POINT('Ctrl Pts',(-7.72539386900006,11.6,-7.10728161400001));
#279736=CARTESIAN_POINT('Ctrl Pts',(-7.72642787400006,15.2,-7.10863799800002));
#279737=CARTESIAN_POINT('Ctrl Pts',(-7.72642787400006,11.6,-7.10863799800002));
#279738=CARTESIAN_POINT('Ctrl Pts',(-7.72746524300005,15.2,-7.11000141900002));
#279739=CARTESIAN_POINT('Ctrl Pts',(-7.72746524300005,11.6,-7.11000141900002));
#279740=CARTESIAN_POINT('Ctrl Pts',(-7.72850595600006,15.2,-7.11137187600002));
#279741=CARTESIAN_POINT('Ctrl Pts',(-7.72850595600006,11.6,-7.11137187600002));
#279742=CARTESIAN_POINT('Ctrl Pts',(-7.72954999300006,15.2,-7.11274935900001));
#279743=CARTESIAN_POINT('Ctrl Pts',(-7.72954999300006,11.6,-7.11274935900001));
#279744=CARTESIAN_POINT('Ctrl Pts',(-7.73059733100006,15.2,-7.11413386300002));
#279745=CARTESIAN_POINT('Ctrl Pts',(-7.73059733100006,11.6,-7.11413386300002));
#279746=CARTESIAN_POINT('Ctrl Pts',(-7.73164795100006,15.2,-7.11552538200002));
#279747=CARTESIAN_POINT('Ctrl Pts',(-7.73164795100006,11.6,-7.11552538200002));
#279748=CARTESIAN_POINT('Ctrl Pts',(-7.73270183200006,15.2,-7.11692391000001));
#279749=CARTESIAN_POINT('Ctrl Pts',(-7.73270183200006,11.6,-7.11692391000001));
#279750=CARTESIAN_POINT('Ctrl Pts',(-7.73375895200005,15.2,-7.11832944100002));
#279751=CARTESIAN_POINT('Ctrl Pts',(-7.73375895200005,11.6,-7.11832944100002));
#279752=CARTESIAN_POINT('Ctrl Pts',(-7.73481929200006,15.2,-7.11974196800002));
#279753=CARTESIAN_POINT('Ctrl Pts',(-7.73481929200006,11.6,-7.11974196800002));
#279754=CARTESIAN_POINT('Ctrl Pts',(-7.73588283000005,15.2,-7.12116148600002));
#279755=CARTESIAN_POINT('Ctrl Pts',(-7.73588283000005,11.6,-7.12116148600002));
#279756=CARTESIAN_POINT('Ctrl Pts',(-7.73694954800006,15.2,-7.12258798800002));
#279757=CARTESIAN_POINT('Ctrl Pts',(-7.73694954800006,11.6,-7.12258798800002));
#279758=CARTESIAN_POINT('Ctrl Pts',(-7.73801942400006,15.2,-7.12402146700001));
#279759=CARTESIAN_POINT('Ctrl Pts',(-7.73801942400006,11.6,-7.12402146700001));
#279760=CARTESIAN_POINT('Ctrl Pts',(-7.73909243700006,15.2,-7.12546191900002));
#279761=CARTESIAN_POINT('Ctrl Pts',(-7.73909243700006,11.6,-7.12546191900002));
#279762=CARTESIAN_POINT('Ctrl Pts',(-7.74016856800006,15.2,-7.12690933700002));
#279763=CARTESIAN_POINT('Ctrl Pts',(-7.74016856800006,11.6,-7.12690933700002));
#279764=CARTESIAN_POINT('Ctrl Pts',(-7.74124779800006,15.2,-7.12836371300002));
#279765=CARTESIAN_POINT('Ctrl Pts',(-7.74124779800006,11.6,-7.12836371300002));
#279766=CARTESIAN_POINT('Ctrl Pts',(-7.74233010400006,15.2,-7.12982504500002));
#279767=CARTESIAN_POINT('Ctrl Pts',(-7.74233010400006,11.6,-7.12982504500002));
#279768=CARTESIAN_POINT('Ctrl Pts',(-7.74341546800006,15.2,-7.13129332400002));
#279769=CARTESIAN_POINT('Ctrl Pts',(-7.74341546800006,11.6,-7.13129332400002));
#279770=CARTESIAN_POINT('Ctrl Pts',(-7.74450387100006,15.2,-7.13276854400001));
#279771=CARTESIAN_POINT('Ctrl Pts',(-7.74450387100006,11.6,-7.13276854400001));
#279772=CARTESIAN_POINT('Ctrl Pts',(-7.74559529200006,15.2,-7.13425070000002));
#279773=CARTESIAN_POINT('Ctrl Pts',(-7.74559529200006,11.6,-7.13425070000002));
#279774=CARTESIAN_POINT('Ctrl Pts',(-7.74668971000006,15.2,-7.13573978500002));
#279775=CARTESIAN_POINT('Ctrl Pts',(-7.74668971000006,11.6,-7.13573978500002));
#279776=CARTESIAN_POINT('Ctrl Pts',(-7.74778710800006,15.2,-7.13723579300002));
#279777=CARTESIAN_POINT('Ctrl Pts',(-7.74778710800006,11.6,-7.13723579300002));
#279778=CARTESIAN_POINT('Ctrl Pts',(-7.74888746500006,15.2,-7.13873871900002));
#279779=CARTESIAN_POINT('Ctrl Pts',(-7.74888746500006,11.6,-7.13873871900002));
#279780=CARTESIAN_POINT('Ctrl Pts',(-7.74999076100006,15.2,-7.14024855600002));
#279781=CARTESIAN_POINT('Ctrl Pts',(-7.74999076100006,11.6,-7.14024855600002));
#279782=CARTESIAN_POINT('Ctrl Pts',(-7.75109697900006,15.2,-7.14176529900002));
#279783=CARTESIAN_POINT('Ctrl Pts',(-7.75109697900006,11.6,-7.14176529900002));
#279784=CARTESIAN_POINT('Ctrl Pts',(-7.75220609600006,15.2,-7.14328894200002));
#279785=CARTESIAN_POINT('Ctrl Pts',(-7.75220609600006,11.6,-7.14328894200002));
#279786=CARTESIAN_POINT('Ctrl Pts',(-7.75331809500006,15.2,-7.14481947600002));
#279787=CARTESIAN_POINT('Ctrl Pts',(-7.75331809500006,11.6,-7.14481947600002));
#279788=CARTESIAN_POINT('Ctrl Pts',(-7.75443295700006,15.2,-7.14635689900001));
#279789=CARTESIAN_POINT('Ctrl Pts',(-7.75443295700006,11.6,-7.14635689900001));
#279790=CARTESIAN_POINT('Ctrl Pts',(-7.75555066300005,15.2,-7.14790120400002));
#279791=CARTESIAN_POINT('Ctrl Pts',(-7.75555066300005,11.6,-7.14790120400002));
#279792=CARTESIAN_POINT('Ctrl Pts',(-7.75667119100006,15.2,-7.14945238400002));
#279793=CARTESIAN_POINT('Ctrl Pts',(-7.75667119100006,11.6,-7.14945238400002));
#279794=CARTESIAN_POINT('Ctrl Pts',(-7.75779452600006,15.2,-7.15101043300002));
#279795=CARTESIAN_POINT('Ctrl Pts',(-7.75779452600006,11.6,-7.15101043300002));
#279796=CARTESIAN_POINT('Ctrl Pts',(-7.75892064700006,15.2,-7.15257534600001));
#279797=CARTESIAN_POINT('Ctrl Pts',(-7.75892064700006,11.6,-7.15257534600001));
#279798=CARTESIAN_POINT('Ctrl Pts',(-7.76004953500006,15.2,-7.15414711700002));
#279799=CARTESIAN_POINT('Ctrl Pts',(-7.76004953500006,11.6,-7.15414711700002));
#279800=CARTESIAN_POINT('Ctrl Pts',(-7.76118117200006,15.2,-7.15572573900002));
#279801=CARTESIAN_POINT('Ctrl Pts',(-7.76118117200006,11.6,-7.15572573900002));
#279802=CARTESIAN_POINT('Ctrl Pts',(-7.76231553900006,15.2,-7.15731120800001));
#279803=CARTESIAN_POINT('Ctrl Pts',(-7.76231553900006,11.6,-7.15731120800001));
#279804=CARTESIAN_POINT('Ctrl Pts',(-7.76345261600006,15.2,-7.15890351600001));
#279805=CARTESIAN_POINT('Ctrl Pts',(-7.76345261600006,11.6,-7.15890351600001));
#279806=CARTESIAN_POINT('Ctrl Pts',(-7.76459238700006,15.2,-7.16050265800002));
#279807=CARTESIAN_POINT('Ctrl Pts',(-7.76459238700006,11.6,-7.16050265800002));
#279808=CARTESIAN_POINT('Ctrl Pts',(-7.76573483200006,15.2,-7.16210862900001));
#279809=CARTESIAN_POINT('Ctrl Pts',(-7.76573483200006,11.6,-7.16210862900001));
#279810=CARTESIAN_POINT('Ctrl Pts',(-7.76687993200006,15.2,-7.16372142100001));
#279811=CARTESIAN_POINT('Ctrl Pts',(-7.76687993200006,11.6,-7.16372142100001));
#279812=CARTESIAN_POINT('Ctrl Pts',(-7.76802767000006,15.2,-7.16534103000001));
#279813=CARTESIAN_POINT('Ctrl Pts',(-7.76802767000006,11.6,-7.16534103000001));
#279814=CARTESIAN_POINT('Ctrl Pts',(-7.76917802700006,15.2,-7.16696745000001));
#279815=CARTESIAN_POINT('Ctrl Pts',(-7.76917802700006,11.6,-7.16696745000001));
#279816=CARTESIAN_POINT('Ctrl Pts',(-7.77033098400005,15.2,-7.16860067400001));
#279817=CARTESIAN_POINT('Ctrl Pts',(-7.77033098400005,11.6,-7.16860067400001));
#279818=CARTESIAN_POINT('Ctrl Pts',(-7.77148652400006,15.2,-7.17024069600001));
#279819=CARTESIAN_POINT('Ctrl Pts',(-7.77148652400006,11.6,-7.17024069600001));
#279820=CARTESIAN_POINT('Ctrl Pts',(-7.77264462900006,15.2,-7.17188751300001));
#279821=CARTESIAN_POINT('Ctrl Pts',(-7.77264462900006,11.6,-7.17188751300001));
#279822=CARTESIAN_POINT('Ctrl Pts',(-7.77380527900006,15.2,-7.17354111600002));
#279823=CARTESIAN_POINT('Ctrl Pts',(-7.77380527900006,11.6,-7.17354111600002));
#279824=CARTESIAN_POINT('Ctrl Pts',(-7.77496845900006,15.2,-7.17520150000002));
#279825=CARTESIAN_POINT('Ctrl Pts',(-7.77496845900006,11.6,-7.17520150000002));
#279826=CARTESIAN_POINT('Ctrl Pts',(-7.77613414800006,15.2,-7.17686866000002));
#279827=CARTESIAN_POINT('Ctrl Pts',(-7.77613414800006,11.6,-7.17686866000002));
#279828=CARTESIAN_POINT('Ctrl Pts',(-7.77730233100005,15.2,-7.17854259000001));
#279829=CARTESIAN_POINT('Ctrl Pts',(-7.77730233100005,11.6,-7.17854259000001));
#279830=CARTESIAN_POINT('Ctrl Pts',(-7.77847298700006,15.2,-7.18022328300002));
#279831=CARTESIAN_POINT('Ctrl Pts',(-7.77847298700006,11.6,-7.18022328300002));
#279832=CARTESIAN_POINT('Ctrl Pts',(-7.77964610100006,15.2,-7.18191073400002));
#279833=CARTESIAN_POINT('Ctrl Pts',(-7.77964610100006,11.6,-7.18191073400002));
#279834=CARTESIAN_POINT('Ctrl Pts',(-7.78082165300006,15.2,-7.18360493900001));
#279835=CARTESIAN_POINT('Ctrl Pts',(-7.78082165300006,11.6,-7.18360493900001));
#279836=CARTESIAN_POINT('Ctrl Pts',(-7.78199962800005,15.2,-7.18530588900002));
#279837=CARTESIAN_POINT('Ctrl Pts',(-7.78199962800005,11.6,-7.18530588900002));
#279838=CARTESIAN_POINT('Ctrl Pts',(-7.78318000600006,15.2,-7.18701358000001));
#279839=CARTESIAN_POINT('Ctrl Pts',(-7.78318000600006,11.6,-7.18701358000001));
#279840=CARTESIAN_POINT('Ctrl Pts',(-7.78436277200005,15.2,-7.18872800600002));
#279841=CARTESIAN_POINT('Ctrl Pts',(-7.78436277200005,11.6,-7.18872800600002));
#279842=CARTESIAN_POINT('Ctrl Pts',(-7.78554790600006,15.2,-7.19044916200002));
#279843=CARTESIAN_POINT('Ctrl Pts',(-7.78554790600006,11.6,-7.19044916200002));
#279844=CARTESIAN_POINT('Ctrl Pts',(-7.78673539200006,15.2,-7.19217704100001));
#279845=CARTESIAN_POINT('Ctrl Pts',(-7.78673539200006,11.6,-7.19217704100001));
#279846=CARTESIAN_POINT('Ctrl Pts',(-7.78792521300005,15.2,-7.19391163700001));
#279847=CARTESIAN_POINT('Ctrl Pts',(-7.78792521300005,11.6,-7.19391163700001));
#279848=CARTESIAN_POINT('Ctrl Pts',(-7.78911735000006,15.2,-7.19565294600002));
#279849=CARTESIAN_POINT('Ctrl Pts',(-7.78911735000006,11.6,-7.19565294600002));
#279850=CARTESIAN_POINT('Ctrl Pts',(-7.79031178800006,15.2,-7.19740096100002));
#279851=CARTESIAN_POINT('Ctrl Pts',(-7.79031178800006,11.6,-7.19740096100002));
#279852=CARTESIAN_POINT('Ctrl Pts',(-7.79150850800006,15.2,-7.19915567700002));
#279853=CARTESIAN_POINT('Ctrl Pts',(-7.79150850800006,11.6,-7.19915567700002));
#279854=CARTESIAN_POINT('Ctrl Pts',(-7.79270749500006,15.2,-7.20091708700001));
#279855=CARTESIAN_POINT('Ctrl Pts',(-7.79270749500006,11.6,-7.20091708700001));
#279856=CARTESIAN_POINT('Ctrl Pts',(-7.79390872900006,15.2,-7.20268518700002));
#279857=CARTESIAN_POINT('Ctrl Pts',(-7.79390872900006,11.6,-7.20268518700002));
#279858=CARTESIAN_POINT('Ctrl Pts',(-7.79511219600005,15.2,-7.20445996900001));
#279859=CARTESIAN_POINT('Ctrl Pts',(-7.79511219600005,11.6,-7.20445996900001));
#279860=CARTESIAN_POINT('Ctrl Pts',(-7.79631787700006,15.2,-7.20624143100002));
#279861=CARTESIAN_POINT('Ctrl Pts',(-7.79631787700006,11.6,-7.20624143100002));
#279862=CARTESIAN_POINT('Ctrl Pts',(-7.79752575600006,15.2,-7.20802956400002));
#279863=CARTESIAN_POINT('Ctrl Pts',(-7.79752575600006,11.6,-7.20802956400002));
#279864=CARTESIAN_POINT('Ctrl Pts',(-7.79873581700006,15.2,-7.20982436300002));
#279865=CARTESIAN_POINT('Ctrl Pts',(-7.79873581700006,11.6,-7.20982436300002));
#279866=CARTESIAN_POINT('Ctrl Pts',(-7.79994804200006,15.2,-7.21162582400002));
#279867=CARTESIAN_POINT('Ctrl Pts',(-7.79994804200006,11.6,-7.21162582400002));
#279868=CARTESIAN_POINT('Ctrl Pts',(-7.80116241500006,15.2,-7.21343393900002));
#279869=CARTESIAN_POINT('Ctrl Pts',(-7.80116241500006,11.6,-7.21343393900002));
#279870=CARTESIAN_POINT('Ctrl Pts',(-7.80237891700006,15.2,-7.21524870400001));
#279871=CARTESIAN_POINT('Ctrl Pts',(-7.80237891700006,11.6,-7.21524870400001));
#279872=CARTESIAN_POINT('Ctrl Pts',(-7.80359753600005,15.2,-7.21707011200002));
#279873=CARTESIAN_POINT('Ctrl Pts',(-7.80359753600005,11.6,-7.21707011200002));
#279874=CARTESIAN_POINT('Ctrl Pts',(-7.80481825200006,15.2,-7.21889815900001));
#279875=CARTESIAN_POINT('Ctrl Pts',(-7.80481825200006,11.6,-7.21889815900001));
#279876=CARTESIAN_POINT('Ctrl Pts',(-7.80604105000006,15.2,-7.22073283800002));
#279877=CARTESIAN_POINT('Ctrl Pts',(-7.80604105000006,11.6,-7.22073283800002));
#279878=CARTESIAN_POINT('Ctrl Pts',(-7.80726591200006,15.2,-7.22257414400002));
#279879=CARTESIAN_POINT('Ctrl Pts',(-7.80726591200006,11.6,-7.22257414400002));
#279880=CARTESIAN_POINT('Ctrl Pts',(-7.80849282300006,15.2,-7.22442207200002));
#279881=CARTESIAN_POINT('Ctrl Pts',(-7.80849282300006,11.6,-7.22442207200002));
#279882=CARTESIAN_POINT('Ctrl Pts',(-7.80972176800006,15.2,-7.22627661400002));
#279883=CARTESIAN_POINT('Ctrl Pts',(-7.80972176800006,11.6,-7.22627661400002));
#279884=CARTESIAN_POINT('Ctrl Pts',(-7.81095272700006,15.2,-7.22813776700002));
#279885=CARTESIAN_POINT('Ctrl Pts',(-7.81095272700006,11.6,-7.22813776700002));
#279886=CARTESIAN_POINT('Ctrl Pts',(-7.81218568800006,15.2,-7.23000552500002));
#279887=CARTESIAN_POINT('Ctrl Pts',(-7.81218568800006,11.6,-7.23000552500002));
#279888=CARTESIAN_POINT('Ctrl Pts',(-7.81342063200006,15.2,-7.23187988100002));
#279889=CARTESIAN_POINT('Ctrl Pts',(-7.81342063200006,11.6,-7.23187988100002));
#279890=CARTESIAN_POINT('Ctrl Pts',(-7.81465754300006,15.2,-7.23376083000002));
#279891=CARTESIAN_POINT('Ctrl Pts',(-7.81465754300006,11.6,-7.23376083000002));
#279892=CARTESIAN_POINT('Ctrl Pts',(-7.81589640700006,15.2,-7.23564836800002));
#279893=CARTESIAN_POINT('Ctrl Pts',(-7.81589640700006,11.6,-7.23564836800002));
#279894=CARTESIAN_POINT('Ctrl Pts',(-7.81713720600005,15.2,-7.23754248800001));
#279895=CARTESIAN_POINT('Ctrl Pts',(-7.81713720600005,11.6,-7.23754248800001));
#279896=CARTESIAN_POINT('Ctrl Pts',(-7.81837992500006,15.2,-7.23944318200001));
#279897=CARTESIAN_POINT('Ctrl Pts',(-7.81837992500006,11.6,-7.23944318200001));
#279898=CARTESIAN_POINT('Ctrl Pts',(-7.81962454700006,15.2,-7.24135045000001));
#279899=CARTESIAN_POINT('Ctrl Pts',(-7.81962454700006,11.6,-7.24135045000001));
#279900=CARTESIAN_POINT('Ctrl Pts',(-7.82087105900005,15.2,-7.24326428200002));
#279901=CARTESIAN_POINT('Ctrl Pts',(-7.82087105900005,11.6,-7.24326428200002));
#279902=CARTESIAN_POINT('Ctrl Pts',(-7.82211944200006,15.2,-7.24518467400002));
#279903=CARTESIAN_POINT('Ctrl Pts',(-7.82211944200006,11.6,-7.24518467400002));
#279904=CARTESIAN_POINT('Ctrl Pts',(-7.82336968300006,15.2,-7.24711161900002));
#279905=CARTESIAN_POINT('Ctrl Pts',(-7.82336968300006,11.6,-7.24711161900002));
#279906=CARTESIAN_POINT('Ctrl Pts',(-7.82462176300006,15.2,-7.24904511400001));
#279907=CARTESIAN_POINT('Ctrl Pts',(-7.82462176300006,11.6,-7.24904511400001));
#279908=CARTESIAN_POINT('Ctrl Pts',(-7.82587566900006,15.2,-7.25098515300001));
#279909=CARTESIAN_POINT('Ctrl Pts',(-7.82587566900006,11.6,-7.25098515300001));
#279910=CARTESIAN_POINT('Ctrl Pts',(-7.82713138500006,15.2,-7.25293172800002));
#279911=CARTESIAN_POINT('Ctrl Pts',(-7.82713138500006,11.6,-7.25293172800002));
#279912=CARTESIAN_POINT('Ctrl Pts',(-7.82838889500006,15.2,-7.25488483600002));
#279913=CARTESIAN_POINT('Ctrl Pts',(-7.82838889500006,11.6,-7.25488483600002));
#279914=CARTESIAN_POINT('Ctrl Pts',(-7.82964818300006,15.2,-7.25684447100001));
#279915=CARTESIAN_POINT('Ctrl Pts',(-7.82964818300006,11.6,-7.25684447100001));
#279916=CARTESIAN_POINT('Ctrl Pts',(-7.83090923600006,15.2,-7.25881062600001));
#279917=CARTESIAN_POINT('Ctrl Pts',(-7.83090923600006,11.6,-7.25881062600001));
#279918=CARTESIAN_POINT('Ctrl Pts',(-7.83217203600006,15.2,-7.26078329800002));
#279919=CARTESIAN_POINT('Ctrl Pts',(-7.83217203600006,11.6,-7.26078329800002));
#279920=CARTESIAN_POINT('Ctrl Pts',(-7.83343656900006,15.2,-7.26276247900002));
#279921=CARTESIAN_POINT('Ctrl Pts',(-7.83343656900006,11.6,-7.26276247900002));
#279922=CARTESIAN_POINT('Ctrl Pts',(-7.83470281800006,15.2,-7.26474816500001));
#279923=CARTESIAN_POINT('Ctrl Pts',(-7.83470281800006,11.6,-7.26474816500001));
#279924=CARTESIAN_POINT('Ctrl Pts',(-7.83597077100006,15.2,-7.26674035100002));
#279925=CARTESIAN_POINT('Ctrl Pts',(-7.83597077100006,11.6,-7.26674035100002));
#279926=CARTESIAN_POINT('Ctrl Pts',(-7.83724040900006,15.2,-7.26873902900002));
#279927=CARTESIAN_POINT('Ctrl Pts',(-7.83724040900006,11.6,-7.26873902900002));
#279928=CARTESIAN_POINT('Ctrl Pts',(-7.83851172000006,15.2,-7.27074419600001));
#279929=CARTESIAN_POINT('Ctrl Pts',(-7.83851172000006,11.6,-7.27074419600001));
#279930=CARTESIAN_POINT('Ctrl Pts',(-7.83978468700005,15.2,-7.27275584500001));
#279931=CARTESIAN_POINT('Ctrl Pts',(-7.83978468700005,11.6,-7.27275584500001));
#279932=CARTESIAN_POINT('Ctrl Pts',(-7.84105929600006,15.2,-7.27477397100002));
#279933=CARTESIAN_POINT('Ctrl Pts',(-7.84105929600006,11.6,-7.27477397100002));
#279934=CARTESIAN_POINT('Ctrl Pts',(-7.84233553200006,15.2,-7.27679857100001));
#279935=CARTESIAN_POINT('Ctrl Pts',(-7.84233553200006,11.6,-7.27679857100001));
#279936=CARTESIAN_POINT('Ctrl Pts',(-7.84361337800006,15.2,-7.27882963500001));
#279937=CARTESIAN_POINT('Ctrl Pts',(-7.84361337800006,11.6,-7.27882963500001));
#279938=CARTESIAN_POINT('Ctrl Pts',(-7.84489282200005,15.2,-7.28086716100002));
#279939=CARTESIAN_POINT('Ctrl Pts',(-7.84489282200005,11.6,-7.28086716100002));
#279940=CARTESIAN_POINT('Ctrl Pts',(-7.84617384900006,15.2,-7.28291114200001));
#279941=CARTESIAN_POINT('Ctrl Pts',(-7.84617384900006,11.6,-7.28291114200001));
#279942=CARTESIAN_POINT('Ctrl Pts',(-7.84745644200005,15.2,-7.28496157300001));
#279943=CARTESIAN_POINT('Ctrl Pts',(-7.84745644200005,11.6,-7.28496157300001));
#279944=CARTESIAN_POINT('Ctrl Pts',(-7.84874058700006,15.2,-7.28701844800002));
#279945=CARTESIAN_POINT('Ctrl Pts',(-7.84874058700006,11.6,-7.28701844800002));
#279946=CARTESIAN_POINT('Ctrl Pts',(-7.85002627100006,15.2,-7.28908176300001));
#279947=CARTESIAN_POINT('Ctrl Pts',(-7.85002627100006,11.6,-7.28908176300001));
#279948=CARTESIAN_POINT('Ctrl Pts',(-7.85131347600006,15.2,-7.29115151100002));
#279949=CARTESIAN_POINT('Ctrl Pts',(-7.85131347600006,11.6,-7.29115151100002));
#279950=CARTESIAN_POINT('Ctrl Pts',(-7.85260219100006,15.2,-7.29322768800002));
#279951=CARTESIAN_POINT('Ctrl Pts',(-7.85260219100006,11.6,-7.29322768800002));
#279952=CARTESIAN_POINT('Ctrl Pts',(-7.85389239900006,15.2,-7.29531028800002));
#279953=CARTESIAN_POINT('Ctrl Pts',(-7.85389239900006,11.6,-7.29531028800002));
#279954=CARTESIAN_POINT('Ctrl Pts',(-7.85518408700005,15.2,-7.29739930400001));
#279955=CARTESIAN_POINT('Ctrl Pts',(-7.85518408700005,11.6,-7.29739930400001));
#279956=CARTESIAN_POINT('Ctrl Pts',(-7.85647723900006,15.2,-7.29949473300002));
#279957=CARTESIAN_POINT('Ctrl Pts',(-7.85647723900006,11.6,-7.29949473300002));
#279958=CARTESIAN_POINT('Ctrl Pts',(-7.85777184100005,15.2,-7.30159656800001));
#279959=CARTESIAN_POINT('Ctrl Pts',(-7.85777184100005,11.6,-7.30159656800001));
#279960=CARTESIAN_POINT('Ctrl Pts',(-7.85906787900006,15.2,-7.30370480400002));
#279961=CARTESIAN_POINT('Ctrl Pts',(-7.85906787900006,11.6,-7.30370480400002));
#279962=CARTESIAN_POINT('Ctrl Pts',(-7.86036533900005,15.2,-7.30581943700002));
#279963=CARTESIAN_POINT('Ctrl Pts',(-7.86036533900005,11.6,-7.30581943700002));
#279964=CARTESIAN_POINT('Ctrl Pts',(-7.86166420600006,15.2,-7.30794046000002));
#279965=CARTESIAN_POINT('Ctrl Pts',(-7.86166420600006,11.6,-7.30794046000002));
#279966=CARTESIAN_POINT('Ctrl Pts',(-7.86296446600005,15.2,-7.31006786700001));
#279967=CARTESIAN_POINT('Ctrl Pts',(-7.86296446600005,11.6,-7.31006786700001));
#279968=CARTESIAN_POINT('Ctrl Pts',(-7.86426610500006,15.2,-7.31220165500002));
#279969=CARTESIAN_POINT('Ctrl Pts',(-7.86426610500006,11.6,-7.31220165500002));
#279970=CARTESIAN_POINT('Ctrl Pts',(-7.86556910800006,15.2,-7.31434181700001));
#279971=CARTESIAN_POINT('Ctrl Pts',(-7.86556910800006,11.6,-7.31434181700001));
#279972=CARTESIAN_POINT('Ctrl Pts',(-7.86687346200006,15.2,-7.31648834800002));
#279973=CARTESIAN_POINT('Ctrl Pts',(-7.86687346200006,11.6,-7.31648834800002));
#279974=CARTESIAN_POINT('Ctrl Pts',(-7.86817915300006,15.2,-7.31864124200002));
#279975=CARTESIAN_POINT('Ctrl Pts',(-7.86817915300006,11.6,-7.31864124200002));
#279976=CARTESIAN_POINT('Ctrl Pts',(-7.86948616400006,15.2,-7.32080049500002));
#279977=CARTESIAN_POINT('Ctrl Pts',(-7.86948616400006,11.6,-7.32080049500002));
#279978=CARTESIAN_POINT('Ctrl Pts',(-7.87079448500006,15.2,-7.32296610000001));
#279979=CARTESIAN_POINT('Ctrl Pts',(-7.87079448500006,11.6,-7.32296610000001));
#279980=CARTESIAN_POINT('Ctrl Pts',(-7.87210409900006,15.2,-7.32513805300002));
#279981=CARTESIAN_POINT('Ctrl Pts',(-7.87210409900006,11.6,-7.32513805300002));
#279982=CARTESIAN_POINT('Ctrl Pts',(-7.87341499400006,15.2,-7.32731634800002));
#279983=CARTESIAN_POINT('Ctrl Pts',(-7.87341499400006,11.6,-7.32731634800002));
#279984=CARTESIAN_POINT('Ctrl Pts',(-7.87472715600006,15.2,-7.32950098000002));
#279985=CARTESIAN_POINT('Ctrl Pts',(-7.87472715600006,11.6,-7.32950098000002));
#279986=CARTESIAN_POINT('Ctrl Pts',(-7.87604057000006,15.2,-7.33169194300002));
#279987=CARTESIAN_POINT('Ctrl Pts',(-7.87604057000006,11.6,-7.33169194300002));
#279988=CARTESIAN_POINT('Ctrl Pts',(-7.87735522200006,15.2,-7.33388923300001));
#279989=CARTESIAN_POINT('Ctrl Pts',(-7.87735522200006,11.6,-7.33388923300001));
#279990=CARTESIAN_POINT('Ctrl Pts',(-7.87867110000006,15.2,-7.33609284300002));
#279991=CARTESIAN_POINT('Ctrl Pts',(-7.87867110000006,11.6,-7.33609284300002));
#279992=CARTESIAN_POINT('Ctrl Pts',(-7.87998818900006,15.2,-7.33830276900001));
#279993=CARTESIAN_POINT('Ctrl Pts',(-7.87998818900006,11.6,-7.33830276900001));
#279994=CARTESIAN_POINT('Ctrl Pts',(-7.88130647600005,15.2,-7.34051900600001));
#279995=CARTESIAN_POINT('Ctrl Pts',(-7.88130647600005,11.6,-7.34051900600001));
#279996=CARTESIAN_POINT('Ctrl Pts',(-7.88262594600005,15.2,-7.34274154700002));
#279997=CARTESIAN_POINT('Ctrl Pts',(-7.88262594600005,11.6,-7.34274154700002));
#279998=CARTESIAN_POINT('Ctrl Pts',(-7.88394658700006,15.2,-7.34497038800002));
#279999=CARTESIAN_POINT('Ctrl Pts',(-7.88394658700006,11.6,-7.34497038800002));
#280000=CARTESIAN_POINT('Ctrl Pts',(-7.88526838500006,15.2,-7.34720552200002));
#280001=CARTESIAN_POINT('Ctrl Pts',(-7.88526838500006,11.6,-7.34720552200002));
#280002=CARTESIAN_POINT('Ctrl Pts',(-7.88659132600006,15.2,-7.34944694700002));
#280003=CARTESIAN_POINT('Ctrl Pts',(-7.88659132600006,11.6,-7.34944694700002));
#280004=CARTESIAN_POINT('Ctrl Pts',(-7.88791539700006,15.2,-7.35169465400002));
#280005=CARTESIAN_POINT('Ctrl Pts',(-7.88791539700006,11.6,-7.35169465400002));
#280006=CARTESIAN_POINT('Ctrl Pts',(-7.88924058300006,15.2,-7.35394864100002));
#280007=CARTESIAN_POINT('Ctrl Pts',(-7.88924058300006,11.6,-7.35394864100002));
#280008=CARTESIAN_POINT('Ctrl Pts',(-7.89056687300006,15.2,-7.35620890000002));
#280009=CARTESIAN_POINT('Ctrl Pts',(-7.89056687300006,11.6,-7.35620890000002));
#280010=CARTESIAN_POINT('Ctrl Pts',(-7.89189425200006,15.2,-7.35847542700002));
#280011=CARTESIAN_POINT('Ctrl Pts',(-7.89189425200006,11.6,-7.35847542700002));
#280012=CARTESIAN_POINT('Ctrl Pts',(-7.89322270800006,15.2,-7.36074821600001));
#280013=CARTESIAN_POINT('Ctrl Pts',(-7.89322270800006,11.6,-7.36074821600001));
#280014=CARTESIAN_POINT('Ctrl Pts',(-7.89455222700005,15.2,-7.36302726400002));
#280015=CARTESIAN_POINT('Ctrl Pts',(-7.89455222700005,11.6,-7.36302726400002));
#280016=CARTESIAN_POINT('Ctrl Pts',(-7.89588279500006,15.2,-7.36531256200001));
#280017=CARTESIAN_POINT('Ctrl Pts',(-7.89588279500006,11.6,-7.36531256200001));
#280018=CARTESIAN_POINT('Ctrl Pts',(-7.89721440000006,15.2,-7.36760410800001));
#280019=CARTESIAN_POINT('Ctrl Pts',(-7.89721440000006,11.6,-7.36760410800001));
#280020=CARTESIAN_POINT('Ctrl Pts',(-7.89854702700006,15.2,-7.36990189500002));
#280021=CARTESIAN_POINT('Ctrl Pts',(-7.89854702700006,11.6,-7.36990189500002));
#280022=CARTESIAN_POINT('Ctrl Pts',(-7.89988066500006,15.2,-7.37220591900002));
#280023=CARTESIAN_POINT('Ctrl Pts',(-7.89988066500006,11.6,-7.37220591900002));
#280024=CARTESIAN_POINT('Ctrl Pts',(-7.90121530100006,15.2,-7.37451617400002));
#280025=CARTESIAN_POINT('Ctrl Pts',(-7.90121530100006,11.6,-7.37451617400002));
#280026=CARTESIAN_POINT('Ctrl Pts',(-7.90255092000006,15.2,-7.37683265400002));
#280027=CARTESIAN_POINT('Ctrl Pts',(-7.90255092000006,11.6,-7.37683265400002));
#280028=CARTESIAN_POINT('Ctrl Pts',(-7.90388750900006,15.2,-7.37915535500001));
#280029=CARTESIAN_POINT('Ctrl Pts',(-7.90388750900006,11.6,-7.37915535500001));
#280030=CARTESIAN_POINT('Ctrl Pts',(-7.90522505700006,15.2,-7.38148427100001));
#280031=CARTESIAN_POINT('Ctrl Pts',(-7.90522505700006,11.6,-7.38148427100001));
#280032=CARTESIAN_POINT('Ctrl Pts',(-7.90656355000006,15.2,-7.38381939700002));
#280033=CARTESIAN_POINT('Ctrl Pts',(-7.90656355000006,11.6,-7.38381939700002));
#280034=CARTESIAN_POINT('Ctrl Pts',(-7.90790297600005,15.2,-7.38616072800002));
#280035=CARTESIAN_POINT('Ctrl Pts',(-7.90790297600005,11.6,-7.38616072800002));
#280036=CARTESIAN_POINT('Ctrl Pts',(-7.90924332000006,15.2,-7.38850825800001));
#280037=CARTESIAN_POINT('Ctrl Pts',(-7.90924332000006,11.6,-7.38850825800001));
#280038=CARTESIAN_POINT('Ctrl Pts',(-7.91058457100006,15.2,-7.39086198300001));
#280039=CARTESIAN_POINT('Ctrl Pts',(-7.91058457100006,11.6,-7.39086198300001));
#280040=CARTESIAN_POINT('Ctrl Pts',(-7.91192671500006,15.2,-7.39322189600002));
#280041=CARTESIAN_POINT('Ctrl Pts',(-7.91192671500006,11.6,-7.39322189600002));
#280042=CARTESIAN_POINT('Ctrl Pts',(-7.91326974000006,15.2,-7.39558799400001));
#280043=CARTESIAN_POINT('Ctrl Pts',(-7.91326974000006,11.6,-7.39558799400001));
#280044=CARTESIAN_POINT('Ctrl Pts',(-7.91461363300006,15.2,-7.39796027100001));
#280045=CARTESIAN_POINT('Ctrl Pts',(-7.91461363300006,11.6,-7.39796027100001));
#280046=CARTESIAN_POINT('Ctrl Pts',(-7.91595838200006,15.2,-7.40033872100001));
#280047=CARTESIAN_POINT('Ctrl Pts',(-7.91595838200006,11.6,-7.40033872100001));
#280048=CARTESIAN_POINT('Ctrl Pts',(-7.91730397300006,15.2,-7.40272333900001));
#280049=CARTESIAN_POINT('Ctrl Pts',(-7.91730397300006,11.6,-7.40272333900001));
#280050=CARTESIAN_POINT('Ctrl Pts',(-7.91865039500006,15.2,-7.40511412000001));
#280051=CARTESIAN_POINT('Ctrl Pts',(-7.91865039500006,11.6,-7.40511412000001));
#280052=CARTESIAN_POINT('Ctrl Pts',(-7.91999763300005,15.2,-7.40751106000002));
#280053=CARTESIAN_POINT('Ctrl Pts',(-7.91999763300005,11.6,-7.40751106000002));
#280054=CARTESIAN_POINT('Ctrl Pts',(-7.92134567800005,15.2,-7.40991415100002));
#280055=CARTESIAN_POINT('Ctrl Pts',(-7.92134567800005,11.6,-7.40991415100002));
#280056=CARTESIAN_POINT('Ctrl Pts',(-7.92269451400006,15.2,-7.41232339000002));
#280057=CARTESIAN_POINT('Ctrl Pts',(-7.92269451400006,11.6,-7.41232339000002));
#280058=CARTESIAN_POINT('Ctrl Pts',(-7.92404413000006,15.2,-7.41473877200002));
#280059=CARTESIAN_POINT('Ctrl Pts',(-7.92404413000006,11.6,-7.41473877200002));
#280060=CARTESIAN_POINT('Ctrl Pts',(-7.92539451300006,15.2,-7.41716029100001));
#280061=CARTESIAN_POINT('Ctrl Pts',(-7.92539451300006,11.6,-7.41716029100001));
#280062=CARTESIAN_POINT('Ctrl Pts',(-7.92674565300005,15.2,-7.41958794100002));
#280063=CARTESIAN_POINT('Ctrl Pts',(-7.92674565300005,11.6,-7.41958794100002));
#280064=CARTESIAN_POINT('Ctrl Pts',(-7.92809753400006,15.2,-7.42202171900002));
#280065=CARTESIAN_POINT('Ctrl Pts',(-7.92809753400006,11.6,-7.42202171900002));
#280066=CARTESIAN_POINT('Ctrl Pts',(-7.92945014600006,15.2,-7.42446161800002));
#280067=CARTESIAN_POINT('Ctrl Pts',(-7.92945014600006,11.6,-7.42446161800002));
#280068=CARTESIAN_POINT('Ctrl Pts',(-7.93080347700006,15.2,-7.42690763300001));
#280069=CARTESIAN_POINT('Ctrl Pts',(-7.93080347700006,11.6,-7.42690763300001));
#280070=CARTESIAN_POINT('Ctrl Pts',(-7.93215751200006,15.2,-7.42935976000001));
#280071=CARTESIAN_POINT('Ctrl Pts',(-7.93215751200006,11.6,-7.42935976000001));
#280072=CARTESIAN_POINT('Ctrl Pts',(-7.93351224100006,15.2,-7.43181799300002));
#280073=CARTESIAN_POINT('Ctrl Pts',(-7.93351224100006,11.6,-7.43181799300002));
#280074=CARTESIAN_POINT('Ctrl Pts',(-7.93486765300005,15.2,-7.43428232700002));
#280075=CARTESIAN_POINT('Ctrl Pts',(-7.93486765300005,11.6,-7.43428232700002));
#280076=CARTESIAN_POINT('Ctrl Pts',(-7.93622373300006,15.2,-7.43675275700002));
#280077=CARTESIAN_POINT('Ctrl Pts',(-7.93622373300006,11.6,-7.43675275700002));
#280078=CARTESIAN_POINT('Ctrl Pts',(-7.93758046900006,15.2,-7.43922927700002));
#280079=CARTESIAN_POINT('Ctrl Pts',(-7.93758046900006,11.6,-7.43922927700002));
#280080=CARTESIAN_POINT('Ctrl Pts',(-7.93893785100006,15.2,-7.44171188300002));
#280081=CARTESIAN_POINT('Ctrl Pts',(-7.93893785100006,11.6,-7.44171188300002));
#280082=CARTESIAN_POINT('Ctrl Pts',(-7.94029586500006,15.2,-7.44420056900001));
#280083=CARTESIAN_POINT('Ctrl Pts',(-7.94029586500006,11.6,-7.44420056900001));
#280084=CARTESIAN_POINT('Ctrl Pts',(-7.94165450000006,15.2,-7.44669533000001));
#280085=CARTESIAN_POINT('Ctrl Pts',(-7.94165450000006,11.6,-7.44669533000001));
#280086=CARTESIAN_POINT('Ctrl Pts',(-7.94301374500006,15.2,-7.44919616200002));
#280087=CARTESIAN_POINT('Ctrl Pts',(-7.94301374500006,11.6,-7.44919616200002));
#280088=CARTESIAN_POINT('Ctrl Pts',(-7.94437358600005,15.2,-7.45170305800002));
#280089=CARTESIAN_POINT('Ctrl Pts',(-7.94437358600005,11.6,-7.45170305800002));
#280090=CARTESIAN_POINT('Ctrl Pts',(-7.94573401200006,15.2,-7.45421601400002));
#280091=CARTESIAN_POINT('Ctrl Pts',(-7.94573401200006,11.6,-7.45421601400002));
#280092=CARTESIAN_POINT('Ctrl Pts',(-7.94709501100006,15.2,-7.45673502500001));
#280093=CARTESIAN_POINT('Ctrl Pts',(-7.94709501100006,11.6,-7.45673502500001));
#280094=CARTESIAN_POINT('Ctrl Pts',(-7.94845657000005,15.2,-7.45926008500001));
#280095=CARTESIAN_POINT('Ctrl Pts',(-7.94845657000005,11.6,-7.45926008500001));
#280096=CARTESIAN_POINT('Ctrl Pts',(-7.94981868000006,15.2,-7.46179119000002));
#280097=CARTESIAN_POINT('Ctrl Pts',(-7.94981868000006,11.6,-7.46179119000002));
#280098=CARTESIAN_POINT('Ctrl Pts',(-7.95118132600006,15.2,-7.46432833400001));
#280099=CARTESIAN_POINT('Ctrl Pts',(-7.95118132600006,11.6,-7.46432833400001));
#280100=CARTESIAN_POINT('Ctrl Pts',(-7.95254449800006,15.2,-7.46687151200002));
#280101=CARTESIAN_POINT('Ctrl Pts',(-7.95254449800006,11.6,-7.46687151200002));
#280102=CARTESIAN_POINT('Ctrl Pts',(-7.95390818400006,15.2,-7.46942072000002));
#280103=CARTESIAN_POINT('Ctrl Pts',(-7.95390818400006,11.6,-7.46942072000002));
#280104=CARTESIAN_POINT('Ctrl Pts',(-7.95527237200006,15.2,-7.47197595100002));
#280105=CARTESIAN_POINT('Ctrl Pts',(-7.95527237200006,11.6,-7.47197595100002));
#280106=CARTESIAN_POINT('Ctrl Pts',(-7.95663705000005,15.2,-7.47453720100002));
#280107=CARTESIAN_POINT('Ctrl Pts',(-7.95663705000005,11.6,-7.47453720100002));
#280108=CARTESIAN_POINT('Ctrl Pts',(-7.95800220700006,15.2,-7.47710446400002));
#280109=CARTESIAN_POINT('Ctrl Pts',(-7.95800220700006,11.6,-7.47710446400002));
#280110=CARTESIAN_POINT('Ctrl Pts',(-7.95936783200006,15.2,-7.47967773800001));
#280111=CARTESIAN_POINT('Ctrl Pts',(-7.95936783200006,11.6,-7.47967773800001));
#280112=CARTESIAN_POINT('Ctrl Pts',(-7.96073391200006,15.2,-7.48225701400001));
#280113=CARTESIAN_POINT('Ctrl Pts',(-7.96073391200006,11.6,-7.48225701400001));
#280114=CARTESIAN_POINT('Ctrl Pts',(-7.96210043600006,15.2,-7.48484228900002));
#280115=CARTESIAN_POINT('Ctrl Pts',(-7.96210043600006,11.6,-7.48484228900002));
#280116=CARTESIAN_POINT('Ctrl Pts',(-7.96346739300006,15.2,-7.48743355600002));
#280117=CARTESIAN_POINT('Ctrl Pts',(-7.96346739300006,11.6,-7.48743355600002));
#280118=CARTESIAN_POINT('Ctrl Pts',(-7.96483477000006,15.2,-7.49003081400001));
#280119=CARTESIAN_POINT('Ctrl Pts',(-7.96483477000006,11.6,-7.49003081400001));
#280120=CARTESIAN_POINT('Ctrl Pts',(-7.96620255700006,15.2,-7.49263405300002));
#280121=CARTESIAN_POINT('Ctrl Pts',(-7.96620255700006,11.6,-7.49263405300002));
#280122=CARTESIAN_POINT('Ctrl Pts',(-7.96757074100006,15.2,-7.49524327100002));
#280123=CARTESIAN_POINT('Ctrl Pts',(-7.96757074100006,11.6,-7.49524327100002));
#280124=CARTESIAN_POINT('Ctrl Pts',(-7.96893931300006,15.2,-7.49785846200002));
#280125=CARTESIAN_POINT('Ctrl Pts',(-7.96893931300006,11.6,-7.49785846200002));
#280126=CARTESIAN_POINT('Ctrl Pts',(-7.97030826000006,15.2,-7.50047962100002));
#280127=CARTESIAN_POINT('Ctrl Pts',(-7.97030826000006,11.6,-7.50047962100002));
#280128=CARTESIAN_POINT('Ctrl Pts',(-7.97167757100006,15.2,-7.50310674200002));
#280129=CARTESIAN_POINT('Ctrl Pts',(-7.97167757100006,11.6,-7.50310674200002));
#280130=CARTESIAN_POINT('Ctrl Pts',(-7.97304723400006,15.2,-7.50573982200001));
#280131=CARTESIAN_POINT('Ctrl Pts',(-7.97304723400006,11.6,-7.50573982200001));
#280132=CARTESIAN_POINT('Ctrl Pts',(-7.97441723900005,15.2,-7.50837885600002));
#280133=CARTESIAN_POINT('Ctrl Pts',(-7.97441723900005,11.6,-7.50837885600002));
#280134=CARTESIAN_POINT('Ctrl Pts',(-7.97578757400006,15.2,-7.51102383600001));
#280135=CARTESIAN_POINT('Ctrl Pts',(-7.97578757400006,11.6,-7.51102383600001));
#280136=CARTESIAN_POINT('Ctrl Pts',(-7.97715822700006,15.2,-7.51367475900001));
#280137=CARTESIAN_POINT('Ctrl Pts',(-7.97715822700006,11.6,-7.51367475900001));
#280138=CARTESIAN_POINT('Ctrl Pts',(-7.97852918800006,15.2,-7.51633161900001));
#280139=CARTESIAN_POINT('Ctrl Pts',(-7.97852918800006,11.6,-7.51633161900001));
#280140=CARTESIAN_POINT('Ctrl Pts',(-7.97990044600006,15.2,-7.51899441200001));
#280141=CARTESIAN_POINT('Ctrl Pts',(-7.97990044600006,11.6,-7.51899441200001));
#280142=CARTESIAN_POINT('Ctrl Pts',(-7.98127198900006,15.2,-7.52166313300001));
#280143=CARTESIAN_POINT('Ctrl Pts',(-7.98127198900006,11.6,-7.52166313300001));
#280144=CARTESIAN_POINT('Ctrl Pts',(-7.98264380500005,15.2,-7.52433777700002));
#280145=CARTESIAN_POINT('Ctrl Pts',(-7.98264380500005,11.6,-7.52433777700002));
#280146=CARTESIAN_POINT('Ctrl Pts',(-7.98401588500005,15.2,-7.52701833700002));
#280147=CARTESIAN_POINT('Ctrl Pts',(-7.98401588500005,11.6,-7.52701833700002));
#280148=CARTESIAN_POINT('Ctrl Pts',(-7.98538821700006,15.2,-7.52970480900002));
#280149=CARTESIAN_POINT('Ctrl Pts',(-7.98538821700006,11.6,-7.52970480900002));
#280150=CARTESIAN_POINT('Ctrl Pts',(-7.98676079000006,15.2,-7.53239719000002));
#280151=CARTESIAN_POINT('Ctrl Pts',(-7.98676079000006,11.6,-7.53239719000002));
#280152=CARTESIAN_POINT('Ctrl Pts',(-7.98813359300006,15.2,-7.53509547300002));
#280153=CARTESIAN_POINT('Ctrl Pts',(-7.98813359300006,11.6,-7.53509547300002));
#280154=CARTESIAN_POINT('Ctrl Pts',(-7.98950661400006,15.2,-7.53779965300001));
#280155=CARTESIAN_POINT('Ctrl Pts',(-7.98950661400006,11.6,-7.53779965300001));
#280156=CARTESIAN_POINT('Ctrl Pts',(-7.99087984500006,15.2,-7.54050972600002));
#280157=CARTESIAN_POINT('Ctrl Pts',(-7.99087984500006,11.6,-7.54050972600002));
#280158=CARTESIAN_POINT('Ctrl Pts',(-7.99225327200006,15.2,-7.54322568500001));
#280159=CARTESIAN_POINT('Ctrl Pts',(-7.99225327200006,11.6,-7.54322568500001));
#280160=CARTESIAN_POINT('Ctrl Pts',(-7.99362688500005,15.2,-7.54594752700001));
#280161=CARTESIAN_POINT('Ctrl Pts',(-7.99362688500005,11.6,-7.54594752700001));
#280162=CARTESIAN_POINT('Ctrl Pts',(-7.99500067400006,15.2,-7.54867524600002));
#280163=CARTESIAN_POINT('Ctrl Pts',(-7.99500067400006,11.6,-7.54867524600002));
#280164=CARTESIAN_POINT('Ctrl Pts',(-7.99637462700005,15.2,-7.55140883700002));
#280165=CARTESIAN_POINT('Ctrl Pts',(-7.99637462700005,11.6,-7.55140883700002));
#280166=CARTESIAN_POINT('Ctrl Pts',(-7.99774873400006,15.2,-7.55414829500002));
#280167=CARTESIAN_POINT('Ctrl Pts',(-7.99774873400006,11.6,-7.55414829500002));
#280168=CARTESIAN_POINT('Ctrl Pts',(-7.99912298400006,15.2,-7.55689361500002));
#280169=CARTESIAN_POINT('Ctrl Pts',(-7.99912298400006,11.6,-7.55689361500002));
#280170=CARTESIAN_POINT('Ctrl Pts',(-8.00049736600006,15.2,-7.55964479300002));
#280171=CARTESIAN_POINT('Ctrl Pts',(-8.00049736600006,11.6,-7.55964479300002));
#280172=CARTESIAN_POINT('Ctrl Pts',(-8.00187187000006,15.2,-7.56240182300001));
#280173=CARTESIAN_POINT('Ctrl Pts',(-8.00187187000006,11.6,-7.56240182300001));
#280174=CARTESIAN_POINT('Ctrl Pts',(-8.00324648500006,15.2,-7.56516470000002));
#280175=CARTESIAN_POINT('Ctrl Pts',(-8.00324648500006,11.6,-7.56516470000002));
#280176=CARTESIAN_POINT('Ctrl Pts',(-8.00462120000006,15.2,-7.56793341800002));
#280177=CARTESIAN_POINT('Ctrl Pts',(-8.00462120000006,11.6,-7.56793341800002));
#280178=CARTESIAN_POINT('Ctrl Pts',(-8.00599600400006,15.2,-7.57070797400001));
#280179=CARTESIAN_POINT('Ctrl Pts',(-8.00599600400006,11.6,-7.57070797400001));
#280180=CARTESIAN_POINT('Ctrl Pts',(-8.00737088600006,15.2,-7.57348836200002));
#280181=CARTESIAN_POINT('Ctrl Pts',(-8.00737088600006,11.6,-7.57348836200002));
#280182=CARTESIAN_POINT('Ctrl Pts',(-8.00874583800006,15.2,-7.57627457800002));
#280183=CARTESIAN_POINT('Ctrl Pts',(-8.00874583800006,11.6,-7.57627457800002));
#280184=CARTESIAN_POINT('Ctrl Pts',(-8.01012084800006,15.2,-7.57906661500002));
#280185=CARTESIAN_POINT('Ctrl Pts',(-8.01012084800006,11.6,-7.57906661500002));
#280186=CARTESIAN_POINT('Ctrl Pts',(-8.01149590400006,15.2,-7.58186447000002));
#280187=CARTESIAN_POINT('Ctrl Pts',(-8.01149590400006,11.6,-7.58186447000002));
#280188=CARTESIAN_POINT('Ctrl Pts',(-8.01287099700006,15.2,-7.58466813700001));
#280189=CARTESIAN_POINT('Ctrl Pts',(-8.01287099700006,11.6,-7.58466813700001));
#280190=CARTESIAN_POINT('Ctrl Pts',(-8.01424611600006,15.2,-7.58747761000001));
#280191=CARTESIAN_POINT('Ctrl Pts',(-8.01424611600006,11.6,-7.58747761000001));
#280192=CARTESIAN_POINT('Ctrl Pts',(-8.01562125100006,15.2,-7.59029288600002));
#280193=CARTESIAN_POINT('Ctrl Pts',(-8.01562125100006,11.6,-7.59029288600002));
#280194=CARTESIAN_POINT('Ctrl Pts',(-8.01699639200006,15.2,-7.59311396000002));
#280195=CARTESIAN_POINT('Ctrl Pts',(-8.01699639200006,11.6,-7.59311396000002));
#280196=CARTESIAN_POINT('Ctrl Pts',(-8.01837152700006,15.2,-7.59594082500002));
#280197=CARTESIAN_POINT('Ctrl Pts',(-8.01837152700006,11.6,-7.59594082500002));
#280198=CARTESIAN_POINT('Ctrl Pts',(-8.01974664600005,15.2,-7.59877347800002));
#280199=CARTESIAN_POINT('Ctrl Pts',(-8.01974664600005,11.6,-7.59877347800002));
#280200=CARTESIAN_POINT('Ctrl Pts',(-8.02112174100006,15.2,-7.60161191300002));
#280201=CARTESIAN_POINT('Ctrl Pts',(-8.02112174100006,11.6,-7.60161191300002));
#280202=CARTESIAN_POINT('Ctrl Pts',(-8.02249679900006,15.2,-7.60445612600002));
#280203=CARTESIAN_POINT('Ctrl Pts',(-8.02249679900006,11.6,-7.60445612600002));
#280204=CARTESIAN_POINT('Ctrl Pts',(-8.02387181100006,15.2,-7.60730611100002));
#280205=CARTESIAN_POINT('Ctrl Pts',(-8.02387181100006,11.6,-7.60730611100002));
#280206=CARTESIAN_POINT('Ctrl Pts',(-8.02524676500006,15.2,-7.61016186300001));
#280207=CARTESIAN_POINT('Ctrl Pts',(-8.02524676500006,11.6,-7.61016186300001));
#280208=CARTESIAN_POINT('Ctrl Pts',(-8.02662165400006,15.2,-7.61302337700001));
#280209=CARTESIAN_POINT('Ctrl Pts',(-8.02662165400006,11.6,-7.61302337700001));
#280210=CARTESIAN_POINT('Ctrl Pts',(-8.02799646500005,15.2,-7.61589064900001));
#280211=CARTESIAN_POINT('Ctrl Pts',(-8.02799646500005,11.6,-7.61589064900001));
#280212=CARTESIAN_POINT('Ctrl Pts',(-8.02937118700006,15.2,-7.61876367400002));
#280213=CARTESIAN_POINT('Ctrl Pts',(-8.02937118700006,11.6,-7.61876367400002));
#280214=CARTESIAN_POINT('Ctrl Pts',(-8.03074581300006,15.2,-7.62164244600001));
#280215=CARTESIAN_POINT('Ctrl Pts',(-8.03074581300006,11.6,-7.62164244600001));
#280216=CARTESIAN_POINT('Ctrl Pts',(-8.03212033200005,15.2,-7.62452696000001));
#280217=CARTESIAN_POINT('Ctrl Pts',(-8.03212033200005,11.6,-7.62452696000001));
#280218=CARTESIAN_POINT('Ctrl Pts',(-8.03349473300005,15.2,-7.62741721300002));
#280219=CARTESIAN_POINT('Ctrl Pts',(-8.03349473300005,11.6,-7.62741721300002));
#280220=CARTESIAN_POINT('Ctrl Pts',(-8.03486900600006,15.2,-7.63031319800002));
#280221=CARTESIAN_POINT('Ctrl Pts',(-8.03486900600006,11.6,-7.63031319800002));
#280222=CARTESIAN_POINT('Ctrl Pts',(-8.03624314100006,15.2,-7.63321491200001));
#280223=CARTESIAN_POINT('Ctrl Pts',(-8.03624314100006,11.6,-7.63321491200001));
#280224=CARTESIAN_POINT('Ctrl Pts',(-8.03761712700006,15.2,-7.63612234800001));
#280225=CARTESIAN_POINT('Ctrl Pts',(-8.03761712700006,11.6,-7.63612234800001));
#280226=CARTESIAN_POINT('Ctrl Pts',(-8.03899095600006,15.2,-7.63903550000002));
#280227=CARTESIAN_POINT('Ctrl Pts',(-8.03899095600006,11.6,-7.63903550000002));
#280228=CARTESIAN_POINT('Ctrl Pts',(-8.04036461700005,15.2,-7.64195436700002));
#280229=CARTESIAN_POINT('Ctrl Pts',(-8.04036461700005,11.6,-7.64195436700002));
#280230=CARTESIAN_POINT('Ctrl Pts',(-8.04173810000006,15.2,-7.64487894200002));
#280231=CARTESIAN_POINT('Ctrl Pts',(-8.04173810000006,11.6,-7.64487894200002));
#280232=CARTESIAN_POINT('Ctrl Pts',(-8.04311139500006,15.2,-7.64780921900002));
#280233=CARTESIAN_POINT('Ctrl Pts',(-8.04311139500006,11.6,-7.64780921900002));
#280234=CARTESIAN_POINT('Ctrl Pts',(-8.04448449200006,15.2,-7.65074519500001));
#280235=CARTESIAN_POINT('Ctrl Pts',(-8.04448449200006,11.6,-7.65074519500001));
#280236=CARTESIAN_POINT('Ctrl Pts',(-8.04585738100006,15.2,-7.65368686400001));
#280237=CARTESIAN_POINT('Ctrl Pts',(-8.04585738100006,11.6,-7.65368686400001));
#280238=CARTESIAN_POINT('Ctrl Pts',(-8.04723005200006,15.2,-7.65663422200002));
#280239=CARTESIAN_POINT('Ctrl Pts',(-8.04723005200006,11.6,-7.65663422200002));
#280240=CARTESIAN_POINT('Ctrl Pts',(-8.04860249700006,15.2,-7.65958726300001));
#280241=CARTESIAN_POINT('Ctrl Pts',(-8.04860249700006,11.6,-7.65958726300001));
#280242=CARTESIAN_POINT('Ctrl Pts',(-8.04997470400006,15.2,-7.66254598200002));
#280243=CARTESIAN_POINT('Ctrl Pts',(-8.04997470400006,11.6,-7.66254598200002));
#280244=CARTESIAN_POINT('Ctrl Pts',(-8.05134666400006,15.2,-7.66551037400002));
#280245=CARTESIAN_POINT('Ctrl Pts',(-8.05134666400006,11.6,-7.66551037400002));
#280246=CARTESIAN_POINT('Ctrl Pts',(-8.05271836600006,15.2,-7.66848043600002));
#280247=CARTESIAN_POINT('Ctrl Pts',(-8.05271836600006,11.6,-7.66848043600002));
#280248=CARTESIAN_POINT('Ctrl Pts',(-8.05408980300006,15.2,-7.67145616100001));
#280249=CARTESIAN_POINT('Ctrl Pts',(-8.05408980300006,11.6,-7.67145616100001));
#280250=CARTESIAN_POINT('Ctrl Pts',(-8.05546096300005,15.2,-7.67443754500002));
#280251=CARTESIAN_POINT('Ctrl Pts',(-8.05546096300005,11.6,-7.67443754500002));
#280252=CARTESIAN_POINT('Ctrl Pts',(-8.05683183700006,15.2,-7.67742458300001));
#280253=CARTESIAN_POINT('Ctrl Pts',(-8.05683183700006,11.6,-7.67742458300001));
#280254=CARTESIAN_POINT('Ctrl Pts',(-8.05820241600006,15.2,-7.68041726900002));
#280255=CARTESIAN_POINT('Ctrl Pts',(-8.05820241600006,11.6,-7.68041726900002));
#280256=CARTESIAN_POINT('Ctrl Pts',(-8.05957268800006,15.2,-7.68341560100002));
#280257=CARTESIAN_POINT('Ctrl Pts',(-8.05957268800006,11.6,-7.68341560100002));
#280258=CARTESIAN_POINT('Ctrl Pts',(-8.06094264600006,15.2,-7.68641957000002));
#280259=CARTESIAN_POINT('Ctrl Pts',(-8.06094264600006,11.6,-7.68641957000002));
#280260=CARTESIAN_POINT('Ctrl Pts',(-8.06231227900006,15.2,-7.68942917500001));
#280261=CARTESIAN_POINT('Ctrl Pts',(-8.06231227900006,11.6,-7.68942917500001));
#280262=CARTESIAN_POINT('Ctrl Pts',(-8.06368157800006,15.2,-7.69244440900002));
#280263=CARTESIAN_POINT('Ctrl Pts',(-8.06368157800006,11.6,-7.69244440900002));
#280264=CARTESIAN_POINT('Ctrl Pts',(-8.06505053200006,15.2,-7.69546526700001));
#280265=CARTESIAN_POINT('Ctrl Pts',(-8.06505053200006,11.6,-7.69546526700001));
#280266=CARTESIAN_POINT('Ctrl Pts',(-8.06641913400006,15.2,-7.69849174400001));
#280267=CARTESIAN_POINT('Ctrl Pts',(-8.06641913400006,11.6,-7.69849174400001));
#280268=CARTESIAN_POINT('Ctrl Pts',(-8.06778737300006,15.2,-7.70152383700001));
#280269=CARTESIAN_POINT('Ctrl Pts',(-8.06778737300006,11.6,-7.70152383700001));
#280270=CARTESIAN_POINT('Ctrl Pts',(-8.06915523900006,15.2,-7.70456153800002));
#280271=CARTESIAN_POINT('Ctrl Pts',(-8.06915523900006,11.6,-7.70456153800002));
#280272=CARTESIAN_POINT('Ctrl Pts',(-8.07052272400006,15.2,-7.70760484600002));
#280273=CARTESIAN_POINT('Ctrl Pts',(-8.07052272400006,11.6,-7.70760484600002));
#280274=CARTESIAN_POINT('Ctrl Pts',(-8.07188981800006,15.2,-7.71065375300001));
#280275=CARTESIAN_POINT('Ctrl Pts',(-8.07188981800006,11.6,-7.71065375300001));
#280276=CARTESIAN_POINT('Ctrl Pts',(-8.07325651000006,15.2,-7.71370825500002));
#280277=CARTESIAN_POINT('Ctrl Pts',(-8.07325651000006,11.6,-7.71370825500002));
#280278=CARTESIAN_POINT('Ctrl Pts',(-8.07462279200006,15.2,-7.71676834700001));
#280279=CARTESIAN_POINT('Ctrl Pts',(-8.07462279200006,11.6,-7.71676834700001));
#280280=CARTESIAN_POINT('Ctrl Pts',(-8.07598865500006,15.2,-7.71983402500001));
#280281=CARTESIAN_POINT('Ctrl Pts',(-8.07598865500006,11.6,-7.71983402500001));
#280282=CARTESIAN_POINT('Ctrl Pts',(-8.07735408800006,15.2,-7.72290528300001));
#280283=CARTESIAN_POINT('Ctrl Pts',(-8.07735408800006,11.6,-7.72290528300001));
#280284=CARTESIAN_POINT('Ctrl Pts',(-8.07871908400006,15.2,-7.72598211700001));
#280285=CARTESIAN_POINT('Ctrl Pts',(-8.07871908400006,11.6,-7.72598211700001));
#280286=CARTESIAN_POINT('Ctrl Pts',(-8.08008363200006,15.2,-7.72906452200001));
#280287=CARTESIAN_POINT('Ctrl Pts',(-8.08008363200006,11.6,-7.72906452200001));
#280288=CARTESIAN_POINT('Ctrl Pts',(-8.08144772300006,15.2,-7.73215249200002));
#280289=CARTESIAN_POINT('Ctrl Pts',(-8.08144772300006,11.6,-7.73215249200002));
#280290=CARTESIAN_POINT('Ctrl Pts',(-8.08281134800006,15.2,-7.73524602300002));
#280291=CARTESIAN_POINT('Ctrl Pts',(-8.08281134800006,11.6,-7.73524602300002));
#280292=CARTESIAN_POINT('Ctrl Pts',(-8.08417449700006,15.2,-7.73834511200001));
#280293=CARTESIAN_POINT('Ctrl Pts',(-8.08417449700006,11.6,-7.73834511200001));
#280294=CARTESIAN_POINT('Ctrl Pts',(-8.08553716200005,15.2,-7.74144975000001));
#280295=CARTESIAN_POINT('Ctrl Pts',(-8.08553716200005,11.6,-7.74144975000001));
#280296=CARTESIAN_POINT('Ctrl Pts',(-8.08689933300006,15.2,-7.74455993500001));
#280297=CARTESIAN_POINT('Ctrl Pts',(-8.08689933300006,11.6,-7.74455993500001));
#280298=CARTESIAN_POINT('Ctrl Pts',(-8.08826100100006,15.2,-7.74767566300002));
#280299=CARTESIAN_POINT('Ctrl Pts',(-8.08826100100006,11.6,-7.74767566300002));
#280300=CARTESIAN_POINT('Ctrl Pts',(-8.08962215600006,15.2,-7.75079692600002));
#280301=CARTESIAN_POINT('Ctrl Pts',(-8.08962215600006,11.6,-7.75079692600002));
#280302=CARTESIAN_POINT('Ctrl Pts',(-8.09098279100006,15.2,-7.75392372200002));
#280303=CARTESIAN_POINT('Ctrl Pts',(-8.09098279100006,11.6,-7.75392372200002));
#280304=CARTESIAN_POINT('Ctrl Pts',(-8.09234289500005,15.2,-7.75705604400001));
#280305=CARTESIAN_POINT('Ctrl Pts',(-8.09234289500005,11.6,-7.75705604400001));
#280306=CARTESIAN_POINT('Ctrl Pts',(-8.09370246000006,15.2,-7.76019388800002));
#280307=CARTESIAN_POINT('Ctrl Pts',(-8.09370246000006,11.6,-7.76019388800002));
#280308=CARTESIAN_POINT('Ctrl Pts',(-8.09506147400005,15.2,-7.76333725000002));
#280309=CARTESIAN_POINT('Ctrl Pts',(-8.09506147400005,11.6,-7.76333725000002));
#280310=CARTESIAN_POINT('Ctrl Pts',(-8.09641993300006,15.2,-7.76648612400002));
#280311=CARTESIAN_POINT('Ctrl Pts',(-8.09641993300006,11.6,-7.76648612400002));
#280312=CARTESIAN_POINT('Ctrl Pts',(-8.09777782400005,15.2,-7.76964050600002));
#280313=CARTESIAN_POINT('Ctrl Pts',(-8.09777782400005,11.6,-7.76964050600002));
#280314=CARTESIAN_POINT('Ctrl Pts',(-8.09913513900005,15.2,-7.77280039000001));
#280315=CARTESIAN_POINT('Ctrl Pts',(-8.09913513900005,11.6,-7.77280039000001));
#280316=CARTESIAN_POINT('Ctrl Pts',(-8.10049186900006,15.2,-7.77596577200002));
#280317=CARTESIAN_POINT('Ctrl Pts',(-8.10049186900006,11.6,-7.77596577200002));
#280318=CARTESIAN_POINT('Ctrl Pts',(-8.10184800600006,15.2,-7.77913664800002));
#280319=CARTESIAN_POINT('Ctrl Pts',(-8.10184800600006,11.6,-7.77913664800002));
#280320=CARTESIAN_POINT('Ctrl Pts',(-8.10320354000006,15.2,-7.78231301200002));
#280321=CARTESIAN_POINT('Ctrl Pts',(-8.10320354000006,11.6,-7.78231301200002));
#280322=CARTESIAN_POINT('Ctrl Pts',(-8.10455846200006,15.2,-7.78549485800001));
#280323=CARTESIAN_POINT('Ctrl Pts',(-8.10455846200006,11.6,-7.78549485800001));
#280324=CARTESIAN_POINT('Ctrl Pts',(-8.10591276400006,15.2,-7.78868218400002));
#280325=CARTESIAN_POINT('Ctrl Pts',(-8.10591276400006,11.6,-7.78868218400002));
#280326=CARTESIAN_POINT('Ctrl Pts',(-8.10726643600006,15.2,-7.79187498200002));
#280327=CARTESIAN_POINT('Ctrl Pts',(-8.10726643600006,11.6,-7.79187498200002));
#280328=CARTESIAN_POINT('Ctrl Pts',(-8.10861947000006,15.2,-7.79507325000001));
#280329=CARTESIAN_POINT('Ctrl Pts',(-8.10861947000006,11.6,-7.79507325000001));
#280330=CARTESIAN_POINT('Ctrl Pts',(-8.10997185700005,15.2,-7.79827698300001));
#280331=CARTESIAN_POINT('Ctrl Pts',(-8.10997185700005,11.6,-7.79827698300001));
#280332=CARTESIAN_POINT('Ctrl Pts',(-8.11132358700006,15.2,-7.80148617400001));
#280333=CARTESIAN_POINT('Ctrl Pts',(-8.11132358700006,11.6,-7.80148617400001));
#280334=CARTESIAN_POINT('Ctrl Pts',(-8.11267465400006,15.2,-7.80470081900001));
#280335=CARTESIAN_POINT('Ctrl Pts',(-8.11267465400006,11.6,-7.80470081900001));
#280336=CARTESIAN_POINT('Ctrl Pts',(-8.11402504600006,15.2,-7.80792091400001));
#280337=CARTESIAN_POINT('Ctrl Pts',(-8.11402504600006,11.6,-7.80792091400001));
#280338=CARTESIAN_POINT('Ctrl Pts',(-8.11537475500005,15.2,-7.81114645400002));
#280339=CARTESIAN_POINT('Ctrl Pts',(-8.11537475500005,11.6,-7.81114645400002));
#280340=CARTESIAN_POINT('Ctrl Pts',(-8.11672377400006,15.2,-7.81437743400001));
#280341=CARTESIAN_POINT('Ctrl Pts',(-8.11672377400006,11.6,-7.81437743400001));
#280342=CARTESIAN_POINT('Ctrl Pts',(-8.11807209300006,15.2,-7.81761384900002));
#280343=CARTESIAN_POINT('Ctrl Pts',(-8.11807209300006,11.6,-7.81761384900002));
#280344=CARTESIAN_POINT('Ctrl Pts',(-8.11941970300006,15.2,-7.82085569400002));
#280345=CARTESIAN_POINT('Ctrl Pts',(-8.11941970300006,11.6,-7.82085569400002));
#280346=CARTESIAN_POINT('Ctrl Pts',(-8.12076659600006,15.2,-7.82410296400001));
#280347=CARTESIAN_POINT('Ctrl Pts',(-8.12076659600006,11.6,-7.82410296400001));
#280348=CARTESIAN_POINT('Ctrl Pts',(-8.12211276200006,15.2,-7.82735565500002));
#280349=CARTESIAN_POINT('Ctrl Pts',(-8.12211276200006,11.6,-7.82735565500002));
#280350=CARTESIAN_POINT('Ctrl Pts',(-8.12345819500005,15.2,-7.83061376200001));
#280351=CARTESIAN_POINT('Ctrl Pts',(-8.12345819500005,11.6,-7.83061376200001));
#280352=CARTESIAN_POINT('Ctrl Pts',(-8.12480288300006,15.2,-7.83387728000001));
#280353=CARTESIAN_POINT('Ctrl Pts',(-8.12480288300006,11.6,-7.83387728000001));
#280354=CARTESIAN_POINT('Ctrl Pts',(-8.12614682100006,15.2,-7.83714620400002));
#280355=CARTESIAN_POINT('Ctrl Pts',(-8.12614682100006,11.6,-7.83714620400002));
#280356=CARTESIAN_POINT('Ctrl Pts',(-8.12748999700006,15.2,-7.84042052900002));
#280357=CARTESIAN_POINT('Ctrl Pts',(-8.12748999700006,11.6,-7.84042052900002));
#280358=CARTESIAN_POINT('Ctrl Pts',(-8.12883240400006,15.2,-7.84370025200002));
#280359=CARTESIAN_POINT('Ctrl Pts',(-8.12883240400006,11.6,-7.84370025200002));
#280360=CARTESIAN_POINT('Ctrl Pts',(-8.13017403400006,15.2,-7.84698536500001));
#280361=CARTESIAN_POINT('Ctrl Pts',(-8.13017403400006,11.6,-7.84698536500001));
#280362=CARTESIAN_POINT('Ctrl Pts',(-8.13151487800006,15.2,-7.85027586600001));
#280363=CARTESIAN_POINT('Ctrl Pts',(-8.13151487800006,11.6,-7.85027586600001));
#280364=CARTESIAN_POINT('Ctrl Pts',(-8.13285492800006,15.2,-7.85357174900001));
#280365=CARTESIAN_POINT('Ctrl Pts',(-8.13285492800006,11.6,-7.85357174900001));
#280366=CARTESIAN_POINT('Ctrl Pts',(-8.13419417400005,15.2,-7.85687301000002));
#280367=CARTESIAN_POINT('Ctrl Pts',(-8.13419417400005,11.6,-7.85687301000002));
#280368=CARTESIAN_POINT('Ctrl Pts',(-8.13553260800006,15.2,-7.86017964300001));
#280369=CARTESIAN_POINT('Ctrl Pts',(-8.13553260800006,11.6,-7.86017964300001));
#280370=CARTESIAN_POINT('Ctrl Pts',(-8.13687022200006,15.2,-7.86349164400002));
#280371=CARTESIAN_POINT('Ctrl Pts',(-8.13687022200006,11.6,-7.86349164400002));
#280372=CARTESIAN_POINT('Ctrl Pts',(-8.13820700800006,15.2,-7.86680900800001));
#280373=CARTESIAN_POINT('Ctrl Pts',(-8.13820700800006,11.6,-7.86680900800001));
#280374=CARTESIAN_POINT('Ctrl Pts',(-8.13954295700006,15.2,-7.87013173000001));
#280375=CARTESIAN_POINT('Ctrl Pts',(-8.13954295700006,11.6,-7.87013173000001));
#280376=CARTESIAN_POINT('Ctrl Pts',(-8.14087806000006,15.2,-7.87345980500002));
#280377=CARTESIAN_POINT('Ctrl Pts',(-8.14087806000006,11.6,-7.87345980500002));
#280378=CARTESIAN_POINT('Ctrl Pts',(-8.14221230900005,15.2,-7.87679322900001));
#280379=CARTESIAN_POINT('Ctrl Pts',(-8.14221230900005,11.6,-7.87679322900001));
#280380=CARTESIAN_POINT('Ctrl Pts',(-8.14354569800006,15.2,-7.88013199700002));
#280381=CARTESIAN_POINT('Ctrl Pts',(-8.14354569800006,11.6,-7.88013199700002));
#280382=CARTESIAN_POINT('Ctrl Pts',(-8.14487821400006,15.2,-7.88347610400002));
#280383=CARTESIAN_POINT('Ctrl Pts',(-8.14487821400006,11.6,-7.88347610400002));
#280384=CARTESIAN_POINT('Ctrl Pts',(-8.14620985300006,15.2,-7.88682554500002));
#280385=CARTESIAN_POINT('Ctrl Pts',(-8.14620985300006,11.6,-7.88682554500002));
#280386=CARTESIAN_POINT('Ctrl Pts',(-8.14754060400006,15.2,-7.89018031600002));
#280387=CARTESIAN_POINT('Ctrl Pts',(-8.14754060400006,11.6,-7.89018031600002));
#280388=CARTESIAN_POINT('Ctrl Pts',(-8.14887046000005,15.2,-7.89354041100002));
#280389=CARTESIAN_POINT('Ctrl Pts',(-8.14887046000005,11.6,-7.89354041100002));
#280390=CARTESIAN_POINT('Ctrl Pts',(-8.15019941300006,15.2,-7.89690582600001));
#280391=CARTESIAN_POINT('Ctrl Pts',(-8.15019941300006,11.6,-7.89690582600001));
#280392=CARTESIAN_POINT('Ctrl Pts',(-8.15152745300006,15.2,-7.90027655700002));
#280393=CARTESIAN_POINT('Ctrl Pts',(-8.15152745300006,11.6,-7.90027655700002));
#280394=CARTESIAN_POINT('Ctrl Pts',(-8.15285457300006,15.2,-7.90365259800001));
#280395=CARTESIAN_POINT('Ctrl Pts',(-8.15285457300006,11.6,-7.90365259800001));
#280396=CARTESIAN_POINT('Ctrl Pts',(-8.15418076600006,15.2,-7.90703394400002));
#280397=CARTESIAN_POINT('Ctrl Pts',(-8.15418076600006,11.6,-7.90703394400002));
#280398=CARTESIAN_POINT('Ctrl Pts',(-8.15550602100006,15.2,-7.91042059200001));
#280399=CARTESIAN_POINT('Ctrl Pts',(-8.15550602100006,11.6,-7.91042059200001));
#280400=CARTESIAN_POINT('Ctrl Pts',(-8.15683033200006,15.2,-7.91381253500001));
#280401=CARTESIAN_POINT('Ctrl Pts',(-8.15683033200006,11.6,-7.91381253500001));
#280402=CARTESIAN_POINT('Ctrl Pts',(-8.15815368900006,15.2,-7.91720976900002));
#280403=CARTESIAN_POINT('Ctrl Pts',(-8.15815368900006,11.6,-7.91720976900002));
#280404=CARTESIAN_POINT('Ctrl Pts',(-8.15947608700006,15.2,-7.92061229100002));
#280405=CARTESIAN_POINT('Ctrl Pts',(-8.15947608700006,11.6,-7.92061229100002));
#280406=CARTESIAN_POINT('Ctrl Pts',(-8.16079751400006,15.2,-7.92402009500002));
#280407=CARTESIAN_POINT('Ctrl Pts',(-8.16079751400006,11.6,-7.92402009500002));
#280408=CARTESIAN_POINT('Ctrl Pts',(-8.16211796400006,15.2,-7.92743317400002));
#280409=CARTESIAN_POINT('Ctrl Pts',(-8.16211796400006,11.6,-7.92743317400002));
#280410=CARTESIAN_POINT('Ctrl Pts',(-8.16343743000006,15.2,-7.93085152700002));
#280411=CARTESIAN_POINT('Ctrl Pts',(-8.16343743000006,11.6,-7.93085152700002));
#280412=CARTESIAN_POINT('Ctrl Pts',(-8.16475590200006,15.2,-7.93427514600002));
#280413=CARTESIAN_POINT('Ctrl Pts',(-8.16475590200006,11.6,-7.93427514600002));
#280414=CARTESIAN_POINT('Ctrl Pts',(-8.16607337200006,15.2,-7.93770403000002));
#280415=CARTESIAN_POINT('Ctrl Pts',(-8.16607337200006,11.6,-7.93770403000002));
#280416=CARTESIAN_POINT('Ctrl Pts',(-8.16738983300005,15.2,-7.94113817000002));
#280417=CARTESIAN_POINT('Ctrl Pts',(-8.16738983300005,11.6,-7.94113817000002));
#280418=CARTESIAN_POINT('Ctrl Pts',(-8.16870527600006,15.2,-7.94457756400002));
#280419=CARTESIAN_POINT('Ctrl Pts',(-8.16870527600006,11.6,-7.94457756400002));
#280420=CARTESIAN_POINT('Ctrl Pts',(-8.17001969400006,15.2,-7.94802220500002));
#280421=CARTESIAN_POINT('Ctrl Pts',(-8.17001969400006,11.6,-7.94802220500002));
#280422=CARTESIAN_POINT('Ctrl Pts',(-8.17133307700006,15.2,-7.95147209200002));
#280423=CARTESIAN_POINT('Ctrl Pts',(-8.17133307700006,11.6,-7.95147209200002));
#280424=CARTESIAN_POINT('Ctrl Pts',(-8.17264542000006,15.2,-7.95492721600001));
#280425=CARTESIAN_POINT('Ctrl Pts',(-8.17264542000006,11.6,-7.95492721600001));
#280426=CARTESIAN_POINT('Ctrl Pts',(-8.17395671300006,15.2,-7.95838757500002));
#280427=CARTESIAN_POINT('Ctrl Pts',(-8.17395671300006,11.6,-7.95838757500002));
#280428=CARTESIAN_POINT('Ctrl Pts',(-8.17526694900006,15.2,-7.96185316300001));
#280429=CARTESIAN_POINT('Ctrl Pts',(-8.17526694900006,11.6,-7.96185316300001));
#280430=CARTESIAN_POINT('Ctrl Pts',(-8.17657612000006,15.2,-7.96532397700001));
#280431=CARTESIAN_POINT('Ctrl Pts',(-8.17657612000006,11.6,-7.96532397700001));
#280432=CARTESIAN_POINT('Ctrl Pts',(-8.17788421700006,15.2,-7.96880001000002));
#280433=CARTESIAN_POINT('Ctrl Pts',(-8.17788421700006,11.6,-7.96880001000002));
#280434=CARTESIAN_POINT('Ctrl Pts',(-8.17919123500005,15.2,-7.97228125900002));
#280435=CARTESIAN_POINT('Ctrl Pts',(-8.17919123500005,11.6,-7.97228125900002));
#280436=CARTESIAN_POINT('Ctrl Pts',(-8.18049716300006,15.2,-7.97576771900002));
#280437=CARTESIAN_POINT('Ctrl Pts',(-8.18049716300006,11.6,-7.97576771900002));
#280438=CARTESIAN_POINT('Ctrl Pts',(-8.18180199500006,15.2,-7.97925938400001));
#280439=CARTESIAN_POINT('Ctrl Pts',(-8.18180199500006,11.6,-7.97925938400001));
#280440=CARTESIAN_POINT('Ctrl Pts',(-8.18310572200006,15.2,-7.98275625000001));
#280441=CARTESIAN_POINT('Ctrl Pts',(-8.18310572200006,11.6,-7.98275625000001));
#280442=CARTESIAN_POINT('Ctrl Pts',(-8.18440833700006,15.2,-7.98625831200001));
#280443=CARTESIAN_POINT('Ctrl Pts',(-8.18440833700006,11.6,-7.98625831200001));
#280444=CARTESIAN_POINT('Ctrl Pts',(-8.18570982900006,15.2,-7.98976556500002));
#280445=CARTESIAN_POINT('Ctrl Pts',(-8.18570982900006,11.6,-7.98976556500002));
#280446=CARTESIAN_POINT('Ctrl Pts',(-8.18701019300006,15.2,-7.99327800400001));
#280447=CARTESIAN_POINT('Ctrl Pts',(-8.18701019300006,11.6,-7.99327800400001));
#280448=CARTESIAN_POINT('Ctrl Pts',(-8.18830942000006,15.2,-7.99679562500001));
#280449=CARTESIAN_POINT('Ctrl Pts',(-8.18830942000006,11.6,-7.99679562500001));
#280450=CARTESIAN_POINT('Ctrl Pts',(-8.18960750500005,15.2,-8.00031842400001));
#280451=CARTESIAN_POINT('Ctrl Pts',(-8.18960750500005,11.6,-8.00031842400001));
#280452=CARTESIAN_POINT('Ctrl Pts',(-8.19090444000006,15.2,-8.00384639600002));
#280453=CARTESIAN_POINT('Ctrl Pts',(-8.19090444000006,11.6,-8.00384639600002));
#280454=CARTESIAN_POINT('Ctrl Pts',(-8.19220021800006,15.2,-8.00737953800001));
#280455=CARTESIAN_POINT('Ctrl Pts',(-8.19220021800006,11.6,-8.00737953800001));
#280456=CARTESIAN_POINT('Ctrl Pts',(-8.19349483100006,15.2,-8.01091784200001));
#280457=CARTESIAN_POINT('Ctrl Pts',(-8.19349483100006,11.6,-8.01091784200001));
#280458=CARTESIAN_POINT('Ctrl Pts',(-8.19478827300006,15.2,-8.01446130700001));
#280459=CARTESIAN_POINT('Ctrl Pts',(-8.19478827300006,11.6,-8.01446130700001));
#280460=CARTESIAN_POINT('Ctrl Pts',(-8.19608053200006,15.2,-8.01800992700001));
#280461=CARTESIAN_POINT('Ctrl Pts',(-8.19608053200006,11.6,-8.01800992700001));
#280462=CARTESIAN_POINT('Ctrl Pts',(-8.19737160100006,15.2,-8.02156369400001));
#280463=CARTESIAN_POINT('Ctrl Pts',(-8.19737160100006,11.6,-8.02156369400001));
#280464=CARTESIAN_POINT('Ctrl Pts',(-8.19866147000005,15.2,-8.02512260400002));
#280465=CARTESIAN_POINT('Ctrl Pts',(-8.19866147000005,11.6,-8.02512260400002));
#280466=CARTESIAN_POINT('Ctrl Pts',(-8.19995012900005,15.2,-8.02868665000002));
#280467=CARTESIAN_POINT('Ctrl Pts',(-8.19995012900005,11.6,-8.02868665000002));
#280468=CARTESIAN_POINT('Ctrl Pts',(-8.20123757100006,15.2,-8.03225582900001));
#280469=CARTESIAN_POINT('Ctrl Pts',(-8.20123757100006,11.6,-8.03225582900001));
#280470=CARTESIAN_POINT('Ctrl Pts',(-8.20252378800006,15.2,-8.03583013400001));
#280471=CARTESIAN_POINT('Ctrl Pts',(-8.20252378800006,11.6,-8.03583013400001));
#280472=CARTESIAN_POINT('Ctrl Pts',(-8.20380877600006,15.2,-8.03940956400002));
#280473=CARTESIAN_POINT('Ctrl Pts',(-8.20380877600006,11.6,-8.03940956400002));
#280474=CARTESIAN_POINT('Ctrl Pts',(-8.20509253000006,15.2,-8.04299411600002));
#280475=CARTESIAN_POINT('Ctrl Pts',(-8.20509253000006,11.6,-8.04299411600002));
#280476=CARTESIAN_POINT('Ctrl Pts',(-8.20637504900006,15.2,-8.04658378800001));
#280477=CARTESIAN_POINT('Ctrl Pts',(-8.20637504900006,11.6,-8.04658378800001));
#280478=CARTESIAN_POINT('Ctrl Pts',(-8.20740007500006,15.2,-8.04945962200001));
#280479=CARTESIAN_POINT('Ctrl Pts',(-8.20740007500006,11.6,-8.04945962200001));
#280480=CARTESIAN_POINT('Ctrl Pts',(-8.20816828900006,15.2,-8.05161880000002));
#280481=CARTESIAN_POINT('Ctrl Pts',(-8.20816828900006,11.6,-8.05161880000002));
#280482=CARTESIAN_POINT('Ctrl Pts',(-8.20868018400006,15.2,-8.05305927700001));
#280483=CARTESIAN_POINT('Ctrl Pts',(-8.20868018400006,11.6,-8.05305927700001));
#280484=CARTESIAN_POINT('Ctrl Pts',(-8.20893607000006,15.2,-8.05377977100001));
#280485=CARTESIAN_POINT('Ctrl Pts',(-8.20893607000006,11.6,-8.05377977100001));
#280486=CARTESIAN_POINT('Ctrl Pts',(-7.64657512400006,15.2,-7.01216898700002));
#280487=CARTESIAN_POINT('Ctrl Pts',(-7.64778328679899,15.2,-7.01348522587027));
#280488=CARTESIAN_POINT('Ctrl Pts',(-7.64902613388113,15.2,-7.01484722203433));
#280489=CARTESIAN_POINT('Ctrl Pts',(-7.65030255133521,15.2,-7.01625467938746));
#280490=CARTESIAN_POINT('Ctrl Pts',(-7.65158512431943,15.2,-7.01766892421138));
#280491=CARTESIAN_POINT('Ctrl Pts',(-7.65290158882944,15.2,-7.01912907735244));
#280492=CARTESIAN_POINT('Ctrl Pts',(-7.65425083088893,15.2,-7.02063486217904));
#280493=CARTESIAN_POINT('Ctrl Pts',(-7.65560007282589,15.2,-7.02214064686888));
#280494=CARTESIAN_POINT('Ctrl Pts',(-7.6569820926347,15.2,-7.02369206393294));
#280495=CARTESIAN_POINT('Ctrl Pts',(-7.65839581074999,15.2,-7.02528884179159));
#280496=CARTESIAN_POINT('Ctrl Pts',(-7.65980952886529,15.2,-7.02688561965024));
#280497=CARTESIAN_POINT('Ctrl Pts',(-7.66125494568895,15.1999999999999,
-7.02852776104979));
#280498=CARTESIAN_POINT('Ctrl Pts',(-7.66273101487395,15.2,-7.03021499707016));
#280499=CARTESIAN_POINT('Ctrl Pts',(-7.66420708419303,15.2,-7.03190223324379));
#280500=CARTESIAN_POINT('Ctrl Pts',(-7.66571380278172,15.2,-7.03363456758543));
#280501=CARTESIAN_POINT('Ctrl Pts',(-7.66725015536747,15.2,-7.03541173743532));
#280502=CARTESIAN_POINT('Ctrl Pts',(-7.66878650781365,15.2,-7.03718890712378));
#280503=CARTESIAN_POINT('Ctrl Pts',(-7.67035249574304,15.2,-7.03901091194339));
#280504=CARTESIAN_POINT('Ctrl Pts',(-7.67194712427573,15.2,-7.04087749571745));
#280505=CARTESIAN_POINT('Ctrl Pts',(-7.67354175280843,15.2,-7.04274407949153));
#280506=CARTESIAN_POINT('Ctrl Pts',(-7.67516502602135,15.2,-7.04465524296655));
#280507=CARTESIAN_POINT('Ctrl Pts',(-7.67681598062681,15.2,-7.04661073189355));
#280508=CARTESIAN_POINT('Ctrl Pts',(-7.67846693538224,15.2,-7.04856622099817));
#280509=CARTESIAN_POINT('Ctrl Pts',(-7.68014557084944,15.2,-7.05056603617498));
#280510=CARTESIAN_POINT('Ctrl Pts',(-7.68185095069424,15.2,-7.05260992995607));
#280511=CARTESIAN_POINT('Ctrl Pts',(-7.68355633038413,15.2,-7.05465382355151));
#280512=CARTESIAN_POINT('Ctrl Pts',(-7.68528845682534,15.2,-7.05674179384187));
#280513=CARTESIAN_POINT('Ctrl Pts',(-7.68704641459593,15.2,-7.05887359659964));
#280514=CARTESIAN_POINT('Ctrl Pts',(-7.68880437236652,15.2,-7.06100539935743));
#280515=CARTESIAN_POINT('Ctrl Pts',(-7.69058816346834,15.2,-7.06318103452004));
#280516=CARTESIAN_POINT('Ctrl Pts',(-7.69239689940154,15.2,-7.06540025935418));
#280517=CARTESIAN_POINT('Ctrl Pts',(-7.69420563533474,15.2,-7.06761948418832));
#280518=CARTESIAN_POINT('Ctrl Pts',(-7.69603931658333,15.2,-7.06988230103532));
#280519=CARTESIAN_POINT('Ctrl Pts',(-7.69789707751419,15.2,-7.07218846778191));
#280520=CARTESIAN_POINT('Ctrl Pts',(-7.6997548386138,15.2,-7.07449463473798));
#280521=CARTESIAN_POINT('Ctrl Pts',(-7.7016366791741,15.2,-7.07684415463993));
#280522=CARTESIAN_POINT('Ctrl Pts',(-7.70354175636227,15.2,-7.07923678885552));
#280523=CARTESIAN_POINT('Ctrl Pts',(-7.70544683337737,15.2,-7.08162942285377));
#280524=CARTESIAN_POINT('Ctrl Pts',(-7.70737514672789,15.2,-7.08406517436941));
#280525=CARTESIAN_POINT('Ctrl Pts',(-7.70932587299913,15.2,-7.08654380820715));
#280526=CARTESIAN_POINT('Ctrl Pts',(-7.71127659927036,15.2,-7.08902244204489));
#280527=CARTESIAN_POINT('Ctrl Pts',(-7.71324973925656,15.2,-7.09154395937487));
#280528=CARTESIAN_POINT('Ctrl Pts',(-7.71524449051593,15.2,-7.09410813019545));
#280529=CARTESIAN_POINT('Ctrl Pts',(-7.71723924195649,15.2,-7.09667230124895));
#280530=CARTESIAN_POINT('Ctrl Pts',(-7.71925560443252,15.2,-7.09927912477326));
#280531=CARTESIAN_POINT('Ctrl Pts',(-7.7212927938778,15.2,-7.10192837566951));
#280532=CARTESIAN_POINT('Ctrl Pts',(-7.72332998313804,15.2,-7.10457762632511));
#280533=CARTESIAN_POINT('Ctrl Pts',(-7.72538800039852,15.2,-7.10726930092739));
#280534=CARTESIAN_POINT('Ctrl Pts',(-7.72746607899908,15.2,-7.1100031779237));
#280535=CARTESIAN_POINT('Ctrl Pts',(-7.72954415759964,15.2,-7.11273705492003));
#280536=CARTESIAN_POINT('Ctrl Pts',(-7.73164230023916,15.2,-7.11551313281472));
#280537=CARTESIAN_POINT('Ctrl Pts',(-7.73375975674422,15.2,-7.11833118970945));
#280538=CARTESIAN_POINT('Ctrl Pts',(-7.73587721344161,15.2,-7.12114924686015));
#280539=CARTESIAN_POINT('Ctrl Pts',(-7.73801398519903,15.2,-7.12400928335858));
#280540=CARTESIAN_POINT('Ctrl Pts',(-7.74016934292524,15.2,-7.12691107683075));
#280541=CARTESIAN_POINT('Ctrl Pts',(-7.74232470045566,15.2,-7.12981287003936));
#280542=CARTESIAN_POINT('Ctrl Pts',(-7.74449864221298,15.2,-7.13275642378339));
#280543=CARTESIAN_POINT('Ctrl Pts',(-7.74669045496669,15.2,-7.13574151575828));
#280544=CARTESIAN_POINT('Ctrl Pts',(-7.74888226772041,15.2,-7.13872660773317));
#280545=CARTESIAN_POINT('Ctrl Pts',(-7.751091952672,15.2,-7.14175324162221));
#280546=CARTESIAN_POINT('Ctrl Pts',(-7.75331881053465,15.2,-7.14482119791159));
#280547=CARTESIAN_POINT('Ctrl Pts',(-7.75554566859958,15.2,-7.14788915447964));
#280548=CARTESIAN_POINT('Ctrl Pts',(-7.75778970044714,15.2,-7.15099843786054));
#280549=CARTESIAN_POINT('Ctrl Pts',(-7.76005022248809,15.2,-7.15414883011834));
#280550=CARTESIAN_POINT('Ctrl Pts',(-7.76231074432373,15.2,-7.15729922208999));
#280551=CARTESIAN_POINT('Ctrl Pts',(-7.76458775655725,15.2,-7.16049072517074));
#280552=CARTESIAN_POINT('Ctrl Pts',(-7.76688059148441,15.2,-7.16372312523475));
#280553=CARTESIAN_POINT('Ctrl Pts',(-7.76917342641157,15.2,-7.16695552529877));
#280554=CARTESIAN_POINT('Ctrl Pts',(-7.77148208440855,15.2,-7.17022882502503));
#280555=CARTESIAN_POINT('Ctrl Pts',(-7.77380591132344,15.2,-7.1735428110695));
#280556=CARTESIAN_POINT('Ctrl Pts',(-7.77574243382289,15.2,-7.1763044662069));
#280557=CARTESIAN_POINT('Ctrl Pts',(-7.77768949117817,15.2,-7.17909437651173));
#280558=CARTESIAN_POINT('Ctrl Pts',(-7.77964671041376,15.2,-7.18191242227416));
#280559=CARTESIAN_POINT('Ctrl Pts',(-7.78160392964934,15.2,-7.18473046803657));
#280560=CARTESIAN_POINT('Ctrl Pts',(-7.78357131294,15.2,-7.18757664781318));
#280561=CARTESIAN_POINT('Ctrl Pts',(-7.78554849399062,15.2,-7.19045084275672));
#280562=CARTESIAN_POINT('Ctrl Pts',(-7.78752567504124,15.2,-7.19332503770024));
#280563=CARTESIAN_POINT('Ctrl Pts',(-7.78951265463893,15.2,-7.19622724628885));
#280564=CARTESIAN_POINT('Ctrl Pts',(-7.79150907470837,15.2,-7.19915735052494));
#280565=CARTESIAN_POINT('Ctrl Pts',(-7.79350549477779,15.2,-7.20208745476103));
#280566=CARTESIAN_POINT('Ctrl Pts',(-7.79551135383639,15.2,-7.2050454544546));
#280567=CARTESIAN_POINT('Ctrl Pts',(-7.79752630148447,15.2,-7.20803123050991));
#280568=CARTESIAN_POINT('Ctrl Pts',(-7.79954124913253,15.2,-7.21101700656521));
#280569=CARTESIAN_POINT('Ctrl Pts',(-7.80156528368813,15.2,-7.21403056018646));
#280570=CARTESIAN_POINT('Ctrl Pts',(-7.80359806042469,15.2,-7.21707177192401));
#280571=CARTESIAN_POINT('Ctrl Pts',(-7.80563083716125,15.2,-7.22011298366154));
#280572=CARTESIAN_POINT('Ctrl Pts',(-7.80767235392262,15.2,-7.2231818550512));
#280573=CARTESIAN_POINT('Ctrl Pts',(-7.80972227170081,15.2,-7.22627826692762));
#280574=CARTESIAN_POINT('Ctrl Pts',(-7.81177218947903,15.2,-7.22937467880403));
#280575=CARTESIAN_POINT('Ctrl Pts',(-7.81383050736948,15.2,-7.23249863307319));
#280576=CARTESIAN_POINT('Ctrl Pts',(-7.81589689101494,15.2,-7.23565001385754));
#280577=CARTESIAN_POINT('Ctrl Pts',(-7.81796327466039,15.2,-7.23880139464188));
#280578=CARTESIAN_POINT('Ctrl Pts',(-7.8200377222773,15.2,-7.24198019922819));
#280579=CARTESIAN_POINT('Ctrl Pts',(-7.82211990672239,15.2,-7.24518631270265));
#280580=CARTESIAN_POINT('Ctrl Pts',(-7.82420209116748,15.2,-7.24839242617711));
#280581=CARTESIAN_POINT('Ctrl Pts',(-7.826292010146,15.2,-7.251625849902));
#280582=CARTESIAN_POINT('Ctrl Pts',(-7.82838933979937,15.2,-7.25488646816811));
#280583=CARTESIAN_POINT('Ctrl Pts',(-7.83048666922415,15.2,-7.25814708607882));
#280584=CARTESIAN_POINT('Ctrl Pts',(-7.83259141104903,15.2,-7.26143489747436));
#280585=CARTESIAN_POINT('Ctrl Pts',(-7.83470324366548,15.2,-7.26474978954136));
#280586=CARTESIAN_POINT('Ctrl Pts',(-7.8368150765121,15.2,-7.26806468196968));
#280587=CARTESIAN_POINT('Ctrl Pts',(-7.83893400051145,15.2,-7.27140665157262));
#280588=CARTESIAN_POINT('Ctrl Pts',(-7.84105970245533,15.2,-7.27477558900096));
#280589=CARTESIAN_POINT('Ctrl Pts',(-7.84318540439921,15.2,-7.2781445264293));
#280590=CARTESIAN_POINT('Ctrl Pts',(-7.84531788327079,15.2,-7.28154042926555));
#280591=CARTESIAN_POINT('Ctrl Pts',(-7.8474568297286,15.2,-7.28496318356893));
#280592=CARTESIAN_POINT('Ctrl Pts',(-7.84959577618641,15.2,-7.2883859378723));
#280593=CARTESIAN_POINT('Ctrl Pts',(-7.85174119063211,15.2,-7.29183554548579));
#280594=CARTESIAN_POINT('Ctrl Pts',(-7.8538927687253,15.2,-7.29531189162982));
#280595=CARTESIAN_POINT('Ctrl Pts',(-7.85647466257781,15.2,-7.29948350723001));
#280596=CARTESIAN_POINT('Ctrl Pts',(-7.85906542972445,15.2,-7.30369362700386));
#280597=CARTESIAN_POINT('Ctrl Pts',(-7.86166455453335,15.2,-7.30794205648804));
#280598=CARTESIAN_POINT('Ctrl Pts',(-7.86339730416987,15.2,-7.31077434242493));
#280599=CARTESIAN_POINT('Ctrl Pts',(-7.86513376794754,15.2,-7.31362365599012));
#280600=CARTESIAN_POINT('Ctrl Pts',(-7.86687379608283,15.2,-7.31648993853246));
#280601=CARTESIAN_POINT('Ctrl Pts',(-7.8686138244552,15.2,-7.31935622146532));
#280602=CARTESIAN_POINT('Ctrl Pts',(-7.87035741474857,15.2,-7.32223947390259));
#280603=CARTESIAN_POINT('Ctrl Pts',(-7.8721044194869,15.2,-7.32513963892921));
#280604=CARTESIAN_POINT('Ctrl Pts',(-7.8742881752908,15.2,-7.32876484501491));
#280605=CARTESIAN_POINT('Ctrl Pts',(-7.87647726583108,15.2,-7.33241647642887));
#280606=CARTESIAN_POINT('Ctrl Pts',(-7.8786714030537,15.2,-7.3360944224727));
#280607=CARTESIAN_POINT('Ctrl Pts',(-7.88042671268832,15.2,-7.33903677906723));
#280608=CARTESIAN_POINT('Ctrl Pts',(-7.88218525180583,15.2,-7.34199597845954));
#280609=CARTESIAN_POINT('Ctrl Pts',(-7.88394687610606,15.2,-7.34497196104849));
#280610=CARTESIAN_POINT('Ctrl Pts',(-7.88570850064631,15.2,-7.34794794404292));
#280611=CARTESIAN_POINT('Ctrl Pts',(-7.88747320981608,15.2,-7.35094071248756));
#280612=CARTESIAN_POINT('Ctrl Pts',(-7.88924085922323,15.2,-7.35395020947007));
#280613=CARTESIAN_POINT('Ctrl Pts',(-7.89100850838952,15.2,-7.35695970604254));
#280614=CARTESIAN_POINT('Ctrl Pts',(-7.89277909937803,15.2,-7.3599859298373));
#280615=CARTESIAN_POINT('Ctrl Pts',(-7.89455248912176,15.2,-7.36302882630968));
#280616=CARTESIAN_POINT('Ctrl Pts',(-7.89632587910712,15.2,-7.36607172319666));
#280617=CARTESIAN_POINT('Ctrl Pts',(-7.89810206675392,15.2,-7.36913129149951));
#280618=CARTESIAN_POINT('Ctrl Pts',(-7.89988091462883,15.2,-7.37220747700159));
#280619=CARTESIAN_POINT('Ctrl Pts',(-7.90165976226136,15.2,-7.37528366208454));
#280620=CARTESIAN_POINT('Ctrl Pts',(-7.9034412671759,15.2,-7.37837646237136));
#280621=CARTESIAN_POINT('Ctrl Pts',(-7.90522529300786,15.2,-7.38148582304886));
#280622=CARTESIAN_POINT('Ctrl Pts',(-7.90700931908289,15.2,-7.38459518415));
#280623=CARTESIAN_POINT('Ctrl Pts',(-7.90879586575977,15.2,-7.38772110534022));
#280624=CARTESIAN_POINT('Ctrl Pts',(-7.91058479441298,15.2,-7.39086353029033));
#280625=CARTESIAN_POINT('Ctrl Pts',(-7.91237372282244,15.2,-7.39400595481229));
#280626=CARTESIAN_POINT('Ctrl Pts',(-7.91416503376754,15.2,-7.39716488463093));
#280627=CARTESIAN_POINT('Ctrl Pts',(-7.9159585922318,15.2,-7.40034026248078));
#280628=CARTESIAN_POINT('Ctrl Pts',(-7.91820054049541,15.2,-7.40430948511758));
#280629=CARTESIAN_POINT('Ctrl Pts',(-7.92044600027689,15.2,-7.40830440833977));
#280630=CARTESIAN_POINT('Ctrl Pts',(-7.92269470872235,15.2,-7.41232492527499));
#280631=CARTESIAN_POINT('Ctrl Pts',(-7.92449367557676,15.2,-7.41554133899845));
#280632=CARTESIAN_POINT('Ctrl Pts',(-7.92629472267131,15.2,-7.41877413202094));
#280633=CARTESIAN_POINT('Ctrl Pts',(-7.92809771688079,15.2,-7.42202324953238));
#280634=CARTESIAN_POINT('Ctrl Pts',(-7.92990071084462,15.2,-7.42527236660113));
#280635=CARTESIAN_POINT('Ctrl Pts',(-7.93170565234697,15.2,-7.42853780720556));
#280636=CARTESIAN_POINT('Ctrl Pts',(-7.93351241142132,15.2,-7.43181951771341));
#280637=CARTESIAN_POINT('Ctrl Pts',(-7.93531917074182,15.2,-7.43510122866839));
#280638=CARTESIAN_POINT('Ctrl Pts',(-7.93712774630829,15.2,-7.43839920875926));
#280639=CARTESIAN_POINT('Ctrl Pts',(-7.93893800902628,15.2,-7.44171340301054));
#280640=CARTESIAN_POINT('Ctrl Pts',(-7.94074827149763,15.2,-7.44502759681028));
#280641=CARTESIAN_POINT('Ctrl Pts',(-7.94256022203805,15.2,-7.44835800521968));
#280642=CARTESIAN_POINT('Ctrl Pts',(-7.94437373194521,15.2,-7.45170457244446));
#280643=CARTESIAN_POINT('Ctrl Pts',(-7.94618724209945,15.2,-7.45505114012521));
#280644=CARTESIAN_POINT('Ctrl Pts',(-7.9480023113316,15.2,-7.45841386751856));
#280645=CARTESIAN_POINT('Ctrl Pts',(-7.94981881404171,15.2,-7.46179269975828));
#280646=CARTESIAN_POINT('Ctrl Pts',(-7.95163531675183,15.2,-7.46517153199799));
#280647=CARTESIAN_POINT('Ctrl Pts',(-7.95345325198433,15.2,-7.46856646932567));
#280648=CARTESIAN_POINT('Ctrl Pts',(-7.95527249480583,15.2,-7.47197745629099));
#280649=CARTESIAN_POINT('Ctrl Pts',(-7.95709173737946,15.2,-7.47538844279156));
#280650=CARTESIAN_POINT('Ctrl Pts',(-7.95891228836167,15.2,-7.4788154805357));
#280651=CARTESIAN_POINT('Ctrl Pts',(-7.96073402299881,15.2,-7.48225851371428));
#280652=CARTESIAN_POINT('Ctrl Pts',(-7.96301119148139,15.2,-7.48656230553934));
#280653=CARTESIAN_POINT('Ctrl Pts',(-7.96529020949449,15.2,-7.49089109085549));
#280654=CARTESIAN_POINT('Ctrl Pts',(-7.96757083796672,15.2,-7.49524476425828));
#280655=CARTESIAN_POINT('Ctrl Pts',(-7.96939534084394,15.2,-7.49872770317033));
#280656=CARTESIAN_POINT('Ctrl Pts',(-7.97122087557127,15.2,-7.50222656891201));
#280657=CARTESIAN_POINT('Ctrl Pts',(-7.97304731978201,15.2,-7.50574131104962));
#280658=CARTESIAN_POINT('Ctrl Pts',(-7.97487376374389,15.2,-7.50925605270834));
#280659=CARTESIAN_POINT('Ctrl Pts',(-7.97670111765941,15.2,-7.51278666767974));
#280660=CARTESIAN_POINT('Ctrl Pts',(-7.97852926224048,15.2,-7.51633310223921));
#280661=CARTESIAN_POINT('Ctrl Pts',(-7.98035740707063,15.2,-7.51987953728188));
#280662=CARTESIAN_POINT('Ctrl Pts',(-7.98218634148551,15.2,-7.52344179445225));
#280663=CARTESIAN_POINT('Ctrl Pts',(-7.98401594830752,15.2,-7.5270198155933));
#280664=CARTESIAN_POINT('Ctrl Pts',(-7.98584555488024,15.2,-7.53059783624684));
#280665=CARTESIAN_POINT('Ctrl Pts',(-7.98767583300565,15.2,-7.53419162483724));
#280666=CARTESIAN_POINT('Ctrl Pts',(-7.98950666630039,15.2,-7.53780112593003));
#280667=CARTESIAN_POINT('Ctrl Pts',(-7.99133749984458,15.2,-7.54141062751461));
#280668=CARTESIAN_POINT('Ctrl Pts',(-7.99316888828883,15.2,-7.54503584132052));
#280669=CARTESIAN_POINT('Ctrl Pts',(-7.99500071516648,15.2,-7.54867671429774));
#280670=CARTESIAN_POINT('Ctrl Pts',(-7.99683254179453,15.2,-7.5523175867789));
#280671=CARTESIAN_POINT('Ctrl Pts',(-7.99866480678408,15.2,-7.55597411753806));
#280672=CARTESIAN_POINT('Ctrl Pts',(-8.00049739622581,15.2,-7.55964625547553));
#280673=CARTESIAN_POINT('Ctrl Pts',(-8.00232998591722,15.2,-7.56331839391334));
#280674=CARTESIAN_POINT('Ctrl Pts',(-8.00416290063055,15.2,-7.56700613667224));
#280675=CARTESIAN_POINT('Ctrl Pts',(-8.00599602367491,15.2,-7.57070943231951));
#280676=CARTESIAN_POINT('Ctrl Pts',(-8.00782914646951,15.2,-7.57441272746221));
#280677=CARTESIAN_POINT('Ctrl Pts',(-8.00966248152796,15.2,-7.57813157536295));
#280678=CARTESIAN_POINT('Ctrl Pts',(-8.01149591293363,15.2,-7.5818659223894));
#280679=CARTESIAN_POINT('Ctrl Pts',(-8.01332934458909,15.2,-7.58560026992465));
#280680=CARTESIAN_POINT('Ctrl Pts',(-8.01516287429861,15.2,-7.58935011545238));
#280681=CARTESIAN_POINT('Ctrl Pts',(-8.01699639051797,15.2,-7.59311540778586));
#280682=CARTESIAN_POINT('Ctrl Pts',(-8.01882990648751,15.2,-7.59688069960631));
#280683=CARTESIAN_POINT('Ctrl Pts',(-8.02066340849183,15.2,-7.60066143731065));
#280684=CARTESIAN_POINT('Ctrl Pts',(-8.0224967871753,15.2,-7.60445756838763));
#280685=CARTESIAN_POINT('Ctrl Pts',(-8.02433016610857,15.2,-7.60825369998183));
#280686=CARTESIAN_POINT('Ctrl Pts',(-8.02616342168349,15.2,-7.6120652229775));
#280687=CARTESIAN_POINT('Ctrl Pts',(-8.02799644278339,15.2,-7.61589208724161));
#280688=CARTESIAN_POINT('Ctrl Pts',(-8.02982946388329,15.2,-7.61971895150572));
#280689=CARTESIAN_POINT('Ctrl Pts',(-8.0316622529776,15.2,-7.62356115500774));
#280690=CARTESIAN_POINT('Ctrl Pts',(-8.03349470129966,15.2,-7.627418646664));
#280691=CARTESIAN_POINT('Ctrl Pts',(-8.03532714937206,15.2,-7.63127613779468));
#280692=CARTESIAN_POINT('Ctrl Pts',(-8.03715925531522,15.2,-7.63514891677531));
#280693=CARTESIAN_POINT('Ctrl Pts',(-8.03899091400714,15.2,-7.6390369286973));
#280694=CARTESIAN_POINT('Ctrl Pts',(-8.04082257294861,15.2,-7.64292494114903));
#280695=CARTESIAN_POINT('Ctrl Pts',(-8.04265378397744,15.2,-7.64682818924774));
#280696=CARTESIAN_POINT('Ctrl Pts',(-8.04448444029937,15.2,-7.65074661890729));
#280697=CARTESIAN_POINT('Ctrl Pts',(-8.04631509637188,15.2,-7.65466504803296));
#280698=CARTESIAN_POINT('Ctrl Pts',(-8.04814519867778,15.2,-7.65859866004553));
#280699=CARTESIAN_POINT('Ctrl Pts',(-8.04997464208383,15.2,-7.66254739994396));
#280700=CARTESIAN_POINT('Ctrl Pts',(-8.05180408573913,15.2,-7.6664961403804));
#280701=CARTESIAN_POINT('Ctrl Pts',(-8.05363286990777,15.2,-7.67046001126325));
#280702=CARTESIAN_POINT('Ctrl Pts',(-8.05546089176531,15.2,-7.67443895906907));
#280703=CARTESIAN_POINT('Ctrl Pts',(-8.0577459189627,15.2,-7.67941264355528));
#280704=CARTESIAN_POINT('Ctrl Pts',(-8.06002975383759,15.2,-7.68440988458806));
#280705=CARTESIAN_POINT('Ctrl Pts',(-8.06231219578194,15.2,-7.68943058292334));
#280706=CARTESIAN_POINT('Ctrl Pts',(-8.06459463772628,15.2,-7.69445128125862));
#280707=CARTESIAN_POINT('Ctrl Pts',(-8.06687568611503,15.2,-7.69949543347758));
#280708=CARTESIAN_POINT('Ctrl Pts',(-8.06915514403155,15.2,-7.70456294035446));
#280709=CARTESIAN_POINT('Ctrl Pts',(-8.07052281873177,15.2,-7.70760344437012));
#280710=CARTESIAN_POINT('Ctrl Pts',(-8.07188992144589,15.2,-7.71065235643226));
#280711=CARTESIAN_POINT('Ctrl Pts',(-8.0732564077561,15.2,-7.71370965309988));
#280712=CARTESIAN_POINT('Ctrl Pts',(-8.07462289406632,15.2,-7.71676694976752));
#280713=CARTESIAN_POINT('Ctrl Pts',(-8.07598876516518,15.2,-7.71983263181279));
#280714=CARTESIAN_POINT('Ctrl Pts',(-8.07735397886553,15.2,-7.72290667732684));
#280715=CARTESIAN_POINT('Ctrl Pts',(-8.07871919256587,15.2,-7.72598072284089));
#280716=CARTESIAN_POINT('Ctrl Pts',(-8.08008374933296,15.2,-7.72906313216229));
#280717=CARTESIAN_POINT('Ctrl Pts',(-8.08144760649173,15.2,-7.73215388225828));
#280718=CARTESIAN_POINT('Ctrl Pts',(-8.08281146365049,15.2,-7.73524463235428));
#280719=CARTESIAN_POINT('Ctrl Pts',(-8.08417462120098,15.2,-7.73834372525835));
#280720=CARTESIAN_POINT('Ctrl Pts',(-8.08553703835988,15.2,-7.74145113639472));
#280721=CARTESIAN_POINT('Ctrl Pts',(-8.08689945551878,15.2,-7.7445585475311));
#280722=CARTESIAN_POINT('Ctrl Pts',(-8.08826113143478,15.2,-7.74767427943733));
#280723=CARTESIAN_POINT('Ctrl Pts',(-8.08962202570342,15.2,-7.75079830860395));
#280724=CARTESIAN_POINT('Ctrl Pts',(-8.09098291997206,15.2,-7.75392233777057));
#280725=CARTESIAN_POINT('Ctrl Pts',(-8.09234303323634,15.2,-7.75705466433054));
#280726=CARTESIAN_POINT('Ctrl Pts',(-8.09370232202041,15.2,-7.76019526679865));
#280727=CARTESIAN_POINT('Ctrl Pts',(-8.09506161105141,15.2,-7.76333586983731));
#280728=CARTESIAN_POINT('Ctrl Pts',(-8.09642007779883,15.2,-7.7664847491616));
#280729=CARTESIAN_POINT('Ctrl Pts',(-8.09777768028768,15.2,-7.76964188220488));
#280730=CARTESIAN_POINT('Ctrl Pts',(-8.09913528252989,15.2,-7.77279901467461));
#280731=CARTESIAN_POINT('Ctrl Pts',(-8.10049202074717,15.2,-7.77596440096061));
#280732=CARTESIAN_POINT('Ctrl Pts',(-8.10184785540617,15.2,-7.77913802034602));
#280733=CARTESIAN_POINT('Ctrl Pts',(-8.10320369006516,15.2,-7.78231163973143));
#280734=CARTESIAN_POINT('Ctrl Pts',(-8.10455862031101,15.2,-7.7854934905709));
#280735=CARTESIAN_POINT('Ctrl Pts',(-8.10591260651796,15.2,-7.78868355205287));
#280736=CARTESIAN_POINT('Ctrl Pts',(-8.10726659272491,15.2,-7.79187361353483));
#280737=CARTESIAN_POINT('Ctrl Pts',(-8.10861963499181,15.2,-7.79507188608236));
#280738=CARTESIAN_POINT('Ctrl Pts',(-8.10997169278217,15.2,-7.79827834752205));
#280739=CARTESIAN_POINT('Ctrl Pts',(-8.11132375057252,15.2,-7.80148480896174));
#280740=CARTESIAN_POINT('Ctrl Pts',(-8.11267482528518,15.2,-7.80469945793326));
#280741=CARTESIAN_POINT('Ctrl Pts',(-8.11402487511122,15.2,-7.80792227489881));
#280742=CARTESIAN_POINT('Ctrl Pts',(-8.11537492493727,15.2,-7.81114509186436));
#280743=CARTESIAN_POINT('Ctrl Pts',(-8.1167239517217,15.2,-7.81437607632928));
#280744=CARTESIAN_POINT('Ctrl Pts',(-8.11807191546454,15.2,-7.81761520579384));
#280745=CARTESIAN_POINT('Ctrl Pts',(-8.11941987945226,15.2,-7.82085433584683));
#280746=CARTESIAN_POINT('Ctrl Pts',(-8.12076678004801,15.2,-7.82410161065208));
#280747=CARTESIAN_POINT('Ctrl Pts',(-8.12211257899344,15.2,-7.82735700970964));
#280748=CARTESIAN_POINT('Ctrl Pts',(-8.12345837769439,15.2,-7.8306124081758));
#280749=CARTESIAN_POINT('Ctrl Pts',(-8.12480307457515,15.2,-7.8338759306875));
#280750=CARTESIAN_POINT('Ctrl Pts',(-8.12614663080166,15.2,-7.83714755489968));
#280751=CARTESIAN_POINT('Ctrl Pts',(-8.12749018702817,15.2,-7.84041917911187));
#280752=CARTESIAN_POINT('Ctrl Pts',(-8.12883260141174,15.2,-7.84369890577722));
#280753=CARTESIAN_POINT('Ctrl Pts',(-8.13017383765457,15.2,-7.84698671232513));
#280754=CARTESIAN_POINT('Ctrl Pts',(-8.1315150738974,15.2,-7.85027451887304));
#280755=CARTESIAN_POINT('Ctrl Pts',(-8.13285513171538,15.2,-7.85357040655335));
#280756=CARTESIAN_POINT('Ctrl Pts',(-8.13419397100006,15.2,-7.85687435301662));
#280757=CARTESIAN_POINT('Ctrl Pts',(-8.13597909020845,15.2,-7.8612796153678));
#280758=CARTESIAN_POINT('Ctrl Pts',(-8.13776204531384,15.2,-7.86569920457347));
#280759=CARTESIAN_POINT('Ctrl Pts',(-8.13954274579954,15.2,-7.87013306898324));
#280760=CARTESIAN_POINT('Ctrl Pts',(-8.1408782710425,15.2,-7.8734584669885));
#280761=CARTESIAN_POINT('Ctrl Pts',(-8.14221252822721,15.2,-7.87679189515169));
#280762=CARTESIAN_POINT('Ctrl Pts',(-8.14354547997034,15.2,-7.88013333211432));
#280763=CARTESIAN_POINT('Ctrl Pts',(-8.14487843171346,15.2,-7.88347476907694));
#280764=CARTESIAN_POINT('Ctrl Pts',(-8.14621007741024,15.2,-7.88682421454305));
#280765=CARTESIAN_POINT('Ctrl Pts',(-8.14754038024294,15.2,-7.89018164701968));
#280766=CARTESIAN_POINT('Ctrl Pts',(-8.14887068307564,15.2,-7.8935390794963));
#280767=CARTESIAN_POINT('Ctrl Pts',(-8.15019964362439,15.2,-7.89690449907083));
#280768=CARTESIAN_POINT('Ctrl Pts',(-8.15152722299886,15.2,-7.90027788450523));
#280769=CARTESIAN_POINT('Ctrl Pts',(-8.15285480237333,15.2,-7.90365126993963));
#280770=CARTESIAN_POINT('Ctrl Pts',(-8.15418100253699,15.2,-7.90703262048783));
#280771=CARTESIAN_POINT('Ctrl Pts',(-8.15550578482231,15.2,-7.91042191540566));
#280772=CARTESIAN_POINT('Ctrl Pts',(-8.15683056710763,15.2,-7.91381121032349));
#280773=CARTESIAN_POINT('Ctrl Pts',(-8.15815393230972,15.2,-7.91720844841578));
#280774=CARTESIAN_POINT('Ctrl Pts',(-8.15947584401189,15.2,-7.92061361074931));
#280775=CARTESIAN_POINT('Ctrl Pts',(-8.1607977559542,15.2,-7.92401877370144));
#280776=CARTESIAN_POINT('Ctrl Pts',(-8.16211821336277,15.2,-7.9274318581808));
#280777=CARTESIAN_POINT('Ctrl Pts',(-8.16343718180427,15.2,-7.93085284430408));
#280778=CARTESIAN_POINT('Ctrl Pts',(-8.16475615000615,15.2,-7.93427382980588));
#280779=CARTESIAN_POINT('Ctrl Pts',(-8.16607362742023,15.2,-7.93770271745056));
#280780=CARTESIAN_POINT('Ctrl Pts',(-8.16738957877132,15.2,-7.9411394841233));
#280781=CARTESIAN_POINT('Ctrl Pts',(-8.1687055301224,15.2,-7.94457625079604));
#280782=CARTESIAN_POINT('Ctrl Pts',(-8.17001995477432,15.2,-7.94802089676783));
#280783=CARTESIAN_POINT('Ctrl Pts',(-8.17133281710148,15.2,-7.95147340168475));
#280784=CARTESIAN_POINT('Ctrl Pts',(-8.17264567942864,15.2,-7.95492590660167));
#280785=CARTESIAN_POINT('Ctrl Pts',(-8.17395697999766,15.2,-7.95838626900931));
#280786=CARTESIAN_POINT('Ctrl Pts',(-8.17526668274173,15.2,-7.96185446946661));
#280787=CARTESIAN_POINT('Ctrl Pts',(-8.17701295322578,15.2,-7.96647873716306));
#280788=CARTESIAN_POINT('Ctrl Pts',(-8.17875638333175,15.2,-7.97111693799453));
#280789=CARTESIAN_POINT('Ctrl Pts',(-8.18049688925963,15.2,-7.97576902102724));
#280790=CARTESIAN_POINT('Ctrl Pts',(-8.18180226858697,15.2,-7.97925808298485));
#280791=CARTESIAN_POINT('Ctrl Pts',(-8.18310600370109,15.2,-7.98275495329611));
#280792=CARTESIAN_POINT('Ctrl Pts',(-8.18440805655197,15.2,-7.9862596104281));
#280793=CARTESIAN_POINT('Ctrl Pts',(-8.18571010940285,15.2,-7.98976426756009));
#280794=CARTESIAN_POINT('Ctrl Pts',(-8.1870104792056,15.2,-7.9932767103777));
#280795=CARTESIAN_POINT('Ctrl Pts',(-8.18830913461659,15.2,-7.99679691987545));
#280796=CARTESIAN_POINT('Ctrl Pts',(-8.18960779002758,15.2,-8.00031712937321));
#280797=CARTESIAN_POINT('Ctrl Pts',(-8.19090473189713,15.2,-8.00384510606176));
#280798=CARTESIAN_POINT('Ctrl Pts',(-8.19219992676674,15.2,-8.00738082855829));
#280799=CARTESIAN_POINT('Ctrl Pts',(-8.19349512163635,15.2,-8.01091655105482));
#280800=CARTESIAN_POINT('Ctrl Pts',(-8.19478857108935,15.2,-8.01446002052605));
#280801=CARTESIAN_POINT('Ctrl Pts',(-8.19608023433425,15.2,-8.01801121339634));
#280802=CARTESIAN_POINT('Ctrl Pts',(-8.19737189757914,15.2,-8.02156240626663));
#280803=CARTESIAN_POINT('Ctrl Pts',(-8.19866177459974,15.2,-8.02512132039559));
#280804=CARTESIAN_POINT('Ctrl Pts',(-8.19994982449251,15.2,-8.02868793252666));
#280805=CARTESIAN_POINT('Ctrl Pts',(-8.20123787438529,15.2,-8.03225454465772));
#280806=CARTESIAN_POINT('Ctrl Pts',(-8.20252409654982,15.2,-8.03582885306697));
#280807=CARTESIAN_POINT('Ctrl Pts',(-8.20380846725341,15.2,-8.03941084372744));
#280808=CARTESIAN_POINT('Ctrl Pts',(-8.2055209616804,15.2,-8.04418683170854));
#280809=CARTESIAN_POINT('Ctrl Pts',(-8.20723016286852,15.2,-8.04897647635779));
#280810=CARTESIAN_POINT('Ctrl Pts',(-8.20893607000006,15.2,-8.05377977100001));
#280811=CARTESIAN_POINT('Ctrl Pts',(-7.64657512400006,12.2,-7.01216898700002));
#280812=CARTESIAN_POINT('Ctrl Pts',(-7.64778328679899,12.2,-7.01348522587027));
#280813=CARTESIAN_POINT('Ctrl Pts',(-7.64902613388113,12.2,-7.01484722203433));
#280814=CARTESIAN_POINT('Ctrl Pts',(-7.65030255133521,12.2,-7.01625467938746));
#280815=CARTESIAN_POINT('Ctrl Pts',(-7.65158512431943,12.2,-7.01766892421138));
#280816=CARTESIAN_POINT('Ctrl Pts',(-7.65290158882944,12.2,-7.01912907735244));
#280817=CARTESIAN_POINT('Ctrl Pts',(-7.65425083088893,12.2,-7.02063486217904));
#280818=CARTESIAN_POINT('Ctrl Pts',(-7.65560007282589,12.2,-7.02214064686888));
#280819=CARTESIAN_POINT('Ctrl Pts',(-7.6569820926347,12.2,-7.02369206393294));
#280820=CARTESIAN_POINT('Ctrl Pts',(-7.65839581074999,12.2,-7.02528884179159));
#280821=CARTESIAN_POINT('Ctrl Pts',(-7.65980952886529,12.2,-7.02688561965024));
#280822=CARTESIAN_POINT('Ctrl Pts',(-7.66125494568895,12.2,-7.02852776104979));
#280823=CARTESIAN_POINT('Ctrl Pts',(-7.66273101487395,12.2,-7.03021499707016));
#280824=CARTESIAN_POINT('Ctrl Pts',(-7.66420708419303,12.2,-7.03190223324379));
#280825=CARTESIAN_POINT('Ctrl Pts',(-7.66571380278172,12.2,-7.03363456758543));
#280826=CARTESIAN_POINT('Ctrl Pts',(-7.66725015536747,12.2,-7.03541173743532));
#280827=CARTESIAN_POINT('Ctrl Pts',(-7.66878650781365,12.2,-7.03718890712378));
#280828=CARTESIAN_POINT('Ctrl Pts',(-7.67035249574304,12.2,-7.03901091194339));
#280829=CARTESIAN_POINT('Ctrl Pts',(-7.67194712427573,12.2,-7.04087749571745));
#280830=CARTESIAN_POINT('Ctrl Pts',(-7.67354175280843,12.2,-7.04274407949153));
#280831=CARTESIAN_POINT('Ctrl Pts',(-7.67516502602135,12.2,-7.04465524296655));
#280832=CARTESIAN_POINT('Ctrl Pts',(-7.67681598062681,12.2,-7.04661073189355));
#280833=CARTESIAN_POINT('Ctrl Pts',(-7.67846693538224,12.2,-7.04856622099817));
#280834=CARTESIAN_POINT('Ctrl Pts',(-7.68014557084944,12.2,-7.05056603617498));
#280835=CARTESIAN_POINT('Ctrl Pts',(-7.68185095069424,12.2,-7.05260992995607));
#280836=CARTESIAN_POINT('Ctrl Pts',(-7.68355633038413,12.2,-7.05465382355151));
#280837=CARTESIAN_POINT('Ctrl Pts',(-7.68528845682534,12.2,-7.05674179384187));
#280838=CARTESIAN_POINT('Ctrl Pts',(-7.68704641459593,12.2,-7.05887359659964));
#280839=CARTESIAN_POINT('Ctrl Pts',(-7.68880437236652,12.2,-7.06100539935743));
#280840=CARTESIAN_POINT('Ctrl Pts',(-7.69058816346834,12.2,-7.06318103452004));
#280841=CARTESIAN_POINT('Ctrl Pts',(-7.69239689940154,12.2,-7.06540025935418));
#280842=CARTESIAN_POINT('Ctrl Pts',(-7.69420563533474,12.2,-7.06761948418832));
#280843=CARTESIAN_POINT('Ctrl Pts',(-7.69603931658333,12.2,-7.06988230103532));
#280844=CARTESIAN_POINT('Ctrl Pts',(-7.69789707751419,12.2,-7.07218846778191));
#280845=CARTESIAN_POINT('Ctrl Pts',(-7.6997548386138,12.2,-7.07449463473798));
#280846=CARTESIAN_POINT('Ctrl Pts',(-7.7016366791741,12.2,-7.07684415463993));
#280847=CARTESIAN_POINT('Ctrl Pts',(-7.70354175636227,12.2,-7.07923678885552));
#280848=CARTESIAN_POINT('Ctrl Pts',(-7.70544683337737,12.2,-7.08162942285377));
#280849=CARTESIAN_POINT('Ctrl Pts',(-7.70737514672789,12.2,-7.08406517436941));
#280850=CARTESIAN_POINT('Ctrl Pts',(-7.70932587299913,12.2,-7.08654380820715));
#280851=CARTESIAN_POINT('Ctrl Pts',(-7.71127659927036,12.2,-7.08902244204489));
#280852=CARTESIAN_POINT('Ctrl Pts',(-7.71324973925656,12.2,-7.09154395937487));
#280853=CARTESIAN_POINT('Ctrl Pts',(-7.71524449051593,12.2,-7.09410813019545));
#280854=CARTESIAN_POINT('Ctrl Pts',(-7.71723924195649,12.2,-7.09667230124895));
#280855=CARTESIAN_POINT('Ctrl Pts',(-7.71925560443252,12.2,-7.09927912477326));
#280856=CARTESIAN_POINT('Ctrl Pts',(-7.7212927938778,12.2,-7.10192837566951));
#280857=CARTESIAN_POINT('Ctrl Pts',(-7.72332998313804,12.2,-7.10457762632511));
#280858=CARTESIAN_POINT('Ctrl Pts',(-7.72538800039851,12.2,-7.10726930092738));
#280859=CARTESIAN_POINT('Ctrl Pts',(-7.72746607899907,12.2,-7.11000317792369));
#280860=CARTESIAN_POINT('Ctrl Pts',(-7.72954415759963,12.2,-7.11273705492002));
#280861=CARTESIAN_POINT('Ctrl Pts',(-7.73164230023916,12.2,-7.11551313281472));
#280862=CARTESIAN_POINT('Ctrl Pts',(-7.73375975674422,12.2,-7.11833118970945));
#280863=CARTESIAN_POINT('Ctrl Pts',(-7.73587721344161,12.2,-7.12114924686015));
#280864=CARTESIAN_POINT('Ctrl Pts',(-7.73801398519903,12.2,-7.12400928335858));
#280865=CARTESIAN_POINT('Ctrl Pts',(-7.74016934292524,12.2,-7.12691107683076));
#280866=CARTESIAN_POINT('Ctrl Pts',(-7.74232470045566,12.2,-7.12981287003937));
#280867=CARTESIAN_POINT('Ctrl Pts',(-7.74449864221298,12.2,-7.13275642378339));
#280868=CARTESIAN_POINT('Ctrl Pts',(-7.74669045496669,12.2,-7.13574151575828));
#280869=CARTESIAN_POINT('Ctrl Pts',(-7.74888226772041,12.2,-7.13872660773317));
#280870=CARTESIAN_POINT('Ctrl Pts',(-7.751091952672,12.2,-7.14175324162222));
#280871=CARTESIAN_POINT('Ctrl Pts',(-7.75331881053465,12.2,-7.14482119791159));
#280872=CARTESIAN_POINT('Ctrl Pts',(-7.75554566859958,12.2,-7.14788915447965));
#280873=CARTESIAN_POINT('Ctrl Pts',(-7.75778970044715,12.2,-7.15099843786056));
#280874=CARTESIAN_POINT('Ctrl Pts',(-7.7600502224881,12.2,-7.15414883011836));
#280875=CARTESIAN_POINT('Ctrl Pts',(-7.76231074432374,12.2,-7.15729922209));
#280876=CARTESIAN_POINT('Ctrl Pts',(-7.76458775655725,12.2,-7.16049072517075));
#280877=CARTESIAN_POINT('Ctrl Pts',(-7.76688059148441,12.2,-7.16372312523475));
#280878=CARTESIAN_POINT('Ctrl Pts',(-7.76917342641157,12.2,-7.16695552529877));
#280879=CARTESIAN_POINT('Ctrl Pts',(-7.77148208440854,12.2,-7.17022882502502));
#280880=CARTESIAN_POINT('Ctrl Pts',(-7.77380591132343,12.2,-7.17354281106948));
#280881=CARTESIAN_POINT('Ctrl Pts',(-7.77574243382287,12.2,-7.17630446620688));
#280882=CARTESIAN_POINT('Ctrl Pts',(-7.77768949117817,12.2,-7.17909437651173));
#280883=CARTESIAN_POINT('Ctrl Pts',(-7.77964671041376,12.2,-7.18191242227415));
#280884=CARTESIAN_POINT('Ctrl Pts',(-7.78160392964934,12.2,-7.18473046803657));
#280885=CARTESIAN_POINT('Ctrl Pts',(-7.78357131294001,12.2,-7.18757664781319));
#280886=CARTESIAN_POINT('Ctrl Pts',(-7.78554849399063,12.2,-7.19045084275673));
#280887=CARTESIAN_POINT('Ctrl Pts',(-7.78752567504125,12.2,-7.19332503770025));
#280888=CARTESIAN_POINT('Ctrl Pts',(-7.78951265463893,12.2,-7.19622724628885));
#280889=CARTESIAN_POINT('Ctrl Pts',(-7.79150907470837,12.2,-7.19915735052494));
#280890=CARTESIAN_POINT('Ctrl Pts',(-7.79350549477779,12.2,-7.20208745476104));
#280891=CARTESIAN_POINT('Ctrl Pts',(-7.79551135383639,12.2,-7.2050454544546));
#280892=CARTESIAN_POINT('Ctrl Pts',(-7.79752630148447,12.2,-7.20803123050992));
#280893=CARTESIAN_POINT('Ctrl Pts',(-7.79954124913254,12.2,-7.21101700656522));
#280894=CARTESIAN_POINT('Ctrl Pts',(-7.80156528368812,12.2,-7.21403056018645));
#280895=CARTESIAN_POINT('Ctrl Pts',(-7.80359806042469,12.2,-7.217071771924));
#280896=CARTESIAN_POINT('Ctrl Pts',(-7.80563083716125,12.2,-7.22011298366153));
#280897=CARTESIAN_POINT('Ctrl Pts',(-7.80767235392262,12.2,-7.2231818550512));
#280898=CARTESIAN_POINT('Ctrl Pts',(-7.80972227170081,12.2,-7.22627826692761));
#280899=CARTESIAN_POINT('Ctrl Pts',(-7.81177218947903,12.2,-7.22937467880403));
#280900=CARTESIAN_POINT('Ctrl Pts',(-7.81383050736948,12.2,-7.2324986330732));
#280901=CARTESIAN_POINT('Ctrl Pts',(-7.81589689101494,12.2,-7.23565001385754));
#280902=CARTESIAN_POINT('Ctrl Pts',(-7.81796327466039,12.2,-7.23880139464188));
#280903=CARTESIAN_POINT('Ctrl Pts',(-7.82003772227731,12.2,-7.24198019922819));
#280904=CARTESIAN_POINT('Ctrl Pts',(-7.8221199067224,12.2,-7.24518631270266));
#280905=CARTESIAN_POINT('Ctrl Pts',(-7.82420209116748,12.2,-7.24839242617712));
#280906=CARTESIAN_POINT('Ctrl Pts',(-7.826292010146,12.2,-7.251625849902));
#280907=CARTESIAN_POINT('Ctrl Pts',(-7.82838933979937,12.2,-7.25488646816811));
#280908=CARTESIAN_POINT('Ctrl Pts',(-7.83048666922415,12.2,-7.25814708607882));
#280909=CARTESIAN_POINT('Ctrl Pts',(-7.83259141104903,12.2,-7.26143489747436));
#280910=CARTESIAN_POINT('Ctrl Pts',(-7.83470324366548,12.2,-7.26474978954136));
#280911=CARTESIAN_POINT('Ctrl Pts',(-7.8368150765121,12.2,-7.26806468196968));
#280912=CARTESIAN_POINT('Ctrl Pts',(-7.83893400051145,12.2,-7.27140665157263));
#280913=CARTESIAN_POINT('Ctrl Pts',(-7.84105970245533,12.2,-7.27477558900097));
#280914=CARTESIAN_POINT('Ctrl Pts',(-7.84318540439921,12.2,-7.2781445264293));
#280915=CARTESIAN_POINT('Ctrl Pts',(-7.8453178832708,12.2,-7.28154042926556));
#280916=CARTESIAN_POINT('Ctrl Pts',(-7.84745682972861,12.2,-7.28496318356893));
#280917=CARTESIAN_POINT('Ctrl Pts',(-7.84959577618641,12.2,-7.2883859378723));
#280918=CARTESIAN_POINT('Ctrl Pts',(-7.85174119063212,12.2,-7.2918355454858));
#280919=CARTESIAN_POINT('Ctrl Pts',(-7.8538927687253,12.2,-7.29531189162983));
#280920=CARTESIAN_POINT('Ctrl Pts',(-7.85604434681847,12.2,-7.29878823777386));
#280921=CARTESIAN_POINT('Ctrl Pts',(-7.85820208679777,12.2,-7.30229132184845));
#280922=CARTESIAN_POINT('Ctrl Pts',(-7.86036569061691,12.2,-7.3058210342776));
#280923=CARTESIAN_POINT('Ctrl Pts',(-7.86252929443604,12.2,-7.30935074670676));
#280924=CARTESIAN_POINT('Ctrl Pts',(-7.86469876073591,12.2,-7.31290708506164));
#280925=CARTESIAN_POINT('Ctrl Pts',(-7.86687379608283,12.2,-7.31648993853245));
#280926=CARTESIAN_POINT('Ctrl Pts',(-7.86904883142975,12.2,-7.32007279200327));
#280927=CARTESIAN_POINT('Ctrl Pts',(-7.87122943191116,12.2,-7.32368216048709));
#280928=CARTESIAN_POINT('Ctrl Pts',(-7.87341531074052,12.2,-7.32731793223964));
#280929=CARTESIAN_POINT('Ctrl Pts',(-7.87516401389931,12.2,-7.3302265498002));
#280930=CARTESIAN_POINT('Ctrl Pts',(-7.87691609317994,12.2,-7.33315206547728));
#280931=CARTESIAN_POINT('Ctrl Pts',(-7.8786714030537,12.2,-7.3360944224727));
#280932=CARTESIAN_POINT('Ctrl Pts',(-7.88042671268832,12.2,-7.33903677906723));
#280933=CARTESIAN_POINT('Ctrl Pts',(-7.88218525180583,12.2,-7.34199597845954));
#280934=CARTESIAN_POINT('Ctrl Pts',(-7.88394687610606,12.2,-7.34497196104849));
#280935=CARTESIAN_POINT('Ctrl Pts',(-7.88570850064631,12.2,-7.34794794404292));
#280936=CARTESIAN_POINT('Ctrl Pts',(-7.88747320981609,12.2,-7.35094071248757));
#280937=CARTESIAN_POINT('Ctrl Pts',(-7.88924085922323,12.2,-7.35395020947008));
#280938=CARTESIAN_POINT('Ctrl Pts',(-7.89100850838953,12.2,-7.35695970604255));
#280939=CARTESIAN_POINT('Ctrl Pts',(-7.89277909937803,12.2,-7.3599859298373));
#280940=CARTESIAN_POINT('Ctrl Pts',(-7.89455248912176,12.2,-7.36302882630968));
#280941=CARTESIAN_POINT('Ctrl Pts',(-7.89632587910712,12.2,-7.36607172319666));
#280942=CARTESIAN_POINT('Ctrl Pts',(-7.89810206675392,12.2,-7.36913129149951));
#280943=CARTESIAN_POINT('Ctrl Pts',(-7.89988091462883,12.2,-7.37220747700159));
#280944=CARTESIAN_POINT('Ctrl Pts',(-7.90165976226136,12.2,-7.37528366208455));
#280945=CARTESIAN_POINT('Ctrl Pts',(-7.9034412671759,12.2,-7.37837646237136));
#280946=CARTESIAN_POINT('Ctrl Pts',(-7.90522529300786,12.2,-7.38148582304886));
#280947=CARTESIAN_POINT('Ctrl Pts',(-7.90700931908289,12.2,-7.38459518415));
#280948=CARTESIAN_POINT('Ctrl Pts',(-7.90879586575977,12.2,-7.38772110534021));
#280949=CARTESIAN_POINT('Ctrl Pts',(-7.91058479441298,12.2,-7.39086353029033));
#280950=CARTESIAN_POINT('Ctrl Pts',(-7.91237372282244,12.2,-7.39400595481229));
#280951=CARTESIAN_POINT('Ctrl Pts',(-7.91416503376754,12.2,-7.39716488463093));
#280952=CARTESIAN_POINT('Ctrl Pts',(-7.9159585922318,12.2,-7.40034026248078));
#280953=CARTESIAN_POINT('Ctrl Pts',(-7.91775215094043,12.2,-7.40351564076328));
#280954=CARTESIAN_POINT('Ctrl Pts',(-7.91954795652011,12.2,-7.40670746824044));
#280955=CARTESIAN_POINT('Ctrl Pts',(-7.92134587579294,12.2,-7.40991568798548));
#280956=CARTESIAN_POINT('Ctrl Pts',(-7.9231437948208,12.2,-7.41312390729339));
#280957=CARTESIAN_POINT('Ctrl Pts',(-7.92494382559738,12.2,-7.41634852125891));
#280958=CARTESIAN_POINT('Ctrl Pts',(-7.92674583800542,12.2,-7.41958947243673));
#280959=CARTESIAN_POINT('Ctrl Pts',(-7.92854785065898,12.2,-7.42283042405612));
#280960=CARTESIAN_POINT('Ctrl Pts',(-7.93035184389329,12.2,-7.42608771360763));
#280961=CARTESIAN_POINT('Ctrl Pts',(-7.93215768549172,12.2,-7.42936128650828));
#280962=CARTESIAN_POINT('Ctrl Pts',(-7.93396352709014,12.2,-7.43263485940892));
#280963=CARTESIAN_POINT('Ctrl Pts',(-7.9357712199971,12.2,-7.43592471539755));
#280964=CARTESIAN_POINT('Ctrl Pts',(-7.93758063076256,12.2,-7.43923079902384));
#280965=CARTESIAN_POINT('Ctrl Pts',(-7.93939004128148,12.2,-7.44253688219967));
#280966=CARTESIAN_POINT('Ctrl Pts',(-7.94120117155267,12.2,-7.44585919355828));
#280967=CARTESIAN_POINT('Ctrl Pts',(-7.94301389402381,12.2,-7.44919767802268));
#280968=CARTESIAN_POINT('Ctrl Pts',(-7.94482661674193,12.2,-7.45253616294194));
#280969=CARTESIAN_POINT('Ctrl Pts',(-7.94664092989783,12.2,-7.45589082048797));
#280970=CARTESIAN_POINT('Ctrl Pts',(-7.94845670799693,12.2,-7.45926159678441));
#280971=CARTESIAN_POINT('Ctrl Pts',(-7.95027248584863,12.2,-7.46263237262158));
#280972=CARTESIAN_POINT('Ctrl Pts',(-7.95208972816681,12.2,-7.46601926705391));
#280973=CARTESIAN_POINT('Ctrl Pts',(-7.9539083093514,12.2,-7.46942222549692));
#280974=CARTESIAN_POINT('Ctrl Pts',(-7.95572689078377,12.2,-7.47282518440357));
#280975=CARTESIAN_POINT('Ctrl Pts',(-7.95754681050731,12.2,-7.47624420602161));
#280976=CARTESIAN_POINT('Ctrl Pts',(-7.95936794603098,12.2,-7.47967923904849));
#280977=CARTESIAN_POINT('Ctrl Pts',(-7.96118908130653,12.2,-7.48311427160735));
#280978=CARTESIAN_POINT('Ctrl Pts',(-7.96301143108625,12.2,-7.48656531198448));
#280979=CARTESIAN_POINT('Ctrl Pts',(-7.964834872326,12.2,-7.49003230903334));
#280980=CARTESIAN_POINT('Ctrl Pts',(-7.96711417406201,12.2,-7.4943660556987));
#280981=CARTESIAN_POINT('Ctrl Pts',(-7.96939518206196,12.2,-7.49872473117026));
#280982=CARTESIAN_POINT('Ctrl Pts',(-7.97167765886746,12.2,-7.50310823144676));
#280983=CARTESIAN_POINT('Ctrl Pts',(-7.97350364041137,12.2,-7.50661503185908));
#280984=CARTESIAN_POINT('Ctrl Pts',(-7.97533056256594,12.2,-7.51013772196472));
#280985=CARTESIAN_POINT('Ctrl Pts',(-7.97715830425694,12.2,-7.51367624378017));
#280986=CARTESIAN_POINT('Ctrl Pts',(-7.9789860456989,12.2,-7.51721476511349));
#280987=CARTESIAN_POINT('Ctrl Pts',(-7.98081460814177,12.2,-7.52076912063723));
#280988=CARTESIAN_POINT('Ctrl Pts',(-7.98264387082552,12.2,-7.52433925573324));
#280989=CARTESIAN_POINT('Ctrl Pts',(-7.9844731337585,12.2,-7.52790939131568));
#280990=CARTESIAN_POINT('Ctrl Pts',(-7.98630309936101,12.2,-7.53149530585554));
#280991=CARTESIAN_POINT('Ctrl Pts',(-7.98813364768304,12.2,-7.53509694755286));
#280992=CARTESIAN_POINT('Ctrl Pts',(-7.98996419575566,12.2,-7.53869858875946));
#280993=CARTESIAN_POINT('Ctrl Pts',(-7.9917953287226,12.2,-7.54231595590735));
#280994=CARTESIAN_POINT('Ctrl Pts',(-7.99362692868392,12.2,-7.5459489956643));
#280995=CARTESIAN_POINT('Ctrl Pts',(-7.9954585288948,12.2,-7.54958203591625));
#280996=CARTESIAN_POINT('Ctrl Pts',(-7.99729059673478,12.2,-7.55323074782494));
#280997=CARTESIAN_POINT('Ctrl Pts',(-7.99912301700964,12.2,-7.55689507948579));
#280998=CARTESIAN_POINT('Ctrl Pts',(-8.00095543703482,12.2,-7.56055941064737));
#280999=CARTESIAN_POINT('Ctrl Pts',(-8.00278821065578,12.2,-7.56423936167444));
#281000=CARTESIAN_POINT('Ctrl Pts',(-8.00462122195036,12.2,-7.56793487687075));
#281001=CARTESIAN_POINT('Ctrl Pts',(-8.00645423349468,12.2,-7.57163039257056));
#281002=CARTESIAN_POINT('Ctrl Pts',(-8.00828748325846,12.2,-7.57534147510517));
#281003=CARTESIAN_POINT('Ctrl Pts',(-8.01012085952506,12.2,-7.57906806947495));
#281004=CARTESIAN_POINT('Ctrl Pts',(-8.01195423579165,12.2,-7.58279466384472));
#281005=CARTESIAN_POINT('Ctrl Pts',(-8.01378773657214,12.2,-7.58653676989129));
#281006=CARTESIAN_POINT('Ctrl Pts',(-8.01562125278317,12.2,-7.59029433609766));
#281007=CARTESIAN_POINT('Ctrl Pts',(-8.01745476874439,12.2,-7.59405190179206));
#281008=CARTESIAN_POINT('Ctrl Pts',(-8.01928829781258,12.2,-7.59782492632881));
#281009=CARTESIAN_POINT('Ctrl Pts',(-8.02112173178214,12.2,-7.6016133574807));
#281010=CARTESIAN_POINT('Ctrl Pts',(-8.0229551660015,12.2,-7.60540178914877));
#281011=CARTESIAN_POINT('Ctrl Pts',(-8.02478850271655,12.2,-7.60920562673968));
#281012=CARTESIAN_POINT('Ctrl Pts',(-8.02662163481644,12.2,-7.61302481711606));
#281013=CARTESIAN_POINT('Ctrl Pts',(-8.02845476666656,12.2,-7.61684400697208));
#281014=CARTESIAN_POINT('Ctrl Pts',(-8.0302876903417,12.2,-7.62067855060665));
#281015=CARTESIAN_POINT('Ctrl Pts',(-8.03212030235857,12.2,-7.62452839440204));
#281016=CARTESIAN_POINT('Ctrl Pts',(-8.03395291462513,12.2,-7.62837823872196));
#281017=CARTESIAN_POINT('Ctrl Pts',(-8.03578521218844,12.2,-7.632243385587));
#281018=CARTESIAN_POINT('Ctrl Pts',(-8.03761708799087,12.2,-7.63612377760477));
#281019=CARTESIAN_POINT('Ctrl Pts',(-8.03944896354372,12.2,-7.64000416909386));
#281020=CARTESIAN_POINT('Ctrl Pts',(-8.04128041861114,12.2,-7.64389980889278));
#281021=CARTESIAN_POINT('Ctrl Pts',(-8.04311134535038,12.2,-7.64781064340539));
#281022=CARTESIAN_POINT('Ctrl Pts',(-8.04494227233908,12.2,-7.65172147845086));
#281023=CARTESIAN_POINT('Ctrl Pts',(-8.04677267074162,12.2,-7.65564750982872));
#281024=CARTESIAN_POINT('Ctrl Pts',(-8.04860243767464,12.2,-7.65958868282229));
#281025=CARTESIAN_POINT('Ctrl Pts',(-8.05043220435835,12.2,-7.66352985527887));
#281026=CARTESIAN_POINT('Ctrl Pts',(-8.05226133673446,12.2,-7.66748616979299));
#281027=CARTESIAN_POINT('Ctrl Pts',(-8.05408973350974,12.2,-7.67145757516543));
#281028=CARTESIAN_POINT('Ctrl Pts',(-8.05591813053414,12.2,-7.67542898107897));
#281029=CARTESIAN_POINT('Ctrl Pts',(-8.05774579051655,12.2,-7.67941547698038));
#281030=CARTESIAN_POINT('Ctrl Pts',(-8.05957260961606,12.2,-7.68341701064389));
#281031=CARTESIAN_POINT('Ctrl Pts',(-8.061856133366,12.2,-7.68841892745067));
#281032=CARTESIAN_POINT('Ctrl Pts',(-8.06413834403262,12.2,-7.69344434071793));
#281033=CARTESIAN_POINT('Ctrl Pts',(-8.06641904340754,12.2,-7.69849314828861));
#281034=CARTESIAN_POINT('Ctrl Pts',(-8.06824360275832,12.2,-7.70253219401496));
#281035=CARTESIAN_POINT('Ctrl Pts',(-8.070067194374,12.2,-7.70658621244861));
#281036=CARTESIAN_POINT('Ctrl Pts',(-8.0718897172606,12.2,-7.71065515115128));
#281037=CARTESIAN_POINT('Ctrl Pts',(-8.0737122403955,12.2,-7.71472409040834));
#281038=CARTESIAN_POINT('Ctrl Pts',(-8.07553369376639,12.2,-7.71880794960248));
#281039=CARTESIAN_POINT('Ctrl Pts',(-8.07735397886553,12.2,-7.72290667732684));
#281040=CARTESIAN_POINT('Ctrl Pts',(-8.07871919256587,12.2,-7.72598072284089));
#281041=CARTESIAN_POINT('Ctrl Pts',(-8.08008374933296,12.2,-7.72906313216229));
#281042=CARTESIAN_POINT('Ctrl Pts',(-8.08144760649173,12.2,-7.73215388225828));
#281043=CARTESIAN_POINT('Ctrl Pts',(-8.08281146365049,12.2,-7.73524463235428));
#281044=CARTESIAN_POINT('Ctrl Pts',(-8.08417462120097,12.2,-7.73834372525835));
#281045=CARTESIAN_POINT('Ctrl Pts',(-8.08553703835988,12.2,-7.74145113639472));
#281046=CARTESIAN_POINT('Ctrl Pts',(-8.08689945551878,12.2,-7.7445585475311));
#281047=CARTESIAN_POINT('Ctrl Pts',(-8.08826113143478,12.2,-7.74767427943733));
#281048=CARTESIAN_POINT('Ctrl Pts',(-8.08962202570342,12.2,-7.75079830860395));
#281049=CARTESIAN_POINT('Ctrl Pts',(-8.09098291997206,12.2,-7.75392233777057));
#281050=CARTESIAN_POINT('Ctrl Pts',(-8.09234303323634,12.2,-7.75705466433054));
#281051=CARTESIAN_POINT('Ctrl Pts',(-8.09370232202041,12.2,-7.76019526679865));
#281052=CARTESIAN_POINT('Ctrl Pts',(-8.09506161105141,12.2,-7.76333586983731));
#281053=CARTESIAN_POINT('Ctrl Pts',(-8.09642007779883,12.2,-7.7664847491616));
#281054=CARTESIAN_POINT('Ctrl Pts',(-8.09777768028768,12.2,-7.76964188220488));
#281055=CARTESIAN_POINT('Ctrl Pts',(-8.09913528252989,12.2,-7.77279901467461));
#281056=CARTESIAN_POINT('Ctrl Pts',(-8.10049202074717,12.2,-7.77596440096061));
#281057=CARTESIAN_POINT('Ctrl Pts',(-8.10184785540617,12.2,-7.77913802034602));
#281058=CARTESIAN_POINT('Ctrl Pts',(-8.10320369006516,12.2,-7.78231163973142));
#281059=CARTESIAN_POINT('Ctrl Pts',(-8.10455862031101,12.2,-7.7854934905709));
#281060=CARTESIAN_POINT('Ctrl Pts',(-8.10591260651796,12.2,-7.78868355205286));
#281061=CARTESIAN_POINT('Ctrl Pts',(-8.10726659272491,12.2,-7.79187361353483));
#281062=CARTESIAN_POINT('Ctrl Pts',(-8.10861963499181,12.2,-7.79507188608236));
#281063=CARTESIAN_POINT('Ctrl Pts',(-8.10997169278217,12.2,-7.79827834752205));
#281064=CARTESIAN_POINT('Ctrl Pts',(-8.11132375057252,12.2,-7.80148480896174));
#281065=CARTESIAN_POINT('Ctrl Pts',(-8.11267482528518,12.2,-7.80469945793325));
#281066=CARTESIAN_POINT('Ctrl Pts',(-8.11402487511122,12.2,-7.80792227489881));
#281067=CARTESIAN_POINT('Ctrl Pts',(-8.11537492493727,12.2,-7.81114509186436));
#281068=CARTESIAN_POINT('Ctrl Pts',(-8.1167239517217,12.2,-7.81437607632928));
#281069=CARTESIAN_POINT('Ctrl Pts',(-8.11807191546454,12.2,-7.81761520579384));
#281070=CARTESIAN_POINT('Ctrl Pts',(-8.11941987945226,12.2,-7.82085433584683));
#281071=CARTESIAN_POINT('Ctrl Pts',(-8.12076678004801,12.2,-7.82410161065208));
#281072=CARTESIAN_POINT('Ctrl Pts',(-8.12211257899344,12.2,-7.82735700970964));
#281073=CARTESIAN_POINT('Ctrl Pts',(-8.12390697717988,12.2,-7.83169754080072));
#281074=CARTESIAN_POINT('Ctrl Pts',(-8.12569941704539,12.2,-7.83605251407049));
#281075=CARTESIAN_POINT('Ctrl Pts',(-8.12748980474051,12.2,-7.84042187845532));
#281076=CARTESIAN_POINT('Ctrl Pts',(-8.12883259557284,12.2,-7.84369890189279));
#281077=CARTESIAN_POINT('Ctrl Pts',(-8.13017423313587,12.2,-7.84698401969482));
#281078=CARTESIAN_POINT('Ctrl Pts',(-8.13151467933727,12.2,-7.85027721115781));
#281079=CARTESIAN_POINT('Ctrl Pts',(-8.13330194110149,12.2,-7.85466813350729));
#281080=CARTESIAN_POINT('Ctrl Pts',(-8.13508708265155,12.2,-7.8590734087585));
#281081=CARTESIAN_POINT('Ctrl Pts',(-8.13687001513746,12.2,-7.86349298511139));
#281082=CARTESIAN_POINT('Ctrl Pts',(-8.13820721438043,12.2,-7.86680766707499));
#281083=CARTESIAN_POINT('Ctrl Pts',(-8.13954317114856,12.2,-7.87013039323764));
#281084=CARTESIAN_POINT('Ctrl Pts',(-8.14087784651673,12.2,-7.87346114224161));
#281085=CARTESIAN_POINT('Ctrl Pts',(-8.1422125218849,12.2,-7.87679189124559));
#281086=CARTESIAN_POINT('Ctrl Pts',(-8.14354591771979,12.2,-7.88013066364091));
#281087=CARTESIAN_POINT('Ctrl Pts',(-8.14487799454652,12.2,-7.88347743714363));
#281088=CARTESIAN_POINT('Ctrl Pts',(-8.14621007137323,12.2,-7.88682421064635));
#281089=CARTESIAN_POINT('Ctrl Pts',(-8.1475408302079,12.2,-7.89017898563784));
#281090=CARTESIAN_POINT('Ctrl Pts',(-8.14887023397618,12.2,-7.89354174034943));
#281091=CARTESIAN_POINT('Ctrl Pts',(-8.15019963774445,12.2,-7.89690449506101));
#281092=CARTESIAN_POINT('Ctrl Pts',(-8.15152768522553,12.2,-7.90027523048724));
#281093=CARTESIAN_POINT('Ctrl Pts',(-8.15285434092753,12.2,-7.9036539235301));
#281094=CARTESIAN_POINT('Ctrl Pts',(-8.15418099687053,12.2,-7.90703261718674));
#281095=CARTESIAN_POINT('Ctrl Pts',(-8.15550626026313,12.2,-7.91041926979558));
#281096=CARTESIAN_POINT('Ctrl Pts',(-8.15683009383033,12.2,-7.91381385849832));
#281097=CARTESIAN_POINT('Ctrl Pts',(-8.15815392715703,12.2,-7.91720844658438));
#281098=CARTESIAN_POINT('Ctrl Pts',(-8.15947633197548,12.2,-7.92061097312839));
#281099=CARTESIAN_POINT('Ctrl Pts',(-8.16079726988569,12.2,-7.92402141417183));
#281100=CARTESIAN_POINT('Ctrl Pts',(-8.16211820779591,12.2,-7.92743185521529));
#281101=CARTESIAN_POINT('Ctrl Pts',(-8.1634376811765,12.2,-7.93085021121197));
#281102=CARTESIAN_POINT('Ctrl Pts',(-8.1647556515096,12.2,-7.93427646218641));
#281103=CARTESIAN_POINT('Ctrl Pts',(-8.1660736218427,12.2,-7.93770271316086));
#281104=CARTESIAN_POINT('Ctrl Pts',(-8.16739008997401,12.2,-7.94113685873964));
#281105=CARTESIAN_POINT('Ctrl Pts',(-8.16870501972387,12.2,-7.94457887579683));
#281106=CARTESIAN_POINT('Ctrl Pts',(-8.17001994947374,12.2,-7.94802089285403));
#281107=CARTESIAN_POINT('Ctrl Pts',(-8.1713333401379,12.2,-7.95147078329948));
#281108=CARTESIAN_POINT('Ctrl Pts',(-8.17264515738206,12.2,-7.95492852433987));
#281109=CARTESIAN_POINT('Ctrl Pts',(-8.17395697462621,12.2,-7.95838626538026));
#281110=CARTESIAN_POINT('Ctrl Pts',(-8.17526721787878,12.2,-7.96185185807003));
#281111=CARTESIAN_POINT('Ctrl Pts',(-8.17657585124812,12.2,-7.9653252810261));
#281112=CARTESIAN_POINT('Ctrl Pts',(-8.17788448485519,12.2,-7.96879870461317));
#281113=CARTESIAN_POINT('Ctrl Pts',(-8.17919150969515,12.2,-7.97227995843579));
#281114=CARTESIAN_POINT('Ctrl Pts',(-8.18049688925964,12.2,-7.97576902102725));
#281115=CARTESIAN_POINT('Ctrl Pts',(-8.18180226858697,12.2,-7.97925808298485));
#281116=CARTESIAN_POINT('Ctrl Pts',(-8.18310600370109,12.2,-7.98275495329611));
#281117=CARTESIAN_POINT('Ctrl Pts',(-8.18440805655197,12.2,-7.9862596104281));
#281118=CARTESIAN_POINT('Ctrl Pts',(-8.18614412694096,12.2,-7.99093248639187));
#281119=CARTESIAN_POINT('Ctrl Pts',(-8.18787720500818,12.2,-7.99561920371212));
#281120=CARTESIAN_POINT('Ctrl Pts',(-8.18960721736694,12.2,-8.00031971688249));
#281121=CARTESIAN_POINT('Ctrl Pts',(-8.19133722996142,12.2,-8.0050202306933));
#281122=CARTESIAN_POINT('Ctrl Pts',(-8.19306417772778,12.2,-8.00973453997248));
#281123=CARTESIAN_POINT('Ctrl Pts',(-8.19478797743263,12.2,-8.01446259611994));
#281124=CARTESIAN_POINT('Ctrl Pts',(-8.19608082709383,12.2,-8.01800863790843));
#281125=CARTESIAN_POINT('Ctrl Pts',(-8.19737190427557,12.2,-8.0215624105664));
#281126=CARTESIAN_POINT('Ctrl Pts',(-8.19866116752624,12.2,-8.02512388803653));
#281127=CARTESIAN_POINT('Ctrl Pts',(-8.19995043077691,12.2,-8.02868536550668));
#281128=CARTESIAN_POINT('Ctrl Pts',(-8.20123787865643,12.2,-8.03225454801044));
#281129=CARTESIAN_POINT('Ctrl Pts',(-8.20252348074057,12.2,-8.03583141523005));
#281130=CARTESIAN_POINT('Ctrl Pts',(-8.20466615095866,12.2,-8.04179286081266));
#281131=CARTESIAN_POINT('Ctrl Pts',(-8.20680368620185,12.2,-8.04777565302446));
#281132=CARTESIAN_POINT('Ctrl Pts',(-8.20893607000006,12.2,-8.05377977100001));
#281133=CARTESIAN_POINT('Ctrl Pts',(-7.93573928400006,15.2,-8.32310290900002));
#281134=CARTESIAN_POINT('Ctrl Pts',(-7.93573928400006,11.6,-8.32310290900002));
#281135=CARTESIAN_POINT('Ctrl Pts',(-7.93502251600006,15.2,-8.32283676100002));
#281136=CARTESIAN_POINT('Ctrl Pts',(-7.93502251600006,11.6,-8.32283676100002));
#281137=CARTESIAN_POINT('Ctrl Pts',(-7.93358949600006,15.2,-8.32230434800002));
#281138=CARTESIAN_POINT('Ctrl Pts',(-7.93358949600006,11.6,-8.32230434800002));
#281139=CARTESIAN_POINT('Ctrl Pts',(-7.93144150800006,15.2,-8.32150538100001));
#281140=CARTESIAN_POINT('Ctrl Pts',(-7.93144150800006,11.6,-8.32150538100001));
#281141=CARTESIAN_POINT('Ctrl Pts',(-7.92858060400006,15.2,-8.32043939400002));
#281142=CARTESIAN_POINT('Ctrl Pts',(-7.92858060400006,11.6,-8.32043939400002));
#281143=CARTESIAN_POINT('Ctrl Pts',(-7.92500961100006,15.2,-8.31910574700002));
#281144=CARTESIAN_POINT('Ctrl Pts',(-7.92500961100006,11.6,-8.31910574700002));
#281145=CARTESIAN_POINT('Ctrl Pts',(-7.92144375600006,15.2,-8.31777093800002));
#281146=CARTESIAN_POINT('Ctrl Pts',(-7.92144375600006,11.6,-8.31777093800002));
#281147=CARTESIAN_POINT('Ctrl Pts',(-7.91788304100006,15.2,-8.31643496900002));
#281148=CARTESIAN_POINT('Ctrl Pts',(-7.91788304100006,11.6,-8.31643496900002));
#281149=CARTESIAN_POINT('Ctrl Pts',(-7.91432746600006,15.2,-8.31509784400002));
#281150=CARTESIAN_POINT('Ctrl Pts',(-7.91432746600006,11.6,-8.31509784400002));
#281151=CARTESIAN_POINT('Ctrl Pts',(-7.91077703600005,15.2,-8.31375956800001));
#281152=CARTESIAN_POINT('Ctrl Pts',(-7.91077703600005,11.6,-8.31375956800001));
#281153=CARTESIAN_POINT('Ctrl Pts',(-7.90723175400006,15.2,-8.31242014700001));
#281154=CARTESIAN_POINT('Ctrl Pts',(-7.90723175400006,11.6,-8.31242014700001));
#281155=CARTESIAN_POINT('Ctrl Pts',(-7.90369162500006,15.2,-8.31107959100001));
#281156=CARTESIAN_POINT('Ctrl Pts',(-7.90369162500006,11.6,-8.31107959100001));
#281157=CARTESIAN_POINT('Ctrl Pts',(-7.90015665700006,15.2,-8.30973790700002));
#281158=CARTESIAN_POINT('Ctrl Pts',(-7.90015665700006,11.6,-8.30973790700002));
#281159=CARTESIAN_POINT('Ctrl Pts',(-7.89662685200006,15.2,-8.30839510700002));
#281160=CARTESIAN_POINT('Ctrl Pts',(-7.89662685200006,11.6,-8.30839510700002));
#281161=CARTESIAN_POINT('Ctrl Pts',(-7.89310221700006,15.2,-8.30705119800001));
#281162=CARTESIAN_POINT('Ctrl Pts',(-7.89310221700006,11.6,-8.30705119800001));
#281163=CARTESIAN_POINT('Ctrl Pts',(-7.88958275900006,15.2,-8.30570619200002));
#281164=CARTESIAN_POINT('Ctrl Pts',(-7.88958275900006,11.6,-8.30570619200002));
#281165=CARTESIAN_POINT('Ctrl Pts',(-7.88606848200006,15.2,-8.30436009400002));
#281166=CARTESIAN_POINT('Ctrl Pts',(-7.88606848200006,11.6,-8.30436009400002));
#281167=CARTESIAN_POINT('Ctrl Pts',(-7.88255938900006,15.2,-8.30301291500002));
#281168=CARTESIAN_POINT('Ctrl Pts',(-7.88255938900006,11.6,-8.30301291500002));
#281169=CARTESIAN_POINT('Ctrl Pts',(-7.87905548600006,15.2,-8.30166465900002));
#281170=CARTESIAN_POINT('Ctrl Pts',(-7.87905548600006,11.6,-8.30166465900002));
#281171=CARTESIAN_POINT('Ctrl Pts',(-7.87555677500006,15.2,-8.30031533300001));
#281172=CARTESIAN_POINT('Ctrl Pts',(-7.87555677500006,11.6,-8.30031533300001));
#281173=CARTESIAN_POINT('Ctrl Pts',(-7.87206326300005,15.2,-8.29896494600002));
#281174=CARTESIAN_POINT('Ctrl Pts',(-7.87206326300005,11.6,-8.29896494600002));
#281175=CARTESIAN_POINT('Ctrl Pts',(-7.86857495100006,15.2,-8.29761350400002));
#281176=CARTESIAN_POINT('Ctrl Pts',(-7.86857495100006,11.6,-8.29761350400002));
#281177=CARTESIAN_POINT('Ctrl Pts',(-7.86509184800006,15.2,-8.29626101600001));
#281178=CARTESIAN_POINT('Ctrl Pts',(-7.86509184800006,11.6,-8.29626101600001));
#281179=CARTESIAN_POINT('Ctrl Pts',(-7.86161395500006,15.2,-8.29490748900002));
#281180=CARTESIAN_POINT('Ctrl Pts',(-7.86161395500006,11.6,-8.29490748900002));
#281181=CARTESIAN_POINT('Ctrl Pts',(-7.85814127800006,15.2,-8.29355293000001));
#281182=CARTESIAN_POINT('Ctrl Pts',(-7.85814127800006,11.6,-8.29355293000001));
#281183=CARTESIAN_POINT('Ctrl Pts',(-7.85467382200006,15.2,-8.29219735000001));
#281184=CARTESIAN_POINT('Ctrl Pts',(-7.85467382200006,11.6,-8.29219735000001));
#281185=CARTESIAN_POINT('Ctrl Pts',(-7.85121159100005,15.2,-8.29084075600001));
#281186=CARTESIAN_POINT('Ctrl Pts',(-7.85121159100005,11.6,-8.29084075600001));
#281187=CARTESIAN_POINT('Ctrl Pts',(-7.84775459100005,15.2,-8.28948315400002));
#281188=CARTESIAN_POINT('Ctrl Pts',(-7.84775459100005,11.6,-8.28948315400002));
#281189=CARTESIAN_POINT('Ctrl Pts',(-7.84430282600006,15.2,-8.28812455600002));
#281190=CARTESIAN_POINT('Ctrl Pts',(-7.84430282600006,11.6,-8.28812455600002));
#281191=CARTESIAN_POINT('Ctrl Pts',(-7.84085629900006,15.2,-8.28676496700002));
#281192=CARTESIAN_POINT('Ctrl Pts',(-7.84085629900006,11.6,-8.28676496700002));
#281193=CARTESIAN_POINT('Ctrl Pts',(-7.83741501900005,15.2,-8.28540439500001));
#281194=CARTESIAN_POINT('Ctrl Pts',(-7.83741501900005,11.6,-8.28540439500001));
#281195=CARTESIAN_POINT('Ctrl Pts',(-7.83397898600006,15.2,-8.28404285000002));
#281196=CARTESIAN_POINT('Ctrl Pts',(-7.83397898600006,11.6,-8.28404285000002));
#281197=CARTESIAN_POINT('Ctrl Pts',(-7.83054820600006,15.2,-8.28268033700001));
#281198=CARTESIAN_POINT('Ctrl Pts',(-7.83054820600006,11.6,-8.28268033700001));
#281199=CARTESIAN_POINT('Ctrl Pts',(-7.82712268500006,15.2,-8.28131686600001));
#281200=CARTESIAN_POINT('Ctrl Pts',(-7.82712268500006,11.6,-8.28131686600001));
#281201=CARTESIAN_POINT('Ctrl Pts',(-7.82370242500006,15.2,-8.27995244400002));
#281202=CARTESIAN_POINT('Ctrl Pts',(-7.82370242500006,11.6,-8.27995244400002));
#281203=CARTESIAN_POINT('Ctrl Pts',(-7.82028743300006,15.2,-8.27858708000001));
#281204=CARTESIAN_POINT('Ctrl Pts',(-7.82028743300006,11.6,-8.27858708000001));
#281205=CARTESIAN_POINT('Ctrl Pts',(-7.81687771300006,15.2,-8.27722078100001));
#281206=CARTESIAN_POINT('Ctrl Pts',(-7.81687771300006,11.6,-8.27722078100001));
#281207=CARTESIAN_POINT('Ctrl Pts',(-7.81347326900006,15.2,-8.27585355600002));
#281208=CARTESIAN_POINT('Ctrl Pts',(-7.81347326900006,11.6,-8.27585355600002));
#281209=CARTESIAN_POINT('Ctrl Pts',(-7.81007410700005,15.2,-8.27448541300001));
#281210=CARTESIAN_POINT('Ctrl Pts',(-7.81007410700005,11.6,-8.27448541300001));
#281211=CARTESIAN_POINT('Ctrl Pts',(-7.80668023000005,15.2,-8.27311636000001));
#281212=CARTESIAN_POINT('Ctrl Pts',(-7.80668023000005,11.6,-8.27311636000001));
#281213=CARTESIAN_POINT('Ctrl Pts',(-7.80329164300006,15.2,-8.27174640500001));
#281214=CARTESIAN_POINT('Ctrl Pts',(-7.80329164300006,11.6,-8.27174640500001));
#281215=CARTESIAN_POINT('Ctrl Pts',(-7.79990835200006,15.2,-8.27037555700001));
#281216=CARTESIAN_POINT('Ctrl Pts',(-7.79990835200006,11.6,-8.27037555700001));
#281217=CARTESIAN_POINT('Ctrl Pts',(-7.79653036100005,15.2,-8.26900382300002));
#281218=CARTESIAN_POINT('Ctrl Pts',(-7.79653036100005,11.6,-8.26900382300002));
#281219=CARTESIAN_POINT('Ctrl Pts',(-7.79315767400006,15.2,-8.26763121300001));
#281220=CARTESIAN_POINT('Ctrl Pts',(-7.79315767400006,11.6,-8.26763121300001));
#281221=CARTESIAN_POINT('Ctrl Pts',(-7.78979029600006,15.2,-8.26625773300002));
#281222=CARTESIAN_POINT('Ctrl Pts',(-7.78979029600006,11.6,-8.26625773300002));
#281223=CARTESIAN_POINT('Ctrl Pts',(-7.78642823100006,15.2,-8.26488339200001));
#281224=CARTESIAN_POINT('Ctrl Pts',(-7.78642823100006,11.6,-8.26488339200001));
#281225=CARTESIAN_POINT('Ctrl Pts',(-7.78307148500006,15.2,-8.26350819900001));
#281226=CARTESIAN_POINT('Ctrl Pts',(-7.78307148500006,11.6,-8.26350819900001));
#281227=CARTESIAN_POINT('Ctrl Pts',(-7.77972006200006,15.2,-8.26213216200001));
#281228=CARTESIAN_POINT('Ctrl Pts',(-7.77972006200006,11.6,-8.26213216200001));
#281229=CARTESIAN_POINT('Ctrl Pts',(-7.77637396600006,15.2,-8.26075528800001));
#281230=CARTESIAN_POINT('Ctrl Pts',(-7.77637396600006,11.6,-8.26075528800001));
#281231=CARTESIAN_POINT('Ctrl Pts',(-7.77303320300006,15.2,-8.25937758700002));
#281232=CARTESIAN_POINT('Ctrl Pts',(-7.77303320300006,11.6,-8.25937758700002));
#281233=CARTESIAN_POINT('Ctrl Pts',(-7.76969777700005,15.2,-8.25799906700002));
#281234=CARTESIAN_POINT('Ctrl Pts',(-7.76969777700005,11.6,-8.25799906700002));
#281235=CARTESIAN_POINT('Ctrl Pts',(-7.76636769300006,15.2,-8.25661973600001));
#281236=CARTESIAN_POINT('Ctrl Pts',(-7.76636769300006,11.6,-8.25661973600001));
#281237=CARTESIAN_POINT('Ctrl Pts',(-7.76304295400006,15.2,-8.25523960300002));
#281238=CARTESIAN_POINT('Ctrl Pts',(-7.76304295400006,11.6,-8.25523960300002));
#281239=CARTESIAN_POINT('Ctrl Pts',(-7.75972356700006,15.2,-8.25385867500002));
#281240=CARTESIAN_POINT('Ctrl Pts',(-7.75972356700006,11.6,-8.25385867500002));
#281241=CARTESIAN_POINT('Ctrl Pts',(-7.75640953500006,15.2,-8.25247696200002));
#281242=CARTESIAN_POINT('Ctrl Pts',(-7.75640953500006,11.6,-8.25247696200002));
#281243=CARTESIAN_POINT('Ctrl Pts',(-7.75310086300006,15.2,-8.25109447100001));
#281244=CARTESIAN_POINT('Ctrl Pts',(-7.75310086300006,11.6,-8.25109447100001));
#281245=CARTESIAN_POINT('Ctrl Pts',(-7.74979755700006,15.2,-8.24971121200001));
#281246=CARTESIAN_POINT('Ctrl Pts',(-7.74979755700006,11.6,-8.24971121200001));
#281247=CARTESIAN_POINT('Ctrl Pts',(-7.74649962000005,15.2,-8.24832719300002));
#281248=CARTESIAN_POINT('Ctrl Pts',(-7.74649962000005,11.6,-8.24832719300002));
#281249=CARTESIAN_POINT('Ctrl Pts',(-7.74320705800006,15.2,-8.24694242100002));
#281250=CARTESIAN_POINT('Ctrl Pts',(-7.74320705800006,11.6,-8.24694242100002));
#281251=CARTESIAN_POINT('Ctrl Pts',(-7.73991987400005,15.2,-8.24555690600001));
#281252=CARTESIAN_POINT('Ctrl Pts',(-7.73991987400005,11.6,-8.24555690600001));
#281253=CARTESIAN_POINT('Ctrl Pts',(-7.73663807400006,15.2,-8.24417065600001));
#281254=CARTESIAN_POINT('Ctrl Pts',(-7.73663807400006,11.6,-8.24417065600001));
#281255=CARTESIAN_POINT('Ctrl Pts',(-7.73336166200006,15.2,-8.24278368100002));
#281256=CARTESIAN_POINT('Ctrl Pts',(-7.73336166200006,11.6,-8.24278368100002));
#281257=CARTESIAN_POINT('Ctrl Pts',(-7.73009064300006,15.2,-8.24139598700001));
#281258=CARTESIAN_POINT('Ctrl Pts',(-7.73009064300006,11.6,-8.24139598700001));
#281259=CARTESIAN_POINT('Ctrl Pts',(-7.72682502200006,15.2,-8.24000758400001));
#281260=CARTESIAN_POINT('Ctrl Pts',(-7.72682502200006,11.6,-8.24000758400001));
#281261=CARTESIAN_POINT('Ctrl Pts',(-7.72356480300005,15.2,-8.23861848000002));
#281262=CARTESIAN_POINT('Ctrl Pts',(-7.72356480300005,11.6,-8.23861848000002));
#281263=CARTESIAN_POINT('Ctrl Pts',(-7.72030999100006,15.2,-8.23722868500001));
#281264=CARTESIAN_POINT('Ctrl Pts',(-7.72030999100006,11.6,-8.23722868500001));
#281265=CARTESIAN_POINT('Ctrl Pts',(-7.71706059200006,15.2,-8.23583820700001));
#281266=CARTESIAN_POINT('Ctrl Pts',(-7.71706059200006,11.6,-8.23583820700001));
#281267=CARTESIAN_POINT('Ctrl Pts',(-7.71381660800006,15.2,-8.23444705300002));
#281268=CARTESIAN_POINT('Ctrl Pts',(-7.71381660800006,11.6,-8.23444705300002));
#281269=CARTESIAN_POINT('Ctrl Pts',(-7.71057804500006,15.2,-8.23305523500002));
#281270=CARTESIAN_POINT('Ctrl Pts',(-7.71057804500006,11.6,-8.23305523500002));
#281271=CARTESIAN_POINT('Ctrl Pts',(-7.70734490800006,15.2,-8.23166275800002));
#281272=CARTESIAN_POINT('Ctrl Pts',(-7.70734490800006,11.6,-8.23166275800002));
#281273=CARTESIAN_POINT('Ctrl Pts',(-7.70411720100006,15.2,-8.23026963400002));
#281274=CARTESIAN_POINT('Ctrl Pts',(-7.70411720100006,11.6,-8.23026963400002));
#281275=CARTESIAN_POINT('Ctrl Pts',(-7.70089493000006,15.2,-8.22887586900002));
#281276=CARTESIAN_POINT('Ctrl Pts',(-7.70089493000006,11.6,-8.22887586900002));
#281277=CARTESIAN_POINT('Ctrl Pts',(-7.69767809900006,15.2,-8.22748147300001));
#281278=CARTESIAN_POINT('Ctrl Pts',(-7.69767809900006,11.6,-8.22748147300001));
#281279=CARTESIAN_POINT('Ctrl Pts',(-7.69446671100006,15.2,-8.22608645500001));
#281280=CARTESIAN_POINT('Ctrl Pts',(-7.69446671100006,11.6,-8.22608645500001));
#281281=CARTESIAN_POINT('Ctrl Pts',(-7.69126077400006,15.2,-8.22469082400002));
#281282=CARTESIAN_POINT('Ctrl Pts',(-7.69126077400006,11.6,-8.22469082400002));
#281283=CARTESIAN_POINT('Ctrl Pts',(-7.68806028900006,15.2,-8.22329458900001));
#281284=CARTESIAN_POINT('Ctrl Pts',(-7.68806028900006,11.6,-8.22329458900001));
#281285=CARTESIAN_POINT('Ctrl Pts',(-7.68486526500006,15.2,-8.22189775700001));
#281286=CARTESIAN_POINT('Ctrl Pts',(-7.68486526500006,11.6,-8.22189775700001));
#281287=CARTESIAN_POINT('Ctrl Pts',(-7.68167570300006,15.2,-8.22050033900002));
#281288=CARTESIAN_POINT('Ctrl Pts',(-7.68167570300006,11.6,-8.22050033900002));
#281289=CARTESIAN_POINT('Ctrl Pts',(-7.67849160900005,15.2,-8.21910234200002));
#281290=CARTESIAN_POINT('Ctrl Pts',(-7.67849160900005,11.6,-8.21910234200002));
#281291=CARTESIAN_POINT('Ctrl Pts',(-7.67531298800006,15.2,-8.21770377700001));
#281292=CARTESIAN_POINT('Ctrl Pts',(-7.67531298800006,11.6,-8.21770377700001));
#281293=CARTESIAN_POINT('Ctrl Pts',(-7.67213984400006,15.2,-8.21630465100002));
#281294=CARTESIAN_POINT('Ctrl Pts',(-7.67213984400006,11.6,-8.21630465100002));
#281295=CARTESIAN_POINT('Ctrl Pts',(-7.66897218200006,15.2,-8.21490497400001));
#281296=CARTESIAN_POINT('Ctrl Pts',(-7.66897218200006,11.6,-8.21490497400001));
#281297=CARTESIAN_POINT('Ctrl Pts',(-7.66581000700005,15.2,-8.21350475500001));
#281298=CARTESIAN_POINT('Ctrl Pts',(-7.66581000700005,11.6,-8.21350475500001));
#281299=CARTESIAN_POINT('Ctrl Pts',(-7.66265332400006,15.2,-8.21210400200002));
#281300=CARTESIAN_POINT('Ctrl Pts',(-7.66265332400006,11.6,-8.21210400200002));
#281301=CARTESIAN_POINT('Ctrl Pts',(-7.65950213700006,15.2,-8.21070272500002));
#281302=CARTESIAN_POINT('Ctrl Pts',(-7.65950213700006,11.6,-8.21070272500002));
#281303=CARTESIAN_POINT('Ctrl Pts',(-7.65635645000006,15.2,-8.20930093200002));
#281304=CARTESIAN_POINT('Ctrl Pts',(-7.65635645000006,11.6,-8.20930093200002));
#281305=CARTESIAN_POINT('Ctrl Pts',(-7.65321627000005,15.2,-8.20789863500002));
#281306=CARTESIAN_POINT('Ctrl Pts',(-7.65321627000005,11.6,-8.20789863500002));
#281307=CARTESIAN_POINT('Ctrl Pts',(-7.65008160000006,15.2,-8.20649583800002));
#281308=CARTESIAN_POINT('Ctrl Pts',(-7.65008160000006,11.6,-8.20649583800002));
#281309=CARTESIAN_POINT('Ctrl Pts',(-7.64695244500006,15.2,-8.20509255500001));
#281310=CARTESIAN_POINT('Ctrl Pts',(-7.64695244500006,11.6,-8.20509255500001));
#281311=CARTESIAN_POINT('Ctrl Pts',(-7.64382881000006,15.2,-8.20368879300002));
#281312=CARTESIAN_POINT('Ctrl Pts',(-7.64382881000006,11.6,-8.20368879300002));
#281313=CARTESIAN_POINT('Ctrl Pts',(-7.64071069900006,15.2,-8.20228456000001));
#281314=CARTESIAN_POINT('Ctrl Pts',(-7.64071069900006,11.6,-8.20228456000001));
#281315=CARTESIAN_POINT('Ctrl Pts',(-7.63759811700006,15.2,-8.20087986700001));
#281316=CARTESIAN_POINT('Ctrl Pts',(-7.63759811700006,11.6,-8.20087986700001));
#281317=CARTESIAN_POINT('Ctrl Pts',(-7.63449107100006,15.2,-8.19947472200001));
#281318=CARTESIAN_POINT('Ctrl Pts',(-7.63449107100006,11.6,-8.19947472200001));
#281319=CARTESIAN_POINT('Ctrl Pts',(-7.63138956200006,15.2,-8.19806913500001));
#281320=CARTESIAN_POINT('Ctrl Pts',(-7.63138956200006,11.6,-8.19806913500001));
#281321=CARTESIAN_POINT('Ctrl Pts',(-7.62829359600006,15.2,-8.19666311500002));
#281322=CARTESIAN_POINT('Ctrl Pts',(-7.62829359600006,11.6,-8.19666311500002));
#281323=CARTESIAN_POINT('Ctrl Pts',(-7.62520317900006,15.2,-8.19525667200002));
#281324=CARTESIAN_POINT('Ctrl Pts',(-7.62520317900006,11.6,-8.19525667200002));
#281325=CARTESIAN_POINT('Ctrl Pts',(-7.62211831500006,15.2,-8.19384981300002));
#281326=CARTESIAN_POINT('Ctrl Pts',(-7.62211831500006,11.6,-8.19384981300002));
#281327=CARTESIAN_POINT('Ctrl Pts',(-7.61903900800006,15.2,-8.19244254900001));
#281328=CARTESIAN_POINT('Ctrl Pts',(-7.61903900800006,11.6,-8.19244254900001));
#281329=CARTESIAN_POINT('Ctrl Pts',(-7.61596526500006,15.2,-8.19103488900002));
#281330=CARTESIAN_POINT('Ctrl Pts',(-7.61596526500006,11.6,-8.19103488900002));
#281331=CARTESIAN_POINT('Ctrl Pts',(-7.61289708700006,15.2,-8.18962684300002));
#281332=CARTESIAN_POINT('Ctrl Pts',(-7.61289708700006,11.6,-8.18962684300002));
#281333=CARTESIAN_POINT('Ctrl Pts',(-7.60983448200006,15.2,-8.18821841900002));
#281334=CARTESIAN_POINT('Ctrl Pts',(-7.60983448200006,11.6,-8.18821841900002));
#281335=CARTESIAN_POINT('Ctrl Pts',(-7.60677745300006,15.2,-8.18680962700002));
#281336=CARTESIAN_POINT('Ctrl Pts',(-7.60677745300006,11.6,-8.18680962700002));
#281337=CARTESIAN_POINT('Ctrl Pts',(-7.60372600600006,15.2,-8.18540047600001));
#281338=CARTESIAN_POINT('Ctrl Pts',(-7.60372600600006,11.6,-8.18540047600001));
#281339=CARTESIAN_POINT('Ctrl Pts',(-7.60068014400006,15.2,-8.18399097600001));
#281340=CARTESIAN_POINT('Ctrl Pts',(-7.60068014400006,11.6,-8.18399097600001));
#281341=CARTESIAN_POINT('Ctrl Pts',(-7.59763987400006,15.2,-8.18258113800002));
#281342=CARTESIAN_POINT('Ctrl Pts',(-7.59763987400006,11.6,-8.18258113800002));
#281343=CARTESIAN_POINT('Ctrl Pts',(-7.59460519800006,15.2,-8.18117096700002));
#281344=CARTESIAN_POINT('Ctrl Pts',(-7.59460519800006,11.6,-8.18117096700002));
#281345=CARTESIAN_POINT('Ctrl Pts',(-7.59157612400006,15.2,-8.17976047600002));
#281346=CARTESIAN_POINT('Ctrl Pts',(-7.59157612400006,11.6,-8.17976047600002));
#281347=CARTESIAN_POINT('Ctrl Pts',(-7.58855265400006,15.2,-8.17834967500002));
#281348=CARTESIAN_POINT('Ctrl Pts',(-7.58855265400006,11.6,-8.17834967500002));
#281349=CARTESIAN_POINT('Ctrl Pts',(-7.58553479300006,15.2,-8.17693857100002));
#281350=CARTESIAN_POINT('Ctrl Pts',(-7.58553479300006,11.6,-8.17693857100002));
#281351=CARTESIAN_POINT('Ctrl Pts',(-7.58252254900006,15.2,-8.17552717500002));
#281352=CARTESIAN_POINT('Ctrl Pts',(-7.58252254900006,11.6,-8.17552717500002));
#281353=CARTESIAN_POINT('Ctrl Pts',(-7.57951592200006,15.2,-8.17411549700001));
#281354=CARTESIAN_POINT('Ctrl Pts',(-7.57951592200006,11.6,-8.17411549700001));
#281355=CARTESIAN_POINT('Ctrl Pts',(-7.57651492000005,15.2,-8.17270354500002));
#281356=CARTESIAN_POINT('Ctrl Pts',(-7.57651492000005,11.6,-8.17270354500002));
#281357=CARTESIAN_POINT('Ctrl Pts',(-7.57351954700006,15.2,-8.17129132900002));
#281358=CARTESIAN_POINT('Ctrl Pts',(-7.57351954700006,11.6,-8.17129132900002));
#281359=CARTESIAN_POINT('Ctrl Pts',(-7.57052980700006,15.2,-8.16987886100002));
#281360=CARTESIAN_POINT('Ctrl Pts',(-7.57052980700006,11.6,-8.16987886100002));
#281361=CARTESIAN_POINT('Ctrl Pts',(-7.56754570500006,15.2,-8.16846614700001));
#281362=CARTESIAN_POINT('Ctrl Pts',(-7.56754570500006,11.6,-8.16846614700001));
#281363=CARTESIAN_POINT('Ctrl Pts',(-7.56456724700006,15.2,-8.16705320000001));
#281364=CARTESIAN_POINT('Ctrl Pts',(-7.56456724700006,11.6,-8.16705320000001));
#281365=CARTESIAN_POINT('Ctrl Pts',(-7.56159443700006,15.2,-8.16564002700002));
#281366=CARTESIAN_POINT('Ctrl Pts',(-7.56159443700006,11.6,-8.16564002700002));
#281367=CARTESIAN_POINT('Ctrl Pts',(-7.55862727900006,15.2,-8.16422664000001));
#281368=CARTESIAN_POINT('Ctrl Pts',(-7.55862727900006,11.6,-8.16422664000001));
#281369=CARTESIAN_POINT('Ctrl Pts',(-7.55566577800005,15.2,-8.16281304700002));
#281370=CARTESIAN_POINT('Ctrl Pts',(-7.55566577800005,11.6,-8.16281304700002));
#281371=CARTESIAN_POINT('Ctrl Pts',(-7.55270994000006,15.2,-8.16139925900002));
#281372=CARTESIAN_POINT('Ctrl Pts',(-7.55270994000006,11.6,-8.16139925900002));
#281373=CARTESIAN_POINT('Ctrl Pts',(-7.54975976900005,15.2,-8.15998528500002));
#281374=CARTESIAN_POINT('Ctrl Pts',(-7.54975976900005,11.6,-8.15998528500002));
#281375=CARTESIAN_POINT('Ctrl Pts',(-7.54681526900006,15.2,-8.15857113500002));
#281376=CARTESIAN_POINT('Ctrl Pts',(-7.54681526900006,11.6,-8.15857113500002));
#281377=CARTESIAN_POINT('Ctrl Pts',(-7.54387644600006,15.2,-8.15715681800001));
#281378=CARTESIAN_POINT('Ctrl Pts',(-7.54387644600006,11.6,-8.15715681800001));
#281379=CARTESIAN_POINT('Ctrl Pts',(-7.54094330500005,15.2,-8.15574234600002));
#281380=CARTESIAN_POINT('Ctrl Pts',(-7.54094330500005,11.6,-8.15574234600002));
#281381=CARTESIAN_POINT('Ctrl Pts',(-7.53801584800006,15.2,-8.15432772800002));
#281382=CARTESIAN_POINT('Ctrl Pts',(-7.53801584800006,11.6,-8.15432772800002));
#281383=CARTESIAN_POINT('Ctrl Pts',(-7.53509408300006,15.2,-8.15291297300002));
#281384=CARTESIAN_POINT('Ctrl Pts',(-7.53509408300006,11.6,-8.15291297300002));
#281385=CARTESIAN_POINT('Ctrl Pts',(-7.53217801300006,15.2,-8.15149809200001));
#281386=CARTESIAN_POINT('Ctrl Pts',(-7.53217801300006,11.6,-8.15149809200001));
#281387=CARTESIAN_POINT('Ctrl Pts',(-7.52926764400006,15.2,-8.15008309300002));
#281388=CARTESIAN_POINT('Ctrl Pts',(-7.52926764400006,11.6,-8.15008309300002));
#281389=CARTESIAN_POINT('Ctrl Pts',(-7.52636298100006,15.2,-8.14866798900002));
#281390=CARTESIAN_POINT('Ctrl Pts',(-7.52636298100006,11.6,-8.14866798900002));
#281391=CARTESIAN_POINT('Ctrl Pts',(-7.52346402700006,15.2,-8.14725278900001));
#281392=CARTESIAN_POINT('Ctrl Pts',(-7.52346402700006,11.6,-8.14725278900001));
#281393=CARTESIAN_POINT('Ctrl Pts',(-7.52057078800006,15.2,-8.14583750100002));
#281394=CARTESIAN_POINT('Ctrl Pts',(-7.52057078800006,11.6,-8.14583750100002));
#281395=CARTESIAN_POINT('Ctrl Pts',(-7.51768326900006,15.2,-8.14442213800002));
#281396=CARTESIAN_POINT('Ctrl Pts',(-7.51768326900006,11.6,-8.14442213800002));
#281397=CARTESIAN_POINT('Ctrl Pts',(-7.51480147300006,15.2,-8.14300670900002));
#281398=CARTESIAN_POINT('Ctrl Pts',(-7.51480147300006,11.6,-8.14300670900002));
#281399=CARTESIAN_POINT('Ctrl Pts',(-7.51192540700006,15.2,-8.14159122300002));
#281400=CARTESIAN_POINT('Ctrl Pts',(-7.51192540700006,11.6,-8.14159122300002));
#281401=CARTESIAN_POINT('Ctrl Pts',(-7.50905507600006,15.2,-8.14017569100002));
#281402=CARTESIAN_POINT('Ctrl Pts',(-7.50905507600006,11.6,-8.14017569100002));
#281403=CARTESIAN_POINT('Ctrl Pts',(-7.50619048200006,15.2,-8.13876012300002));
#281404=CARTESIAN_POINT('Ctrl Pts',(-7.50619048200006,11.6,-8.13876012300002));
#281405=CARTESIAN_POINT('Ctrl Pts',(-7.50333163300006,15.2,-8.13734453000002));
#281406=CARTESIAN_POINT('Ctrl Pts',(-7.50333163300006,11.6,-8.13734453000002));
#281407=CARTESIAN_POINT('Ctrl Pts',(-7.50047853100006,15.2,-8.13592892200001));
#281408=CARTESIAN_POINT('Ctrl Pts',(-7.50047853100006,11.6,-8.13592892200001));
#281409=CARTESIAN_POINT('Ctrl Pts',(-7.49763118300006,15.2,-8.13451330800002));
#281410=CARTESIAN_POINT('Ctrl Pts',(-7.49763118300006,11.6,-8.13451330800002));
#281411=CARTESIAN_POINT('Ctrl Pts',(-7.49478959200006,15.2,-8.13309769900001));
#281412=CARTESIAN_POINT('Ctrl Pts',(-7.49478959200006,11.6,-8.13309769900001));
#281413=CARTESIAN_POINT('Ctrl Pts',(-7.49195376600006,15.2,-8.13168210600002));
#281414=CARTESIAN_POINT('Ctrl Pts',(-7.49195376600006,11.6,-8.13168210600002));
#281415=CARTESIAN_POINT('Ctrl Pts',(-7.48912370600006,15.2,-8.13026653800001));
#281416=CARTESIAN_POINT('Ctrl Pts',(-7.48912370600006,11.6,-8.13026653800001));
#281417=CARTESIAN_POINT('Ctrl Pts',(-7.48629941800006,15.2,-8.12885100600001));
#281418=CARTESIAN_POINT('Ctrl Pts',(-7.48629941800006,11.6,-8.12885100600001));
#281419=CARTESIAN_POINT('Ctrl Pts',(-7.48348090800006,15.2,-8.12743552100001));
#281420=CARTESIAN_POINT('Ctrl Pts',(-7.48348090800006,11.6,-8.12743552100001));
#281421=CARTESIAN_POINT('Ctrl Pts',(-7.48066818000006,15.2,-8.12602009200001));
#281422=CARTESIAN_POINT('Ctrl Pts',(-7.48066818000006,11.6,-8.12602009200001));
#281423=CARTESIAN_POINT('Ctrl Pts',(-7.47786123900006,15.2,-8.12460473100002));
#281424=CARTESIAN_POINT('Ctrl Pts',(-7.47786123900006,11.6,-8.12460473100002));
#281425=CARTESIAN_POINT('Ctrl Pts',(-7.47506009000006,15.2,-8.12318944700002));
#281426=CARTESIAN_POINT('Ctrl Pts',(-7.47506009000006,11.6,-8.12318944700002));
#281427=CARTESIAN_POINT('Ctrl Pts',(-7.47226473700006,15.2,-8.12177425100002));
#281428=CARTESIAN_POINT('Ctrl Pts',(-7.47226473700006,11.6,-8.12177425100002));
#281429=CARTESIAN_POINT('Ctrl Pts',(-7.46947518600006,15.2,-8.12035915500001));
#281430=CARTESIAN_POINT('Ctrl Pts',(-7.46947518600006,11.6,-8.12035915500001));
#281431=CARTESIAN_POINT('Ctrl Pts',(-7.46669144100006,15.2,-8.11894416700002));
#281432=CARTESIAN_POINT('Ctrl Pts',(-7.46669144100006,11.6,-8.11894416700002));
#281433=CARTESIAN_POINT('Ctrl Pts',(-7.46391350600006,15.2,-8.11752929900001));
#281434=CARTESIAN_POINT('Ctrl Pts',(-7.46391350600006,11.6,-8.11752929900001));
#281435=CARTESIAN_POINT('Ctrl Pts',(-7.46114138800006,15.2,-8.11611456100002));
#281436=CARTESIAN_POINT('Ctrl Pts',(-7.46114138800006,11.6,-8.11611456100002));
#281437=CARTESIAN_POINT('Ctrl Pts',(-7.45837509000006,15.2,-8.11469996500002));
#281438=CARTESIAN_POINT('Ctrl Pts',(-7.45837509000006,11.6,-8.11469996500002));
#281439=CARTESIAN_POINT('Ctrl Pts',(-7.45561461800006,15.2,-8.11328551900001));
#281440=CARTESIAN_POINT('Ctrl Pts',(-7.45561461800006,11.6,-8.11328551900001));
#281441=CARTESIAN_POINT('Ctrl Pts',(-7.45285997600006,15.2,-8.11187123600002));
#281442=CARTESIAN_POINT('Ctrl Pts',(-7.45285997600006,11.6,-8.11187123600002));
#281443=CARTESIAN_POINT('Ctrl Pts',(-7.45011117000006,15.2,-8.11045712500002));
#281444=CARTESIAN_POINT('Ctrl Pts',(-7.45011117000006,11.6,-8.11045712500002));
#281445=CARTESIAN_POINT('Ctrl Pts',(-7.44736820400006,15.2,-8.10904319800001));
#281446=CARTESIAN_POINT('Ctrl Pts',(-7.44736820400006,11.6,-8.10904319800001));
#281447=CARTESIAN_POINT('Ctrl Pts',(-7.44463108200006,15.2,-8.10762946600001));
#281448=CARTESIAN_POINT('Ctrl Pts',(-7.44463108200006,11.6,-8.10762946600001));
#281449=CARTESIAN_POINT('Ctrl Pts',(-7.44189981100006,15.2,-8.10621593800001));
#281450=CARTESIAN_POINT('Ctrl Pts',(-7.44189981100006,11.6,-8.10621593800001));
#281451=CARTESIAN_POINT('Ctrl Pts',(-7.43917439300006,15.2,-8.10480262600001));
#281452=CARTESIAN_POINT('Ctrl Pts',(-7.43917439300006,11.6,-8.10480262600001));
#281453=CARTESIAN_POINT('Ctrl Pts',(-7.43645483600006,15.2,-8.10338954200001));
#281454=CARTESIAN_POINT('Ctrl Pts',(-7.43645483600006,11.6,-8.10338954200001));
#281455=CARTESIAN_POINT('Ctrl Pts',(-7.43374114300006,15.2,-8.10197669500001));
#281456=CARTESIAN_POINT('Ctrl Pts',(-7.43374114300006,11.6,-8.10197669500001));
#281457=CARTESIAN_POINT('Ctrl Pts',(-7.43103332000006,15.2,-8.10056409500002));
#281458=CARTESIAN_POINT('Ctrl Pts',(-7.43103332000006,11.6,-8.10056409500002));
#281459=CARTESIAN_POINT('Ctrl Pts',(-7.42833137000006,15.2,-8.09915175500001));
#281460=CARTESIAN_POINT('Ctrl Pts',(-7.42833137000006,11.6,-8.09915175500001));
#281461=CARTESIAN_POINT('Ctrl Pts',(-7.42563529900006,15.2,-8.09773968600001));
#281462=CARTESIAN_POINT('Ctrl Pts',(-7.42563529900006,11.6,-8.09773968600001));
#281463=CARTESIAN_POINT('Ctrl Pts',(-7.42294511200006,15.2,-8.09632789700002));
#281464=CARTESIAN_POINT('Ctrl Pts',(-7.42294511200006,11.6,-8.09632789700002));
#281465=CARTESIAN_POINT('Ctrl Pts',(-7.42026081300006,15.2,-8.09491640100001));
#281466=CARTESIAN_POINT('Ctrl Pts',(-7.42026081300006,11.6,-8.09491640100001));
#281467=CARTESIAN_POINT('Ctrl Pts',(-7.41758240900006,15.2,-8.09350520800002));
#281468=CARTESIAN_POINT('Ctrl Pts',(-7.41758240900006,11.6,-8.09350520800002));
#281469=CARTESIAN_POINT('Ctrl Pts',(-7.41490990300006,15.2,-8.09209433000002));
#281470=CARTESIAN_POINT('Ctrl Pts',(-7.41490990300006,11.6,-8.09209433000002));
#281471=CARTESIAN_POINT('Ctrl Pts',(-7.41224330000006,15.2,-8.09068377600001));
#281472=CARTESIAN_POINT('Ctrl Pts',(-7.41224330000006,11.6,-8.09068377600001));
#281473=CARTESIAN_POINT('Ctrl Pts',(-7.40958260500006,15.2,-8.08927355900002));
#281474=CARTESIAN_POINT('Ctrl Pts',(-7.40958260500006,11.6,-8.08927355900002));
#281475=CARTESIAN_POINT('Ctrl Pts',(-7.40692782300005,15.2,-8.08786369000002));
#281476=CARTESIAN_POINT('Ctrl Pts',(-7.40692782300005,11.6,-8.08786369000002));
#281477=CARTESIAN_POINT('Ctrl Pts',(-7.40427895900006,15.2,-8.08645417900001));
#281478=CARTESIAN_POINT('Ctrl Pts',(-7.40427895900006,11.6,-8.08645417900001));
#281479=CARTESIAN_POINT('Ctrl Pts',(-7.40163601900006,15.2,-8.08504503800001));
#281480=CARTESIAN_POINT('Ctrl Pts',(-7.40163601900006,11.6,-8.08504503800001));
#281481=CARTESIAN_POINT('Ctrl Pts',(-7.39899900500006,15.2,-8.08363627800002));
#281482=CARTESIAN_POINT('Ctrl Pts',(-7.39899900500006,11.6,-8.08363627800002));
#281483=CARTESIAN_POINT('Ctrl Pts',(-7.39636792500006,15.2,-8.08222791100001));
#281484=CARTESIAN_POINT('Ctrl Pts',(-7.39636792500006,11.6,-8.08222791100001));
#281485=CARTESIAN_POINT('Ctrl Pts',(-7.39374278200006,15.2,-8.08081994600002));
#281486=CARTESIAN_POINT('Ctrl Pts',(-7.39374278200006,11.6,-8.08081994600002));
#281487=CARTESIAN_POINT('Ctrl Pts',(-7.39112358200006,15.2,-8.07941239800002));
#281488=CARTESIAN_POINT('Ctrl Pts',(-7.39112358200006,11.6,-8.07941239800002));
#281489=CARTESIAN_POINT('Ctrl Pts',(-7.38851032900006,15.2,-8.07800527400002));
#281490=CARTESIAN_POINT('Ctrl Pts',(-7.38851032900006,11.6,-8.07800527400002));
#281491=CARTESIAN_POINT('Ctrl Pts',(-7.38590302800006,15.2,-8.07659859000001));
#281492=CARTESIAN_POINT('Ctrl Pts',(-7.38590302800006,11.6,-8.07659859000001));
#281493=CARTESIAN_POINT('Ctrl Pts',(-7.38330168300006,15.2,-8.07519235400001));
#281494=CARTESIAN_POINT('Ctrl Pts',(-7.38330168300006,11.6,-8.07519235400001));
#281495=CARTESIAN_POINT('Ctrl Pts',(-7.38070630100006,15.2,-8.07378657700001));
#281496=CARTESIAN_POINT('Ctrl Pts',(-7.38070630100006,11.6,-8.07378657700001));
#281497=CARTESIAN_POINT('Ctrl Pts',(-7.37811688700006,15.2,-8.07238127400002));
#281498=CARTESIAN_POINT('Ctrl Pts',(-7.37811688700006,11.6,-8.07238127400002));
#281499=CARTESIAN_POINT('Ctrl Pts',(-7.37553344400006,15.2,-8.07097645400002));
#281500=CARTESIAN_POINT('Ctrl Pts',(-7.37553344400006,11.6,-8.07097645400002));
#281501=CARTESIAN_POINT('Ctrl Pts',(-7.37295597700006,15.2,-8.06957212800001));
#281502=CARTESIAN_POINT('Ctrl Pts',(-7.37295597700006,11.6,-8.06957212800001));
#281503=CARTESIAN_POINT('Ctrl Pts',(-7.37038449300006,15.2,-8.06816830900001));
#281504=CARTESIAN_POINT('Ctrl Pts',(-7.37038449300006,11.6,-8.06816830900001));
#281505=CARTESIAN_POINT('Ctrl Pts',(-7.36781899500006,15.2,-8.06676500900002));
#281506=CARTESIAN_POINT('Ctrl Pts',(-7.36781899500006,11.6,-8.06676500900002));
#281507=CARTESIAN_POINT('Ctrl Pts',(-7.36525948900006,15.2,-8.06536223600002));
#281508=CARTESIAN_POINT('Ctrl Pts',(-7.36525948900006,11.6,-8.06536223600002));
#281509=CARTESIAN_POINT('Ctrl Pts',(-7.36270597800006,15.2,-8.06396000700002));
#281510=CARTESIAN_POINT('Ctrl Pts',(-7.36270597800006,11.6,-8.06396000700002));
#281511=CARTESIAN_POINT('Ctrl Pts',(-7.36015847000006,15.2,-8.06255832900002));
#281512=CARTESIAN_POINT('Ctrl Pts',(-7.36015847000006,11.6,-8.06255832900002));
#281513=CARTESIAN_POINT('Ctrl Pts',(-7.35761696800005,15.2,-8.06115721700002));
#281514=CARTESIAN_POINT('Ctrl Pts',(-7.35761696800005,11.6,-8.06115721700002));
#281515=CARTESIAN_POINT('Ctrl Pts',(-7.35508147700005,15.2,-8.05975668000002));
#281516=CARTESIAN_POINT('Ctrl Pts',(-7.35508147700005,11.6,-8.05975668000002));
#281517=CARTESIAN_POINT('Ctrl Pts',(-7.35255200200006,15.2,-8.05835673200002));
#281518=CARTESIAN_POINT('Ctrl Pts',(-7.35255200200006,11.6,-8.05835673200002));
#281519=CARTESIAN_POINT('Ctrl Pts',(-7.35002854900006,15.2,-8.05695738400001));
#281520=CARTESIAN_POINT('Ctrl Pts',(-7.35002854900006,11.6,-8.05695738400001));
#281521=CARTESIAN_POINT('Ctrl Pts',(-7.34751112100006,15.2,-8.05555864700001));
#281522=CARTESIAN_POINT('Ctrl Pts',(-7.34751112100006,11.6,-8.05555864700001));
#281523=CARTESIAN_POINT('Ctrl Pts',(-7.34499972500006,15.2,-8.05416053400002));
#281524=CARTESIAN_POINT('Ctrl Pts',(-7.34499972500006,11.6,-8.05416053400002));
#281525=CARTESIAN_POINT('Ctrl Pts',(-7.34249436400006,15.2,-8.05276305700002));
#281526=CARTESIAN_POINT('Ctrl Pts',(-7.34249436400006,11.6,-8.05276305700002));
#281527=CARTESIAN_POINT('Ctrl Pts',(-7.33999504500006,15.2,-8.05136622600001));
#281528=CARTESIAN_POINT('Ctrl Pts',(-7.33999504500006,11.6,-8.05136622600001));
#281529=CARTESIAN_POINT('Ctrl Pts',(-7.33750177100006,15.2,-8.04997005600002));
#281530=CARTESIAN_POINT('Ctrl Pts',(-7.33750177100006,11.6,-8.04997005600002));
#281531=CARTESIAN_POINT('Ctrl Pts',(-7.33501454800006,15.2,-8.04857455600001));
#281532=CARTESIAN_POINT('Ctrl Pts',(-7.33501454800006,11.6,-8.04857455600001));
#281533=CARTESIAN_POINT('Ctrl Pts',(-7.33253338100006,15.2,-8.04717974000001));
#281534=CARTESIAN_POINT('Ctrl Pts',(-7.33253338100006,11.6,-8.04717974000001));
#281535=CARTESIAN_POINT('Ctrl Pts',(-7.33005827500006,15.2,-8.04578561900002));
#281536=CARTESIAN_POINT('Ctrl Pts',(-7.33005827500006,11.6,-8.04578561900002));
#281537=CARTESIAN_POINT('Ctrl Pts',(-7.32758923400006,15.2,-8.04439220600001));
#281538=CARTESIAN_POINT('Ctrl Pts',(-7.32758923400006,11.6,-8.04439220600001));
#281539=CARTESIAN_POINT('Ctrl Pts',(-7.32512626500006,15.2,-8.04299951200001));
#281540=CARTESIAN_POINT('Ctrl Pts',(-7.32512626500006,11.6,-8.04299951200001));
#281541=CARTESIAN_POINT('Ctrl Pts',(-7.32266937000006,15.2,-8.04160755000002));
#281542=CARTESIAN_POINT('Ctrl Pts',(-7.32266937000006,11.6,-8.04160755000002));
#281543=CARTESIAN_POINT('Ctrl Pts',(-7.32021855600006,15.2,-8.04021633200002));
#281544=CARTESIAN_POINT('Ctrl Pts',(-7.32021855600006,11.6,-8.04021633200002));
#281545=CARTESIAN_POINT('Ctrl Pts',(-7.31777382800006,15.2,-8.03882587000002));
#281546=CARTESIAN_POINT('Ctrl Pts',(-7.31777382800006,11.6,-8.03882587000002));
#281547=CARTESIAN_POINT('Ctrl Pts',(-7.31533519000005,15.2,-8.03743617600002));
#281548=CARTESIAN_POINT('Ctrl Pts',(-7.31533519000005,11.6,-8.03743617600002));
#281549=CARTESIAN_POINT('Ctrl Pts',(-7.31290264900006,15.2,-8.03604726400001));
#281550=CARTESIAN_POINT('Ctrl Pts',(-7.31290264900006,11.6,-8.03604726400001));
#281551=CARTESIAN_POINT('Ctrl Pts',(-7.31047620800005,15.2,-8.03465914400002));
#281552=CARTESIAN_POINT('Ctrl Pts',(-7.31047620800005,11.6,-8.03465914400002));
#281553=CARTESIAN_POINT('Ctrl Pts',(-7.30805587300006,15.2,-8.03327182900002));
#281554=CARTESIAN_POINT('Ctrl Pts',(-7.30805587300006,11.6,-8.03327182900002));
#281555=CARTESIAN_POINT('Ctrl Pts',(-7.30564164700006,15.2,-8.03188533200002));
#281556=CARTESIAN_POINT('Ctrl Pts',(-7.30564164700006,11.6,-8.03188533200002));
#281557=CARTESIAN_POINT('Ctrl Pts',(-7.30323353700006,15.2,-8.03049966500001));
#281558=CARTESIAN_POINT('Ctrl Pts',(-7.30323353700006,11.6,-8.03049966500001));
#281559=CARTESIAN_POINT('Ctrl Pts',(-7.30083154800006,15.2,-8.02911484100001));
#281560=CARTESIAN_POINT('Ctrl Pts',(-7.30083154800006,11.6,-8.02911484100001));
#281561=CARTESIAN_POINT('Ctrl Pts',(-7.29843568500006,15.2,-8.02773087300002));
#281562=CARTESIAN_POINT('Ctrl Pts',(-7.29843568500006,11.6,-8.02773087300002));
#281563=CARTESIAN_POINT('Ctrl Pts',(-7.29604595200006,15.2,-8.02634777100002));
#281564=CARTESIAN_POINT('Ctrl Pts',(-7.29604595200006,11.6,-8.02634777100002));
#281565=CARTESIAN_POINT('Ctrl Pts',(-7.29366235400006,15.2,-8.02496555000002));
#281566=CARTESIAN_POINT('Ctrl Pts',(-7.29366235400006,11.6,-8.02496555000002));
#281567=CARTESIAN_POINT('Ctrl Pts',(-7.29128489700006,15.2,-8.02358422100001));
#281568=CARTESIAN_POINT('Ctrl Pts',(-7.29128489700006,11.6,-8.02358422100001));
#281569=CARTESIAN_POINT('Ctrl Pts',(-7.28891358600006,15.2,-8.02220379800002));
#281570=CARTESIAN_POINT('Ctrl Pts',(-7.28891358600006,11.6,-8.02220379800002));
#281571=CARTESIAN_POINT('Ctrl Pts',(-7.28654842500006,15.2,-8.02082429200001));
#281572=CARTESIAN_POINT('Ctrl Pts',(-7.28654842500006,11.6,-8.02082429200001));
#281573=CARTESIAN_POINT('Ctrl Pts',(-7.28418942000006,15.2,-8.01944571800002));
#281574=CARTESIAN_POINT('Ctrl Pts',(-7.28418942000006,11.6,-8.01944571800002));
#281575=CARTESIAN_POINT('Ctrl Pts',(-7.28183657600006,15.2,-8.01806808600002));
#281576=CARTESIAN_POINT('Ctrl Pts',(-7.28183657600006,11.6,-8.01806808600002));
#281577=CARTESIAN_POINT('Ctrl Pts',(-7.27948989700006,15.2,-8.01669141200002));
#281578=CARTESIAN_POINT('Ctrl Pts',(-7.27948989700006,11.6,-8.01669141200002));
#281579=CARTESIAN_POINT('Ctrl Pts',(-7.27714938800006,15.2,-8.01531570600002));
#281580=CARTESIAN_POINT('Ctrl Pts',(-7.27714938800006,11.6,-8.01531570600002));
#281581=CARTESIAN_POINT('Ctrl Pts',(-7.27481505600006,15.2,-8.01394098200002));
#281582=CARTESIAN_POINT('Ctrl Pts',(-7.27481505600006,11.6,-8.01394098200002));
#281583=CARTESIAN_POINT('Ctrl Pts',(-7.27248690400006,15.2,-8.01256725300002));
#281584=CARTESIAN_POINT('Ctrl Pts',(-7.27248690400006,11.6,-8.01256725300002));
#281585=CARTESIAN_POINT('Ctrl Pts',(-7.27016493900006,15.2,-8.01119453200002));
#281586=CARTESIAN_POINT('Ctrl Pts',(-7.27016493900006,11.6,-8.01119453200002));
#281587=CARTESIAN_POINT('Ctrl Pts',(-7.26784916400006,15.2,-8.00982283100002));
#281588=CARTESIAN_POINT('Ctrl Pts',(-7.26784916400006,11.6,-8.00982283100002));
#281589=CARTESIAN_POINT('Ctrl Pts',(-7.26553958500006,15.2,-8.00845216300001));
#281590=CARTESIAN_POINT('Ctrl Pts',(-7.26553958500006,11.6,-8.00845216300001));
#281591=CARTESIAN_POINT('Ctrl Pts',(-7.26323620700006,15.2,-8.00708254200002));
#281592=CARTESIAN_POINT('Ctrl Pts',(-7.26323620700006,11.6,-8.00708254200002));
#281593=CARTESIAN_POINT('Ctrl Pts',(-7.26093903400006,15.2,-8.00571398200002));
#281594=CARTESIAN_POINT('Ctrl Pts',(-7.26093903400006,11.6,-8.00571398200002));
#281595=CARTESIAN_POINT('Ctrl Pts',(-7.25864807300006,15.2,-8.00434649300002));
#281596=CARTESIAN_POINT('Ctrl Pts',(-7.25864807300006,11.6,-8.00434649300002));
#281597=CARTESIAN_POINT('Ctrl Pts',(-7.25636332800006,15.2,-8.00298009100001));
#281598=CARTESIAN_POINT('Ctrl Pts',(-7.25636332800006,11.6,-8.00298009100001));
#281599=CARTESIAN_POINT('Ctrl Pts',(-7.25408480500006,15.2,-8.00161478700002));
#281600=CARTESIAN_POINT('Ctrl Pts',(-7.25408480500006,11.6,-8.00161478700002));
#281601=CARTESIAN_POINT('Ctrl Pts',(-7.25181250700006,15.2,-8.00025059700002));
#281602=CARTESIAN_POINT('Ctrl Pts',(-7.25181250700006,11.6,-8.00025059700002));
#281603=CARTESIAN_POINT('Ctrl Pts',(-7.24954644200006,15.2,-7.99888753100002));
#281604=CARTESIAN_POINT('Ctrl Pts',(-7.24954644200006,11.6,-7.99888753100002));
#281605=CARTESIAN_POINT('Ctrl Pts',(-7.24728661100006,15.2,-7.99752560500002));
#281606=CARTESIAN_POINT('Ctrl Pts',(-7.24728661100006,11.6,-7.99752560500002));
#281607=CARTESIAN_POINT('Ctrl Pts',(-7.24503302300006,15.2,-7.99616483000002));
#281608=CARTESIAN_POINT('Ctrl Pts',(-7.24503302300006,11.6,-7.99616483000002));
#281609=CARTESIAN_POINT('Ctrl Pts',(-7.24278568100006,15.2,-7.99480522100002));
#281610=CARTESIAN_POINT('Ctrl Pts',(-7.24278568100006,11.6,-7.99480522100002));
#281611=CARTESIAN_POINT('Ctrl Pts',(-7.24054459100006,15.2,-7.99344679100002));
#281612=CARTESIAN_POINT('Ctrl Pts',(-7.24054459100006,11.6,-7.99344679100002));
#281613=CARTESIAN_POINT('Ctrl Pts',(-7.23830975800006,15.2,-7.99208955400001));
#281614=CARTESIAN_POINT('Ctrl Pts',(-7.23830975800006,11.6,-7.99208955400001));
#281615=CARTESIAN_POINT('Ctrl Pts',(-7.23608118600006,15.2,-7.99073352300002));
#281616=CARTESIAN_POINT('Ctrl Pts',(-7.23608118600006,11.6,-7.99073352300002));
#281617=CARTESIAN_POINT('Ctrl Pts',(-7.23385888100006,15.2,-7.98937871000001));
#281618=CARTESIAN_POINT('Ctrl Pts',(-7.23385888100006,11.6,-7.98937871000001));
#281619=CARTESIAN_POINT('Ctrl Pts',(-7.23164285000006,15.2,-7.98802513000001));
#281620=CARTESIAN_POINT('Ctrl Pts',(-7.23164285000006,11.6,-7.98802513000001));
#281621=CARTESIAN_POINT('Ctrl Pts',(-7.22943309400006,15.2,-7.98667279800001));
#281622=CARTESIAN_POINT('Ctrl Pts',(-7.22943309400006,11.6,-7.98667279800001));
#281623=CARTESIAN_POINT('Ctrl Pts',(-7.22722962100006,15.2,-7.98532172500002));
#281624=CARTESIAN_POINT('Ctrl Pts',(-7.22722962100006,11.6,-7.98532172500002));
#281625=CARTESIAN_POINT('Ctrl Pts',(-7.22503243500006,15.2,-7.98397192600002));
#281626=CARTESIAN_POINT('Ctrl Pts',(-7.22503243500006,11.6,-7.98397192600002));
#281627=CARTESIAN_POINT('Ctrl Pts',(-7.22284154100006,15.2,-7.98262341500001));
#281628=CARTESIAN_POINT('Ctrl Pts',(-7.22284154100006,11.6,-7.98262341500001));
#281629=CARTESIAN_POINT('Ctrl Pts',(-7.22065694500006,15.2,-7.98127620500001));
#281630=CARTESIAN_POINT('Ctrl Pts',(-7.22065694500006,11.6,-7.98127620500001));
#281631=CARTESIAN_POINT('Ctrl Pts',(-7.21847865200006,15.2,-7.97993031000002));
#281632=CARTESIAN_POINT('Ctrl Pts',(-7.21847865200006,11.6,-7.97993031000002));
#281633=CARTESIAN_POINT('Ctrl Pts',(-7.21630666700006,15.2,-7.97858574400002));
#281634=CARTESIAN_POINT('Ctrl Pts',(-7.21630666700006,11.6,-7.97858574400002));
#281635=CARTESIAN_POINT('Ctrl Pts',(-7.21414099500006,15.2,-7.97724252200001));
#281636=CARTESIAN_POINT('Ctrl Pts',(-7.21414099500006,11.6,-7.97724252200001));
#281637=CARTESIAN_POINT('Ctrl Pts',(-7.21198164100006,15.2,-7.97590065400002));
#281638=CARTESIAN_POINT('Ctrl Pts',(-7.21198164100006,11.6,-7.97590065400002));
#281639=CARTESIAN_POINT('Ctrl Pts',(-7.20982861000006,15.2,-7.97456016000002));
#281640=CARTESIAN_POINT('Ctrl Pts',(-7.20982861000006,11.6,-7.97456016000002));
#281641=CARTESIAN_POINT('Ctrl Pts',(-7.20768190700006,15.2,-7.97322104900001));
#281642=CARTESIAN_POINT('Ctrl Pts',(-7.20768190700006,11.6,-7.97322104900001));
#281643=CARTESIAN_POINT('Ctrl Pts',(-7.20554153900006,15.2,-7.97188333700002));
#281644=CARTESIAN_POINT('Ctrl Pts',(-7.20554153900006,11.6,-7.97188333700002));
#281645=CARTESIAN_POINT('Ctrl Pts',(-7.20340750800006,15.2,-7.97054703800002));
#281646=CARTESIAN_POINT('Ctrl Pts',(-7.20340750800006,11.6,-7.97054703800002));
#281647=CARTESIAN_POINT('Ctrl Pts',(-7.20127982200006,15.2,-7.96921216600002));
#281648=CARTESIAN_POINT('Ctrl Pts',(-7.20127982200006,11.6,-7.96921216600002));
#281649=CARTESIAN_POINT('Ctrl Pts',(-7.19915848500006,15.2,-7.96787873500002));
#281650=CARTESIAN_POINT('Ctrl Pts',(-7.19915848500006,11.6,-7.96787873500002));
#281651=CARTESIAN_POINT('Ctrl Pts',(-7.19704350100006,15.2,-7.96654675900001));
#281652=CARTESIAN_POINT('Ctrl Pts',(-7.19704350100006,11.6,-7.96654675900001));
#281653=CARTESIAN_POINT('Ctrl Pts',(-7.19493487700006,15.2,-7.96521625400001));
#281654=CARTESIAN_POINT('Ctrl Pts',(-7.19493487700006,11.6,-7.96521625400001));
#281655=CARTESIAN_POINT('Ctrl Pts',(-7.19283261800006,15.2,-7.96388723200002));
#281656=CARTESIAN_POINT('Ctrl Pts',(-7.19283261800006,11.6,-7.96388723200002));
#281657=CARTESIAN_POINT('Ctrl Pts',(-7.19073672800006,15.2,-7.96255970800001));
#281658=CARTESIAN_POINT('Ctrl Pts',(-7.19073672800006,11.6,-7.96255970800001));
#281659=CARTESIAN_POINT('Ctrl Pts',(-7.18864721300006,15.2,-7.96123369700001));
#281660=CARTESIAN_POINT('Ctrl Pts',(-7.18864721300006,11.6,-7.96123369700001));
#281661=CARTESIAN_POINT('Ctrl Pts',(-7.18656407900006,15.2,-7.95990921400002));
#281662=CARTESIAN_POINT('Ctrl Pts',(-7.18656407900006,11.6,-7.95990921400002));
#281663=CARTESIAN_POINT('Ctrl Pts',(-7.18448732900006,15.2,-7.95858627200002));
#281664=CARTESIAN_POINT('Ctrl Pts',(-7.18448732900006,11.6,-7.95858627200002));
#281665=CARTESIAN_POINT('Ctrl Pts',(-7.18241697000006,15.2,-7.95726488600002));
#281666=CARTESIAN_POINT('Ctrl Pts',(-7.18241697000006,11.6,-7.95726488600002));
#281667=CARTESIAN_POINT('Ctrl Pts',(-7.18035300600006,15.2,-7.95594507100001));
#281668=CARTESIAN_POINT('Ctrl Pts',(-7.18035300600006,11.6,-7.95594507100001));
#281669=CARTESIAN_POINT('Ctrl Pts',(-7.17829544400006,15.2,-7.95462684200002));
#281670=CARTESIAN_POINT('Ctrl Pts',(-7.17829544400006,11.6,-7.95462684200002));
#281671=CARTESIAN_POINT('Ctrl Pts',(-7.17624428700006,15.2,-7.95331021100001));
#281672=CARTESIAN_POINT('Ctrl Pts',(-7.17624428700006,11.6,-7.95331021100001));
#281673=CARTESIAN_POINT('Ctrl Pts',(-7.17419954100006,15.2,-7.95199519700001));
#281674=CARTESIAN_POINT('Ctrl Pts',(-7.17419954100006,11.6,-7.95199519700001));
#281675=CARTESIAN_POINT('Ctrl Pts',(-7.17216121300006,15.2,-7.95068181000002));
#281676=CARTESIAN_POINT('Ctrl Pts',(-7.17216121300006,11.6,-7.95068181000002));
#281677=CARTESIAN_POINT('Ctrl Pts',(-7.17012930600006,15.2,-7.94937007000001));
#281678=CARTESIAN_POINT('Ctrl Pts',(-7.17012930600006,11.6,-7.94937007000001));
#281679=CARTESIAN_POINT('Ctrl Pts',(-7.16810382600006,15.2,-7.94805998700002));
#281680=CARTESIAN_POINT('Ctrl Pts',(-7.16810382600006,11.6,-7.94805998700002));
#281681=CARTESIAN_POINT('Ctrl Pts',(-7.16608477700006,15.2,-7.94675157900001));
#281682=CARTESIAN_POINT('Ctrl Pts',(-7.16608477700006,11.6,-7.94675157900001));
#281683=CARTESIAN_POINT('Ctrl Pts',(-7.16407216700006,15.2,-7.94544485900002));
#281684=CARTESIAN_POINT('Ctrl Pts',(-7.16407216700006,11.6,-7.94544485900002));
#281685=CARTESIAN_POINT('Ctrl Pts',(-7.16206599800006,15.2,-7.94413984400002));
#281686=CARTESIAN_POINT('Ctrl Pts',(-7.16206599800006,11.6,-7.94413984400002));
#281687=CARTESIAN_POINT('Ctrl Pts',(-7.16006627800006,15.2,-7.94283654700001));
#281688=CARTESIAN_POINT('Ctrl Pts',(-7.16006627800006,11.6,-7.94283654700001));
#281689=CARTESIAN_POINT('Ctrl Pts',(-7.15807301100006,15.2,-7.94153498400001));
#281690=CARTESIAN_POINT('Ctrl Pts',(-7.15807301100006,11.6,-7.94153498400001));
#281691=CARTESIAN_POINT('Ctrl Pts',(-7.15608620200006,15.2,-7.94023517100002));
#281692=CARTESIAN_POINT('Ctrl Pts',(-7.15608620200006,11.6,-7.94023517100002));
#281693=CARTESIAN_POINT('Ctrl Pts',(-7.15410585700006,15.2,-7.93893712100001));
#281694=CARTESIAN_POINT('Ctrl Pts',(-7.15410585700006,11.6,-7.93893712100001));
#281695=CARTESIAN_POINT('Ctrl Pts',(-7.15213198100006,15.2,-7.93764085100002));
#281696=CARTESIAN_POINT('Ctrl Pts',(-7.15213198100006,11.6,-7.93764085100002));
#281697=CARTESIAN_POINT('Ctrl Pts',(-7.15016457900005,15.2,-7.93634637500002));
#281698=CARTESIAN_POINT('Ctrl Pts',(-7.15016457900005,11.6,-7.93634637500002));
#281699=CARTESIAN_POINT('Ctrl Pts',(-7.14820365700006,15.2,-7.93505371000002));
#281700=CARTESIAN_POINT('Ctrl Pts',(-7.14820365700006,11.6,-7.93505371000002));
#281701=CARTESIAN_POINT('Ctrl Pts',(-7.14624921900006,15.2,-7.93376287100001));
#281702=CARTESIAN_POINT('Ctrl Pts',(-7.14624921900006,11.6,-7.93376287100001));
#281703=CARTESIAN_POINT('Ctrl Pts',(-7.14430127000006,15.2,-7.93247387100001));
#281704=CARTESIAN_POINT('Ctrl Pts',(-7.14430127000006,11.6,-7.93247387100001));
#281705=CARTESIAN_POINT('Ctrl Pts',(-7.14235981800006,15.2,-7.93118672800002));
#281706=CARTESIAN_POINT('Ctrl Pts',(-7.14235981800006,11.6,-7.93118672800002));
#281707=CARTESIAN_POINT('Ctrl Pts',(-7.14042486500006,15.2,-7.92990145700001));
#281708=CARTESIAN_POINT('Ctrl Pts',(-7.14042486500006,11.6,-7.92990145700001));
#281709=CARTESIAN_POINT('Ctrl Pts',(-7.13849641900006,15.2,-7.92861807300002));
#281710=CARTESIAN_POINT('Ctrl Pts',(-7.13849641900006,11.6,-7.92861807300002));
#281711=CARTESIAN_POINT('Ctrl Pts',(-7.13657448400006,15.2,-7.92733659100002));
#281712=CARTESIAN_POINT('Ctrl Pts',(-7.13657448400006,11.6,-7.92733659100002));
#281713=CARTESIAN_POINT('Ctrl Pts',(-7.13465906500006,15.2,-7.92605702900002));
#281714=CARTESIAN_POINT('Ctrl Pts',(-7.13465906500006,11.6,-7.92605702900002));
#281715=CARTESIAN_POINT('Ctrl Pts',(-7.13275016800006,15.2,-7.92477940100002));
#281716=CARTESIAN_POINT('Ctrl Pts',(-7.13275016800006,11.6,-7.92477940100002));
#281717=CARTESIAN_POINT('Ctrl Pts',(-7.13084779900006,15.2,-7.92350372200002));
#281718=CARTESIAN_POINT('Ctrl Pts',(-7.13084779900006,11.6,-7.92350372200002));
#281719=CARTESIAN_POINT('Ctrl Pts',(-7.12895196100006,15.2,-7.92223001000002));
#281720=CARTESIAN_POINT('Ctrl Pts',(-7.12895196100006,11.6,-7.92223001000002));
#281721=CARTESIAN_POINT('Ctrl Pts',(-7.12706266200006,15.2,-7.92095827900001));
#281722=CARTESIAN_POINT('Ctrl Pts',(-7.12706266200006,11.6,-7.92095827900001));
#281723=CARTESIAN_POINT('Ctrl Pts',(-7.12517990500006,15.2,-7.91968854600002));
#281724=CARTESIAN_POINT('Ctrl Pts',(-7.12517990500006,11.6,-7.91968854600002));
#281725=CARTESIAN_POINT('Ctrl Pts',(-7.12330369600005,15.2,-7.91842082600001));
#281726=CARTESIAN_POINT('Ctrl Pts',(-7.12330369600005,11.6,-7.91842082600001));
#281727=CARTESIAN_POINT('Ctrl Pts',(-7.12143404200006,15.2,-7.91715513600002));
#281728=CARTESIAN_POINT('Ctrl Pts',(-7.12143404200006,11.6,-7.91715513600002));
#281729=CARTESIAN_POINT('Ctrl Pts',(-7.11957094800006,15.2,-7.91589149100002));
#281730=CARTESIAN_POINT('Ctrl Pts',(-7.11957094800006,11.6,-7.91589149100002));
#281731=CARTESIAN_POINT('Ctrl Pts',(-7.11771441600006,15.2,-7.91462990800002));
#281732=CARTESIAN_POINT('Ctrl Pts',(-7.11771441600006,11.6,-7.91462990800002));
#281733=CARTESIAN_POINT('Ctrl Pts',(-7.11586445500005,15.2,-7.91337040400002));
#281734=CARTESIAN_POINT('Ctrl Pts',(-7.11586445500005,11.6,-7.91337040400002));
#281735=CARTESIAN_POINT('Ctrl Pts',(-7.11402107000006,15.2,-7.91211299300001));
#281736=CARTESIAN_POINT('Ctrl Pts',(-7.11402107000006,11.6,-7.91211299300001));
#281737=CARTESIAN_POINT('Ctrl Pts',(-7.11218426500006,15.2,-7.91085769300001));
#281738=CARTESIAN_POINT('Ctrl Pts',(-7.11218426500006,11.6,-7.91085769300001));
#281739=CARTESIAN_POINT('Ctrl Pts',(-7.11035404400006,15.2,-7.90960451900002));
#281740=CARTESIAN_POINT('Ctrl Pts',(-7.11035404400006,11.6,-7.90960451900002));
#281741=CARTESIAN_POINT('Ctrl Pts',(-7.10853041700005,15.2,-7.90835348800002));
#281742=CARTESIAN_POINT('Ctrl Pts',(-7.10853041700005,11.6,-7.90835348800002));
#281743=CARTESIAN_POINT('Ctrl Pts',(-7.10671338600006,15.2,-7.90710461700002));
#281744=CARTESIAN_POINT('Ctrl Pts',(-7.10671338600006,11.6,-7.90710461700002));
#281745=CARTESIAN_POINT('Ctrl Pts',(-7.10490295600006,15.2,-7.90585792200002));
#281746=CARTESIAN_POINT('Ctrl Pts',(-7.10490295600006,11.6,-7.90585792200002));
#281747=CARTESIAN_POINT('Ctrl Pts',(-7.10309913500006,15.2,-7.90461341900001));
#281748=CARTESIAN_POINT('Ctrl Pts',(-7.10309913500006,11.6,-7.90461341900001));
#281749=CARTESIAN_POINT('Ctrl Pts',(-7.10130192600006,15.2,-7.90337112600002));
#281750=CARTESIAN_POINT('Ctrl Pts',(-7.10130192600006,11.6,-7.90337112600002));
#281751=CARTESIAN_POINT('Ctrl Pts',(-7.09951133700006,15.2,-7.90213105800002));
#281752=CARTESIAN_POINT('Ctrl Pts',(-7.09951133700006,11.6,-7.90213105800002));
#281753=CARTESIAN_POINT('Ctrl Pts',(-7.09772736900006,15.2,-7.90089323300001));
#281754=CARTESIAN_POINT('Ctrl Pts',(-7.09772736900006,11.6,-7.90089323300001));
#281755=CARTESIAN_POINT('Ctrl Pts',(-7.09595003200006,15.2,-7.89965766700002));
#281756=CARTESIAN_POINT('Ctrl Pts',(-7.09595003200006,11.6,-7.89965766700002));
#281757=CARTESIAN_POINT('Ctrl Pts',(-7.09417932900006,15.2,-7.89842437800001));
#281758=CARTESIAN_POINT('Ctrl Pts',(-7.09417932900006,11.6,-7.89842437800001));
#281759=CARTESIAN_POINT('Ctrl Pts',(-7.09241526600006,15.2,-7.89719338000002));
#281760=CARTESIAN_POINT('Ctrl Pts',(-7.09241526600006,11.6,-7.89719338000002));
#281761=CARTESIAN_POINT('Ctrl Pts',(-7.09065785000006,15.2,-7.89596469400001));
#281762=CARTESIAN_POINT('Ctrl Pts',(-7.09065785000006,11.6,-7.89596469400001));
#281763=CARTESIAN_POINT('Ctrl Pts',(-7.08890708300006,15.2,-7.89473833400002));
#281764=CARTESIAN_POINT('Ctrl Pts',(-7.08890708300006,11.6,-7.89473833400002));
#281765=CARTESIAN_POINT('Ctrl Pts',(-7.08716297200006,15.2,-7.89351431800001));
#281766=CARTESIAN_POINT('Ctrl Pts',(-7.08716297200006,11.6,-7.89351431800001));
#281767=CARTESIAN_POINT('Ctrl Pts',(-7.08542552400006,15.2,-7.89229266300002));
#281768=CARTESIAN_POINT('Ctrl Pts',(-7.08542552400006,11.6,-7.89229266300002));
#281769=CARTESIAN_POINT('Ctrl Pts',(-7.08369474300006,15.2,-7.89107338700001));
#281770=CARTESIAN_POINT('Ctrl Pts',(-7.08369474300006,11.6,-7.89107338700001));
#281771=CARTESIAN_POINT('Ctrl Pts',(-7.08197063600006,15.2,-7.88985650600001));
#281772=CARTESIAN_POINT('Ctrl Pts',(-7.08197063600006,11.6,-7.88985650600001));
#281773=CARTESIAN_POINT('Ctrl Pts',(-7.08025320600006,15.2,-7.88864203800002));
#281774=CARTESIAN_POINT('Ctrl Pts',(-7.08025320600006,11.6,-7.88864203800002));
#281775=CARTESIAN_POINT('Ctrl Pts',(-7.07854246000006,15.2,-7.88742999900002));
#281776=CARTESIAN_POINT('Ctrl Pts',(-7.07854246000006,11.6,-7.88742999900002));
#281777=CARTESIAN_POINT('Ctrl Pts',(-7.07683840300006,15.2,-7.88622040800002));
#281778=CARTESIAN_POINT('Ctrl Pts',(-7.07683840300006,11.6,-7.88622040800002));
#281779=CARTESIAN_POINT('Ctrl Pts',(-7.07514104100006,15.2,-7.88501328300002));
#281780=CARTESIAN_POINT('Ctrl Pts',(-7.07514104100006,11.6,-7.88501328300002));
#281781=CARTESIAN_POINT('Ctrl Pts',(-7.07345037900006,15.2,-7.88380863900001));
#281782=CARTESIAN_POINT('Ctrl Pts',(-7.07345037900006,11.6,-7.88380863900001));
#281783=CARTESIAN_POINT('Ctrl Pts',(-7.07176642300006,15.2,-7.88260649600002));
#281784=CARTESIAN_POINT('Ctrl Pts',(-7.07176642300006,11.6,-7.88260649600002));
#281785=CARTESIAN_POINT('Ctrl Pts',(-7.07008917700006,15.2,-7.88140687100002));
#281786=CARTESIAN_POINT('Ctrl Pts',(-7.07008917700006,11.6,-7.88140687100002));
#281787=CARTESIAN_POINT('Ctrl Pts',(-7.06841864900006,15.2,-7.88020978100001));
#281788=CARTESIAN_POINT('Ctrl Pts',(-7.06841864900006,11.6,-7.88020978100001));
#281789=CARTESIAN_POINT('Ctrl Pts',(-7.06675484400006,15.2,-7.87901524400001));
#281790=CARTESIAN_POINT('Ctrl Pts',(-7.06675484400006,11.6,-7.87901524400001));
#281791=CARTESIAN_POINT('Ctrl Pts',(-7.06509776700006,15.2,-7.87782327800001));
#281792=CARTESIAN_POINT('Ctrl Pts',(-7.06509776700006,11.6,-7.87782327800001));
#281793=CARTESIAN_POINT('Ctrl Pts',(-7.06344742100006,15.2,-7.87663390200001));
#281794=CARTESIAN_POINT('Ctrl Pts',(-7.06344742100006,11.6,-7.87663390200001));
#281795=CARTESIAN_POINT('Ctrl Pts',(-7.06180381600006,15.2,-7.87544713100001));
#281796=CARTESIAN_POINT('Ctrl Pts',(-7.06180381600006,11.6,-7.87544713100001));
#281797=CARTESIAN_POINT('Ctrl Pts',(-7.06016695600006,15.2,-7.87426298700002));
#281798=CARTESIAN_POINT('Ctrl Pts',(-7.06016695600006,11.6,-7.87426298700002));
#281799=CARTESIAN_POINT('Ctrl Pts',(-7.05853684500005,15.2,-7.87308148400002));
#281800=CARTESIAN_POINT('Ctrl Pts',(-7.05853684500005,11.6,-7.87308148400002));
#281801=CARTESIAN_POINT('Ctrl Pts',(-7.05691349000006,15.2,-7.87190264400002));
#281802=CARTESIAN_POINT('Ctrl Pts',(-7.05691349000006,11.6,-7.87190264400002));
#281803=CARTESIAN_POINT('Ctrl Pts',(-7.05529689500006,15.2,-7.87072648200001));
#281804=CARTESIAN_POINT('Ctrl Pts',(-7.05529689500006,11.6,-7.87072648200001));
#281805=CARTESIAN_POINT('Ctrl Pts',(-7.05368706800006,15.2,-7.86955301900001));
#281806=CARTESIAN_POINT('Ctrl Pts',(-7.05368706800006,11.6,-7.86955301900001));
#281807=CARTESIAN_POINT('Ctrl Pts',(-7.05208401300006,15.2,-7.86838227100001));
#281808=CARTESIAN_POINT('Ctrl Pts',(-7.05208401300006,11.6,-7.86838227100001));
#281809=CARTESIAN_POINT('Ctrl Pts',(-7.05048773700006,15.2,-7.86721425700001));
#281810=CARTESIAN_POINT('Ctrl Pts',(-7.05048773700006,11.6,-7.86721425700001));
#281811=CARTESIAN_POINT('Ctrl Pts',(-7.04889824400006,15.2,-7.86604899600002));
#281812=CARTESIAN_POINT('Ctrl Pts',(-7.04889824400006,11.6,-7.86604899600002));
#281813=CARTESIAN_POINT('Ctrl Pts',(-7.04731554000006,15.2,-7.86488650600001));
#281814=CARTESIAN_POINT('Ctrl Pts',(-7.04731554000006,11.6,-7.86488650600001));
#281815=CARTESIAN_POINT('Ctrl Pts',(-7.04573963100006,15.2,-7.86372680800002));
#281816=CARTESIAN_POINT('Ctrl Pts',(-7.04573963100006,11.6,-7.86372680800002));
#281817=CARTESIAN_POINT('Ctrl Pts',(-7.04417052200006,15.2,-7.86256991700002));
#281818=CARTESIAN_POINT('Ctrl Pts',(-7.04417052200006,11.6,-7.86256991700002));
#281819=CARTESIAN_POINT('Ctrl Pts',(-7.04260822000006,15.2,-7.86141585300002));
#281820=CARTESIAN_POINT('Ctrl Pts',(-7.04260822000006,11.6,-7.86141585300002));
#281821=CARTESIAN_POINT('Ctrl Pts',(-7.04105273000006,15.2,-7.86026463600002));
#281822=CARTESIAN_POINT('Ctrl Pts',(-7.04105273000006,11.6,-7.86026463600002));
#281823=CARTESIAN_POINT('Ctrl Pts',(-7.03950405700006,15.2,-7.85911628400001));
#281824=CARTESIAN_POINT('Ctrl Pts',(-7.03950405700006,11.6,-7.85911628400001));
#281825=CARTESIAN_POINT('Ctrl Pts',(-7.03796220600006,15.2,-7.85797081600002));
#281826=CARTESIAN_POINT('Ctrl Pts',(-7.03796220600006,11.6,-7.85797081600002));
#281827=CARTESIAN_POINT('Ctrl Pts',(-7.03642718500006,15.2,-7.85682825100002));
#281828=CARTESIAN_POINT('Ctrl Pts',(-7.03642718500006,11.6,-7.85682825100002));
#281829=CARTESIAN_POINT('Ctrl Pts',(-7.03489899900006,15.2,-7.85568860800002));
#281830=CARTESIAN_POINT('Ctrl Pts',(-7.03489899900006,11.6,-7.85568860800002));
#281831=CARTESIAN_POINT('Ctrl Pts',(-7.03337765200006,15.2,-7.85455190700001));
#281832=CARTESIAN_POINT('Ctrl Pts',(-7.03337765200006,11.6,-7.85455190700001));
#281833=CARTESIAN_POINT('Ctrl Pts',(-7.03186315100006,15.2,-7.85341816500001));
#281834=CARTESIAN_POINT('Ctrl Pts',(-7.03186315100006,11.6,-7.85341816500001));
#281835=CARTESIAN_POINT('Ctrl Pts',(-7.03035550200005,15.2,-7.85228740300001));
#281836=CARTESIAN_POINT('Ctrl Pts',(-7.03035550200005,11.6,-7.85228740300001));
#281837=CARTESIAN_POINT('Ctrl Pts',(-7.02885471100006,15.2,-7.85115964100001));
#281838=CARTESIAN_POINT('Ctrl Pts',(-7.02885471100006,11.6,-7.85115964100001));
#281839=CARTESIAN_POINT('Ctrl Pts',(-7.02736078200005,15.2,-7.85003489800002));
#281840=CARTESIAN_POINT('Ctrl Pts',(-7.02736078200005,11.6,-7.85003489800002));
#281841=CARTESIAN_POINT('Ctrl Pts',(-7.02587372100006,15.2,-7.84891319200002));
#281842=CARTESIAN_POINT('Ctrl Pts',(-7.02587372100006,11.6,-7.84891319200002));
#281843=CARTESIAN_POINT('Ctrl Pts',(-7.02439353500006,15.2,-7.84779454400002));
#281844=CARTESIAN_POINT('Ctrl Pts',(-7.02439353500006,11.6,-7.84779454400002));
#281845=CARTESIAN_POINT('Ctrl Pts',(-7.02292023000005,15.2,-7.84667897200002));
#281846=CARTESIAN_POINT('Ctrl Pts',(-7.02292023000005,11.6,-7.84667897200002));
#281847=CARTESIAN_POINT('Ctrl Pts',(-7.02145381000006,15.2,-7.84556649900002));
#281848=CARTESIAN_POINT('Ctrl Pts',(-7.02145381000006,11.6,-7.84556649900002));
#281849=CARTESIAN_POINT('Ctrl Pts',(-7.01999428200006,15.2,-7.84445714300002));
#281850=CARTESIAN_POINT('Ctrl Pts',(-7.01999428200006,11.6,-7.84445714300002));
#281851=CARTESIAN_POINT('Ctrl Pts',(-7.01854165200006,15.2,-7.84335092300001));
#281852=CARTESIAN_POINT('Ctrl Pts',(-7.01854165200006,11.6,-7.84335092300001));
#281853=CARTESIAN_POINT('Ctrl Pts',(-7.01709592400006,15.2,-7.84224785900002));
#281854=CARTESIAN_POINT('Ctrl Pts',(-7.01709592400006,11.6,-7.84224785900002));
#281855=CARTESIAN_POINT('Ctrl Pts',(-7.01565710600006,15.2,-7.84114797200001));
#281856=CARTESIAN_POINT('Ctrl Pts',(-7.01565710600006,11.6,-7.84114797200001));
#281857=CARTESIAN_POINT('Ctrl Pts',(-7.01422520300006,15.2,-7.84005128300001));
#281858=CARTESIAN_POINT('Ctrl Pts',(-7.01422520300006,11.6,-7.84005128300001));
#281859=CARTESIAN_POINT('Ctrl Pts',(-7.01280022000006,15.2,-7.83895780900002));
#281860=CARTESIAN_POINT('Ctrl Pts',(-7.01280022000006,11.6,-7.83895780900002));
#281861=CARTESIAN_POINT('Ctrl Pts',(-7.01138216400006,15.2,-7.83786757300001));
#281862=CARTESIAN_POINT('Ctrl Pts',(-7.01138216400006,11.6,-7.83786757300001));
#281863=CARTESIAN_POINT('Ctrl Pts',(-7.00997103900006,15.2,-7.83678059500001));
#281864=CARTESIAN_POINT('Ctrl Pts',(-7.00997103900006,11.6,-7.83678059500001));
#281865=CARTESIAN_POINT('Ctrl Pts',(-7.00856685400006,15.2,-7.83569689500001));
#281866=CARTESIAN_POINT('Ctrl Pts',(-7.00856685400006,11.6,-7.83569689500001));
#281867=CARTESIAN_POINT('Ctrl Pts',(-7.00716961100006,15.2,-7.83461649300002));
#281868=CARTESIAN_POINT('Ctrl Pts',(-7.00716961100006,11.6,-7.83461649300002));
#281869=CARTESIAN_POINT('Ctrl Pts',(-7.00577931900006,15.2,-7.83353941000002));
#281870=CARTESIAN_POINT('Ctrl Pts',(-7.00577931900006,11.6,-7.83353941000002));
#281871=CARTESIAN_POINT('Ctrl Pts',(-7.00439598300005,15.2,-7.83246566700001));
#281872=CARTESIAN_POINT('Ctrl Pts',(-7.00439598300005,11.6,-7.83246566700001));
#281873=CARTESIAN_POINT('Ctrl Pts',(-7.00301960800005,15.2,-7.83139528400002));
#281874=CARTESIAN_POINT('Ctrl Pts',(-7.00301960800005,11.6,-7.83139528400002));
#281875=CARTESIAN_POINT('Ctrl Pts',(-7.00165020000005,15.2,-7.83032828300002));
#281876=CARTESIAN_POINT('Ctrl Pts',(-7.00165020000005,11.6,-7.83032828300002));
#281877=CARTESIAN_POINT('Ctrl Pts',(-7.00028776600006,15.2,-7.82926468300002));
#281878=CARTESIAN_POINT('Ctrl Pts',(-7.00028776600006,11.6,-7.82926468300002));
#281879=CARTESIAN_POINT('Ctrl Pts',(-6.99893231000006,15.2,-7.82820450600001));
#281880=CARTESIAN_POINT('Ctrl Pts',(-6.99893231000006,11.6,-7.82820450600001));
#281881=CARTESIAN_POINT('Ctrl Pts',(-6.99758384000006,15.2,-7.82714777300002));
#281882=CARTESIAN_POINT('Ctrl Pts',(-6.99758384000006,11.6,-7.82714777300002));
#281883=CARTESIAN_POINT('Ctrl Pts',(-6.99624236100005,15.2,-7.82609450600001));
#281884=CARTESIAN_POINT('Ctrl Pts',(-6.99624236100005,11.6,-7.82609450600001));
#281885=CARTESIAN_POINT('Ctrl Pts',(-6.99490787900006,15.2,-7.82504472400002));
#281886=CARTESIAN_POINT('Ctrl Pts',(-6.99490787900006,11.6,-7.82504472400002));
#281887=CARTESIAN_POINT('Ctrl Pts',(-6.99358039900006,15.2,-7.82399845200001));
#281888=CARTESIAN_POINT('Ctrl Pts',(-6.99358039900006,11.6,-7.82399845200001));
#281889=CARTESIAN_POINT('Ctrl Pts',(-6.99225992900006,15.2,-7.82295570700001));
#281890=CARTESIAN_POINT('Ctrl Pts',(-6.99225992900006,11.6,-7.82295570700001));
#281891=CARTESIAN_POINT('Ctrl Pts',(-6.99094647300006,15.2,-7.82191651400002));
#281892=CARTESIAN_POINT('Ctrl Pts',(-6.99094647300006,11.6,-7.82191651400002));
#281893=CARTESIAN_POINT('Ctrl Pts',(-6.98964003800006,15.2,-7.82088089200002));
#281894=CARTESIAN_POINT('Ctrl Pts',(-6.98964003800006,11.6,-7.82088089200002));
#281895=CARTESIAN_POINT('Ctrl Pts',(-6.98834063000006,15.2,-7.81984886400001));
#281896=CARTESIAN_POINT('Ctrl Pts',(-6.98834063000006,11.6,-7.81984886400001));
#281897=CARTESIAN_POINT('Ctrl Pts',(-6.98704825400006,15.2,-7.81882045200001));
#281898=CARTESIAN_POINT('Ctrl Pts',(-6.98704825400006,11.6,-7.81882045200001));
#281899=CARTESIAN_POINT('Ctrl Pts',(-6.98576291700006,15.2,-7.81779567700001));
#281900=CARTESIAN_POINT('Ctrl Pts',(-6.98576291700006,11.6,-7.81779567700001));
#281901=CARTESIAN_POINT('Ctrl Pts',(-6.98448462500005,15.2,-7.81677456100001));
#281902=CARTESIAN_POINT('Ctrl Pts',(-6.98448462500005,11.6,-7.81677456100001));
#281903=CARTESIAN_POINT('Ctrl Pts',(-6.98321338300006,15.2,-7.81575712600001));
#281904=CARTESIAN_POINT('Ctrl Pts',(-6.98321338300006,11.6,-7.81575712600001));
#281905=CARTESIAN_POINT('Ctrl Pts',(-6.98194919900006,15.2,-7.81474339500001));
#281906=CARTESIAN_POINT('Ctrl Pts',(-6.98194919900006,11.6,-7.81474339500001));
#281907=CARTESIAN_POINT('Ctrl Pts',(-6.98069207700006,15.2,-7.81373338900002));
#281908=CARTESIAN_POINT('Ctrl Pts',(-6.98069207700006,11.6,-7.81373338900002));
#281909=CARTESIAN_POINT('Ctrl Pts',(-6.97944202300006,15.2,-7.81272712900002));
#281910=CARTESIAN_POINT('Ctrl Pts',(-6.97944202300006,11.6,-7.81272712900002));
#281911=CARTESIAN_POINT('Ctrl Pts',(-6.97819904600006,15.2,-7.81172464200001));
#281912=CARTESIAN_POINT('Ctrl Pts',(-6.97819904600006,11.6,-7.81172464200001));
#281913=CARTESIAN_POINT('Ctrl Pts',(-6.97696314800006,15.2,-7.81072594500002));
#281914=CARTESIAN_POINT('Ctrl Pts',(-6.97696314800006,11.6,-7.81072594500002));
#281915=CARTESIAN_POINT('Ctrl Pts',(-6.97573433800006,15.2,-7.80973106400002));
#281916=CARTESIAN_POINT('Ctrl Pts',(-6.97573433800006,11.6,-7.80973106400002));
#281917=CARTESIAN_POINT('Ctrl Pts',(-6.97451262200006,15.2,-7.80874002000001));
#281918=CARTESIAN_POINT('Ctrl Pts',(-6.97451262200006,11.6,-7.80874002000001));
#281919=CARTESIAN_POINT('Ctrl Pts',(-6.97329800400006,15.2,-7.80775283600001));
#281920=CARTESIAN_POINT('Ctrl Pts',(-6.97329800400006,11.6,-7.80775283600001));
#281921=CARTESIAN_POINT('Ctrl Pts',(-6.97209049200006,15.2,-7.80676953600001));
#281922=CARTESIAN_POINT('Ctrl Pts',(-6.97209049200006,11.6,-7.80676953600001));
#281923=CARTESIAN_POINT('Ctrl Pts',(-6.97089009100006,15.2,-7.80579014100002));
#281924=CARTESIAN_POINT('Ctrl Pts',(-6.97089009100006,11.6,-7.80579014100002));
#281925=CARTESIAN_POINT('Ctrl Pts',(-6.96969680800006,15.2,-7.80481467500002));
#281926=CARTESIAN_POINT('Ctrl Pts',(-6.96969680800006,11.6,-7.80481467500002));
#281927=CARTESIAN_POINT('Ctrl Pts',(-6.96851064900006,15.2,-7.80384316100001));
#281928=CARTESIAN_POINT('Ctrl Pts',(-6.96851064900006,11.6,-7.80384316100001));
#281929=CARTESIAN_POINT('Ctrl Pts',(-6.96733161900006,15.2,-7.80287562300002));
#281930=CARTESIAN_POINT('Ctrl Pts',(-6.96733161900006,11.6,-7.80287562300002));
#281931=CARTESIAN_POINT('Ctrl Pts',(-6.96615972600005,15.2,-7.80191208300002));
#281932=CARTESIAN_POINT('Ctrl Pts',(-6.96615972600005,11.6,-7.80191208300002));
#281933=CARTESIAN_POINT('Ctrl Pts',(-6.96499497600006,15.2,-7.80095256500001));
#281934=CARTESIAN_POINT('Ctrl Pts',(-6.96499497600006,11.6,-7.80095256500001));
#281935=CARTESIAN_POINT('Ctrl Pts',(-6.96383737400006,15.2,-7.79999709300002));
#281936=CARTESIAN_POINT('Ctrl Pts',(-6.96383737400006,11.6,-7.79999709300002));
#281937=CARTESIAN_POINT('Ctrl Pts',(-6.96268692700006,15.2,-7.79904568800001));
#281938=CARTESIAN_POINT('Ctrl Pts',(-6.96268692700006,11.6,-7.79904568800001));
#281939=CARTESIAN_POINT('Ctrl Pts',(-6.96154364000006,15.2,-7.79809837700002));
#281940=CARTESIAN_POINT('Ctrl Pts',(-6.96154364000006,11.6,-7.79809837700002));
#281941=CARTESIAN_POINT('Ctrl Pts',(-6.96040752100005,15.2,-7.79715518200002));
#281942=CARTESIAN_POINT('Ctrl Pts',(-6.96040752100005,11.6,-7.79715518200002));
#281943=CARTESIAN_POINT('Ctrl Pts',(-6.95927857600006,15.2,-7.79621612700002));
#281944=CARTESIAN_POINT('Ctrl Pts',(-6.95927857600006,11.6,-7.79621612700002));
#281945=CARTESIAN_POINT('Ctrl Pts',(-6.95815681000005,15.2,-7.79528123600001));
#281946=CARTESIAN_POINT('Ctrl Pts',(-6.95815681000005,11.6,-7.79528123600001));
#281947=CARTESIAN_POINT('Ctrl Pts',(-6.95704223000006,15.2,-7.79435053500002));
#281948=CARTESIAN_POINT('Ctrl Pts',(-6.95704223000006,11.6,-7.79435053500002));
#281949=CARTESIAN_POINT('Ctrl Pts',(-6.95593484300006,15.2,-7.79342404500002));
#281950=CARTESIAN_POINT('Ctrl Pts',(-6.95593484300006,11.6,-7.79342404500002));
#281951=CARTESIAN_POINT('Ctrl Pts',(-6.95483465400006,15.2,-7.79250179100002));
#281952=CARTESIAN_POINT('Ctrl Pts',(-6.95483465400006,11.6,-7.79250179100002));
#281953=CARTESIAN_POINT('Ctrl Pts',(-6.95374167100006,15.2,-7.79158379900001));
#281954=CARTESIAN_POINT('Ctrl Pts',(-6.95374167100006,11.6,-7.79158379900001));
#281955=CARTESIAN_POINT('Ctrl Pts',(-6.95265589800006,15.2,-7.79067009300002));
#281956=CARTESIAN_POINT('Ctrl Pts',(-6.95265589800006,11.6,-7.79067009300002));
#281957=CARTESIAN_POINT('Ctrl Pts',(-6.95157734400006,15.2,-7.78976069600001));
#281958=CARTESIAN_POINT('Ctrl Pts',(-6.95157734400006,11.6,-7.78976069600001));
#281959=CARTESIAN_POINT('Ctrl Pts',(-6.95050601300006,15.2,-7.78885563600002));
#281960=CARTESIAN_POINT('Ctrl Pts',(-6.95050601300006,11.6,-7.78885563600002));
#281961=CARTESIAN_POINT('Ctrl Pts',(-6.94944191300006,15.2,-7.78795493400001));
#281962=CARTESIAN_POINT('Ctrl Pts',(-6.94944191300006,11.6,-7.78795493400001));
#281963=CARTESIAN_POINT('Ctrl Pts',(-6.94838505000006,15.2,-7.78705861700002));
#281964=CARTESIAN_POINT('Ctrl Pts',(-6.94838505000006,11.6,-7.78705861700002));
#281965=CARTESIAN_POINT('Ctrl Pts',(-6.94733542900006,15.2,-7.78616671000002));
#281966=CARTESIAN_POINT('Ctrl Pts',(-6.94733542900006,11.6,-7.78616671000002));
#281967=CARTESIAN_POINT('Ctrl Pts',(-6.94629305800006,15.2,-7.78527923700001));
#281968=CARTESIAN_POINT('Ctrl Pts',(-6.94629305800006,11.6,-7.78527923700001));
#281969=CARTESIAN_POINT('Ctrl Pts',(-6.94525794400006,15.2,-7.78439622500001));
#281970=CARTESIAN_POINT('Ctrl Pts',(-6.94525794400006,11.6,-7.78439622500001));
#281971=CARTESIAN_POINT('Ctrl Pts',(-6.94423009200006,15.2,-7.78351769800001));
#281972=CARTESIAN_POINT('Ctrl Pts',(-6.94423009200006,11.6,-7.78351769800001));
#281973=CARTESIAN_POINT('Ctrl Pts',(-6.94320950800006,15.2,-7.78264368200002));
#281974=CARTESIAN_POINT('Ctrl Pts',(-6.94320950800006,11.6,-7.78264368200002));
#281975=CARTESIAN_POINT('Ctrl Pts',(-6.94219620100006,15.2,-7.78177420300001));
#281976=CARTESIAN_POINT('Ctrl Pts',(-6.94219620100006,11.6,-7.78177420300001));
#281977=CARTESIAN_POINT('Ctrl Pts',(-6.94119017500006,15.2,-7.78090928600002));
#281978=CARTESIAN_POINT('Ctrl Pts',(-6.94119017500006,11.6,-7.78090928600002));
#281979=CARTESIAN_POINT('Ctrl Pts',(-6.94019143600006,15.2,-7.78004895700001));
#281980=CARTESIAN_POINT('Ctrl Pts',(-6.94019143600006,11.6,-7.78004895700001));
#281981=CARTESIAN_POINT('Ctrl Pts',(-6.93919999400006,15.2,-7.77919324200001));
#281982=CARTESIAN_POINT('Ctrl Pts',(-6.93919999400006,11.6,-7.77919324200001));
#281983=CARTESIAN_POINT('Ctrl Pts',(-6.93821585300006,15.2,-7.77834216700001));
#281984=CARTESIAN_POINT('Ctrl Pts',(-6.93821585300006,11.6,-7.77834216700001));
#281985=CARTESIAN_POINT('Ctrl Pts',(-6.93723901900006,15.2,-7.77749575800001));
#281986=CARTESIAN_POINT('Ctrl Pts',(-6.93723901900006,11.6,-7.77749575800001));
#281987=CARTESIAN_POINT('Ctrl Pts',(-6.93626950100006,15.2,-7.77665404200001));
#281988=CARTESIAN_POINT('Ctrl Pts',(-6.93626950100006,11.6,-7.77665404200001));
#281989=CARTESIAN_POINT('Ctrl Pts',(-6.93530730300006,15.2,-7.77581704500002));
#281990=CARTESIAN_POINT('Ctrl Pts',(-6.93530730300006,11.6,-7.77581704500002));
#281991=CARTESIAN_POINT('Ctrl Pts',(-6.93435243400006,15.2,-7.77498479200001));
#281992=CARTESIAN_POINT('Ctrl Pts',(-6.93435243400006,11.6,-7.77498479200001));
#281993=CARTESIAN_POINT('Ctrl Pts',(-6.93340489800006,15.2,-7.77415731300002));
#281994=CARTESIAN_POINT('Ctrl Pts',(-6.93340489800006,11.6,-7.77415731300002));
#281995=CARTESIAN_POINT('Ctrl Pts',(-6.93246470300006,15.2,-7.77333463100002));
#281996=CARTESIAN_POINT('Ctrl Pts',(-6.93246470300006,11.6,-7.77333463100002));
#281997=CARTESIAN_POINT('Ctrl Pts',(-6.93153185600006,15.2,-7.77251677600002));
#281998=CARTESIAN_POINT('Ctrl Pts',(-6.93153185600006,11.6,-7.77251677600002));
#281999=CARTESIAN_POINT('Ctrl Pts',(-6.93060636400006,15.2,-7.77170377300001));
#282000=CARTESIAN_POINT('Ctrl Pts',(-6.93060636400006,11.6,-7.77170377300001));
#282001=CARTESIAN_POINT('Ctrl Pts',(-6.92968823200006,15.2,-7.77089565100002));
#282002=CARTESIAN_POINT('Ctrl Pts',(-6.92968823200006,11.6,-7.77089565100002));
#282003=CARTESIAN_POINT('Ctrl Pts',(-6.92877746800006,15.2,-7.77009243500002));
#282004=CARTESIAN_POINT('Ctrl Pts',(-6.92877746800006,11.6,-7.77009243500002));
#282005=CARTESIAN_POINT('Ctrl Pts',(-6.92787407800005,15.2,-7.76929415300001));
#282006=CARTESIAN_POINT('Ctrl Pts',(-6.92787407800005,11.6,-7.76929415300001));
#282007=CARTESIAN_POINT('Ctrl Pts',(-6.92697807000005,15.2,-7.76850083500002));
#282008=CARTESIAN_POINT('Ctrl Pts',(-6.92697807000005,11.6,-7.76850083500002));
#282009=CARTESIAN_POINT('Ctrl Pts',(-6.92608944900006,15.2,-7.76771250600002));
#282010=CARTESIAN_POINT('Ctrl Pts',(-6.92608944900006,11.6,-7.76771250600002));
#282011=CARTESIAN_POINT('Ctrl Pts',(-6.92520822300006,15.2,-7.76692919400002));
#282012=CARTESIAN_POINT('Ctrl Pts',(-6.92520822300006,11.6,-7.76692919400002));
#282013=CARTESIAN_POINT('Ctrl Pts',(-6.92433439800006,15.2,-7.76615092800002));
#282014=CARTESIAN_POINT('Ctrl Pts',(-6.92433439800006,11.6,-7.76615092800002));
#282015=CARTESIAN_POINT('Ctrl Pts',(-6.92346798200006,15.2,-7.76537773600002));
#282016=CARTESIAN_POINT('Ctrl Pts',(-6.92346798200006,11.6,-7.76537773600002));
#282017=CARTESIAN_POINT('Ctrl Pts',(-6.92260898000006,15.2,-7.76460964400002));
#282018=CARTESIAN_POINT('Ctrl Pts',(-6.92260898000006,11.6,-7.76460964400002));
#282019=CARTESIAN_POINT('Ctrl Pts',(-6.92175740000006,15.2,-7.76384668300001));
#282020=CARTESIAN_POINT('Ctrl Pts',(-6.92175740000006,11.6,-7.76384668300001));
#282021=CARTESIAN_POINT('Ctrl Pts',(-6.92091324900006,15.2,-7.76308888100001));
#282022=CARTESIAN_POINT('Ctrl Pts',(-6.92091324900006,11.6,-7.76308888100001));
#282023=CARTESIAN_POINT('Ctrl Pts',(-6.92007653400006,15.2,-7.76233626500002));
#282024=CARTESIAN_POINT('Ctrl Pts',(-6.92007653400006,11.6,-7.76233626500002));
#282025=CARTESIAN_POINT('Ctrl Pts',(-6.91924726000006,15.2,-7.76158886500002));
#282026=CARTESIAN_POINT('Ctrl Pts',(-6.91924726000006,11.6,-7.76158886500002));
#282027=CARTESIAN_POINT('Ctrl Pts',(-6.91842543700006,15.2,-7.76084670900002));
#282028=CARTESIAN_POINT('Ctrl Pts',(-6.91842543700006,11.6,-7.76084670900002));
#282029=CARTESIAN_POINT('Ctrl Pts',(-6.91761106900006,15.2,-7.76010982800001));
#282030=CARTESIAN_POINT('Ctrl Pts',(-6.91761106900006,11.6,-7.76010982800001));
#282031=CARTESIAN_POINT('Ctrl Pts',(-6.91680416500006,15.2,-7.75937824900002));
#282032=CARTESIAN_POINT('Ctrl Pts',(-6.91680416500006,11.6,-7.75937824900002));
#282033=CARTESIAN_POINT('Ctrl Pts',(-6.91600473100006,15.2,-7.75865200100001));
#282034=CARTESIAN_POINT('Ctrl Pts',(-6.91600473100006,11.6,-7.75865200100001));
#282035=CARTESIAN_POINT('Ctrl Pts',(-6.91521277400006,15.2,-7.75793111500001));
#282036=CARTESIAN_POINT('Ctrl Pts',(-6.91521277400006,11.6,-7.75793111500001));
#282037=CARTESIAN_POINT('Ctrl Pts',(-6.91442830100006,15.2,-7.75721562100002));
#282038=CARTESIAN_POINT('Ctrl Pts',(-6.91442830100006,11.6,-7.75721562100002));
#282039=CARTESIAN_POINT('Ctrl Pts',(-6.91365131900006,15.2,-7.75650554700002));
#282040=CARTESIAN_POINT('Ctrl Pts',(-6.91365131900006,11.6,-7.75650554700002));
#282041=CARTESIAN_POINT('Ctrl Pts',(-6.91288183600006,15.2,-7.75580092300002));
#282042=CARTESIAN_POINT('Ctrl Pts',(-6.91288183600006,11.6,-7.75580092300002));
#282043=CARTESIAN_POINT('Ctrl Pts',(-6.91211985800006,15.2,-7.75510178100002));
#282044=CARTESIAN_POINT('Ctrl Pts',(-6.91211985800006,11.6,-7.75510178100002));
#282045=CARTESIAN_POINT('Ctrl Pts',(-6.91136539200006,15.2,-7.75440814800002));
#282046=CARTESIAN_POINT('Ctrl Pts',(-6.91136539200006,11.6,-7.75440814800002));
#282047=CARTESIAN_POINT('Ctrl Pts',(-6.91061844600006,15.2,-7.75372005700002));
#282048=CARTESIAN_POINT('Ctrl Pts',(-6.91061844600006,11.6,-7.75372005700002));
#282049=CARTESIAN_POINT('Ctrl Pts',(-6.90987902600006,15.2,-7.75303753700002));
#282050=CARTESIAN_POINT('Ctrl Pts',(-6.90987902600006,11.6,-7.75303753700002));
#282051=CARTESIAN_POINT('Ctrl Pts',(-6.90914714100006,15.2,-7.75236061900002));
#282052=CARTESIAN_POINT('Ctrl Pts',(-6.90914714100006,11.6,-7.75236061900002));
#282053=CARTESIAN_POINT('Ctrl Pts',(-6.90842279600006,15.2,-7.75168933500002));
#282054=CARTESIAN_POINT('Ctrl Pts',(-6.90842279600006,11.6,-7.75168933500002));
#282055=CARTESIAN_POINT('Ctrl Pts',(-6.90770600000006,15.2,-7.75102371400001));
#282056=CARTESIAN_POINT('Ctrl Pts',(-6.90770600000006,11.6,-7.75102371400001));
#282057=CARTESIAN_POINT('Ctrl Pts',(-6.90699675800006,15.2,-7.75036378800002));
#282058=CARTESIAN_POINT('Ctrl Pts',(-6.90699675800006,11.6,-7.75036378800002));
#282059=CARTESIAN_POINT('Ctrl Pts',(-6.90629508000006,15.2,-7.74970958700001));
#282060=CARTESIAN_POINT('Ctrl Pts',(-6.90629508000006,11.6,-7.74970958700001));
#282061=CARTESIAN_POINT('Ctrl Pts',(-6.90560097000006,15.2,-7.74906114500002));
#282062=CARTESIAN_POINT('Ctrl Pts',(-6.90560097000006,11.6,-7.74906114500002));
#282063=CARTESIAN_POINT('Ctrl Pts',(-6.90491443800005,15.2,-7.74841849200002));
#282064=CARTESIAN_POINT('Ctrl Pts',(-6.90491443800005,11.6,-7.74841849200002));
#282065=CARTESIAN_POINT('Ctrl Pts',(-6.90423549100006,15.2,-7.74778165800001));
#282066=CARTESIAN_POINT('Ctrl Pts',(-6.90423549100006,11.6,-7.74778165800001));
#282067=CARTESIAN_POINT('Ctrl Pts',(-6.90356800200006,15.2,-7.74715431200002));
#282068=CARTESIAN_POINT('Ctrl Pts',(-6.90356800200006,11.6,-7.74715431200002));
#282069=CARTESIAN_POINT('Ctrl Pts',(-6.90304077600006,15.2,-7.74665780200002));
#282070=CARTESIAN_POINT('Ctrl Pts',(-6.90304077600006,11.6,-7.74665780200002));
#282071=CARTESIAN_POINT('Ctrl Pts',(-6.90264967000005,15.2,-7.74628893100001));
#282072=CARTESIAN_POINT('Ctrl Pts',(-6.90264967000005,11.6,-7.74628893100001));
#282073=CARTESIAN_POINT('Ctrl Pts',(-6.90239167400006,15.2,-7.74604536200002));
#282074=CARTESIAN_POINT('Ctrl Pts',(-6.90239167400006,11.6,-7.74604536200002));
#282075=CARTESIAN_POINT('Ctrl Pts',(-6.90226492000006,15.2,-7.74592563800002));
#282076=CARTESIAN_POINT('Ctrl Pts',(-6.90226492000006,11.6,-7.74592563800002));
#282077=CARTESIAN_POINT('',(-6.90226492000223,12.2,-7.74592563733579));
#282078=CARTESIAN_POINT('',(-6.90226492000223,15.2,-7.74592563733579));
#282079=CARTESIAN_POINT('',(-6.90226492000006,12.2,-7.74592563700002));
#282080=CARTESIAN_POINT('Ctrl Pts',(-7.93573928312123,12.2,-8.32310290867369));
#282081=CARTESIAN_POINT('Ctrl Pts',(-7.93215544686481,12.2,-8.32177217006299));
#282082=CARTESIAN_POINT('Ctrl Pts',(-7.9285793196337,12.2,-8.320439684464));
#282083=CARTESIAN_POINT('Ctrl Pts',(-7.9250108958958,12.2,-8.31910545665107));
#282084=CARTESIAN_POINT('Ctrl Pts',(-7.92144247215791,12.2,-8.31777122883814));
#282085=CARTESIAN_POINT('Ctrl Pts',(-7.9178817551368,12.2,-8.31643525657686));
#282086=CARTESIAN_POINT('Ctrl Pts',(-7.91432875292083,12.2,-8.31509755651716));
#282087=CARTESIAN_POINT('Ctrl Pts',(-7.91077575070486,12.2,-8.31375985645747));
#282088=CARTESIAN_POINT('Ctrl Pts',(-7.90723046392704,12.2,-8.31242042849342));
#282089=CARTESIAN_POINT('Ctrl Pts',(-7.9036929159712,12.2,-8.31107930933406));
#282090=CARTESIAN_POINT('Ctrl Pts',(-7.9001553673727,12.2,-8.30973818993105));
#282091=CARTESIAN_POINT('Ctrl Pts',(-7.89662555700969,12.2,-8.30839538038589));
#282092=CARTESIAN_POINT('Ctrl Pts',(-7.89310351045721,12.2,-8.3070509233986));
#282093=CARTESIAN_POINT('Ctrl Pts',(-7.88958146454457,12.2,-8.30570646665556));
#282094=CARTESIAN_POINT('Ctrl Pts',(-7.88606718362318,12.2,-8.30436036262094));
#282095=CARTESIAN_POINT('Ctrl Pts',(-7.88256068608459,12.2,-8.3030126456281));
#282096=CARTESIAN_POINT('Ctrl Pts',(-7.87905418854601,12.2,-8.30166492863525));
#282097=CARTESIAN_POINT('Ctrl Pts',(-7.87555547453582,12.2,-8.30031559610586));
#282098=CARTESIAN_POINT('Ctrl Pts',(-7.8720645630635,12.2,-8.2989646822738));
#282099=CARTESIAN_POINT('Ctrl Pts',(-7.86741001464514,12.2,-8.29716346391286));
#282100=CARTESIAN_POINT('Ctrl Pts',(-7.86276933845468,12.2,-8.29535943319745));
#282101=CARTESIAN_POINT('Ctrl Pts',(-7.85814258399815,12.2,-8.29355267501209));
#282102=CARTESIAN_POINT('Ctrl Pts',(-7.85467251736775,12.2,-8.29219760606535));
#282103=CARTESIAN_POINT('Ctrl Pts',(-7.85121028169792,12.2,-8.29084100413487));
#282104=CARTESIAN_POINT('Ctrl Pts',(-7.84775589898862,12.2,-8.28948290464563));
#282105=CARTESIAN_POINT('Ctrl Pts',(-7.84430151690686,12.2,-8.28812480540311));
#282106=CARTESIAN_POINT('Ctrl Pts',(-7.8408549865497,12.2,-8.28676520938565));
#282107=CARTESIAN_POINT('Ctrl Pts',(-7.83741633042532,12.2,-8.28540415155998));
#282108=CARTESIAN_POINT('Ctrl Pts',(-7.83397767430094,12.2,-8.28404309373431));
#282109=CARTESIAN_POINT('Ctrl Pts',(-7.83054689030472,12.2,-8.28268057405543));
#282110=CARTESIAN_POINT('Ctrl Pts',(-7.82712400028857,12.2,-8.28131662826545));
#282111=CARTESIAN_POINT('Ctrl Pts',(-7.82370111027241,12.2,-8.27995268247547));
#282112=CARTESIAN_POINT('Ctrl Pts',(-7.82028611349482,12.2,-8.27858731074114));
#282113=CARTESIAN_POINT('Ctrl Pts',(-7.81687903201977,12.2,-8.27722054949293));
#282114=CARTESIAN_POINT('Ctrl Pts',(-7.81347195054471,12.2,-8.27585378824472));
#282115=CARTESIAN_POINT('Ctrl Pts',(-7.81007278429725,12.2,-8.27448563789939));
#282116=CARTESIAN_POINT('Ctrl Pts',(-7.80668155287811,12.2,-8.27311613465761));
#282117=CARTESIAN_POINT('Ctrl Pts',(-7.80329032145898,12.2,-8.27174663141583));
#282118=CARTESIAN_POINT('Ctrl Pts',(-7.79990702624761,12.2,-8.27037577554912));
#282119=CARTESIAN_POINT('Ctrl Pts',(-7.79653168774416,12.2,-8.26900360426582));
#282120=CARTESIAN_POINT('Ctrl Pts',(-7.79315634862753,12.2,-8.26763143273325));
#282121=CARTESIAN_POINT('Ctrl Pts',(-7.78978896557149,12.2,-8.26625794518364));
#282122=CARTESIAN_POINT('Ctrl Pts',(-7.78642956000099,12.2,-8.26488317869199));
#282123=CARTESIAN_POINT('Ctrl Pts',(-7.78307015504078,12.2,-8.26350841245009));
#282124=CARTESIAN_POINT('Ctrl Pts',(-7.77971872771451,12.2,-8.26213236773578));
#282125=CARTESIAN_POINT('Ctrl Pts',(-7.77637529858655,12.2,-8.26075508096688));
#282126=CARTESIAN_POINT('Ctrl Pts',(-7.77303186945859,12.2,-8.25937779419796));
#282127=CARTESIAN_POINT('Ctrl Pts',(-7.76969643988251,12.2,-8.25799926661625));
#282128=CARTESIAN_POINT('Ctrl Pts',(-7.76636902892078,12.2,-8.25661953533294));
#282129=CARTESIAN_POINT('Ctrl Pts',(-7.76304161795905,12.2,-8.25523980404964));
#282130=CARTESIAN_POINT('Ctrl Pts',(-7.75972222642969,12.2,-8.25385886876648));
#282131=CARTESIAN_POINT('Ctrl Pts',(-7.75641087500833,12.2,-8.25247676752503));
#282132=CARTESIAN_POINT('Ctrl Pts',(-7.75309952358697,12.2,-8.25109466628356));
#282133=CARTESIAN_POINT('Ctrl Pts',(-7.7497962130903,12.2,-8.24971139966717));
#282134=CARTESIAN_POINT('Ctrl Pts',(-7.74650096408431,12.2,-8.2483270049259));
#282135=CARTESIAN_POINT('Ctrl Pts',(-7.74320571507833,12.2,-8.24694261018463));
#282136=CARTESIAN_POINT('Ctrl Pts',(-7.73991852723015,12.2,-8.24555708680177));
#282137=CARTESIAN_POINT('Ctrl Pts',(-7.73663942172319,12.2,-8.24417047501897));
#282138=CARTESIAN_POINT('Ctrl Pts',(-7.73336031562052,12.2,-8.24278386298426));
#282139=CARTESIAN_POINT('Ctrl Pts',(-7.73008929189515,12.2,-8.24139616141592));
#282140=CARTESIAN_POINT('Ctrl Pts',(-7.72682637179704,12.2,-8.24000740846395));
#282141=CARTESIAN_POINT('Ctrl Pts',(-7.7235634522917,12.2,-8.23861865576426));
#282142=CARTESIAN_POINT('Ctrl Pts',(-7.72030863636521,12.2,-8.23722885299999));
#282143=CARTESIAN_POINT('Ctrl Pts',(-7.71706194515526,12.2,-8.23583803777259));
#282144=CARTESIAN_POINT('Ctrl Pts',(-7.7138152539453,12.2,-8.23444722254519));
#282145=CARTESIAN_POINT('Ctrl Pts',(-7.71057668662994,12.2,-8.23305539574767));
#282146=CARTESIAN_POINT('Ctrl Pts',(-7.70734626516469,12.2,-8.23166259604819));
#282147=CARTESIAN_POINT('Ctrl Pts',(-7.70411584369943,12.2,-8.23026979634871));
#282148=CARTESIAN_POINT('Ctrl Pts',(-7.70089356871654,12.2,-8.22887602369935));
#282149=CARTESIAN_POINT('Ctrl Pts',(-7.69767945979166,12.2,-8.22748131750002));
#282150=CARTESIAN_POINT('Ctrl Pts',(-7.69446535086678,12.2,-8.2260866113007));
#282151=CARTESIAN_POINT('Ctrl Pts',(-7.69125940849989,12.2,-8.22469097263474));
#282152=CARTESIAN_POINT('Ctrl Pts',(-7.68806165453202,12.2,-8.22329443993556));
#282153=CARTESIAN_POINT('Ctrl Pts',(-7.68486390056416,12.2,-8.22189790723637));
#282154=CARTESIAN_POINT('Ctrl Pts',(-7.68167433502656,12.2,-8.22050048050616));
#282155=CARTESIAN_POINT('Ctrl Pts',(-7.67849297785725,12.2,-8.21910220023721));
#282156=CARTESIAN_POINT('Ctrl Pts',(-7.67531162068794,12.2,-8.21770391996824));
#282157=CARTESIAN_POINT('Ctrl Pts',(-7.67213847240943,12.2,-8.21630478603757));
#282158=CARTESIAN_POINT('Ctrl Pts',(-7.66897355443996,12.2,-8.21490483879688));
#282159=CARTESIAN_POINT('Ctrl Pts',(-7.66580863589553,12.2,-8.21350489130186));
#282160=CARTESIAN_POINT('Ctrl Pts',(-7.66265194833678,12.2,-8.21210413009828));
#282161=CARTESIAN_POINT('Ctrl Pts',(-7.65950351133866,12.2,-8.21070259572783));
#282162=CARTESIAN_POINT('Ctrl Pts',(-7.65635507491252,12.2,-8.20930106161198));
#282163=CARTESIAN_POINT('Ctrl Pts',(-7.65321489037758,12.2,-8.20789875536284));
#282164=CARTESIAN_POINT('Ctrl Pts',(-7.65008297840876,12.2,-8.20649571628874));
#282165=CARTESIAN_POINT('Ctrl Pts',(-7.64695106643993,12.2,-8.20509267721465));
#282166=CARTESIAN_POINT('Ctrl Pts',(-7.64382742716476,12.2,-8.20368890713743));
#282167=CARTESIAN_POINT('Ctrl Pts',(-7.64071208126384,12.2,-8.20228444497374));
#282168=CARTESIAN_POINT('Ctrl Pts',(-7.63759673536292,12.2,-8.20087998281006));
#282169=CARTESIAN_POINT('Ctrl Pts',(-7.63448968465434,12.2,-8.19947482942327));
#282170=CARTESIAN_POINT('Ctrl Pts',(-7.63139094775282,12.2,-8.19806902675963));
#282171=CARTESIAN_POINT('Ctrl Pts',(-7.62829221085129,12.2,-8.19666322409599));
#282172=CARTESIAN_POINT('Ctrl Pts',(-7.6252017895415,12.2,-8.1952567725022));
#282173=CARTESIAN_POINT('Ctrl Pts',(-7.62211970461109,12.2,-8.19384971188671));
#282174=CARTESIAN_POINT('Ctrl Pts',(-7.61903761968067,12.2,-8.19244265127122));
#282175=CARTESIAN_POINT('Ctrl Pts',(-7.61596387180803,12.2,-8.19103498302244));
#282176=CARTESIAN_POINT('Ctrl Pts',(-7.6128984808766,12.2,-8.18962674882368));
#282177=CARTESIAN_POINT('Ctrl Pts',(-7.60983308938827,12.2,-8.18821851436909));
#282178=CARTESIAN_POINT('Ctrl Pts',(-7.60677605614401,12.2,-8.18680971328102));
#282179=CARTESIAN_POINT('Ctrl Pts',(-7.60372740161874,12.2,-8.18540038845112));
#282180=CARTESIAN_POINT('Ctrl Pts',(-7.60067874764731,12.2,-8.18399106387725));
#282181=CARTESIAN_POINT('Ctrl Pts',(-7.59763847248716,12.2,-8.18258121676309));
#282182=CARTESIAN_POINT('Ctrl Pts',(-7.59460659786349,12.2,-8.18117088670215));
#282183=CARTESIAN_POINT('Ctrl Pts',(-7.59157472323982,12.2,-8.17976055664121));
#282184=CARTESIAN_POINT('Ctrl Pts',(-7.58855124891122,12.2,-8.17834974691161));
#282185=CARTESIAN_POINT('Ctrl Pts',(-7.58553619685484,12.2,-8.17693849783785));
#282186=CARTESIAN_POINT('Ctrl Pts',(-7.58151612762892,12.2,-8.17505683249163));
#282187=CARTESIAN_POINT('Ctrl Pts',(-7.57751103041939,12.2,-8.17317438777057));
#282188=CARTESIAN_POINT('Ctrl Pts',(-7.57352095591071,12.2,-8.17129126625791));
#282189=CARTESIAN_POINT('Ctrl Pts',(-7.56953088085838,12.2,-8.16940814448868));
#282190=CARTESIAN_POINT('Ctrl Pts',(-7.56555582840605,12.2,-8.16752434579888));
#282191=CARTESIAN_POINT('Ctrl Pts',(-7.56159585000564,12.2,-8.1656399734654));
#282192=CARTESIAN_POINT('Ctrl Pts',(-7.55763587214477,12.2,-8.16375560138867));
#282193=CARTESIAN_POINT('Ctrl Pts',(-7.55369096720059,12.2,-8.16187065609021));
#282194=CARTESIAN_POINT('Ctrl Pts',(-7.54976118740919,12.2,-8.15998524129995));
#282195=CARTESIAN_POINT('Ctrl Pts',(-7.54583140708236,12.2,-8.1580998262528));
#282196=CARTESIAN_POINT('Ctrl Pts',(-7.54191675189306,12.2,-8.15621394142504));
#282197=CARTESIAN_POINT('Ctrl Pts',(-7.53801727095833,12.2,-8.15432769376669));
#282198=CARTESIAN_POINT('Ctrl Pts',(-7.53411779002358,12.2,-8.15244144610833));
#282199=CARTESIAN_POINT('Ctrl Pts',(-7.53023348535174,12.2,-8.15055483317495));
#282200=CARTESIAN_POINT('Ctrl Pts',(-7.5263644076424,12.2,-8.14866796468318));
#282201=CARTESIAN_POINT('Ctrl Pts',(-7.52249533046023,12.2,-8.1467810964485));
#282202=CARTESIAN_POINT('Ctrl Pts',(-7.51864147918963,12.2,-8.14489397017781));
#282203=CARTESIAN_POINT('Ctrl Pts',(-7.51480290548595,12.2,-8.14300669476797));
#282204=CARTESIAN_POINT('Ctrl Pts',(-7.51096433125928,12.2,-8.141119419101));
#282205=CARTESIAN_POINT('Ctrl Pts',(-7.50714103620837,12.2,-8.13923199231373));
#282206=CARTESIAN_POINT('Ctrl Pts',(-7.50333306916907,12.2,-8.13734452593308));
#282207=CARTESIAN_POINT('Ctrl Pts',(-7.4995251026486,12.2,-8.1354570598096));
#282208=CARTESIAN_POINT('Ctrl Pts',(-7.49573246448723,12.2,-8.13356955182223));
#282209=CARTESIAN_POINT('Ctrl Pts',(-7.4919552078506,12.2,-8.13168211242098));
#282210=CARTESIAN_POINT('Ctrl Pts',(-7.48817795069932,12.2,-8.12979467276257));
#282211=CARTESIAN_POINT('Ctrl Pts',(-7.48441607204093,12.2,-8.12790730106497));
#282212=CARTESIAN_POINT('Ctrl Pts',(-7.48066962620645,12.2,-8.12602010870117));
#282213=CARTESIAN_POINT('Ctrl Pts',(-7.47692318088242,12.2,-8.1241329165945));
#282214=CARTESIAN_POINT('Ctrl Pts',(-7.4731921677234,12.2,-8.12224590358893));
#282215=CARTESIAN_POINT('Ctrl Pts',(-7.46947663780388,12.2,-8.12035918218759));
#282216=CARTESIAN_POINT('Ctrl Pts',(-7.46576110737813,12.2,-8.11847246052918));
#282217=CARTESIAN_POINT('Ctrl Pts',(-7.46206105915984,12.2,-8.1165860293236));
#282218=CARTESIAN_POINT('Ctrl Pts',(-7.45837654618227,12.2,-8.1147000023875));
#282219=CARTESIAN_POINT('Ctrl Pts',(-7.45469203370671,12.2,-8.11281397570838));
#282220=CARTESIAN_POINT('Ctrl Pts',(-7.4510230568293,12.2,-8.11092835183589));
#282221=CARTESIAN_POINT('Ctrl Pts',(-7.4473696655552,12.2,-8.10904324700689));
#282222=CARTESIAN_POINT('Ctrl Pts',(-7.44371627378333,12.2,-8.10715814192103));
#282223=CARTESIAN_POINT('Ctrl Pts',(-7.44007846809209,12.2,-8.10527355415142));
#282224=CARTESIAN_POINT('Ctrl Pts',(-7.43645630172902,12.2,-8.10338960110433));
#282225=CARTESIAN_POINT('Ctrl Pts',(-7.43283413585948,12.2,-8.10150564831394));
#282226=CARTESIAN_POINT('Ctrl Pts',(-7.42922760845351,12.2,-8.0996223269651));
#282227=CARTESIAN_POINT('Ctrl Pts',(-7.42563677057877,12.2,-8.09773975634114));
#282228=CARTESIAN_POINT('Ctrl Pts',(-7.42204593221477,12.2,-8.09585718546067));
#282229=CARTESIAN_POINT('Ctrl Pts',(-7.41847078438843,12.2,-8.0939753645803));
#282230=CARTESIAN_POINT('Ctrl Pts',(-7.41491137874999,12.2,-8.09209441103335));
#282231=CARTESIAN_POINT('Ctrl Pts',(-7.41135197311155,12.2,-8.09021345748639));
#282232=CARTESIAN_POINT('Ctrl Pts',(-7.4078083084694,12.2,-8.08833337134231));
#282233=CARTESIAN_POINT('Ctrl Pts',(-7.40428043938986,12.2,-8.08645427118445));
#282234=CARTESIAN_POINT('Ctrl Pts',(-7.40075257079099,12.2,-8.08457517128261));
#282235=CARTESIAN_POINT('Ctrl Pts',(-7.39724049557693,12.2,-8.08269705748415));
#282236=CARTESIAN_POINT('Ctrl Pts',(-7.39374426773571,12.2,-8.08082005018462));
#282237=CARTESIAN_POINT('Ctrl Pts',(-7.39024803941813,12.2,-8.07894304262935));
#282238=CARTESIAN_POINT('Ctrl Pts',(-7.38676765735409,12.2,-8.07706714246778));
#282239=CARTESIAN_POINT('Ctrl Pts',(-7.38330317316689,12.2,-8.07519246847683));
#282240=CARTESIAN_POINT('Ctrl Pts',(-7.37983868945174,12.2,-8.07331779474132));
#282241=CARTESIAN_POINT('Ctrl Pts',(-7.3763901061623,12.2,-8.07144435001955));
#282242=CARTESIAN_POINT('Ctrl Pts',(-7.37295747299743,12.2,-8.06957225489473));
#282243=CARTESIAN_POINT('Ctrl Pts',(-7.36952483936486,12.2,-8.06770015951484));
#282244=CARTESIAN_POINT('Ctrl Pts',(-7.36610815729102,12.2,-8.06582941485169));
#282245=CARTESIAN_POINT('Ctrl Pts',(-7.36270747821495,12.2,-8.06396014454544));
#282246=CARTESIAN_POINT('Ctrl Pts',(-7.35930679960223,12.2,-8.06209087449389));
#282247=CARTESIAN_POINT('Ctrl Pts',(-7.35592212564285,12.2,-8.06022307811124));
#282248=CARTESIAN_POINT('Ctrl Pts',(-7.35255350775053,12.2,-8.05835688215259));
#282249=CARTESIAN_POINT('Ctrl Pts',(-7.34918488939922,12.2,-8.05649068593966));
#282250=CARTESIAN_POINT('Ctrl Pts',(-7.34583232715261,12.2,-8.05462608910192));
#282251=CARTESIAN_POINT('Ctrl Pts',(-7.34249587419406,12.2,-8.0527632183894));
#282252=CARTESIAN_POINT('Ctrl Pts',(-7.33915942169009,12.2,-8.0509003479307));
#282253=CARTESIAN_POINT('Ctrl Pts',(-7.33583907811755,12.2,-8.04903920397751));
#282254=CARTESIAN_POINT('Ctrl Pts',(-7.33253489672121,12.2,-8.04717991403648));
#282255=CARTESIAN_POINT('Ctrl Pts',(-7.32923071487467,12.2,-8.04532062384212));
#282256=CARTESIAN_POINT('Ctrl Pts',(-7.32594269547659,12.2,-8.04346318794932));
#282257=CARTESIAN_POINT('Ctrl Pts',(-7.32267088996601,12.2,-8.04160773584834));
#282258=CARTESIAN_POINT('Ctrl Pts',(-7.31939908490122,12.2,-8.03975228400016));
#282259=CARTESIAN_POINT('Ctrl Pts',(-7.3161434951248,12.2,-8.03789881556546));
#282260=CARTESIAN_POINT('Ctrl Pts',(-7.31290417455464,12.2,-8.03604746232771));
#282261=CARTESIAN_POINT('Ctrl Pts',(-7.3096648535431,12.2,-8.03419610883771));
#282262=CARTESIAN_POINT('Ctrl Pts',(-7.3064417995482,12.2,-8.03234686841334));
#282263=CARTESIAN_POINT('Ctrl Pts',(-7.30323506724781,12.2,-8.03049987574875));
#282264=CARTESIAN_POINT('Ctrl Pts',(-7.30002833538435,12.2,-8.02865288333581));
#282265=CARTESIAN_POINT('Ctrl Pts',(-7.29683792555837,12.2,-8.02680813845364));
#282266=CARTESIAN_POINT('Ctrl Pts',(-7.29366388976062,12.2,-8.02496577332624));
#282267=CARTESIAN_POINT('Ctrl Pts',(-7.29048985353041,12.2,-8.0231234079478));
#282268=CARTESIAN_POINT('Ctrl Pts',(-7.28733219257952,12.2,-8.02128342287237));
#282269=CARTESIAN_POINT('Ctrl Pts',(-7.28419096024165,12.2,-8.01944595355));
#282270=CARTESIAN_POINT('Ctrl Pts',(-7.28104972790377,12.2,-8.01760848422763));
#282271=CARTESIAN_POINT('Ctrl Pts',(-7.27792492280393,12.2,-8.01577353110556));
#282272=CARTESIAN_POINT('Ctrl Pts',(-7.27481660052511,12.2,-8.01394123045042));
#282273=CARTESIAN_POINT('Ctrl Pts',(-7.2717082786698,12.2,-8.01210893004493));
#282274=CARTESIAN_POINT('Ctrl Pts',(-7.26861643917305,12.2,-8.01027928238799));
#282275=CARTESIAN_POINT('Ctrl Pts',(-7.26554113524376,12.2,-8.00845242475125));
#282276=CARTESIAN_POINT('Ctrl Pts',(-7.26246583089545,12.2,-8.00662556686559));
#282277=CARTESIAN_POINT('Ctrl Pts',(-7.2594070613084,12.2,-8.00480150117622));
#282278=CARTESIAN_POINT('Ctrl Pts',(-7.25636488297762,12.2,-8.00298036524392));
#282279=CARTESIAN_POINT('Ctrl Pts',(-7.25332270506134,12.2,-8.00115922955977));
#282280=CARTESIAN_POINT('Ctrl Pts',(-7.25029711703457,12.2,-7.99934102533912));
#282281=CARTESIAN_POINT('Ctrl Pts',(-7.24728817194613,12.2,-7.99752589293175));
#282282=CARTESIAN_POINT('Ctrl Pts',(-7.24277475410848,12.2,-7.99480319419703));
#282283=CARTESIAN_POINT('Ctrl Pts',(-7.23829878510839,12.2,-7.99208740894731));
#282284=CARTESIAN_POINT('Ctrl Pts',(-7.23386044993378,12.2,-7.98937901854522));
#282285=CARTESIAN_POINT('Ctrl Pts',(-7.23090155954861,12.2,-7.98757342477982));
#282286=CARTESIAN_POINT('Ctrl Pts',(-7.22795939422332,12.2,-7.98577111992305));
#282287=CARTESIAN_POINT('Ctrl Pts',(-7.22503400800832,12.2,-7.98397224799167));
#282288=CARTESIAN_POINT('Ctrl Pts',(-7.22210862179332,12.2,-7.98217337606029));
#282289=CARTESIAN_POINT('Ctrl Pts',(-7.21920001571086,12.2,-7.98037793704044));
#282290=CARTESIAN_POINT('Ctrl Pts',(-7.21630824477718,12.2,-7.97858607966536));
#282291=CARTESIAN_POINT('Ctrl Pts',(-7.21341647423752,12.2,-7.97679422253443));
#282292=CARTESIAN_POINT('Ctrl Pts',(-7.210541537323,12.2,-7.97500594559678));
#282293=CARTESIAN_POINT('Ctrl Pts',(-7.20768349071027,12.2,-7.97322139873455));
#282294=CARTESIAN_POINT('Ctrl Pts',(-7.20482544370815,12.2,-7.97143685162918));
#282295=CARTESIAN_POINT('Ctrl Pts',(-7.20198428635432,12.2,-7.96965603490592));
#282296=CARTESIAN_POINT('Ctrl Pts',(-7.19916007281324,12.2,-7.96787909847614));
#282297=CARTESIAN_POINT('Ctrl Pts',(-7.19562980607929,12.2,-7.96565792805996));
#282298=CARTESIAN_POINT('Ctrl Pts',(-7.192126014643,12.2,-7.96344282174945));
#282299=CARTESIAN_POINT('Ctrl Pts',(-7.18864880777018,12.2,-7.96123407869443));
#282300=CARTESIAN_POINT('Ctrl Pts',(-7.18517160127638,12.2,-7.95902533588016));
#282301=CARTESIAN_POINT('Ctrl Pts',(-7.1817209772268,12.2,-7.95682295612061));
#282302=CARTESIAN_POINT('Ctrl Pts',(-7.17829704572285,12.2,-7.95462724184554));
#282303=CARTESIAN_POINT('Ctrl Pts',(-7.1748731138457,12.2,-7.95243152733112));
#282304=CARTESIAN_POINT('Ctrl Pts',(-7.17147587422639,12.2,-7.95024247967488));
#282305=CARTESIAN_POINT('Ctrl Pts',(-7.16810543422419,12.2,-7.94806040599375));
#282306=CARTESIAN_POINT('Ctrl Pts',(-7.16473499422198,12.2,-7.94587833231261));
#282307=CARTESIAN_POINT('Ctrl Pts',(-7.16139135518046,12.2,-7.94370323307859));
#282308=CARTESIAN_POINT('Ctrl Pts',(-7.15807462594216,12.2,-7.94153542175855));
#282309=CARTESIAN_POINT('Ctrl Pts',(-7.15475789670386,12.2,-7.93936761043851));
#282310=CARTESIAN_POINT('Ctrl Pts',(-7.15146807792705,12.2,-7.93720708489693));
#282311=CARTESIAN_POINT('Ctrl Pts',(-7.14820527838718,12.2,-7.93505416673328));
#282312=CARTESIAN_POINT('Ctrl Pts',(-7.1449424788473,12.2,-7.93290124856964));
#282313=CARTESIAN_POINT('Ctrl Pts',(-7.14170669717808,12.2,-7.93075593470691));
#282314=CARTESIAN_POINT('Ctrl Pts',(-7.13849804696834,12.2,-7.92861854866483));
#282315=CARTESIAN_POINT('Ctrl Pts',(-7.1352893967586,12.2,-7.92648116262276));
#282316=CARTESIAN_POINT('Ctrl Pts',(-7.13210787598566,12.2,-7.92435170576144));
#282317=CARTESIAN_POINT('Ctrl Pts',(-7.12895359591477,12.2,-7.92223050541377));
#282318=CARTESIAN_POINT('Ctrl Pts',(-7.12579931584389,12.2,-7.9201093050661));
#282319=CARTESIAN_POINT('Ctrl Pts',(-7.12267227614361,12.2,-7.91799636081627));
#282320=CARTESIAN_POINT('Ctrl Pts',(-7.11957258856001,12.2,-7.91589200650114));
#282321=CARTESIAN_POINT('Ctrl Pts',(-7.11647290097642,12.2,-7.91378765218601));
#282322=CARTESIAN_POINT('Ctrl Pts',(-7.11340056493333,12.2,-7.91169188988889));
#282323=CARTESIAN_POINT('Ctrl Pts',(-7.11035569243332,12.2,-7.90960505474999));
#282324=CARTESIAN_POINT('Ctrl Pts',(-7.1073108199333,12.2,-7.9075182196111));
#282325=CARTESIAN_POINT('Ctrl Pts',(-7.1042934119952,12.2,-7.90544031415824));
#282326=CARTESIAN_POINT('Ctrl Pts',(-7.10130358094003,12.2,-7.90337168227387));
#282327=CARTESIAN_POINT('Ctrl Pts',(-7.09831374988486,12.2,-7.9013030503895));
#282328=CARTESIAN_POINT('Ctrl Pts',(-7.09535149272347,12.2,-7.89924369204327));
#282329=CARTESIAN_POINT('Ctrl Pts',(-7.09241692751658,12.2,-7.89719395780768));
#282330=CARTESIAN_POINT('Ctrl Pts',(-7.08948236230969,12.2,-7.89514422357207));
#282331=CARTESIAN_POINT('Ctrl Pts',(-7.08657548391596,12.2,-7.89310411410564));
#282332=CARTESIAN_POINT('Ctrl Pts',(-7.08369641127853,12.2,-7.89107398563395));
#282333=CARTESIAN_POINT('Ctrl Pts',(-7.08081733864111,12.2,-7.88904385716226));
#282334=CARTESIAN_POINT('Ctrl Pts',(-7.07796606838923,12.2,-7.88702370822752));
#282335=CARTESIAN_POINT('Ctrl Pts',(-7.07514271568067,12.2,-7.88501390305838));
#282336=CARTESIAN_POINT('Ctrl Pts',(-7.07231936297211,12.2,-7.88300409788925));
#282337=CARTESIAN_POINT('Ctrl Pts',(-7.06952392673015,12.2,-7.88100463642787));
#282338=CARTESIAN_POINT('Ctrl Pts',(-7.06675652562136,12.2,-7.8790158864982));
#282339=CARTESIAN_POINT('Ctrl Pts',(-7.06398912451256,12.2,-7.87702713656852));
#282340=CARTESIAN_POINT('Ctrl Pts',(-7.06124975452084,12.2,-7.87504909936403));
#282341=CARTESIAN_POINT('Ctrl Pts',(-7.05853853362037,12.2,-7.87308214943438));
#282342=CARTESIAN_POINT('Ctrl Pts',(-7.05528506865801,12.2,-7.87072180960457));
#282343=CARTESIAN_POINT('Ctrl Pts',(-7.05207213696025,12.2,-7.8683774363129));
#282344=CARTESIAN_POINT('Ctrl Pts',(-7.04889994107727,12.2,-7.86604968864819));
#282345=CARTESIAN_POINT('Ctrl Pts',(-7.0457277451943,12.2,-7.86372194098349));
#282346=CARTESIAN_POINT('Ctrl Pts',(-7.04259628549976,12.2,-7.86141082187582));
#282347=CARTESIAN_POINT('Ctrl Pts',(-7.03950576269359,12.2,-7.85911700512507));
#282348=CARTESIAN_POINT('Ctrl Pts',(-7.03641523988741,12.2,-7.85682318837432));
#282349=CARTESIAN_POINT('Ctrl Pts',(-7.03336565587143,12.2,-7.854546673907));
#282350=CARTESIAN_POINT('Ctrl Pts',(-7.03035721681124,12.2,-7.85228815323783));
#282351=CARTESIAN_POINT('Ctrl Pts',(-7.02734877747779,12.2,-7.8500296323635));
#282352=CARTESIAN_POINT('Ctrl Pts',(-7.02438147990668,12.2,-7.84778910417424));
#282353=CARTESIAN_POINT('Ctrl Pts',(-7.02145553283236,12.2,-7.84556727813731));
#282354=CARTESIAN_POINT('Ctrl Pts',(-7.01852958602383,12.2,-7.84334545230219));
#282355=CARTESIAN_POINT('Ctrl Pts',(-7.0156449897193,12.2,-7.84114232482326));
#282356=CARTESIAN_POINT('Ctrl Pts',(-7.01280195172628,12.2,-7.83895861847598));
#282357=CARTESIAN_POINT('Ctrl Pts',(-7.00995891373326,12.2,-7.83677491212871));
#282358=CARTESIAN_POINT('Ctrl Pts',(-7.00715743354507,12.2,-7.83461062967385));
#282359=CARTESIAN_POINT('Ctrl Pts',(-7.00439772355913,12.2,-7.83246650725036));
#282360=CARTESIAN_POINT('Ctrl Pts',(-7.00163801332253,12.2,-7.83032238463211));
#282361=CARTESIAN_POINT('Ctrl Pts',(-6.99892007034333,12.2,-7.82819842264841));
#282362=CARTESIAN_POINT('Ctrl Pts',(-6.99624410998289,12.2,-7.82609537709659));
#282363=CARTESIAN_POINT('Ctrl Pts',(-6.99356814986552,12.2,-7.82399233173581));
#282364=CARTESIAN_POINT('Ctrl Pts',(-6.99093417092248,12.2,-7.82191020433345));
#282365=CARTESIAN_POINT('Ctrl Pts',(-6.98834238801665,12.2,-7.81984976799165));
#282366=CARTESIAN_POINT('Ctrl Pts',(-6.98575060511082,12.2,-7.81778933164984));
#282367=CARTESIAN_POINT('Ctrl Pts',(-6.98320101896006,12.2,-7.81575058769804));
#282368=CARTESIAN_POINT('Ctrl Pts',(-6.98069384429828,12.2,-7.81373432576976));
#282369=CARTESIAN_POINT('Ctrl Pts',(-6.97818666940873,12.2,-7.81171806365833));
#282370=CARTESIAN_POINT('Ctrl Pts',(-6.97572190940799,12.2,-7.80972428723889));
#282371=CARTESIAN_POINT('Ctrl Pts',(-6.97329978024078,12.2,-7.80775380678441));
#282372=CARTESIAN_POINT('Ctrl Pts',(-6.97087765129358,12.2,-7.80578332650892));
#282373=CARTESIAN_POINT('Ctrl Pts',(-6.96849815374008,12.2,-7.80383614243011));
#282374=CARTESIAN_POINT('Ctrl Pts',(-6.96616151174164,12.2,-7.80191308849997));
#282375=CARTESIAN_POINT('Ctrl Pts',(-6.96382486974319,12.2,-7.79999003456982));
#282376=CARTESIAN_POINT('Ctrl Pts',(-6.96153108101764,12.2,-7.79809111005829));
#282377=CARTESIAN_POINT('Ctrl Pts',(-6.95928037098448,12.2,-7.79621716819798));
#282378=CARTESIAN_POINT('Ctrl Pts',(-6.95702966074689,12.2,-7.79434322616746));
#282379=CARTESIAN_POINT('Ctrl Pts',(-6.95482202850409,12.2,-7.79249426894052));
#282380=CARTESIAN_POINT('Ctrl Pts',(-6.95265770247241,12.2,-7.79067117009293));
#282381=CARTESIAN_POINT('Ctrl Pts',(-6.95049337663734,12.2,-7.78884807141093));
#282382=CARTESIAN_POINT('Ctrl Pts',(-6.94837235616622,12.2,-7.78705083291782));
#282383=CARTESIAN_POINT('Ctrl Pts',(-6.94629487223237,12.2,-7.78528035222416));
#282384=CARTESIAN_POINT('Ctrl Pts',(-6.94421738829851,12.2,-7.7835098715305));
#282385=CARTESIAN_POINT('Ctrl Pts',(-6.94218344007158,12.2,-7.78176615019914));
#282386=CARTESIAN_POINT('Ctrl Pts',(-6.94019326030863,12.2,-7.7800501105936));
#282387=CARTESIAN_POINT('Ctrl Pts',(-6.93820308036491,12.2,-7.7783340708322));
#282388=CARTESIAN_POINT('Ctrl Pts',(-6.93625667117666,12.2,-7.77664571293258));
#282389=CARTESIAN_POINT('Ctrl Pts',(-6.93435426707596,12.2,-7.77498598526073));
#282390=CARTESIAN_POINT('Ctrl Pts',(-6.93245186314808,12.2,-7.77332625773965));
#282391=CARTESIAN_POINT('Ctrl Pts',(-6.93059346418344,12.2,-7.77169516153665));
#282392=CARTESIAN_POINT('Ctrl Pts',(-6.92877931141796,12.2,-7.77009366842948));
#282393=CARTESIAN_POINT('Ctrl Pts',(-6.92696515865248,12.2,-7.7684921753223));
#282394=CARTESIAN_POINT('Ctrl Pts',(-6.92519525247513,12.2,-7.76692029032111));
#282395=CARTESIAN_POINT('Ctrl Pts',(-6.9234698356192,12.2,-7.76537901112575));
#282396=CARTESIAN_POINT('Ctrl Pts',(-6.92174441876326,12.2,-7.76383773193041));
#282397=CARTESIAN_POINT('Ctrl Pts',(-6.92006349083027,12.2,-7.76232705999294));
#282398=CARTESIAN_POINT('Ctrl Pts',(-6.91842730097,12.2,-7.76084802787785));
#282399=CARTESIAN_POINT('Ctrl Pts',(-6.91679111096111,12.2,-7.7593689956284));
#282400=CARTESIAN_POINT('Ctrl Pts',(-6.91519965756486,12.2,-7.75792160234866));
#282401=CARTESIAN_POINT('Ctrl Pts',(-6.91365319364922,12.2,-7.75650690943966));
#282402=CARTESIAN_POINT('Ctrl Pts',(-6.91210672987404,12.2,-7.75509221665915));
#282403=CARTESIAN_POINT('Ctrl Pts',(-6.91060525482109,12.2,-7.75371022434943));
#282404=CARTESIAN_POINT('Ctrl Pts',(-6.90914902603396,12.2,-7.75236202747556));
#282405=CARTESIAN_POINT('Ctrl Pts',(-6.90672896680257,12.2,-7.75012150296511));
#282406=CARTESIAN_POINT('Ctrl Pts',(-6.90443386327613,12.2,-7.74797428786345));
#282407=CARTESIAN_POINT('Ctrl Pts',(-6.90226492000006,12.2,-7.74592563800002));
#282408=CARTESIAN_POINT('Ctrl Pts',(-6.90226492000006,15.2,-7.74592563800002));
#282409=CARTESIAN_POINT('Ctrl Pts',(-6.90356378046103,15.2,-7.7471524613731));
#282410=CARTESIAN_POINT('Ctrl Pts',(-6.90490788387611,15.2,-7.74841464066746));
#282411=CARTESIAN_POINT('Ctrl Pts',(-6.90629697189785,15.2,-7.74971102657464));
#282412=CARTESIAN_POINT('Ctrl Pts',(-6.90769275880418,15.2,-7.75101366430997));
#282413=CARTESIAN_POINT('Ctrl Pts',(-6.90913396276099,15.2,-7.75235084375419));
#282414=CARTESIAN_POINT('Ctrl Pts',(-6.91062032766887,15.2,-7.75372144989929));
#282415=CARTESIAN_POINT('Ctrl Pts',(-6.91210669244173,15.2,-7.7550920559199));
#282416=CARTESIAN_POINT('Ctrl Pts',(-6.9136382162239,15.2,-7.75649608786879));
#282417=CARTESIAN_POINT('Ctrl Pts',(-6.91521464499997,15.2,-7.75793246298329));
#282418=CARTESIAN_POINT('Ctrl Pts',(-6.91679107377605,15.2,-7.75936883809779));
#282419=CARTESIAN_POINT('Ctrl Pts',(-6.91841240636048,15.2,-7.76083755765297));
#282420=CARTESIAN_POINT('Ctrl Pts',(-6.9200783941306,15.2,-7.76233756883827));
#282421=CARTESIAN_POINT('Ctrl Pts',(-6.92174438205206,15.2,-7.76383758015982));
#282422=CARTESIAN_POINT('Ctrl Pts',(-6.92345502352597,15.2,-7.76536888232471));
#282423=CARTESIAN_POINT('Ctrl Pts',(-6.92521007345795,15.2,-7.76693045566184));
#282424=CARTESIAN_POINT('Ctrl Pts',(-6.92696512323052,15.2,-7.76849202885716));
#282425=CARTESIAN_POINT('Ctrl Pts',(-6.92876458116769,15.2,-7.77008387276886));
#282426=CARTESIAN_POINT('Ctrl Pts',(-6.93060820402582,15.2,-7.77170499321737));
#282427=CARTESIAN_POINT('Ctrl Pts',(-6.93245182688396,15.2,-7.77332611366589));
#282428=CARTESIAN_POINT('Ctrl Pts',(-6.93433961609195,15.2,-7.77497651296247));
#282429=CARTESIAN_POINT('Ctrl Pts',(-6.93627133093655,15.2,-7.77665522165026));
#282430=CARTESIAN_POINT('Ctrl Pts',(-6.9382030459566,15.2,-7.77833393049054));
#282431=CARTESIAN_POINT('Ctrl Pts',(-6.94017868920707,15.2,-7.78004095185096));
#282432=CARTESIAN_POINT('Ctrl Pts',(-6.94219802148676,15.2,-7.78177534369736));
#282433=CARTESIAN_POINT('Ctrl Pts',(-6.94421735358306,15.2,-7.78350973538623));
#282434=CARTESIAN_POINT('Ctrl Pts',(-6.94628037779796,15.2,-7.78527149973637));
#282435=CARTESIAN_POINT('Ctrl Pts',(-6.94838686063996,15.2,-7.7870597195892));
#282436=CARTESIAN_POINT('Ctrl Pts',(-6.95049334348198,15.2,-7.78884793944203));
#282437=CARTESIAN_POINT('Ctrl Pts',(-6.95264328442885,15.2,-7.79066261461775));
#282438=CARTESIAN_POINT('Ctrl Pts',(-6.9548364553473,15.2,-7.79250285638312));
#282439=CARTESIAN_POINT('Ctrl Pts',(-6.95702962626574,15.2,-7.79434309814849));
#282440=CARTESIAN_POINT('Ctrl Pts',(-6.9592660269873,15.2,-7.79620890371429));
#282441=CARTESIAN_POINT('Ctrl Pts',(-6.96154543173487,15.2,-7.79809940581058));
#282442=CARTESIAN_POINT('Ctrl Pts',(-6.96382483668951,15.2,-7.7999899080786));
#282443=CARTESIAN_POINT('Ctrl Pts',(-6.96614724335662,15.2,-7.80190510681569));
#282444=CARTESIAN_POINT('Ctrl Pts',(-6.96851243140407,15.2,-7.80384415508909));
#282445=CARTESIAN_POINT('Ctrl Pts',(-6.97087761923667,15.2,-7.80578320318635));
#282446=CARTESIAN_POINT('Ctrl Pts',(-6.97328558639354,15.2,-7.8077461019956));
#282447=CARTESIAN_POINT('Ctrl Pts',(-6.97573611148221,15.2,-7.80973202326574));
#282448=CARTESIAN_POINT('Ctrl Pts',(-6.97818663657087,15.2,-7.81171794453589));
#282449=CARTESIAN_POINT('Ctrl Pts',(-6.98067972228528,15.2,-7.81372688950389));
#282450=CARTESIAN_POINT('Ctrl Pts',(-6.9832151471903,15.2,-7.81575805176192));
#282451=CARTESIAN_POINT('Ctrl Pts',(-6.98575057232562,15.2,-7.81778921420446));
#282452=CARTESIAN_POINT('Ctrl Pts',(-6.98832833832333,15.2,-7.81984259528247));
#282453=CARTESIAN_POINT('Ctrl Pts',(-6.99094822838461,15.2,-7.82191740689648));
#282454=CARTESIAN_POINT('Ctrl Pts',(-6.99356811820792,15.2,-7.82399221832202));
#282455=CARTESIAN_POINT('Ctrl Pts',(-6.99623013164313,15.2,-7.82608846065803));
#282456=CARTESIAN_POINT('Ctrl Pts',(-6.99893405647376,15.2,-7.82820536700736));
#282457=CARTESIAN_POINT('Ctrl Pts',(-7.00163798130439,15.2,-7.83032227335668));
#282458=CARTESIAN_POINT('Ctrl Pts',(-7.00438381468365,15.2,-7.83245984109461));
#282459=CARTESIAN_POINT('Ctrl Pts',(-7.00717134841282,15.2,-7.83461732251482));
#282460=CARTESIAN_POINT('Ctrl Pts',(-7.00995888239519,15.2,-7.83677480413101));
#282461=CARTESIAN_POINT('Ctrl Pts',(-7.01278811455884,15.2,-7.83895219861528));
#282462=CARTESIAN_POINT('Ctrl Pts',(-7.01565883502779,15.2,-7.84114877167919));
#282463=CARTESIAN_POINT('Ctrl Pts',(-7.018529555236,15.2,-7.84334534454358));
#282464=CARTESIAN_POINT('Ctrl Pts',(-7.02144176517394,15.2,-7.84556109653948));
#282465=CARTESIAN_POINT('Ctrl Pts',(-7.02439525523331,15.2,-7.84779531304165));
#282466=CARTESIAN_POINT('Ctrl Pts',(-7.0273487452927,15.2,-7.85002952954382));
#282467=CARTESIAN_POINT('Ctrl Pts',(-7.03034351624243,15.2,-7.85228220670049));
#282468=CARTESIAN_POINT('Ctrl Pts',(-7.03337936319807,15.2,-7.85455264656372));
#282469=CARTESIAN_POINT('Ctrl Pts',(-7.03641521042948,15.2,-7.85682308663319));
#282470=CARTESIAN_POINT('Ctrl Pts',(-7.03949213200048,15.2,-7.85911128702447));
#282471=CARTESIAN_POINT('Ctrl Pts',(-7.04260992333984,15.2,-7.8614165649846));
#282472=CARTESIAN_POINT('Ctrl Pts',(-7.045727714396,15.2,-7.86372184273533));
#282473=CARTESIAN_POINT('Ctrl Pts',(-7.04888637774473,15.2,-7.86604419574202));
#282474=CARTESIAN_POINT('Ctrl Pts',(-7.05208570772644,15.2,-7.86838295450105));
#282475=CARTESIAN_POINT('Ctrl Pts',(-7.05528503770815,15.2,-7.87072171326007));
#282476=CARTESIAN_POINT('Ctrl Pts',(-7.05852503785898,15.2,-7.87307687564098));
#282477=CARTESIAN_POINT('Ctrl Pts',(-7.06180550207137,15.2,-7.87544778755417));
#282478=CARTESIAN_POINT('Ctrl Pts',(-7.06453922234769,15.2,-7.8774235475536));
#282479=CARTESIAN_POINT('Ctrl Pts',(-7.06730104553029,15.2,-7.87941024455887));
#282480=CARTESIAN_POINT('Ctrl Pts',(-7.0700908562927,15.2,-7.88140750462777));
#282481=CARTESIAN_POINT('Ctrl Pts',(-7.07288066705511,15.2,-7.88340476469665));
#282482=CARTESIAN_POINT('Ctrl Pts',(-7.07569846384115,15.2,-7.88541258855086));
#282483=CARTESIAN_POINT('Ctrl Pts',(-7.07854413225677,15.2,-7.88743061099056));
#282484=CARTESIAN_POINT('Ctrl Pts',(-7.0813898006724,15.2,-7.88944863343025));
#282485=CARTESIAN_POINT('Ctrl Pts',(-7.08426333932221,15.2,-7.89147685152221));
#282486=CARTESIAN_POINT('Ctrl Pts',(-7.08716463772498,15.2,-7.89351490825832));
#282487=CARTESIAN_POINT('Ctrl Pts',(-7.09006593612776,15.2,-7.89555296499443));
#282488=CARTESIAN_POINT('Ctrl Pts',(-7.0929949911381,15.2,-7.89760085926397));
#282489=CARTESIAN_POINT('Ctrl Pts',(-7.0959516905266,15.2,-7.89965823621778));
#282490=CARTESIAN_POINT('Ctrl Pts',(-7.0989083899151,15.2,-7.9017156131716));
#282491=CARTESIAN_POINT('Ctrl Pts',(-7.10189273333459,15.2,-7.90378247417979));
#282492=CARTESIAN_POINT('Ctrl Pts',(-7.10490460840547,15.2,-7.90585847015249));
#282493=CARTESIAN_POINT('Ctrl Pts',(-7.10791648347634,15.2,-7.90793446612519));
#282494=CARTESIAN_POINT('Ctrl Pts',(-7.11095589075484,15.2,-7.91001959731986));
#282495=CARTESIAN_POINT('Ctrl Pts',(-7.11402271520072,15.2,-7.91211352086199));
#282496=CARTESIAN_POINT('Ctrl Pts',(-7.1170895396466,15.2,-7.91420744440412));
#282497=CARTESIAN_POINT('Ctrl Pts',(-7.12018378327127,15.2,-7.9163101608446));
#282498=CARTESIAN_POINT('Ctrl Pts',(-7.12330533509578,15.2,-7.91842133372843));
#282499=CARTESIAN_POINT('Ctrl Pts',(-7.1264268869203,15.2,-7.92053250661227));
#282500=CARTESIAN_POINT('Ctrl Pts',(-7.12957574601321,15.2,-7.92265213501098));
#282501=CARTESIAN_POINT('Ctrl Pts',(-7.13275180039043,15.2,-7.92477988855331));
#282502=CARTESIAN_POINT('Ctrl Pts',(-7.13592785476766,15.2,-7.92690764209564));
#282503=CARTESIAN_POINT('Ctrl Pts',(-7.13913110641476,15.2,-7.92904352002977));
#282504=CARTESIAN_POINT('Ctrl Pts',(-7.14236144322252,15.2,-7.93118719628039));
#282505=CARTESIAN_POINT('Ctrl Pts',(-7.14559177967818,15.2,-7.93333087229737));
#282506=CARTESIAN_POINT('Ctrl Pts',(-7.14884920186948,15.2,-7.93548234663131));
#282507=CARTESIAN_POINT('Ctrl Pts',(-7.15213359907873,15.2,-7.93764129924261));
#282508=CARTESIAN_POINT('Ctrl Pts',(-7.15541799664599,15.2,-7.93980025208922));
#282509=CARTESIAN_POINT('Ctrl Pts',(-7.15872936978221,15.2,-7.94196668192182));
#282510=CARTESIAN_POINT('Ctrl Pts',(-7.16206760978002,15.2,-7.94414027324069));
#282511=CARTESIAN_POINT('Ctrl Pts',(-7.16540584977783,15.2,-7.94631386455955));
#282512=CARTESIAN_POINT('Ctrl Pts',(-7.1687709559585,15.2,-7.94849461763107));
#282513=CARTESIAN_POINT('Ctrl Pts',(-7.17216281783134,15.2,-7.95068222138053));
#282514=CARTESIAN_POINT('Ctrl Pts',(-7.17555467970418,15.2,-7.95286982512998));
#282515=CARTESIAN_POINT('Ctrl Pts',(-7.1789732998021,15.2,-7.95506427963502));
#282516=CARTESIAN_POINT('Ctrl Pts',(-7.18241856837514,15.2,-7.95726527849452));
#282517=CARTESIAN_POINT('Ctrl Pts',(-7.18586383694817,15.2,-7.95946627735403));
#282518=CARTESIAN_POINT('Ctrl Pts',(-7.18933575323386,15.2,-7.96167382010558));
#282519=CARTESIAN_POINT('Ctrl Pts',(-7.19283421003802,15.2,-7.96388760635526));
#282520=CARTESIAN_POINT('Ctrl Pts',(-7.19633266684219,15.2,-7.96610139260493));
#282521=CARTESIAN_POINT('Ctrl Pts',(-7.19985766398591,15.2,-7.96832142071588));
#282522=CARTESIAN_POINT('Ctrl Pts',(-7.20340909398455,15.2,-7.97054739460446));
#282523=CARTESIAN_POINT('Ctrl Pts',(-7.20625023813829,15.2,-7.97232817381238));
#282524=CARTESIAN_POINT('Ctrl Pts',(-7.20910829908769,15.2,-7.9741127577585));
#282525=CARTESIAN_POINT('Ctrl Pts',(-7.21198322216725,15.2,-7.97590099766784));
#282526=CARTESIAN_POINT('Ctrl Pts',(-7.2148581448551,15.2,-7.97768923733353));
#282527=CARTESIAN_POINT('Ctrl Pts',(-7.21774992864015,15.2,-7.97948113197249));
#282528=CARTESIAN_POINT('Ctrl Pts',(-7.22065852051237,15.2,-7.98127653360326));
#282529=CARTESIAN_POINT('Ctrl Pts',(-7.22356711278089,15.2,-7.98307193547865));
#282530=CARTESIAN_POINT('Ctrl Pts',(-7.22649251279589,15.2,-7.9848708442767));
#282531=CARTESIAN_POINT('Ctrl Pts',(-7.22943466495734,15.2,-7.9866731129307));
#282532=CARTESIAN_POINT('Ctrl Pts',(-7.23237681671792,15.2,-7.98847538133914));
#282533=CARTESIAN_POINT('Ctrl Pts',(-7.23533572015325,15.2,-7.99028101134255));
#282534=CARTESIAN_POINT('Ctrl Pts',(-7.23831132283497,15.2,-7.99208985522921));
#282535=CARTESIAN_POINT('Ctrl Pts',(-7.24203082649119,15.2,-7.99435091027237));
#282536=CARTESIAN_POINT('Ctrl Pts',(-7.24577642101596,15.2,-7.99661699101844));
#282537=CARTESIAN_POINT('Ctrl Pts',(-7.24954800032015,15.2,-7.99888781580985));
#282538=CARTESIAN_POINT('Ctrl Pts',(-7.25256526392795,15.2,-8.000704475742));
#282539=CARTESIAN_POINT('Ctrl Pts',(-7.25559915698775,15.2,-8.00252417225784));
#282540=CARTESIAN_POINT('Ctrl Pts',(-7.25864962726619,15.2,-8.00434676485736));
#282541=CARTESIAN_POINT('Ctrl Pts',(-7.26170009712902,15.2,-8.00616935720856));
#282542=CARTESIAN_POINT('Ctrl Pts',(-7.26476714392154,15.2,-8.00799484455141));
#282543=CARTESIAN_POINT('Ctrl Pts',(-7.26785071254431,15.2,-8.00982308899306));
#282544=CARTESIAN_POINT('Ctrl Pts',(-7.27093428158721,15.2,-8.01165133368381));
#282545=CARTESIAN_POINT('Ctrl Pts',(-7.27403437218955,15.2,-8.01348233304148));
#282546=CARTESIAN_POINT('Ctrl Pts',(-7.27715093247159,15.2,-8.0153159516416));
#282547=CARTESIAN_POINT('Ctrl Pts',(-7.28026749232901,15.2,-8.01714956999188));
#282548=CARTESIAN_POINT('Ctrl Pts',(-7.283400520347,15.2,-8.01898580619718));
#282549=CARTESIAN_POINT('Ctrl Pts',(-7.28654996347673,15.2,-8.02082452465771));
#282550=CARTESIAN_POINT('Ctrl Pts',(-7.28969940703557,15.2,-8.02266324336877));
#282551=CARTESIAN_POINT('Ctrl Pts',(-7.292865265517,15.2,-8.02450444388685));
#282552=CARTESIAN_POINT('Ctrl Pts',(-7.29604748576049,15.2,-8.02634799121793));
#282553=CARTESIAN_POINT('Ctrl Pts',(-7.29922970557041,15.2,-8.02819153829781));
#282554=CARTESIAN_POINT('Ctrl Pts',(-7.30242828572217,15.2,-8.03003743141303));
#282555=CARTESIAN_POINT('Ctrl Pts',(-7.3056431754577,15.2,-8.03188553920617));
#282556=CARTESIAN_POINT('Ctrl Pts',(-7.30885806563126,15.2,-8.03373364725113));
#282557=CARTESIAN_POINT('Ctrl Pts',(-7.31208926192854,15.2,-8.03558396869904));
#282558=CARTESIAN_POINT('Ctrl Pts',(-7.31533671421666,15.2,-8.03743637146668));
#282559=CARTESIAN_POINT('Ctrl Pts',(-7.31858416650477,15.2,-8.03928877423431));
#282560=CARTESIAN_POINT('Ctrl Pts',(-7.3218478750642,15.2,-8.04114325924939));
#282561=CARTESIAN_POINT('Ctrl Pts',(-7.32512778407793,15.2,-8.0429996952952));
#282562=CARTESIAN_POINT('Ctrl Pts',(-7.32840769264477,15.2,-8.04485613108806));
#282563=CARTESIAN_POINT('Ctrl Pts',(-7.33170380280908,15.2,-8.04671451783959));
#282564=CARTESIAN_POINT('Ctrl Pts',(-7.33501606199774,15.2,-8.04857472697374));
#282565=CARTESIAN_POINT('Ctrl Pts',(-7.3383283216377,15.2,-8.05043493636135));
#282566=CARTESIAN_POINT('Ctrl Pts',(-7.34165673003512,15.2,-8.05229696774187));
#282567=CARTESIAN_POINT('Ctrl Pts',(-7.34500123433016,15.2,-8.05416069328806));
#282568=CARTESIAN_POINT('Ctrl Pts',(-7.34834573816952,15.2,-8.05602441858032));
#282569=CARTESIAN_POINT('Ctrl Pts',(-7.35170633762062,15.2,-8.05788983861401));
#282570=CARTESIAN_POINT('Ctrl Pts',(-7.35508298073244,15.2,-8.0597568270724));
#282571=CARTESIAN_POINT('Ctrl Pts',(-7.35845962430432,15.2,-8.06162381578516));
#282572=CARTESIAN_POINT('Ctrl Pts',(-7.36185231054002,15.2,-8.06349237199257));
#282573=CARTESIAN_POINT('Ctrl Pts',(-7.36526098828637,15.2,-8.06536237218803));
#282574=CARTESIAN_POINT('Ctrl Pts',(-7.36866966556828,15.2,-8.06723237212871));
#282575=CARTESIAN_POINT('Ctrl Pts',(-7.37209433201785,15.2,-8.06910381485011));
#282576=CARTESIAN_POINT('Ctrl Pts',(-7.37553493773554,15.2,-8.07097657736359));
#282577=CARTESIAN_POINT('Ctrl Pts',(-7.37897554392202,15.2,-8.07284934013224));
#282578=CARTESIAN_POINT('Ctrl Pts',(-7.38243208706319,15.2,-8.07472342313161));
#282579=CARTESIAN_POINT('Ctrl Pts',(-7.38590451730901,15.2,-8.07659870217832));
#282580=CARTESIAN_POINT('Ctrl Pts',(-7.38937694708172,15.2,-8.07847398096954));
#282581=CARTESIAN_POINT('Ctrl Pts',(-7.39286526071272,15.2,-8.08035045800401));
#282582=CARTESIAN_POINT('Ctrl Pts',(-7.39636940876661,15.2,-8.08222801127757));
#282583=CARTESIAN_POINT('Ctrl Pts',(-7.39987355729795,15.2,-8.08410556480694));
#282584=CARTESIAN_POINT('Ctrl Pts',(-7.4033935392149,15.2,-8.0859841941234));
#282585=CARTESIAN_POINT('Ctrl Pts',(-7.40692930279752,15.2,-8.08786377967034));
#282586=CARTESIAN_POINT('Ctrl Pts',(-7.41046506589838,15.2,-8.08974336496119));
#282587=CARTESIAN_POINT('Ctrl Pts',(-7.41401661033778,15.2,-8.0916239070713));
#282588=CARTESIAN_POINT('Ctrl Pts',(-7.41758388293342,15.2,-8.09350528641741));
#282589=CARTESIAN_POINT('Ctrl Pts',(-7.42115115601511,15.2,-8.09538666601985));
#282590=CARTESIAN_POINT('Ctrl Pts',(-7.42473415948997,15.2,-8.09726888440849));
#282591=CARTESIAN_POINT('Ctrl Pts',(-7.42833283974166,15.2,-8.09915182273335));
#282592=CARTESIAN_POINT('Ctrl Pts',(-7.43193151999336,15.2,-8.1010347610582));
#282593=CARTESIAN_POINT('Ctrl Pts',(-7.4355458758802,15.2,-8.10291842034701));
#282594=CARTESIAN_POINT('Ctrl Pts',(-7.43917585880184,15.2,-8.10480268328309));
#282595=CARTESIAN_POINT('Ctrl Pts',(-7.4428058412289,15.2,-8.10668694596244));
#282596=CARTESIAN_POINT('Ctrl Pts',(-7.44645144939133,15.2,-8.10857181374707));
#282597=CARTESIAN_POINT('Ctrl Pts',(-7.45011262999751,15.2,-8.1104571709904));
#282598=CARTESIAN_POINT('Ctrl Pts',(-7.45377381110251,15.2,-8.1123425284906));
#282599=CARTESIAN_POINT('Ctrl Pts',(-7.45745056659253,15.2,-8.11422837511668));
#282600=CARTESIAN_POINT('Ctrl Pts',(-7.46114284362869,15.2,-8.11611459677508));
#282601=CARTESIAN_POINT('Ctrl Pts',(-7.46483512016178,15.2,-8.11800081817648));
#282602=CARTESIAN_POINT('Ctrl Pts',(-7.46854291870671,15.2,-8.11988741574448));
#282603=CARTESIAN_POINT('Ctrl Pts',(-7.4722661871791,15.2,-8.12177427581243));
#282604=CARTESIAN_POINT('Ctrl Pts',(-7.4759894561588,15.2,-8.12366113613748));
#282605=CARTESIAN_POINT('Ctrl Pts',(-7.47972819549303,15.2,-8.1255482602684));
#282606=CARTESIAN_POINT('Ctrl Pts',(-7.48348235405317,15.2,-8.12743553529887));
#282607=CARTESIAN_POINT('Ctrl Pts',(-7.48723651210181,15.2,-8.12932281007221));
#282608=CARTESIAN_POINT('Ctrl Pts',(-7.49100608902614,15.2,-8.13121023609446));
#282609=CARTESIAN_POINT('Ctrl Pts',(-7.49479103288239,15.2,-8.13309770282905));
#282610=CARTESIAN_POINT('Ctrl Pts',(-7.49857597725434,15.2,-8.1349851698208));
#282611=CARTESIAN_POINT('Ctrl Pts',(-7.50237629019201,15.2,-8.13687267729312));
#282612=CARTESIAN_POINT('Ctrl Pts',(-7.50619191851206,15.2,-8.13876011689598));
#282613=CARTESIAN_POINT('Ctrl Pts',(-7.51000754631224,15.2,-8.14064755624167));
#282614=CARTESIAN_POINT('Ctrl Pts',(-7.51383848990446,15.2,-8.14253492761949));
#282615=CARTESIAN_POINT('Ctrl Pts',(-7.5176846992253,15.2,-8.14442212122617));
#282616=CARTESIAN_POINT('Ctrl Pts',(-7.52153090907019,15.2,-8.14630931508999));
#282617=CARTESIAN_POINT('Ctrl Pts',(-7.52539238303256,15.2,-8.148196332657));
#282618=CARTESIAN_POINT('Ctrl Pts',(-7.5292690708004,15.2,-8.15008306687093));
#282619=CARTESIAN_POINT('Ctrl Pts',(-7.53314575804004,15.2,-8.15196980082778));
#282620=CARTESIAN_POINT('Ctrl Pts',(-7.53703766095438,15.2,-8.15385625034579));
#282621=CARTESIAN_POINT('Ctrl Pts',(-7.5409447254112,15.2,-8.15574230919165));
#282622=CARTESIAN_POINT('Ctrl Pts',(-7.54485179040036,15.2,-8.15762836829447));
#282623=CARTESIAN_POINT('Ctrl Pts',(-7.54877401763127,15.2,-8.15951403878722));
#282624=CARTESIAN_POINT('Ctrl Pts',(-7.55271135675268,15.2,-8.16139921250964));
#282625=CARTESIAN_POINT('Ctrl Pts',(-7.55664869533762,15.2,-8.16328438597519));
#282626=CARTESIAN_POINT('Ctrl Pts',(-7.56060114712165,15.2,-8.16516906444316));
#282627=CARTESIAN_POINT('Ctrl Pts',(-7.56456865835132,15.2,-8.16705314323364));
#282628=CARTESIAN_POINT('Ctrl Pts',(-7.56853617012155,15.2,-8.16893722228082));
#282629=CARTESIAN_POINT('Ctrl Pts',(-7.57251874414324,15.2,-8.17082070146963));
#282630=CARTESIAN_POINT('Ctrl Pts',(-7.57651632724999,15.2,-8.17270347901669));
#282631=CARTESIAN_POINT('Ctrl Pts',(-7.5815133058611,15.2,-8.17505695082224));
#282632=CARTESIAN_POINT('Ctrl Pts',(-7.58653373882422,15.2,-8.17740932297951));
#282633=CARTESIAN_POINT('Ctrl Pts',(-7.59157752502775,15.2,-8.1797603984763));
#282634=CARTESIAN_POINT('Ctrl Pts',(-7.59460379663991,15.2,-8.18117104372312));
#282635=CARTESIAN_POINT('Ctrl Pts',(-7.59763847642735,15.2,-8.18258122316021));
#282636=CARTESIAN_POINT('Ctrl Pts',(-7.60068154195557,15.2,-8.18399089144874));
#282637=CARTESIAN_POINT('Ctrl Pts',(-7.60372460748379,15.2,-8.18540055973726));
#282638=CARTESIAN_POINT('Ctrl Pts',(-7.60677605917854,15.2,-8.18680971968094));
#282639=CARTESIAN_POINT('Ctrl Pts',(-7.60983587569162,15.2,-8.18821832683814));
#282640=CARTESIAN_POINT('Ctrl Pts',(-7.6128956922047,15.2,-8.18962693399533));
#282641=CARTESIAN_POINT('Ctrl Pts',(-7.61596387372557,15.2,-8.19103498854425));
#282642=CARTESIAN_POINT('Ctrl Pts',(-7.61904039827933,15.2,-8.19244244970152));
#282643=CARTESIAN_POINT('Ctrl Pts',(-7.62211692339197,15.2,-8.19384991111449));
#282644=CARTESIAN_POINT('Ctrl Pts',(-7.62520179237365,15.2,-8.19525677853563));
#282645=CARTESIAN_POINT('Ctrl Pts',(-7.62829498390766,15.2,-8.19666300953158));
#282646=CARTESIAN_POINT('Ctrl Pts',(-7.63138817487973,15.2,-8.19806924027206));
#282647=CARTESIAN_POINT('Ctrl Pts',(-7.63448968784177,15.2,-8.19947483601944));
#282648=CARTESIAN_POINT('Ctrl Pts',(-7.63759950155175,15.2,-8.2008797542885));
#282649=CARTESIAN_POINT('Ctrl Pts',(-7.64070931526173,15.2,-8.20228467255755));
#282650=CARTESIAN_POINT('Ctrl Pts',(-7.64382743082045,15.2,-8.20368891358738));
#282651=CARTESIAN_POINT('Ctrl Pts',(-7.64695382533258,15.2,-8.20509243541132));
#282652=CARTESIAN_POINT('Ctrl Pts',(-7.65008021984471,15.2,-8.20649595723526));
#282653=CARTESIAN_POINT('Ctrl Pts',(-7.65321489374752,15.2,-8.20789876165096));
#282654=CARTESIAN_POINT('Ctrl Pts',(-7.65635782671666,15.2,-8.20930080593335));
#282655=CARTESIAN_POINT('Ctrl Pts',(-7.6595007596858,15.2,-8.21070285021575));
#282656=CARTESIAN_POINT('Ctrl Pts',(-7.66265195113792,15.2,-8.21210413616483));
#282657=CARTESIAN_POINT('Ctrl Pts',(-7.66581137964743,15.2,-8.21350462136402));
#282658=CARTESIAN_POINT('Ctrl Pts',(-7.66897080815692,15.2,-8.21490510656321));
#282659=CARTESIAN_POINT('Ctrl Pts',(-7.67213847447665,15.2,-8.21630479169355));
#282660=CARTESIAN_POINT('Ctrl Pts',(-7.67531435664396,15.2,-8.21770363650437));
#282661=CARTESIAN_POINT('Ctrl Pts',(-7.67849023881125,15.2,-8.21910248131519));
#282662=CARTESIAN_POINT('Ctrl Pts',(-7.68167433725452,15.2,-8.22050048596276));
#282663=CARTESIAN_POINT('Ctrl Pts',(-7.68486662984576,15.2,-8.22189761016211));
#282664=CARTESIAN_POINT('Ctrl Pts',(-7.68805892301693,15.2,-8.22329473461529));
#282665=CARTESIAN_POINT('Ctrl Pts',(-7.69125941179872,15.2,-8.22469097810154));
#282666=CARTESIAN_POINT('Ctrl Pts',(-7.69446807439117,15.2,-8.2260863020542));
#282667=CARTESIAN_POINT('Ctrl Pts',(-7.69767673640071,15.2,-8.22748162575338));
#282668=CARTESIAN_POINT('Ctrl Pts',(-7.70089357186813,15.2,-8.2288760301526));
#282669=CARTESIAN_POINT('Ctrl Pts',(-7.70411856033499,15.2,-8.23026947393523));
#282670=CARTESIAN_POINT('Ctrl Pts',(-7.70734354880185,15.2,-8.23166291771784));
#282671=CARTESIAN_POINT('Ctrl Pts',(-7.71057669030596,15.2,-8.23305540169553));
#282672=CARTESIAN_POINT('Ctrl Pts',(-7.71381796324461,15.2,-8.23444688694295));
#282673=CARTESIAN_POINT('Ctrl Pts',(-7.71705923618327,15.2,-8.23583837219038));
#282674=CARTESIAN_POINT('Ctrl Pts',(-7.7203086398173,15.2,-8.23722885852626));
#282675=CARTESIAN_POINT('Ctrl Pts',(-7.72356615475538,15.2,-8.23861830723209));
#282676=CARTESIAN_POINT('Ctrl Pts',(-7.72682366969345,15.2,-8.24000775593793));
#282677=CARTESIAN_POINT('Ctrl Pts',(-7.73008929492962,15.2,-8.2413961673491));
#282678=CARTESIAN_POINT('Ctrl Pts',(-7.7333630098933,15.2,-8.24278350113212));
#282679=CARTESIAN_POINT('Ctrl Pts',(-7.73663672485699,15.2,-8.24417083491514));
#282680=CARTESIAN_POINT('Ctrl Pts',(-7.73991852930344,15.2,-8.24555709223157));
#282681=CARTESIAN_POINT('Ctrl Pts',(-7.74320840180781,15.2,-8.2469422349314));
#282682=CARTESIAN_POINT('Ctrl Pts',(-7.74649827490985,15.2,-8.24832737788286));
#282683=CARTESIAN_POINT('Ctrl Pts',(-7.74979621608915,15.2,-8.249711404834));
#282684=CARTESIAN_POINT('Ctrl Pts',(-7.75310220519572,15.2,-8.25109427928482));
#282685=CARTESIAN_POINT('Ctrl Pts',(-7.7564081937017,15.2,-8.25247715348442));
#282686=CARTESIAN_POINT('Ctrl Pts',(-7.75972222986558,15.2,-8.25385887468408));
#282687=CARTESIAN_POINT('Ctrl Pts',(-7.76304429232891,15.2,-8.25523940442548));
#282688=CARTESIAN_POINT('Ctrl Pts',(-7.76636635479223,15.2,-8.25661993416688));
#282689=CARTESIAN_POINT('Ctrl Pts',(-7.76969644324246,15.2,-8.25799927246176));
#282690=CARTESIAN_POINT('Ctrl Pts',(-7.77303453726137,15.2,-8.25937738225128));
#282691=CARTESIAN_POINT('Ctrl Pts',(-7.77637263128028,15.2,-8.26075549204079));
#282692=CARTESIAN_POINT('Ctrl Pts',(-7.77971873168696,15.2,-8.26213237365917));
#282693=CARTESIAN_POINT('Ctrl Pts',(-7.78307281574696,15.2,-8.26350798799044));
#282694=CARTESIAN_POINT('Ctrl Pts',(-7.78642689980696,15.2,-8.26488360232171));
#282695=CARTESIAN_POINT('Ctrl Pts',(-7.7897889688726,15.2,-8.26625795105011));
#282696=CARTESIAN_POINT('Ctrl Pts',(-7.79315900087447,15.2,-8.26763099537534));
#282697=CARTESIAN_POINT('Ctrl Pts',(-7.79652903287633,15.2,-8.26900403970057));
#282698=CARTESIAN_POINT('Ctrl Pts',(-7.79990702778598,15.2,-8.27037578065088));
#282699=CARTESIAN_POINT('Ctrl Pts',(-7.80329296624521,15.2,-8.27174618143461));
#282700=CARTESIAN_POINT('Ctrl Pts',(-7.80667890531956,15.2,-8.2731165824673));
#282701=CARTESIAN_POINT('Ctrl Pts',(-7.81007278709614,15.2,-8.27448564326627));
#282702=CARTESIAN_POINT('Ctrl Pts',(-7.8134745902166,15.2,-8.27585332679818));
#282703=CARTESIAN_POINT('Ctrl Pts',(-7.81687639271907,15.2,-8.27722101008163));
#282704=CARTESIAN_POINT('Ctrl Pts',(-7.82028611704716,15.2,-8.27858731639565));
#282705=CARTESIAN_POINT('Ctrl Pts',(-7.82370374263631,15.2,-8.27995220874742));
#282706=CARTESIAN_POINT('Ctrl Pts',(-7.82712136822545,15.2,-8.28131710109918));
#282707=CARTESIAN_POINT('Ctrl Pts',(-7.83054689374844,15.2,-8.28268057986474));
#282708=CARTESIAN_POINT('Ctrl Pts',(-7.83398029962438,15.2,-8.28404260819013));
#282709=CARTESIAN_POINT('Ctrl Pts',(-7.83741370550031,15.2,-8.28540463651551));
#282710=CARTESIAN_POINT('Ctrl Pts',(-7.8408549901753,15.2,-8.28676521536607));
#282711=CARTESIAN_POINT('Ctrl Pts',(-7.84430413555,15.2,-8.28812430827503));
#282712=CARTESIAN_POINT('Ctrl Pts',(-7.8477532809247,15.2,-8.28948340118399));
#282713=CARTESIAN_POINT('Ctrl Pts',(-7.85121028493238,15.2,-8.29084100993467));
#282714=CARTESIAN_POINT('Ctrl Pts',(-7.85467512788913,15.2,-8.29219709634385));
#282715=CARTESIAN_POINT('Ctrl Pts',(-7.85813997084589,15.2,-8.29355318275304));
#282716=CARTESIAN_POINT('Ctrl Pts',(-7.8616126521135,15.2,-8.29490774905296));
#282717=CARTESIAN_POINT('Ctrl Pts',(-7.86509314986836,15.2,-8.29626075598824));
#282718=CARTESIAN_POINT('Ctrl Pts',(-7.86857364762321,15.2,-8.29761376292352));
#282719=CARTESIAN_POINT('Ctrl Pts',(-7.87206196289928,15.2,-8.29896521160459));
#282720=CARTESIAN_POINT('Ctrl Pts',(-7.87555807393786,15.2,-8.30031506743076));
#282721=CARTESIAN_POINT('Ctrl Pts',(-7.87905418561156,15.2,-8.30166492350216));
#282722=CARTESIAN_POINT('Ctrl Pts',(-7.88255809365415,15.2,-8.30301318591478));
#282723=CARTESIAN_POINT('Ctrl Pts',(-7.88606977879056,15.2,-8.30435982398526));
#282724=CARTESIAN_POINT('Ctrl Pts',(-7.88958146328901,15.2,-8.30570646181111));
#282725=CARTESIAN_POINT('Ctrl Pts',(-7.89310092559542,15.2,-8.30705147627872));
#282726=CARTESIAN_POINT('Ctrl Pts',(-7.8966281448846,15.2,-8.30839482993809));
#282727=CARTESIAN_POINT('Ctrl Pts',(-7.90015536417378,15.2,-8.30973818359747));
#282728=CARTESIAN_POINT('Ctrl Pts',(-7.90369033743249,15.2,-8.31107987547719));
#282729=CARTESIAN_POINT('Ctrl Pts',(-7.90723304227822,15.2,-8.31241986322624));
#282730=CARTESIAN_POINT('Ctrl Pts',(-7.91077574712395,15.2,-8.31375985097529));
#282731=CARTESIAN_POINT('Ctrl Pts',(-7.91432618135994,15.2,-8.31509813342464));
#282732=CARTESIAN_POINT('Ctrl Pts',(-7.91788432603843,15.2,-8.31643468000715));
#282733=CARTESIAN_POINT('Ctrl Pts',(-7.92381456738474,15.2,-8.31866225772561));
#282734=CARTESIAN_POINT('Ctrl Pts',(-7.92976622247684,15.2,-8.32088501090861));
#282735=CARTESIAN_POINT('Ctrl Pts',(-7.93573928312123,15.2,-8.32310290867369));
#282736=CARTESIAN_POINT('Origin',(-5.66257110645729E-14,15.2,-1.77635683940025E-14));
#282737=CARTESIAN_POINT('',(-6.57080831900006,15.2,-8.02901631800001));
#282738=CARTESIAN_POINT('',(-6.57080831900006,12.2,-8.02901631800001));
#282739=CARTESIAN_POINT('',(-6.57080831900006,15.2,-8.02901631800001));
#282740=CARTESIAN_POINT('Origin',(-5.66257110645729E-14,12.2,-1.77635683940025E-14));
#282741=CARTESIAN_POINT('Origin',(-5.66257110645729E-14,15.2,-1.77635683940025E-14));
#282742=CARTESIAN_POINT('Origin',(-5.66257110645729E-14,15.2,-1.77635683940025E-14));
#282743=CARTESIAN_POINT('',(-6.97920857100006,15.2,-9.14005731500002));
#282744=CARTESIAN_POINT('',(-6.67046385600006,15.2,-9.36775917400002));
#282745=CARTESIAN_POINT('Origin',(-5.66257110645729E-14,15.2,-1.77635683940025E-14));
#282746=CARTESIAN_POINT('',(-6.67046385600006,12.2,-9.36775917400002));
#282747=CARTESIAN_POINT('',(-6.67046385600006,15.2,-9.36775917400002));
#282748=CARTESIAN_POINT('',(-6.97920857100006,12.2,-9.14005731500002));
#282749=CARTESIAN_POINT('Origin',(-5.66257110645729E-14,12.2,-1.77635683940025E-14));
#282750=CARTESIAN_POINT('',(-6.97920857100006,15.2,-9.14005731500002));
#282751=CARTESIAN_POINT('Ctrl Pts',(-6.67046385600006,15.2,-9.36775917400002));
#282752=CARTESIAN_POINT('Ctrl Pts',(-6.67046385600006,11.6,-9.36775917400002));
#282753=CARTESIAN_POINT('Ctrl Pts',(-6.66979226100006,15.2,-9.36739373000002));
#282754=CARTESIAN_POINT('Ctrl Pts',(-6.66979226100006,11.6,-9.36739373000002));
#282755=CARTESIAN_POINT('Ctrl Pts',(-6.66844959800006,15.2,-9.36666279600002));
#282756=CARTESIAN_POINT('Ctrl Pts',(-6.66844959800006,11.6,-9.36666279600002));
#282757=CARTESIAN_POINT('Ctrl Pts',(-6.66643717700006,15.2,-9.36556627000002));
#282758=CARTESIAN_POINT('Ctrl Pts',(-6.66643717700006,11.6,-9.36556627000002));
#282759=CARTESIAN_POINT('Ctrl Pts',(-6.66375709900006,15.2,-9.36410398400002));
#282760=CARTESIAN_POINT('Ctrl Pts',(-6.66375709900006,11.6,-9.36410398400002));
#282761=CARTESIAN_POINT('Ctrl Pts',(-6.66041225200006,15.2,-9.36227570600002));
#282762=CARTESIAN_POINT('Ctrl Pts',(-6.66041225200006,11.6,-9.36227570600002));
#282763=CARTESIAN_POINT('Ctrl Pts',(-6.65707265500005,15.2,-9.36044701000002));
#282764=CARTESIAN_POINT('Ctrl Pts',(-6.65707265500005,11.6,-9.36044701000002));
#282765=CARTESIAN_POINT('Ctrl Pts',(-6.65373831000006,15.2,-9.35861789600001));
#282766=CARTESIAN_POINT('Ctrl Pts',(-6.65373831000006,11.6,-9.35861789600001));
#282767=CARTESIAN_POINT('Ctrl Pts',(-6.65040921900006,15.2,-9.35678837000001));
#282768=CARTESIAN_POINT('Ctrl Pts',(-6.65040921900006,11.6,-9.35678837000001));
#282769=CARTESIAN_POINT('Ctrl Pts',(-6.64708538300006,15.2,-9.35495843700001));
#282770=CARTESIAN_POINT('Ctrl Pts',(-6.64708538300006,11.6,-9.35495843700001));
#282771=CARTESIAN_POINT('Ctrl Pts',(-6.64376680700006,15.2,-9.35312810300001));
#282772=CARTESIAN_POINT('Ctrl Pts',(-6.64376680700006,11.6,-9.35312810300001));
#282773=CARTESIAN_POINT('Ctrl Pts',(-6.64045349300006,15.2,-9.35129737900001));
#282774=CARTESIAN_POINT('Ctrl Pts',(-6.64045349300006,11.6,-9.35129737900001));
#282775=CARTESIAN_POINT('Ctrl Pts',(-6.63714544700006,15.2,-9.34946627300001));
#282776=CARTESIAN_POINT('Ctrl Pts',(-6.63714544700006,11.6,-9.34946627300001));
#282777=CARTESIAN_POINT('Ctrl Pts',(-6.63384267100006,15.2,-9.34763479700001));
#282778=CARTESIAN_POINT('Ctrl Pts',(-6.63384267100006,11.6,-9.34763479700001));
#282779=CARTESIAN_POINT('Ctrl Pts',(-6.63054517000006,15.2,-9.34580296000001));
#282780=CARTESIAN_POINT('Ctrl Pts',(-6.63054517000006,11.6,-9.34580296000001));
#282781=CARTESIAN_POINT('Ctrl Pts',(-6.62725294900006,15.2,-9.34397077300002));
#282782=CARTESIAN_POINT('Ctrl Pts',(-6.62725294900006,11.6,-9.34397077300002));
#282783=CARTESIAN_POINT('Ctrl Pts',(-6.62396601100006,15.2,-9.34213824300001));
#282784=CARTESIAN_POINT('Ctrl Pts',(-6.62396601100006,11.6,-9.34213824300001));
#282785=CARTESIAN_POINT('Ctrl Pts',(-6.62068436000006,15.2,-9.34030538000002));
#282786=CARTESIAN_POINT('Ctrl Pts',(-6.62068436000006,11.6,-9.34030538000002));
#282787=CARTESIAN_POINT('Ctrl Pts',(-6.61740799800006,15.2,-9.33847218900001));
#282788=CARTESIAN_POINT('Ctrl Pts',(-6.61740799800006,11.6,-9.33847218900001));
#282789=CARTESIAN_POINT('Ctrl Pts',(-6.61413692800005,15.2,-9.33663868000002));
#282790=CARTESIAN_POINT('Ctrl Pts',(-6.61413692800005,11.6,-9.33663868000002));
#282791=CARTESIAN_POINT('Ctrl Pts',(-6.61087115500006,15.2,-9.33480485900001));
#282792=CARTESIAN_POINT('Ctrl Pts',(-6.61087115500006,11.6,-9.33480485900001));
#282793=CARTESIAN_POINT('Ctrl Pts',(-6.60761068100006,15.2,-9.33297073500002));
#282794=CARTESIAN_POINT('Ctrl Pts',(-6.60761068100006,11.6,-9.33297073500002));
#282795=CARTESIAN_POINT('Ctrl Pts',(-6.60435550800006,15.2,-9.33113631500002));
#282796=CARTESIAN_POINT('Ctrl Pts',(-6.60435550800006,11.6,-9.33113631500002));
#282797=CARTESIAN_POINT('Ctrl Pts',(-6.60110564300005,15.2,-9.32930161000002));
#282798=CARTESIAN_POINT('Ctrl Pts',(-6.60110564300005,11.6,-9.32930161000002));
#282799=CARTESIAN_POINT('Ctrl Pts',(-6.59786108600006,15.2,-9.32746662500002));
#282800=CARTESIAN_POINT('Ctrl Pts',(-6.59786108600006,11.6,-9.32746662500002));
#282801=CARTESIAN_POINT('Ctrl Pts',(-6.59462184300006,15.2,-9.32563137200002));
#282802=CARTESIAN_POINT('Ctrl Pts',(-6.59462184300006,11.6,-9.32563137200002));
#282803=CARTESIAN_POINT('Ctrl Pts',(-6.59138791700006,15.2,-9.32379585900001));
#282804=CARTESIAN_POINT('Ctrl Pts',(-6.59138791700006,11.6,-9.32379585900001));
#282805=CARTESIAN_POINT('Ctrl Pts',(-6.58815931000006,15.2,-9.32196009500002));
#282806=CARTESIAN_POINT('Ctrl Pts',(-6.58815931000006,11.6,-9.32196009500002));
#282807=CARTESIAN_POINT('Ctrl Pts',(-6.58493602700006,15.2,-9.32012408600002));
#282808=CARTESIAN_POINT('Ctrl Pts',(-6.58493602700006,11.6,-9.32012408600002));
#282809=CARTESIAN_POINT('Ctrl Pts',(-6.58171807300006,15.2,-9.31828784500001));
#282810=CARTESIAN_POINT('Ctrl Pts',(-6.58171807300006,11.6,-9.31828784500001));
#282811=CARTESIAN_POINT('Ctrl Pts',(-6.57850544800006,15.2,-9.31645137700002));
#282812=CARTESIAN_POINT('Ctrl Pts',(-6.57850544800006,11.6,-9.31645137700002));
#282813=CARTESIAN_POINT('Ctrl Pts',(-6.57529815700006,15.2,-9.31461469100002));
#282814=CARTESIAN_POINT('Ctrl Pts',(-6.57529815700006,11.6,-9.31461469100002));
#282815=CARTESIAN_POINT('Ctrl Pts',(-6.57209620400006,15.2,-9.31277779500002));
#282816=CARTESIAN_POINT('Ctrl Pts',(-6.57209620400006,11.6,-9.31277779500002));
#282817=CARTESIAN_POINT('Ctrl Pts',(-6.56889959100006,15.2,-9.31094070000002));
#282818=CARTESIAN_POINT('Ctrl Pts',(-6.56889959100006,11.6,-9.31094070000002));
#282819=CARTESIAN_POINT('Ctrl Pts',(-6.56570832300006,15.2,-9.30910341200001));
#282820=CARTESIAN_POINT('Ctrl Pts',(-6.56570832300006,11.6,-9.30910341200001));
#282821=CARTESIAN_POINT('Ctrl Pts',(-6.56252240200006,15.2,-9.30726594200002));
#282822=CARTESIAN_POINT('Ctrl Pts',(-6.56252240200006,11.6,-9.30726594200002));
#282823=CARTESIAN_POINT('Ctrl Pts',(-6.55934183200006,15.2,-9.30542829500002));
#282824=CARTESIAN_POINT('Ctrl Pts',(-6.55934183200006,11.6,-9.30542829500002));
#282825=CARTESIAN_POINT('Ctrl Pts',(-6.55616661700006,15.2,-9.30359048400001));
#282826=CARTESIAN_POINT('Ctrl Pts',(-6.55616661700006,11.6,-9.30359048400001));
#282827=CARTESIAN_POINT('Ctrl Pts',(-6.55299676000006,15.2,-9.30175251500001));
#282828=CARTESIAN_POINT('Ctrl Pts',(-6.55299676000006,11.6,-9.30175251500001));
#282829=CARTESIAN_POINT('Ctrl Pts',(-6.54983226500006,15.2,-9.29991439900002));
#282830=CARTESIAN_POINT('Ctrl Pts',(-6.54983226500006,11.6,-9.29991439900002));
#282831=CARTESIAN_POINT('Ctrl Pts',(-6.54667313400005,15.2,-9.29807614200002));
#282832=CARTESIAN_POINT('Ctrl Pts',(-6.54667313400005,11.6,-9.29807614200002));
#282833=CARTESIAN_POINT('Ctrl Pts',(-6.54351937200006,15.2,-9.29623775500002));
#282834=CARTESIAN_POINT('Ctrl Pts',(-6.54351937200006,11.6,-9.29623775500002));
#282835=CARTESIAN_POINT('Ctrl Pts',(-6.54037098100006,15.2,-9.29439924500001));
#282836=CARTESIAN_POINT('Ctrl Pts',(-6.54037098100006,11.6,-9.29439924500001));
#282837=CARTESIAN_POINT('Ctrl Pts',(-6.53722796600006,15.2,-9.29256062200002));
#282838=CARTESIAN_POINT('Ctrl Pts',(-6.53722796600006,11.6,-9.29256062200002));
#282839=CARTESIAN_POINT('Ctrl Pts',(-6.53409033000006,15.2,-9.29072189400001));
#282840=CARTESIAN_POINT('Ctrl Pts',(-6.53409033000006,11.6,-9.29072189400001));
#282841=CARTESIAN_POINT('Ctrl Pts',(-6.53095807500006,15.2,-9.28888307000001));
#282842=CARTESIAN_POINT('Ctrl Pts',(-6.53095807500006,11.6,-9.28888307000001));
#282843=CARTESIAN_POINT('Ctrl Pts',(-6.52783120600006,15.2,-9.28704416000001));
#282844=CARTESIAN_POINT('Ctrl Pts',(-6.52783120600006,11.6,-9.28704416000001));
#282845=CARTESIAN_POINT('Ctrl Pts',(-6.52470972700006,15.2,-9.28520517200001));
#282846=CARTESIAN_POINT('Ctrl Pts',(-6.52470972700006,11.6,-9.28520517200001));
#282847=CARTESIAN_POINT('Ctrl Pts',(-6.52159363900005,15.2,-9.28336611300002));
#282848=CARTESIAN_POINT('Ctrl Pts',(-6.52159363900005,11.6,-9.28336611300002));
#282849=CARTESIAN_POINT('Ctrl Pts',(-6.51848294800006,15.2,-9.28152699600002));
#282850=CARTESIAN_POINT('Ctrl Pts',(-6.51848294800006,11.6,-9.28152699600002));
#282851=CARTESIAN_POINT('Ctrl Pts',(-6.51537765500006,15.2,-9.27968782700002));
#282852=CARTESIAN_POINT('Ctrl Pts',(-6.51537765500006,11.6,-9.27968782700002));
#282853=CARTESIAN_POINT('Ctrl Pts',(-6.51227776500006,15.2,-9.27784861500001));
#282854=CARTESIAN_POINT('Ctrl Pts',(-6.51227776500006,11.6,-9.27784861500001));
#282855=CARTESIAN_POINT('Ctrl Pts',(-6.50918328200006,15.2,-9.27600936900001));
#282856=CARTESIAN_POINT('Ctrl Pts',(-6.50918328200006,11.6,-9.27600936900001));
#282857=CARTESIAN_POINT('Ctrl Pts',(-6.50609420700006,15.2,-9.27417010000001));
#282858=CARTESIAN_POINT('Ctrl Pts',(-6.50609420700006,11.6,-9.27417010000001));
#282859=CARTESIAN_POINT('Ctrl Pts',(-6.50301054600006,15.2,-9.27233081400002));
#282860=CARTESIAN_POINT('Ctrl Pts',(-6.50301054600006,11.6,-9.27233081400002));
#282861=CARTESIAN_POINT('Ctrl Pts',(-6.49993230100006,15.2,-9.27049152200001));
#282862=CARTESIAN_POINT('Ctrl Pts',(-6.49993230100006,11.6,-9.27049152200001));
#282863=CARTESIAN_POINT('Ctrl Pts',(-6.49685947500006,15.2,-9.26865223300002));
#282864=CARTESIAN_POINT('Ctrl Pts',(-6.49685947500006,11.6,-9.26865223300002));
#282865=CARTESIAN_POINT('Ctrl Pts',(-6.49379207300006,15.2,-9.26681295500002));
#282866=CARTESIAN_POINT('Ctrl Pts',(-6.49379207300006,11.6,-9.26681295500002));
#282867=CARTESIAN_POINT('Ctrl Pts',(-6.49073009700006,15.2,-9.26497369800002));
#282868=CARTESIAN_POINT('Ctrl Pts',(-6.49073009700006,11.6,-9.26497369800002));
#282869=CARTESIAN_POINT('Ctrl Pts',(-6.48767355200006,15.2,-9.26313447100001));
#282870=CARTESIAN_POINT('Ctrl Pts',(-6.48767355200006,11.6,-9.26313447100001));
#282871=CARTESIAN_POINT('Ctrl Pts',(-6.48462244000005,15.2,-9.26129528200001));
#282872=CARTESIAN_POINT('Ctrl Pts',(-6.48462244000005,11.6,-9.26129528200001));
#282873=CARTESIAN_POINT('Ctrl Pts',(-6.48157676400006,15.2,-9.25945614200002));
#282874=CARTESIAN_POINT('Ctrl Pts',(-6.48157676400006,11.6,-9.25945614200002));
#282875=CARTESIAN_POINT('Ctrl Pts',(-6.47853652900006,15.2,-9.25761705800002));
#282876=CARTESIAN_POINT('Ctrl Pts',(-6.47853652900006,11.6,-9.25761705800002));
#282877=CARTESIAN_POINT('Ctrl Pts',(-6.47550173800005,15.2,-9.25577804100002));
#282878=CARTESIAN_POINT('Ctrl Pts',(-6.47550173800005,11.6,-9.25577804100002));
#282879=CARTESIAN_POINT('Ctrl Pts',(-6.47247239300006,15.2,-9.25393910000002));
#282880=CARTESIAN_POINT('Ctrl Pts',(-6.47247239300006,11.6,-9.25393910000002));
#282881=CARTESIAN_POINT('Ctrl Pts',(-6.46944849900006,15.2,-9.25210024200002));
#282882=CARTESIAN_POINT('Ctrl Pts',(-6.46944849900006,11.6,-9.25210024200002));
#282883=CARTESIAN_POINT('Ctrl Pts',(-6.46643005900006,15.2,-9.25026147900001));
#282884=CARTESIAN_POINT('Ctrl Pts',(-6.46643005900006,11.6,-9.25026147900001));
#282885=CARTESIAN_POINT('Ctrl Pts',(-6.46341707600006,15.2,-9.24842281800002));
#282886=CARTESIAN_POINT('Ctrl Pts',(-6.46341707600006,11.6,-9.24842281800002));
#282887=CARTESIAN_POINT('Ctrl Pts',(-6.46040955400006,15.2,-9.24658427100002));
#282888=CARTESIAN_POINT('Ctrl Pts',(-6.46040955400006,11.6,-9.24658427100002));
#282889=CARTESIAN_POINT('Ctrl Pts',(-6.45740749600006,15.2,-9.24474584400001));
#282890=CARTESIAN_POINT('Ctrl Pts',(-6.45740749600006,11.6,-9.24474584400001));
#282891=CARTESIAN_POINT('Ctrl Pts',(-6.45441090500006,15.2,-9.24290754900002));
#282892=CARTESIAN_POINT('Ctrl Pts',(-6.45441090500006,11.6,-9.24290754900002));
#282893=CARTESIAN_POINT('Ctrl Pts',(-6.45141978500006,15.2,-9.24106939400002));
#282894=CARTESIAN_POINT('Ctrl Pts',(-6.45141978500006,11.6,-9.24106939400002));
#282895=CARTESIAN_POINT('Ctrl Pts',(-6.44843413900006,15.2,-9.23923138800001));
#282896=CARTESIAN_POINT('Ctrl Pts',(-6.44843413900006,11.6,-9.23923138800001));
#282897=CARTESIAN_POINT('Ctrl Pts',(-6.44545397200006,15.2,-9.23739354200002));
#282898=CARTESIAN_POINT('Ctrl Pts',(-6.44545397200006,11.6,-9.23739354200002));
#282899=CARTESIAN_POINT('Ctrl Pts',(-6.44247928500006,15.2,-9.23555586400001));
#282900=CARTESIAN_POINT('Ctrl Pts',(-6.44247928500006,11.6,-9.23555586400001));
#282901=CARTESIAN_POINT('Ctrl Pts',(-6.43951008200006,15.2,-9.23371836400002));
#282902=CARTESIAN_POINT('Ctrl Pts',(-6.43951008200006,11.6,-9.23371836400002));
#282903=CARTESIAN_POINT('Ctrl Pts',(-6.43654636800005,15.2,-9.23188105000002));
#282904=CARTESIAN_POINT('Ctrl Pts',(-6.43654636800005,11.6,-9.23188105000002));
#282905=CARTESIAN_POINT('Ctrl Pts',(-6.43358814400006,15.2,-9.23004393300002));
#282906=CARTESIAN_POINT('Ctrl Pts',(-6.43358814400006,11.6,-9.23004393300002));
#282907=CARTESIAN_POINT('Ctrl Pts',(-6.43063541500006,15.2,-9.22820702200001));
#282908=CARTESIAN_POINT('Ctrl Pts',(-6.43063541500006,11.6,-9.22820702200001));
#282909=CARTESIAN_POINT('Ctrl Pts',(-6.42768818400006,15.2,-9.22637032800001));
#282910=CARTESIAN_POINT('Ctrl Pts',(-6.42768818400006,11.6,-9.22637032800001));
#282911=CARTESIAN_POINT('Ctrl Pts',(-6.42474645500006,15.2,-9.22453385700001));
#282912=CARTESIAN_POINT('Ctrl Pts',(-6.42474645500006,11.6,-9.22453385700001));
#282913=CARTESIAN_POINT('Ctrl Pts',(-6.42181023000005,15.2,-9.22269762200001));
#282914=CARTESIAN_POINT('Ctrl Pts',(-6.42181023000005,11.6,-9.22269762200001));
#282915=CARTESIAN_POINT('Ctrl Pts',(-6.41887951300006,15.2,-9.22086163100002));
#282916=CARTESIAN_POINT('Ctrl Pts',(-6.41887951300006,11.6,-9.22086163100002));
#282917=CARTESIAN_POINT('Ctrl Pts',(-6.41595430900006,15.2,-9.21902589200002));
#282918=CARTESIAN_POINT('Ctrl Pts',(-6.41595430900006,11.6,-9.21902589200002));
#282919=CARTESIAN_POINT('Ctrl Pts',(-6.41303461900006,15.2,-9.21719041800002));
#282920=CARTESIAN_POINT('Ctrl Pts',(-6.41303461900006,11.6,-9.21719041800002));
#282921=CARTESIAN_POINT('Ctrl Pts',(-6.41012044700005,15.2,-9.21535521600001));
#282922=CARTESIAN_POINT('Ctrl Pts',(-6.41012044700005,11.6,-9.21535521600001));
#282923=CARTESIAN_POINT('Ctrl Pts',(-6.40721179700006,15.2,-9.21352029700002));
#282924=CARTESIAN_POINT('Ctrl Pts',(-6.40721179700006,11.6,-9.21352029700002));
#282925=CARTESIAN_POINT('Ctrl Pts',(-6.40430867200006,15.2,-9.21168566900001));
#282926=CARTESIAN_POINT('Ctrl Pts',(-6.40430867200006,11.6,-9.21168566900001));
#282927=CARTESIAN_POINT('Ctrl Pts',(-6.40141107500006,15.2,-9.20985134500001));
#282928=CARTESIAN_POINT('Ctrl Pts',(-6.40141107500006,11.6,-9.20985134500001));
#282929=CARTESIAN_POINT('Ctrl Pts',(-6.39851901000006,15.2,-9.20801733000001));
#282930=CARTESIAN_POINT('Ctrl Pts',(-6.39851901000006,11.6,-9.20801733000001));
#282931=CARTESIAN_POINT('Ctrl Pts',(-6.39563248000006,15.2,-9.20618363800001));
#282932=CARTESIAN_POINT('Ctrl Pts',(-6.39563248000006,11.6,-9.20618363800001));
#282933=CARTESIAN_POINT('Ctrl Pts',(-6.39275149000006,15.2,-9.20435027600002));
#282934=CARTESIAN_POINT('Ctrl Pts',(-6.39275149000006,11.6,-9.20435027600002));
#282935=CARTESIAN_POINT('Ctrl Pts',(-6.38987604000006,15.2,-9.20251725400002));
#282936=CARTESIAN_POINT('Ctrl Pts',(-6.38987604000006,11.6,-9.20251725400002));
#282937=CARTESIAN_POINT('Ctrl Pts',(-6.38700613600006,15.2,-9.20068458400002));
#282938=CARTESIAN_POINT('Ctrl Pts',(-6.38700613600006,11.6,-9.20068458400002));
#282939=CARTESIAN_POINT('Ctrl Pts',(-6.38414178100006,15.2,-9.19885227300002));
#282940=CARTESIAN_POINT('Ctrl Pts',(-6.38414178100006,11.6,-9.19885227300002));
#282941=CARTESIAN_POINT('Ctrl Pts',(-6.38128297700006,15.2,-9.19702033200002));
#282942=CARTESIAN_POINT('Ctrl Pts',(-6.38128297700006,11.6,-9.19702033200002));
#282943=CARTESIAN_POINT('Ctrl Pts',(-6.37842973000006,15.2,-9.19518877200002));
#282944=CARTESIAN_POINT('Ctrl Pts',(-6.37842973000006,11.6,-9.19518877200002));
#282945=CARTESIAN_POINT('Ctrl Pts',(-6.37558204100006,15.2,-9.19335760100001));
#282946=CARTESIAN_POINT('Ctrl Pts',(-6.37558204100006,11.6,-9.19335760100001));
#282947=CARTESIAN_POINT('Ctrl Pts',(-6.37273991300006,15.2,-9.19152682900001));
#282948=CARTESIAN_POINT('Ctrl Pts',(-6.37273991300006,11.6,-9.19152682900001));
#282949=CARTESIAN_POINT('Ctrl Pts',(-6.36990335200006,15.2,-9.18969646800001));
#282950=CARTESIAN_POINT('Ctrl Pts',(-6.36990335200006,11.6,-9.18969646800001));
#282951=CARTESIAN_POINT('Ctrl Pts',(-6.36707236000006,15.2,-9.18786652500001));
#282952=CARTESIAN_POINT('Ctrl Pts',(-6.36707236000006,11.6,-9.18786652500001));
#282953=CARTESIAN_POINT('Ctrl Pts',(-6.36424693800006,15.2,-9.18603701200002));
#282954=CARTESIAN_POINT('Ctrl Pts',(-6.36424693800006,11.6,-9.18603701200002));
#282955=CARTESIAN_POINT('Ctrl Pts',(-6.36142709400006,15.2,-9.18420793900001));
#282956=CARTESIAN_POINT('Ctrl Pts',(-6.36142709400006,11.6,-9.18420793900001));
#282957=CARTESIAN_POINT('Ctrl Pts',(-6.35861282700006,15.2,-9.18237931400002));
#282958=CARTESIAN_POINT('Ctrl Pts',(-6.35861282700006,11.6,-9.18237931400002));
#282959=CARTESIAN_POINT('Ctrl Pts',(-6.35580414300006,15.2,-9.18055114900002));
#282960=CARTESIAN_POINT('Ctrl Pts',(-6.35580414300006,11.6,-9.18055114900002));
#282961=CARTESIAN_POINT('Ctrl Pts',(-6.35300104500006,15.2,-9.17872345400001));
#282962=CARTESIAN_POINT('Ctrl Pts',(-6.35300104500006,11.6,-9.17872345400001));
#282963=CARTESIAN_POINT('Ctrl Pts',(-6.35020353500006,15.2,-9.17689623700002));
#282964=CARTESIAN_POINT('Ctrl Pts',(-6.35020353500006,11.6,-9.17689623700002));
#282965=CARTESIAN_POINT('Ctrl Pts',(-6.34741161800005,15.2,-9.17506951100002));
#282966=CARTESIAN_POINT('Ctrl Pts',(-6.34741161800005,11.6,-9.17506951100002));
#282967=CARTESIAN_POINT('Ctrl Pts',(-6.34462529700006,15.2,-9.17324328400002));
#282968=CARTESIAN_POINT('Ctrl Pts',(-6.34462529700006,11.6,-9.17324328400002));
#282969=CARTESIAN_POINT('Ctrl Pts',(-6.34184457400006,15.2,-9.17141756700002));
#282970=CARTESIAN_POINT('Ctrl Pts',(-6.34184457400006,11.6,-9.17141756700002));
#282971=CARTESIAN_POINT('Ctrl Pts',(-6.33906945400006,15.2,-9.16959237000002));
#282972=CARTESIAN_POINT('Ctrl Pts',(-6.33906945400006,11.6,-9.16959237000002));
#282973=CARTESIAN_POINT('Ctrl Pts',(-6.33629993900006,15.2,-9.16776770200002));
#282974=CARTESIAN_POINT('Ctrl Pts',(-6.33629993900006,11.6,-9.16776770200002));
#282975=CARTESIAN_POINT('Ctrl Pts',(-6.33353603400006,15.2,-9.16594357600001));
#282976=CARTESIAN_POINT('Ctrl Pts',(-6.33353603400006,11.6,-9.16594357600001));
#282977=CARTESIAN_POINT('Ctrl Pts',(-6.33077774100006,15.2,-9.16411999900001));
#282978=CARTESIAN_POINT('Ctrl Pts',(-6.33077774100006,11.6,-9.16411999900001));
#282979=CARTESIAN_POINT('Ctrl Pts',(-6.32802506300005,15.2,-9.16229698300001));
#282980=CARTESIAN_POINT('Ctrl Pts',(-6.32802506300005,11.6,-9.16229698300001));
#282981=CARTESIAN_POINT('Ctrl Pts',(-6.32527800500006,15.2,-9.16047453800001));
#282982=CARTESIAN_POINT('Ctrl Pts',(-6.32527800500006,11.6,-9.16047453800001));
#282983=CARTESIAN_POINT('Ctrl Pts',(-6.32253656800006,15.2,-9.15865267500001));
#282984=CARTESIAN_POINT('Ctrl Pts',(-6.32253656800006,11.6,-9.15865267500001));
#282985=CARTESIAN_POINT('Ctrl Pts',(-6.31980075800006,15.2,-9.15683140300001));
#282986=CARTESIAN_POINT('Ctrl Pts',(-6.31980075800006,11.6,-9.15683140300001));
#282987=CARTESIAN_POINT('Ctrl Pts',(-6.31707057700006,15.2,-9.15501073400002));
#282988=CARTESIAN_POINT('Ctrl Pts',(-6.31707057700006,11.6,-9.15501073400002));
#282989=CARTESIAN_POINT('Ctrl Pts',(-6.31434602800006,15.2,-9.15319067500001));
#282990=CARTESIAN_POINT('Ctrl Pts',(-6.31434602800006,11.6,-9.15319067500001));
#282991=CARTESIAN_POINT('Ctrl Pts',(-6.31162711400005,15.2,-9.15137124000001));
#282992=CARTESIAN_POINT('Ctrl Pts',(-6.31162711400005,11.6,-9.15137124000001));
#282993=CARTESIAN_POINT('Ctrl Pts',(-6.30891384000006,15.2,-9.14955243900001));
#282994=CARTESIAN_POINT('Ctrl Pts',(-6.30891384000006,11.6,-9.14955243900001));
#282995=CARTESIAN_POINT('Ctrl Pts',(-6.30620620800006,15.2,-9.14773428000002));
#282996=CARTESIAN_POINT('Ctrl Pts',(-6.30620620800006,11.6,-9.14773428000002));
#282997=CARTESIAN_POINT('Ctrl Pts',(-6.30350422100006,15.2,-9.14591677500002));
#282998=CARTESIAN_POINT('Ctrl Pts',(-6.30350422100006,11.6,-9.14591677500002));
#282999=CARTESIAN_POINT('Ctrl Pts',(-6.30080788400006,15.2,-9.14409993500002));
#283000=CARTESIAN_POINT('Ctrl Pts',(-6.30080788400006,11.6,-9.14409993500002));
#283001=CARTESIAN_POINT('Ctrl Pts',(-6.29811719900006,15.2,-9.14228377000001));
#283002=CARTESIAN_POINT('Ctrl Pts',(-6.29811719900006,11.6,-9.14228377000001));
#283003=CARTESIAN_POINT('Ctrl Pts',(-6.29543217000006,15.2,-9.14046829000002));
#283004=CARTESIAN_POINT('Ctrl Pts',(-6.29543217000006,11.6,-9.14046829000002));
#283005=CARTESIAN_POINT('Ctrl Pts',(-6.29275279900006,15.2,-9.13865350600001));
#283006=CARTESIAN_POINT('Ctrl Pts',(-6.29275279900006,11.6,-9.13865350600001));
#283007=CARTESIAN_POINT('Ctrl Pts',(-6.29007909100006,15.2,-9.13683942900001));
#283008=CARTESIAN_POINT('Ctrl Pts',(-6.29007909100006,11.6,-9.13683942900001));
#283009=CARTESIAN_POINT('Ctrl Pts',(-6.28741104800006,15.2,-9.13502606900002));
#283010=CARTESIAN_POINT('Ctrl Pts',(-6.28741104800006,11.6,-9.13502606900002));
#283011=CARTESIAN_POINT('Ctrl Pts',(-6.28474867400006,15.2,-9.13321343700002));
#283012=CARTESIAN_POINT('Ctrl Pts',(-6.28474867400006,11.6,-9.13321343700002));
#283013=CARTESIAN_POINT('Ctrl Pts',(-6.28209197200006,15.2,-9.13140154300002));
#283014=CARTESIAN_POINT('Ctrl Pts',(-6.28209197200006,11.6,-9.13140154300002));
#283015=CARTESIAN_POINT('Ctrl Pts',(-6.27944094700006,15.2,-9.12959039800001));
#283016=CARTESIAN_POINT('Ctrl Pts',(-6.27944094700006,11.6,-9.12959039800001));
#283017=CARTESIAN_POINT('Ctrl Pts',(-6.27679559900006,15.2,-9.12778001300002));
#283018=CARTESIAN_POINT('Ctrl Pts',(-6.27679559900006,11.6,-9.12778001300002));
#283019=CARTESIAN_POINT('Ctrl Pts',(-6.27415593500006,15.2,-9.12597039800002));
#283020=CARTESIAN_POINT('Ctrl Pts',(-6.27415593500006,11.6,-9.12597039800002));
#283021=CARTESIAN_POINT('Ctrl Pts',(-6.27152195600006,15.2,-9.12416156500001));
#283022=CARTESIAN_POINT('Ctrl Pts',(-6.27152195600006,11.6,-9.12416156500001));
#283023=CARTESIAN_POINT('Ctrl Pts',(-6.26889366400006,15.2,-9.12235352300002));
#283024=CARTESIAN_POINT('Ctrl Pts',(-6.26889366400006,11.6,-9.12235352300002));
#283025=CARTESIAN_POINT('Ctrl Pts',(-6.26627106600006,15.2,-9.12054628500002));
#283026=CARTESIAN_POINT('Ctrl Pts',(-6.26627106600006,11.6,-9.12054628500002));
#283027=CARTESIAN_POINT('Ctrl Pts',(-6.26365416200006,15.2,-9.11873986000002));
#283028=CARTESIAN_POINT('Ctrl Pts',(-6.26365416200006,11.6,-9.11873986000002));
#283029=CARTESIAN_POINT('Ctrl Pts',(-6.26104295800006,15.2,-9.11693426000001));
#283030=CARTESIAN_POINT('Ctrl Pts',(-6.26104295800006,11.6,-9.11693426000001));
#283031=CARTESIAN_POINT('Ctrl Pts',(-6.25843745500006,15.2,-9.11512949500001));
#283032=CARTESIAN_POINT('Ctrl Pts',(-6.25843745500006,11.6,-9.11512949500001));
#283033=CARTESIAN_POINT('Ctrl Pts',(-6.25583765700005,15.2,-9.11332557600002));
#283034=CARTESIAN_POINT('Ctrl Pts',(-6.25583765700005,11.6,-9.11332557600002));
#283035=CARTESIAN_POINT('Ctrl Pts',(-6.25324356800006,15.2,-9.11152251400001));
#283036=CARTESIAN_POINT('Ctrl Pts',(-6.25324356800006,11.6,-9.11152251400001));
#283037=CARTESIAN_POINT('Ctrl Pts',(-6.25065519100006,15.2,-9.10972032100002));
#283038=CARTESIAN_POINT('Ctrl Pts',(-6.25065519100006,11.6,-9.10972032100002));
#283039=CARTESIAN_POINT('Ctrl Pts',(-6.24807252900006,15.2,-9.10791900700002));
#283040=CARTESIAN_POINT('Ctrl Pts',(-6.24807252900006,11.6,-9.10791900700002));
#283041=CARTESIAN_POINT('Ctrl Pts',(-6.24549558500005,15.2,-9.10611858200001));
#283042=CARTESIAN_POINT('Ctrl Pts',(-6.24549558500005,11.6,-9.10611858200001));
#283043=CARTESIAN_POINT('Ctrl Pts',(-6.24292436400006,15.2,-9.10431905900002));
#283044=CARTESIAN_POINT('Ctrl Pts',(-6.24292436400006,11.6,-9.10431905900002));
#283045=CARTESIAN_POINT('Ctrl Pts',(-6.24035886600006,15.2,-9.10252044800002));
#283046=CARTESIAN_POINT('Ctrl Pts',(-6.24035886600006,11.6,-9.10252044800002));
#283047=CARTESIAN_POINT('Ctrl Pts',(-6.23779909800006,15.2,-9.10072276100001));
#283048=CARTESIAN_POINT('Ctrl Pts',(-6.23779909800006,11.6,-9.10072276100001));
#283049=CARTESIAN_POINT('Ctrl Pts',(-6.23524506100006,15.2,-9.09892600700001));
#283050=CARTESIAN_POINT('Ctrl Pts',(-6.23524506100006,11.6,-9.09892600700001));
#283051=CARTESIAN_POINT('Ctrl Pts',(-6.23269675900006,15.2,-9.09713019900002));
#283052=CARTESIAN_POINT('Ctrl Pts',(-6.23269675900006,11.6,-9.09713019900002));
#283053=CARTESIAN_POINT('Ctrl Pts',(-6.23015419600006,15.2,-9.09533534700002));
#283054=CARTESIAN_POINT('Ctrl Pts',(-6.23015419600006,11.6,-9.09533534700002));
#283055=CARTESIAN_POINT('Ctrl Pts',(-6.22761737300006,15.2,-9.09354146400002));
#283056=CARTESIAN_POINT('Ctrl Pts',(-6.22761737300006,11.6,-9.09354146400002));
#283057=CARTESIAN_POINT('Ctrl Pts',(-6.22508629500006,15.2,-9.09174855900002));
#283058=CARTESIAN_POINT('Ctrl Pts',(-6.22508629500006,11.6,-9.09174855900002));
#283059=CARTESIAN_POINT('Ctrl Pts',(-6.22256096500006,15.2,-9.08995664500001));
#283060=CARTESIAN_POINT('Ctrl Pts',(-6.22256096500006,11.6,-9.08995664500001));
#283061=CARTESIAN_POINT('Ctrl Pts',(-6.22004138600006,15.2,-9.08816573200001));
#283062=CARTESIAN_POINT('Ctrl Pts',(-6.22004138600006,11.6,-9.08816573200001));
#283063=CARTESIAN_POINT('Ctrl Pts',(-6.21752756200006,15.2,-9.08637583200001));
#283064=CARTESIAN_POINT('Ctrl Pts',(-6.21752756200006,11.6,-9.08637583200001));
#283065=CARTESIAN_POINT('Ctrl Pts',(-6.21501949600006,15.2,-9.08458695700002));
#283066=CARTESIAN_POINT('Ctrl Pts',(-6.21501949600006,11.6,-9.08458695700002));
#283067=CARTESIAN_POINT('Ctrl Pts',(-6.21251719100006,15.2,-9.08279911600001));
#283068=CARTESIAN_POINT('Ctrl Pts',(-6.21251719100006,11.6,-9.08279911600001));
#283069=CARTESIAN_POINT('Ctrl Pts',(-6.21002065000006,15.2,-9.08101232300002));
#283070=CARTESIAN_POINT('Ctrl Pts',(-6.21002065000006,11.6,-9.08101232300002));
#283071=CARTESIAN_POINT('Ctrl Pts',(-6.20752987700006,15.2,-9.07922658700001));
#283072=CARTESIAN_POINT('Ctrl Pts',(-6.20752987700006,11.6,-9.07922658700001));
#283073=CARTESIAN_POINT('Ctrl Pts',(-6.20504487400006,15.2,-9.07744192200001));
#283074=CARTESIAN_POINT('Ctrl Pts',(-6.20504487400006,11.6,-9.07744192200001));
#283075=CARTESIAN_POINT('Ctrl Pts',(-6.20256564600006,15.2,-9.07565833800002));
#283076=CARTESIAN_POINT('Ctrl Pts',(-6.20256564600006,11.6,-9.07565833800002));
#283077=CARTESIAN_POINT('Ctrl Pts',(-6.20009219500006,15.2,-9.07387584600002));
#283078=CARTESIAN_POINT('Ctrl Pts',(-6.20009219500006,11.6,-9.07387584600002));
#283079=CARTESIAN_POINT('Ctrl Pts',(-6.19762452500006,15.2,-9.07209445800002));
#283080=CARTESIAN_POINT('Ctrl Pts',(-6.19762452500006,11.6,-9.07209445800002));
#283081=CARTESIAN_POINT('Ctrl Pts',(-6.19516263900006,15.2,-9.07031418600001));
#283082=CARTESIAN_POINT('Ctrl Pts',(-6.19516263900006,11.6,-9.07031418600001));
#283083=CARTESIAN_POINT('Ctrl Pts',(-6.19270653900006,15.2,-9.06853504200001));
#283084=CARTESIAN_POINT('Ctrl Pts',(-6.19270653900006,11.6,-9.06853504200001));
#283085=CARTESIAN_POINT('Ctrl Pts',(-6.19025623000006,15.2,-9.06675703600002));
#283086=CARTESIAN_POINT('Ctrl Pts',(-6.19025623000006,11.6,-9.06675703600002));
#283087=CARTESIAN_POINT('Ctrl Pts',(-6.18781171500006,15.2,-9.06498018100002));
#283088=CARTESIAN_POINT('Ctrl Pts',(-6.18781171500006,11.6,-9.06498018100002));
#283089=CARTESIAN_POINT('Ctrl Pts',(-6.18537299700006,15.2,-9.06320448700002));
#283090=CARTESIAN_POINT('Ctrl Pts',(-6.18537299700006,11.6,-9.06320448700002));
#283091=CARTESIAN_POINT('Ctrl Pts',(-6.18294008000006,15.2,-9.06142996800002));
#283092=CARTESIAN_POINT('Ctrl Pts',(-6.18294008000006,11.6,-9.06142996800002));
#283093=CARTESIAN_POINT('Ctrl Pts',(-6.18051296500005,15.2,-9.05965663400002));
#283094=CARTESIAN_POINT('Ctrl Pts',(-6.18051296500005,11.6,-9.05965663400002));
#283095=CARTESIAN_POINT('Ctrl Pts',(-6.17809165700006,15.2,-9.05788449800001));
#283096=CARTESIAN_POINT('Ctrl Pts',(-6.17809165700006,11.6,-9.05788449800001));
#283097=CARTESIAN_POINT('Ctrl Pts',(-6.17567615900006,15.2,-9.05611357000002));
#283098=CARTESIAN_POINT('Ctrl Pts',(-6.17567615900006,11.6,-9.05611357000002));
#283099=CARTESIAN_POINT('Ctrl Pts',(-6.17326647500006,15.2,-9.05434386300002));
#283100=CARTESIAN_POINT('Ctrl Pts',(-6.17326647500006,11.6,-9.05434386300002));
#283101=CARTESIAN_POINT('Ctrl Pts',(-6.17086260700006,15.2,-9.05257538800001));
#283102=CARTESIAN_POINT('Ctrl Pts',(-6.17086260700006,11.6,-9.05257538800001));
#283103=CARTESIAN_POINT('Ctrl Pts',(-6.16846455700006,15.2,-9.05080815900002));
#283104=CARTESIAN_POINT('Ctrl Pts',(-6.16846455700006,11.6,-9.05080815900002));
#283105=CARTESIAN_POINT('Ctrl Pts',(-6.16607233200006,15.2,-9.04904218600001));
#283106=CARTESIAN_POINT('Ctrl Pts',(-6.16607233200006,11.6,-9.04904218600001));
#283107=CARTESIAN_POINT('Ctrl Pts',(-6.16368593200006,15.2,-9.04727748100001));
#283108=CARTESIAN_POINT('Ctrl Pts',(-6.16368593200006,11.6,-9.04727748100001));
#283109=CARTESIAN_POINT('Ctrl Pts',(-6.16130536200005,15.2,-9.04551405600002));
#283110=CARTESIAN_POINT('Ctrl Pts',(-6.16130536200005,11.6,-9.04551405600002));
#283111=CARTESIAN_POINT('Ctrl Pts',(-6.15893062400006,15.2,-9.04375192400002));
#283112=CARTESIAN_POINT('Ctrl Pts',(-6.15893062400006,11.6,-9.04375192400002));
#283113=CARTESIAN_POINT('Ctrl Pts',(-6.15656172200006,15.2,-9.04199109600002));
#283114=CARTESIAN_POINT('Ctrl Pts',(-6.15656172200006,11.6,-9.04199109600002));
#283115=CARTESIAN_POINT('Ctrl Pts',(-6.15419866000006,15.2,-9.04023158300001));
#283116=CARTESIAN_POINT('Ctrl Pts',(-6.15419866000006,11.6,-9.04023158300001));
#283117=CARTESIAN_POINT('Ctrl Pts',(-6.15184143900006,15.2,-9.03847340000001));
#283118=CARTESIAN_POINT('Ctrl Pts',(-6.15184143900006,11.6,-9.03847340000001));
#283119=CARTESIAN_POINT('Ctrl Pts',(-6.14949006400006,15.2,-9.03671655700002));
#283120=CARTESIAN_POINT('Ctrl Pts',(-6.14949006400006,11.6,-9.03671655700002));
#283121=CARTESIAN_POINT('Ctrl Pts',(-6.14714453800006,15.2,-9.03496106700001));
#283122=CARTESIAN_POINT('Ctrl Pts',(-6.14714453800006,11.6,-9.03496106700001));
#283123=CARTESIAN_POINT('Ctrl Pts',(-6.14480486400006,15.2,-9.03320694000002));
#283124=CARTESIAN_POINT('Ctrl Pts',(-6.14480486400006,11.6,-9.03320694000002));
#283125=CARTESIAN_POINT('Ctrl Pts',(-6.14247104500006,15.2,-9.03145419100002));
#283126=CARTESIAN_POINT('Ctrl Pts',(-6.14247104500006,11.6,-9.03145419100002));
#283127=CARTESIAN_POINT('Ctrl Pts',(-6.14014308400006,15.2,-9.02970283200002));
#283128=CARTESIAN_POINT('Ctrl Pts',(-6.14014308400006,11.6,-9.02970283200002));
#283129=CARTESIAN_POINT('Ctrl Pts',(-6.13782098400006,15.2,-9.02795287300002));
#283130=CARTESIAN_POINT('Ctrl Pts',(-6.13782098400006,11.6,-9.02795287300002));
#283131=CARTESIAN_POINT('Ctrl Pts',(-6.13550475100006,15.2,-9.02620432800001));
#283132=CARTESIAN_POINT('Ctrl Pts',(-6.13550475100006,11.6,-9.02620432800001));
#283133=CARTESIAN_POINT('Ctrl Pts',(-6.13319438500006,15.2,-9.02445720900002));
#283134=CARTESIAN_POINT('Ctrl Pts',(-6.13319438500006,11.6,-9.02445720900002));
#283135=CARTESIAN_POINT('Ctrl Pts',(-6.13088988900006,15.2,-9.02271152900001));
#283136=CARTESIAN_POINT('Ctrl Pts',(-6.13088988900006,11.6,-9.02271152900001));
#283137=CARTESIAN_POINT('Ctrl Pts',(-6.12859126900006,15.2,-9.02096729900002));
#283138=CARTESIAN_POINT('Ctrl Pts',(-6.12859126900006,11.6,-9.02096729900002));
#283139=CARTESIAN_POINT('Ctrl Pts',(-6.12629852600006,15.2,-9.01922453300001));
#283140=CARTESIAN_POINT('Ctrl Pts',(-6.12629852600006,11.6,-9.01922453300001));
#283141=CARTESIAN_POINT('Ctrl Pts',(-6.12401166400006,15.2,-9.01748324100001));
#283142=CARTESIAN_POINT('Ctrl Pts',(-6.12401166400006,11.6,-9.01748324100001));
#283143=CARTESIAN_POINT('Ctrl Pts',(-6.12173068600006,15.2,-9.01574343800002));
#283144=CARTESIAN_POINT('Ctrl Pts',(-6.12173068600006,11.6,-9.01574343800002));
#283145=CARTESIAN_POINT('Ctrl Pts',(-6.11945559600006,15.2,-9.01400513500001));
#283146=CARTESIAN_POINT('Ctrl Pts',(-6.11945559600006,11.6,-9.01400513500001));
#283147=CARTESIAN_POINT('Ctrl Pts',(-6.11718639600006,15.2,-9.01226834500001));
#283148=CARTESIAN_POINT('Ctrl Pts',(-6.11718639600006,11.6,-9.01226834500001));
#283149=CARTESIAN_POINT('Ctrl Pts',(-6.11492309000006,15.2,-9.01053308200002));
#283150=CARTESIAN_POINT('Ctrl Pts',(-6.11492309000006,11.6,-9.01053308200002));
#283151=CARTESIAN_POINT('Ctrl Pts',(-6.11266568000006,15.2,-9.00879935600001));
#283152=CARTESIAN_POINT('Ctrl Pts',(-6.11266568000006,11.6,-9.00879935600001));
#283153=CARTESIAN_POINT('Ctrl Pts',(-6.11041417200005,15.2,-9.00706718000002));
#283154=CARTESIAN_POINT('Ctrl Pts',(-6.11041417200005,11.6,-9.00706718000002));
#283155=CARTESIAN_POINT('Ctrl Pts',(-6.10816856500006,15.2,-9.00533656900001));
#283156=CARTESIAN_POINT('Ctrl Pts',(-6.10816856500006,11.6,-9.00533656900001));
#283157=CARTESIAN_POINT('Ctrl Pts',(-6.10592886600006,15.2,-9.00360753300001));
#283158=CARTESIAN_POINT('Ctrl Pts',(-6.10592886600006,11.6,-9.00360753300001));
#283159=CARTESIAN_POINT('Ctrl Pts',(-6.10369507600006,15.2,-9.00188008700002));
#283160=CARTESIAN_POINT('Ctrl Pts',(-6.10369507600006,11.6,-9.00188008700002));
#283161=CARTESIAN_POINT('Ctrl Pts',(-6.10146719900006,15.2,-9.00015424200001));
#283162=CARTESIAN_POINT('Ctrl Pts',(-6.10146719900006,11.6,-9.00015424200001));
#283163=CARTESIAN_POINT('Ctrl Pts',(-6.09924523800006,15.2,-8.99843001200002));
#283164=CARTESIAN_POINT('Ctrl Pts',(-6.09924523800006,11.6,-8.99843001200002));
#283165=CARTESIAN_POINT('Ctrl Pts',(-6.09702919700006,15.2,-8.99670741000002));
#283166=CARTESIAN_POINT('Ctrl Pts',(-6.09702919700006,11.6,-8.99670741000002));
#283167=CARTESIAN_POINT('Ctrl Pts',(-6.09481907700006,15.2,-8.99498644800002));
#283168=CARTESIAN_POINT('Ctrl Pts',(-6.09481907700006,11.6,-8.99498644800002));
#283169=CARTESIAN_POINT('Ctrl Pts',(-6.09261488400006,15.2,-8.99326713800002));
#283170=CARTESIAN_POINT('Ctrl Pts',(-6.09261488400006,11.6,-8.99326713800002));
#283171=CARTESIAN_POINT('Ctrl Pts',(-6.09041662000006,15.2,-8.99154949500002));
#283172=CARTESIAN_POINT('Ctrl Pts',(-6.09041662000006,11.6,-8.99154949500002));
#283173=CARTESIAN_POINT('Ctrl Pts',(-6.08822428600006,15.2,-8.98983353000002));
#283174=CARTESIAN_POINT('Ctrl Pts',(-6.08822428600006,11.6,-8.98983353000002));
#283175=CARTESIAN_POINT('Ctrl Pts',(-6.08603788900006,15.2,-8.98811925800001));
#283176=CARTESIAN_POINT('Ctrl Pts',(-6.08603788900006,11.6,-8.98811925800001));
#283177=CARTESIAN_POINT('Ctrl Pts',(-6.08385743000006,15.2,-8.98640669100002));
#283178=CARTESIAN_POINT('Ctrl Pts',(-6.08385743000006,11.6,-8.98640669100002));
#283179=CARTESIAN_POINT('Ctrl Pts',(-6.08168291200006,15.2,-8.98469584100001));
#283180=CARTESIAN_POINT('Ctrl Pts',(-6.08168291200006,11.6,-8.98469584100001));
#283181=CARTESIAN_POINT('Ctrl Pts',(-6.07951433900006,15.2,-8.98298672300001));
#283182=CARTESIAN_POINT('Ctrl Pts',(-6.07951433900006,11.6,-8.98298672300001));
#283183=CARTESIAN_POINT('Ctrl Pts',(-6.07735171400006,15.2,-8.98127934900002));
#283184=CARTESIAN_POINT('Ctrl Pts',(-6.07735171400006,11.6,-8.98127934900002));
#283185=CARTESIAN_POINT('Ctrl Pts',(-6.07519504000006,15.2,-8.97957373400001));
#283186=CARTESIAN_POINT('Ctrl Pts',(-6.07519504000006,11.6,-8.97957373400001));
#283187=CARTESIAN_POINT('Ctrl Pts',(-6.07304431900006,15.2,-8.97786988800001));
#283188=CARTESIAN_POINT('Ctrl Pts',(-6.07304431900006,11.6,-8.97786988800001));
#283189=CARTESIAN_POINT('Ctrl Pts',(-6.07089955600006,15.2,-8.97616782700002));
#283190=CARTESIAN_POINT('Ctrl Pts',(-6.07089955600006,11.6,-8.97616782700002));
#283191=CARTESIAN_POINT('Ctrl Pts',(-6.06876075400006,15.2,-8.97446756300001));
#283192=CARTESIAN_POINT('Ctrl Pts',(-6.06876075400006,11.6,-8.97446756300001));
#283193=CARTESIAN_POINT('Ctrl Pts',(-6.06662791600006,15.2,-8.97276910900001));
#283194=CARTESIAN_POINT('Ctrl Pts',(-6.06662791600006,11.6,-8.97276910900001));
#283195=CARTESIAN_POINT('Ctrl Pts',(-6.06450104400006,15.2,-8.97107248000001));
#283196=CARTESIAN_POINT('Ctrl Pts',(-6.06450104400006,11.6,-8.97107248000001));
#283197=CARTESIAN_POINT('Ctrl Pts',(-6.06238014200006,15.2,-8.96937768800001));
#283198=CARTESIAN_POINT('Ctrl Pts',(-6.06238014200006,11.6,-8.96937768800001));
#283199=CARTESIAN_POINT('Ctrl Pts',(-6.06026521300006,15.2,-8.96768474600002));
#283200=CARTESIAN_POINT('Ctrl Pts',(-6.06026521300006,11.6,-8.96768474600002));
#283201=CARTESIAN_POINT('Ctrl Pts',(-6.05815626100005,15.2,-8.96599367000002));
#283202=CARTESIAN_POINT('Ctrl Pts',(-6.05815626100005,11.6,-8.96599367000002));
#283203=CARTESIAN_POINT('Ctrl Pts',(-6.05605328900006,15.2,-8.96430447000002));
#283204=CARTESIAN_POINT('Ctrl Pts',(-6.05605328900006,11.6,-8.96430447000002));
#283205=CARTESIAN_POINT('Ctrl Pts',(-6.05395629800006,15.2,-8.96261716200002));
#283206=CARTESIAN_POINT('Ctrl Pts',(-6.05395629800006,11.6,-8.96261716200002));
#283207=CARTESIAN_POINT('Ctrl Pts',(-6.05186529400005,15.2,-8.96093175800001));
#283208=CARTESIAN_POINT('Ctrl Pts',(-6.05186529400005,11.6,-8.96093175800001));
#283209=CARTESIAN_POINT('Ctrl Pts',(-6.04978027800006,15.2,-8.95924827300002));
#283210=CARTESIAN_POINT('Ctrl Pts',(-6.04978027800006,11.6,-8.95924827300002));
#283211=CARTESIAN_POINT('Ctrl Pts',(-6.04770125400006,15.2,-8.95756672100001));
#283212=CARTESIAN_POINT('Ctrl Pts',(-6.04770125400006,11.6,-8.95756672100001));
#283213=CARTESIAN_POINT('Ctrl Pts',(-6.04562822600006,15.2,-8.95588711400002));
#283214=CARTESIAN_POINT('Ctrl Pts',(-6.04562822600006,11.6,-8.95588711400002));
#283215=CARTESIAN_POINT('Ctrl Pts',(-6.04356119600006,15.2,-8.95420946700002));
#283216=CARTESIAN_POINT('Ctrl Pts',(-6.04356119600006,11.6,-8.95420946700002));
#283217=CARTESIAN_POINT('Ctrl Pts',(-6.04150016700006,15.2,-8.95253379300001));
#283218=CARTESIAN_POINT('Ctrl Pts',(-6.04150016700006,11.6,-8.95253379300001));
#283219=CARTESIAN_POINT('Ctrl Pts',(-6.03944514200006,15.2,-8.95086010500002));
#283220=CARTESIAN_POINT('Ctrl Pts',(-6.03944514200006,11.6,-8.95086010500002));
#283221=CARTESIAN_POINT('Ctrl Pts',(-6.03739612600006,15.2,-8.94918841900001));
#283222=CARTESIAN_POINT('Ctrl Pts',(-6.03739612600006,11.6,-8.94918841900001));
#283223=CARTESIAN_POINT('Ctrl Pts',(-6.03535312000006,15.2,-8.94751874800002));
#283224=CARTESIAN_POINT('Ctrl Pts',(-6.03535312000006,11.6,-8.94751874800002));
#283225=CARTESIAN_POINT('Ctrl Pts',(-6.03331612900006,15.2,-8.94585110500002));
#283226=CARTESIAN_POINT('Ctrl Pts',(-6.03331612900006,11.6,-8.94585110500002));
#283227=CARTESIAN_POINT('Ctrl Pts',(-6.03128515400006,15.2,-8.94418550400001));
#283228=CARTESIAN_POINT('Ctrl Pts',(-6.03128515400006,11.6,-8.94418550400001));
#283229=CARTESIAN_POINT('Ctrl Pts',(-6.02926019900006,15.2,-8.94252196100001));
#283230=CARTESIAN_POINT('Ctrl Pts',(-6.02926019900006,11.6,-8.94252196100001));
#283231=CARTESIAN_POINT('Ctrl Pts',(-6.02724126900006,15.2,-8.94086048800002));
#283232=CARTESIAN_POINT('Ctrl Pts',(-6.02724126900006,11.6,-8.94086048800002));
#283233=CARTESIAN_POINT('Ctrl Pts',(-6.02522836400006,15.2,-8.93920110000002));
#283234=CARTESIAN_POINT('Ctrl Pts',(-6.02522836400006,11.6,-8.93920110000002));
#283235=CARTESIAN_POINT('Ctrl Pts',(-6.02322148900006,15.2,-8.93754381100001));
#283236=CARTESIAN_POINT('Ctrl Pts',(-6.02322148900006,11.6,-8.93754381100001));
#283237=CARTESIAN_POINT('Ctrl Pts',(-6.02122064700006,15.2,-8.93588863500002));
#283238=CARTESIAN_POINT('Ctrl Pts',(-6.02122064700006,11.6,-8.93588863500002));
#283239=CARTESIAN_POINT('Ctrl Pts',(-6.01922584100006,15.2,-8.93423558600002));
#283240=CARTESIAN_POINT('Ctrl Pts',(-6.01922584100006,11.6,-8.93423558600002));
#283241=CARTESIAN_POINT('Ctrl Pts',(-6.01723707400006,15.2,-8.93258467900001));
#283242=CARTESIAN_POINT('Ctrl Pts',(-6.01723707400006,11.6,-8.93258467900001));
#283243=CARTESIAN_POINT('Ctrl Pts',(-6.01525434800006,15.2,-8.93093592700002));
#283244=CARTESIAN_POINT('Ctrl Pts',(-6.01525434800006,11.6,-8.93093592700002));
#283245=CARTESIAN_POINT('Ctrl Pts',(-6.01327766800006,15.2,-8.92928934400001));
#283246=CARTESIAN_POINT('Ctrl Pts',(-6.01327766800006,11.6,-8.92928934400001));
#283247=CARTESIAN_POINT('Ctrl Pts',(-6.01130703700006,15.2,-8.92764494600002));
#283248=CARTESIAN_POINT('Ctrl Pts',(-6.01130703700006,11.6,-8.92764494600002));
#283249=CARTESIAN_POINT('Ctrl Pts',(-6.00934245600006,15.2,-8.92600274700002));
#283250=CARTESIAN_POINT('Ctrl Pts',(-6.00934245600006,11.6,-8.92600274700002));
#283251=CARTESIAN_POINT('Ctrl Pts',(-6.00738393100006,15.2,-8.92436276200002));
#283252=CARTESIAN_POINT('Ctrl Pts',(-6.00738393100006,11.6,-8.92436276200002));
#283253=CARTESIAN_POINT('Ctrl Pts',(-6.00543146200006,15.2,-8.92272500300002));
#283254=CARTESIAN_POINT('Ctrl Pts',(-6.00543146200006,11.6,-8.92272500300002));
#283255=CARTESIAN_POINT('Ctrl Pts',(-6.00348505500006,15.2,-8.92108948700002));
#283256=CARTESIAN_POINT('Ctrl Pts',(-6.00348505500006,11.6,-8.92108948700002));
#283257=CARTESIAN_POINT('Ctrl Pts',(-6.00154471100006,15.2,-8.91945622800002));
#283258=CARTESIAN_POINT('Ctrl Pts',(-6.00154471100006,11.6,-8.91945622800002));
#283259=CARTESIAN_POINT('Ctrl Pts',(-5.99961043400006,15.2,-8.91782524000002));
#283260=CARTESIAN_POINT('Ctrl Pts',(-5.99961043400006,11.6,-8.91782524000002));
#283261=CARTESIAN_POINT('Ctrl Pts',(-5.99768222800006,15.2,-8.91619653700002));
#283262=CARTESIAN_POINT('Ctrl Pts',(-5.99768222800006,11.6,-8.91619653700002));
#283263=CARTESIAN_POINT('Ctrl Pts',(-5.99576009400006,15.2,-8.91457013600002));
#283264=CARTESIAN_POINT('Ctrl Pts',(-5.99576009400006,11.6,-8.91457013600002));
#283265=CARTESIAN_POINT('Ctrl Pts',(-5.99384403600006,15.2,-8.91294604900001));
#283266=CARTESIAN_POINT('Ctrl Pts',(-5.99384403600006,11.6,-8.91294604900001));
#283267=CARTESIAN_POINT('Ctrl Pts',(-5.99193405800006,15.2,-8.91132429300002));
#283268=CARTESIAN_POINT('Ctrl Pts',(-5.99193405800006,11.6,-8.91132429300002));
#283269=CARTESIAN_POINT('Ctrl Pts',(-5.99003016200006,15.2,-8.90970488200002));
#283270=CARTESIAN_POINT('Ctrl Pts',(-5.99003016200006,11.6,-8.90970488200002));
#283271=CARTESIAN_POINT('Ctrl Pts',(-5.98813235200006,15.2,-8.90808783100002));
#283272=CARTESIAN_POINT('Ctrl Pts',(-5.98813235200006,11.6,-8.90808783100002));
#283273=CARTESIAN_POINT('Ctrl Pts',(-5.98624062900006,15.2,-8.90647315300001));
#283274=CARTESIAN_POINT('Ctrl Pts',(-5.98624062900006,11.6,-8.90647315300001));
#283275=CARTESIAN_POINT('Ctrl Pts',(-5.98435500000006,15.2,-8.90486086600001));
#283276=CARTESIAN_POINT('Ctrl Pts',(-5.98435500000006,11.6,-8.90486086600001));
#283277=CARTESIAN_POINT('Ctrl Pts',(-5.98247546400006,15.2,-8.90325098400002));
#283278=CARTESIAN_POINT('Ctrl Pts',(-5.98247546400006,11.6,-8.90325098400002));
#283279=CARTESIAN_POINT('Ctrl Pts',(-5.98060202600006,15.2,-8.90164352000001));
#283280=CARTESIAN_POINT('Ctrl Pts',(-5.98060202600006,11.6,-8.90164352000001));
#283281=CARTESIAN_POINT('Ctrl Pts',(-5.97873468900006,15.2,-8.90003849100001));
#283282=CARTESIAN_POINT('Ctrl Pts',(-5.97873468900006,11.6,-8.90003849100001));
#283283=CARTESIAN_POINT('Ctrl Pts',(-5.97687345600006,15.2,-8.89843591300002));
#283284=CARTESIAN_POINT('Ctrl Pts',(-5.97687345600006,11.6,-8.89843591300002));
#283285=CARTESIAN_POINT('Ctrl Pts',(-5.97501833000006,15.2,-8.89683579900002));
#283286=CARTESIAN_POINT('Ctrl Pts',(-5.97501833000006,11.6,-8.89683579900002));
#283287=CARTESIAN_POINT('Ctrl Pts',(-5.97316931400006,15.2,-8.89523816500001));
#283288=CARTESIAN_POINT('Ctrl Pts',(-5.97316931400006,11.6,-8.89523816500001));
#283289=CARTESIAN_POINT('Ctrl Pts',(-5.97132641200006,15.2,-8.89364302600002));
#283290=CARTESIAN_POINT('Ctrl Pts',(-5.97132641200006,11.6,-8.89364302600002));
#283291=CARTESIAN_POINT('Ctrl Pts',(-5.96948962500006,15.2,-8.89205039900002));
#283292=CARTESIAN_POINT('Ctrl Pts',(-5.96948962500006,11.6,-8.89205039900002));
#283293=CARTESIAN_POINT('Ctrl Pts',(-5.96765895700006,15.2,-8.89046029700001));
#283294=CARTESIAN_POINT('Ctrl Pts',(-5.96765895700006,11.6,-8.89046029700001));
#283295=CARTESIAN_POINT('Ctrl Pts',(-5.96583441200006,15.2,-8.88887273700002));
#283296=CARTESIAN_POINT('Ctrl Pts',(-5.96583441200006,11.6,-8.88887273700002));
#283297=CARTESIAN_POINT('Ctrl Pts',(-5.96401599300005,15.2,-8.88728773400001));
#283298=CARTESIAN_POINT('Ctrl Pts',(-5.96401599300005,11.6,-8.88728773400001));
#283299=CARTESIAN_POINT('Ctrl Pts',(-5.96220370200006,15.2,-8.88570530200001));
#283300=CARTESIAN_POINT('Ctrl Pts',(-5.96220370200006,11.6,-8.88570530200001));
#283301=CARTESIAN_POINT('Ctrl Pts',(-5.96039754200006,15.2,-8.88412545900002));
#283302=CARTESIAN_POINT('Ctrl Pts',(-5.96039754200006,11.6,-8.88412545900002));
#283303=CARTESIAN_POINT('Ctrl Pts',(-5.95859751600006,15.2,-8.88254821900002));
#283304=CARTESIAN_POINT('Ctrl Pts',(-5.95859751600006,11.6,-8.88254821900002));
#283305=CARTESIAN_POINT('Ctrl Pts',(-5.95680362900006,15.2,-8.88097359800001));
#283306=CARTESIAN_POINT('Ctrl Pts',(-5.95680362900006,11.6,-8.88097359800001));
#283307=CARTESIAN_POINT('Ctrl Pts',(-5.95501588200006,15.2,-8.87940161100002));
#283308=CARTESIAN_POINT('Ctrl Pts',(-5.95501588200006,11.6,-8.87940161100002));
#283309=CARTESIAN_POINT('Ctrl Pts',(-5.95323427900006,15.2,-8.87783227600002));
#283310=CARTESIAN_POINT('Ctrl Pts',(-5.95323427900006,11.6,-8.87783227600002));
#283311=CARTESIAN_POINT('Ctrl Pts',(-5.95145882200006,15.2,-8.87626560600001));
#283312=CARTESIAN_POINT('Ctrl Pts',(-5.95145882200006,11.6,-8.87626560600001));
#283313=CARTESIAN_POINT('Ctrl Pts',(-5.94968951600006,15.2,-8.87470161900002));
#283314=CARTESIAN_POINT('Ctrl Pts',(-5.94968951600006,11.6,-8.87470161900002));
#283315=CARTESIAN_POINT('Ctrl Pts',(-5.94792636200006,15.2,-8.87314032800001));
#283316=CARTESIAN_POINT('Ctrl Pts',(-5.94792636200006,11.6,-8.87314032800001));
#283317=CARTESIAN_POINT('Ctrl Pts',(-5.94616936500006,15.2,-8.87158175200002));
#283318=CARTESIAN_POINT('Ctrl Pts',(-5.94616936500006,11.6,-8.87158175200002));
#283319=CARTESIAN_POINT('Ctrl Pts',(-5.94441852600006,15.2,-8.87002590600002));
#283320=CARTESIAN_POINT('Ctrl Pts',(-5.94441852600006,11.6,-8.87002590600002));
#283321=CARTESIAN_POINT('Ctrl Pts',(-5.94267384900006,15.2,-8.86847280400002));
#283322=CARTESIAN_POINT('Ctrl Pts',(-5.94267384900006,11.6,-8.86847280400002));
#283323=CARTESIAN_POINT('Ctrl Pts',(-5.94093533700006,15.2,-8.86692246600001));
#283324=CARTESIAN_POINT('Ctrl Pts',(-5.94093533700006,11.6,-8.86692246600001));
#283325=CARTESIAN_POINT('Ctrl Pts',(-5.93920299300006,15.2,-8.86537490400002));
#283326=CARTESIAN_POINT('Ctrl Pts',(-5.93920299300006,11.6,-8.86537490400002));
#283327=CARTESIAN_POINT('Ctrl Pts',(-5.93747681900005,15.2,-8.86383013700001));
#283328=CARTESIAN_POINT('Ctrl Pts',(-5.93747681900005,11.6,-8.86383013700001));
#283329=CARTESIAN_POINT('Ctrl Pts',(-5.93575682000006,15.2,-8.86228817900001));
#283330=CARTESIAN_POINT('Ctrl Pts',(-5.93575682000006,11.6,-8.86228817900001));
#283331=CARTESIAN_POINT('Ctrl Pts',(-5.93404299900006,15.2,-8.86074904800001));
#283332=CARTESIAN_POINT('Ctrl Pts',(-5.93404299900006,11.6,-8.86074904800001));
#283333=CARTESIAN_POINT('Ctrl Pts',(-5.93233535700006,15.2,-8.85921276000002));
#283334=CARTESIAN_POINT('Ctrl Pts',(-5.93233535700006,11.6,-8.85921276000002));
#283335=CARTESIAN_POINT('Ctrl Pts',(-5.93063389800006,15.2,-8.85767933100002));
#283336=CARTESIAN_POINT('Ctrl Pts',(-5.93063389800006,11.6,-8.85767933100002));
#283337=CARTESIAN_POINT('Ctrl Pts',(-5.92893862600006,15.2,-8.85614877700002));
#283338=CARTESIAN_POINT('Ctrl Pts',(-5.92893862600006,11.6,-8.85614877700002));
#283339=CARTESIAN_POINT('Ctrl Pts',(-5.92724954300006,15.2,-8.85462111500001));
#283340=CARTESIAN_POINT('Ctrl Pts',(-5.92724954300006,11.6,-8.85462111500001));
#283341=CARTESIAN_POINT('Ctrl Pts',(-5.92556665300005,15.2,-8.85309636200001));
#283342=CARTESIAN_POINT('Ctrl Pts',(-5.92556665300005,11.6,-8.85309636200001));
#283343=CARTESIAN_POINT('Ctrl Pts',(-5.92388995600006,15.2,-8.85157453400002));
#283344=CARTESIAN_POINT('Ctrl Pts',(-5.92388995600006,11.6,-8.85157453400002));
#283345=CARTESIAN_POINT('Ctrl Pts',(-5.92221945900006,15.2,-8.85005564700002));
#283346=CARTESIAN_POINT('Ctrl Pts',(-5.92221945900006,11.6,-8.85005564700002));
#283347=CARTESIAN_POINT('Ctrl Pts',(-5.92055516300006,15.2,-8.84853971800002));
#283348=CARTESIAN_POINT('Ctrl Pts',(-5.92055516300006,11.6,-8.84853971800002));
#283349=CARTESIAN_POINT('Ctrl Pts',(-5.91889707100006,15.2,-8.84702676400002));
#283350=CARTESIAN_POINT('Ctrl Pts',(-5.91889707100006,11.6,-8.84702676400002));
#283351=CARTESIAN_POINT('Ctrl Pts',(-5.91724518600006,15.2,-8.84551680200002));
#283352=CARTESIAN_POINT('Ctrl Pts',(-5.91724518600006,11.6,-8.84551680200002));
#283353=CARTESIAN_POINT('Ctrl Pts',(-5.91559951200006,15.2,-8.84400984900001));
#283354=CARTESIAN_POINT('Ctrl Pts',(-5.91559951200006,11.6,-8.84400984900001));
#283355=CARTESIAN_POINT('Ctrl Pts',(-5.91396005000006,15.2,-8.84250592100001));
#283356=CARTESIAN_POINT('Ctrl Pts',(-5.91396005000006,11.6,-8.84250592100001));
#283357=CARTESIAN_POINT('Ctrl Pts',(-5.91232680500006,15.2,-8.84100503500001));
#283358=CARTESIAN_POINT('Ctrl Pts',(-5.91232680500006,11.6,-8.84100503500001));
#283359=CARTESIAN_POINT('Ctrl Pts',(-5.91069977900006,15.2,-8.83950721000001));
#283360=CARTESIAN_POINT('Ctrl Pts',(-5.91069977900006,11.6,-8.83950721000001));
#283361=CARTESIAN_POINT('Ctrl Pts',(-5.90907897600006,15.2,-8.83801246000001));
#283362=CARTESIAN_POINT('Ctrl Pts',(-5.90907897600006,11.6,-8.83801246000001));
#283363=CARTESIAN_POINT('Ctrl Pts',(-5.90746439700006,15.2,-8.83652080200001));
#283364=CARTESIAN_POINT('Ctrl Pts',(-5.90746439700006,11.6,-8.83652080200001));
#283365=CARTESIAN_POINT('Ctrl Pts',(-5.90585604700006,15.2,-8.83503225700002));
#283366=CARTESIAN_POINT('Ctrl Pts',(-5.90585604700006,11.6,-8.83503225700002));
#283367=CARTESIAN_POINT('Ctrl Pts',(-5.90425392900006,15.2,-8.83354683900002));
#283368=CARTESIAN_POINT('Ctrl Pts',(-5.90425392900006,11.6,-8.83354683900002));
#283369=CARTESIAN_POINT('Ctrl Pts',(-5.90265804300006,15.2,-8.83206456600002));
#283370=CARTESIAN_POINT('Ctrl Pts',(-5.90265804300006,11.6,-8.83206456600002));
#283371=CARTESIAN_POINT('Ctrl Pts',(-5.90106839700006,15.2,-8.83058545500001));
#283372=CARTESIAN_POINT('Ctrl Pts',(-5.90106839700006,11.6,-8.83058545500001));
#283373=CARTESIAN_POINT('Ctrl Pts',(-5.89948498900006,15.2,-8.82910952300002));
#283374=CARTESIAN_POINT('Ctrl Pts',(-5.89948498900006,11.6,-8.82910952300002));
#283375=CARTESIAN_POINT('Ctrl Pts',(-5.89790782500006,15.2,-8.82763679000002));
#283376=CARTESIAN_POINT('Ctrl Pts',(-5.89790782500006,11.6,-8.82763679000002));
#283377=CARTESIAN_POINT('Ctrl Pts',(-5.89633690700006,15.2,-8.82616727000002));
#283378=CARTESIAN_POINT('Ctrl Pts',(-5.89633690700006,11.6,-8.82616727000002));
#283379=CARTESIAN_POINT('Ctrl Pts',(-5.89477223700006,15.2,-8.82470098400002));
#283380=CARTESIAN_POINT('Ctrl Pts',(-5.89477223700006,11.6,-8.82470098400002));
#283381=CARTESIAN_POINT('Ctrl Pts',(-5.89321382100006,15.2,-8.82323794600002));
#283382=CARTESIAN_POINT('Ctrl Pts',(-5.89321382100006,11.6,-8.82323794600002));
#283383=CARTESIAN_POINT('Ctrl Pts',(-5.89166165900005,15.2,-8.82177817600001));
#283384=CARTESIAN_POINT('Ctrl Pts',(-5.89166165900005,11.6,-8.82177817600001));
#283385=CARTESIAN_POINT('Ctrl Pts',(-5.89011575500006,15.2,-8.82032169100002));
#283386=CARTESIAN_POINT('Ctrl Pts',(-5.89011575500006,11.6,-8.82032169100002));
#283387=CARTESIAN_POINT('Ctrl Pts',(-5.88857611200006,15.2,-8.81886851000001));
#283388=CARTESIAN_POINT('Ctrl Pts',(-5.88857611200006,11.6,-8.81886851000001));
#283389=CARTESIAN_POINT('Ctrl Pts',(-5.88704273400006,15.2,-8.81741864800002));
#283390=CARTESIAN_POINT('Ctrl Pts',(-5.88704273400006,11.6,-8.81741864800002));
#283391=CARTESIAN_POINT('Ctrl Pts',(-5.88551562100006,15.2,-8.81597212600001));
#283392=CARTESIAN_POINT('Ctrl Pts',(-5.88551562100006,11.6,-8.81597212600001));
#283393=CARTESIAN_POINT('Ctrl Pts',(-5.88399477900006,15.2,-8.81452896000001));
#283394=CARTESIAN_POINT('Ctrl Pts',(-5.88399477900006,11.6,-8.81452896000001));
#283395=CARTESIAN_POINT('Ctrl Pts',(-5.88248021000005,15.2,-8.81308916900002));
#283396=CARTESIAN_POINT('Ctrl Pts',(-5.88248021000005,11.6,-8.81308916900002));
#283397=CARTESIAN_POINT('Ctrl Pts',(-5.88097191600006,15.2,-8.81165276900001));
#283398=CARTESIAN_POINT('Ctrl Pts',(-5.88097191600006,11.6,-8.81165276900001));
#283399=CARTESIAN_POINT('Ctrl Pts',(-5.87946990200006,15.2,-8.81021978100001));
#283400=CARTESIAN_POINT('Ctrl Pts',(-5.87946990200006,11.6,-8.81021978100001));
#283401=CARTESIAN_POINT('Ctrl Pts',(-5.87797416900006,15.2,-8.80879022300002));
#283402=CARTESIAN_POINT('Ctrl Pts',(-5.87797416900006,11.6,-8.80879022300002));
#283403=CARTESIAN_POINT('Ctrl Pts',(-5.87648472000006,15.2,-8.80736411100001));
#283404=CARTESIAN_POINT('Ctrl Pts',(-5.87648472000006,11.6,-8.80736411100001));
#283405=CARTESIAN_POINT('Ctrl Pts',(-5.87500155900006,15.2,-8.80594146500002));
#283406=CARTESIAN_POINT('Ctrl Pts',(-5.87500155900006,11.6,-8.80594146500002));
#283407=CARTESIAN_POINT('Ctrl Pts',(-5.87352468900006,15.2,-8.80452230300002));
#283408=CARTESIAN_POINT('Ctrl Pts',(-5.87352468900006,11.6,-8.80452230300002));
#283409=CARTESIAN_POINT('Ctrl Pts',(-5.87205411200006,15.2,-8.80310664200002));
#283410=CARTESIAN_POINT('Ctrl Pts',(-5.87205411200006,11.6,-8.80310664200002));
#283411=CARTESIAN_POINT('Ctrl Pts',(-5.87058983200006,15.2,-8.80169450300002));
#283412=CARTESIAN_POINT('Ctrl Pts',(-5.87058983200006,11.6,-8.80169450300002));
#283413=CARTESIAN_POINT('Ctrl Pts',(-5.86913185000006,15.2,-8.80028590300002));
#283414=CARTESIAN_POINT('Ctrl Pts',(-5.86913185000006,11.6,-8.80028590300002));
#283415=CARTESIAN_POINT('Ctrl Pts',(-5.86768017200006,15.2,-8.79888086200001));
#283416=CARTESIAN_POINT('Ctrl Pts',(-5.86768017200006,11.6,-8.79888086200001));
#283417=CARTESIAN_POINT('Ctrl Pts',(-5.86623479900005,15.2,-8.79747939600002));
#283418=CARTESIAN_POINT('Ctrl Pts',(-5.86623479900005,11.6,-8.79747939600002));
#283419=CARTESIAN_POINT('Ctrl Pts',(-5.86479573400006,15.2,-8.79608152700002));
#283420=CARTESIAN_POINT('Ctrl Pts',(-5.86479573400006,11.6,-8.79608152700002));
#283421=CARTESIAN_POINT('Ctrl Pts',(-5.86336298000006,15.2,-8.79468727200001));
#283422=CARTESIAN_POINT('Ctrl Pts',(-5.86336298000006,11.6,-8.79468727200001));
#283423=CARTESIAN_POINT('Ctrl Pts',(-5.86193653900006,15.2,-8.79329665000002));
#283424=CARTESIAN_POINT('Ctrl Pts',(-5.86193653900006,11.6,-8.79329665000002));
#283425=CARTESIAN_POINT('Ctrl Pts',(-5.86051641600006,15.2,-8.79190968000002));
#283426=CARTESIAN_POINT('Ctrl Pts',(-5.86051641600006,11.6,-8.79190968000002));
#283427=CARTESIAN_POINT('Ctrl Pts',(-5.85910261300006,15.2,-8.79052638100001));
#283428=CARTESIAN_POINT('Ctrl Pts',(-5.85910261300006,11.6,-8.79052638100001));
#283429=CARTESIAN_POINT('Ctrl Pts',(-5.85769513200006,15.2,-8.78914677200001));
#283430=CARTESIAN_POINT('Ctrl Pts',(-5.85769513200006,11.6,-8.78914677200001));
#283431=CARTESIAN_POINT('Ctrl Pts',(-5.85629397700006,15.2,-8.78777087300002));
#283432=CARTESIAN_POINT('Ctrl Pts',(-5.85629397700006,11.6,-8.78777087300002));
#283433=CARTESIAN_POINT('Ctrl Pts',(-5.85489915200006,15.2,-8.78639870300002));
#283434=CARTESIAN_POINT('Ctrl Pts',(-5.85489915200006,11.6,-8.78639870300002));
#283435=CARTESIAN_POINT('Ctrl Pts',(-5.85351065700006,15.2,-8.78503028000001));
#283436=CARTESIAN_POINT('Ctrl Pts',(-5.85351065700006,11.6,-8.78503028000001));
#283437=CARTESIAN_POINT('Ctrl Pts',(-5.85212849700006,15.2,-8.78366562400002));
#283438=CARTESIAN_POINT('Ctrl Pts',(-5.85212849700006,11.6,-8.78366562400002));
#283439=CARTESIAN_POINT('Ctrl Pts',(-5.85075267500006,15.2,-8.78230475600001));
#283440=CARTESIAN_POINT('Ctrl Pts',(-5.85075267500006,11.6,-8.78230475600001));
#283441=CARTESIAN_POINT('Ctrl Pts',(-5.84938319300006,15.2,-8.78094769400001));
#283442=CARTESIAN_POINT('Ctrl Pts',(-5.84938319300006,11.6,-8.78094769400001));
#283443=CARTESIAN_POINT('Ctrl Pts',(-5.84802005400006,15.2,-8.77959445700002));
#283444=CARTESIAN_POINT('Ctrl Pts',(-5.84802005400006,11.6,-8.77959445700002));
#283445=CARTESIAN_POINT('Ctrl Pts',(-5.84666326000006,15.2,-8.77824506500002));
#283446=CARTESIAN_POINT('Ctrl Pts',(-5.84666326000006,11.6,-8.77824506500002));
#283447=CARTESIAN_POINT('Ctrl Pts',(-5.84531281700006,15.2,-8.77689953800001));
#283448=CARTESIAN_POINT('Ctrl Pts',(-5.84531281700006,11.6,-8.77689953800001));
#283449=CARTESIAN_POINT('Ctrl Pts',(-5.84396872500006,15.2,-8.77555789600001));
#283450=CARTESIAN_POINT('Ctrl Pts',(-5.84396872500006,11.6,-8.77555789600001));
#283451=CARTESIAN_POINT('Ctrl Pts',(-5.84263098700006,15.2,-8.77422015900001));
#283452=CARTESIAN_POINT('Ctrl Pts',(-5.84263098700006,11.6,-8.77422015900001));
#283453=CARTESIAN_POINT('Ctrl Pts',(-5.84129960800006,15.2,-8.77288634600001));
#283454=CARTESIAN_POINT('Ctrl Pts',(-5.84129960800006,11.6,-8.77288634600001));
#283455=CARTESIAN_POINT('Ctrl Pts',(-5.83997459000006,15.2,-8.77155647700001));
#283456=CARTESIAN_POINT('Ctrl Pts',(-5.83997459000006,11.6,-8.77155647700001));
#283457=CARTESIAN_POINT('Ctrl Pts',(-5.83865593500006,15.2,-8.77023057400002));
#283458=CARTESIAN_POINT('Ctrl Pts',(-5.83865593500006,11.6,-8.77023057400002));
#283459=CARTESIAN_POINT('Ctrl Pts',(-5.83734364600006,15.2,-8.76890865500001));
#283460=CARTESIAN_POINT('Ctrl Pts',(-5.83734364600006,11.6,-8.76890865500001));
#283461=CARTESIAN_POINT('Ctrl Pts',(-5.83603772700005,15.2,-8.76759074100002));
#283462=CARTESIAN_POINT('Ctrl Pts',(-5.83603772700005,11.6,-8.76759074100002));
#283463=CARTESIAN_POINT('Ctrl Pts',(-5.83473817900006,15.2,-8.76627685200001));
#283464=CARTESIAN_POINT('Ctrl Pts',(-5.83473817900006,11.6,-8.76627685200001));
#283465=CARTESIAN_POINT('Ctrl Pts',(-5.83344500700006,15.2,-8.76496700800002));
#283466=CARTESIAN_POINT('Ctrl Pts',(-5.83344500700006,11.6,-8.76496700800002));
#283467=CARTESIAN_POINT('Ctrl Pts',(-5.83215821300006,15.2,-8.76366123100001));
#283468=CARTESIAN_POINT('Ctrl Pts',(-5.83215821300006,11.6,-8.76366123100001));
#283469=CARTESIAN_POINT('Ctrl Pts',(-5.83087780000006,15.2,-8.76235953900002));
#283470=CARTESIAN_POINT('Ctrl Pts',(-5.83087780000006,11.6,-8.76235953900002));
#283471=CARTESIAN_POINT('Ctrl Pts',(-5.82960377000005,15.2,-8.76106195500002));
#283472=CARTESIAN_POINT('Ctrl Pts',(-5.82960377000005,11.6,-8.76106195500002));
#283473=CARTESIAN_POINT('Ctrl Pts',(-5.82833612700006,15.2,-8.75976849900002));
#283474=CARTESIAN_POINT('Ctrl Pts',(-5.82833612700006,11.6,-8.75976849900002));
#283475=CARTESIAN_POINT('Ctrl Pts',(-5.82707487300006,15.2,-8.75847919000002));
#283476=CARTESIAN_POINT('Ctrl Pts',(-5.82707487300006,11.6,-8.75847919000002));
#283477=CARTESIAN_POINT('Ctrl Pts',(-5.82582001200006,15.2,-8.75719405100002));
#283478=CARTESIAN_POINT('Ctrl Pts',(-5.82582001200006,11.6,-8.75719405100002));
#283479=CARTESIAN_POINT('Ctrl Pts',(-5.82457154700006,15.2,-8.75591310200001));
#283480=CARTESIAN_POINT('Ctrl Pts',(-5.82457154700006,11.6,-8.75591310200001));
#283481=CARTESIAN_POINT('Ctrl Pts',(-5.82332948000006,15.2,-8.75463636300001));
#283482=CARTESIAN_POINT('Ctrl Pts',(-5.82332948000006,11.6,-8.75463636300001));
#283483=CARTESIAN_POINT('Ctrl Pts',(-5.82209381200006,15.2,-8.75336385700002));
#283484=CARTESIAN_POINT('Ctrl Pts',(-5.82209381200006,11.6,-8.75336385700002));
#283485=CARTESIAN_POINT('Ctrl Pts',(-5.82086454900006,15.2,-8.75209560300001));
#283486=CARTESIAN_POINT('Ctrl Pts',(-5.82086454900006,11.6,-8.75209560300001));
#283487=CARTESIAN_POINT('Ctrl Pts',(-5.81964169300006,15.2,-8.75083162500001));
#283488=CARTESIAN_POINT('Ctrl Pts',(-5.81964169300006,11.6,-8.75083162500001));
#283489=CARTESIAN_POINT('Ctrl Pts',(-5.81842524600006,15.2,-8.74957194100002));
#283490=CARTESIAN_POINT('Ctrl Pts',(-5.81842524600006,11.6,-8.74957194100002));
#283491=CARTESIAN_POINT('Ctrl Pts',(-5.81721521200006,15.2,-8.74831657400001));
#283492=CARTESIAN_POINT('Ctrl Pts',(-5.81721521200006,11.6,-8.74831657400001));
#283493=CARTESIAN_POINT('Ctrl Pts',(-5.81601159400006,15.2,-8.74706554600002));
#283494=CARTESIAN_POINT('Ctrl Pts',(-5.81601159400006,11.6,-8.74706554600002));
#283495=CARTESIAN_POINT('Ctrl Pts',(-5.81481439300005,15.2,-8.74581887800002));
#283496=CARTESIAN_POINT('Ctrl Pts',(-5.81481439300005,11.6,-8.74581887800002));
#283497=CARTESIAN_POINT('Ctrl Pts',(-5.81362361300005,15.2,-8.74457659100001));
#283498=CARTESIAN_POINT('Ctrl Pts',(-5.81362361300005,11.6,-8.74457659100001));
#283499=CARTESIAN_POINT('Ctrl Pts',(-5.81243925700006,15.2,-8.74333870700001));
#283500=CARTESIAN_POINT('Ctrl Pts',(-5.81243925700006,11.6,-8.74333870700001));
#283501=CARTESIAN_POINT('Ctrl Pts',(-5.81126132800006,15.2,-8.74210524800001));
#283502=CARTESIAN_POINT('Ctrl Pts',(-5.81126132800006,11.6,-8.74210524800001));
#283503=CARTESIAN_POINT('Ctrl Pts',(-5.81008982800006,15.2,-8.74087623600002));
#283504=CARTESIAN_POINT('Ctrl Pts',(-5.81008982800006,11.6,-8.74087623600002));
#283505=CARTESIAN_POINT('Ctrl Pts',(-5.80892476100006,15.2,-8.73965169300002));
#283506=CARTESIAN_POINT('Ctrl Pts',(-5.80892476100006,11.6,-8.73965169300002));
#283507=CARTESIAN_POINT('Ctrl Pts',(-5.80776612900006,15.2,-8.73843163900002));
#283508=CARTESIAN_POINT('Ctrl Pts',(-5.80776612900006,11.6,-8.73843163900002));
#283509=CARTESIAN_POINT('Ctrl Pts',(-5.80661393400006,15.2,-8.73721609800001));
#283510=CARTESIAN_POINT('Ctrl Pts',(-5.80661393400006,11.6,-8.73721609800001));
#283511=CARTESIAN_POINT('Ctrl Pts',(-5.80546818100006,15.2,-8.73600509300001));
#283512=CARTESIAN_POINT('Ctrl Pts',(-5.80546818100006,11.6,-8.73600509300001));
#283513=CARTESIAN_POINT('Ctrl Pts',(-5.80432887200006,15.2,-8.73479864500002));
#283514=CARTESIAN_POINT('Ctrl Pts',(-5.80432887200006,11.6,-8.73479864500002));
#283515=CARTESIAN_POINT('Ctrl Pts',(-5.80319600900006,15.2,-8.73359677600002));
#283516=CARTESIAN_POINT('Ctrl Pts',(-5.80319600900006,11.6,-8.73359677600002));
#283517=CARTESIAN_POINT('Ctrl Pts',(-5.80206959600006,15.2,-8.73239950900001));
#283518=CARTESIAN_POINT('Ctrl Pts',(-5.80206959600006,11.6,-8.73239950900001));
#283519=CARTESIAN_POINT('Ctrl Pts',(-5.80094963500006,15.2,-8.73120686600002));
#283520=CARTESIAN_POINT('Ctrl Pts',(-5.80094963500006,11.6,-8.73120686600002));
#283521=CARTESIAN_POINT('Ctrl Pts',(-5.79983612800006,15.2,-8.73001887100001));
#283522=CARTESIAN_POINT('Ctrl Pts',(-5.79983612800006,11.6,-8.73001887100001));
#283523=CARTESIAN_POINT('Ctrl Pts',(-5.79872908000006,15.2,-8.72883554600002));
#283524=CARTESIAN_POINT('Ctrl Pts',(-5.79872908000006,11.6,-8.72883554600002));
#283525=CARTESIAN_POINT('Ctrl Pts',(-5.79762849300006,15.2,-8.72765691300001));
#283526=CARTESIAN_POINT('Ctrl Pts',(-5.79762849300006,11.6,-8.72765691300001));
#283527=CARTESIAN_POINT('Ctrl Pts',(-5.79653437000006,15.2,-8.72648299600002));
#283528=CARTESIAN_POINT('Ctrl Pts',(-5.79653437000006,11.6,-8.72648299600002));
#283529=CARTESIAN_POINT('Ctrl Pts',(-5.79544671200006,15.2,-8.72531381700002));
#283530=CARTESIAN_POINT('Ctrl Pts',(-5.79544671200006,11.6,-8.72531381700002));
#283531=CARTESIAN_POINT('Ctrl Pts',(-5.79436552400006,15.2,-8.72414939900001));
#283532=CARTESIAN_POINT('Ctrl Pts',(-5.79436552400006,11.6,-8.72414939900001));
#283533=CARTESIAN_POINT('Ctrl Pts',(-5.79329080800006,15.2,-8.72298976600002));
#283534=CARTESIAN_POINT('Ctrl Pts',(-5.79329080800006,11.6,-8.72298976600002));
#283535=CARTESIAN_POINT('Ctrl Pts',(-5.79222256600006,15.2,-8.72183494100002));
#283536=CARTESIAN_POINT('Ctrl Pts',(-5.79222256600006,11.6,-8.72183494100002));
#283537=CARTESIAN_POINT('Ctrl Pts',(-5.79116080300006,15.2,-8.72068494800001));
#283538=CARTESIAN_POINT('Ctrl Pts',(-5.79116080300006,11.6,-8.72068494800001));
#283539=CARTESIAN_POINT('Ctrl Pts',(-5.79010551900006,15.2,-8.71953980900001));
#283540=CARTESIAN_POINT('Ctrl Pts',(-5.79010551900006,11.6,-8.71953980900001));
#283541=CARTESIAN_POINT('Ctrl Pts',(-5.78905671900006,15.2,-8.71839954800001));
#283542=CARTESIAN_POINT('Ctrl Pts',(-5.78905671900006,11.6,-8.71839954800001));
#283543=CARTESIAN_POINT('Ctrl Pts',(-5.78801440500006,15.2,-8.71726418900002));
#283544=CARTESIAN_POINT('Ctrl Pts',(-5.78801440500006,11.6,-8.71726418900002));
#283545=CARTESIAN_POINT('Ctrl Pts',(-5.78697858000006,15.2,-8.71613375700001));
#283546=CARTESIAN_POINT('Ctrl Pts',(-5.78697858000006,11.6,-8.71613375700001));
#283547=CARTESIAN_POINT('Ctrl Pts',(-5.78594924700006,15.2,-8.71500827300002));
#283548=CARTESIAN_POINT('Ctrl Pts',(-5.78594924700006,11.6,-8.71500827300002));
#283549=CARTESIAN_POINT('Ctrl Pts',(-5.78492640800006,15.2,-8.71388776300002));
#283550=CARTESIAN_POINT('Ctrl Pts',(-5.78492640800006,11.6,-8.71388776300002));
#283551=CARTESIAN_POINT('Ctrl Pts',(-5.78391006700006,15.2,-8.71277225000001));
#283552=CARTESIAN_POINT('Ctrl Pts',(-5.78391006700006,11.6,-8.71277225000001));
#283553=CARTESIAN_POINT('Ctrl Pts',(-5.78290022600005,15.2,-8.71166175800001));
#283554=CARTESIAN_POINT('Ctrl Pts',(-5.78290022600005,11.6,-8.71166175800001));
#283555=CARTESIAN_POINT('Ctrl Pts',(-5.78189688700006,15.2,-8.71055631200001));
#283556=CARTESIAN_POINT('Ctrl Pts',(-5.78189688700006,11.6,-8.71055631200001));
#283557=CARTESIAN_POINT('Ctrl Pts',(-5.78090005400006,15.2,-8.70945593700002));
#283558=CARTESIAN_POINT('Ctrl Pts',(-5.78090005400006,11.6,-8.70945593700002));
#283559=CARTESIAN_POINT('Ctrl Pts',(-5.77990973100006,15.2,-8.70836065500002));
#283560=CARTESIAN_POINT('Ctrl Pts',(-5.77990973100006,11.6,-8.70836065500002));
#283561=CARTESIAN_POINT('Ctrl Pts',(-5.77892591700006,15.2,-8.70727049300001));
#283562=CARTESIAN_POINT('Ctrl Pts',(-5.77892591700006,11.6,-8.70727049300001));
#283563=CARTESIAN_POINT('Ctrl Pts',(-5.77794861800006,15.2,-8.70618547500002));
#283564=CARTESIAN_POINT('Ctrl Pts',(-5.77794861800006,11.6,-8.70618547500002));
#283565=CARTESIAN_POINT('Ctrl Pts',(-5.77697783600006,15.2,-8.70510562400002));
#283566=CARTESIAN_POINT('Ctrl Pts',(-5.77697783600006,11.6,-8.70510562400002));
#283567=CARTESIAN_POINT('Ctrl Pts',(-5.77601357300006,15.2,-8.70403096700001));
#283568=CARTESIAN_POINT('Ctrl Pts',(-5.77601357300006,11.6,-8.70403096700001));
#283569=CARTESIAN_POINT('Ctrl Pts',(-5.77505583400006,15.2,-8.70296152800002));
#283570=CARTESIAN_POINT('Ctrl Pts',(-5.77505583400006,11.6,-8.70296152800002));
#283571=CARTESIAN_POINT('Ctrl Pts',(-5.77410461900006,15.2,-8.70189733200002));
#283572=CARTESIAN_POINT('Ctrl Pts',(-5.77410461900006,11.6,-8.70189733200002));
#283573=CARTESIAN_POINT('Ctrl Pts',(-5.77315993200005,15.2,-8.70083840400002));
#283574=CARTESIAN_POINT('Ctrl Pts',(-5.77315993200005,11.6,-8.70083840400002));
#283575=CARTESIAN_POINT('Ctrl Pts',(-5.77222177600006,15.2,-8.69978477000002));
#283576=CARTESIAN_POINT('Ctrl Pts',(-5.77222177600006,11.6,-8.69978477000002));
#283577=CARTESIAN_POINT('Ctrl Pts',(-5.77129015400006,15.2,-8.69873645500002));
#283578=CARTESIAN_POINT('Ctrl Pts',(-5.77129015400006,11.6,-8.69873645500002));
#283579=CARTESIAN_POINT('Ctrl Pts',(-5.77036506700006,15.2,-8.69769348400002));
#283580=CARTESIAN_POINT('Ctrl Pts',(-5.77036506700006,11.6,-8.69769348400002));
#283581=CARTESIAN_POINT('Ctrl Pts',(-5.76944652100006,15.2,-8.69665588300002));
#283582=CARTESIAN_POINT('Ctrl Pts',(-5.76944652100006,11.6,-8.69665588300002));
#283583=CARTESIAN_POINT('Ctrl Pts',(-5.76853451500006,15.2,-8.69562367700001));
#283584=CARTESIAN_POINT('Ctrl Pts',(-5.76853451500006,11.6,-8.69562367700001));
#283585=CARTESIAN_POINT('Ctrl Pts',(-5.76762905500006,15.2,-8.69459689400001));
#283586=CARTESIAN_POINT('Ctrl Pts',(-5.76762905500006,11.6,-8.69459689400001));
#283587=CARTESIAN_POINT('Ctrl Pts',(-5.76673014200006,15.2,-8.69357555700002));
#283588=CARTESIAN_POINT('Ctrl Pts',(-5.76673014200006,11.6,-8.69357555700002));
#283589=CARTESIAN_POINT('Ctrl Pts',(-5.76583777900006,15.2,-8.69255969400001));
#283590=CARTESIAN_POINT('Ctrl Pts',(-5.76583777900006,11.6,-8.69255969400001));
#283591=CARTESIAN_POINT('Ctrl Pts',(-5.76495197000006,15.2,-8.69154933000001));
#283592=CARTESIAN_POINT('Ctrl Pts',(-5.76495197000006,11.6,-8.69154933000001));
#283593=CARTESIAN_POINT('Ctrl Pts',(-5.76407271500006,15.2,-8.69054449200001));
#283594=CARTESIAN_POINT('Ctrl Pts',(-5.76407271500006,11.6,-8.69054449200001));
#283595=CARTESIAN_POINT('Ctrl Pts',(-5.76320002000006,15.2,-8.68954520600001));
#283596=CARTESIAN_POINT('Ctrl Pts',(-5.76320002000006,11.6,-8.68954520600001));
#283597=CARTESIAN_POINT('Ctrl Pts',(-5.76233388600006,15.2,-8.68855149800002));
#283598=CARTESIAN_POINT('Ctrl Pts',(-5.76233388600006,11.6,-8.68855149800002));
#283599=CARTESIAN_POINT('Ctrl Pts',(-5.76147431600006,15.2,-8.68756339600001));
#283600=CARTESIAN_POINT('Ctrl Pts',(-5.76147431600006,11.6,-8.68756339600001));
#283601=CARTESIAN_POINT('Ctrl Pts',(-5.76062131200006,15.2,-8.68658092600001));
#283602=CARTESIAN_POINT('Ctrl Pts',(-5.76062131200006,11.6,-8.68658092600001));
#283603=CARTESIAN_POINT('Ctrl Pts',(-5.75977487800006,15.2,-8.68560411500002));
#283604=CARTESIAN_POINT('Ctrl Pts',(-5.75977487800006,11.6,-8.68560411500002));
#283605=CARTESIAN_POINT('Ctrl Pts',(-5.75893501600006,15.2,-8.68463298900001));
#283606=CARTESIAN_POINT('Ctrl Pts',(-5.75893501600006,11.6,-8.68463298900001));
#283607=CARTESIAN_POINT('Ctrl Pts',(-5.75810173000006,15.2,-8.68366757600001));
#283608=CARTESIAN_POINT('Ctrl Pts',(-5.75810173000006,11.6,-8.68366757600001));
#283609=CARTESIAN_POINT('Ctrl Pts',(-5.75727502100006,15.2,-8.68270790200001));
#283610=CARTESIAN_POINT('Ctrl Pts',(-5.75727502100006,11.6,-8.68270790200001));
#283611=CARTESIAN_POINT('Ctrl Pts',(-5.75645489300006,15.2,-8.68175399800002));
#283612=CARTESIAN_POINT('Ctrl Pts',(-5.75645489300006,11.6,-8.68175399800002));
#283613=CARTESIAN_POINT('Ctrl Pts',(-5.75564134700006,15.2,-8.68080588500002));
#283614=CARTESIAN_POINT('Ctrl Pts',(-5.75564134700006,11.6,-8.68080588500002));
#283615=CARTESIAN_POINT('Ctrl Pts',(-5.75483438800005,15.2,-8.67986359700001));
#283616=CARTESIAN_POINT('Ctrl Pts',(-5.75483438800005,11.6,-8.67986359700001));
#283617=CARTESIAN_POINT('Ctrl Pts',(-5.75403401900005,15.2,-8.67892715900001));
#283618=CARTESIAN_POINT('Ctrl Pts',(-5.75403401900005,11.6,-8.67892715900001));
#283619=CARTESIAN_POINT('Ctrl Pts',(-5.75324024000006,15.2,-8.67799659800001));
#283620=CARTESIAN_POINT('Ctrl Pts',(-5.75324024000006,11.6,-8.67799659800001));
#283621=CARTESIAN_POINT('Ctrl Pts',(-5.75245305600006,15.2,-8.67707194200002));
#283622=CARTESIAN_POINT('Ctrl Pts',(-5.75245305600006,11.6,-8.67707194200002));
#283623=CARTESIAN_POINT('Ctrl Pts',(-5.75167246900006,15.2,-8.67615322100002));
#283624=CARTESIAN_POINT('Ctrl Pts',(-5.75167246900006,11.6,-8.67615322100002));
#283625=CARTESIAN_POINT('Ctrl Pts',(-5.75089848100006,15.2,-8.67524046100002));
#283626=CARTESIAN_POINT('Ctrl Pts',(-5.75089848100006,11.6,-8.67524046100002));
#283627=CARTESIAN_POINT('Ctrl Pts',(-5.75013109600006,15.2,-8.67433369300001));
#283628=CARTESIAN_POINT('Ctrl Pts',(-5.75013109600006,11.6,-8.67433369300001));
#283629=CARTESIAN_POINT('Ctrl Pts',(-5.74937031600006,15.2,-8.67343294300002));
#283630=CARTESIAN_POINT('Ctrl Pts',(-5.74937031600006,11.6,-8.67343294300002));
#283631=CARTESIAN_POINT('Ctrl Pts',(-5.74861614500006,15.2,-8.67253824000001));
#283632=CARTESIAN_POINT('Ctrl Pts',(-5.74861614500006,11.6,-8.67253824000001));
#283633=CARTESIAN_POINT('Ctrl Pts',(-5.74786858400006,15.2,-8.67164961300002));
#283634=CARTESIAN_POINT('Ctrl Pts',(-5.74786858400006,11.6,-8.67164961300002));
#283635=CARTESIAN_POINT('Ctrl Pts',(-5.74712763600006,15.2,-8.67076709200001));
#283636=CARTESIAN_POINT('Ctrl Pts',(-5.74712763600006,11.6,-8.67076709200001));
#283637=CARTESIAN_POINT('Ctrl Pts',(-5.74639330500006,15.2,-8.66989070400002));
#283638=CARTESIAN_POINT('Ctrl Pts',(-5.74639330500006,11.6,-8.66989070400002));
#283639=CARTESIAN_POINT('Ctrl Pts',(-5.74566559300006,15.2,-8.66902047900002));
#283640=CARTESIAN_POINT('Ctrl Pts',(-5.74566559300006,11.6,-8.66902047900002));
#283641=CARTESIAN_POINT('Ctrl Pts',(-5.74494450300006,15.2,-8.66815644700001));
#283642=CARTESIAN_POINT('Ctrl Pts',(-5.74494450300006,11.6,-8.66815644700001));
#283643=CARTESIAN_POINT('Ctrl Pts',(-5.74423003600006,15.2,-8.66729863600002));
#283644=CARTESIAN_POINT('Ctrl Pts',(-5.74423003600006,11.6,-8.66729863600002));
#283645=CARTESIAN_POINT('Ctrl Pts',(-5.74352219700006,15.2,-8.66644707700001));
#283646=CARTESIAN_POINT('Ctrl Pts',(-5.74352219700006,11.6,-8.66644707700001));
#283647=CARTESIAN_POINT('Ctrl Pts',(-5.74282098800006,15.2,-8.66560180000001));
#283648=CARTESIAN_POINT('Ctrl Pts',(-5.74282098800006,11.6,-8.66560180000001));
#283649=CARTESIAN_POINT('Ctrl Pts',(-5.74212641100006,15.2,-8.66476283200001));
#283650=CARTESIAN_POINT('Ctrl Pts',(-5.74212641100006,11.6,-8.66476283200001));
#283651=CARTESIAN_POINT('Ctrl Pts',(-5.74143847000006,15.2,-8.66393020500002));
#283652=CARTESIAN_POINT('Ctrl Pts',(-5.74143847000006,11.6,-8.66393020500002));
#283653=CARTESIAN_POINT('Ctrl Pts',(-5.74075716700006,15.2,-8.66310395100001));
#283654=CARTESIAN_POINT('Ctrl Pts',(-5.74075716700006,11.6,-8.66310395100001));
#283655=CARTESIAN_POINT('Ctrl Pts',(-5.74008250400006,15.2,-8.66228409600001));
#283656=CARTESIAN_POINT('Ctrl Pts',(-5.74008250400006,11.6,-8.66228409600001));
#283657=CARTESIAN_POINT('Ctrl Pts',(-5.73941448500006,15.2,-8.66147067400002));
#283658=CARTESIAN_POINT('Ctrl Pts',(-5.73941448500006,11.6,-8.66147067400002));
#283659=CARTESIAN_POINT('Ctrl Pts',(-5.73875311300006,15.2,-8.66066371300001));
#283660=CARTESIAN_POINT('Ctrl Pts',(-5.73875311300006,11.6,-8.66066371300001));
#283661=CARTESIAN_POINT('Ctrl Pts',(-5.73809838900006,15.2,-8.65986324600001));
#283662=CARTESIAN_POINT('Ctrl Pts',(-5.73809838900006,11.6,-8.65986324600001));
#283663=CARTESIAN_POINT('Ctrl Pts',(-5.73745031600006,15.2,-8.65906930200002));
#283664=CARTESIAN_POINT('Ctrl Pts',(-5.73745031600006,11.6,-8.65906930200002));
#283665=CARTESIAN_POINT('Ctrl Pts',(-5.73680889900006,15.2,-8.65828191300002));
#283666=CARTESIAN_POINT('Ctrl Pts',(-5.73680889900006,11.6,-8.65828191300002));
#283667=CARTESIAN_POINT('Ctrl Pts',(-5.73617413900006,15.2,-8.65750111000001));
#283668=CARTESIAN_POINT('Ctrl Pts',(-5.73617413900006,11.6,-8.65750111000001));
#283669=CARTESIAN_POINT('Ctrl Pts',(-5.73554603700006,15.2,-8.65672692500001));
#283670=CARTESIAN_POINT('Ctrl Pts',(-5.73554603700006,11.6,-8.65672692500001));
#283671=CARTESIAN_POINT('Ctrl Pts',(-5.73492459900006,15.2,-8.65595938700002));
#283672=CARTESIAN_POINT('Ctrl Pts',(-5.73492459900006,11.6,-8.65595938700002));
#283673=CARTESIAN_POINT('Ctrl Pts',(-5.73430982600006,15.2,-8.65519853100002));
#283674=CARTESIAN_POINT('Ctrl Pts',(-5.73430982600006,11.6,-8.65519853100002));
#283675=CARTESIAN_POINT('Ctrl Pts',(-5.73370172100006,15.2,-8.65444438600001));
#283676=CARTESIAN_POINT('Ctrl Pts',(-5.73370172100006,11.6,-8.65444438600001));
#283677=CARTESIAN_POINT('Ctrl Pts',(-5.73310028700006,15.2,-8.65369698500002));
#283678=CARTESIAN_POINT('Ctrl Pts',(-5.73310028700006,11.6,-8.65369698500002));
#283679=CARTESIAN_POINT('Ctrl Pts',(-5.73250552600006,15.2,-8.65295636100001));
#283680=CARTESIAN_POINT('Ctrl Pts',(-5.73250552600006,11.6,-8.65295636100001));
#283681=CARTESIAN_POINT('Ctrl Pts',(-5.73191744100006,15.2,-8.65222254500001));
#283682=CARTESIAN_POINT('Ctrl Pts',(-5.73191744100006,11.6,-8.65222254500001));
#283683=CARTESIAN_POINT('Ctrl Pts',(-5.73133603500006,15.2,-8.65149557000001));
#283684=CARTESIAN_POINT('Ctrl Pts',(-5.73133603500006,11.6,-8.65149557000001));
#283685=CARTESIAN_POINT('Ctrl Pts',(-5.73076462000006,15.2,-8.65077961500001));
#283686=CARTESIAN_POINT('Ctrl Pts',(-5.73076462000006,11.6,-8.65077961500001));
#283687=CARTESIAN_POINT('Ctrl Pts',(-5.73031342200006,15.2,-8.65021312700001));
#283688=CARTESIAN_POINT('Ctrl Pts',(-5.73031342200006,11.6,-8.65021312700001));
#283689=CARTESIAN_POINT('Ctrl Pts',(-5.72997879300006,15.2,-8.64979235000002));
#283690=CARTESIAN_POINT('Ctrl Pts',(-5.72997879300006,11.6,-8.64979235000002));
#283691=CARTESIAN_POINT('Ctrl Pts',(-5.72975808700006,15.2,-8.64951454400002));
#283692=CARTESIAN_POINT('Ctrl Pts',(-5.72975808700006,11.6,-8.64951454400002));
#283693=CARTESIAN_POINT('Ctrl Pts',(-5.72964966100006,15.2,-8.64937799900002));
#283694=CARTESIAN_POINT('Ctrl Pts',(-5.72964966100006,11.6,-8.64937799900002));
#283695=CARTESIAN_POINT('',(-5.72964966108803,12.2,-8.64937799846615));
#283696=CARTESIAN_POINT('',(-5.72964966108803,15.2,-8.64937799846615));
#283697=CARTESIAN_POINT('',(-5.72964966100006,12.2,-8.64937799800002));
#283698=CARTESIAN_POINT('Ctrl Pts',(-6.67046385600006,12.2,-9.36775917400002));
#283699=CARTESIAN_POINT('Ctrl Pts',(-6.66979226100006,12.2,-9.36739373000002));
#283700=CARTESIAN_POINT('Ctrl Pts',(-6.66844959800006,12.2,-9.36666279600002));
#283701=CARTESIAN_POINT('Ctrl Pts',(-6.66643717700006,12.2,-9.36556627000002));
#283702=CARTESIAN_POINT('Ctrl Pts',(-6.66375709900006,12.2,-9.36410398400002));
#283703=CARTESIAN_POINT('Ctrl Pts',(-6.66041225200006,12.2,-9.36227570600002));
#283704=CARTESIAN_POINT('Ctrl Pts',(-6.65707265500005,12.2,-9.36044701000002));
#283705=CARTESIAN_POINT('Ctrl Pts',(-6.65373831000006,12.2,-9.35861789600001));
#283706=CARTESIAN_POINT('Ctrl Pts',(-6.65040921900006,12.2,-9.35678837000001));
#283707=CARTESIAN_POINT('Ctrl Pts',(-6.64708538300006,12.2,-9.35495843700001));
#283708=CARTESIAN_POINT('Ctrl Pts',(-6.64376680700006,12.2,-9.35312810300001));
#283709=CARTESIAN_POINT('Ctrl Pts',(-6.64045349300006,12.2,-9.35129737900001));
#283710=CARTESIAN_POINT('Ctrl Pts',(-6.63714544700006,12.2,-9.34946627300001));
#283711=CARTESIAN_POINT('Ctrl Pts',(-6.63384267100006,12.2,-9.34763479700001));
#283712=CARTESIAN_POINT('Ctrl Pts',(-6.63054517000006,12.2,-9.34580296000001));
#283713=CARTESIAN_POINT('Ctrl Pts',(-6.62725294900006,12.2,-9.34397077300002));
#283714=CARTESIAN_POINT('Ctrl Pts',(-6.62396601100006,12.2,-9.34213824300001));
#283715=CARTESIAN_POINT('Ctrl Pts',(-6.62068436000006,12.2,-9.34030538000002));
#283716=CARTESIAN_POINT('Ctrl Pts',(-6.61740799800006,12.2,-9.33847218900001));
#283717=CARTESIAN_POINT('Ctrl Pts',(-6.61413692800005,12.2,-9.33663868000002));
#283718=CARTESIAN_POINT('Ctrl Pts',(-6.61087115500006,12.2,-9.33480485900001));
#283719=CARTESIAN_POINT('Ctrl Pts',(-6.60761068100006,12.2,-9.33297073500002));
#283720=CARTESIAN_POINT('Ctrl Pts',(-6.60435550800006,12.2,-9.33113631500002));
#283721=CARTESIAN_POINT('Ctrl Pts',(-6.60110564300005,12.2,-9.32930161000002));
#283722=CARTESIAN_POINT('Ctrl Pts',(-6.59786108600006,12.2,-9.32746662500002));
#283723=CARTESIAN_POINT('Ctrl Pts',(-6.59462184300006,12.2,-9.32563137200002));
#283724=CARTESIAN_POINT('Ctrl Pts',(-6.59138791700006,12.2,-9.32379585900001));
#283725=CARTESIAN_POINT('Ctrl Pts',(-6.58815931000006,12.2,-9.32196009500002));
#283726=CARTESIAN_POINT('Ctrl Pts',(-6.58493602700006,12.2,-9.32012408600002));
#283727=CARTESIAN_POINT('Ctrl Pts',(-6.58171807300006,12.2,-9.31828784500001));
#283728=CARTESIAN_POINT('Ctrl Pts',(-6.57850544800006,12.2,-9.31645137700002));
#283729=CARTESIAN_POINT('Ctrl Pts',(-6.57529815700006,12.2,-9.31461469100002));
#283730=CARTESIAN_POINT('Ctrl Pts',(-6.57209620400006,12.2,-9.31277779500002));
#283731=CARTESIAN_POINT('Ctrl Pts',(-6.56889959100006,12.2,-9.31094070000002));
#283732=CARTESIAN_POINT('Ctrl Pts',(-6.56570832300006,12.2,-9.30910341200001));
#283733=CARTESIAN_POINT('Ctrl Pts',(-6.56252240200006,12.2,-9.30726594200002));
#283734=CARTESIAN_POINT('Ctrl Pts',(-6.55934183200006,12.2,-9.30542829500002));
#283735=CARTESIAN_POINT('Ctrl Pts',(-6.55616661700006,12.2,-9.30359048400001));
#283736=CARTESIAN_POINT('Ctrl Pts',(-6.55299676000006,12.2,-9.30175251500001));
#283737=CARTESIAN_POINT('Ctrl Pts',(-6.54983226500006,12.2,-9.29991439900002));
#283738=CARTESIAN_POINT('Ctrl Pts',(-6.54667313400005,12.2,-9.29807614200002));
#283739=CARTESIAN_POINT('Ctrl Pts',(-6.54351937200006,12.2,-9.29623775500002));
#283740=CARTESIAN_POINT('Ctrl Pts',(-6.54037098100006,12.2,-9.29439924500001));
#283741=CARTESIAN_POINT('Ctrl Pts',(-6.53722796600006,12.2,-9.29256062200002));
#283742=CARTESIAN_POINT('Ctrl Pts',(-6.53409033000006,12.2,-9.29072189400001));
#283743=CARTESIAN_POINT('Ctrl Pts',(-6.53095807500006,12.2,-9.28888307000001));
#283744=CARTESIAN_POINT('Ctrl Pts',(-6.52783120600006,12.2,-9.28704416000001));
#283745=CARTESIAN_POINT('Ctrl Pts',(-6.52470972700006,12.2,-9.28520517200001));
#283746=CARTESIAN_POINT('Ctrl Pts',(-6.52159363900005,12.2,-9.28336611300002));
#283747=CARTESIAN_POINT('Ctrl Pts',(-6.51848294800006,12.2,-9.28152699600002));
#283748=CARTESIAN_POINT('Ctrl Pts',(-6.51537765500006,12.2,-9.27968782700002));
#283749=CARTESIAN_POINT('Ctrl Pts',(-6.51227776500006,12.2,-9.27784861500001));
#283750=CARTESIAN_POINT('Ctrl Pts',(-6.50918328200006,12.2,-9.27600936900001));
#283751=CARTESIAN_POINT('Ctrl Pts',(-6.50609420700006,12.2,-9.27417010000001));
#283752=CARTESIAN_POINT('Ctrl Pts',(-6.50301054600006,12.2,-9.27233081400002));
#283753=CARTESIAN_POINT('Ctrl Pts',(-6.49993230100006,12.2,-9.27049152200001));
#283754=CARTESIAN_POINT('Ctrl Pts',(-6.49685947500006,12.2,-9.26865223300002));
#283755=CARTESIAN_POINT('Ctrl Pts',(-6.49379207300006,12.2,-9.26681295500002));
#283756=CARTESIAN_POINT('Ctrl Pts',(-6.49073009700006,12.2,-9.26497369800002));
#283757=CARTESIAN_POINT('Ctrl Pts',(-6.48767355200006,12.2,-9.26313447100001));
#283758=CARTESIAN_POINT('Ctrl Pts',(-6.48462244000005,12.2,-9.26129528200001));
#283759=CARTESIAN_POINT('Ctrl Pts',(-6.48157676400006,12.2,-9.25945614200002));
#283760=CARTESIAN_POINT('Ctrl Pts',(-6.47853652900006,12.2,-9.25761705800002));
#283761=CARTESIAN_POINT('Ctrl Pts',(-6.47550173800005,12.2,-9.25577804100002));
#283762=CARTESIAN_POINT('Ctrl Pts',(-6.47247239300006,12.2,-9.25393910000002));
#283763=CARTESIAN_POINT('Ctrl Pts',(-6.46944849900006,12.2,-9.25210024200002));
#283764=CARTESIAN_POINT('Ctrl Pts',(-6.46643005900006,12.2,-9.25026147900001));
#283765=CARTESIAN_POINT('Ctrl Pts',(-6.46341707600006,12.2,-9.24842281800002));
#283766=CARTESIAN_POINT('Ctrl Pts',(-6.46040955400006,12.2,-9.24658427100002));
#283767=CARTESIAN_POINT('Ctrl Pts',(-6.45740749600006,12.2,-9.24474584400001));
#283768=CARTESIAN_POINT('Ctrl Pts',(-6.45441090500006,12.2,-9.24290754900002));
#283769=CARTESIAN_POINT('Ctrl Pts',(-6.45141978500006,12.2,-9.24106939400002));
#283770=CARTESIAN_POINT('Ctrl Pts',(-6.44843413900006,12.2,-9.23923138800001));
#283771=CARTESIAN_POINT('Ctrl Pts',(-6.44545397200006,12.2,-9.23739354200002));
#283772=CARTESIAN_POINT('Ctrl Pts',(-6.44247928500006,12.2,-9.23555586400001));
#283773=CARTESIAN_POINT('Ctrl Pts',(-6.43951008200006,12.2,-9.23371836400002));
#283774=CARTESIAN_POINT('Ctrl Pts',(-6.43654636800005,12.2,-9.23188105000002));
#283775=CARTESIAN_POINT('Ctrl Pts',(-6.43358814400006,12.2,-9.23004393300002));
#283776=CARTESIAN_POINT('Ctrl Pts',(-6.43063541500006,12.2,-9.22820702200001));
#283777=CARTESIAN_POINT('Ctrl Pts',(-6.42768818400006,12.2,-9.22637032800001));
#283778=CARTESIAN_POINT('Ctrl Pts',(-6.42474645500006,12.2,-9.22453385700001));
#283779=CARTESIAN_POINT('Ctrl Pts',(-6.42181023000005,12.2,-9.22269762200001));
#283780=CARTESIAN_POINT('Ctrl Pts',(-6.41887951300006,12.2,-9.22086163100002));
#283781=CARTESIAN_POINT('Ctrl Pts',(-6.41595430900006,12.2,-9.21902589200002));
#283782=CARTESIAN_POINT('Ctrl Pts',(-6.41303461900006,12.2,-9.21719041800002));
#283783=CARTESIAN_POINT('Ctrl Pts',(-6.41012044700005,12.2,-9.21535521600001));
#283784=CARTESIAN_POINT('Ctrl Pts',(-6.40721179700006,12.2,-9.21352029700002));
#283785=CARTESIAN_POINT('Ctrl Pts',(-6.40430867200006,12.2,-9.21168566900001));
#283786=CARTESIAN_POINT('Ctrl Pts',(-6.40141107500006,12.2,-9.20985134500001));
#283787=CARTESIAN_POINT('Ctrl Pts',(-6.39851901000006,12.2,-9.20801733000001));
#283788=CARTESIAN_POINT('Ctrl Pts',(-6.39563248000006,12.2,-9.20618363800001));
#283789=CARTESIAN_POINT('Ctrl Pts',(-6.39275149000006,12.2,-9.20435027600002));
#283790=CARTESIAN_POINT('Ctrl Pts',(-6.38987604000006,12.2,-9.20251725400002));
#283791=CARTESIAN_POINT('Ctrl Pts',(-6.38700613600006,12.2,-9.20068458400002));
#283792=CARTESIAN_POINT('Ctrl Pts',(-6.38414178100006,12.2,-9.19885227300002));
#283793=CARTESIAN_POINT('Ctrl Pts',(-6.38128297700006,12.2,-9.19702033200002));
#283794=CARTESIAN_POINT('Ctrl Pts',(-6.37842973000006,12.2,-9.19518877200002));
#283795=CARTESIAN_POINT('Ctrl Pts',(-6.37558204100006,12.2,-9.19335760100001));
#283796=CARTESIAN_POINT('Ctrl Pts',(-6.37273991300006,12.2,-9.19152682900001));
#283797=CARTESIAN_POINT('Ctrl Pts',(-6.36990335200006,12.2,-9.18969646800001));
#283798=CARTESIAN_POINT('Ctrl Pts',(-6.36707236000006,12.2,-9.18786652500001));
#283799=CARTESIAN_POINT('Ctrl Pts',(-6.36424693800006,12.2,-9.18603701200002));
#283800=CARTESIAN_POINT('Ctrl Pts',(-6.36142709400006,12.2,-9.18420793900001));
#283801=CARTESIAN_POINT('Ctrl Pts',(-6.35861282700006,12.2,-9.18237931400002));
#283802=CARTESIAN_POINT('Ctrl Pts',(-6.35580414300006,12.2,-9.18055114900002));
#283803=CARTESIAN_POINT('Ctrl Pts',(-6.35300104500006,12.2,-9.17872345400001));
#283804=CARTESIAN_POINT('Ctrl Pts',(-6.35020353500006,12.2,-9.17689623700002));
#283805=CARTESIAN_POINT('Ctrl Pts',(-6.34741161800005,12.2,-9.17506951100002));
#283806=CARTESIAN_POINT('Ctrl Pts',(-6.34462529700006,12.2,-9.17324328400002));
#283807=CARTESIAN_POINT('Ctrl Pts',(-6.34184457400006,12.2,-9.17141756700002));
#283808=CARTESIAN_POINT('Ctrl Pts',(-6.33906945400006,12.2,-9.16959237000002));
#283809=CARTESIAN_POINT('Ctrl Pts',(-6.33629993900006,12.2,-9.16776770200002));
#283810=CARTESIAN_POINT('Ctrl Pts',(-6.33353603400006,12.2,-9.16594357600001));
#283811=CARTESIAN_POINT('Ctrl Pts',(-6.33077774100006,12.2,-9.16411999900001));
#283812=CARTESIAN_POINT('Ctrl Pts',(-6.32802506300005,12.2,-9.16229698300001));
#283813=CARTESIAN_POINT('Ctrl Pts',(-6.32527800500006,12.2,-9.16047453800001));
#283814=CARTESIAN_POINT('Ctrl Pts',(-6.32253656800006,12.2,-9.15865267500001));
#283815=CARTESIAN_POINT('Ctrl Pts',(-6.31980075800006,12.2,-9.15683140300001));
#283816=CARTESIAN_POINT('Ctrl Pts',(-6.31707057700006,12.2,-9.15501073400002));
#283817=CARTESIAN_POINT('Ctrl Pts',(-6.31434602800006,12.2,-9.15319067500001));
#283818=CARTESIAN_POINT('Ctrl Pts',(-6.31162711400005,12.2,-9.15137124000001));
#283819=CARTESIAN_POINT('Ctrl Pts',(-6.30891384000006,12.2,-9.14955243900001));
#283820=CARTESIAN_POINT('Ctrl Pts',(-6.30620620800006,12.2,-9.14773428000002));
#283821=CARTESIAN_POINT('Ctrl Pts',(-6.30350422100006,12.2,-9.14591677500002));
#283822=CARTESIAN_POINT('Ctrl Pts',(-6.30080788400006,12.2,-9.14409993500002));
#283823=CARTESIAN_POINT('Ctrl Pts',(-6.29811719900006,12.2,-9.14228377000001));
#283824=CARTESIAN_POINT('Ctrl Pts',(-6.29543217000006,12.2,-9.14046829000002));
#283825=CARTESIAN_POINT('Ctrl Pts',(-6.29275279900006,12.2,-9.13865350600001));
#283826=CARTESIAN_POINT('Ctrl Pts',(-6.29007909100006,12.2,-9.13683942900001));
#283827=CARTESIAN_POINT('Ctrl Pts',(-6.28741104800006,12.2,-9.13502606900002));
#283828=CARTESIAN_POINT('Ctrl Pts',(-6.28474867400006,12.2,-9.13321343700002));
#283829=CARTESIAN_POINT('Ctrl Pts',(-6.28209197200006,12.2,-9.13140154300002));
#283830=CARTESIAN_POINT('Ctrl Pts',(-6.27944094700006,12.2,-9.12959039800001));
#283831=CARTESIAN_POINT('Ctrl Pts',(-6.27679559900006,12.2,-9.12778001300002));
#283832=CARTESIAN_POINT('Ctrl Pts',(-6.27415593500006,12.2,-9.12597039800002));
#283833=CARTESIAN_POINT('Ctrl Pts',(-6.27152195600006,12.2,-9.12416156500001));
#283834=CARTESIAN_POINT('Ctrl Pts',(-6.26889366400006,12.2,-9.12235352300002));
#283835=CARTESIAN_POINT('Ctrl Pts',(-6.26627106600006,12.2,-9.12054628500002));
#283836=CARTESIAN_POINT('Ctrl Pts',(-6.26365416200006,12.2,-9.11873986000002));
#283837=CARTESIAN_POINT('Ctrl Pts',(-6.26104295800006,12.2,-9.11693426000001));
#283838=CARTESIAN_POINT('Ctrl Pts',(-6.25843745500006,12.2,-9.11512949500001));
#283839=CARTESIAN_POINT('Ctrl Pts',(-6.25583765700005,12.2,-9.11332557600002));
#283840=CARTESIAN_POINT('Ctrl Pts',(-6.25324356800006,12.2,-9.11152251400001));
#283841=CARTESIAN_POINT('Ctrl Pts',(-6.25065519100006,12.2,-9.10972032100002));
#283842=CARTESIAN_POINT('Ctrl Pts',(-6.24807252900006,12.2,-9.10791900700002));
#283843=CARTESIAN_POINT('Ctrl Pts',(-6.24549558500005,12.2,-9.10611858200001));
#283844=CARTESIAN_POINT('Ctrl Pts',(-6.24292436400006,12.2,-9.10431905900002));
#283845=CARTESIAN_POINT('Ctrl Pts',(-6.24035886600006,12.2,-9.10252044800002));
#283846=CARTESIAN_POINT('Ctrl Pts',(-6.23779909800006,12.2,-9.10072276100001));
#283847=CARTESIAN_POINT('Ctrl Pts',(-6.23524506100006,12.2,-9.09892600700001));
#283848=CARTESIAN_POINT('Ctrl Pts',(-6.23269675900006,12.2,-9.09713019900002));
#283849=CARTESIAN_POINT('Ctrl Pts',(-6.23015419600006,12.2,-9.09533534700002));
#283850=CARTESIAN_POINT('Ctrl Pts',(-6.22761737300006,12.2,-9.09354146400002));
#283851=CARTESIAN_POINT('Ctrl Pts',(-6.22508629500006,12.2,-9.09174855900002));
#283852=CARTESIAN_POINT('Ctrl Pts',(-6.22256096500006,12.2,-9.08995664500001));
#283853=CARTESIAN_POINT('Ctrl Pts',(-6.22004138600006,12.2,-9.08816573200001));
#283854=CARTESIAN_POINT('Ctrl Pts',(-6.21752756200006,12.2,-9.08637583200001));
#283855=CARTESIAN_POINT('Ctrl Pts',(-6.21501949600006,12.2,-9.08458695700002));
#283856=CARTESIAN_POINT('Ctrl Pts',(-6.21251719100006,12.2,-9.08279911600001));
#283857=CARTESIAN_POINT('Ctrl Pts',(-6.21002065000006,12.2,-9.08101232300002));
#283858=CARTESIAN_POINT('Ctrl Pts',(-6.20752987700006,12.2,-9.07922658700001));
#283859=CARTESIAN_POINT('Ctrl Pts',(-6.20504487400006,12.2,-9.07744192200001));
#283860=CARTESIAN_POINT('Ctrl Pts',(-6.20256564600006,12.2,-9.07565833800002));
#283861=CARTESIAN_POINT('Ctrl Pts',(-6.20009219500006,12.2,-9.07387584600002));
#283862=CARTESIAN_POINT('Ctrl Pts',(-6.19762452500006,12.2,-9.07209445800002));
#283863=CARTESIAN_POINT('Ctrl Pts',(-6.19516263900006,12.2,-9.07031418600001));
#283864=CARTESIAN_POINT('Ctrl Pts',(-6.19270653900006,12.2,-9.06853504200001));
#283865=CARTESIAN_POINT('Ctrl Pts',(-6.19025623000006,12.2,-9.06675703600002));
#283866=CARTESIAN_POINT('Ctrl Pts',(-6.18781171500006,12.2,-9.06498018100002));
#283867=CARTESIAN_POINT('Ctrl Pts',(-6.18537299700006,12.2,-9.06320448700002));
#283868=CARTESIAN_POINT('Ctrl Pts',(-6.18294008000006,12.2,-9.06142996800002));
#283869=CARTESIAN_POINT('Ctrl Pts',(-6.18051296500005,12.2,-9.05965663400002));
#283870=CARTESIAN_POINT('Ctrl Pts',(-6.17809165700006,12.2,-9.05788449800001));
#283871=CARTESIAN_POINT('Ctrl Pts',(-6.17567615900006,12.2,-9.05611357000002));
#283872=CARTESIAN_POINT('Ctrl Pts',(-6.17326647500006,12.2,-9.05434386300002));
#283873=CARTESIAN_POINT('Ctrl Pts',(-6.17086260700006,12.2,-9.05257538800001));
#283874=CARTESIAN_POINT('Ctrl Pts',(-6.16846455700006,12.2,-9.05080815900002));
#283875=CARTESIAN_POINT('Ctrl Pts',(-6.16607233200006,12.2,-9.04904218600001));
#283876=CARTESIAN_POINT('Ctrl Pts',(-6.16368593200006,12.2,-9.04727748100001));
#283877=CARTESIAN_POINT('Ctrl Pts',(-6.16130536200005,12.2,-9.04551405600002));
#283878=CARTESIAN_POINT('Ctrl Pts',(-6.15893062400006,12.2,-9.04375192400002));
#283879=CARTESIAN_POINT('Ctrl Pts',(-6.15656172200006,12.2,-9.04199109600002));
#283880=CARTESIAN_POINT('Ctrl Pts',(-6.15419866000006,12.2,-9.04023158300001));
#283881=CARTESIAN_POINT('Ctrl Pts',(-6.15184143900006,12.2,-9.03847340000001));
#283882=CARTESIAN_POINT('Ctrl Pts',(-6.14949006400006,12.2,-9.03671655700002));
#283883=CARTESIAN_POINT('Ctrl Pts',(-6.14714453800006,12.2,-9.03496106700001));
#283884=CARTESIAN_POINT('Ctrl Pts',(-6.14480486400006,12.2,-9.03320694000002));
#283885=CARTESIAN_POINT('Ctrl Pts',(-6.14247104500006,12.2,-9.03145419100002));
#283886=CARTESIAN_POINT('Ctrl Pts',(-6.14014308400006,12.2,-9.02970283200002));
#283887=CARTESIAN_POINT('Ctrl Pts',(-6.13782098400006,12.2,-9.02795287300002));
#283888=CARTESIAN_POINT('Ctrl Pts',(-6.13550475100006,12.2,-9.02620432800001));
#283889=CARTESIAN_POINT('Ctrl Pts',(-6.13319438500006,12.2,-9.02445720900002));
#283890=CARTESIAN_POINT('Ctrl Pts',(-6.13088988900006,12.2,-9.02271152900001));
#283891=CARTESIAN_POINT('Ctrl Pts',(-6.12859126900006,12.2,-9.02096729900002));
#283892=CARTESIAN_POINT('Ctrl Pts',(-6.12629852600006,12.2,-9.01922453300001));
#283893=CARTESIAN_POINT('Ctrl Pts',(-6.12401166400006,12.2,-9.01748324100001));
#283894=CARTESIAN_POINT('Ctrl Pts',(-6.12173068600006,12.2,-9.01574343800002));
#283895=CARTESIAN_POINT('Ctrl Pts',(-6.11945559600006,12.2,-9.01400513500001));
#283896=CARTESIAN_POINT('Ctrl Pts',(-6.11718639600006,12.2,-9.01226834500001));
#283897=CARTESIAN_POINT('Ctrl Pts',(-6.11492309000006,12.2,-9.01053308200002));
#283898=CARTESIAN_POINT('Ctrl Pts',(-6.11266568000006,12.2,-9.00879935600001));
#283899=CARTESIAN_POINT('Ctrl Pts',(-6.11041417200005,12.2,-9.00706718000002));
#283900=CARTESIAN_POINT('Ctrl Pts',(-6.10816856500006,12.2,-9.00533656900001));
#283901=CARTESIAN_POINT('Ctrl Pts',(-6.10592886600006,12.2,-9.00360753300001));
#283902=CARTESIAN_POINT('Ctrl Pts',(-6.10369507600006,12.2,-9.00188008700002));
#283903=CARTESIAN_POINT('Ctrl Pts',(-6.10146719900006,12.2,-9.00015424200001));
#283904=CARTESIAN_POINT('Ctrl Pts',(-6.09924523800006,12.2,-8.99843001200002));
#283905=CARTESIAN_POINT('Ctrl Pts',(-6.09702919700006,12.2,-8.99670741000002));
#283906=CARTESIAN_POINT('Ctrl Pts',(-6.09481907700006,12.2,-8.99498644800002));
#283907=CARTESIAN_POINT('Ctrl Pts',(-6.09261488400006,12.2,-8.99326713800002));
#283908=CARTESIAN_POINT('Ctrl Pts',(-6.09041662000006,12.2,-8.99154949500002));
#283909=CARTESIAN_POINT('Ctrl Pts',(-6.08822428600006,12.2,-8.98983353000002));
#283910=CARTESIAN_POINT('Ctrl Pts',(-6.08603788900006,12.2,-8.98811925800001));
#283911=CARTESIAN_POINT('Ctrl Pts',(-6.08385743000006,12.2,-8.98640669100002));
#283912=CARTESIAN_POINT('Ctrl Pts',(-6.08168291200006,12.2,-8.98469584100001));
#283913=CARTESIAN_POINT('Ctrl Pts',(-6.07951433900006,12.2,-8.98298672300001));
#283914=CARTESIAN_POINT('Ctrl Pts',(-6.07735171400006,12.2,-8.98127934900002));
#283915=CARTESIAN_POINT('Ctrl Pts',(-6.07519504000006,12.2,-8.97957373400001));
#283916=CARTESIAN_POINT('Ctrl Pts',(-6.07304431900006,12.2,-8.97786988800001));
#283917=CARTESIAN_POINT('Ctrl Pts',(-6.07089955600006,12.2,-8.97616782700002));
#283918=CARTESIAN_POINT('Ctrl Pts',(-6.06876075400006,12.2,-8.97446756300001));
#283919=CARTESIAN_POINT('Ctrl Pts',(-6.06662791600006,12.2,-8.97276910900001));
#283920=CARTESIAN_POINT('Ctrl Pts',(-6.06450104400006,12.2,-8.97107248000001));
#283921=CARTESIAN_POINT('Ctrl Pts',(-6.06238014200006,12.2,-8.96937768800001));
#283922=CARTESIAN_POINT('Ctrl Pts',(-6.06026521300006,12.2,-8.96768474600002));
#283923=CARTESIAN_POINT('Ctrl Pts',(-6.05815626100005,12.2,-8.96599367000002));
#283924=CARTESIAN_POINT('Ctrl Pts',(-6.05605328900006,12.2,-8.96430447000002));
#283925=CARTESIAN_POINT('Ctrl Pts',(-6.05395629800006,12.2,-8.96261716200002));
#283926=CARTESIAN_POINT('Ctrl Pts',(-6.05186529400005,12.2,-8.96093175800001));
#283927=CARTESIAN_POINT('Ctrl Pts',(-6.04978027800006,12.2,-8.95924827300002));
#283928=CARTESIAN_POINT('Ctrl Pts',(-6.04770125400006,12.2,-8.95756672100001));
#283929=CARTESIAN_POINT('Ctrl Pts',(-6.04562822600006,12.2,-8.95588711400002));
#283930=CARTESIAN_POINT('Ctrl Pts',(-6.04356119600006,12.2,-8.95420946700002));
#283931=CARTESIAN_POINT('Ctrl Pts',(-6.04150016700006,12.2,-8.95253379300001));
#283932=CARTESIAN_POINT('Ctrl Pts',(-6.03944514200006,12.2,-8.95086010500002));
#283933=CARTESIAN_POINT('Ctrl Pts',(-6.03739612600006,12.2,-8.94918841900001));
#283934=CARTESIAN_POINT('Ctrl Pts',(-6.03535312000006,12.2,-8.94751874800002));
#283935=CARTESIAN_POINT('Ctrl Pts',(-6.03331612900006,12.2,-8.94585110500002));
#283936=CARTESIAN_POINT('Ctrl Pts',(-6.03128515400006,12.2,-8.94418550400001));
#283937=CARTESIAN_POINT('Ctrl Pts',(-6.02926019900006,12.2,-8.94252196100001));
#283938=CARTESIAN_POINT('Ctrl Pts',(-6.02724126900006,12.2,-8.94086048800002));
#283939=CARTESIAN_POINT('Ctrl Pts',(-6.02522836400006,12.2,-8.93920110000002));
#283940=CARTESIAN_POINT('Ctrl Pts',(-6.02322148900006,12.2,-8.93754381100001));
#283941=CARTESIAN_POINT('Ctrl Pts',(-6.02122064700006,12.2,-8.93588863500002));
#283942=CARTESIAN_POINT('Ctrl Pts',(-6.01922584100006,12.2,-8.93423558600002));
#283943=CARTESIAN_POINT('Ctrl Pts',(-6.01723707400006,12.2,-8.93258467900001));
#283944=CARTESIAN_POINT('Ctrl Pts',(-6.01525434800006,12.2,-8.93093592700002));
#283945=CARTESIAN_POINT('Ctrl Pts',(-6.01327766800006,12.2,-8.92928934400001));
#283946=CARTESIAN_POINT('Ctrl Pts',(-6.01130703700006,12.2,-8.92764494600002));
#283947=CARTESIAN_POINT('Ctrl Pts',(-6.00934245600006,12.2,-8.92600274700002));
#283948=CARTESIAN_POINT('Ctrl Pts',(-6.00738393100006,12.2,-8.92436276200002));
#283949=CARTESIAN_POINT('Ctrl Pts',(-6.00543146200006,12.2,-8.92272500300002));
#283950=CARTESIAN_POINT('Ctrl Pts',(-6.00348505500006,12.2,-8.92108948700002));
#283951=CARTESIAN_POINT('Ctrl Pts',(-6.00154471100006,12.2,-8.91945622800002));
#283952=CARTESIAN_POINT('Ctrl Pts',(-5.99961043400006,12.2,-8.91782524000002));
#283953=CARTESIAN_POINT('Ctrl Pts',(-5.99768222800006,12.2,-8.91619653700002));
#283954=CARTESIAN_POINT('Ctrl Pts',(-5.99576009400006,12.2,-8.91457013600002));
#283955=CARTESIAN_POINT('Ctrl Pts',(-5.99384403600006,12.2,-8.91294604900001));
#283956=CARTESIAN_POINT('Ctrl Pts',(-5.99193405800006,12.2,-8.91132429300002));
#283957=CARTESIAN_POINT('Ctrl Pts',(-5.99003016200006,12.2,-8.90970488200002));
#283958=CARTESIAN_POINT('Ctrl Pts',(-5.98813235200006,12.2,-8.90808783100002));
#283959=CARTESIAN_POINT('Ctrl Pts',(-5.98624062900006,12.2,-8.90647315300001));
#283960=CARTESIAN_POINT('Ctrl Pts',(-5.98435500000006,12.2,-8.90486086600001));
#283961=CARTESIAN_POINT('Ctrl Pts',(-5.98247546400006,12.2,-8.90325098400002));
#283962=CARTESIAN_POINT('Ctrl Pts',(-5.98060202600006,12.2,-8.90164352000001));
#283963=CARTESIAN_POINT('Ctrl Pts',(-5.97873468900006,12.2,-8.90003849100001));
#283964=CARTESIAN_POINT('Ctrl Pts',(-5.97687345600006,12.2,-8.89843591300002));
#283965=CARTESIAN_POINT('Ctrl Pts',(-5.97501833000006,12.2,-8.89683579900002));
#283966=CARTESIAN_POINT('Ctrl Pts',(-5.97316931400006,12.2,-8.89523816500001));
#283967=CARTESIAN_POINT('Ctrl Pts',(-5.97132641200006,12.2,-8.89364302600002));
#283968=CARTESIAN_POINT('Ctrl Pts',(-5.96948962500006,12.2,-8.89205039900002));
#283969=CARTESIAN_POINT('Ctrl Pts',(-5.96765895700006,12.2,-8.89046029700001));
#283970=CARTESIAN_POINT('Ctrl Pts',(-5.96583441200006,12.2,-8.88887273700002));
#283971=CARTESIAN_POINT('Ctrl Pts',(-5.96401599300005,12.2,-8.88728773400001));
#283972=CARTESIAN_POINT('Ctrl Pts',(-5.96220370200006,12.2,-8.88570530200001));
#283973=CARTESIAN_POINT('Ctrl Pts',(-5.96039754200006,12.2,-8.88412545900002));
#283974=CARTESIAN_POINT('Ctrl Pts',(-5.95859751600006,12.2,-8.88254821900002));
#283975=CARTESIAN_POINT('Ctrl Pts',(-5.95680362900006,12.2,-8.88097359800001));
#283976=CARTESIAN_POINT('Ctrl Pts',(-5.95501588200006,12.2,-8.87940161100002));
#283977=CARTESIAN_POINT('Ctrl Pts',(-5.95323427900006,12.2,-8.87783227600002));
#283978=CARTESIAN_POINT('Ctrl Pts',(-5.95145882200006,12.2,-8.87626560600001));
#283979=CARTESIAN_POINT('Ctrl Pts',(-5.94968951600006,12.2,-8.87470161900002));
#283980=CARTESIAN_POINT('Ctrl Pts',(-5.94792636200006,12.2,-8.87314032800001));
#283981=CARTESIAN_POINT('Ctrl Pts',(-5.94616936500006,12.2,-8.87158175200002));
#283982=CARTESIAN_POINT('Ctrl Pts',(-5.94441852600006,12.2,-8.87002590600002));
#283983=CARTESIAN_POINT('Ctrl Pts',(-5.94267384900006,12.2,-8.86847280400002));
#283984=CARTESIAN_POINT('Ctrl Pts',(-5.94093533700006,12.2,-8.86692246600001));
#283985=CARTESIAN_POINT('Ctrl Pts',(-5.93920299300006,12.2,-8.86537490400002));
#283986=CARTESIAN_POINT('Ctrl Pts',(-5.93747681900005,12.2,-8.86383013700001));
#283987=CARTESIAN_POINT('Ctrl Pts',(-5.93575682000006,12.2,-8.86228817900001));
#283988=CARTESIAN_POINT('Ctrl Pts',(-5.93404299900006,12.2,-8.86074904800001));
#283989=CARTESIAN_POINT('Ctrl Pts',(-5.93233535700006,12.2,-8.85921276000002));
#283990=CARTESIAN_POINT('Ctrl Pts',(-5.93063389800006,12.2,-8.85767933100002));
#283991=CARTESIAN_POINT('Ctrl Pts',(-5.92893862600006,12.2,-8.85614877700002));
#283992=CARTESIAN_POINT('Ctrl Pts',(-5.92724954300006,12.2,-8.85462111500001));
#283993=CARTESIAN_POINT('Ctrl Pts',(-5.92556665300005,12.2,-8.85309636200001));
#283994=CARTESIAN_POINT('Ctrl Pts',(-5.92388995600006,12.2,-8.85157453400002));
#283995=CARTESIAN_POINT('Ctrl Pts',(-5.92221945900006,12.2,-8.85005564700002));
#283996=CARTESIAN_POINT('Ctrl Pts',(-5.92055516300006,12.2,-8.84853971800002));
#283997=CARTESIAN_POINT('Ctrl Pts',(-5.91889707100006,12.2,-8.84702676400002));
#283998=CARTESIAN_POINT('Ctrl Pts',(-5.91724518600006,12.2,-8.84551680200002));
#283999=CARTESIAN_POINT('Ctrl Pts',(-5.91559951200006,12.2,-8.84400984900001));
#284000=CARTESIAN_POINT('Ctrl Pts',(-5.91396005000006,12.2,-8.84250592100001));
#284001=CARTESIAN_POINT('Ctrl Pts',(-5.91232680500006,12.2,-8.84100503500001));
#284002=CARTESIAN_POINT('Ctrl Pts',(-5.91069977900006,12.2,-8.83950721000001));
#284003=CARTESIAN_POINT('Ctrl Pts',(-5.90907897600006,12.2,-8.83801246000001));
#284004=CARTESIAN_POINT('Ctrl Pts',(-5.90746439700006,12.2,-8.83652080200001));
#284005=CARTESIAN_POINT('Ctrl Pts',(-5.90585604700006,12.2,-8.83503225700002));
#284006=CARTESIAN_POINT('Ctrl Pts',(-5.90425392900006,12.2,-8.83354683900002));
#284007=CARTESIAN_POINT('Ctrl Pts',(-5.90265804300006,12.2,-8.83206456600002));
#284008=CARTESIAN_POINT('Ctrl Pts',(-5.90106839700006,12.2,-8.83058545500001));
#284009=CARTESIAN_POINT('Ctrl Pts',(-5.89948498900006,12.2,-8.82910952300002));
#284010=CARTESIAN_POINT('Ctrl Pts',(-5.89790782500006,12.2,-8.82763679000002));
#284011=CARTESIAN_POINT('Ctrl Pts',(-5.89633690700006,12.2,-8.82616727000002));
#284012=CARTESIAN_POINT('Ctrl Pts',(-5.89477223700006,12.2,-8.82470098400002));
#284013=CARTESIAN_POINT('Ctrl Pts',(-5.89321382100006,12.2,-8.82323794600002));
#284014=CARTESIAN_POINT('Ctrl Pts',(-5.89166165900005,12.2,-8.82177817600001));
#284015=CARTESIAN_POINT('Ctrl Pts',(-5.89011575500006,12.2,-8.82032169100002));
#284016=CARTESIAN_POINT('Ctrl Pts',(-5.88857611200006,12.2,-8.81886851000001));
#284017=CARTESIAN_POINT('Ctrl Pts',(-5.88704273400006,12.2,-8.81741864800002));
#284018=CARTESIAN_POINT('Ctrl Pts',(-5.88551562100006,12.2,-8.81597212600001));
#284019=CARTESIAN_POINT('Ctrl Pts',(-5.88399477900006,12.2,-8.81452896000001));
#284020=CARTESIAN_POINT('Ctrl Pts',(-5.88248021000005,12.2,-8.81308916900002));
#284021=CARTESIAN_POINT('Ctrl Pts',(-5.88097191600006,12.2,-8.81165276900001));
#284022=CARTESIAN_POINT('Ctrl Pts',(-5.87946990200006,12.2,-8.81021978100001));
#284023=CARTESIAN_POINT('Ctrl Pts',(-5.87797416900006,12.2,-8.80879022300002));
#284024=CARTESIAN_POINT('Ctrl Pts',(-5.87648472000006,12.2,-8.80736411100001));
#284025=CARTESIAN_POINT('Ctrl Pts',(-5.87500155900006,12.2,-8.80594146500002));
#284026=CARTESIAN_POINT('Ctrl Pts',(-5.87352468900006,12.2,-8.80452230300002));
#284027=CARTESIAN_POINT('Ctrl Pts',(-5.87205411200006,12.2,-8.80310664200002));
#284028=CARTESIAN_POINT('Ctrl Pts',(-5.87058983200006,12.2,-8.80169450300002));
#284029=CARTESIAN_POINT('Ctrl Pts',(-5.86913185000006,12.2,-8.80028590300002));
#284030=CARTESIAN_POINT('Ctrl Pts',(-5.86768017200006,12.2,-8.79888086200001));
#284031=CARTESIAN_POINT('Ctrl Pts',(-5.86623479900005,12.2,-8.79747939600002));
#284032=CARTESIAN_POINT('Ctrl Pts',(-5.86479573400006,12.2,-8.79608152700002));
#284033=CARTESIAN_POINT('Ctrl Pts',(-5.86336298000006,12.2,-8.79468727200001));
#284034=CARTESIAN_POINT('Ctrl Pts',(-5.86193653900006,12.2,-8.79329665000002));
#284035=CARTESIAN_POINT('Ctrl Pts',(-5.86051641600006,12.2,-8.79190968000002));
#284036=CARTESIAN_POINT('Ctrl Pts',(-5.85910261300006,12.2,-8.79052638100001));
#284037=CARTESIAN_POINT('Ctrl Pts',(-5.85769513200006,12.2,-8.78914677200001));
#284038=CARTESIAN_POINT('Ctrl Pts',(-5.85629397700006,12.2,-8.78777087300002));
#284039=CARTESIAN_POINT('Ctrl Pts',(-5.85489915200006,12.2,-8.78639870300002));
#284040=CARTESIAN_POINT('Ctrl Pts',(-5.85351065700006,12.2,-8.78503028000001));
#284041=CARTESIAN_POINT('Ctrl Pts',(-5.85212849700006,12.2,-8.78366562400002));
#284042=CARTESIAN_POINT('Ctrl Pts',(-5.85075267500006,12.2,-8.78230475600001));
#284043=CARTESIAN_POINT('Ctrl Pts',(-5.84938319300006,12.2,-8.78094769400001));
#284044=CARTESIAN_POINT('Ctrl Pts',(-5.84802005400006,12.2,-8.77959445700002));
#284045=CARTESIAN_POINT('Ctrl Pts',(-5.84666326000006,12.2,-8.77824506500002));
#284046=CARTESIAN_POINT('Ctrl Pts',(-5.84531281700006,12.2,-8.77689953800001));
#284047=CARTESIAN_POINT('Ctrl Pts',(-5.84396872500006,12.2,-8.77555789600001));
#284048=CARTESIAN_POINT('Ctrl Pts',(-5.84263098700006,12.2,-8.77422015900001));
#284049=CARTESIAN_POINT('Ctrl Pts',(-5.84129960800006,12.2,-8.77288634600001));
#284050=CARTESIAN_POINT('Ctrl Pts',(-5.83997459000006,12.2,-8.77155647700001));
#284051=CARTESIAN_POINT('Ctrl Pts',(-5.83865593500006,12.2,-8.77023057400002));
#284052=CARTESIAN_POINT('Ctrl Pts',(-5.83734364600006,12.2,-8.76890865500001));
#284053=CARTESIAN_POINT('Ctrl Pts',(-5.83603772700005,12.2,-8.76759074100002));
#284054=CARTESIAN_POINT('Ctrl Pts',(-5.83473817900006,12.2,-8.76627685200001));
#284055=CARTESIAN_POINT('Ctrl Pts',(-5.83344500700006,12.2,-8.76496700800002));
#284056=CARTESIAN_POINT('Ctrl Pts',(-5.83215821300006,12.2,-8.76366123100001));
#284057=CARTESIAN_POINT('Ctrl Pts',(-5.83087780000006,12.2,-8.76235953900002));
#284058=CARTESIAN_POINT('Ctrl Pts',(-5.82960377000005,12.2,-8.76106195500002));
#284059=CARTESIAN_POINT('Ctrl Pts',(-5.82833612700006,12.2,-8.75976849900002));
#284060=CARTESIAN_POINT('Ctrl Pts',(-5.82707487300006,12.2,-8.75847919000002));
#284061=CARTESIAN_POINT('Ctrl Pts',(-5.82582001200006,12.2,-8.75719405100002));
#284062=CARTESIAN_POINT('Ctrl Pts',(-5.82457154700006,12.2,-8.75591310200001));
#284063=CARTESIAN_POINT('Ctrl Pts',(-5.82332948000006,12.2,-8.75463636300001));
#284064=CARTESIAN_POINT('Ctrl Pts',(-5.82209381200006,12.2,-8.75336385700002));
#284065=CARTESIAN_POINT('Ctrl Pts',(-5.82086454900006,12.2,-8.75209560300001));
#284066=CARTESIAN_POINT('Ctrl Pts',(-5.81964169300006,12.2,-8.75083162500001));
#284067=CARTESIAN_POINT('Ctrl Pts',(-5.81842524600006,12.2,-8.74957194100002));
#284068=CARTESIAN_POINT('Ctrl Pts',(-5.81721521200006,12.2,-8.74831657400001));
#284069=CARTESIAN_POINT('Ctrl Pts',(-5.81601159400006,12.2,-8.74706554600002));
#284070=CARTESIAN_POINT('Ctrl Pts',(-5.81481439300005,12.2,-8.74581887800002));
#284071=CARTESIAN_POINT('Ctrl Pts',(-5.81362361300005,12.2,-8.74457659100001));
#284072=CARTESIAN_POINT('Ctrl Pts',(-5.81243925700006,12.2,-8.74333870700001));
#284073=CARTESIAN_POINT('Ctrl Pts',(-5.81126132800006,12.2,-8.74210524800001));
#284074=CARTESIAN_POINT('Ctrl Pts',(-5.81008982800006,12.2,-8.74087623600002));
#284075=CARTESIAN_POINT('Ctrl Pts',(-5.80892476100006,12.2,-8.73965169300002));
#284076=CARTESIAN_POINT('Ctrl Pts',(-5.80776612900006,12.2,-8.73843163900002));
#284077=CARTESIAN_POINT('Ctrl Pts',(-5.80661393400006,12.2,-8.73721609800001));
#284078=CARTESIAN_POINT('Ctrl Pts',(-5.80546818100006,12.2,-8.73600509300001));
#284079=CARTESIAN_POINT('Ctrl Pts',(-5.80432887200006,12.2,-8.73479864500002));
#284080=CARTESIAN_POINT('Ctrl Pts',(-5.80319600900006,12.2,-8.73359677600002));
#284081=CARTESIAN_POINT('Ctrl Pts',(-5.80206959600006,12.2,-8.73239950900001));
#284082=CARTESIAN_POINT('Ctrl Pts',(-5.80094963500006,12.2,-8.73120686600002));
#284083=CARTESIAN_POINT('Ctrl Pts',(-5.79983612800006,12.2,-8.73001887100001));
#284084=CARTESIAN_POINT('Ctrl Pts',(-5.79872908000006,12.2,-8.72883554600002));
#284085=CARTESIAN_POINT('Ctrl Pts',(-5.79762849300006,12.2,-8.72765691300001));
#284086=CARTESIAN_POINT('Ctrl Pts',(-5.79653437000006,12.2,-8.72648299600002));
#284087=CARTESIAN_POINT('Ctrl Pts',(-5.79544671200006,12.2,-8.72531381700002));
#284088=CARTESIAN_POINT('Ctrl Pts',(-5.79436552400006,12.2,-8.72414939900001));
#284089=CARTESIAN_POINT('Ctrl Pts',(-5.79329080800006,12.2,-8.72298976600002));
#284090=CARTESIAN_POINT('Ctrl Pts',(-5.79222256600006,12.2,-8.72183494100002));
#284091=CARTESIAN_POINT('Ctrl Pts',(-5.79116080300006,12.2,-8.72068494800001));
#284092=CARTESIAN_POINT('Ctrl Pts',(-5.79010551900006,12.2,-8.71953980900001));
#284093=CARTESIAN_POINT('Ctrl Pts',(-5.78905671900006,12.2,-8.71839954800001));
#284094=CARTESIAN_POINT('Ctrl Pts',(-5.78801440500006,12.2,-8.71726418900002));
#284095=CARTESIAN_POINT('Ctrl Pts',(-5.78697858000006,12.2,-8.71613375700001));
#284096=CARTESIAN_POINT('Ctrl Pts',(-5.78594924700006,12.2,-8.71500827300002));
#284097=CARTESIAN_POINT('Ctrl Pts',(-5.78492640800006,12.2,-8.71388776300002));
#284098=CARTESIAN_POINT('Ctrl Pts',(-5.78391006700006,12.2,-8.71277225000001));
#284099=CARTESIAN_POINT('Ctrl Pts',(-5.78290022600005,12.2,-8.71166175800001));
#284100=CARTESIAN_POINT('Ctrl Pts',(-5.78189688700006,12.2,-8.71055631200001));
#284101=CARTESIAN_POINT('Ctrl Pts',(-5.78090005400006,12.2,-8.70945593700002));
#284102=CARTESIAN_POINT('Ctrl Pts',(-5.77990973100006,12.2,-8.70836065500002));
#284103=CARTESIAN_POINT('Ctrl Pts',(-5.77892591700006,12.2,-8.70727049300001));
#284104=CARTESIAN_POINT('Ctrl Pts',(-5.77794861800006,12.2,-8.70618547500002));
#284105=CARTESIAN_POINT('Ctrl Pts',(-5.77697783600006,12.2,-8.70510562400002));
#284106=CARTESIAN_POINT('Ctrl Pts',(-5.77601357300006,12.2,-8.70403096700001));
#284107=CARTESIAN_POINT('Ctrl Pts',(-5.77505583400006,12.2,-8.70296152800002));
#284108=CARTESIAN_POINT('Ctrl Pts',(-5.77410461900006,12.2,-8.70189733200002));
#284109=CARTESIAN_POINT('Ctrl Pts',(-5.77315993200005,12.2,-8.70083840400002));
#284110=CARTESIAN_POINT('Ctrl Pts',(-5.77222177600006,12.2,-8.69978477000002));
#284111=CARTESIAN_POINT('Ctrl Pts',(-5.77129015400006,12.2,-8.69873645500002));
#284112=CARTESIAN_POINT('Ctrl Pts',(-5.77036506700006,12.2,-8.69769348400002));
#284113=CARTESIAN_POINT('Ctrl Pts',(-5.76944652100006,12.2,-8.69665588300002));
#284114=CARTESIAN_POINT('Ctrl Pts',(-5.76853451500006,12.2,-8.69562367700001));
#284115=CARTESIAN_POINT('Ctrl Pts',(-5.76762905500006,12.2,-8.69459689400001));
#284116=CARTESIAN_POINT('Ctrl Pts',(-5.76673014200006,12.2,-8.69357555700002));
#284117=CARTESIAN_POINT('Ctrl Pts',(-5.76583777900006,12.2,-8.69255969400001));
#284118=CARTESIAN_POINT('Ctrl Pts',(-5.76495197000006,12.2,-8.69154933000001));
#284119=CARTESIAN_POINT('Ctrl Pts',(-5.76407271500006,12.2,-8.69054449200001));
#284120=CARTESIAN_POINT('Ctrl Pts',(-5.76320002000006,12.2,-8.68954520600001));
#284121=CARTESIAN_POINT('Ctrl Pts',(-5.76233388600006,12.2,-8.68855149800002));
#284122=CARTESIAN_POINT('Ctrl Pts',(-5.76147431600006,12.2,-8.68756339600001));
#284123=CARTESIAN_POINT('Ctrl Pts',(-5.76062131200006,12.2,-8.68658092600001));
#284124=CARTESIAN_POINT('Ctrl Pts',(-5.75977487800006,12.2,-8.68560411500002));
#284125=CARTESIAN_POINT('Ctrl Pts',(-5.75893501600006,12.2,-8.68463298900001));
#284126=CARTESIAN_POINT('Ctrl Pts',(-5.75810173000006,12.2,-8.68366757600001));
#284127=CARTESIAN_POINT('Ctrl Pts',(-5.75727502100006,12.2,-8.68270790200001));
#284128=CARTESIAN_POINT('Ctrl Pts',(-5.75645489300006,12.2,-8.68175399800002));
#284129=CARTESIAN_POINT('Ctrl Pts',(-5.75564134700006,12.2,-8.68080588500002));
#284130=CARTESIAN_POINT('Ctrl Pts',(-5.75483438800005,12.2,-8.67986359700001));
#284131=CARTESIAN_POINT('Ctrl Pts',(-5.75403401900005,12.2,-8.67892715900001));
#284132=CARTESIAN_POINT('Ctrl Pts',(-5.75324024000006,12.2,-8.67799659800001));
#284133=CARTESIAN_POINT('Ctrl Pts',(-5.75245305600006,12.2,-8.67707194200002));
#284134=CARTESIAN_POINT('Ctrl Pts',(-5.75167246900006,12.2,-8.67615322100002));
#284135=CARTESIAN_POINT('Ctrl Pts',(-5.75089848100006,12.2,-8.67524046100002));
#284136=CARTESIAN_POINT('Ctrl Pts',(-5.75013109600006,12.2,-8.67433369300001));
#284137=CARTESIAN_POINT('Ctrl Pts',(-5.74937031600006,12.2,-8.67343294300002));
#284138=CARTESIAN_POINT('Ctrl Pts',(-5.74861614500006,12.2,-8.67253824000001));
#284139=CARTESIAN_POINT('Ctrl Pts',(-5.74786858400006,12.2,-8.67164961300002));
#284140=CARTESIAN_POINT('Ctrl Pts',(-5.74712763600006,12.2,-8.67076709200001));
#284141=CARTESIAN_POINT('Ctrl Pts',(-5.74639330500006,12.2,-8.66989070400002));
#284142=CARTESIAN_POINT('Ctrl Pts',(-5.74566559300006,12.2,-8.66902047900002));
#284143=CARTESIAN_POINT('Ctrl Pts',(-5.74494450300006,12.2,-8.66815644700001));
#284144=CARTESIAN_POINT('Ctrl Pts',(-5.74423003600006,12.2,-8.66729863600002));
#284145=CARTESIAN_POINT('Ctrl Pts',(-5.74352219700006,12.2,-8.66644707700001));
#284146=CARTESIAN_POINT('Ctrl Pts',(-5.74282098800006,12.2,-8.66560180000001));
#284147=CARTESIAN_POINT('Ctrl Pts',(-5.74212641100006,12.2,-8.66476283200001));
#284148=CARTESIAN_POINT('Ctrl Pts',(-5.74143847000006,12.2,-8.66393020500002));
#284149=CARTESIAN_POINT('Ctrl Pts',(-5.74075716700006,12.2,-8.66310395100001));
#284150=CARTESIAN_POINT('Ctrl Pts',(-5.74008250400006,12.2,-8.66228409600001));
#284151=CARTESIAN_POINT('Ctrl Pts',(-5.73941448500006,12.2,-8.66147067400002));
#284152=CARTESIAN_POINT('Ctrl Pts',(-5.73875311300006,12.2,-8.66066371300001));
#284153=CARTESIAN_POINT('Ctrl Pts',(-5.73809838900006,12.2,-8.65986324600001));
#284154=CARTESIAN_POINT('Ctrl Pts',(-5.73745031600006,12.2,-8.65906930200002));
#284155=CARTESIAN_POINT('Ctrl Pts',(-5.73680889900006,12.2,-8.65828191300002));
#284156=CARTESIAN_POINT('Ctrl Pts',(-5.73617413900006,12.2,-8.65750111000001));
#284157=CARTESIAN_POINT('Ctrl Pts',(-5.73554603700006,12.2,-8.65672692500001));
#284158=CARTESIAN_POINT('Ctrl Pts',(-5.73492459900006,12.2,-8.65595938700002));
#284159=CARTESIAN_POINT('Ctrl Pts',(-5.73430982600006,12.2,-8.65519853100002));
#284160=CARTESIAN_POINT('Ctrl Pts',(-5.73370172100006,12.2,-8.65444438600001));
#284161=CARTESIAN_POINT('Ctrl Pts',(-5.73310028700006,12.2,-8.65369698500002));
#284162=CARTESIAN_POINT('Ctrl Pts',(-5.73250552600006,12.2,-8.65295636100001));
#284163=CARTESIAN_POINT('Ctrl Pts',(-5.73191744100006,12.2,-8.65222254500001));
#284164=CARTESIAN_POINT('Ctrl Pts',(-5.73133603500006,12.2,-8.65149557000001));
#284165=CARTESIAN_POINT('Ctrl Pts',(-5.73076462000006,12.2,-8.65077961500001));
#284166=CARTESIAN_POINT('Ctrl Pts',(-5.73031342200006,12.2,-8.65021312700001));
#284167=CARTESIAN_POINT('Ctrl Pts',(-5.72997879300006,12.2,-8.64979235000002));
#284168=CARTESIAN_POINT('Ctrl Pts',(-5.72975808700006,12.2,-8.64951454400002));
#284169=CARTESIAN_POINT('Ctrl Pts',(-5.72964966100006,12.2,-8.64937799900002));
#284170=CARTESIAN_POINT('Ctrl Pts',(-5.72964966100006,15.2,-8.64937799900002));
#284171=CARTESIAN_POINT('Ctrl Pts',(-5.72975808700006,15.2,-8.64951454400002));
#284172=CARTESIAN_POINT('Ctrl Pts',(-5.72997879300006,15.2,-8.64979235000002));
#284173=CARTESIAN_POINT('Ctrl Pts',(-5.73031342200006,15.2,-8.65021312700001));
#284174=CARTESIAN_POINT('Ctrl Pts',(-5.73076462000006,15.2,-8.65077961500001));
#284175=CARTESIAN_POINT('Ctrl Pts',(-5.73133603500006,15.2,-8.65149557000001));
#284176=CARTESIAN_POINT('Ctrl Pts',(-5.73191744100006,15.2,-8.65222254500001));
#284177=CARTESIAN_POINT('Ctrl Pts',(-5.73250552600006,15.2,-8.65295636100001));
#284178=CARTESIAN_POINT('Ctrl Pts',(-5.73310028700006,15.2,-8.65369698500002));
#284179=CARTESIAN_POINT('Ctrl Pts',(-5.73370172100006,15.2,-8.65444438600001));
#284180=CARTESIAN_POINT('Ctrl Pts',(-5.73430982600006,15.2,-8.65519853100002));
#284181=CARTESIAN_POINT('Ctrl Pts',(-5.73492459900006,15.2,-8.65595938700002));
#284182=CARTESIAN_POINT('Ctrl Pts',(-5.73554603700006,15.2,-8.65672692500001));
#284183=CARTESIAN_POINT('Ctrl Pts',(-5.73617413900006,15.2,-8.65750111000001));
#284184=CARTESIAN_POINT('Ctrl Pts',(-5.73680889900006,15.2,-8.65828191300002));
#284185=CARTESIAN_POINT('Ctrl Pts',(-5.73745031600006,15.2,-8.65906930200002));
#284186=CARTESIAN_POINT('Ctrl Pts',(-5.73809838900006,15.2,-8.65986324600001));
#284187=CARTESIAN_POINT('Ctrl Pts',(-5.73875311300006,15.2,-8.66066371300001));
#284188=CARTESIAN_POINT('Ctrl Pts',(-5.73941448500006,15.2,-8.66147067400002));
#284189=CARTESIAN_POINT('Ctrl Pts',(-5.74008250400006,15.2,-8.66228409600001));
#284190=CARTESIAN_POINT('Ctrl Pts',(-5.74075716700006,15.2,-8.66310395100001));
#284191=CARTESIAN_POINT('Ctrl Pts',(-5.74143847000006,15.2,-8.66393020500002));
#284192=CARTESIAN_POINT('Ctrl Pts',(-5.74212641100006,15.2,-8.66476283200001));
#284193=CARTESIAN_POINT('Ctrl Pts',(-5.74282098800006,15.2,-8.66560180000001));
#284194=CARTESIAN_POINT('Ctrl Pts',(-5.74352219700006,15.2,-8.66644707700001));
#284195=CARTESIAN_POINT('Ctrl Pts',(-5.74423003600006,15.2,-8.66729863600002));
#284196=CARTESIAN_POINT('Ctrl Pts',(-5.74494450300006,15.2,-8.66815644700001));
#284197=CARTESIAN_POINT('Ctrl Pts',(-5.74566559300006,15.2,-8.66902047900002));
#284198=CARTESIAN_POINT('Ctrl Pts',(-5.74639330500006,15.2,-8.66989070400002));
#284199=CARTESIAN_POINT('Ctrl Pts',(-5.74712763600006,15.2,-8.67076709200001));
#284200=CARTESIAN_POINT('Ctrl Pts',(-5.74786858400006,15.2,-8.67164961300002));
#284201=CARTESIAN_POINT('Ctrl Pts',(-5.74861614500006,15.2,-8.67253824000001));
#284202=CARTESIAN_POINT('Ctrl Pts',(-5.74937031600006,15.2,-8.67343294300002));
#284203=CARTESIAN_POINT('Ctrl Pts',(-5.75013109600006,15.2,-8.67433369300001));
#284204=CARTESIAN_POINT('Ctrl Pts',(-5.75089848100006,15.2,-8.67524046100002));
#284205=CARTESIAN_POINT('Ctrl Pts',(-5.75167246900006,15.2,-8.67615322100002));
#284206=CARTESIAN_POINT('Ctrl Pts',(-5.75245305600006,15.2,-8.67707194200002));
#284207=CARTESIAN_POINT('Ctrl Pts',(-5.75324024000006,15.2,-8.67799659800001));
#284208=CARTESIAN_POINT('Ctrl Pts',(-5.75403401900005,15.2,-8.67892715900001));
#284209=CARTESIAN_POINT('Ctrl Pts',(-5.75483438800005,15.2,-8.67986359700001));
#284210=CARTESIAN_POINT('Ctrl Pts',(-5.75564134700006,15.2,-8.68080588500002));
#284211=CARTESIAN_POINT('Ctrl Pts',(-5.75645489300006,15.2,-8.68175399800002));
#284212=CARTESIAN_POINT('Ctrl Pts',(-5.75727502100006,15.2,-8.68270790200001));
#284213=CARTESIAN_POINT('Ctrl Pts',(-5.75810173000006,15.2,-8.68366757600001));
#284214=CARTESIAN_POINT('Ctrl Pts',(-5.75893501600006,15.2,-8.68463298900001));
#284215=CARTESIAN_POINT('Ctrl Pts',(-5.75977487800006,15.2,-8.68560411500002));
#284216=CARTESIAN_POINT('Ctrl Pts',(-5.76062131200006,15.2,-8.68658092600001));
#284217=CARTESIAN_POINT('Ctrl Pts',(-5.76147431600006,15.2,-8.68756339600001));
#284218=CARTESIAN_POINT('Ctrl Pts',(-5.76233388600006,15.2,-8.68855149800002));
#284219=CARTESIAN_POINT('Ctrl Pts',(-5.76320002000006,15.2,-8.68954520600001));
#284220=CARTESIAN_POINT('Ctrl Pts',(-5.76407271500006,15.2,-8.69054449200001));
#284221=CARTESIAN_POINT('Ctrl Pts',(-5.76495197000006,15.2,-8.69154933000001));
#284222=CARTESIAN_POINT('Ctrl Pts',(-5.76583777900006,15.2,-8.69255969400001));
#284223=CARTESIAN_POINT('Ctrl Pts',(-5.76673014200006,15.2,-8.69357555700002));
#284224=CARTESIAN_POINT('Ctrl Pts',(-5.76762905500006,15.2,-8.69459689400001));
#284225=CARTESIAN_POINT('Ctrl Pts',(-5.76853451500006,15.2,-8.69562367700001));
#284226=CARTESIAN_POINT('Ctrl Pts',(-5.76944652100006,15.2,-8.69665588300002));
#284227=CARTESIAN_POINT('Ctrl Pts',(-5.77036506700006,15.2,-8.69769348400002));
#284228=CARTESIAN_POINT('Ctrl Pts',(-5.77129015400006,15.2,-8.69873645500002));
#284229=CARTESIAN_POINT('Ctrl Pts',(-5.77222177600006,15.2,-8.69978477000002));
#284230=CARTESIAN_POINT('Ctrl Pts',(-5.77315993200005,15.2,-8.70083840400002));
#284231=CARTESIAN_POINT('Ctrl Pts',(-5.77410461900006,15.2,-8.70189733200002));
#284232=CARTESIAN_POINT('Ctrl Pts',(-5.77505583400006,15.2,-8.70296152800002));
#284233=CARTESIAN_POINT('Ctrl Pts',(-5.77601357300006,15.2,-8.70403096700001));
#284234=CARTESIAN_POINT('Ctrl Pts',(-5.77697783600006,15.2,-8.70510562400002));
#284235=CARTESIAN_POINT('Ctrl Pts',(-5.77794861800006,15.2,-8.70618547500002));
#284236=CARTESIAN_POINT('Ctrl Pts',(-5.77892591700006,15.2,-8.70727049300001));
#284237=CARTESIAN_POINT('Ctrl Pts',(-5.77990973100006,15.2,-8.70836065500002));
#284238=CARTESIAN_POINT('Ctrl Pts',(-5.78090005400006,15.2,-8.70945593700002));
#284239=CARTESIAN_POINT('Ctrl Pts',(-5.78189688700006,15.2,-8.71055631200001));
#284240=CARTESIAN_POINT('Ctrl Pts',(-5.78290022600005,15.2,-8.71166175800001));
#284241=CARTESIAN_POINT('Ctrl Pts',(-5.78391006700006,15.2,-8.71277225000001));
#284242=CARTESIAN_POINT('Ctrl Pts',(-5.78492640800006,15.2,-8.71388776300002));
#284243=CARTESIAN_POINT('Ctrl Pts',(-5.78594924700006,15.2,-8.71500827300002));
#284244=CARTESIAN_POINT('Ctrl Pts',(-5.78697858000006,15.2,-8.71613375700001));
#284245=CARTESIAN_POINT('Ctrl Pts',(-5.78801440500006,15.2,-8.71726418900002));
#284246=CARTESIAN_POINT('Ctrl Pts',(-5.78905671900006,15.2,-8.71839954800001));
#284247=CARTESIAN_POINT('Ctrl Pts',(-5.79010551900006,15.2,-8.71953980900001));
#284248=CARTESIAN_POINT('Ctrl Pts',(-5.79116080300006,15.2,-8.72068494800001));
#284249=CARTESIAN_POINT('Ctrl Pts',(-5.79222256600006,15.2,-8.72183494100002));
#284250=CARTESIAN_POINT('Ctrl Pts',(-5.79329080800006,15.2,-8.72298976600002));
#284251=CARTESIAN_POINT('Ctrl Pts',(-5.79436552400006,15.2,-8.72414939900001));
#284252=CARTESIAN_POINT('Ctrl Pts',(-5.79544671200006,15.2,-8.72531381700002));
#284253=CARTESIAN_POINT('Ctrl Pts',(-5.79653437000006,15.2,-8.72648299600002));
#284254=CARTESIAN_POINT('Ctrl Pts',(-5.79762849300006,15.2,-8.72765691300001));
#284255=CARTESIAN_POINT('Ctrl Pts',(-5.79872908000006,15.2,-8.72883554600002));
#284256=CARTESIAN_POINT('Ctrl Pts',(-5.79983612800006,15.2,-8.73001887100001));
#284257=CARTESIAN_POINT('Ctrl Pts',(-5.80094963500006,15.2,-8.73120686600002));
#284258=CARTESIAN_POINT('Ctrl Pts',(-5.80206959600006,15.2,-8.73239950900001));
#284259=CARTESIAN_POINT('Ctrl Pts',(-5.80319600900006,15.2,-8.73359677600002));
#284260=CARTESIAN_POINT('Ctrl Pts',(-5.80432887200006,15.2,-8.73479864500002));
#284261=CARTESIAN_POINT('Ctrl Pts',(-5.80546818100006,15.2,-8.73600509300001));
#284262=CARTESIAN_POINT('Ctrl Pts',(-5.80661393400006,15.2,-8.73721609800001));
#284263=CARTESIAN_POINT('Ctrl Pts',(-5.80776612900006,15.2,-8.73843163900002));
#284264=CARTESIAN_POINT('Ctrl Pts',(-5.80892476100006,15.2,-8.73965169300002));
#284265=CARTESIAN_POINT('Ctrl Pts',(-5.81008982800006,15.2,-8.74087623600002));
#284266=CARTESIAN_POINT('Ctrl Pts',(-5.81126132800006,15.2,-8.74210524800001));
#284267=CARTESIAN_POINT('Ctrl Pts',(-5.81243925700006,15.2,-8.74333870700001));
#284268=CARTESIAN_POINT('Ctrl Pts',(-5.81362361300005,15.2,-8.74457659100001));
#284269=CARTESIAN_POINT('Ctrl Pts',(-5.81481439300005,15.2,-8.74581887800002));
#284270=CARTESIAN_POINT('Ctrl Pts',(-5.81601159400006,15.2,-8.74706554600002));
#284271=CARTESIAN_POINT('Ctrl Pts',(-5.81721521200006,15.2,-8.74831657400001));
#284272=CARTESIAN_POINT('Ctrl Pts',(-5.81842524600006,15.2,-8.74957194100002));
#284273=CARTESIAN_POINT('Ctrl Pts',(-5.81964169300006,15.2,-8.75083162500001));
#284274=CARTESIAN_POINT('Ctrl Pts',(-5.82086454900006,15.2,-8.75209560300001));
#284275=CARTESIAN_POINT('Ctrl Pts',(-5.82209381200006,15.2,-8.75336385700002));
#284276=CARTESIAN_POINT('Ctrl Pts',(-5.82332948000006,15.2,-8.75463636300001));
#284277=CARTESIAN_POINT('Ctrl Pts',(-5.82457154700006,15.2,-8.75591310200001));
#284278=CARTESIAN_POINT('Ctrl Pts',(-5.82582001200006,15.2,-8.75719405100002));
#284279=CARTESIAN_POINT('Ctrl Pts',(-5.82707487300006,15.2,-8.75847919000002));
#284280=CARTESIAN_POINT('Ctrl Pts',(-5.82833612700006,15.2,-8.75976849900002));
#284281=CARTESIAN_POINT('Ctrl Pts',(-5.82960377000005,15.2,-8.76106195500002));
#284282=CARTESIAN_POINT('Ctrl Pts',(-5.83087780000006,15.2,-8.76235953900002));
#284283=CARTESIAN_POINT('Ctrl Pts',(-5.83215821300006,15.2,-8.76366123100001));
#284284=CARTESIAN_POINT('Ctrl Pts',(-5.83344500700006,15.2,-8.76496700800002));
#284285=CARTESIAN_POINT('Ctrl Pts',(-5.83473817900006,15.2,-8.76627685200001));
#284286=CARTESIAN_POINT('Ctrl Pts',(-5.83603772700005,15.2,-8.76759074100002));
#284287=CARTESIAN_POINT('Ctrl Pts',(-5.83734364600006,15.2,-8.76890865500001));
#284288=CARTESIAN_POINT('Ctrl Pts',(-5.83865593500006,15.2,-8.77023057400002));
#284289=CARTESIAN_POINT('Ctrl Pts',(-5.83997459000006,15.2,-8.77155647700001));
#284290=CARTESIAN_POINT('Ctrl Pts',(-5.84129960800006,15.2,-8.77288634600001));
#284291=CARTESIAN_POINT('Ctrl Pts',(-5.84263098700006,15.2,-8.77422015900001));
#284292=CARTESIAN_POINT('Ctrl Pts',(-5.84396872500006,15.2,-8.77555789600001));
#284293=CARTESIAN_POINT('Ctrl Pts',(-5.84531281700006,15.2,-8.77689953800001));
#284294=CARTESIAN_POINT('Ctrl Pts',(-5.84666326000006,15.2,-8.77824506500002));
#284295=CARTESIAN_POINT('Ctrl Pts',(-5.84802005400006,15.2,-8.77959445700002));
#284296=CARTESIAN_POINT('Ctrl Pts',(-5.84938319300006,15.2,-8.78094769400001));
#284297=CARTESIAN_POINT('Ctrl Pts',(-5.85075267500006,15.2,-8.78230475600001));
#284298=CARTESIAN_POINT('Ctrl Pts',(-5.85212849700006,15.2,-8.78366562400002));
#284299=CARTESIAN_POINT('Ctrl Pts',(-5.85351065700006,15.2,-8.78503028000001));
#284300=CARTESIAN_POINT('Ctrl Pts',(-5.85489915200006,15.2,-8.78639870300002));
#284301=CARTESIAN_POINT('Ctrl Pts',(-5.85629397700006,15.2,-8.78777087300002));
#284302=CARTESIAN_POINT('Ctrl Pts',(-5.85769513200006,15.2,-8.78914677200001));
#284303=CARTESIAN_POINT('Ctrl Pts',(-5.85910261300006,15.2,-8.79052638100001));
#284304=CARTESIAN_POINT('Ctrl Pts',(-5.86051641600006,15.2,-8.79190968000002));
#284305=CARTESIAN_POINT('Ctrl Pts',(-5.86193653900006,15.2,-8.79329665000002));
#284306=CARTESIAN_POINT('Ctrl Pts',(-5.86336298000006,15.2,-8.79468727200001));
#284307=CARTESIAN_POINT('Ctrl Pts',(-5.86479573400006,15.2,-8.79608152700002));
#284308=CARTESIAN_POINT('Ctrl Pts',(-5.86623479900005,15.2,-8.79747939600002));
#284309=CARTESIAN_POINT('Ctrl Pts',(-5.86768017200006,15.2,-8.79888086200001));
#284310=CARTESIAN_POINT('Ctrl Pts',(-5.86913185000006,15.2,-8.80028590300002));
#284311=CARTESIAN_POINT('Ctrl Pts',(-5.87058983200006,15.2,-8.80169450300002));
#284312=CARTESIAN_POINT('Ctrl Pts',(-5.87205411200006,15.2,-8.80310664200002));
#284313=CARTESIAN_POINT('Ctrl Pts',(-5.87352468900006,15.2,-8.80452230300002));
#284314=CARTESIAN_POINT('Ctrl Pts',(-5.87500155900006,15.2,-8.80594146500002));
#284315=CARTESIAN_POINT('Ctrl Pts',(-5.87648472000006,15.2,-8.80736411100001));
#284316=CARTESIAN_POINT('Ctrl Pts',(-5.87797416900006,15.2,-8.80879022300002));
#284317=CARTESIAN_POINT('Ctrl Pts',(-5.87946990200006,15.2,-8.81021978100001));
#284318=CARTESIAN_POINT('Ctrl Pts',(-5.88097191600006,15.2,-8.81165276900001));
#284319=CARTESIAN_POINT('Ctrl Pts',(-5.88248021000005,15.2,-8.81308916900002));
#284320=CARTESIAN_POINT('Ctrl Pts',(-5.88399477900006,15.2,-8.81452896000001));
#284321=CARTESIAN_POINT('Ctrl Pts',(-5.88551562100006,15.2,-8.81597212600001));
#284322=CARTESIAN_POINT('Ctrl Pts',(-5.88704273400006,15.2,-8.81741864800002));
#284323=CARTESIAN_POINT('Ctrl Pts',(-5.88857611200006,15.2,-8.81886851000001));
#284324=CARTESIAN_POINT('Ctrl Pts',(-5.89011575500006,15.2,-8.82032169100002));
#284325=CARTESIAN_POINT('Ctrl Pts',(-5.89166165900005,15.2,-8.82177817600001));
#284326=CARTESIAN_POINT('Ctrl Pts',(-5.89321382100006,15.2,-8.82323794600002));
#284327=CARTESIAN_POINT('Ctrl Pts',(-5.89477223700006,15.2,-8.82470098400002));
#284328=CARTESIAN_POINT('Ctrl Pts',(-5.89633690700006,15.2,-8.82616727000002));
#284329=CARTESIAN_POINT('Ctrl Pts',(-5.89790782500006,15.2,-8.82763679000002));
#284330=CARTESIAN_POINT('Ctrl Pts',(-5.89948498900006,15.2,-8.82910952300002));
#284331=CARTESIAN_POINT('Ctrl Pts',(-5.90106839700006,15.2,-8.83058545500001));
#284332=CARTESIAN_POINT('Ctrl Pts',(-5.90265804300006,15.2,-8.83206456600002));
#284333=CARTESIAN_POINT('Ctrl Pts',(-5.90425392900006,15.2,-8.83354683900002));
#284334=CARTESIAN_POINT('Ctrl Pts',(-5.90585604700006,15.2,-8.83503225700002));
#284335=CARTESIAN_POINT('Ctrl Pts',(-5.90746439700006,15.2,-8.83652080200001));
#284336=CARTESIAN_POINT('Ctrl Pts',(-5.90907897600006,15.2,-8.83801246000001));
#284337=CARTESIAN_POINT('Ctrl Pts',(-5.91069977900006,15.2,-8.83950721000001));
#284338=CARTESIAN_POINT('Ctrl Pts',(-5.91232680500006,15.2,-8.84100503500001));
#284339=CARTESIAN_POINT('Ctrl Pts',(-5.91396005000006,15.2,-8.84250592100001));
#284340=CARTESIAN_POINT('Ctrl Pts',(-5.91559951200006,15.2,-8.84400984900001));
#284341=CARTESIAN_POINT('Ctrl Pts',(-5.91724518600006,15.2,-8.84551680200002));
#284342=CARTESIAN_POINT('Ctrl Pts',(-5.91889707100006,15.2,-8.84702676400002));
#284343=CARTESIAN_POINT('Ctrl Pts',(-5.92055516300006,15.2,-8.84853971800002));
#284344=CARTESIAN_POINT('Ctrl Pts',(-5.92221945900006,15.2,-8.85005564700002));
#284345=CARTESIAN_POINT('Ctrl Pts',(-5.92388995600006,15.2,-8.85157453400002));
#284346=CARTESIAN_POINT('Ctrl Pts',(-5.92556665300005,15.2,-8.85309636200001));
#284347=CARTESIAN_POINT('Ctrl Pts',(-5.92724954300006,15.2,-8.85462111500001));
#284348=CARTESIAN_POINT('Ctrl Pts',(-5.92893862600006,15.2,-8.85614877700002));
#284349=CARTESIAN_POINT('Ctrl Pts',(-5.93063389800006,15.2,-8.85767933100002));
#284350=CARTESIAN_POINT('Ctrl Pts',(-5.93233535700006,15.2,-8.85921276000002));
#284351=CARTESIAN_POINT('Ctrl Pts',(-5.93404299900006,15.2,-8.86074904800001));
#284352=CARTESIAN_POINT('Ctrl Pts',(-5.93575682000006,15.2,-8.86228817900001));
#284353=CARTESIAN_POINT('Ctrl Pts',(-5.93747681900005,15.2,-8.86383013700001));
#284354=CARTESIAN_POINT('Ctrl Pts',(-5.93920299300006,15.2,-8.86537490400002));
#284355=CARTESIAN_POINT('Ctrl Pts',(-5.94093533700006,15.2,-8.86692246600001));
#284356=CARTESIAN_POINT('Ctrl Pts',(-5.94267384900006,15.2,-8.86847280400002));
#284357=CARTESIAN_POINT('Ctrl Pts',(-5.94441852600006,15.2,-8.87002590600002));
#284358=CARTESIAN_POINT('Ctrl Pts',(-5.94616936500006,15.2,-8.87158175200002));
#284359=CARTESIAN_POINT('Ctrl Pts',(-5.94792636200006,15.2,-8.87314032800001));
#284360=CARTESIAN_POINT('Ctrl Pts',(-5.94968951600006,15.2,-8.87470161900002));
#284361=CARTESIAN_POINT('Ctrl Pts',(-5.95145882200006,15.2,-8.87626560600001));
#284362=CARTESIAN_POINT('Ctrl Pts',(-5.95323427900006,15.2,-8.87783227600002));
#284363=CARTESIAN_POINT('Ctrl Pts',(-5.95501588200006,15.2,-8.87940161100002));
#284364=CARTESIAN_POINT('Ctrl Pts',(-5.95680362900006,15.2,-8.88097359800001));
#284365=CARTESIAN_POINT('Ctrl Pts',(-5.95859751600006,15.2,-8.88254821900002));
#284366=CARTESIAN_POINT('Ctrl Pts',(-5.96039754200006,15.2,-8.88412545900002));
#284367=CARTESIAN_POINT('Ctrl Pts',(-5.96220370200006,15.2,-8.88570530200001));
#284368=CARTESIAN_POINT('Ctrl Pts',(-5.96401599300005,15.2,-8.88728773400001));
#284369=CARTESIAN_POINT('Ctrl Pts',(-5.96583441200006,15.2,-8.88887273700002));
#284370=CARTESIAN_POINT('Ctrl Pts',(-5.96765895700006,15.2,-8.89046029700001));
#284371=CARTESIAN_POINT('Ctrl Pts',(-5.96948962500006,15.2,-8.89205039900002));
#284372=CARTESIAN_POINT('Ctrl Pts',(-5.97132641200006,15.2,-8.89364302600002));
#284373=CARTESIAN_POINT('Ctrl Pts',(-5.97316931400006,15.2,-8.89523816500001));
#284374=CARTESIAN_POINT('Ctrl Pts',(-5.97501833000006,15.2,-8.89683579900002));
#284375=CARTESIAN_POINT('Ctrl Pts',(-5.97687345600006,15.2,-8.89843591300002));
#284376=CARTESIAN_POINT('Ctrl Pts',(-5.97873468900006,15.2,-8.90003849100001));
#284377=CARTESIAN_POINT('Ctrl Pts',(-5.98060202600006,15.2,-8.90164352000001));
#284378=CARTESIAN_POINT('Ctrl Pts',(-5.98247546400006,15.2,-8.90325098400002));
#284379=CARTESIAN_POINT('Ctrl Pts',(-5.98435500000006,15.2,-8.90486086600001));
#284380=CARTESIAN_POINT('Ctrl Pts',(-5.98624062900006,15.2,-8.90647315300001));
#284381=CARTESIAN_POINT('Ctrl Pts',(-5.98813235200006,15.2,-8.90808783100002));
#284382=CARTESIAN_POINT('Ctrl Pts',(-5.99003016200006,15.2,-8.90970488200002));
#284383=CARTESIAN_POINT('Ctrl Pts',(-5.99193405800006,15.2,-8.91132429300002));
#284384=CARTESIAN_POINT('Ctrl Pts',(-5.99384403600006,15.2,-8.91294604900001));
#284385=CARTESIAN_POINT('Ctrl Pts',(-5.99576009400006,15.2,-8.91457013600002));
#284386=CARTESIAN_POINT('Ctrl Pts',(-5.99768222800006,15.2,-8.91619653700002));
#284387=CARTESIAN_POINT('Ctrl Pts',(-5.99961043400006,15.2,-8.91782524000002));
#284388=CARTESIAN_POINT('Ctrl Pts',(-6.00154471100006,15.2,-8.91945622800002));
#284389=CARTESIAN_POINT('Ctrl Pts',(-6.00348505500006,15.2,-8.92108948700002));
#284390=CARTESIAN_POINT('Ctrl Pts',(-6.00543146200006,15.2,-8.92272500300002));
#284391=CARTESIAN_POINT('Ctrl Pts',(-6.00738393100006,15.2,-8.92436276200002));
#284392=CARTESIAN_POINT('Ctrl Pts',(-6.00934245600006,15.2,-8.92600274700002));
#284393=CARTESIAN_POINT('Ctrl Pts',(-6.01130703700006,15.2,-8.92764494600002));
#284394=CARTESIAN_POINT('Ctrl Pts',(-6.01327766800006,15.2,-8.92928934400001));
#284395=CARTESIAN_POINT('Ctrl Pts',(-6.01525434800006,15.2,-8.93093592700002));
#284396=CARTESIAN_POINT('Ctrl Pts',(-6.01723707400006,15.2,-8.93258467900001));
#284397=CARTESIAN_POINT('Ctrl Pts',(-6.01922584100006,15.2,-8.93423558600002));
#284398=CARTESIAN_POINT('Ctrl Pts',(-6.02122064700006,15.2,-8.93588863500002));
#284399=CARTESIAN_POINT('Ctrl Pts',(-6.02322148900006,15.2,-8.93754381100001));
#284400=CARTESIAN_POINT('Ctrl Pts',(-6.02522836400006,15.2,-8.93920110000002));
#284401=CARTESIAN_POINT('Ctrl Pts',(-6.02724126900006,15.2,-8.94086048800002));
#284402=CARTESIAN_POINT('Ctrl Pts',(-6.02926019900006,15.2,-8.94252196100001));
#284403=CARTESIAN_POINT('Ctrl Pts',(-6.03128515400006,15.2,-8.94418550400001));
#284404=CARTESIAN_POINT('Ctrl Pts',(-6.03331612900006,15.2,-8.94585110500002));
#284405=CARTESIAN_POINT('Ctrl Pts',(-6.03535312000006,15.2,-8.94751874800002));
#284406=CARTESIAN_POINT('Ctrl Pts',(-6.03739612600006,15.2,-8.94918841900001));
#284407=CARTESIAN_POINT('Ctrl Pts',(-6.03944514200006,15.2,-8.95086010500002));
#284408=CARTESIAN_POINT('Ctrl Pts',(-6.04150016700006,15.2,-8.95253379300001));
#284409=CARTESIAN_POINT('Ctrl Pts',(-6.04356119600006,15.2,-8.95420946700002));
#284410=CARTESIAN_POINT('Ctrl Pts',(-6.04562822600006,15.2,-8.95588711400002));
#284411=CARTESIAN_POINT('Ctrl Pts',(-6.04770125400006,15.2,-8.95756672100001));
#284412=CARTESIAN_POINT('Ctrl Pts',(-6.04978027800006,15.2,-8.95924827300002));
#284413=CARTESIAN_POINT('Ctrl Pts',(-6.05186529400005,15.2,-8.96093175800001));
#284414=CARTESIAN_POINT('Ctrl Pts',(-6.05395629800006,15.2,-8.96261716200002));
#284415=CARTESIAN_POINT('Ctrl Pts',(-6.05605328900006,15.2,-8.96430447000002));
#284416=CARTESIAN_POINT('Ctrl Pts',(-6.05815626100005,15.2,-8.96599367000002));
#284417=CARTESIAN_POINT('Ctrl Pts',(-6.06026521300006,15.2,-8.96768474600002));
#284418=CARTESIAN_POINT('Ctrl Pts',(-6.06238014200006,15.2,-8.96937768800001));
#284419=CARTESIAN_POINT('Ctrl Pts',(-6.06450104400006,15.2,-8.97107248000001));
#284420=CARTESIAN_POINT('Ctrl Pts',(-6.06662791600006,15.2,-8.97276910900001));
#284421=CARTESIAN_POINT('Ctrl Pts',(-6.06876075400006,15.2,-8.97446756300001));
#284422=CARTESIAN_POINT('Ctrl Pts',(-6.07089955600006,15.2,-8.97616782700002));
#284423=CARTESIAN_POINT('Ctrl Pts',(-6.07304431900006,15.2,-8.97786988800001));
#284424=CARTESIAN_POINT('Ctrl Pts',(-6.07519504000006,15.2,-8.97957373400001));
#284425=CARTESIAN_POINT('Ctrl Pts',(-6.07735171400006,15.2,-8.98127934900002));
#284426=CARTESIAN_POINT('Ctrl Pts',(-6.07951433900006,15.2,-8.98298672300001));
#284427=CARTESIAN_POINT('Ctrl Pts',(-6.08168291200006,15.2,-8.98469584100001));
#284428=CARTESIAN_POINT('Ctrl Pts',(-6.08385743000006,15.2,-8.98640669100002));
#284429=CARTESIAN_POINT('Ctrl Pts',(-6.08603788900006,15.2,-8.98811925800001));
#284430=CARTESIAN_POINT('Ctrl Pts',(-6.08822428600006,15.2,-8.98983353000002));
#284431=CARTESIAN_POINT('Ctrl Pts',(-6.09041662000006,15.2,-8.99154949500002));
#284432=CARTESIAN_POINT('Ctrl Pts',(-6.09261488400006,15.2,-8.99326713800002));
#284433=CARTESIAN_POINT('Ctrl Pts',(-6.09481907700006,15.2,-8.99498644800002));
#284434=CARTESIAN_POINT('Ctrl Pts',(-6.09702919700006,15.2,-8.99670741000002));
#284435=CARTESIAN_POINT('Ctrl Pts',(-6.09924523800006,15.2,-8.99843001200002));
#284436=CARTESIAN_POINT('Ctrl Pts',(-6.10146719900006,15.2,-9.00015424200001));
#284437=CARTESIAN_POINT('Ctrl Pts',(-6.10369507600006,15.2,-9.00188008700002));
#284438=CARTESIAN_POINT('Ctrl Pts',(-6.10592886600006,15.2,-9.00360753300001));
#284439=CARTESIAN_POINT('Ctrl Pts',(-6.10816856500006,15.2,-9.00533656900001));
#284440=CARTESIAN_POINT('Ctrl Pts',(-6.11041417200005,15.2,-9.00706718000002));
#284441=CARTESIAN_POINT('Ctrl Pts',(-6.11266568000006,15.2,-9.00879935600001));
#284442=CARTESIAN_POINT('Ctrl Pts',(-6.11492309000006,15.2,-9.01053308200002));
#284443=CARTESIAN_POINT('Ctrl Pts',(-6.11718639600006,15.2,-9.01226834500001));
#284444=CARTESIAN_POINT('Ctrl Pts',(-6.11945559600006,15.2,-9.01400513500001));
#284445=CARTESIAN_POINT('Ctrl Pts',(-6.12173068600006,15.2,-9.01574343800002));
#284446=CARTESIAN_POINT('Ctrl Pts',(-6.12401166400006,15.2,-9.01748324100001));
#284447=CARTESIAN_POINT('Ctrl Pts',(-6.12629852600006,15.2,-9.01922453300001));
#284448=CARTESIAN_POINT('Ctrl Pts',(-6.12859126900006,15.2,-9.02096729900002));
#284449=CARTESIAN_POINT('Ctrl Pts',(-6.13088988900006,15.2,-9.02271152900001));
#284450=CARTESIAN_POINT('Ctrl Pts',(-6.13319438500006,15.2,-9.02445720900002));
#284451=CARTESIAN_POINT('Ctrl Pts',(-6.13550475100006,15.2,-9.02620432800001));
#284452=CARTESIAN_POINT('Ctrl Pts',(-6.13782098400006,15.2,-9.02795287300002));
#284453=CARTESIAN_POINT('Ctrl Pts',(-6.14014308400006,15.2,-9.02970283200002));
#284454=CARTESIAN_POINT('Ctrl Pts',(-6.14247104500006,15.2,-9.03145419100002));
#284455=CARTESIAN_POINT('Ctrl Pts',(-6.14480486400006,15.2,-9.03320694000002));
#284456=CARTESIAN_POINT('Ctrl Pts',(-6.14714453800006,15.2,-9.03496106700001));
#284457=CARTESIAN_POINT('Ctrl Pts',(-6.14949006400006,15.2,-9.03671655700002));
#284458=CARTESIAN_POINT('Ctrl Pts',(-6.15184143900006,15.2,-9.03847340000001));
#284459=CARTESIAN_POINT('Ctrl Pts',(-6.15419866000006,15.2,-9.04023158300001));
#284460=CARTESIAN_POINT('Ctrl Pts',(-6.15656172200006,15.2,-9.04199109600002));
#284461=CARTESIAN_POINT('Ctrl Pts',(-6.15893062400006,15.2,-9.04375192400002));
#284462=CARTESIAN_POINT('Ctrl Pts',(-6.16130536200005,15.2,-9.04551405600002));
#284463=CARTESIAN_POINT('Ctrl Pts',(-6.16368593200006,15.2,-9.04727748100001));
#284464=CARTESIAN_POINT('Ctrl Pts',(-6.16607233200006,15.2,-9.04904218600001));
#284465=CARTESIAN_POINT('Ctrl Pts',(-6.16846455700006,15.2,-9.05080815900002));
#284466=CARTESIAN_POINT('Ctrl Pts',(-6.17086260700006,15.2,-9.05257538800001));
#284467=CARTESIAN_POINT('Ctrl Pts',(-6.17326647500006,15.2,-9.05434386300002));
#284468=CARTESIAN_POINT('Ctrl Pts',(-6.17567615900006,15.2,-9.05611357000002));
#284469=CARTESIAN_POINT('Ctrl Pts',(-6.17809165700006,15.2,-9.05788449800001));
#284470=CARTESIAN_POINT('Ctrl Pts',(-6.18051296500005,15.2,-9.05965663400002));
#284471=CARTESIAN_POINT('Ctrl Pts',(-6.18294008000006,15.2,-9.06142996800002));
#284472=CARTESIAN_POINT('Ctrl Pts',(-6.18537299700006,15.2,-9.06320448700002));
#284473=CARTESIAN_POINT('Ctrl Pts',(-6.18781171500006,15.2,-9.06498018100002));
#284474=CARTESIAN_POINT('Ctrl Pts',(-6.19025623000006,15.2,-9.06675703600002));
#284475=CARTESIAN_POINT('Ctrl Pts',(-6.19270653900006,15.2,-9.06853504200001));
#284476=CARTESIAN_POINT('Ctrl Pts',(-6.19516263900006,15.2,-9.07031418600001));
#284477=CARTESIAN_POINT('Ctrl Pts',(-6.19762452500006,15.2,-9.07209445800002));
#284478=CARTESIAN_POINT('Ctrl Pts',(-6.20009219500006,15.2,-9.07387584600002));
#284479=CARTESIAN_POINT('Ctrl Pts',(-6.20256564600006,15.2,-9.07565833800002));
#284480=CARTESIAN_POINT('Ctrl Pts',(-6.20504487400006,15.2,-9.07744192200001));
#284481=CARTESIAN_POINT('Ctrl Pts',(-6.20752987700006,15.2,-9.07922658700001));
#284482=CARTESIAN_POINT('Ctrl Pts',(-6.21002065000006,15.2,-9.08101232300002));
#284483=CARTESIAN_POINT('Ctrl Pts',(-6.21251719100006,15.2,-9.08279911600001));
#284484=CARTESIAN_POINT('Ctrl Pts',(-6.21501949600006,15.2,-9.08458695700002));
#284485=CARTESIAN_POINT('Ctrl Pts',(-6.21752756200006,15.2,-9.08637583200001));
#284486=CARTESIAN_POINT('Ctrl Pts',(-6.22004138600006,15.2,-9.08816573200001));
#284487=CARTESIAN_POINT('Ctrl Pts',(-6.22256096500006,15.2,-9.08995664500001));
#284488=CARTESIAN_POINT('Ctrl Pts',(-6.22508629500006,15.2,-9.09174855900002));
#284489=CARTESIAN_POINT('Ctrl Pts',(-6.22761737300006,15.2,-9.09354146400002));
#284490=CARTESIAN_POINT('Ctrl Pts',(-6.23015419600006,15.2,-9.09533534700002));
#284491=CARTESIAN_POINT('Ctrl Pts',(-6.23269675900006,15.2,-9.09713019900002));
#284492=CARTESIAN_POINT('Ctrl Pts',(-6.23524506100006,15.2,-9.09892600700001));
#284493=CARTESIAN_POINT('Ctrl Pts',(-6.23779909800006,15.2,-9.10072276100001));
#284494=CARTESIAN_POINT('Ctrl Pts',(-6.24035886600006,15.2,-9.10252044800002));
#284495=CARTESIAN_POINT('Ctrl Pts',(-6.24292436400006,15.2,-9.10431905900002));
#284496=CARTESIAN_POINT('Ctrl Pts',(-6.24549558500005,15.2,-9.10611858200001));
#284497=CARTESIAN_POINT('Ctrl Pts',(-6.24807252900006,15.2,-9.10791900700002));
#284498=CARTESIAN_POINT('Ctrl Pts',(-6.25065519100006,15.2,-9.10972032100002));
#284499=CARTESIAN_POINT('Ctrl Pts',(-6.25324356800006,15.2,-9.11152251400001));
#284500=CARTESIAN_POINT('Ctrl Pts',(-6.25583765700005,15.2,-9.11332557600002));
#284501=CARTESIAN_POINT('Ctrl Pts',(-6.25843745500006,15.2,-9.11512949500001));
#284502=CARTESIAN_POINT('Ctrl Pts',(-6.26104295800006,15.2,-9.11693426000001));
#284503=CARTESIAN_POINT('Ctrl Pts',(-6.26365416200006,15.2,-9.11873986000002));
#284504=CARTESIAN_POINT('Ctrl Pts',(-6.26627106600006,15.2,-9.12054628500002));
#284505=CARTESIAN_POINT('Ctrl Pts',(-6.26889366400006,15.2,-9.12235352300002));
#284506=CARTESIAN_POINT('Ctrl Pts',(-6.27152195600006,15.2,-9.12416156500001));
#284507=CARTESIAN_POINT('Ctrl Pts',(-6.27415593500006,15.2,-9.12597039800002));
#284508=CARTESIAN_POINT('Ctrl Pts',(-6.27679559900006,15.2,-9.12778001300002));
#284509=CARTESIAN_POINT('Ctrl Pts',(-6.27944094700006,15.2,-9.12959039800001));
#284510=CARTESIAN_POINT('Ctrl Pts',(-6.28209197200006,15.2,-9.13140154300002));
#284511=CARTESIAN_POINT('Ctrl Pts',(-6.28474867400006,15.2,-9.13321343700002));
#284512=CARTESIAN_POINT('Ctrl Pts',(-6.28741104800006,15.2,-9.13502606900002));
#284513=CARTESIAN_POINT('Ctrl Pts',(-6.29007909100006,15.2,-9.13683942900001));
#284514=CARTESIAN_POINT('Ctrl Pts',(-6.29275279900006,15.2,-9.13865350600001));
#284515=CARTESIAN_POINT('Ctrl Pts',(-6.29543217000006,15.2,-9.14046829000002));
#284516=CARTESIAN_POINT('Ctrl Pts',(-6.29811719900006,15.2,-9.14228377000001));
#284517=CARTESIAN_POINT('Ctrl Pts',(-6.30080788400006,15.2,-9.14409993500002));
#284518=CARTESIAN_POINT('Ctrl Pts',(-6.30350422100006,15.2,-9.14591677500002));
#284519=CARTESIAN_POINT('Ctrl Pts',(-6.30620620800006,15.2,-9.14773428000002));
#284520=CARTESIAN_POINT('Ctrl Pts',(-6.30891384000006,15.2,-9.14955243900001));
#284521=CARTESIAN_POINT('Ctrl Pts',(-6.31162711400005,15.2,-9.15137124000001));
#284522=CARTESIAN_POINT('Ctrl Pts',(-6.31434602800006,15.2,-9.15319067500001));
#284523=CARTESIAN_POINT('Ctrl Pts',(-6.31707057700006,15.2,-9.15501073400002));
#284524=CARTESIAN_POINT('Ctrl Pts',(-6.31980075800006,15.2,-9.15683140300001));
#284525=CARTESIAN_POINT('Ctrl Pts',(-6.32253656800006,15.2,-9.15865267500001));
#284526=CARTESIAN_POINT('Ctrl Pts',(-6.32527800500006,15.2,-9.16047453800001));
#284527=CARTESIAN_POINT('Ctrl Pts',(-6.32802506300005,15.2,-9.16229698300001));
#284528=CARTESIAN_POINT('Ctrl Pts',(-6.33077774100006,15.2,-9.16411999900001));
#284529=CARTESIAN_POINT('Ctrl Pts',(-6.33353603400006,15.2,-9.16594357600001));
#284530=CARTESIAN_POINT('Ctrl Pts',(-6.33629993900006,15.2,-9.16776770200002));
#284531=CARTESIAN_POINT('Ctrl Pts',(-6.33906945400006,15.2,-9.16959237000002));
#284532=CARTESIAN_POINT('Ctrl Pts',(-6.34184457400006,15.2,-9.17141756700002));
#284533=CARTESIAN_POINT('Ctrl Pts',(-6.34462529700006,15.2,-9.17324328400002));
#284534=CARTESIAN_POINT('Ctrl Pts',(-6.34741161800005,15.2,-9.17506951100002));
#284535=CARTESIAN_POINT('Ctrl Pts',(-6.35020353500006,15.2,-9.17689623700002));
#284536=CARTESIAN_POINT('Ctrl Pts',(-6.35300104500006,15.2,-9.17872345400001));
#284537=CARTESIAN_POINT('Ctrl Pts',(-6.35580414300006,15.2,-9.18055114900002));
#284538=CARTESIAN_POINT('Ctrl Pts',(-6.35861282700006,15.2,-9.18237931400002));
#284539=CARTESIAN_POINT('Ctrl Pts',(-6.36142709400006,15.2,-9.18420793900001));
#284540=CARTESIAN_POINT('Ctrl Pts',(-6.36424693800006,15.2,-9.18603701200002));
#284541=CARTESIAN_POINT('Ctrl Pts',(-6.36707236000006,15.2,-9.18786652500001));
#284542=CARTESIAN_POINT('Ctrl Pts',(-6.36990335200006,15.2,-9.18969646800001));
#284543=CARTESIAN_POINT('Ctrl Pts',(-6.37273991300006,15.2,-9.19152682900001));
#284544=CARTESIAN_POINT('Ctrl Pts',(-6.37558204100006,15.2,-9.19335760100001));
#284545=CARTESIAN_POINT('Ctrl Pts',(-6.37842973000006,15.2,-9.19518877200002));
#284546=CARTESIAN_POINT('Ctrl Pts',(-6.38128297700006,15.2,-9.19702033200002));
#284547=CARTESIAN_POINT('Ctrl Pts',(-6.38414178100006,15.2,-9.19885227300002));
#284548=CARTESIAN_POINT('Ctrl Pts',(-6.38700613600006,15.2,-9.20068458400002));
#284549=CARTESIAN_POINT('Ctrl Pts',(-6.38987604000006,15.2,-9.20251725400002));
#284550=CARTESIAN_POINT('Ctrl Pts',(-6.39275149000006,15.2,-9.20435027600002));
#284551=CARTESIAN_POINT('Ctrl Pts',(-6.39563248000006,15.2,-9.20618363800001));
#284552=CARTESIAN_POINT('Ctrl Pts',(-6.39851901000006,15.2,-9.20801733000001));
#284553=CARTESIAN_POINT('Ctrl Pts',(-6.40141107500006,15.2,-9.20985134500001));
#284554=CARTESIAN_POINT('Ctrl Pts',(-6.40430867200006,15.2,-9.21168566900001));
#284555=CARTESIAN_POINT('Ctrl Pts',(-6.40721179700006,15.2,-9.21352029700002));
#284556=CARTESIAN_POINT('Ctrl Pts',(-6.41012044700005,15.2,-9.21535521600001));
#284557=CARTESIAN_POINT('Ctrl Pts',(-6.41303461900006,15.2,-9.21719041800002));
#284558=CARTESIAN_POINT('Ctrl Pts',(-6.41595430900006,15.2,-9.21902589200002));
#284559=CARTESIAN_POINT('Ctrl Pts',(-6.41887951300006,15.2,-9.22086163100002));
#284560=CARTESIAN_POINT('Ctrl Pts',(-6.42181023000005,15.2,-9.22269762200001));
#284561=CARTESIAN_POINT('Ctrl Pts',(-6.42474645500006,15.2,-9.22453385700001));
#284562=CARTESIAN_POINT('Ctrl Pts',(-6.42768818400006,15.2,-9.22637032800001));
#284563=CARTESIAN_POINT('Ctrl Pts',(-6.43063541500006,15.2,-9.22820702200001));
#284564=CARTESIAN_POINT('Ctrl Pts',(-6.43358814400006,15.2,-9.23004393300002));
#284565=CARTESIAN_POINT('Ctrl Pts',(-6.43654636800005,15.2,-9.23188105000002));
#284566=CARTESIAN_POINT('Ctrl Pts',(-6.43951008200006,15.2,-9.23371836400002));
#284567=CARTESIAN_POINT('Ctrl Pts',(-6.44247928500006,15.2,-9.23555586400001));
#284568=CARTESIAN_POINT('Ctrl Pts',(-6.44545397200006,15.2,-9.23739354200002));
#284569=CARTESIAN_POINT('Ctrl Pts',(-6.44843413900006,15.2,-9.23923138800001));
#284570=CARTESIAN_POINT('Ctrl Pts',(-6.45141978500006,15.2,-9.24106939400002));
#284571=CARTESIAN_POINT('Ctrl Pts',(-6.45441090500006,15.2,-9.24290754900002));
#284572=CARTESIAN_POINT('Ctrl Pts',(-6.45740749600006,15.2,-9.24474584400001));
#284573=CARTESIAN_POINT('Ctrl Pts',(-6.46040955400006,15.2,-9.24658427100002));
#284574=CARTESIAN_POINT('Ctrl Pts',(-6.46341707600006,15.2,-9.24842281800002));
#284575=CARTESIAN_POINT('Ctrl Pts',(-6.46643005900006,15.2,-9.25026147900001));
#284576=CARTESIAN_POINT('Ctrl Pts',(-6.46944849900006,15.2,-9.25210024200002));
#284577=CARTESIAN_POINT('Ctrl Pts',(-6.47247239300006,15.2,-9.25393910000002));
#284578=CARTESIAN_POINT('Ctrl Pts',(-6.47550173800005,15.2,-9.25577804100002));
#284579=CARTESIAN_POINT('Ctrl Pts',(-6.47853652900006,15.2,-9.25761705800002));
#284580=CARTESIAN_POINT('Ctrl Pts',(-6.48157676400006,15.2,-9.25945614200002));
#284581=CARTESIAN_POINT('Ctrl Pts',(-6.48462244000005,15.2,-9.26129528200001));
#284582=CARTESIAN_POINT('Ctrl Pts',(-6.48767355200006,15.2,-9.26313447100001));
#284583=CARTESIAN_POINT('Ctrl Pts',(-6.49073009700006,15.2,-9.26497369800002));
#284584=CARTESIAN_POINT('Ctrl Pts',(-6.49379207300006,15.2,-9.26681295500002));
#284585=CARTESIAN_POINT('Ctrl Pts',(-6.49685947500006,15.2,-9.26865223300002));
#284586=CARTESIAN_POINT('Ctrl Pts',(-6.49993230100006,15.2,-9.27049152200001));
#284587=CARTESIAN_POINT('Ctrl Pts',(-6.50301054600006,15.2,-9.27233081400002));
#284588=CARTESIAN_POINT('Ctrl Pts',(-6.50609420700006,15.2,-9.27417010000001));
#284589=CARTESIAN_POINT('Ctrl Pts',(-6.50918328200006,15.2,-9.27600936900001));
#284590=CARTESIAN_POINT('Ctrl Pts',(-6.51227776500006,15.2,-9.27784861500001));
#284591=CARTESIAN_POINT('Ctrl Pts',(-6.51537765500006,15.2,-9.27968782700002));
#284592=CARTESIAN_POINT('Ctrl Pts',(-6.51848294800006,15.2,-9.28152699600002));
#284593=CARTESIAN_POINT('Ctrl Pts',(-6.52159363900005,15.2,-9.28336611300002));
#284594=CARTESIAN_POINT('Ctrl Pts',(-6.52470972700006,15.2,-9.28520517200001));
#284595=CARTESIAN_POINT('Ctrl Pts',(-6.52783120600006,15.2,-9.28704416000001));
#284596=CARTESIAN_POINT('Ctrl Pts',(-6.53095807500006,15.2,-9.28888307000001));
#284597=CARTESIAN_POINT('Ctrl Pts',(-6.53409033000006,15.2,-9.29072189400001));
#284598=CARTESIAN_POINT('Ctrl Pts',(-6.53722796600006,15.2,-9.29256062200002));
#284599=CARTESIAN_POINT('Ctrl Pts',(-6.54037098100006,15.2,-9.29439924500001));
#284600=CARTESIAN_POINT('Ctrl Pts',(-6.54351937200006,15.2,-9.29623775500002));
#284601=CARTESIAN_POINT('Ctrl Pts',(-6.54667313400005,15.2,-9.29807614200002));
#284602=CARTESIAN_POINT('Ctrl Pts',(-6.54983226500006,15.2,-9.29991439900002));
#284603=CARTESIAN_POINT('Ctrl Pts',(-6.55299676000006,15.2,-9.30175251500001));
#284604=CARTESIAN_POINT('Ctrl Pts',(-6.55616661700006,15.2,-9.30359048400001));
#284605=CARTESIAN_POINT('Ctrl Pts',(-6.55934183200006,15.2,-9.30542829500002));
#284606=CARTESIAN_POINT('Ctrl Pts',(-6.56252240200006,15.2,-9.30726594200002));
#284607=CARTESIAN_POINT('Ctrl Pts',(-6.56570832300006,15.2,-9.30910341200001));
#284608=CARTESIAN_POINT('Ctrl Pts',(-6.56889959100006,15.2,-9.31094070000002));
#284609=CARTESIAN_POINT('Ctrl Pts',(-6.57209620400006,15.2,-9.31277779500002));
#284610=CARTESIAN_POINT('Ctrl Pts',(-6.57529815700006,15.2,-9.31461469100002));
#284611=CARTESIAN_POINT('Ctrl Pts',(-6.57850544800006,15.2,-9.31645137700002));
#284612=CARTESIAN_POINT('Ctrl Pts',(-6.58171807300006,15.2,-9.31828784500001));
#284613=CARTESIAN_POINT('Ctrl Pts',(-6.58493602700006,15.2,-9.32012408600002));
#284614=CARTESIAN_POINT('Ctrl Pts',(-6.58815931000006,15.2,-9.32196009500002));
#284615=CARTESIAN_POINT('Ctrl Pts',(-6.59138791700006,15.2,-9.32379585900001));
#284616=CARTESIAN_POINT('Ctrl Pts',(-6.59462184300006,15.2,-9.32563137200002));
#284617=CARTESIAN_POINT('Ctrl Pts',(-6.59786108600006,15.2,-9.32746662500002));
#284618=CARTESIAN_POINT('Ctrl Pts',(-6.60110564300005,15.2,-9.32930161000002));
#284619=CARTESIAN_POINT('Ctrl Pts',(-6.60435550800006,15.2,-9.33113631500002));
#284620=CARTESIAN_POINT('Ctrl Pts',(-6.60761068100006,15.2,-9.33297073500002));
#284621=CARTESIAN_POINT('Ctrl Pts',(-6.61087115500006,15.2,-9.33480485900001));
#284622=CARTESIAN_POINT('Ctrl Pts',(-6.61413692800005,15.2,-9.33663868000002));
#284623=CARTESIAN_POINT('Ctrl Pts',(-6.61740799800006,15.2,-9.33847218900001));
#284624=CARTESIAN_POINT('Ctrl Pts',(-6.62068436000006,15.2,-9.34030538000002));
#284625=CARTESIAN_POINT('Ctrl Pts',(-6.62396601100006,15.2,-9.34213824300001));
#284626=CARTESIAN_POINT('Ctrl Pts',(-6.62725294900006,15.2,-9.34397077300002));
#284627=CARTESIAN_POINT('Ctrl Pts',(-6.63054517000006,15.2,-9.34580296000001));
#284628=CARTESIAN_POINT('Ctrl Pts',(-6.63384267100006,15.2,-9.34763479700001));
#284629=CARTESIAN_POINT('Ctrl Pts',(-6.63714544700006,15.2,-9.34946627300001));
#284630=CARTESIAN_POINT('Ctrl Pts',(-6.64045349300006,15.2,-9.35129737900001));
#284631=CARTESIAN_POINT('Ctrl Pts',(-6.64376680700006,15.2,-9.35312810300001));
#284632=CARTESIAN_POINT('Ctrl Pts',(-6.64708538300006,15.2,-9.35495843700001));
#284633=CARTESIAN_POINT('Ctrl Pts',(-6.65040921900006,15.2,-9.35678837000001));
#284634=CARTESIAN_POINT('Ctrl Pts',(-6.65373831000006,15.2,-9.35861789600001));
#284635=CARTESIAN_POINT('Ctrl Pts',(-6.65707265500005,15.2,-9.36044701000002));
#284636=CARTESIAN_POINT('Ctrl Pts',(-6.66041225200006,15.2,-9.36227570600002));
#284637=CARTESIAN_POINT('Ctrl Pts',(-6.66375709900006,15.2,-9.36410398400002));
#284638=CARTESIAN_POINT('Ctrl Pts',(-6.66643717700006,15.2,-9.36556627000002));
#284639=CARTESIAN_POINT('Ctrl Pts',(-6.66844959800006,15.2,-9.36666279600002));
#284640=CARTESIAN_POINT('Ctrl Pts',(-6.66979226100006,15.2,-9.36739373000002));
#284641=CARTESIAN_POINT('Ctrl Pts',(-6.67046385600006,15.2,-9.36775917400002));
#284642=CARTESIAN_POINT('Ctrl Pts',(-6.57080831900006,15.2,-8.02901631800001));
#284643=CARTESIAN_POINT('Ctrl Pts',(-6.57080831900006,11.6,-8.02901631800001));
#284644=CARTESIAN_POINT('Ctrl Pts',(-6.57090674100006,15.2,-8.02916024100002));
#284645=CARTESIAN_POINT('Ctrl Pts',(-6.57090674100006,11.6,-8.02916024100002));
#284646=CARTESIAN_POINT('Ctrl Pts',(-6.57110695100006,15.2,-8.02945316300002));
#284647=CARTESIAN_POINT('Ctrl Pts',(-6.57110695100006,11.6,-8.02945316300002));
#284648=CARTESIAN_POINT('Ctrl Pts',(-6.57141009900006,15.2,-8.02989715700001));
#284649=CARTESIAN_POINT('Ctrl Pts',(-6.57141009900006,11.6,-8.02989715700001));
#284650=CARTESIAN_POINT('Ctrl Pts',(-6.57181802000006,15.2,-8.03049556400002));
#284651=CARTESIAN_POINT('Ctrl Pts',(-6.57181802000006,11.6,-8.03049556400002));
#284652=CARTESIAN_POINT('Ctrl Pts',(-6.57233322400006,15.2,-8.03125297300002));
#284653=CARTESIAN_POINT('Ctrl Pts',(-6.57233322400006,11.6,-8.03125297300002));
#284654=CARTESIAN_POINT('Ctrl Pts',(-6.57285600600006,15.2,-8.03202318500002));
#284655=CARTESIAN_POINT('Ctrl Pts',(-6.57285600600006,11.6,-8.03202318500002));
#284656=CARTESIAN_POINT('Ctrl Pts',(-6.57338335000006,15.2,-8.03280179700002));
#284657=CARTESIAN_POINT('Ctrl Pts',(-6.57338335000006,11.6,-8.03280179700002));
#284658=CARTESIAN_POINT('Ctrl Pts',(-6.57391522700006,15.2,-8.03358880000001));
#284659=CARTESIAN_POINT('Ctrl Pts',(-6.57391522700006,11.6,-8.03358880000001));
#284660=CARTESIAN_POINT('Ctrl Pts',(-6.57445160600005,15.2,-8.03438417800002));
#284661=CARTESIAN_POINT('Ctrl Pts',(-6.57445160600005,11.6,-8.03438417800002));
#284662=CARTESIAN_POINT('Ctrl Pts',(-6.57499245700006,15.2,-8.03518792300002));
#284663=CARTESIAN_POINT('Ctrl Pts',(-6.57499245700006,11.6,-8.03518792300002));
#284664=CARTESIAN_POINT('Ctrl Pts',(-6.57553775200006,15.2,-8.03600002100002));
#284665=CARTESIAN_POINT('Ctrl Pts',(-6.57553775200006,11.6,-8.03600002100002));
#284666=CARTESIAN_POINT('Ctrl Pts',(-6.57608746000006,15.2,-8.03682046000001));
#284667=CARTESIAN_POINT('Ctrl Pts',(-6.57608746000006,11.6,-8.03682046000001));
#284668=CARTESIAN_POINT('Ctrl Pts',(-6.57664155100006,15.2,-8.03764922800001));
#284669=CARTESIAN_POINT('Ctrl Pts',(-6.57664155100006,11.6,-8.03764922800001));
#284670=CARTESIAN_POINT('Ctrl Pts',(-6.57719999700006,15.2,-8.03848631500001));
#284671=CARTESIAN_POINT('Ctrl Pts',(-6.57719999700006,11.6,-8.03848631500001));
#284672=CARTESIAN_POINT('Ctrl Pts',(-6.57776276900006,15.2,-8.03933170500001));
#284673=CARTESIAN_POINT('Ctrl Pts',(-6.57776276900006,11.6,-8.03933170500001));
#284674=CARTESIAN_POINT('Ctrl Pts',(-6.57832983700006,15.2,-8.04018539000002));
#284675=CARTESIAN_POINT('Ctrl Pts',(-6.57832983700006,11.6,-8.04018539000002));
#284676=CARTESIAN_POINT('Ctrl Pts',(-6.57890117200005,15.2,-8.04104735800001));
#284677=CARTESIAN_POINT('Ctrl Pts',(-6.57890117200005,11.6,-8.04104735800001));
#284678=CARTESIAN_POINT('Ctrl Pts',(-6.57947674700006,15.2,-8.04191759500002));
#284679=CARTESIAN_POINT('Ctrl Pts',(-6.57947674700006,11.6,-8.04191759500002));
#284680=CARTESIAN_POINT('Ctrl Pts',(-6.58005653200005,15.2,-8.04279609000002));
#284681=CARTESIAN_POINT('Ctrl Pts',(-6.58005653200005,11.6,-8.04279609000002));
#284682=CARTESIAN_POINT('Ctrl Pts',(-6.58064050000006,15.2,-8.04368283300001));
#284683=CARTESIAN_POINT('Ctrl Pts',(-6.58064050000006,11.6,-8.04368283300001));
#284684=CARTESIAN_POINT('Ctrl Pts',(-6.58122862000006,15.2,-8.04457781100002));
#284685=CARTESIAN_POINT('Ctrl Pts',(-6.58122862000006,11.6,-8.04457781100002));
#284686=CARTESIAN_POINT('Ctrl Pts',(-6.58182086700006,15.2,-8.04548101200002));
#284687=CARTESIAN_POINT('Ctrl Pts',(-6.58182086700006,11.6,-8.04548101200002));
#284688=CARTESIAN_POINT('Ctrl Pts',(-6.58241721200006,15.2,-8.04639242700001));
#284689=CARTESIAN_POINT('Ctrl Pts',(-6.58241721200006,11.6,-8.04639242700001));
#284690=CARTESIAN_POINT('Ctrl Pts',(-6.58301762700006,15.2,-8.04731204200002));
#284691=CARTESIAN_POINT('Ctrl Pts',(-6.58301762700006,11.6,-8.04731204200002));
#284692=CARTESIAN_POINT('Ctrl Pts',(-6.58362208300006,15.2,-8.04823984600001));
#284693=CARTESIAN_POINT('Ctrl Pts',(-6.58362208300006,11.6,-8.04823984600001));
#284694=CARTESIAN_POINT('Ctrl Pts',(-6.58423055400006,15.2,-8.04917582900002));
#284695=CARTESIAN_POINT('Ctrl Pts',(-6.58423055400006,11.6,-8.04917582900002));
#284696=CARTESIAN_POINT('Ctrl Pts',(-6.58484301300006,15.2,-8.05011997800002));
#284697=CARTESIAN_POINT('Ctrl Pts',(-6.58484301300006,11.6,-8.05011997800002));
#284698=CARTESIAN_POINT('Ctrl Pts',(-6.58545943100005,15.2,-8.05107228200002));
#284699=CARTESIAN_POINT('Ctrl Pts',(-6.58545943100005,11.6,-8.05107228200002));
#284700=CARTESIAN_POINT('Ctrl Pts',(-6.58607978300005,15.2,-8.05203273100001));
#284701=CARTESIAN_POINT('Ctrl Pts',(-6.58607978300005,11.6,-8.05203273100001));
#284702=CARTESIAN_POINT('Ctrl Pts',(-6.58670404000006,15.2,-8.05300131300001));
#284703=CARTESIAN_POINT('Ctrl Pts',(-6.58670404000006,11.6,-8.05300131300001));
#284704=CARTESIAN_POINT('Ctrl Pts',(-6.58733217600005,15.2,-8.05397801700002));
#284705=CARTESIAN_POINT('Ctrl Pts',(-6.58733217600005,11.6,-8.05397801700002));
#284706=CARTESIAN_POINT('Ctrl Pts',(-6.58796416400006,15.2,-8.05496283100002));
#284707=CARTESIAN_POINT('Ctrl Pts',(-6.58796416400006,11.6,-8.05496283100002));
#284708=CARTESIAN_POINT('Ctrl Pts',(-6.58859997800006,15.2,-8.05595574500002));
#284709=CARTESIAN_POINT('Ctrl Pts',(-6.58859997800006,11.6,-8.05595574500002));
#284710=CARTESIAN_POINT('Ctrl Pts',(-6.58923959000006,15.2,-8.05695674700001));
#284711=CARTESIAN_POINT('Ctrl Pts',(-6.58923959000006,11.6,-8.05695674700001));
#284712=CARTESIAN_POINT('Ctrl Pts',(-6.58988297600006,15.2,-8.05796582700001));
#284713=CARTESIAN_POINT('Ctrl Pts',(-6.58988297600006,11.6,-8.05796582700001));
#284714=CARTESIAN_POINT('Ctrl Pts',(-6.59053010700006,15.2,-8.05898297300002));
#284715=CARTESIAN_POINT('Ctrl Pts',(-6.59053010700006,11.6,-8.05898297300002));
#284716=CARTESIAN_POINT('Ctrl Pts',(-6.59118095900006,15.2,-8.06000817400001));
#284717=CARTESIAN_POINT('Ctrl Pts',(-6.59118095900006,11.6,-8.06000817400001));
#284718=CARTESIAN_POINT('Ctrl Pts',(-6.59183550500006,15.2,-8.06104142000001));
#284719=CARTESIAN_POINT('Ctrl Pts',(-6.59183550500006,11.6,-8.06104142000001));
#284720=CARTESIAN_POINT('Ctrl Pts',(-6.59249371900006,15.2,-8.06208270100001));
#284721=CARTESIAN_POINT('Ctrl Pts',(-6.59249371900006,11.6,-8.06208270100001));
#284722=CARTESIAN_POINT('Ctrl Pts',(-6.59315557600006,15.2,-8.06313200300002));
#284723=CARTESIAN_POINT('Ctrl Pts',(-6.59315557600006,11.6,-8.06313200300002));
#284724=CARTESIAN_POINT('Ctrl Pts',(-6.59382104900006,15.2,-8.06418931800001));
#284725=CARTESIAN_POINT('Ctrl Pts',(-6.59382104900006,11.6,-8.06418931800001));
#284726=CARTESIAN_POINT('Ctrl Pts',(-6.59449011500006,15.2,-8.06525463500002));
#284727=CARTESIAN_POINT('Ctrl Pts',(-6.59449011500006,11.6,-8.06525463500002));
#284728=CARTESIAN_POINT('Ctrl Pts',(-6.59516274600006,15.2,-8.06632794100001));
#284729=CARTESIAN_POINT('Ctrl Pts',(-6.59516274600006,11.6,-8.06632794100001));
#284730=CARTESIAN_POINT('Ctrl Pts',(-6.59583891700006,15.2,-8.06740922800002));
#284731=CARTESIAN_POINT('Ctrl Pts',(-6.59583891700006,11.6,-8.06740922800002));
#284732=CARTESIAN_POINT('Ctrl Pts',(-6.59651860500006,15.2,-8.06849848300002));
#284733=CARTESIAN_POINT('Ctrl Pts',(-6.59651860500006,11.6,-8.06849848300002));
#284734=CARTESIAN_POINT('Ctrl Pts',(-6.59720178300006,15.2,-8.06959569800001));
#284735=CARTESIAN_POINT('Ctrl Pts',(-6.59720178300006,11.6,-8.06959569800001));
#284736=CARTESIAN_POINT('Ctrl Pts',(-6.59788842600006,15.2,-8.07070086000002));
#284737=CARTESIAN_POINT('Ctrl Pts',(-6.59788842600006,11.6,-8.07070086000002));
#284738=CARTESIAN_POINT('Ctrl Pts',(-6.59857851000006,15.2,-8.07181396000002));
#284739=CARTESIAN_POINT('Ctrl Pts',(-6.59857851000006,11.6,-8.07181396000002));
#284740=CARTESIAN_POINT('Ctrl Pts',(-6.59927200900006,15.2,-8.07293498700002));
#284741=CARTESIAN_POINT('Ctrl Pts',(-6.59927200900006,11.6,-8.07293498700002));
#284742=CARTESIAN_POINT('Ctrl Pts',(-6.59996890100006,15.2,-8.07406392900001));
#284743=CARTESIAN_POINT('Ctrl Pts',(-6.59996890100006,11.6,-8.07406392900001));
#284744=CARTESIAN_POINT('Ctrl Pts',(-6.60066916000006,15.2,-8.07520077800002));
#284745=CARTESIAN_POINT('Ctrl Pts',(-6.60066916000006,11.6,-8.07520077800002));
#284746=CARTESIAN_POINT('Ctrl Pts',(-6.60137276000006,15.2,-8.07634552200001));
#284747=CARTESIAN_POINT('Ctrl Pts',(-6.60137276000006,11.6,-8.07634552200001));
#284748=CARTESIAN_POINT('Ctrl Pts',(-6.60207968000006,15.2,-8.07749815200001));
#284749=CARTESIAN_POINT('Ctrl Pts',(-6.60207968000006,11.6,-8.07749815200001));
#284750=CARTESIAN_POINT('Ctrl Pts',(-6.60278989300005,15.2,-8.07865865600002));
#284751=CARTESIAN_POINT('Ctrl Pts',(-6.60278989300005,11.6,-8.07865865600002));
#284752=CARTESIAN_POINT('Ctrl Pts',(-6.60350337600006,15.2,-8.07982702500002));
#284753=CARTESIAN_POINT('Ctrl Pts',(-6.60350337600006,11.6,-8.07982702500002));
#284754=CARTESIAN_POINT('Ctrl Pts',(-6.60422010600006,15.2,-8.08100324800002));
#284755=CARTESIAN_POINT('Ctrl Pts',(-6.60422010600006,11.6,-8.08100324800002));
#284756=CARTESIAN_POINT('Ctrl Pts',(-6.60494005800006,15.2,-8.08218731500002));
#284757=CARTESIAN_POINT('Ctrl Pts',(-6.60494005800006,11.6,-8.08218731500002));
#284758=CARTESIAN_POINT('Ctrl Pts',(-6.60566320900006,15.2,-8.08337921500001));
#284759=CARTESIAN_POINT('Ctrl Pts',(-6.60566320900006,11.6,-8.08337921500001));
#284760=CARTESIAN_POINT('Ctrl Pts',(-6.60638953400006,15.2,-8.08457893900002));
#284761=CARTESIAN_POINT('Ctrl Pts',(-6.60638953400006,11.6,-8.08457893900002));
#284762=CARTESIAN_POINT('Ctrl Pts',(-6.60711901100006,15.2,-8.08578647500001));
#284763=CARTESIAN_POINT('Ctrl Pts',(-6.60711901100006,11.6,-8.08578647500001));
#284764=CARTESIAN_POINT('Ctrl Pts',(-6.60785161500006,15.2,-8.08700181500001));
#284765=CARTESIAN_POINT('Ctrl Pts',(-6.60785161500006,11.6,-8.08700181500001));
#284766=CARTESIAN_POINT('Ctrl Pts',(-6.60858732500006,15.2,-8.08822494800001));
#284767=CARTESIAN_POINT('Ctrl Pts',(-6.60858732500006,11.6,-8.08822494800001));
#284768=CARTESIAN_POINT('Ctrl Pts',(-6.60932611700006,15.2,-8.08945586400002));
#284769=CARTESIAN_POINT('Ctrl Pts',(-6.60932611700006,11.6,-8.08945586400002));
#284770=CARTESIAN_POINT('Ctrl Pts',(-6.61006796600006,15.2,-8.09069455200002));
#284771=CARTESIAN_POINT('Ctrl Pts',(-6.61006796600006,11.6,-8.09069455200002));
#284772=CARTESIAN_POINT('Ctrl Pts',(-6.61081285100006,15.2,-8.09194100300001));
#284773=CARTESIAN_POINT('Ctrl Pts',(-6.61081285100006,11.6,-8.09194100300001));
#284774=CARTESIAN_POINT('Ctrl Pts',(-6.61156074900005,15.2,-8.09319520700001));
#284775=CARTESIAN_POINT('Ctrl Pts',(-6.61156074900005,11.6,-8.09319520700001));
#284776=CARTESIAN_POINT('Ctrl Pts',(-6.61231163600006,15.2,-8.09445715400001));
#284777=CARTESIAN_POINT('Ctrl Pts',(-6.61231163600006,11.6,-8.09445715400001));
#284778=CARTESIAN_POINT('Ctrl Pts',(-6.61306549000006,15.2,-8.09572683400001));
#284779=CARTESIAN_POINT('Ctrl Pts',(-6.61306549000006,11.6,-8.09572683400001));
#284780=CARTESIAN_POINT('Ctrl Pts',(-6.61382229000006,15.2,-8.09700423600002));
#284781=CARTESIAN_POINT('Ctrl Pts',(-6.61382229000006,11.6,-8.09700423600002));
#284782=CARTESIAN_POINT('Ctrl Pts',(-6.61458201100006,15.2,-8.09828935200001));
#284783=CARTESIAN_POINT('Ctrl Pts',(-6.61458201100006,11.6,-8.09828935200001));
#284784=CARTESIAN_POINT('Ctrl Pts',(-6.61534463100006,15.2,-8.09958217100002));
#284785=CARTESIAN_POINT('Ctrl Pts',(-6.61534463100006,11.6,-8.09958217100002));
#284786=CARTESIAN_POINT('Ctrl Pts',(-6.61611012900006,15.2,-8.10088268300002));
#284787=CARTESIAN_POINT('Ctrl Pts',(-6.61611012900006,11.6,-8.10088268300002));
#284788=CARTESIAN_POINT('Ctrl Pts',(-6.61687848200006,15.2,-8.10219087900002));
#284789=CARTESIAN_POINT('Ctrl Pts',(-6.61687848200006,11.6,-8.10219087900002));
#284790=CARTESIAN_POINT('Ctrl Pts',(-6.61764966700006,15.2,-8.10350674900001));
#284791=CARTESIAN_POINT('Ctrl Pts',(-6.61764966700006,11.6,-8.10350674900001));
#284792=CARTESIAN_POINT('Ctrl Pts',(-6.61842366400006,15.2,-8.10483028300002));
#284793=CARTESIAN_POINT('Ctrl Pts',(-6.61842366400006,11.6,-8.10483028300002));
#284794=CARTESIAN_POINT('Ctrl Pts',(-6.61920045000006,15.2,-8.10616147100001));
#284795=CARTESIAN_POINT('Ctrl Pts',(-6.61920045000006,11.6,-8.10616147100001));
#284796=CARTESIAN_POINT('Ctrl Pts',(-6.61998000200006,15.2,-8.10750030400002));
#284797=CARTESIAN_POINT('Ctrl Pts',(-6.61998000200006,11.6,-8.10750030400002));
#284798=CARTESIAN_POINT('Ctrl Pts',(-6.62076230000006,15.2,-8.10884677100002));
#284799=CARTESIAN_POINT('Ctrl Pts',(-6.62076230000006,11.6,-8.10884677100002));
#284800=CARTESIAN_POINT('Ctrl Pts',(-6.62154732100006,15.2,-8.11020086400001));
#284801=CARTESIAN_POINT('Ctrl Pts',(-6.62154732100006,11.6,-8.11020086400001));
#284802=CARTESIAN_POINT('Ctrl Pts',(-6.62233504600006,15.2,-8.11156257400001));
#284803=CARTESIAN_POINT('Ctrl Pts',(-6.62233504600006,11.6,-8.11156257400001));
#284804=CARTESIAN_POINT('Ctrl Pts',(-6.62312545000006,15.2,-8.11293188900001));
#284805=CARTESIAN_POINT('Ctrl Pts',(-6.62312545000006,11.6,-8.11293188900001));
#284806=CARTESIAN_POINT('Ctrl Pts',(-6.62391851400006,15.2,-8.11430880100002));
#284807=CARTESIAN_POINT('Ctrl Pts',(-6.62391851400006,11.6,-8.11430880100002));
#284808=CARTESIAN_POINT('Ctrl Pts',(-6.62471421500006,15.2,-8.11569329900001));
#284809=CARTESIAN_POINT('Ctrl Pts',(-6.62471421500006,11.6,-8.11569329900001));
#284810=CARTESIAN_POINT('Ctrl Pts',(-6.62551253400006,15.2,-8.11708537600002));
#284811=CARTESIAN_POINT('Ctrl Pts',(-6.62551253400006,11.6,-8.11708537600002));
#284812=CARTESIAN_POINT('Ctrl Pts',(-6.62631344800006,15.2,-8.11848502000002));
#284813=CARTESIAN_POINT('Ctrl Pts',(-6.62631344800006,11.6,-8.11848502000002));
#284814=CARTESIAN_POINT('Ctrl Pts',(-6.62711693700006,15.2,-8.11989222400002));
#284815=CARTESIAN_POINT('Ctrl Pts',(-6.62711693700006,11.6,-8.11989222400002));
#284816=CARTESIAN_POINT('Ctrl Pts',(-6.62792298000006,15.2,-8.12130697600002));
#284817=CARTESIAN_POINT('Ctrl Pts',(-6.62792298000006,11.6,-8.12130697600002));
#284818=CARTESIAN_POINT('Ctrl Pts',(-6.62873155500006,15.2,-8.12272926700001));
#284819=CARTESIAN_POINT('Ctrl Pts',(-6.62873155500006,11.6,-8.12272926700001));
#284820=CARTESIAN_POINT('Ctrl Pts',(-6.62954264200006,15.2,-8.12415909000002));
#284821=CARTESIAN_POINT('Ctrl Pts',(-6.62954264200006,11.6,-8.12415909000002));
#284822=CARTESIAN_POINT('Ctrl Pts',(-6.63035622100006,15.2,-8.12559643400002));
#284823=CARTESIAN_POINT('Ctrl Pts',(-6.63035622100006,11.6,-8.12559643400002));
#284824=CARTESIAN_POINT('Ctrl Pts',(-6.63117227000006,15.2,-8.12704128900002));
#284825=CARTESIAN_POINT('Ctrl Pts',(-6.63117227000006,11.6,-8.12704128900002));
#284826=CARTESIAN_POINT('Ctrl Pts',(-6.63199077100006,15.2,-8.12849364600002));
#284827=CARTESIAN_POINT('Ctrl Pts',(-6.63199077100006,11.6,-8.12849364600002));
#284828=CARTESIAN_POINT('Ctrl Pts',(-6.63281170000006,15.2,-8.12995349700002));
#284829=CARTESIAN_POINT('Ctrl Pts',(-6.63281170000006,11.6,-8.12995349700002));
#284830=CARTESIAN_POINT('Ctrl Pts',(-6.63363504000006,15.2,-8.13142083100002));
#284831=CARTESIAN_POINT('Ctrl Pts',(-6.63363504000006,11.6,-8.13142083100002));
#284832=CARTESIAN_POINT('Ctrl Pts',(-6.63446076800006,15.2,-8.13289564100002));
#284833=CARTESIAN_POINT('Ctrl Pts',(-6.63446076800006,11.6,-8.13289564100002));
#284834=CARTESIAN_POINT('Ctrl Pts',(-6.63528886600006,15.2,-8.13437791500002));
#284835=CARTESIAN_POINT('Ctrl Pts',(-6.63528886600006,11.6,-8.13437791500002));
#284836=CARTESIAN_POINT('Ctrl Pts',(-6.63611931200006,15.2,-8.13586764600002));
#284837=CARTESIAN_POINT('Ctrl Pts',(-6.63611931200006,11.6,-8.13586764600002));
#284838=CARTESIAN_POINT('Ctrl Pts',(-6.63695208700006,15.2,-8.13736482400002));
#284839=CARTESIAN_POINT('Ctrl Pts',(-6.63695208700006,11.6,-8.13736482400002));
#284840=CARTESIAN_POINT('Ctrl Pts',(-6.63778717100006,15.2,-8.13886943900001));
#284841=CARTESIAN_POINT('Ctrl Pts',(-6.63778717100006,11.6,-8.13886943900001));
#284842=CARTESIAN_POINT('Ctrl Pts',(-6.63862454400006,15.2,-8.14038148300002));
#284843=CARTESIAN_POINT('Ctrl Pts',(-6.63862454400006,11.6,-8.14038148300002));
#284844=CARTESIAN_POINT('Ctrl Pts',(-6.63946418700006,15.2,-8.14190094700002));
#284845=CARTESIAN_POINT('Ctrl Pts',(-6.63946418700006,11.6,-8.14190094700002));
#284846=CARTESIAN_POINT('Ctrl Pts',(-6.64030607900005,15.2,-8.14342782100002));
#284847=CARTESIAN_POINT('Ctrl Pts',(-6.64030607900005,11.6,-8.14342782100002));
#284848=CARTESIAN_POINT('Ctrl Pts',(-6.64115020100006,15.2,-8.14496209700001));
#284849=CARTESIAN_POINT('Ctrl Pts',(-6.64115020100006,11.6,-8.14496209700001));
#284850=CARTESIAN_POINT('Ctrl Pts',(-6.64199653400006,15.2,-8.14650376600002));
#284851=CARTESIAN_POINT('Ctrl Pts',(-6.64199653400006,11.6,-8.14650376600002));
#284852=CARTESIAN_POINT('Ctrl Pts',(-6.64284505800006,15.2,-8.14805281700002));
#284853=CARTESIAN_POINT('Ctrl Pts',(-6.64284505800006,11.6,-8.14805281700002));
#284854=CARTESIAN_POINT('Ctrl Pts',(-6.64369575300006,15.2,-8.14960924300001));
#284855=CARTESIAN_POINT('Ctrl Pts',(-6.64369575300006,11.6,-8.14960924300001));
#284856=CARTESIAN_POINT('Ctrl Pts',(-6.64454859900006,15.2,-8.15117303500001));
#284857=CARTESIAN_POINT('Ctrl Pts',(-6.64454859900006,11.6,-8.15117303500001));
#284858=CARTESIAN_POINT('Ctrl Pts',(-6.64540358000006,15.2,-8.15274418300002));
#284859=CARTESIAN_POINT('Ctrl Pts',(-6.64540358000006,11.6,-8.15274418300002));
#284860=CARTESIAN_POINT('Ctrl Pts',(-6.64626067400006,15.2,-8.15432267900002));
#284861=CARTESIAN_POINT('Ctrl Pts',(-6.64626067400006,11.6,-8.15432267900002));
#284862=CARTESIAN_POINT('Ctrl Pts',(-6.64711986400006,15.2,-8.15590851400002));
#284863=CARTESIAN_POINT('Ctrl Pts',(-6.64711986400006,11.6,-8.15590851400002));
#284864=CARTESIAN_POINT('Ctrl Pts',(-6.64798112800006,15.2,-8.15750167800001));
#284865=CARTESIAN_POINT('Ctrl Pts',(-6.64798112800006,11.6,-8.15750167800001));
#284866=CARTESIAN_POINT('Ctrl Pts',(-6.64884444900006,15.2,-8.15910216300002));
#284867=CARTESIAN_POINT('Ctrl Pts',(-6.64884444900006,11.6,-8.15910216300002));
#284868=CARTESIAN_POINT('Ctrl Pts',(-6.64970980800006,15.2,-8.16070996000001));
#284869=CARTESIAN_POINT('Ctrl Pts',(-6.64970980800006,11.6,-8.16070996000001));
#284870=CARTESIAN_POINT('Ctrl Pts',(-6.65057718600006,15.2,-8.16232506100001));
#284871=CARTESIAN_POINT('Ctrl Pts',(-6.65057718600006,11.6,-8.16232506100001));
#284872=CARTESIAN_POINT('Ctrl Pts',(-6.65144656600006,15.2,-8.16394745500002));
#284873=CARTESIAN_POINT('Ctrl Pts',(-6.65144656600006,11.6,-8.16394745500002));
#284874=CARTESIAN_POINT('Ctrl Pts',(-6.65231792600006,15.2,-8.16557713600002));
#284875=CARTESIAN_POINT('Ctrl Pts',(-6.65231792600006,11.6,-8.16557713600002));
#284876=CARTESIAN_POINT('Ctrl Pts',(-6.65319124900006,15.2,-8.16721409300002));
#284877=CARTESIAN_POINT('Ctrl Pts',(-6.65319124900006,11.6,-8.16721409300002));
#284878=CARTESIAN_POINT('Ctrl Pts',(-6.65406651700006,15.2,-8.16885831900001));
#284879=CARTESIAN_POINT('Ctrl Pts',(-6.65406651700006,11.6,-8.16885831900001));
#284880=CARTESIAN_POINT('Ctrl Pts',(-6.65494371100006,15.2,-8.17050980400002));
#284881=CARTESIAN_POINT('Ctrl Pts',(-6.65494371100006,11.6,-8.17050980400002));
#284882=CARTESIAN_POINT('Ctrl Pts',(-6.65582281300006,15.2,-8.17216853900002));
#284883=CARTESIAN_POINT('Ctrl Pts',(-6.65582281300006,11.6,-8.17216853900002));
#284884=CARTESIAN_POINT('Ctrl Pts',(-6.65670380500006,15.2,-8.17383451600002));
#284885=CARTESIAN_POINT('Ctrl Pts',(-6.65670380500006,11.6,-8.17383451600002));
#284886=CARTESIAN_POINT('Ctrl Pts',(-6.65758666800006,15.2,-8.17550772700002));
#284887=CARTESIAN_POINT('Ctrl Pts',(-6.65758666800006,11.6,-8.17550772700002));
#284888=CARTESIAN_POINT('Ctrl Pts',(-6.65847138400006,15.2,-8.17718816300001));
#284889=CARTESIAN_POINT('Ctrl Pts',(-6.65847138400006,11.6,-8.17718816300001));
#284890=CARTESIAN_POINT('Ctrl Pts',(-6.65935793500006,15.2,-8.17887581400001));
#284891=CARTESIAN_POINT('Ctrl Pts',(-6.65935793500006,11.6,-8.17887581400001));
#284892=CARTESIAN_POINT('Ctrl Pts',(-6.66024630300006,15.2,-8.18057067400002));
#284893=CARTESIAN_POINT('Ctrl Pts',(-6.66024630300006,11.6,-8.18057067400002));
#284894=CARTESIAN_POINT('Ctrl Pts',(-6.66113647000006,15.2,-8.18227273100002));
#284895=CARTESIAN_POINT('Ctrl Pts',(-6.66113647000006,11.6,-8.18227273100002));
#284896=CARTESIAN_POINT('Ctrl Pts',(-6.66202841900006,15.2,-8.18398198000001));
#284897=CARTESIAN_POINT('Ctrl Pts',(-6.66202841900006,11.6,-8.18398198000001));
#284898=CARTESIAN_POINT('Ctrl Pts',(-6.66292212900006,15.2,-8.18569840900001));
#284899=CARTESIAN_POINT('Ctrl Pts',(-6.66292212900006,11.6,-8.18569840900001));
#284900=CARTESIAN_POINT('Ctrl Pts',(-6.66381758700005,15.2,-8.18742201300001));
#284901=CARTESIAN_POINT('Ctrl Pts',(-6.66381758700005,11.6,-8.18742201300001));
#284902=CARTESIAN_POINT('Ctrl Pts',(-6.66471477200006,15.2,-8.18915278000001));
#284903=CARTESIAN_POINT('Ctrl Pts',(-6.66471477200006,11.6,-8.18915278000001));
#284904=CARTESIAN_POINT('Ctrl Pts',(-6.66561366700006,15.2,-8.19089070400001));
#284905=CARTESIAN_POINT('Ctrl Pts',(-6.66561366700006,11.6,-8.19089070400001));
#284906=CARTESIAN_POINT('Ctrl Pts',(-6.66651425400006,15.2,-8.19263577600001));
#284907=CARTESIAN_POINT('Ctrl Pts',(-6.66651425400006,11.6,-8.19263577600001));
#284908=CARTESIAN_POINT('Ctrl Pts',(-6.66741651800006,15.2,-8.19438798600002));
#284909=CARTESIAN_POINT('Ctrl Pts',(-6.66741651800006,11.6,-8.19438798600002));
#284910=CARTESIAN_POINT('Ctrl Pts',(-6.66832043800006,15.2,-8.19614732700002));
#284911=CARTESIAN_POINT('Ctrl Pts',(-6.66832043800006,11.6,-8.19614732700002));
#284912=CARTESIAN_POINT('Ctrl Pts',(-6.66922600000006,15.2,-8.19791379200002));
#284913=CARTESIAN_POINT('Ctrl Pts',(-6.66922600000006,11.6,-8.19791379200002));
#284914=CARTESIAN_POINT('Ctrl Pts',(-6.67013318300006,15.2,-8.19968736900002));
#284915=CARTESIAN_POINT('Ctrl Pts',(-6.67013318300006,11.6,-8.19968736900002));
#284916=CARTESIAN_POINT('Ctrl Pts',(-6.67104197300006,15.2,-8.20146805200002));
#284917=CARTESIAN_POINT('Ctrl Pts',(-6.67104197300006,11.6,-8.20146805200002));
#284918=CARTESIAN_POINT('Ctrl Pts',(-6.67195235200006,15.2,-8.20325583300002));
#284919=CARTESIAN_POINT('Ctrl Pts',(-6.67195235200006,11.6,-8.20325583300002));
#284920=CARTESIAN_POINT('Ctrl Pts',(-6.67286430200006,15.2,-8.20505070200002));
#284921=CARTESIAN_POINT('Ctrl Pts',(-6.67286430200006,11.6,-8.20505070200002));
#284922=CARTESIAN_POINT('Ctrl Pts',(-6.67377780700006,15.2,-8.20685265200002));
#284923=CARTESIAN_POINT('Ctrl Pts',(-6.67377780700006,11.6,-8.20685265200002));
#284924=CARTESIAN_POINT('Ctrl Pts',(-6.67469285000006,15.2,-8.20866167300002));
#284925=CARTESIAN_POINT('Ctrl Pts',(-6.67469285000006,11.6,-8.20866167300002));
#284926=CARTESIAN_POINT('Ctrl Pts',(-6.67560941300006,15.2,-8.21047775800002));
#284927=CARTESIAN_POINT('Ctrl Pts',(-6.67560941300006,11.6,-8.21047775800002));
#284928=CARTESIAN_POINT('Ctrl Pts',(-6.67652747900005,15.2,-8.21230089900002));
#284929=CARTESIAN_POINT('Ctrl Pts',(-6.67652747900005,11.6,-8.21230089900002));
#284930=CARTESIAN_POINT('Ctrl Pts',(-6.67744703200006,15.2,-8.21413108800002));
#284931=CARTESIAN_POINT('Ctrl Pts',(-6.67744703200006,11.6,-8.21413108800002));
#284932=CARTESIAN_POINT('Ctrl Pts',(-6.67836805600006,15.2,-8.21596831500001));
#284933=CARTESIAN_POINT('Ctrl Pts',(-6.67836805600006,11.6,-8.21596831500001));
#284934=CARTESIAN_POINT('Ctrl Pts',(-6.67929053300006,15.2,-8.21781257300002));
#284935=CARTESIAN_POINT('Ctrl Pts',(-6.67929053300006,11.6,-8.21781257300002));
#284936=CARTESIAN_POINT('Ctrl Pts',(-6.68021444700006,15.2,-8.21966385300002));
#284937=CARTESIAN_POINT('Ctrl Pts',(-6.68021444700006,11.6,-8.21966385300002));
#284938=CARTESIAN_POINT('Ctrl Pts',(-6.68113978100005,15.2,-8.22152214800001));
#284939=CARTESIAN_POINT('Ctrl Pts',(-6.68113978100005,11.6,-8.22152214800001));
#284940=CARTESIAN_POINT('Ctrl Pts',(-6.68206651900006,15.2,-8.22338745000001));
#284941=CARTESIAN_POINT('Ctrl Pts',(-6.68206651900006,11.6,-8.22338745000001));
#284942=CARTESIAN_POINT('Ctrl Pts',(-6.68299464500006,15.2,-8.22525974700002));
#284943=CARTESIAN_POINT('Ctrl Pts',(-6.68299464500006,11.6,-8.22525974700002));
#284944=CARTESIAN_POINT('Ctrl Pts',(-6.68392414200006,15.2,-8.22713903600001));
#284945=CARTESIAN_POINT('Ctrl Pts',(-6.68392414200006,11.6,-8.22713903600001));
#284946=CARTESIAN_POINT('Ctrl Pts',(-6.68485499200006,15.2,-8.22902530700001));
#284947=CARTESIAN_POINT('Ctrl Pts',(-6.68485499200006,11.6,-8.22902530700001));
#284948=CARTESIAN_POINT('Ctrl Pts',(-6.68578718200005,15.2,-8.23091855000002));
#284949=CARTESIAN_POINT('Ctrl Pts',(-6.68578718200005,11.6,-8.23091855000002));
#284950=CARTESIAN_POINT('Ctrl Pts',(-6.68672069300006,15.2,-8.23281875900001));
#284951=CARTESIAN_POINT('Ctrl Pts',(-6.68672069300006,11.6,-8.23281875900001));
#284952=CARTESIAN_POINT('Ctrl Pts',(-6.68765551100006,15.2,-8.23472592600002));
#284953=CARTESIAN_POINT('Ctrl Pts',(-6.68765551100006,11.6,-8.23472592600002));
#284954=CARTESIAN_POINT('Ctrl Pts',(-6.68859161800006,15.2,-8.23664004100002));
#284955=CARTESIAN_POINT('Ctrl Pts',(-6.68859161800006,11.6,-8.23664004100002));
#284956=CARTESIAN_POINT('Ctrl Pts',(-6.68952899900006,15.2,-8.23856109700002));
#284957=CARTESIAN_POINT('Ctrl Pts',(-6.68952899900006,11.6,-8.23856109700002));
#284958=CARTESIAN_POINT('Ctrl Pts',(-6.69046763700006,15.2,-8.24048908700002));
#284959=CARTESIAN_POINT('Ctrl Pts',(-6.69046763700006,11.6,-8.24048908700002));
#284960=CARTESIAN_POINT('Ctrl Pts',(-6.69140751900006,15.2,-8.24242400100001));
#284961=CARTESIAN_POINT('Ctrl Pts',(-6.69140751900006,11.6,-8.24242400100001));
#284962=CARTESIAN_POINT('Ctrl Pts',(-6.69234862600006,15.2,-8.24436583300002));
#284963=CARTESIAN_POINT('Ctrl Pts',(-6.69234862600006,11.6,-8.24436583300002));
#284964=CARTESIAN_POINT('Ctrl Pts',(-6.69329094300006,15.2,-8.24631457300002));
#284965=CARTESIAN_POINT('Ctrl Pts',(-6.69329094300006,11.6,-8.24631457300002));
#284966=CARTESIAN_POINT('Ctrl Pts',(-6.69423445500006,15.2,-8.24827021500001));
#284967=CARTESIAN_POINT('Ctrl Pts',(-6.69423445500006,11.6,-8.24827021500001));
#284968=CARTESIAN_POINT('Ctrl Pts',(-6.69517914500006,15.2,-8.25023274900002));
#284969=CARTESIAN_POINT('Ctrl Pts',(-6.69517914500006,11.6,-8.25023274900002));
#284970=CARTESIAN_POINT('Ctrl Pts',(-6.69612499800006,15.2,-8.25220216900002));
#284971=CARTESIAN_POINT('Ctrl Pts',(-6.69612499800006,11.6,-8.25220216900002));
#284972=CARTESIAN_POINT('Ctrl Pts',(-6.69707199900006,15.2,-8.25417846500001));
#284973=CARTESIAN_POINT('Ctrl Pts',(-6.69707199900006,11.6,-8.25417846500001));
#284974=CARTESIAN_POINT('Ctrl Pts',(-6.69802013200006,15.2,-8.25616163100002));
#284975=CARTESIAN_POINT('Ctrl Pts',(-6.69802013200006,11.6,-8.25616163100002));
#284976=CARTESIAN_POINT('Ctrl Pts',(-6.69896938100006,15.2,-8.25815165900002));
#284977=CARTESIAN_POINT('Ctrl Pts',(-6.69896938100006,11.6,-8.25815165900002));
#284978=CARTESIAN_POINT('Ctrl Pts',(-6.69991973100006,15.2,-8.26014853800002));
#284979=CARTESIAN_POINT('Ctrl Pts',(-6.69991973100006,11.6,-8.26014853800002));
#284980=CARTESIAN_POINT('Ctrl Pts',(-6.70087116700006,15.2,-8.26215226500001));
#284981=CARTESIAN_POINT('Ctrl Pts',(-6.70087116700006,11.6,-8.26215226500001));
#284982=CARTESIAN_POINT('Ctrl Pts',(-6.70182367300006,15.2,-8.26416282800002));
#284983=CARTESIAN_POINT('Ctrl Pts',(-6.70182367300006,11.6,-8.26416282800002));
#284984=CARTESIAN_POINT('Ctrl Pts',(-6.70277723400006,15.2,-8.26618022100002));
#284985=CARTESIAN_POINT('Ctrl Pts',(-6.70277723400006,11.6,-8.26618022100002));
#284986=CARTESIAN_POINT('Ctrl Pts',(-6.70373183500006,15.2,-8.26820443600001));
#284987=CARTESIAN_POINT('Ctrl Pts',(-6.70373183500006,11.6,-8.26820443600001));
#284988=CARTESIAN_POINT('Ctrl Pts',(-6.70468746000005,15.2,-8.27023546500002));
#284989=CARTESIAN_POINT('Ctrl Pts',(-6.70468746000005,11.6,-8.27023546500002));
#284990=CARTESIAN_POINT('Ctrl Pts',(-6.70564409500006,15.2,-8.27227330000002));
#284991=CARTESIAN_POINT('Ctrl Pts',(-6.70564409500006,11.6,-8.27227330000002));
#284992=CARTESIAN_POINT('Ctrl Pts',(-6.70660172400006,15.2,-8.27431793400002));
#284993=CARTESIAN_POINT('Ctrl Pts',(-6.70660172400006,11.6,-8.27431793400002));
#284994=CARTESIAN_POINT('Ctrl Pts',(-6.70756033200006,15.2,-8.27636935700001));
#284995=CARTESIAN_POINT('Ctrl Pts',(-6.70756033200006,11.6,-8.27636935700001));
#284996=CARTESIAN_POINT('Ctrl Pts',(-6.70851990500006,15.2,-8.27842756400001));
#284997=CARTESIAN_POINT('Ctrl Pts',(-6.70851990500006,11.6,-8.27842756400001));
#284998=CARTESIAN_POINT('Ctrl Pts',(-6.70948042600005,15.2,-8.28049254600002));
#284999=CARTESIAN_POINT('Ctrl Pts',(-6.70948042600005,11.6,-8.28049254600002));
#285000=CARTESIAN_POINT('Ctrl Pts',(-6.71044188300006,15.2,-8.28256429500002));
#285001=CARTESIAN_POINT('Ctrl Pts',(-6.71044188300006,11.6,-8.28256429500002));
#285002=CARTESIAN_POINT('Ctrl Pts',(-6.71140426000005,15.2,-8.28464280400001));
#285003=CARTESIAN_POINT('Ctrl Pts',(-6.71140426000005,11.6,-8.28464280400001));
#285004=CARTESIAN_POINT('Ctrl Pts',(-6.71236754100006,15.2,-8.28672806400002));
#285005=CARTESIAN_POINT('Ctrl Pts',(-6.71236754100006,11.6,-8.28672806400002));
#285006=CARTESIAN_POINT('Ctrl Pts',(-6.71333171300006,15.2,-8.28882006800002));
#285007=CARTESIAN_POINT('Ctrl Pts',(-6.71333171300006,11.6,-8.28882006800002));
#285008=CARTESIAN_POINT('Ctrl Pts',(-6.71429675900006,15.2,-8.29091880900001));
#285009=CARTESIAN_POINT('Ctrl Pts',(-6.71429675900006,11.6,-8.29091880900001));
#285010=CARTESIAN_POINT('Ctrl Pts',(-6.71526266700006,15.2,-8.29302427800001));
#285011=CARTESIAN_POINT('Ctrl Pts',(-6.71526266700006,11.6,-8.29302427800001));
#285012=CARTESIAN_POINT('Ctrl Pts',(-6.71622942200006,15.2,-8.29513646900002));
#285013=CARTESIAN_POINT('Ctrl Pts',(-6.71622942200006,11.6,-8.29513646900002));
#285014=CARTESIAN_POINT('Ctrl Pts',(-6.71719700800006,15.2,-8.29725537200002));
#285015=CARTESIAN_POINT('Ctrl Pts',(-6.71719700800006,11.6,-8.29725537200002));
#285016=CARTESIAN_POINT('Ctrl Pts',(-6.71816541100006,15.2,-8.29938098200002));
#285017=CARTESIAN_POINT('Ctrl Pts',(-6.71816541100006,11.6,-8.29938098200002));
#285018=CARTESIAN_POINT('Ctrl Pts',(-6.71913461600006,15.2,-8.30151328900002));
#285019=CARTESIAN_POINT('Ctrl Pts',(-6.71913461600006,11.6,-8.30151328900002));
#285020=CARTESIAN_POINT('Ctrl Pts',(-6.72010461200006,15.2,-8.30365228700002));
#285021=CARTESIAN_POINT('Ctrl Pts',(-6.72010461200006,11.6,-8.30365228700002));
#285022=CARTESIAN_POINT('Ctrl Pts',(-6.72107538000006,15.2,-8.30579796800002));
#285023=CARTESIAN_POINT('Ctrl Pts',(-6.72107538000006,11.6,-8.30579796800002));
#285024=CARTESIAN_POINT('Ctrl Pts',(-6.72204690900006,15.2,-8.30795032300001));
#285025=CARTESIAN_POINT('Ctrl Pts',(-6.72204690900006,11.6,-8.30795032300001));
#285026=CARTESIAN_POINT('Ctrl Pts',(-6.72301918300006,15.2,-8.31010934800002));
#285027=CARTESIAN_POINT('Ctrl Pts',(-6.72301918300006,11.6,-8.31010934800002));
#285028=CARTESIAN_POINT('Ctrl Pts',(-6.72399218800006,15.2,-8.31227503100001));
#285029=CARTESIAN_POINT('Ctrl Pts',(-6.72399218800006,11.6,-8.31227503100001));
#285030=CARTESIAN_POINT('Ctrl Pts',(-6.72496591100006,15.2,-8.31444736700002));
#285031=CARTESIAN_POINT('Ctrl Pts',(-6.72496591100006,11.6,-8.31444736700002));
#285032=CARTESIAN_POINT('Ctrl Pts',(-6.72594033700006,15.2,-8.31662634800002));
#285033=CARTESIAN_POINT('Ctrl Pts',(-6.72594033700006,11.6,-8.31662634800002));
#285034=CARTESIAN_POINT('Ctrl Pts',(-6.72691545200006,15.2,-8.31881196600002));
#285035=CARTESIAN_POINT('Ctrl Pts',(-6.72691545200006,11.6,-8.31881196600002));
#285036=CARTESIAN_POINT('Ctrl Pts',(-6.72789124200006,15.2,-8.32100421400002));
#285037=CARTESIAN_POINT('Ctrl Pts',(-6.72789124200006,11.6,-8.32100421400002));
#285038=CARTESIAN_POINT('Ctrl Pts',(-6.72886769300006,15.2,-8.32320308500002));
#285039=CARTESIAN_POINT('Ctrl Pts',(-6.72886769300006,11.6,-8.32320308500002));
#285040=CARTESIAN_POINT('Ctrl Pts',(-6.72984479100006,15.2,-8.32540857000001));
#285041=CARTESIAN_POINT('Ctrl Pts',(-6.72984479100006,11.6,-8.32540857000001));
#285042=CARTESIAN_POINT('Ctrl Pts',(-6.73082252300006,15.2,-8.32762066300001));
#285043=CARTESIAN_POINT('Ctrl Pts',(-6.73082252300006,11.6,-8.32762066300001));
#285044=CARTESIAN_POINT('Ctrl Pts',(-6.73180087300006,15.2,-8.32983935500001));
#285045=CARTESIAN_POINT('Ctrl Pts',(-6.73180087300006,11.6,-8.32983935500001));
#285046=CARTESIAN_POINT('Ctrl Pts',(-6.73277982900006,15.2,-8.33206464000002));
#285047=CARTESIAN_POINT('Ctrl Pts',(-6.73277982900006,11.6,-8.33206464000002));
#285048=CARTESIAN_POINT('Ctrl Pts',(-6.73375937800006,15.2,-8.33429650900002));
#285049=CARTESIAN_POINT('Ctrl Pts',(-6.73375937800006,11.6,-8.33429650900002));
#285050=CARTESIAN_POINT('Ctrl Pts',(-6.73473950400005,15.2,-8.33653495700002));
#285051=CARTESIAN_POINT('Ctrl Pts',(-6.73473950400005,11.6,-8.33653495700002));
#285052=CARTESIAN_POINT('Ctrl Pts',(-6.73572019500006,15.2,-8.33877997400002));
#285053=CARTESIAN_POINT('Ctrl Pts',(-6.73572019500006,11.6,-8.33877997400002));
#285054=CARTESIAN_POINT('Ctrl Pts',(-6.73670143700006,15.2,-8.34103155300001));
#285055=CARTESIAN_POINT('Ctrl Pts',(-6.73670143700006,11.6,-8.34103155300001));
#285056=CARTESIAN_POINT('Ctrl Pts',(-6.73768321600006,15.2,-8.34328968900002));
#285057=CARTESIAN_POINT('Ctrl Pts',(-6.73768321600006,11.6,-8.34328968900002));
#285058=CARTESIAN_POINT('Ctrl Pts',(-6.73866551900006,15.2,-8.34555437100001));
#285059=CARTESIAN_POINT('Ctrl Pts',(-6.73866551900006,11.6,-8.34555437100001));
#285060=CARTESIAN_POINT('Ctrl Pts',(-6.73964833200006,15.2,-8.34782559500002));
#285061=CARTESIAN_POINT('Ctrl Pts',(-6.73964833200006,11.6,-8.34782559500002));
#285062=CARTESIAN_POINT('Ctrl Pts',(-6.74063164200006,15.2,-8.35010335100002));
#285063=CARTESIAN_POINT('Ctrl Pts',(-6.74063164200006,11.6,-8.35010335100002));
#285064=CARTESIAN_POINT('Ctrl Pts',(-6.74161543500006,15.2,-8.35238763300002));
#285065=CARTESIAN_POINT('Ctrl Pts',(-6.74161543500006,11.6,-8.35238763300002));
#285066=CARTESIAN_POINT('Ctrl Pts',(-6.74259969900006,15.2,-8.35467843300002));
#285067=CARTESIAN_POINT('Ctrl Pts',(-6.74259969900006,11.6,-8.35467843300002));
#285068=CARTESIAN_POINT('Ctrl Pts',(-6.74358442000006,15.2,-8.35697574500001));
#285069=CARTESIAN_POINT('Ctrl Pts',(-6.74358442000006,11.6,-8.35697574500001));
#285070=CARTESIAN_POINT('Ctrl Pts',(-6.74456958400006,15.2,-8.35927956000001));
#285071=CARTESIAN_POINT('Ctrl Pts',(-6.74456958400006,11.6,-8.35927956000001));
#285072=CARTESIAN_POINT('Ctrl Pts',(-6.74555517700006,15.2,-8.36158987000001));
#285073=CARTESIAN_POINT('Ctrl Pts',(-6.74555517700006,11.6,-8.36158987000001));
#285074=CARTESIAN_POINT('Ctrl Pts',(-6.74654118900006,15.2,-8.36390667000002));
#285075=CARTESIAN_POINT('Ctrl Pts',(-6.74654118900006,11.6,-8.36390667000002));
#285076=CARTESIAN_POINT('Ctrl Pts',(-6.74752760400006,15.2,-8.36622995200001));
#285077=CARTESIAN_POINT('Ctrl Pts',(-6.74752760400006,11.6,-8.36622995200001));
#285078=CARTESIAN_POINT('Ctrl Pts',(-6.74851441000006,15.2,-8.36855970800002));
#285079=CARTESIAN_POINT('Ctrl Pts',(-6.74851441000006,11.6,-8.36855970800002));
#285080=CARTESIAN_POINT('Ctrl Pts',(-6.74950159300006,15.2,-8.37089593100002));
#285081=CARTESIAN_POINT('Ctrl Pts',(-6.74950159300006,11.6,-8.37089593100002));
#285082=CARTESIAN_POINT('Ctrl Pts',(-6.75048914200006,15.2,-8.37323861500002));
#285083=CARTESIAN_POINT('Ctrl Pts',(-6.75048914200006,11.6,-8.37323861500002));
#285084=CARTESIAN_POINT('Ctrl Pts',(-6.75147704200006,15.2,-8.37558775000002));
#285085=CARTESIAN_POINT('Ctrl Pts',(-6.75147704200006,11.6,-8.37558775000002));
#285086=CARTESIAN_POINT('Ctrl Pts',(-6.75246528000006,15.2,-8.37794333100002));
#285087=CARTESIAN_POINT('Ctrl Pts',(-6.75246528000006,11.6,-8.37794333100002));
#285088=CARTESIAN_POINT('Ctrl Pts',(-6.75345384400006,15.2,-8.38030535000001));
#285089=CARTESIAN_POINT('Ctrl Pts',(-6.75345384400006,11.6,-8.38030535000001));
#285090=CARTESIAN_POINT('Ctrl Pts',(-6.75444272200005,15.2,-8.38267380000002));
#285091=CARTESIAN_POINT('Ctrl Pts',(-6.75444272200005,11.6,-8.38267380000002));
#285092=CARTESIAN_POINT('Ctrl Pts',(-6.75543189900006,15.2,-8.38504867300001));
#285093=CARTESIAN_POINT('Ctrl Pts',(-6.75543189900006,11.6,-8.38504867300001));
#285094=CARTESIAN_POINT('Ctrl Pts',(-6.75642136400006,15.2,-8.38742996300001));
#285095=CARTESIAN_POINT('Ctrl Pts',(-6.75642136400006,11.6,-8.38742996300001));
#285096=CARTESIAN_POINT('Ctrl Pts',(-6.75741110400006,15.2,-8.38981766200002));
#285097=CARTESIAN_POINT('Ctrl Pts',(-6.75741110400006,11.6,-8.38981766200002));
#285098=CARTESIAN_POINT('Ctrl Pts',(-6.75840110500006,15.2,-8.39221176300001));
#285099=CARTESIAN_POINT('Ctrl Pts',(-6.75840110500006,11.6,-8.39221176300001));
#285100=CARTESIAN_POINT('Ctrl Pts',(-6.75939135700006,15.2,-8.39461225900001));
#285101=CARTESIAN_POINT('Ctrl Pts',(-6.75939135700006,11.6,-8.39461225900001));
#285102=CARTESIAN_POINT('Ctrl Pts',(-6.76038184400006,15.2,-8.39701914200001));
#285103=CARTESIAN_POINT('Ctrl Pts',(-6.76038184400006,11.6,-8.39701914200001));
#285104=CARTESIAN_POINT('Ctrl Pts',(-6.76137255500006,15.2,-8.39943240700002));
#285105=CARTESIAN_POINT('Ctrl Pts',(-6.76137255500006,11.6,-8.39943240700002));
#285106=CARTESIAN_POINT('Ctrl Pts',(-6.76236347800006,15.2,-8.40185204500001));
#285107=CARTESIAN_POINT('Ctrl Pts',(-6.76236347800006,11.6,-8.40185204500001));
#285108=CARTESIAN_POINT('Ctrl Pts',(-6.76335460000006,15.2,-8.40427804800001));
#285109=CARTESIAN_POINT('Ctrl Pts',(-6.76335460000006,11.6,-8.40427804800001));
#285110=CARTESIAN_POINT('Ctrl Pts',(-6.76434590800006,15.2,-8.40671041100002));
#285111=CARTESIAN_POINT('Ctrl Pts',(-6.76434590800006,11.6,-8.40671041100002));
#285112=CARTESIAN_POINT('Ctrl Pts',(-6.76533739000006,15.2,-8.40914912700002));
#285113=CARTESIAN_POINT('Ctrl Pts',(-6.76533739000006,11.6,-8.40914912700002));
#285114=CARTESIAN_POINT('Ctrl Pts',(-6.76632903400006,15.2,-8.41159418600002));
#285115=CARTESIAN_POINT('Ctrl Pts',(-6.76632903400006,11.6,-8.41159418600002));
#285116=CARTESIAN_POINT('Ctrl Pts',(-6.76732082700005,15.2,-8.41404558300002));
#285117=CARTESIAN_POINT('Ctrl Pts',(-6.76732082700005,11.6,-8.41404558300002));
#285118=CARTESIAN_POINT('Ctrl Pts',(-6.76831275600006,15.2,-8.41650331100002));
#285119=CARTESIAN_POINT('Ctrl Pts',(-6.76831275600006,11.6,-8.41650331100002));
#285120=CARTESIAN_POINT('Ctrl Pts',(-6.76930481100006,15.2,-8.41896736400002));
#285121=CARTESIAN_POINT('Ctrl Pts',(-6.76930481100006,11.6,-8.41896736400002));
#285122=CARTESIAN_POINT('Ctrl Pts',(-6.77029697800006,15.2,-8.42143773200002));
#285123=CARTESIAN_POINT('Ctrl Pts',(-6.77029697800006,11.6,-8.42143773200002));
#285124=CARTESIAN_POINT('Ctrl Pts',(-6.77128924400006,15.2,-8.42391441000002));
#285125=CARTESIAN_POINT('Ctrl Pts',(-6.77128924400006,11.6,-8.42391441000002));
#285126=CARTESIAN_POINT('Ctrl Pts',(-6.77228160000006,15.2,-8.42639739000001));
#285127=CARTESIAN_POINT('Ctrl Pts',(-6.77228160000006,11.6,-8.42639739000001));
#285128=CARTESIAN_POINT('Ctrl Pts',(-6.77327403000006,15.2,-8.42888666600001));
#285129=CARTESIAN_POINT('Ctrl Pts',(-6.77327403000006,11.6,-8.42888666600001));
#285130=CARTESIAN_POINT('Ctrl Pts',(-6.77426652500006,15.2,-8.43138223000001));
#285131=CARTESIAN_POINT('Ctrl Pts',(-6.77426652500006,11.6,-8.43138223000001));
#285132=CARTESIAN_POINT('Ctrl Pts',(-6.77525907000006,15.2,-8.43388407500001));
#285133=CARTESIAN_POINT('Ctrl Pts',(-6.77525907000006,11.6,-8.43388407500001));
#285134=CARTESIAN_POINT('Ctrl Pts',(-6.77625165600006,15.2,-8.43639219400002));
#285135=CARTESIAN_POINT('Ctrl Pts',(-6.77625165600006,11.6,-8.43639219400002));
#285136=CARTESIAN_POINT('Ctrl Pts',(-6.77724426900006,15.2,-8.43890658100002));
#285137=CARTESIAN_POINT('Ctrl Pts',(-6.77724426900006,11.6,-8.43890658100002));
#285138=CARTESIAN_POINT('Ctrl Pts',(-6.77823689800006,15.2,-8.44142722800001));
#285139=CARTESIAN_POINT('Ctrl Pts',(-6.77823689800006,11.6,-8.44142722800001));
#285140=CARTESIAN_POINT('Ctrl Pts',(-6.77922953100006,15.2,-8.44395412900001));
#285141=CARTESIAN_POINT('Ctrl Pts',(-6.77922953100006,11.6,-8.44395412900001));
#285142=CARTESIAN_POINT('Ctrl Pts',(-6.78022215500006,15.2,-8.44648727600001));
#285143=CARTESIAN_POINT('Ctrl Pts',(-6.78022215500006,11.6,-8.44648727600001));
#285144=CARTESIAN_POINT('Ctrl Pts',(-6.78121475800006,15.2,-8.44902666100002));
#285145=CARTESIAN_POINT('Ctrl Pts',(-6.78121475800006,11.6,-8.44902666100002));
#285146=CARTESIAN_POINT('Ctrl Pts',(-6.78220733100006,15.2,-8.45157227900001));
#285147=CARTESIAN_POINT('Ctrl Pts',(-6.78220733100006,11.6,-8.45157227900001));
#285148=CARTESIAN_POINT('Ctrl Pts',(-6.78319986000006,15.2,-8.45412412300002));
#285149=CARTESIAN_POINT('Ctrl Pts',(-6.78319986000006,11.6,-8.45412412300002));
#285150=CARTESIAN_POINT('Ctrl Pts',(-6.78419233200006,15.2,-8.45668218600002));
#285151=CARTESIAN_POINT('Ctrl Pts',(-6.78419233200006,11.6,-8.45668218600002));
#285152=CARTESIAN_POINT('Ctrl Pts',(-6.78518473900006,15.2,-8.45924645900002));
#285153=CARTESIAN_POINT('Ctrl Pts',(-6.78518473900006,11.6,-8.45924645900002));
#285154=CARTESIAN_POINT('Ctrl Pts',(-6.78617706600006,15.2,-8.46181693800002));
#285155=CARTESIAN_POINT('Ctrl Pts',(-6.78617706600006,11.6,-8.46181693800002));
#285156=CARTESIAN_POINT('Ctrl Pts',(-6.78716930300006,15.2,-8.46439361500002));
#285157=CARTESIAN_POINT('Ctrl Pts',(-6.78716930300006,11.6,-8.46439361500002));
#285158=CARTESIAN_POINT('Ctrl Pts',(-6.78816143700006,15.2,-8.46697648200001));
#285159=CARTESIAN_POINT('Ctrl Pts',(-6.78816143700006,11.6,-8.46697648200001));
#285160=CARTESIAN_POINT('Ctrl Pts',(-6.78915345800006,15.2,-8.46956553300002));
#285161=CARTESIAN_POINT('Ctrl Pts',(-6.78915345800006,11.6,-8.46956553300002));
#285162=CARTESIAN_POINT('Ctrl Pts',(-6.79014535300006,15.2,-8.47216076000001));
#285163=CARTESIAN_POINT('Ctrl Pts',(-6.79014535300006,11.6,-8.47216076000001));
#285164=CARTESIAN_POINT('Ctrl Pts',(-6.79113711200006,15.2,-8.47476215800001));
#285165=CARTESIAN_POINT('Ctrl Pts',(-6.79113711200006,11.6,-8.47476215800001));
#285166=CARTESIAN_POINT('Ctrl Pts',(-6.79212872200006,15.2,-8.47736971900002));
#285167=CARTESIAN_POINT('Ctrl Pts',(-6.79212872200006,11.6,-8.47736971900002));
#285168=CARTESIAN_POINT('Ctrl Pts',(-6.79312017300005,15.2,-8.47998343700001));
#285169=CARTESIAN_POINT('Ctrl Pts',(-6.79312017300005,11.6,-8.47998343700001));
#285170=CARTESIAN_POINT('Ctrl Pts',(-6.79411145300006,15.2,-8.48260330400001));
#285171=CARTESIAN_POINT('Ctrl Pts',(-6.79411145300006,11.6,-8.48260330400001));
#285172=CARTESIAN_POINT('Ctrl Pts',(-6.79510255000006,15.2,-8.48522931400002));
#285173=CARTESIAN_POINT('Ctrl Pts',(-6.79510255000006,11.6,-8.48522931400002));
#285174=CARTESIAN_POINT('Ctrl Pts',(-6.79609345300006,15.2,-8.48786145900002));
#285175=CARTESIAN_POINT('Ctrl Pts',(-6.79609345300006,11.6,-8.48786145900002));
#285176=CARTESIAN_POINT('Ctrl Pts',(-6.79708415200006,15.2,-8.49049973300002));
#285177=CARTESIAN_POINT('Ctrl Pts',(-6.79708415200006,11.6,-8.49049973300002));
#285178=CARTESIAN_POINT('Ctrl Pts',(-6.79807463300006,15.2,-8.49314413000002));
#285179=CARTESIAN_POINT('Ctrl Pts',(-6.79807463300006,11.6,-8.49314413000002));
#285180=CARTESIAN_POINT('Ctrl Pts',(-6.79906488700006,15.2,-8.49579464200002));
#285181=CARTESIAN_POINT('Ctrl Pts',(-6.79906488700006,11.6,-8.49579464200002));
#285182=CARTESIAN_POINT('Ctrl Pts',(-6.80005490300006,15.2,-8.49845126300002));
#285183=CARTESIAN_POINT('Ctrl Pts',(-6.80005490300006,11.6,-8.49845126300002));
#285184=CARTESIAN_POINT('Ctrl Pts',(-6.80104466800006,15.2,-8.50111398400001));
#285185=CARTESIAN_POINT('Ctrl Pts',(-6.80104466800006,11.6,-8.50111398400001));
#285186=CARTESIAN_POINT('Ctrl Pts',(-6.80203417100006,15.2,-8.50378280200001));
#285187=CARTESIAN_POINT('Ctrl Pts',(-6.80203417100006,11.6,-8.50378280200001));
#285188=CARTESIAN_POINT('Ctrl Pts',(-6.80302340200006,15.2,-8.50645770700002));
#285189=CARTESIAN_POINT('Ctrl Pts',(-6.80302340200006,11.6,-8.50645770700002));
#285190=CARTESIAN_POINT('Ctrl Pts',(-6.80401234900006,15.2,-8.50913869300001));
#285191=CARTESIAN_POINT('Ctrl Pts',(-6.80401234900006,11.6,-8.50913869300001));
#285192=CARTESIAN_POINT('Ctrl Pts',(-6.80500100400006,15.2,-8.51182575500001));
#285193=CARTESIAN_POINT('Ctrl Pts',(-6.80500100400006,11.6,-8.51182575500001));
#285194=CARTESIAN_POINT('Ctrl Pts',(-6.80598935100006,15.2,-8.51451888400002));
#285195=CARTESIAN_POINT('Ctrl Pts',(-6.80598935100006,11.6,-8.51451888400002));
#285196=CARTESIAN_POINT('Ctrl Pts',(-6.80697738200006,15.2,-8.51721807500001));
#285197=CARTESIAN_POINT('Ctrl Pts',(-6.80697738200006,11.6,-8.51721807500001));
#285198=CARTESIAN_POINT('Ctrl Pts',(-6.80796508500006,15.2,-8.51992331800002));
#285199=CARTESIAN_POINT('Ctrl Pts',(-6.80796508500006,11.6,-8.51992331800002));
#285200=CARTESIAN_POINT('Ctrl Pts',(-6.80895244900006,15.2,-8.52263461100002));
#285201=CARTESIAN_POINT('Ctrl Pts',(-6.80895244900006,11.6,-8.52263461100002));
#285202=CARTESIAN_POINT('Ctrl Pts',(-6.80993946500006,15.2,-8.52535194300001));
#285203=CARTESIAN_POINT('Ctrl Pts',(-6.80993946500006,11.6,-8.52535194300001));
#285204=CARTESIAN_POINT('Ctrl Pts',(-6.81092612100006,15.2,-8.52807531000002));
#285205=CARTESIAN_POINT('Ctrl Pts',(-6.81092612100006,11.6,-8.52807531000002));
#285206=CARTESIAN_POINT('Ctrl Pts',(-6.81191240500006,15.2,-8.53080470500002));
#285207=CARTESIAN_POINT('Ctrl Pts',(-6.81191240500006,11.6,-8.53080470500002));
#285208=CARTESIAN_POINT('Ctrl Pts',(-6.81289830700006,15.2,-8.53354012000001));
#285209=CARTESIAN_POINT('Ctrl Pts',(-6.81289830700006,11.6,-8.53354012000001));
#285210=CARTESIAN_POINT('Ctrl Pts',(-6.81388381700006,15.2,-8.53628154900001));
#285211=CARTESIAN_POINT('Ctrl Pts',(-6.81388381700006,11.6,-8.53628154900001));
#285212=CARTESIAN_POINT('Ctrl Pts',(-6.81486892200006,15.2,-8.53902898500002));
#285213=CARTESIAN_POINT('Ctrl Pts',(-6.81486892200006,11.6,-8.53902898500002));
#285214=CARTESIAN_POINT('Ctrl Pts',(-6.81585361400006,15.2,-8.54178242200001));
#285215=CARTESIAN_POINT('Ctrl Pts',(-6.81585361400006,11.6,-8.54178242200001));
#285216=CARTESIAN_POINT('Ctrl Pts',(-6.81683788100006,15.2,-8.54454185300002));
#285217=CARTESIAN_POINT('Ctrl Pts',(-6.81683788100006,11.6,-8.54454185300002));
#285218=CARTESIAN_POINT('Ctrl Pts',(-6.81782171200005,15.2,-8.54730727200002));
#285219=CARTESIAN_POINT('Ctrl Pts',(-6.81782171200005,11.6,-8.54730727200002));
#285220=CARTESIAN_POINT('Ctrl Pts',(-6.81880509800005,15.2,-8.55007867000002));
#285221=CARTESIAN_POINT('Ctrl Pts',(-6.81880509800005,11.6,-8.55007867000002));
#285222=CARTESIAN_POINT('Ctrl Pts',(-6.81978802600006,15.2,-8.55285604300001));
#285223=CARTESIAN_POINT('Ctrl Pts',(-6.81978802600006,11.6,-8.55285604300001));
#285224=CARTESIAN_POINT('Ctrl Pts',(-6.82077048700005,15.2,-8.55563938300002));
#285225=CARTESIAN_POINT('Ctrl Pts',(-6.82077048700005,11.6,-8.55563938300002));
#285226=CARTESIAN_POINT('Ctrl Pts',(-6.82175247000006,15.2,-8.55842868400002));
#285227=CARTESIAN_POINT('Ctrl Pts',(-6.82175247000006,11.6,-8.55842868400002));
#285228=CARTESIAN_POINT('Ctrl Pts',(-6.82273396500006,15.2,-8.56122393900002));
#285229=CARTESIAN_POINT('Ctrl Pts',(-6.82273396500006,11.6,-8.56122393900002));
#285230=CARTESIAN_POINT('Ctrl Pts',(-6.82371496100005,15.2,-8.56402514100001));
#285231=CARTESIAN_POINT('Ctrl Pts',(-6.82371496100005,11.6,-8.56402514100001));
#285232=CARTESIAN_POINT('Ctrl Pts',(-6.82469544700006,15.2,-8.56683228400002));
#285233=CARTESIAN_POINT('Ctrl Pts',(-6.82469544700006,11.6,-8.56683228400002));
#285234=CARTESIAN_POINT('Ctrl Pts',(-6.82567541400006,15.2,-8.56964536100002));
#285235=CARTESIAN_POINT('Ctrl Pts',(-6.82567541400006,11.6,-8.56964536100002));
#285236=CARTESIAN_POINT('Ctrl Pts',(-6.82665485100006,15.2,-8.57246436600001));
#285237=CARTESIAN_POINT('Ctrl Pts',(-6.82665485100006,11.6,-8.57246436600001));
#285238=CARTESIAN_POINT('Ctrl Pts',(-6.82763374600006,15.2,-8.57528929200001));
#285239=CARTESIAN_POINT('Ctrl Pts',(-6.82763374600006,11.6,-8.57528929200001));
#285240=CARTESIAN_POINT('Ctrl Pts',(-6.82861209100006,15.2,-8.57812013100002));
#285241=CARTESIAN_POINT('Ctrl Pts',(-6.82861209100006,11.6,-8.57812013100002));
#285242=CARTESIAN_POINT('Ctrl Pts',(-6.82958987600006,15.2,-8.58095688000001));
#285243=CARTESIAN_POINT('Ctrl Pts',(-6.82958987600006,11.6,-8.58095688000001));
#285244=CARTESIAN_POINT('Ctrl Pts',(-6.83056708700006,15.2,-8.58379952900002));
#285245=CARTESIAN_POINT('Ctrl Pts',(-6.83056708700006,11.6,-8.58379952900002));
#285246=CARTESIAN_POINT('Ctrl Pts',(-6.83154371800006,15.2,-8.58664807300002));
#285247=CARTESIAN_POINT('Ctrl Pts',(-6.83154371800006,11.6,-8.58664807300002));
#285248=CARTESIAN_POINT('Ctrl Pts',(-6.83251975600006,15.2,-8.58950250500002));
#285249=CARTESIAN_POINT('Ctrl Pts',(-6.83251975600006,11.6,-8.58950250500002));
#285250=CARTESIAN_POINT('Ctrl Pts',(-6.83349519400006,15.2,-8.59236281800002));
#285251=CARTESIAN_POINT('Ctrl Pts',(-6.83349519400006,11.6,-8.59236281800002));
#285252=CARTESIAN_POINT('Ctrl Pts',(-6.83447001700006,15.2,-8.59522900700001));
#285253=CARTESIAN_POINT('Ctrl Pts',(-6.83447001700006,11.6,-8.59522900700001));
#285254=CARTESIAN_POINT('Ctrl Pts',(-6.83544421900006,15.2,-8.59810106300002));
#285255=CARTESIAN_POINT('Ctrl Pts',(-6.83544421900006,11.6,-8.59810106300002));
#285256=CARTESIAN_POINT('Ctrl Pts',(-6.83641778800006,15.2,-8.60097898100002));
#285257=CARTESIAN_POINT('Ctrl Pts',(-6.83641778800006,11.6,-8.60097898100002));
#285258=CARTESIAN_POINT('Ctrl Pts',(-6.83739071400006,15.2,-8.60386275500002));
#285259=CARTESIAN_POINT('Ctrl Pts',(-6.83739071400006,11.6,-8.60386275500002));
#285260=CARTESIAN_POINT('Ctrl Pts',(-6.83836298800006,15.2,-8.60675237800002));
#285261=CARTESIAN_POINT('Ctrl Pts',(-6.83836298800006,11.6,-8.60675237800002));
#285262=CARTESIAN_POINT('Ctrl Pts',(-6.83933459800006,15.2,-8.60964784300002));
#285263=CARTESIAN_POINT('Ctrl Pts',(-6.83933459800006,11.6,-8.60964784300002));
#285264=CARTESIAN_POINT('Ctrl Pts',(-6.84030553600006,15.2,-8.61254914500002));
#285265=CARTESIAN_POINT('Ctrl Pts',(-6.84030553600006,11.6,-8.61254914500002));
#285266=CARTESIAN_POINT('Ctrl Pts',(-6.84127579200006,15.2,-8.61545627500002));
#285267=CARTESIAN_POINT('Ctrl Pts',(-6.84127579200006,11.6,-8.61545627500002));
#285268=CARTESIAN_POINT('Ctrl Pts',(-6.84224535400006,15.2,-8.61836922800002));
#285269=CARTESIAN_POINT('Ctrl Pts',(-6.84224535400006,11.6,-8.61836922800002));
#285270=CARTESIAN_POINT('Ctrl Pts',(-6.84321421300006,15.2,-8.62128799800002));
#285271=CARTESIAN_POINT('Ctrl Pts',(-6.84321421300006,11.6,-8.62128799800002));
#285272=CARTESIAN_POINT('Ctrl Pts',(-6.84418236000006,15.2,-8.62421257800002));
#285273=CARTESIAN_POINT('Ctrl Pts',(-6.84418236000006,11.6,-8.62421257800002));
#285274=CARTESIAN_POINT('Ctrl Pts',(-6.84514978400006,15.2,-8.62714296000001));
#285275=CARTESIAN_POINT('Ctrl Pts',(-6.84514978400006,11.6,-8.62714296000001));
#285276=CARTESIAN_POINT('Ctrl Pts',(-6.84611647700006,15.2,-8.63007914000002));
#285277=CARTESIAN_POINT('Ctrl Pts',(-6.84611647700006,11.6,-8.63007914000002));
#285278=CARTESIAN_POINT('Ctrl Pts',(-6.84708242700006,15.2,-8.63302111000002));
#285279=CARTESIAN_POINT('Ctrl Pts',(-6.84708242700006,11.6,-8.63302111000002));
#285280=CARTESIAN_POINT('Ctrl Pts',(-6.84804762500006,15.2,-8.63596886400002));
#285281=CARTESIAN_POINT('Ctrl Pts',(-6.84804762500006,11.6,-8.63596886400002));
#285282=CARTESIAN_POINT('Ctrl Pts',(-6.84901206200006,15.2,-8.63892239500002));
#285283=CARTESIAN_POINT('Ctrl Pts',(-6.84901206200006,11.6,-8.63892239500002));
#285284=CARTESIAN_POINT('Ctrl Pts',(-6.84997572700006,15.2,-8.64188169800002));
#285285=CARTESIAN_POINT('Ctrl Pts',(-6.84997572700006,11.6,-8.64188169800002));
#285286=CARTESIAN_POINT('Ctrl Pts',(-6.85093861100006,15.2,-8.64484676500001));
#285287=CARTESIAN_POINT('Ctrl Pts',(-6.85093861100006,11.6,-8.64484676500001));
#285288=CARTESIAN_POINT('Ctrl Pts',(-6.85190070400005,15.2,-8.64781759100002));
#285289=CARTESIAN_POINT('Ctrl Pts',(-6.85190070400005,11.6,-8.64781759100002));
#285290=CARTESIAN_POINT('Ctrl Pts',(-6.85286199700006,15.2,-8.65079416800001));
#285291=CARTESIAN_POINT('Ctrl Pts',(-6.85286199700006,11.6,-8.65079416800001));
#285292=CARTESIAN_POINT('Ctrl Pts',(-6.85382248000006,15.2,-8.65377649100001));
#285293=CARTESIAN_POINT('Ctrl Pts',(-6.85382248000006,11.6,-8.65377649100001));
#285294=CARTESIAN_POINT('Ctrl Pts',(-6.85478214300006,15.2,-8.65676455300001));
#285295=CARTESIAN_POINT('Ctrl Pts',(-6.85478214300006,11.6,-8.65676455300001));
#285296=CARTESIAN_POINT('Ctrl Pts',(-6.85574097600006,15.2,-8.65975834700001));
#285297=CARTESIAN_POINT('Ctrl Pts',(-6.85574097600006,11.6,-8.65975834700001));
#285298=CARTESIAN_POINT('Ctrl Pts',(-6.85669897100006,15.2,-8.66275786700001));
#285299=CARTESIAN_POINT('Ctrl Pts',(-6.85669897100006,11.6,-8.66275786700001));
#285300=CARTESIAN_POINT('Ctrl Pts',(-6.85765611700006,15.2,-8.66576310700001));
#285301=CARTESIAN_POINT('Ctrl Pts',(-6.85765611700006,11.6,-8.66576310700001));
#285302=CARTESIAN_POINT('Ctrl Pts',(-6.85861240500006,15.2,-8.66877406100001));
#285303=CARTESIAN_POINT('Ctrl Pts',(-6.85861240500006,11.6,-8.66877406100001));
#285304=CARTESIAN_POINT('Ctrl Pts',(-6.85956782600006,15.2,-8.67179072200001));
#285305=CARTESIAN_POINT('Ctrl Pts',(-6.85956782600006,11.6,-8.67179072200001));
#285306=CARTESIAN_POINT('Ctrl Pts',(-6.86052237000006,15.2,-8.67481308300002));
#285307=CARTESIAN_POINT('Ctrl Pts',(-6.86052237000006,11.6,-8.67481308300002));
#285308=CARTESIAN_POINT('Ctrl Pts',(-6.86147602800006,15.2,-8.67784113800001));
#285309=CARTESIAN_POINT('Ctrl Pts',(-6.86147602800006,11.6,-8.67784113800001));
#285310=CARTESIAN_POINT('Ctrl Pts',(-6.86242879000006,15.2,-8.68087488200001));
#285311=CARTESIAN_POINT('Ctrl Pts',(-6.86242879000006,11.6,-8.68087488200001));
#285312=CARTESIAN_POINT('Ctrl Pts',(-6.86338064600006,15.2,-8.68391430700001));
#285313=CARTESIAN_POINT('Ctrl Pts',(-6.86338064600006,11.6,-8.68391430700001));
#285314=CARTESIAN_POINT('Ctrl Pts',(-6.86433158900006,15.2,-8.68695940700002));
#285315=CARTESIAN_POINT('Ctrl Pts',(-6.86433158900006,11.6,-8.68695940700002));
#285316=CARTESIAN_POINT('Ctrl Pts',(-6.86528160700006,15.2,-8.69001017600001));
#285317=CARTESIAN_POINT('Ctrl Pts',(-6.86528160700006,11.6,-8.69001017600001));
#285318=CARTESIAN_POINT('Ctrl Pts',(-6.86623069200006,15.2,-8.69306660700002));
#285319=CARTESIAN_POINT('Ctrl Pts',(-6.86623069200006,11.6,-8.69306660700002));
#285320=CARTESIAN_POINT('Ctrl Pts',(-6.86717883600005,15.2,-8.69612869500001));
#285321=CARTESIAN_POINT('Ctrl Pts',(-6.86717883600005,11.6,-8.69612869500001));
#285322=CARTESIAN_POINT('Ctrl Pts',(-6.86812602700006,15.2,-8.69919643300002));
#285323=CARTESIAN_POINT('Ctrl Pts',(-6.86812602700006,11.6,-8.69919643300002));
#285324=CARTESIAN_POINT('Ctrl Pts',(-6.86907225800006,15.2,-8.70226981300002));
#285325=CARTESIAN_POINT('Ctrl Pts',(-6.86907225800006,11.6,-8.70226981300002));
#285326=CARTESIAN_POINT('Ctrl Pts',(-6.87001751800006,15.2,-8.70534883200002));
#285327=CARTESIAN_POINT('Ctrl Pts',(-6.87001751800006,11.6,-8.70534883200002));
#285328=CARTESIAN_POINT('Ctrl Pts',(-6.87096179900006,15.2,-8.70843348100001));
#285329=CARTESIAN_POINT('Ctrl Pts',(-6.87096179900006,11.6,-8.70843348100001));
#285330=CARTESIAN_POINT('Ctrl Pts',(-6.87190509000006,15.2,-8.71152375400002));
#285331=CARTESIAN_POINT('Ctrl Pts',(-6.87190509000006,11.6,-8.71152375400002));
#285332=CARTESIAN_POINT('Ctrl Pts',(-6.87284738500006,15.2,-8.71461964600002));
#285333=CARTESIAN_POINT('Ctrl Pts',(-6.87284738500006,11.6,-8.71461964600002));
#285334=CARTESIAN_POINT('Ctrl Pts',(-6.87378867400006,15.2,-8.71772115000002));
#285335=CARTESIAN_POINT('Ctrl Pts',(-6.87378867400006,11.6,-8.71772115000002));
#285336=CARTESIAN_POINT('Ctrl Pts',(-6.87472894500006,15.2,-8.72082826000002));
#285337=CARTESIAN_POINT('Ctrl Pts',(-6.87472894500006,11.6,-8.72082826000002));
#285338=CARTESIAN_POINT('Ctrl Pts',(-6.87566819300006,15.2,-8.72394096800001));
#285339=CARTESIAN_POINT('Ctrl Pts',(-6.87566819300006,11.6,-8.72394096800001));
#285340=CARTESIAN_POINT('Ctrl Pts',(-6.87660640700006,15.2,-8.72705927100002));
#285341=CARTESIAN_POINT('Ctrl Pts',(-6.87660640700006,11.6,-8.72705927100002));
#285342=CARTESIAN_POINT('Ctrl Pts',(-6.87754357700006,15.2,-8.73018316100002));
#285343=CARTESIAN_POINT('Ctrl Pts',(-6.87754357700006,11.6,-8.73018316100002));
#285344=CARTESIAN_POINT('Ctrl Pts',(-6.87847969500006,15.2,-8.73331263000001));
#285345=CARTESIAN_POINT('Ctrl Pts',(-6.87847969500006,11.6,-8.73331263000001));
#285346=CARTESIAN_POINT('Ctrl Pts',(-6.87941475200006,15.2,-8.73644767400001));
#285347=CARTESIAN_POINT('Ctrl Pts',(-6.87941475200006,11.6,-8.73644767400001));
#285348=CARTESIAN_POINT('Ctrl Pts',(-6.88034873900006,15.2,-8.73958828600001));
#285349=CARTESIAN_POINT('Ctrl Pts',(-6.88034873900006,11.6,-8.73958828600001));
#285350=CARTESIAN_POINT('Ctrl Pts',(-6.88128164800006,15.2,-8.74273446000002));
#285351=CARTESIAN_POINT('Ctrl Pts',(-6.88128164800006,11.6,-8.74273446000002));
#285352=CARTESIAN_POINT('Ctrl Pts',(-6.88221346800006,15.2,-8.74588619000002));
#285353=CARTESIAN_POINT('Ctrl Pts',(-6.88221346800006,11.6,-8.74588619000002));
#285354=CARTESIAN_POINT('Ctrl Pts',(-6.88314419200006,15.2,-8.74904347000001));
#285355=CARTESIAN_POINT('Ctrl Pts',(-6.88314419200006,11.6,-8.74904347000001));
#285356=CARTESIAN_POINT('Ctrl Pts',(-6.88407381100006,15.2,-8.75220629200001));
#285357=CARTESIAN_POINT('Ctrl Pts',(-6.88407381100006,11.6,-8.75220629200001));
#285358=CARTESIAN_POINT('Ctrl Pts',(-6.88500231400006,15.2,-8.75537465100001));
#285359=CARTESIAN_POINT('Ctrl Pts',(-6.88500231400006,11.6,-8.75537465100001));
#285360=CARTESIAN_POINT('Ctrl Pts',(-6.88592969500006,15.2,-8.75854854100002));
#285361=CARTESIAN_POINT('Ctrl Pts',(-6.88592969500006,11.6,-8.75854854100002));
#285362=CARTESIAN_POINT('Ctrl Pts',(-6.88685594400006,15.2,-8.76172795500001));
#285363=CARTESIAN_POINT('Ctrl Pts',(-6.88685594400006,11.6,-8.76172795500001));
#285364=CARTESIAN_POINT('Ctrl Pts',(-6.88778105300006,15.2,-8.76491288800001));
#285365=CARTESIAN_POINT('Ctrl Pts',(-6.88778105300006,11.6,-8.76491288800001));
#285366=CARTESIAN_POINT('Ctrl Pts',(-6.88870501100006,15.2,-8.76810333200002));
#285367=CARTESIAN_POINT('Ctrl Pts',(-6.88870501100006,11.6,-8.76810333200002));
#285368=CARTESIAN_POINT('Ctrl Pts',(-6.88962781100006,15.2,-8.77129928300001));
#285369=CARTESIAN_POINT('Ctrl Pts',(-6.88962781100006,11.6,-8.77129928300001));
#285370=CARTESIAN_POINT('Ctrl Pts',(-6.89054944500006,15.2,-8.77450073400002));
#285371=CARTESIAN_POINT('Ctrl Pts',(-6.89054944500006,11.6,-8.77450073400002));
#285372=CARTESIAN_POINT('Ctrl Pts',(-6.89146990300006,15.2,-8.77770767800002));
#285373=CARTESIAN_POINT('Ctrl Pts',(-6.89146990300006,11.6,-8.77770767800002));
#285374=CARTESIAN_POINT('Ctrl Pts',(-6.89238917600006,15.2,-8.78092010900002));
#285375=CARTESIAN_POINT('Ctrl Pts',(-6.89238917600006,11.6,-8.78092010900002));
#285376=CARTESIAN_POINT('Ctrl Pts',(-6.89330725700006,15.2,-8.78413802100001));
#285377=CARTESIAN_POINT('Ctrl Pts',(-6.89330725700006,11.6,-8.78413802100001));
#285378=CARTESIAN_POINT('Ctrl Pts',(-6.89422413500006,15.2,-8.78736140900001));
#285379=CARTESIAN_POINT('Ctrl Pts',(-6.89422413500006,11.6,-8.78736140900001));
#285380=CARTESIAN_POINT('Ctrl Pts',(-6.89513980400006,15.2,-8.79059026500002));
#285381=CARTESIAN_POINT('Ctrl Pts',(-6.89513980400006,11.6,-8.79059026500002));
#285382=CARTESIAN_POINT('Ctrl Pts',(-6.89605425400006,15.2,-8.79382458400002));
#285383=CARTESIAN_POINT('Ctrl Pts',(-6.89605425400006,11.6,-8.79382458400002));
#285384=CARTESIAN_POINT('Ctrl Pts',(-6.89696747600006,15.2,-8.79706435900001));
#285385=CARTESIAN_POINT('Ctrl Pts',(-6.89696747600006,11.6,-8.79706435900001));
#285386=CARTESIAN_POINT('Ctrl Pts',(-6.89787946300005,15.2,-8.80030958500001));
#285387=CARTESIAN_POINT('Ctrl Pts',(-6.89787946300005,11.6,-8.80030958500001));
#285388=CARTESIAN_POINT('Ctrl Pts',(-6.89879020600006,15.2,-8.80356025400001));
#285389=CARTESIAN_POINT('Ctrl Pts',(-6.89879020600006,11.6,-8.80356025400001));
#285390=CARTESIAN_POINT('Ctrl Pts',(-6.89969969600006,15.2,-8.80681636200002));
#285391=CARTESIAN_POINT('Ctrl Pts',(-6.89969969600006,11.6,-8.80681636200002));
#285392=CARTESIAN_POINT('Ctrl Pts',(-6.90060792400006,15.2,-8.81007790200002));
#285393=CARTESIAN_POINT('Ctrl Pts',(-6.90060792400006,11.6,-8.81007790200002));
#285394=CARTESIAN_POINT('Ctrl Pts',(-6.90151488200006,15.2,-8.81334486800002));
#285395=CARTESIAN_POINT('Ctrl Pts',(-6.90151488200006,11.6,-8.81334486800002));
#285396=CARTESIAN_POINT('Ctrl Pts',(-6.90242056300006,15.2,-8.81661725300001));
#285397=CARTESIAN_POINT('Ctrl Pts',(-6.90242056300006,11.6,-8.81661725300001));
#285398=CARTESIAN_POINT('Ctrl Pts',(-6.90332495800006,15.2,-8.81989505100002));
#285399=CARTESIAN_POINT('Ctrl Pts',(-6.90332495800006,11.6,-8.81989505100002));
#285400=CARTESIAN_POINT('Ctrl Pts',(-6.90422805600006,15.2,-8.82317825800002));
#285401=CARTESIAN_POINT('Ctrl Pts',(-6.90422805600006,11.6,-8.82317825800002));
#285402=CARTESIAN_POINT('Ctrl Pts',(-6.90512985200006,15.2,-8.82646686600001));
#285403=CARTESIAN_POINT('Ctrl Pts',(-6.90512985200006,11.6,-8.82646686600001));
#285404=CARTESIAN_POINT('Ctrl Pts',(-6.90603033600006,15.2,-8.82976086800002));
#285405=CARTESIAN_POINT('Ctrl Pts',(-6.90603033600006,11.6,-8.82976086800002));
#285406=CARTESIAN_POINT('Ctrl Pts',(-6.90692950100006,15.2,-8.83306026000002));
#285407=CARTESIAN_POINT('Ctrl Pts',(-6.90692950100006,11.6,-8.83306026000002));
#285408=CARTESIAN_POINT('Ctrl Pts',(-6.90782733600006,15.2,-8.83636503500002));
#285409=CARTESIAN_POINT('Ctrl Pts',(-6.90782733600006,11.6,-8.83636503500002));
#285410=CARTESIAN_POINT('Ctrl Pts',(-6.90872383500006,15.2,-8.83967518700001));
#285411=CARTESIAN_POINT('Ctrl Pts',(-6.90872383500006,11.6,-8.83967518700001));
#285412=CARTESIAN_POINT('Ctrl Pts',(-6.90961899000006,15.2,-8.84299071000001));
#285413=CARTESIAN_POINT('Ctrl Pts',(-6.90961899000006,11.6,-8.84299071000001));
#285414=CARTESIAN_POINT('Ctrl Pts',(-6.91051279100006,15.2,-8.84631159700002));
#285415=CARTESIAN_POINT('Ctrl Pts',(-6.91051279100006,11.6,-8.84631159700002));
#285416=CARTESIAN_POINT('Ctrl Pts',(-6.91140523100006,15.2,-8.84963784300002));
#285417=CARTESIAN_POINT('Ctrl Pts',(-6.91140523100006,11.6,-8.84963784300002));
#285418=CARTESIAN_POINT('Ctrl Pts',(-6.91229630100006,15.2,-8.85296944200002));
#285419=CARTESIAN_POINT('Ctrl Pts',(-6.91229630100006,11.6,-8.85296944200002));
#285420=CARTESIAN_POINT('Ctrl Pts',(-6.91318599400006,15.2,-8.85630638800002));
#285421=CARTESIAN_POINT('Ctrl Pts',(-6.91318599400006,11.6,-8.85630638800002));
#285422=CARTESIAN_POINT('Ctrl Pts',(-6.91407430200006,15.2,-8.85964867300002));
#285423=CARTESIAN_POINT('Ctrl Pts',(-6.91407430200006,11.6,-8.85964867300002));
#285424=CARTESIAN_POINT('Ctrl Pts',(-6.91496121500006,15.2,-8.86299629400002));
#285425=CARTESIAN_POINT('Ctrl Pts',(-6.91496121500006,11.6,-8.86299629400002));
#285426=CARTESIAN_POINT('Ctrl Pts',(-6.91584672600006,15.2,-8.86634924200001));
#285427=CARTESIAN_POINT('Ctrl Pts',(-6.91584672600006,11.6,-8.86634924200001));
#285428=CARTESIAN_POINT('Ctrl Pts',(-6.91673082700006,15.2,-8.86970751300002));
#285429=CARTESIAN_POINT('Ctrl Pts',(-6.91673082700006,11.6,-8.86970751300002));
#285430=CARTESIAN_POINT('Ctrl Pts',(-6.91761351000006,15.2,-8.87307110000001));
#285431=CARTESIAN_POINT('Ctrl Pts',(-6.91761351000006,11.6,-8.87307110000001));
#285432=CARTESIAN_POINT('Ctrl Pts',(-6.91849476600006,15.2,-8.87643999800002));
#285433=CARTESIAN_POINT('Ctrl Pts',(-6.91849476600006,11.6,-8.87643999800002));
#285434=CARTESIAN_POINT('Ctrl Pts',(-6.91937458800005,15.2,-8.87981420000001));
#285435=CARTESIAN_POINT('Ctrl Pts',(-6.91937458800005,11.6,-8.87981420000001));
#285436=CARTESIAN_POINT('Ctrl Pts',(-6.92025296800006,15.2,-8.88319369900002));
#285437=CARTESIAN_POINT('Ctrl Pts',(-6.92025296800006,11.6,-8.88319369900002));
#285438=CARTESIAN_POINT('Ctrl Pts',(-6.92112989800005,15.2,-8.88657849200002));
#285439=CARTESIAN_POINT('Ctrl Pts',(-6.92112989800005,11.6,-8.88657849200002));
#285440=CARTESIAN_POINT('Ctrl Pts',(-6.92200536800006,15.2,-8.88996857000001));
#285441=CARTESIAN_POINT('Ctrl Pts',(-6.92200536800006,11.6,-8.88996857000001));
#285442=CARTESIAN_POINT('Ctrl Pts',(-6.92287937300006,15.2,-8.89336392900002));
#285443=CARTESIAN_POINT('Ctrl Pts',(-6.92287937300006,11.6,-8.89336392900002));
#285444=CARTESIAN_POINT('Ctrl Pts',(-6.92375190400006,15.2,-8.89676456100002));
#285445=CARTESIAN_POINT('Ctrl Pts',(-6.92375190400006,11.6,-8.89676456100002));
#285446=CARTESIAN_POINT('Ctrl Pts',(-6.92462295300006,15.2,-8.90017046300001));
#285447=CARTESIAN_POINT('Ctrl Pts',(-6.92462295300006,11.6,-8.90017046300001));
#285448=CARTESIAN_POINT('Ctrl Pts',(-6.92549251200006,15.2,-8.90358162500002));
#285449=CARTESIAN_POINT('Ctrl Pts',(-6.92549251200006,11.6,-8.90358162500002));
#285450=CARTESIAN_POINT('Ctrl Pts',(-6.92636057200006,15.2,-8.90699804400001));
#285451=CARTESIAN_POINT('Ctrl Pts',(-6.92636057200006,11.6,-8.90699804400001));
#285452=CARTESIAN_POINT('Ctrl Pts',(-6.92722712700006,15.2,-8.91041971300002));
#285453=CARTESIAN_POINT('Ctrl Pts',(-6.92722712700006,11.6,-8.91041971300002));
#285454=CARTESIAN_POINT('Ctrl Pts',(-6.92809216800006,15.2,-8.91384662700002));
#285455=CARTESIAN_POINT('Ctrl Pts',(-6.92809216800006,11.6,-8.91384662700002));
#285456=CARTESIAN_POINT('Ctrl Pts',(-6.92895568900005,15.2,-8.91727877800001));
#285457=CARTESIAN_POINT('Ctrl Pts',(-6.92895568900005,11.6,-8.91727877800001));
#285458=CARTESIAN_POINT('Ctrl Pts',(-6.92981767900006,15.2,-8.92071616200001));
#285459=CARTESIAN_POINT('Ctrl Pts',(-6.92981767900006,11.6,-8.92071616200001));
#285460=CARTESIAN_POINT('Ctrl Pts',(-6.93067813200006,15.2,-8.92415877200002));
#285461=CARTESIAN_POINT('Ctrl Pts',(-6.93067813200006,11.6,-8.92415877200002));
#285462=CARTESIAN_POINT('Ctrl Pts',(-6.93153704100006,15.2,-8.92760660300001));
#285463=CARTESIAN_POINT('Ctrl Pts',(-6.93153704100006,11.6,-8.92760660300001));
#285464=CARTESIAN_POINT('Ctrl Pts',(-6.93239439700006,15.2,-8.93105964700002));
#285465=CARTESIAN_POINT('Ctrl Pts',(-6.93239439700006,11.6,-8.93105964700002));
#285466=CARTESIAN_POINT('Ctrl Pts',(-6.93325019300006,15.2,-8.93451789900002));
#285467=CARTESIAN_POINT('Ctrl Pts',(-6.93325019300006,11.6,-8.93451789900002));
#285468=CARTESIAN_POINT('Ctrl Pts',(-6.93410442200006,15.2,-8.93798135500001));
#285469=CARTESIAN_POINT('Ctrl Pts',(-6.93410442200006,11.6,-8.93798135500001));
#285470=CARTESIAN_POINT('Ctrl Pts',(-6.93495707400006,15.2,-8.94145000600002));
#285471=CARTESIAN_POINT('Ctrl Pts',(-6.93495707400006,11.6,-8.94145000600002));
#285472=CARTESIAN_POINT('Ctrl Pts',(-6.93580814300006,15.2,-8.94492384900002));
#285473=CARTESIAN_POINT('Ctrl Pts',(-6.93580814300006,11.6,-8.94492384900002));
#285474=CARTESIAN_POINT('Ctrl Pts',(-6.93665762200006,15.2,-8.94840287600001));
#285475=CARTESIAN_POINT('Ctrl Pts',(-6.93665762200006,11.6,-8.94840287600001));
#285476=CARTESIAN_POINT('Ctrl Pts',(-6.93750550100006,15.2,-8.95188708100001));
#285477=CARTESIAN_POINT('Ctrl Pts',(-6.93750550100006,11.6,-8.95188708100001));
#285478=CARTESIAN_POINT('Ctrl Pts',(-6.93835177400006,15.2,-8.95537645900001));
#285479=CARTESIAN_POINT('Ctrl Pts',(-6.93835177400006,11.6,-8.95537645900001));
#285480=CARTESIAN_POINT('Ctrl Pts',(-6.93919643300006,15.2,-8.95887100400002));
#285481=CARTESIAN_POINT('Ctrl Pts',(-6.93919643300006,11.6,-8.95887100400002));
#285482=CARTESIAN_POINT('Ctrl Pts',(-6.94003947100006,15.2,-8.96237071000002));
#285483=CARTESIAN_POINT('Ctrl Pts',(-6.94003947100006,11.6,-8.96237071000002));
#285484=CARTESIAN_POINT('Ctrl Pts',(-6.94088088100006,15.2,-8.96587557000002));
#285485=CARTESIAN_POINT('Ctrl Pts',(-6.94088088100006,11.6,-8.96587557000002));
#285486=CARTESIAN_POINT('Ctrl Pts',(-6.94172065300006,15.2,-8.96938558000001));
#285487=CARTESIAN_POINT('Ctrl Pts',(-6.94172065300006,11.6,-8.96938558000001));
#285488=CARTESIAN_POINT('Ctrl Pts',(-6.94255878100006,15.2,-8.97290073300002));
#285489=CARTESIAN_POINT('Ctrl Pts',(-6.94255878100006,11.6,-8.97290073300002));
#285490=CARTESIAN_POINT('Ctrl Pts',(-6.94339525800006,15.2,-8.97642102300001));
#285491=CARTESIAN_POINT('Ctrl Pts',(-6.94339525800006,11.6,-8.97642102300001));
#285492=CARTESIAN_POINT('Ctrl Pts',(-6.94423007700006,15.2,-8.97994644400002));
#285493=CARTESIAN_POINT('Ctrl Pts',(-6.94423007700006,11.6,-8.97994644400002));
#285494=CARTESIAN_POINT('Ctrl Pts',(-6.94506322800006,15.2,-8.98347699100002));
#285495=CARTESIAN_POINT('Ctrl Pts',(-6.94506322800006,11.6,-8.98347699100002));
#285496=CARTESIAN_POINT('Ctrl Pts',(-6.94589470500006,15.2,-8.98701265600002));
#285497=CARTESIAN_POINT('Ctrl Pts',(-6.94589470500006,11.6,-8.98701265600002));
#285498=CARTESIAN_POINT('Ctrl Pts',(-6.94672450200006,15.2,-8.99055343700002));
#285499=CARTESIAN_POINT('Ctrl Pts',(-6.94672450200006,11.6,-8.99055343700002));
#285500=CARTESIAN_POINT('Ctrl Pts',(-6.94755260900005,15.2,-8.99409932400001));
#285501=CARTESIAN_POINT('Ctrl Pts',(-6.94755260900005,11.6,-8.99409932400001));
#285502=CARTESIAN_POINT('Ctrl Pts',(-6.94837902000006,15.2,-8.99765031300002));
#285503=CARTESIAN_POINT('Ctrl Pts',(-6.94837902000006,11.6,-8.99765031300002));
#285504=CARTESIAN_POINT('Ctrl Pts',(-6.94920372700006,15.2,-9.00120639800001));
#285505=CARTESIAN_POINT('Ctrl Pts',(-6.94920372700006,11.6,-9.00120639800001));
#285506=CARTESIAN_POINT('Ctrl Pts',(-6.95002672400006,15.2,-9.00476757400002));
#285507=CARTESIAN_POINT('Ctrl Pts',(-6.95002672400006,11.6,-9.00476757400002));
#285508=CARTESIAN_POINT('Ctrl Pts',(-6.95084800200005,15.2,-9.00833383300002));
#285509=CARTESIAN_POINT('Ctrl Pts',(-6.95084800200005,11.6,-9.00833383300002));
#285510=CARTESIAN_POINT('Ctrl Pts',(-6.95166755500006,15.2,-9.01190517100002));
#285511=CARTESIAN_POINT('Ctrl Pts',(-6.95166755500006,11.6,-9.01190517100002));
#285512=CARTESIAN_POINT('Ctrl Pts',(-6.95248537400006,15.2,-9.01548158100002));
#285513=CARTESIAN_POINT('Ctrl Pts',(-6.95248537400006,11.6,-9.01548158100002));
#285514=CARTESIAN_POINT('Ctrl Pts',(-6.95330145500006,15.2,-9.01906305900001));
#285515=CARTESIAN_POINT('Ctrl Pts',(-6.95330145500006,11.6,-9.01906305900001));
#285516=CARTESIAN_POINT('Ctrl Pts',(-6.95411578700006,15.2,-9.02264959600002));
#285517=CARTESIAN_POINT('Ctrl Pts',(-6.95411578700006,11.6,-9.02264959600002));
#285518=CARTESIAN_POINT('Ctrl Pts',(-6.95492836400006,15.2,-9.02624119000001));
#285519=CARTESIAN_POINT('Ctrl Pts',(-6.95492836400006,11.6,-9.02624119000001));
#285520=CARTESIAN_POINT('Ctrl Pts',(-6.95573917800006,15.2,-9.02983783100002));
#285521=CARTESIAN_POINT('Ctrl Pts',(-6.95573917800006,11.6,-9.02983783100002));
#285522=CARTESIAN_POINT('Ctrl Pts',(-6.95654822400006,15.2,-9.03343951600002));
#285523=CARTESIAN_POINT('Ctrl Pts',(-6.95654822400006,11.6,-9.03343951600002));
#285524=CARTESIAN_POINT('Ctrl Pts',(-6.95735549400006,15.2,-9.03704623800002));
#285525=CARTESIAN_POINT('Ctrl Pts',(-6.95735549400006,11.6,-9.03704623800002));
#285526=CARTESIAN_POINT('Ctrl Pts',(-6.95816097900006,15.2,-9.04065799200002));
#285527=CARTESIAN_POINT('Ctrl Pts',(-6.95816097900006,11.6,-9.04065799200002));
#285528=CARTESIAN_POINT('Ctrl Pts',(-6.95896467400006,15.2,-9.04427477200001));
#285529=CARTESIAN_POINT('Ctrl Pts',(-6.95896467400006,11.6,-9.04427477200001));
#285530=CARTESIAN_POINT('Ctrl Pts',(-6.95976657100006,15.2,-9.04789657100002));
#285531=CARTESIAN_POINT('Ctrl Pts',(-6.95976657100006,11.6,-9.04789657100002));
#285532=CARTESIAN_POINT('Ctrl Pts',(-6.96056666300006,15.2,-9.05152338500002));
#285533=CARTESIAN_POINT('Ctrl Pts',(-6.96056666300006,11.6,-9.05152338500002));
#285534=CARTESIAN_POINT('Ctrl Pts',(-6.96136494300006,15.2,-9.05515520900002));
#285535=CARTESIAN_POINT('Ctrl Pts',(-6.96136494300006,11.6,-9.05515520900002));
#285536=CARTESIAN_POINT('Ctrl Pts',(-6.96216140500006,15.2,-9.05879203500002));
#285537=CARTESIAN_POINT('Ctrl Pts',(-6.96216140500006,11.6,-9.05879203500002));
#285538=CARTESIAN_POINT('Ctrl Pts',(-6.96295604000006,15.2,-9.06243385600002));
#285539=CARTESIAN_POINT('Ctrl Pts',(-6.96295604000006,11.6,-9.06243385600002));
#285540=CARTESIAN_POINT('Ctrl Pts',(-6.96374884000006,15.2,-9.06608066900001));
#285541=CARTESIAN_POINT('Ctrl Pts',(-6.96374884000006,11.6,-9.06608066900001));
#285542=CARTESIAN_POINT('Ctrl Pts',(-6.96453980000006,15.2,-9.06973246600002));
#285543=CARTESIAN_POINT('Ctrl Pts',(-6.96453980000006,11.6,-9.06973246600002));
#285544=CARTESIAN_POINT('Ctrl Pts',(-6.96532891100006,15.2,-9.07338924200002));
#285545=CARTESIAN_POINT('Ctrl Pts',(-6.96532891100006,11.6,-9.07338924200002));
#285546=CARTESIAN_POINT('Ctrl Pts',(-6.96611616800006,15.2,-9.07705099100001));
#285547=CARTESIAN_POINT('Ctrl Pts',(-6.96611616800006,11.6,-9.07705099100001));
#285548=CARTESIAN_POINT('Ctrl Pts',(-6.96690156100006,15.2,-9.08071770700002));
#285549=CARTESIAN_POINT('Ctrl Pts',(-6.96690156100006,11.6,-9.08071770700002));
#285550=CARTESIAN_POINT('Ctrl Pts',(-6.96768508700006,15.2,-9.08438938500002));
#285551=CARTESIAN_POINT('Ctrl Pts',(-6.96768508700006,11.6,-9.08438938500002));
#285552=CARTESIAN_POINT('Ctrl Pts',(-6.96846673800006,15.2,-9.08806602100002));
#285553=CARTESIAN_POINT('Ctrl Pts',(-6.96846673800006,11.6,-9.08806602100002));
#285554=CARTESIAN_POINT('Ctrl Pts',(-6.96924650800006,15.2,-9.09174760800001));
#285555=CARTESIAN_POINT('Ctrl Pts',(-6.96924650800006,11.6,-9.09174760800001));
#285556=CARTESIAN_POINT('Ctrl Pts',(-6.97002439000006,15.2,-9.09543414100002));
#285557=CARTESIAN_POINT('Ctrl Pts',(-6.97002439000006,11.6,-9.09543414100002));
#285558=CARTESIAN_POINT('Ctrl Pts',(-6.97080037900006,15.2,-9.09912561500001));
#285559=CARTESIAN_POINT('Ctrl Pts',(-6.97080037900006,11.6,-9.09912561500001));
#285560=CARTESIAN_POINT('Ctrl Pts',(-6.97157446400006,15.2,-9.10282202200002));
#285561=CARTESIAN_POINT('Ctrl Pts',(-6.97157446400006,11.6,-9.10282202200002));
#285562=CARTESIAN_POINT('Ctrl Pts',(-6.97234663900006,15.2,-9.10652335600002));
#285563=CARTESIAN_POINT('Ctrl Pts',(-6.97234663900006,11.6,-9.10652335600002));
#285564=CARTESIAN_POINT('Ctrl Pts',(-6.97311689200006,15.2,-9.11022960800001));
#285565=CARTESIAN_POINT('Ctrl Pts',(-6.97311689200006,11.6,-9.11022960800001));
#285566=CARTESIAN_POINT('Ctrl Pts',(-6.97388521800006,15.2,-9.11394077400002));
#285567=CARTESIAN_POINT('Ctrl Pts',(-6.97388521800006,11.6,-9.11394077400002));
#285568=CARTESIAN_POINT('Ctrl Pts',(-6.97465160800006,15.2,-9.11765684500002));
#285569=CARTESIAN_POINT('Ctrl Pts',(-6.97465160800006,11.6,-9.11765684500002));
#285570=CARTESIAN_POINT('Ctrl Pts',(-6.97541605700006,15.2,-9.12137781700002));
#285571=CARTESIAN_POINT('Ctrl Pts',(-6.97541605700006,11.6,-9.12137781700002));
#285572=CARTESIAN_POINT('Ctrl Pts',(-6.97617855900006,15.2,-9.12510368500002));
#285573=CARTESIAN_POINT('Ctrl Pts',(-6.97617855900006,11.6,-9.12510368500002));
#285574=CARTESIAN_POINT('Ctrl Pts',(-6.97693911100006,15.2,-9.12883444900002));
#285575=CARTESIAN_POINT('Ctrl Pts',(-6.97693911100006,11.6,-9.12883444900002));
#285576=CARTESIAN_POINT('Ctrl Pts',(-6.97769771300006,15.2,-9.13257010500002));
#285577=CARTESIAN_POINT('Ctrl Pts',(-6.97769771300006,11.6,-9.13257010500002));
#285578=CARTESIAN_POINT('Ctrl Pts',(-6.97830303200006,15.2,-9.13556254300002));
#285579=CARTESIAN_POINT('Ctrl Pts',(-6.97830303200006,11.6,-9.13556254300002));
#285580=CARTESIAN_POINT('Ctrl Pts',(-6.97875614300006,15.2,-9.13780907300002));
#285581=CARTESIAN_POINT('Ctrl Pts',(-6.97875614300006,11.6,-9.13780907300002));
#285582=CARTESIAN_POINT('Ctrl Pts',(-6.97905782800006,15.2,-9.13930773800002));
#285583=CARTESIAN_POINT('Ctrl Pts',(-6.97905782800006,11.6,-9.13930773800002));
#285584=CARTESIAN_POINT('Ctrl Pts',(-6.97920857100006,15.2,-9.14005731500002));
#285585=CARTESIAN_POINT('Ctrl Pts',(-6.97920857100006,11.6,-9.14005731500002));
#285586=CARTESIAN_POINT('Ctrl Pts',(-6.57080831900006,15.2,-8.02901631800001));
#285587=CARTESIAN_POINT('Ctrl Pts',(-6.57090674100006,15.2,-8.02916024100002));
#285588=CARTESIAN_POINT('Ctrl Pts',(-6.57110695100006,15.2,-8.02945316300002));
#285589=CARTESIAN_POINT('Ctrl Pts',(-6.57141009900006,15.2,-8.02989715700001));
#285590=CARTESIAN_POINT('Ctrl Pts',(-6.57181802000006,15.2,-8.03049556400002));
#285591=CARTESIAN_POINT('Ctrl Pts',(-6.57233322400006,15.2,-8.03125297300002));
#285592=CARTESIAN_POINT('Ctrl Pts',(-6.57285600600006,15.2,-8.03202318500002));
#285593=CARTESIAN_POINT('Ctrl Pts',(-6.57338335000006,15.2,-8.03280179700002));
#285594=CARTESIAN_POINT('Ctrl Pts',(-6.57391522700006,15.2,-8.03358880000001));
#285595=CARTESIAN_POINT('Ctrl Pts',(-6.57445160600005,15.2,-8.03438417800002));
#285596=CARTESIAN_POINT('Ctrl Pts',(-6.57499245700006,15.2,-8.03518792300002));
#285597=CARTESIAN_POINT('Ctrl Pts',(-6.57553775200006,15.2,-8.03600002100002));
#285598=CARTESIAN_POINT('Ctrl Pts',(-6.57608746000006,15.2,-8.03682046000001));
#285599=CARTESIAN_POINT('Ctrl Pts',(-6.57664155100006,15.2,-8.03764922800001));
#285600=CARTESIAN_POINT('Ctrl Pts',(-6.57719999700006,15.2,-8.03848631500001));
#285601=CARTESIAN_POINT('Ctrl Pts',(-6.57776276900006,15.2,-8.03933170500001));
#285602=CARTESIAN_POINT('Ctrl Pts',(-6.57832983700006,15.2,-8.04018539000002));
#285603=CARTESIAN_POINT('Ctrl Pts',(-6.57890117200005,15.2,-8.04104735800001));
#285604=CARTESIAN_POINT('Ctrl Pts',(-6.57947674700006,15.2,-8.04191759500002));
#285605=CARTESIAN_POINT('Ctrl Pts',(-6.58005653200005,15.2,-8.04279609000002));
#285606=CARTESIAN_POINT('Ctrl Pts',(-6.58064050000006,15.2,-8.04368283300001));
#285607=CARTESIAN_POINT('Ctrl Pts',(-6.58122862000006,15.2,-8.04457781100002));
#285608=CARTESIAN_POINT('Ctrl Pts',(-6.58182086700006,15.2,-8.04548101200002));
#285609=CARTESIAN_POINT('Ctrl Pts',(-6.58241721200006,15.2,-8.04639242700001));
#285610=CARTESIAN_POINT('Ctrl Pts',(-6.58301762700006,15.2,-8.04731204200002));
#285611=CARTESIAN_POINT('Ctrl Pts',(-6.58362208300006,15.2,-8.04823984600001));
#285612=CARTESIAN_POINT('Ctrl Pts',(-6.58423055400006,15.2,-8.04917582900002));
#285613=CARTESIAN_POINT('Ctrl Pts',(-6.58484301300006,15.2,-8.05011997800002));
#285614=CARTESIAN_POINT('Ctrl Pts',(-6.58545943100005,15.2,-8.05107228200002));
#285615=CARTESIAN_POINT('Ctrl Pts',(-6.58607978300005,15.2,-8.05203273100001));
#285616=CARTESIAN_POINT('Ctrl Pts',(-6.58670404000006,15.2,-8.05300131300001));
#285617=CARTESIAN_POINT('Ctrl Pts',(-6.58733217600005,15.2,-8.05397801700002));
#285618=CARTESIAN_POINT('Ctrl Pts',(-6.58796416400006,15.2,-8.05496283100002));
#285619=CARTESIAN_POINT('Ctrl Pts',(-6.58859997800006,15.2,-8.05595574500002));
#285620=CARTESIAN_POINT('Ctrl Pts',(-6.58923959000006,15.2,-8.05695674700001));
#285621=CARTESIAN_POINT('Ctrl Pts',(-6.58988297600006,15.2,-8.05796582700001));
#285622=CARTESIAN_POINT('Ctrl Pts',(-6.59053010700006,15.2,-8.05898297300002));
#285623=CARTESIAN_POINT('Ctrl Pts',(-6.59118095900006,15.2,-8.06000817400001));
#285624=CARTESIAN_POINT('Ctrl Pts',(-6.59183550500006,15.2,-8.06104142000001));
#285625=CARTESIAN_POINT('Ctrl Pts',(-6.59249371900006,15.2,-8.06208270100001));
#285626=CARTESIAN_POINT('Ctrl Pts',(-6.59315557600006,15.2,-8.06313200300002));
#285627=CARTESIAN_POINT('Ctrl Pts',(-6.59382104900006,15.2,-8.06418931800001));
#285628=CARTESIAN_POINT('Ctrl Pts',(-6.59449011500006,15.2,-8.06525463500002));
#285629=CARTESIAN_POINT('Ctrl Pts',(-6.59516274600006,15.2,-8.06632794100001));
#285630=CARTESIAN_POINT('Ctrl Pts',(-6.59583891700006,15.2,-8.06740922800002));
#285631=CARTESIAN_POINT('Ctrl Pts',(-6.59651860500006,15.2,-8.06849848300002));
#285632=CARTESIAN_POINT('Ctrl Pts',(-6.59720178300006,15.2,-8.06959569800001));
#285633=CARTESIAN_POINT('Ctrl Pts',(-6.59788842600006,15.2,-8.07070086000002));
#285634=CARTESIAN_POINT('Ctrl Pts',(-6.59857851000006,15.2,-8.07181396000002));
#285635=CARTESIAN_POINT('Ctrl Pts',(-6.59927200900006,15.2,-8.07293498700002));
#285636=CARTESIAN_POINT('Ctrl Pts',(-6.59996890100006,15.2,-8.07406392900001));
#285637=CARTESIAN_POINT('Ctrl Pts',(-6.60066916000006,15.2,-8.07520077800002));
#285638=CARTESIAN_POINT('Ctrl Pts',(-6.60137276000006,15.2,-8.07634552200001));
#285639=CARTESIAN_POINT('Ctrl Pts',(-6.60207968000006,15.2,-8.07749815200001));
#285640=CARTESIAN_POINT('Ctrl Pts',(-6.60278989300005,15.2,-8.07865865600002));
#285641=CARTESIAN_POINT('Ctrl Pts',(-6.60350337600006,15.2,-8.07982702500002));
#285642=CARTESIAN_POINT('Ctrl Pts',(-6.60422010600006,15.2,-8.08100324800002));
#285643=CARTESIAN_POINT('Ctrl Pts',(-6.60494005800006,15.2,-8.08218731500002));
#285644=CARTESIAN_POINT('Ctrl Pts',(-6.60566320900006,15.2,-8.08337921500001));
#285645=CARTESIAN_POINT('Ctrl Pts',(-6.60638953400006,15.2,-8.08457893900002));
#285646=CARTESIAN_POINT('Ctrl Pts',(-6.60711901100006,15.2,-8.08578647500001));
#285647=CARTESIAN_POINT('Ctrl Pts',(-6.60785161500006,15.2,-8.08700181500001));
#285648=CARTESIAN_POINT('Ctrl Pts',(-6.60858732500006,15.2,-8.08822494800001));
#285649=CARTESIAN_POINT('Ctrl Pts',(-6.60932611700006,15.2,-8.08945586400002));
#285650=CARTESIAN_POINT('Ctrl Pts',(-6.61006796600006,15.2,-8.09069455200002));
#285651=CARTESIAN_POINT('Ctrl Pts',(-6.61081285100006,15.2,-8.09194100300001));
#285652=CARTESIAN_POINT('Ctrl Pts',(-6.61156074900005,15.2,-8.09319520700001));
#285653=CARTESIAN_POINT('Ctrl Pts',(-6.61231163600006,15.2,-8.09445715400001));
#285654=CARTESIAN_POINT('Ctrl Pts',(-6.61306549000006,15.2,-8.09572683400001));
#285655=CARTESIAN_POINT('Ctrl Pts',(-6.61382229000006,15.2,-8.09700423600002));
#285656=CARTESIAN_POINT('Ctrl Pts',(-6.61458201100006,15.2,-8.09828935200001));
#285657=CARTESIAN_POINT('Ctrl Pts',(-6.61534463100006,15.2,-8.09958217100002));
#285658=CARTESIAN_POINT('Ctrl Pts',(-6.61611012900006,15.2,-8.10088268300002));
#285659=CARTESIAN_POINT('Ctrl Pts',(-6.61687848200006,15.2,-8.10219087900002));
#285660=CARTESIAN_POINT('Ctrl Pts',(-6.61764966700006,15.2,-8.10350674900001));
#285661=CARTESIAN_POINT('Ctrl Pts',(-6.61842366400006,15.2,-8.10483028300002));
#285662=CARTESIAN_POINT('Ctrl Pts',(-6.61920045000006,15.2,-8.10616147100001));
#285663=CARTESIAN_POINT('Ctrl Pts',(-6.61998000200006,15.2,-8.10750030400002));
#285664=CARTESIAN_POINT('Ctrl Pts',(-6.62076230000006,15.2,-8.10884677100002));
#285665=CARTESIAN_POINT('Ctrl Pts',(-6.62154732100006,15.2,-8.11020086400001));
#285666=CARTESIAN_POINT('Ctrl Pts',(-6.62233504600006,15.2,-8.11156257400001));
#285667=CARTESIAN_POINT('Ctrl Pts',(-6.62312545000006,15.2,-8.11293188900001));
#285668=CARTESIAN_POINT('Ctrl Pts',(-6.62391851400006,15.2,-8.11430880100002));
#285669=CARTESIAN_POINT('Ctrl Pts',(-6.62471421500006,15.2,-8.11569329900001));
#285670=CARTESIAN_POINT('Ctrl Pts',(-6.62551253400006,15.2,-8.11708537600002));
#285671=CARTESIAN_POINT('Ctrl Pts',(-6.62631344800006,15.2,-8.11848502000002));
#285672=CARTESIAN_POINT('Ctrl Pts',(-6.62711693700006,15.2,-8.11989222400002));
#285673=CARTESIAN_POINT('Ctrl Pts',(-6.62792298000006,15.2,-8.12130697600002));
#285674=CARTESIAN_POINT('Ctrl Pts',(-6.62873155500006,15.2,-8.12272926700001));
#285675=CARTESIAN_POINT('Ctrl Pts',(-6.62954264200006,15.2,-8.12415909000002));
#285676=CARTESIAN_POINT('Ctrl Pts',(-6.63035622100006,15.2,-8.12559643400002));
#285677=CARTESIAN_POINT('Ctrl Pts',(-6.63117227000006,15.2,-8.12704128900002));
#285678=CARTESIAN_POINT('Ctrl Pts',(-6.63199077100006,15.2,-8.12849364600002));
#285679=CARTESIAN_POINT('Ctrl Pts',(-6.63281170000006,15.2,-8.12995349700002));
#285680=CARTESIAN_POINT('Ctrl Pts',(-6.63363504000006,15.2,-8.13142083100002));
#285681=CARTESIAN_POINT('Ctrl Pts',(-6.63446076800006,15.2,-8.13289564100002));
#285682=CARTESIAN_POINT('Ctrl Pts',(-6.63528886600006,15.2,-8.13437791500002));
#285683=CARTESIAN_POINT('Ctrl Pts',(-6.63611931200006,15.2,-8.13586764600002));
#285684=CARTESIAN_POINT('Ctrl Pts',(-6.63695208700006,15.2,-8.13736482400002));
#285685=CARTESIAN_POINT('Ctrl Pts',(-6.63778717100006,15.2,-8.13886943900001));
#285686=CARTESIAN_POINT('Ctrl Pts',(-6.63862454400006,15.2,-8.14038148300002));
#285687=CARTESIAN_POINT('Ctrl Pts',(-6.63946418700006,15.2,-8.14190094700002));
#285688=CARTESIAN_POINT('Ctrl Pts',(-6.64030607900005,15.2,-8.14342782100002));
#285689=CARTESIAN_POINT('Ctrl Pts',(-6.64115020100006,15.2,-8.14496209700001));
#285690=CARTESIAN_POINT('Ctrl Pts',(-6.64199653400006,15.2,-8.14650376600002));
#285691=CARTESIAN_POINT('Ctrl Pts',(-6.64284505800006,15.2,-8.14805281700002));
#285692=CARTESIAN_POINT('Ctrl Pts',(-6.64369575300006,15.2,-8.14960924300001));
#285693=CARTESIAN_POINT('Ctrl Pts',(-6.64454859900006,15.2,-8.15117303500001));
#285694=CARTESIAN_POINT('Ctrl Pts',(-6.64540358000006,15.2,-8.15274418300002));
#285695=CARTESIAN_POINT('Ctrl Pts',(-6.64626067400006,15.2,-8.15432267900002));
#285696=CARTESIAN_POINT('Ctrl Pts',(-6.64711986400006,15.2,-8.15590851400002));
#285697=CARTESIAN_POINT('Ctrl Pts',(-6.64798112800006,15.2,-8.15750167800001));
#285698=CARTESIAN_POINT('Ctrl Pts',(-6.64884444900006,15.2,-8.15910216300002));
#285699=CARTESIAN_POINT('Ctrl Pts',(-6.64970980800006,15.2,-8.16070996000001));
#285700=CARTESIAN_POINT('Ctrl Pts',(-6.65057718600006,15.2,-8.16232506100001));
#285701=CARTESIAN_POINT('Ctrl Pts',(-6.65144656600006,15.2,-8.16394745500002));
#285702=CARTESIAN_POINT('Ctrl Pts',(-6.65231792600006,15.2,-8.16557713600002));
#285703=CARTESIAN_POINT('Ctrl Pts',(-6.65319124900006,15.2,-8.16721409300002));
#285704=CARTESIAN_POINT('Ctrl Pts',(-6.65406651700006,15.2,-8.16885831900001));
#285705=CARTESIAN_POINT('Ctrl Pts',(-6.65494371100006,15.2,-8.17050980400002));
#285706=CARTESIAN_POINT('Ctrl Pts',(-6.65582281300006,15.2,-8.17216853900002));
#285707=CARTESIAN_POINT('Ctrl Pts',(-6.65670380500006,15.2,-8.17383451600002));
#285708=CARTESIAN_POINT('Ctrl Pts',(-6.65758666800006,15.2,-8.17550772700002));
#285709=CARTESIAN_POINT('Ctrl Pts',(-6.65847138400006,15.2,-8.17718816300001));
#285710=CARTESIAN_POINT('Ctrl Pts',(-6.65935793500006,15.2,-8.17887581400001));
#285711=CARTESIAN_POINT('Ctrl Pts',(-6.66024630300006,15.2,-8.18057067400002));
#285712=CARTESIAN_POINT('Ctrl Pts',(-6.66113647000006,15.2,-8.18227273100002));
#285713=CARTESIAN_POINT('Ctrl Pts',(-6.66202841900006,15.2,-8.18398198000001));
#285714=CARTESIAN_POINT('Ctrl Pts',(-6.66292212900006,15.2,-8.18569840900001));
#285715=CARTESIAN_POINT('Ctrl Pts',(-6.66381758700005,15.2,-8.18742201300001));
#285716=CARTESIAN_POINT('Ctrl Pts',(-6.66471477200006,15.2,-8.18915278000001));
#285717=CARTESIAN_POINT('Ctrl Pts',(-6.66561366700006,15.2,-8.19089070400001));
#285718=CARTESIAN_POINT('Ctrl Pts',(-6.66651425400006,15.2,-8.19263577600001));
#285719=CARTESIAN_POINT('Ctrl Pts',(-6.66741651800006,15.2,-8.19438798600002));
#285720=CARTESIAN_POINT('Ctrl Pts',(-6.66832043800006,15.2,-8.19614732700002));
#285721=CARTESIAN_POINT('Ctrl Pts',(-6.66922600000006,15.2,-8.19791379200002));
#285722=CARTESIAN_POINT('Ctrl Pts',(-6.67013318300006,15.2,-8.19968736900002));
#285723=CARTESIAN_POINT('Ctrl Pts',(-6.67104197300006,15.2,-8.20146805200002));
#285724=CARTESIAN_POINT('Ctrl Pts',(-6.67195235200006,15.2,-8.20325583300002));
#285725=CARTESIAN_POINT('Ctrl Pts',(-6.67286430200006,15.2,-8.20505070200002));
#285726=CARTESIAN_POINT('Ctrl Pts',(-6.67377780700006,15.2,-8.20685265200002));
#285727=CARTESIAN_POINT('Ctrl Pts',(-6.67469285000006,15.2,-8.20866167300002));
#285728=CARTESIAN_POINT('Ctrl Pts',(-6.67560941300006,15.2,-8.21047775800002));
#285729=CARTESIAN_POINT('Ctrl Pts',(-6.67652747900005,15.2,-8.21230089900002));
#285730=CARTESIAN_POINT('Ctrl Pts',(-6.67744703200006,15.2,-8.21413108800002));
#285731=CARTESIAN_POINT('Ctrl Pts',(-6.67836805600006,15.2,-8.21596831500001));
#285732=CARTESIAN_POINT('Ctrl Pts',(-6.67929053300006,15.2,-8.21781257300002));
#285733=CARTESIAN_POINT('Ctrl Pts',(-6.68021444700006,15.2,-8.21966385300002));
#285734=CARTESIAN_POINT('Ctrl Pts',(-6.68113978100005,15.2,-8.22152214800001));
#285735=CARTESIAN_POINT('Ctrl Pts',(-6.68206651900006,15.2,-8.22338745000001));
#285736=CARTESIAN_POINT('Ctrl Pts',(-6.68299464500006,15.2,-8.22525974700002));
#285737=CARTESIAN_POINT('Ctrl Pts',(-6.68392414200006,15.2,-8.22713903600001));
#285738=CARTESIAN_POINT('Ctrl Pts',(-6.68485499200006,15.2,-8.22902530700001));
#285739=CARTESIAN_POINT('Ctrl Pts',(-6.68578718200005,15.2,-8.23091855000002));
#285740=CARTESIAN_POINT('Ctrl Pts',(-6.68672069300006,15.2,-8.23281875900001));
#285741=CARTESIAN_POINT('Ctrl Pts',(-6.68765551100006,15.2,-8.23472592600002));
#285742=CARTESIAN_POINT('Ctrl Pts',(-6.68859161800006,15.2,-8.23664004100002));
#285743=CARTESIAN_POINT('Ctrl Pts',(-6.68952899900006,15.2,-8.23856109700002));
#285744=CARTESIAN_POINT('Ctrl Pts',(-6.69046763700006,15.2,-8.24048908700002));
#285745=CARTESIAN_POINT('Ctrl Pts',(-6.69140751900006,15.2,-8.24242400100001));
#285746=CARTESIAN_POINT('Ctrl Pts',(-6.69234862600006,15.2,-8.24436583300002));
#285747=CARTESIAN_POINT('Ctrl Pts',(-6.69329094300006,15.2,-8.24631457300002));
#285748=CARTESIAN_POINT('Ctrl Pts',(-6.69423445500006,15.2,-8.24827021500001));
#285749=CARTESIAN_POINT('Ctrl Pts',(-6.69517914500006,15.2,-8.25023274900002));
#285750=CARTESIAN_POINT('Ctrl Pts',(-6.69612499800006,15.2,-8.25220216900002));
#285751=CARTESIAN_POINT('Ctrl Pts',(-6.69707199900006,15.2,-8.25417846500001));
#285752=CARTESIAN_POINT('Ctrl Pts',(-6.69802013200006,15.2,-8.25616163100002));
#285753=CARTESIAN_POINT('Ctrl Pts',(-6.69896938100006,15.2,-8.25815165900002));
#285754=CARTESIAN_POINT('Ctrl Pts',(-6.69991973100006,15.2,-8.26014853800002));
#285755=CARTESIAN_POINT('Ctrl Pts',(-6.70087116700006,15.2,-8.26215226500001));
#285756=CARTESIAN_POINT('Ctrl Pts',(-6.70182367300006,15.2,-8.26416282800002));
#285757=CARTESIAN_POINT('Ctrl Pts',(-6.70277723400006,15.2,-8.26618022100002));
#285758=CARTESIAN_POINT('Ctrl Pts',(-6.70373183500006,15.2,-8.26820443600001));
#285759=CARTESIAN_POINT('Ctrl Pts',(-6.70468746000005,15.2,-8.27023546500002));
#285760=CARTESIAN_POINT('Ctrl Pts',(-6.70564409500006,15.2,-8.27227330000002));
#285761=CARTESIAN_POINT('Ctrl Pts',(-6.70660172400006,15.2,-8.27431793400002));
#285762=CARTESIAN_POINT('Ctrl Pts',(-6.70756033200006,15.2,-8.27636935700001));
#285763=CARTESIAN_POINT('Ctrl Pts',(-6.70851990500006,15.2,-8.27842756400001));
#285764=CARTESIAN_POINT('Ctrl Pts',(-6.70948042600005,15.2,-8.28049254600002));
#285765=CARTESIAN_POINT('Ctrl Pts',(-6.71044188300006,15.2,-8.28256429500002));
#285766=CARTESIAN_POINT('Ctrl Pts',(-6.71140426000005,15.2,-8.28464280400001));
#285767=CARTESIAN_POINT('Ctrl Pts',(-6.71236754100006,15.2,-8.28672806400002));
#285768=CARTESIAN_POINT('Ctrl Pts',(-6.71333171300006,15.2,-8.28882006800002));
#285769=CARTESIAN_POINT('Ctrl Pts',(-6.71429675900006,15.2,-8.29091880900001));
#285770=CARTESIAN_POINT('Ctrl Pts',(-6.71526266700006,15.2,-8.29302427800001));
#285771=CARTESIAN_POINT('Ctrl Pts',(-6.71622942200006,15.2,-8.29513646900002));
#285772=CARTESIAN_POINT('Ctrl Pts',(-6.71719700800006,15.2,-8.29725537200002));
#285773=CARTESIAN_POINT('Ctrl Pts',(-6.71816541100006,15.2,-8.29938098200002));
#285774=CARTESIAN_POINT('Ctrl Pts',(-6.71913461600006,15.2,-8.30151328900002));
#285775=CARTESIAN_POINT('Ctrl Pts',(-6.72010461200006,15.2,-8.30365228700002));
#285776=CARTESIAN_POINT('Ctrl Pts',(-6.72107538000006,15.2,-8.30579796800002));
#285777=CARTESIAN_POINT('Ctrl Pts',(-6.72204690900006,15.2,-8.30795032300001));
#285778=CARTESIAN_POINT('Ctrl Pts',(-6.72301918300006,15.2,-8.31010934800002));
#285779=CARTESIAN_POINT('Ctrl Pts',(-6.72399218800006,15.2,-8.31227503100001));
#285780=CARTESIAN_POINT('Ctrl Pts',(-6.72496591100006,15.2,-8.31444736700002));
#285781=CARTESIAN_POINT('Ctrl Pts',(-6.72594033700006,15.2,-8.31662634800002));
#285782=CARTESIAN_POINT('Ctrl Pts',(-6.72691545200006,15.2,-8.31881196600002));
#285783=CARTESIAN_POINT('Ctrl Pts',(-6.72789124200006,15.2,-8.32100421400002));
#285784=CARTESIAN_POINT('Ctrl Pts',(-6.72886769300006,15.2,-8.32320308500002));
#285785=CARTESIAN_POINT('Ctrl Pts',(-6.72984479100006,15.2,-8.32540857000001));
#285786=CARTESIAN_POINT('Ctrl Pts',(-6.73082252300006,15.2,-8.32762066300001));
#285787=CARTESIAN_POINT('Ctrl Pts',(-6.73180087300006,15.2,-8.32983935500001));
#285788=CARTESIAN_POINT('Ctrl Pts',(-6.73277982900006,15.2,-8.33206464000002));
#285789=CARTESIAN_POINT('Ctrl Pts',(-6.73375937800006,15.2,-8.33429650900002));
#285790=CARTESIAN_POINT('Ctrl Pts',(-6.73473950400005,15.2,-8.33653495700002));
#285791=CARTESIAN_POINT('Ctrl Pts',(-6.73572019500006,15.2,-8.33877997400002));
#285792=CARTESIAN_POINT('Ctrl Pts',(-6.73670143700006,15.2,-8.34103155300001));
#285793=CARTESIAN_POINT('Ctrl Pts',(-6.73768321600006,15.2,-8.34328968900002));
#285794=CARTESIAN_POINT('Ctrl Pts',(-6.73866551900006,15.2,-8.34555437100001));
#285795=CARTESIAN_POINT('Ctrl Pts',(-6.73964833200006,15.2,-8.34782559500002));
#285796=CARTESIAN_POINT('Ctrl Pts',(-6.74063164200006,15.2,-8.35010335100002));
#285797=CARTESIAN_POINT('Ctrl Pts',(-6.74161543500006,15.2,-8.35238763300002));
#285798=CARTESIAN_POINT('Ctrl Pts',(-6.74259969900006,15.2,-8.35467843300002));
#285799=CARTESIAN_POINT('Ctrl Pts',(-6.74358442000006,15.2,-8.35697574500001));
#285800=CARTESIAN_POINT('Ctrl Pts',(-6.74456958400006,15.2,-8.35927956000001));
#285801=CARTESIAN_POINT('Ctrl Pts',(-6.74555517700006,15.2,-8.36158987000001));
#285802=CARTESIAN_POINT('Ctrl Pts',(-6.74654118900006,15.2,-8.36390667000002));
#285803=CARTESIAN_POINT('Ctrl Pts',(-6.74752760400006,15.2,-8.36622995200001));
#285804=CARTESIAN_POINT('Ctrl Pts',(-6.74851441000006,15.2,-8.36855970800002));
#285805=CARTESIAN_POINT('Ctrl Pts',(-6.74950159300006,15.2,-8.37089593100002));
#285806=CARTESIAN_POINT('Ctrl Pts',(-6.75048914200006,15.2,-8.37323861500002));
#285807=CARTESIAN_POINT('Ctrl Pts',(-6.75147704200006,15.2,-8.37558775000002));
#285808=CARTESIAN_POINT('Ctrl Pts',(-6.75246528000006,15.2,-8.37794333100002));
#285809=CARTESIAN_POINT('Ctrl Pts',(-6.75345384400006,15.2,-8.38030535000001));
#285810=CARTESIAN_POINT('Ctrl Pts',(-6.75444272200005,15.2,-8.38267380000002));
#285811=CARTESIAN_POINT('Ctrl Pts',(-6.75543189900006,15.2,-8.38504867300001));
#285812=CARTESIAN_POINT('Ctrl Pts',(-6.75642136400006,15.2,-8.38742996300001));
#285813=CARTESIAN_POINT('Ctrl Pts',(-6.75741110400006,15.2,-8.38981766200002));
#285814=CARTESIAN_POINT('Ctrl Pts',(-6.75840110500006,15.2,-8.39221176300001));
#285815=CARTESIAN_POINT('Ctrl Pts',(-6.75939135700006,15.2,-8.39461225900001));
#285816=CARTESIAN_POINT('Ctrl Pts',(-6.76038184400006,15.2,-8.39701914200001));
#285817=CARTESIAN_POINT('Ctrl Pts',(-6.76137255500006,15.2,-8.39943240700002));
#285818=CARTESIAN_POINT('Ctrl Pts',(-6.76236347800006,15.2,-8.40185204500001));
#285819=CARTESIAN_POINT('Ctrl Pts',(-6.76335460000006,15.2,-8.40427804800001));
#285820=CARTESIAN_POINT('Ctrl Pts',(-6.76434590800006,15.2,-8.40671041100002));
#285821=CARTESIAN_POINT('Ctrl Pts',(-6.76533739000006,15.2,-8.40914912700002));
#285822=CARTESIAN_POINT('Ctrl Pts',(-6.76632903400006,15.2,-8.41159418600002));
#285823=CARTESIAN_POINT('Ctrl Pts',(-6.76732082700005,15.2,-8.41404558300002));
#285824=CARTESIAN_POINT('Ctrl Pts',(-6.76831275600006,15.2,-8.41650331100002));
#285825=CARTESIAN_POINT('Ctrl Pts',(-6.76930481100006,15.2,-8.41896736400002));
#285826=CARTESIAN_POINT('Ctrl Pts',(-6.77029697800006,15.2,-8.42143773200002));
#285827=CARTESIAN_POINT('Ctrl Pts',(-6.77128924400006,15.2,-8.42391441000002));
#285828=CARTESIAN_POINT('Ctrl Pts',(-6.77228160000006,15.2,-8.42639739000001));
#285829=CARTESIAN_POINT('Ctrl Pts',(-6.77327403000006,15.2,-8.42888666600001));
#285830=CARTESIAN_POINT('Ctrl Pts',(-6.77426652500006,15.2,-8.43138223000001));
#285831=CARTESIAN_POINT('Ctrl Pts',(-6.77525907000006,15.2,-8.43388407500001));
#285832=CARTESIAN_POINT('Ctrl Pts',(-6.77625165600006,15.2,-8.43639219400002));
#285833=CARTESIAN_POINT('Ctrl Pts',(-6.77724426900006,15.2,-8.43890658100002));
#285834=CARTESIAN_POINT('Ctrl Pts',(-6.77823689800006,15.2,-8.44142722800001));
#285835=CARTESIAN_POINT('Ctrl Pts',(-6.77922953100006,15.2,-8.44395412900001));
#285836=CARTESIAN_POINT('Ctrl Pts',(-6.78022215500006,15.2,-8.44648727600001));
#285837=CARTESIAN_POINT('Ctrl Pts',(-6.78121475800006,15.2,-8.44902666100002));
#285838=CARTESIAN_POINT('Ctrl Pts',(-6.78220733100006,15.2,-8.45157227900001));
#285839=CARTESIAN_POINT('Ctrl Pts',(-6.78319986000006,15.2,-8.45412412300002));
#285840=CARTESIAN_POINT('Ctrl Pts',(-6.78419233200006,15.2,-8.45668218600002));
#285841=CARTESIAN_POINT('Ctrl Pts',(-6.78518473900006,15.2,-8.45924645900002));
#285842=CARTESIAN_POINT('Ctrl Pts',(-6.78617706600006,15.2,-8.46181693800002));
#285843=CARTESIAN_POINT('Ctrl Pts',(-6.78716930300006,15.2,-8.46439361500002));
#285844=CARTESIAN_POINT('Ctrl Pts',(-6.78816143700006,15.2,-8.46697648200001));
#285845=CARTESIAN_POINT('Ctrl Pts',(-6.78915345800006,15.2,-8.46956553300002));
#285846=CARTESIAN_POINT('Ctrl Pts',(-6.79014535300006,15.2,-8.47216076000001));
#285847=CARTESIAN_POINT('Ctrl Pts',(-6.79113711200006,15.2,-8.47476215800001));
#285848=CARTESIAN_POINT('Ctrl Pts',(-6.79212872200006,15.2,-8.47736971900002));
#285849=CARTESIAN_POINT('Ctrl Pts',(-6.79312017300005,15.2,-8.47998343700001));
#285850=CARTESIAN_POINT('Ctrl Pts',(-6.79411145300006,15.2,-8.48260330400001));
#285851=CARTESIAN_POINT('Ctrl Pts',(-6.79510255000006,15.2,-8.48522931400002));
#285852=CARTESIAN_POINT('Ctrl Pts',(-6.79609345300006,15.2,-8.48786145900002));
#285853=CARTESIAN_POINT('Ctrl Pts',(-6.79708415200006,15.2,-8.49049973300002));
#285854=CARTESIAN_POINT('Ctrl Pts',(-6.79807463300006,15.2,-8.49314413000002));
#285855=CARTESIAN_POINT('Ctrl Pts',(-6.79906488700006,15.2,-8.49579464200002));
#285856=CARTESIAN_POINT('Ctrl Pts',(-6.80005490300006,15.2,-8.49845126300002));
#285857=CARTESIAN_POINT('Ctrl Pts',(-6.80104466800006,15.2,-8.50111398400001));
#285858=CARTESIAN_POINT('Ctrl Pts',(-6.80203417100006,15.2,-8.50378280200001));
#285859=CARTESIAN_POINT('Ctrl Pts',(-6.80302340200006,15.2,-8.50645770700002));
#285860=CARTESIAN_POINT('Ctrl Pts',(-6.80401234900006,15.2,-8.50913869300001));
#285861=CARTESIAN_POINT('Ctrl Pts',(-6.80500100400006,15.2,-8.51182575500001));
#285862=CARTESIAN_POINT('Ctrl Pts',(-6.80598935100006,15.2,-8.51451888400002));
#285863=CARTESIAN_POINT('Ctrl Pts',(-6.80697738200006,15.2,-8.51721807500001));
#285864=CARTESIAN_POINT('Ctrl Pts',(-6.80796508500006,15.2,-8.51992331800002));
#285865=CARTESIAN_POINT('Ctrl Pts',(-6.80895244900006,15.2,-8.52263461100002));
#285866=CARTESIAN_POINT('Ctrl Pts',(-6.80993946500006,15.2,-8.52535194300001));
#285867=CARTESIAN_POINT('Ctrl Pts',(-6.81092612100006,15.2,-8.52807531000002));
#285868=CARTESIAN_POINT('Ctrl Pts',(-6.81191240500006,15.2,-8.53080470500002));
#285869=CARTESIAN_POINT('Ctrl Pts',(-6.81289830700006,15.2,-8.53354012000001));
#285870=CARTESIAN_POINT('Ctrl Pts',(-6.81388381700006,15.2,-8.53628154900001));
#285871=CARTESIAN_POINT('Ctrl Pts',(-6.81486892200006,15.2,-8.53902898500002));
#285872=CARTESIAN_POINT('Ctrl Pts',(-6.81585361400006,15.2,-8.54178242200001));
#285873=CARTESIAN_POINT('Ctrl Pts',(-6.81683788100006,15.2,-8.54454185300002));
#285874=CARTESIAN_POINT('Ctrl Pts',(-6.81782171200005,15.2,-8.54730727200002));
#285875=CARTESIAN_POINT('Ctrl Pts',(-6.81880509800005,15.2,-8.55007867000002));
#285876=CARTESIAN_POINT('Ctrl Pts',(-6.81978802600006,15.2,-8.55285604300001));
#285877=CARTESIAN_POINT('Ctrl Pts',(-6.82077048700005,15.2,-8.55563938300002));
#285878=CARTESIAN_POINT('Ctrl Pts',(-6.82175247000006,15.2,-8.55842868400002));
#285879=CARTESIAN_POINT('Ctrl Pts',(-6.82273396500006,15.2,-8.56122393900002));
#285880=CARTESIAN_POINT('Ctrl Pts',(-6.82371496100005,15.2,-8.56402514100001));
#285881=CARTESIAN_POINT('Ctrl Pts',(-6.82469544700006,15.2,-8.56683228400002));
#285882=CARTESIAN_POINT('Ctrl Pts',(-6.82567541400006,15.2,-8.56964536100002));
#285883=CARTESIAN_POINT('Ctrl Pts',(-6.82665485100006,15.2,-8.57246436600001));
#285884=CARTESIAN_POINT('Ctrl Pts',(-6.82763374600006,15.2,-8.57528929200001));
#285885=CARTESIAN_POINT('Ctrl Pts',(-6.82861209100006,15.2,-8.57812013100002));
#285886=CARTESIAN_POINT('Ctrl Pts',(-6.82958987600006,15.2,-8.58095688000001));
#285887=CARTESIAN_POINT('Ctrl Pts',(-6.83056708700006,15.2,-8.58379952900002));
#285888=CARTESIAN_POINT('Ctrl Pts',(-6.83154371800006,15.2,-8.58664807300002));
#285889=CARTESIAN_POINT('Ctrl Pts',(-6.83251975600006,15.2,-8.58950250500002));
#285890=CARTESIAN_POINT('Ctrl Pts',(-6.83349519400006,15.2,-8.59236281800002));
#285891=CARTESIAN_POINT('Ctrl Pts',(-6.83447001700006,15.2,-8.59522900700001));
#285892=CARTESIAN_POINT('Ctrl Pts',(-6.83544421900006,15.2,-8.59810106300002));
#285893=CARTESIAN_POINT('Ctrl Pts',(-6.83641778800006,15.2,-8.60097898100002));
#285894=CARTESIAN_POINT('Ctrl Pts',(-6.83739071400006,15.2,-8.60386275500002));
#285895=CARTESIAN_POINT('Ctrl Pts',(-6.83836298800006,15.2,-8.60675237800002));
#285896=CARTESIAN_POINT('Ctrl Pts',(-6.83933459800006,15.2,-8.60964784300002));
#285897=CARTESIAN_POINT('Ctrl Pts',(-6.84030553600006,15.2,-8.61254914500002));
#285898=CARTESIAN_POINT('Ctrl Pts',(-6.84127579200006,15.2,-8.61545627500002));
#285899=CARTESIAN_POINT('Ctrl Pts',(-6.84224535400006,15.2,-8.61836922800002));
#285900=CARTESIAN_POINT('Ctrl Pts',(-6.84321421300006,15.2,-8.62128799800002));
#285901=CARTESIAN_POINT('Ctrl Pts',(-6.84418236000006,15.2,-8.62421257800002));
#285902=CARTESIAN_POINT('Ctrl Pts',(-6.84514978400006,15.2,-8.62714296000001));
#285903=CARTESIAN_POINT('Ctrl Pts',(-6.84611647700006,15.2,-8.63007914000002));
#285904=CARTESIAN_POINT('Ctrl Pts',(-6.84708242700006,15.2,-8.63302111000002));
#285905=CARTESIAN_POINT('Ctrl Pts',(-6.84804762500006,15.2,-8.63596886400002));
#285906=CARTESIAN_POINT('Ctrl Pts',(-6.84901206200006,15.2,-8.63892239500002));
#285907=CARTESIAN_POINT('Ctrl Pts',(-6.84997572700006,15.2,-8.64188169800002));
#285908=CARTESIAN_POINT('Ctrl Pts',(-6.85093861100006,15.2,-8.64484676500001));
#285909=CARTESIAN_POINT('Ctrl Pts',(-6.85190070400005,15.2,-8.64781759100002));
#285910=CARTESIAN_POINT('Ctrl Pts',(-6.85286199700006,15.2,-8.65079416800001));
#285911=CARTESIAN_POINT('Ctrl Pts',(-6.85382248000006,15.2,-8.65377649100001));
#285912=CARTESIAN_POINT('Ctrl Pts',(-6.85478214300006,15.2,-8.65676455300001));
#285913=CARTESIAN_POINT('Ctrl Pts',(-6.85574097600006,15.2,-8.65975834700001));
#285914=CARTESIAN_POINT('Ctrl Pts',(-6.85669897100006,15.2,-8.66275786700001));
#285915=CARTESIAN_POINT('Ctrl Pts',(-6.85765611700006,15.2,-8.66576310700001));
#285916=CARTESIAN_POINT('Ctrl Pts',(-6.85861240500006,15.2,-8.66877406100001));
#285917=CARTESIAN_POINT('Ctrl Pts',(-6.85956782600006,15.2,-8.67179072200001));
#285918=CARTESIAN_POINT('Ctrl Pts',(-6.86052237000006,15.2,-8.67481308300002));
#285919=CARTESIAN_POINT('Ctrl Pts',(-6.86147602800006,15.2,-8.67784113800001));
#285920=CARTESIAN_POINT('Ctrl Pts',(-6.86242879000006,15.2,-8.68087488200001));
#285921=CARTESIAN_POINT('Ctrl Pts',(-6.86338064600006,15.2,-8.68391430700001));
#285922=CARTESIAN_POINT('Ctrl Pts',(-6.86433158900006,15.2,-8.68695940700002));
#285923=CARTESIAN_POINT('Ctrl Pts',(-6.86528160700006,15.2,-8.69001017600001));
#285924=CARTESIAN_POINT('Ctrl Pts',(-6.86623069200006,15.2,-8.69306660700002));
#285925=CARTESIAN_POINT('Ctrl Pts',(-6.86717883600005,15.2,-8.69612869500001));
#285926=CARTESIAN_POINT('Ctrl Pts',(-6.86812602700006,15.2,-8.69919643300002));
#285927=CARTESIAN_POINT('Ctrl Pts',(-6.86907225800006,15.2,-8.70226981300002));
#285928=CARTESIAN_POINT('Ctrl Pts',(-6.87001751800006,15.2,-8.70534883200002));
#285929=CARTESIAN_POINT('Ctrl Pts',(-6.87096179900006,15.2,-8.70843348100001));
#285930=CARTESIAN_POINT('Ctrl Pts',(-6.87190509000006,15.2,-8.71152375400002));
#285931=CARTESIAN_POINT('Ctrl Pts',(-6.87284738500006,15.2,-8.71461964600002));
#285932=CARTESIAN_POINT('Ctrl Pts',(-6.87378867400006,15.2,-8.71772115000002));
#285933=CARTESIAN_POINT('Ctrl Pts',(-6.87472894500006,15.2,-8.72082826000002));
#285934=CARTESIAN_POINT('Ctrl Pts',(-6.87566819300006,15.2,-8.72394096800001));
#285935=CARTESIAN_POINT('Ctrl Pts',(-6.87660640700006,15.2,-8.72705927100002));
#285936=CARTESIAN_POINT('Ctrl Pts',(-6.87754357700006,15.2,-8.73018316100002));
#285937=CARTESIAN_POINT('Ctrl Pts',(-6.87847969500006,15.2,-8.73331263000001));
#285938=CARTESIAN_POINT('Ctrl Pts',(-6.87941475200006,15.2,-8.73644767400001));
#285939=CARTESIAN_POINT('Ctrl Pts',(-6.88034873900006,15.2,-8.73958828600001));
#285940=CARTESIAN_POINT('Ctrl Pts',(-6.88128164800006,15.2,-8.74273446000002));
#285941=CARTESIAN_POINT('Ctrl Pts',(-6.88221346800006,15.2,-8.74588619000002));
#285942=CARTESIAN_POINT('Ctrl Pts',(-6.88314419200006,15.2,-8.74904347000001));
#285943=CARTESIAN_POINT('Ctrl Pts',(-6.88407381100006,15.2,-8.75220629200001));
#285944=CARTESIAN_POINT('Ctrl Pts',(-6.88500231400006,15.2,-8.75537465100001));
#285945=CARTESIAN_POINT('Ctrl Pts',(-6.88592969500006,15.2,-8.75854854100002));
#285946=CARTESIAN_POINT('Ctrl Pts',(-6.88685594400006,15.2,-8.76172795500001));
#285947=CARTESIAN_POINT('Ctrl Pts',(-6.88778105300006,15.2,-8.76491288800001));
#285948=CARTESIAN_POINT('Ctrl Pts',(-6.88870501100006,15.2,-8.76810333200002));
#285949=CARTESIAN_POINT('Ctrl Pts',(-6.88962781100006,15.2,-8.77129928300001));
#285950=CARTESIAN_POINT('Ctrl Pts',(-6.89054944500006,15.2,-8.77450073400002));
#285951=CARTESIAN_POINT('Ctrl Pts',(-6.89146990300006,15.2,-8.77770767800002));
#285952=CARTESIAN_POINT('Ctrl Pts',(-6.89238917600006,15.2,-8.78092010900002));
#285953=CARTESIAN_POINT('Ctrl Pts',(-6.89330725700006,15.2,-8.78413802100001));
#285954=CARTESIAN_POINT('Ctrl Pts',(-6.89422413500006,15.2,-8.78736140900001));
#285955=CARTESIAN_POINT('Ctrl Pts',(-6.89513980400006,15.2,-8.79059026500002));
#285956=CARTESIAN_POINT('Ctrl Pts',(-6.89605425400006,15.2,-8.79382458400002));
#285957=CARTESIAN_POINT('Ctrl Pts',(-6.89696747600006,15.2,-8.79706435900001));
#285958=CARTESIAN_POINT('Ctrl Pts',(-6.89787946300005,15.2,-8.80030958500001));
#285959=CARTESIAN_POINT('Ctrl Pts',(-6.89879020600006,15.2,-8.80356025400001));
#285960=CARTESIAN_POINT('Ctrl Pts',(-6.89969969600006,15.2,-8.80681636200002));
#285961=CARTESIAN_POINT('Ctrl Pts',(-6.90060792400006,15.2,-8.81007790200002));
#285962=CARTESIAN_POINT('Ctrl Pts',(-6.90151488200006,15.2,-8.81334486800002));
#285963=CARTESIAN_POINT('Ctrl Pts',(-6.90242056300006,15.2,-8.81661725300001));
#285964=CARTESIAN_POINT('Ctrl Pts',(-6.90332495800006,15.2,-8.81989505100002));
#285965=CARTESIAN_POINT('Ctrl Pts',(-6.90422805600006,15.2,-8.82317825800002));
#285966=CARTESIAN_POINT('Ctrl Pts',(-6.90512985200006,15.2,-8.82646686600001));
#285967=CARTESIAN_POINT('Ctrl Pts',(-6.90603033600006,15.2,-8.82976086800002));
#285968=CARTESIAN_POINT('Ctrl Pts',(-6.90692950100006,15.2,-8.83306026000002));
#285969=CARTESIAN_POINT('Ctrl Pts',(-6.90782733600006,15.2,-8.83636503500002));
#285970=CARTESIAN_POINT('Ctrl Pts',(-6.90872383500006,15.2,-8.83967518700001));
#285971=CARTESIAN_POINT('Ctrl Pts',(-6.90961899000006,15.2,-8.84299071000001));
#285972=CARTESIAN_POINT('Ctrl Pts',(-6.91051279100006,15.2,-8.84631159700002));
#285973=CARTESIAN_POINT('Ctrl Pts',(-6.91140523100006,15.2,-8.84963784300002));
#285974=CARTESIAN_POINT('Ctrl Pts',(-6.91229630100006,15.2,-8.85296944200002));
#285975=CARTESIAN_POINT('Ctrl Pts',(-6.91318599400006,15.2,-8.85630638800002));
#285976=CARTESIAN_POINT('Ctrl Pts',(-6.91407430200006,15.2,-8.85964867300002));
#285977=CARTESIAN_POINT('Ctrl Pts',(-6.91496121500006,15.2,-8.86299629400002));
#285978=CARTESIAN_POINT('Ctrl Pts',(-6.91584672600006,15.2,-8.86634924200001));
#285979=CARTESIAN_POINT('Ctrl Pts',(-6.91673082700006,15.2,-8.86970751300002));
#285980=CARTESIAN_POINT('Ctrl Pts',(-6.91761351000006,15.2,-8.87307110000001));
#285981=CARTESIAN_POINT('Ctrl Pts',(-6.91849476600006,15.2,-8.87643999800002));
#285982=CARTESIAN_POINT('Ctrl Pts',(-6.91937458800005,15.2,-8.87981420000001));
#285983=CARTESIAN_POINT('Ctrl Pts',(-6.92025296800006,15.2,-8.88319369900002));
#285984=CARTESIAN_POINT('Ctrl Pts',(-6.92112989800005,15.2,-8.88657849200002));
#285985=CARTESIAN_POINT('Ctrl Pts',(-6.92200536800006,15.2,-8.88996857000001));
#285986=CARTESIAN_POINT('Ctrl Pts',(-6.92287937300006,15.2,-8.89336392900002));
#285987=CARTESIAN_POINT('Ctrl Pts',(-6.92375190400006,15.2,-8.89676456100002));
#285988=CARTESIAN_POINT('Ctrl Pts',(-6.92462295300006,15.2,-8.90017046300001));
#285989=CARTESIAN_POINT('Ctrl Pts',(-6.92549251200006,15.2,-8.90358162500002));
#285990=CARTESIAN_POINT('Ctrl Pts',(-6.92636057200006,15.2,-8.90699804400001));
#285991=CARTESIAN_POINT('Ctrl Pts',(-6.92722712700006,15.2,-8.91041971300002));
#285992=CARTESIAN_POINT('Ctrl Pts',(-6.92809216800006,15.2,-8.91384662700002));
#285993=CARTESIAN_POINT('Ctrl Pts',(-6.92895568900005,15.2,-8.91727877800001));
#285994=CARTESIAN_POINT('Ctrl Pts',(-6.92981767900006,15.2,-8.92071616200001));
#285995=CARTESIAN_POINT('Ctrl Pts',(-6.93067813200006,15.2,-8.92415877200002));
#285996=CARTESIAN_POINT('Ctrl Pts',(-6.93153704100006,15.2,-8.92760660300001));
#285997=CARTESIAN_POINT('Ctrl Pts',(-6.93239439700006,15.2,-8.93105964700002));
#285998=CARTESIAN_POINT('Ctrl Pts',(-6.93325019300006,15.2,-8.93451789900002));
#285999=CARTESIAN_POINT('Ctrl Pts',(-6.93410442200006,15.2,-8.93798135500001));
#286000=CARTESIAN_POINT('Ctrl Pts',(-6.93495707400006,15.2,-8.94145000600002));
#286001=CARTESIAN_POINT('Ctrl Pts',(-6.93580814300006,15.2,-8.94492384900002));
#286002=CARTESIAN_POINT('Ctrl Pts',(-6.93665762200006,15.2,-8.94840287600001));
#286003=CARTESIAN_POINT('Ctrl Pts',(-6.93750550100006,15.2,-8.95188708100001));
#286004=CARTESIAN_POINT('Ctrl Pts',(-6.93835177400006,15.2,-8.95537645900001));
#286005=CARTESIAN_POINT('Ctrl Pts',(-6.93919643300006,15.2,-8.95887100400002));
#286006=CARTESIAN_POINT('Ctrl Pts',(-6.94003947100006,15.2,-8.96237071000002));
#286007=CARTESIAN_POINT('Ctrl Pts',(-6.94088088100006,15.2,-8.96587557000002));
#286008=CARTESIAN_POINT('Ctrl Pts',(-6.94172065300006,15.2,-8.96938558000001));
#286009=CARTESIAN_POINT('Ctrl Pts',(-6.94255878100006,15.2,-8.97290073300002));
#286010=CARTESIAN_POINT('Ctrl Pts',(-6.94339525800006,15.2,-8.97642102300001));
#286011=CARTESIAN_POINT('Ctrl Pts',(-6.94423007700006,15.2,-8.97994644400002));
#286012=CARTESIAN_POINT('Ctrl Pts',(-6.94506322800006,15.2,-8.98347699100002));
#286013=CARTESIAN_POINT('Ctrl Pts',(-6.94589470500006,15.2,-8.98701265600002));
#286014=CARTESIAN_POINT('Ctrl Pts',(-6.94672450200006,15.2,-8.99055343700002));
#286015=CARTESIAN_POINT('Ctrl Pts',(-6.94755260900005,15.2,-8.99409932400001));
#286016=CARTESIAN_POINT('Ctrl Pts',(-6.94837902000006,15.2,-8.99765031300002));
#286017=CARTESIAN_POINT('Ctrl Pts',(-6.94920372700006,15.2,-9.00120639800001));
#286018=CARTESIAN_POINT('Ctrl Pts',(-6.95002672400006,15.2,-9.00476757400002));
#286019=CARTESIAN_POINT('Ctrl Pts',(-6.95084800200005,15.2,-9.00833383300002));
#286020=CARTESIAN_POINT('Ctrl Pts',(-6.95166755500006,15.2,-9.01190517100002));
#286021=CARTESIAN_POINT('Ctrl Pts',(-6.95248537400006,15.2,-9.01548158100002));
#286022=CARTESIAN_POINT('Ctrl Pts',(-6.95330145500006,15.2,-9.01906305900001));
#286023=CARTESIAN_POINT('Ctrl Pts',(-6.95411578700006,15.2,-9.02264959600002));
#286024=CARTESIAN_POINT('Ctrl Pts',(-6.95492836400006,15.2,-9.02624119000001));
#286025=CARTESIAN_POINT('Ctrl Pts',(-6.95573917800006,15.2,-9.02983783100002));
#286026=CARTESIAN_POINT('Ctrl Pts',(-6.95654822400006,15.2,-9.03343951600002));
#286027=CARTESIAN_POINT('Ctrl Pts',(-6.95735549400006,15.2,-9.03704623800002));
#286028=CARTESIAN_POINT('Ctrl Pts',(-6.95816097900006,15.2,-9.04065799200002));
#286029=CARTESIAN_POINT('Ctrl Pts',(-6.95896467400006,15.2,-9.04427477200001));
#286030=CARTESIAN_POINT('Ctrl Pts',(-6.95976657100006,15.2,-9.04789657100002));
#286031=CARTESIAN_POINT('Ctrl Pts',(-6.96056666300006,15.2,-9.05152338500002));
#286032=CARTESIAN_POINT('Ctrl Pts',(-6.96136494300006,15.2,-9.05515520900002));
#286033=CARTESIAN_POINT('Ctrl Pts',(-6.96216140500006,15.2,-9.05879203500002));
#286034=CARTESIAN_POINT('Ctrl Pts',(-6.96295604000006,15.2,-9.06243385600002));
#286035=CARTESIAN_POINT('Ctrl Pts',(-6.96374884000006,15.2,-9.06608066900001));
#286036=CARTESIAN_POINT('Ctrl Pts',(-6.96453980000006,15.2,-9.06973246600002));
#286037=CARTESIAN_POINT('Ctrl Pts',(-6.96532891100006,15.2,-9.07338924200002));
#286038=CARTESIAN_POINT('Ctrl Pts',(-6.96611616800006,15.2,-9.07705099100001));
#286039=CARTESIAN_POINT('Ctrl Pts',(-6.96690156100006,15.2,-9.08071770700002));
#286040=CARTESIAN_POINT('Ctrl Pts',(-6.96768508700006,15.2,-9.08438938500002));
#286041=CARTESIAN_POINT('Ctrl Pts',(-6.96846673800006,15.2,-9.08806602100002));
#286042=CARTESIAN_POINT('Ctrl Pts',(-6.96924650800006,15.2,-9.09174760800001));
#286043=CARTESIAN_POINT('Ctrl Pts',(-6.97002439000006,15.2,-9.09543414100002));
#286044=CARTESIAN_POINT('Ctrl Pts',(-6.97080037900006,15.2,-9.09912561500001));
#286045=CARTESIAN_POINT('Ctrl Pts',(-6.97157446400006,15.2,-9.10282202200002));
#286046=CARTESIAN_POINT('Ctrl Pts',(-6.97234663900006,15.2,-9.10652335600002));
#286047=CARTESIAN_POINT('Ctrl Pts',(-6.97311689200006,15.2,-9.11022960800001));
#286048=CARTESIAN_POINT('Ctrl Pts',(-6.97388521800006,15.2,-9.11394077400002));
#286049=CARTESIAN_POINT('Ctrl Pts',(-6.97465160800006,15.2,-9.11765684500002));
#286050=CARTESIAN_POINT('Ctrl Pts',(-6.97541605700006,15.2,-9.12137781700002));
#286051=CARTESIAN_POINT('Ctrl Pts',(-6.97617855900006,15.2,-9.12510368500002));
#286052=CARTESIAN_POINT('Ctrl Pts',(-6.97693911100006,15.2,-9.12883444900002));
#286053=CARTESIAN_POINT('Ctrl Pts',(-6.97769771300006,15.2,-9.13257010500002));
#286054=CARTESIAN_POINT('Ctrl Pts',(-6.97830303200006,15.2,-9.13556254300002));
#286055=CARTESIAN_POINT('Ctrl Pts',(-6.97875614300006,15.2,-9.13780907300002));
#286056=CARTESIAN_POINT('Ctrl Pts',(-6.97905782800006,15.2,-9.13930773800002));
#286057=CARTESIAN_POINT('Ctrl Pts',(-6.97920857100006,15.2,-9.14005731500002));
#286058=CARTESIAN_POINT('Ctrl Pts',(-6.57080831900006,12.2,-8.02901631800001));
#286059=CARTESIAN_POINT('Ctrl Pts',(-6.57090674100006,12.2,-8.02916024100002));
#286060=CARTESIAN_POINT('Ctrl Pts',(-6.57110695100006,12.2,-8.02945316300002));
#286061=CARTESIAN_POINT('Ctrl Pts',(-6.57141009900006,12.2,-8.02989715700001));
#286062=CARTESIAN_POINT('Ctrl Pts',(-6.57181802000006,12.2,-8.03049556400002));
#286063=CARTESIAN_POINT('Ctrl Pts',(-6.57233322400006,12.2,-8.03125297300002));
#286064=CARTESIAN_POINT('Ctrl Pts',(-6.57285600600006,12.2,-8.03202318500002));
#286065=CARTESIAN_POINT('Ctrl Pts',(-6.57338335000006,12.2,-8.03280179700002));
#286066=CARTESIAN_POINT('Ctrl Pts',(-6.57391522700006,12.2,-8.03358880000001));
#286067=CARTESIAN_POINT('Ctrl Pts',(-6.57445160600005,12.2,-8.03438417800002));
#286068=CARTESIAN_POINT('Ctrl Pts',(-6.57499245700006,12.2,-8.03518792300002));
#286069=CARTESIAN_POINT('Ctrl Pts',(-6.57553775200006,12.2,-8.03600002100002));
#286070=CARTESIAN_POINT('Ctrl Pts',(-6.57608746000006,12.2,-8.03682046000001));
#286071=CARTESIAN_POINT('Ctrl Pts',(-6.57664155100006,12.2,-8.03764922800001));
#286072=CARTESIAN_POINT('Ctrl Pts',(-6.57719999700006,12.2,-8.03848631500001));
#286073=CARTESIAN_POINT('Ctrl Pts',(-6.57776276900006,12.2,-8.03933170500001));
#286074=CARTESIAN_POINT('Ctrl Pts',(-6.57832983700006,12.2,-8.04018539000002));
#286075=CARTESIAN_POINT('Ctrl Pts',(-6.57890117200005,12.2,-8.04104735800001));
#286076=CARTESIAN_POINT('Ctrl Pts',(-6.57947674700006,12.2,-8.04191759500002));
#286077=CARTESIAN_POINT('Ctrl Pts',(-6.58005653200005,12.2,-8.04279609000002));
#286078=CARTESIAN_POINT('Ctrl Pts',(-6.58064050000006,12.2,-8.04368283300001));
#286079=CARTESIAN_POINT('Ctrl Pts',(-6.58122862000006,12.2,-8.04457781100002));
#286080=CARTESIAN_POINT('Ctrl Pts',(-6.58182086700006,12.2,-8.04548101200002));
#286081=CARTESIAN_POINT('Ctrl Pts',(-6.58241721200006,12.2,-8.04639242700001));
#286082=CARTESIAN_POINT('Ctrl Pts',(-6.58301762700006,12.2,-8.04731204200002));
#286083=CARTESIAN_POINT('Ctrl Pts',(-6.58362208300006,12.2,-8.04823984600001));
#286084=CARTESIAN_POINT('Ctrl Pts',(-6.58423055400006,12.2,-8.04917582900002));
#286085=CARTESIAN_POINT('Ctrl Pts',(-6.58484301300006,12.2,-8.05011997800002));
#286086=CARTESIAN_POINT('Ctrl Pts',(-6.58545943100005,12.2,-8.05107228200002));
#286087=CARTESIAN_POINT('Ctrl Pts',(-6.58607978300005,12.2,-8.05203273100001));
#286088=CARTESIAN_POINT('Ctrl Pts',(-6.58670404000006,12.2,-8.05300131300001));
#286089=CARTESIAN_POINT('Ctrl Pts',(-6.58733217600005,12.2,-8.05397801700002));
#286090=CARTESIAN_POINT('Ctrl Pts',(-6.58796416400006,12.2,-8.05496283100002));
#286091=CARTESIAN_POINT('Ctrl Pts',(-6.58859997800006,12.2,-8.05595574500002));
#286092=CARTESIAN_POINT('Ctrl Pts',(-6.58923959000006,12.2,-8.05695674700001));
#286093=CARTESIAN_POINT('Ctrl Pts',(-6.58988297600006,12.2,-8.05796582700001));
#286094=CARTESIAN_POINT('Ctrl Pts',(-6.59053010700006,12.2,-8.05898297300002));
#286095=CARTESIAN_POINT('Ctrl Pts',(-6.59118095900006,12.2,-8.06000817400001));
#286096=CARTESIAN_POINT('Ctrl Pts',(-6.59183550500006,12.2,-8.06104142000001));
#286097=CARTESIAN_POINT('Ctrl Pts',(-6.59249371900006,12.2,-8.06208270100001));
#286098=CARTESIAN_POINT('Ctrl Pts',(-6.59315557600006,12.2,-8.06313200300002));
#286099=CARTESIAN_POINT('Ctrl Pts',(-6.59382104900006,12.2,-8.06418931800001));
#286100=CARTESIAN_POINT('Ctrl Pts',(-6.59449011500006,12.2,-8.06525463500002));
#286101=CARTESIAN_POINT('Ctrl Pts',(-6.59516274600006,12.2,-8.06632794100001));
#286102=CARTESIAN_POINT('Ctrl Pts',(-6.59583891700006,12.2,-8.06740922800002));
#286103=CARTESIAN_POINT('Ctrl Pts',(-6.59651860500006,12.2,-8.06849848300002));
#286104=CARTESIAN_POINT('Ctrl Pts',(-6.59720178300006,12.2,-8.06959569800001));
#286105=CARTESIAN_POINT('Ctrl Pts',(-6.59788842600006,12.2,-8.07070086000002));
#286106=CARTESIAN_POINT('Ctrl Pts',(-6.59857851000006,12.2,-8.07181396000002));
#286107=CARTESIAN_POINT('Ctrl Pts',(-6.59927200900006,12.2,-8.07293498700002));
#286108=CARTESIAN_POINT('Ctrl Pts',(-6.59996890100006,12.2,-8.07406392900001));
#286109=CARTESIAN_POINT('Ctrl Pts',(-6.60066916000006,12.2,-8.07520077800002));
#286110=CARTESIAN_POINT('Ctrl Pts',(-6.60137276000006,12.2,-8.07634552200001));
#286111=CARTESIAN_POINT('Ctrl Pts',(-6.60207968000006,12.2,-8.07749815200001));
#286112=CARTESIAN_POINT('Ctrl Pts',(-6.60278989300005,12.2,-8.07865865600002));
#286113=CARTESIAN_POINT('Ctrl Pts',(-6.60350337600006,12.2,-8.07982702500002));
#286114=CARTESIAN_POINT('Ctrl Pts',(-6.60422010600006,12.2,-8.08100324800002));
#286115=CARTESIAN_POINT('Ctrl Pts',(-6.60494005800006,12.2,-8.08218731500002));
#286116=CARTESIAN_POINT('Ctrl Pts',(-6.60566320900006,12.2,-8.08337921500001));
#286117=CARTESIAN_POINT('Ctrl Pts',(-6.60638953400006,12.2,-8.08457893900002));
#286118=CARTESIAN_POINT('Ctrl Pts',(-6.60711901100006,12.2,-8.08578647500001));
#286119=CARTESIAN_POINT('Ctrl Pts',(-6.60785161500006,12.2,-8.08700181500001));
#286120=CARTESIAN_POINT('Ctrl Pts',(-6.60858732500006,12.2,-8.08822494800001));
#286121=CARTESIAN_POINT('Ctrl Pts',(-6.60932611700006,12.2,-8.08945586400002));
#286122=CARTESIAN_POINT('Ctrl Pts',(-6.61006796600006,12.2,-8.09069455200002));
#286123=CARTESIAN_POINT('Ctrl Pts',(-6.61081285100006,12.2,-8.09194100300001));
#286124=CARTESIAN_POINT('Ctrl Pts',(-6.61156074900005,12.2,-8.09319520700001));
#286125=CARTESIAN_POINT('Ctrl Pts',(-6.61231163600006,12.2,-8.09445715400001));
#286126=CARTESIAN_POINT('Ctrl Pts',(-6.61306549000006,12.2,-8.09572683400001));
#286127=CARTESIAN_POINT('Ctrl Pts',(-6.61382229000006,12.2,-8.09700423600002));
#286128=CARTESIAN_POINT('Ctrl Pts',(-6.61458201100006,12.2,-8.09828935200001));
#286129=CARTESIAN_POINT('Ctrl Pts',(-6.61534463100006,12.2,-8.09958217100002));
#286130=CARTESIAN_POINT('Ctrl Pts',(-6.61611012900006,12.2,-8.10088268300002));
#286131=CARTESIAN_POINT('Ctrl Pts',(-6.61687848200006,12.2,-8.10219087900002));
#286132=CARTESIAN_POINT('Ctrl Pts',(-6.61764966700006,12.2,-8.10350674900001));
#286133=CARTESIAN_POINT('Ctrl Pts',(-6.61842366400006,12.2,-8.10483028300002));
#286134=CARTESIAN_POINT('Ctrl Pts',(-6.61920045000006,12.2,-8.10616147100001));
#286135=CARTESIAN_POINT('Ctrl Pts',(-6.61998000200006,12.2,-8.10750030400002));
#286136=CARTESIAN_POINT('Ctrl Pts',(-6.62076230000006,12.2,-8.10884677100002));
#286137=CARTESIAN_POINT('Ctrl Pts',(-6.62154732100006,12.2,-8.11020086400001));
#286138=CARTESIAN_POINT('Ctrl Pts',(-6.62233504600006,12.2,-8.11156257400001));
#286139=CARTESIAN_POINT('Ctrl Pts',(-6.62312545000006,12.2,-8.11293188900001));
#286140=CARTESIAN_POINT('Ctrl Pts',(-6.62391851400006,12.2,-8.11430880100002));
#286141=CARTESIAN_POINT('Ctrl Pts',(-6.62471421500006,12.2,-8.11569329900001));
#286142=CARTESIAN_POINT('Ctrl Pts',(-6.62551253400006,12.2,-8.11708537600002));
#286143=CARTESIAN_POINT('Ctrl Pts',(-6.62631344800006,12.2,-8.11848502000002));
#286144=CARTESIAN_POINT('Ctrl Pts',(-6.62711693700006,12.2,-8.11989222400002));
#286145=CARTESIAN_POINT('Ctrl Pts',(-6.62792298000006,12.2,-8.12130697600002));
#286146=CARTESIAN_POINT('Ctrl Pts',(-6.62873155500006,12.2,-8.12272926700001));
#286147=CARTESIAN_POINT('Ctrl Pts',(-6.62954264200006,12.2,-8.12415909000002));
#286148=CARTESIAN_POINT('Ctrl Pts',(-6.63035622100006,12.2,-8.12559643400002));
#286149=CARTESIAN_POINT('Ctrl Pts',(-6.63117227000006,12.2,-8.12704128900002));
#286150=CARTESIAN_POINT('Ctrl Pts',(-6.63199077100006,12.2,-8.12849364600002));
#286151=CARTESIAN_POINT('Ctrl Pts',(-6.63281170000006,12.2,-8.12995349700002));
#286152=CARTESIAN_POINT('Ctrl Pts',(-6.63363504000006,12.2,-8.13142083100002));
#286153=CARTESIAN_POINT('Ctrl Pts',(-6.63446076800006,12.2,-8.13289564100002));
#286154=CARTESIAN_POINT('Ctrl Pts',(-6.63528886600006,12.2,-8.13437791500002));
#286155=CARTESIAN_POINT('Ctrl Pts',(-6.63611931200006,12.2,-8.13586764600002));
#286156=CARTESIAN_POINT('Ctrl Pts',(-6.63695208700006,12.2,-8.13736482400002));
#286157=CARTESIAN_POINT('Ctrl Pts',(-6.63778717100006,12.2,-8.13886943900001));
#286158=CARTESIAN_POINT('Ctrl Pts',(-6.63862454400006,12.2,-8.14038148300002));
#286159=CARTESIAN_POINT('Ctrl Pts',(-6.63946418700006,12.2,-8.14190094700002));
#286160=CARTESIAN_POINT('Ctrl Pts',(-6.64030607900005,12.2,-8.14342782100002));
#286161=CARTESIAN_POINT('Ctrl Pts',(-6.64115020100006,12.2,-8.14496209700001));
#286162=CARTESIAN_POINT('Ctrl Pts',(-6.64199653400006,12.2,-8.14650376600002));
#286163=CARTESIAN_POINT('Ctrl Pts',(-6.64284505800006,12.2,-8.14805281700002));
#286164=CARTESIAN_POINT('Ctrl Pts',(-6.64369575300006,12.2,-8.14960924300001));
#286165=CARTESIAN_POINT('Ctrl Pts',(-6.64454859900006,12.2,-8.15117303500001));
#286166=CARTESIAN_POINT('Ctrl Pts',(-6.64540358000006,12.2,-8.15274418300002));
#286167=CARTESIAN_POINT('Ctrl Pts',(-6.64626067400006,12.2,-8.15432267900002));
#286168=CARTESIAN_POINT('Ctrl Pts',(-6.64711986400006,12.2,-8.15590851400002));
#286169=CARTESIAN_POINT('Ctrl Pts',(-6.64798112800006,12.2,-8.15750167800001));
#286170=CARTESIAN_POINT('Ctrl Pts',(-6.64884444900006,12.2,-8.15910216300002));
#286171=CARTESIAN_POINT('Ctrl Pts',(-6.64970980800006,12.2,-8.16070996000001));
#286172=CARTESIAN_POINT('Ctrl Pts',(-6.65057718600006,12.2,-8.16232506100001));
#286173=CARTESIAN_POINT('Ctrl Pts',(-6.65144656600006,12.2,-8.16394745500002));
#286174=CARTESIAN_POINT('Ctrl Pts',(-6.65231792600006,12.2,-8.16557713600002));
#286175=CARTESIAN_POINT('Ctrl Pts',(-6.65319124900006,12.2,-8.16721409300002));
#286176=CARTESIAN_POINT('Ctrl Pts',(-6.65406651700006,12.2,-8.16885831900001));
#286177=CARTESIAN_POINT('Ctrl Pts',(-6.65494371100006,12.2,-8.17050980400002));
#286178=CARTESIAN_POINT('Ctrl Pts',(-6.65582281300006,12.2,-8.17216853900002));
#286179=CARTESIAN_POINT('Ctrl Pts',(-6.65670380500006,12.2,-8.17383451600002));
#286180=CARTESIAN_POINT('Ctrl Pts',(-6.65758666800006,12.2,-8.17550772700002));
#286181=CARTESIAN_POINT('Ctrl Pts',(-6.65847138400006,12.2,-8.17718816300001));
#286182=CARTESIAN_POINT('Ctrl Pts',(-6.65935793500006,12.2,-8.17887581400001));
#286183=CARTESIAN_POINT('Ctrl Pts',(-6.66024630300006,12.2,-8.18057067400002));
#286184=CARTESIAN_POINT('Ctrl Pts',(-6.66113647000006,12.2,-8.18227273100002));
#286185=CARTESIAN_POINT('Ctrl Pts',(-6.66202841900006,12.2,-8.18398198000001));
#286186=CARTESIAN_POINT('Ctrl Pts',(-6.66292212900006,12.2,-8.18569840900001));
#286187=CARTESIAN_POINT('Ctrl Pts',(-6.66381758700005,12.2,-8.18742201300001));
#286188=CARTESIAN_POINT('Ctrl Pts',(-6.66471477200006,12.2,-8.18915278000001));
#286189=CARTESIAN_POINT('Ctrl Pts',(-6.66561366700006,12.2,-8.19089070400001));
#286190=CARTESIAN_POINT('Ctrl Pts',(-6.66651425400006,12.2,-8.19263577600001));
#286191=CARTESIAN_POINT('Ctrl Pts',(-6.66741651800006,12.2,-8.19438798600002));
#286192=CARTESIAN_POINT('Ctrl Pts',(-6.66832043800006,12.2,-8.19614732700002));
#286193=CARTESIAN_POINT('Ctrl Pts',(-6.66922600000006,12.2,-8.19791379200002));
#286194=CARTESIAN_POINT('Ctrl Pts',(-6.67013318300006,12.2,-8.19968736900002));
#286195=CARTESIAN_POINT('Ctrl Pts',(-6.67104197300006,12.2,-8.20146805200002));
#286196=CARTESIAN_POINT('Ctrl Pts',(-6.67195235200006,12.2,-8.20325583300002));
#286197=CARTESIAN_POINT('Ctrl Pts',(-6.67286430200006,12.2,-8.20505070200002));
#286198=CARTESIAN_POINT('Ctrl Pts',(-6.67377780700006,12.2,-8.20685265200002));
#286199=CARTESIAN_POINT('Ctrl Pts',(-6.67469285000006,12.2,-8.20866167300002));
#286200=CARTESIAN_POINT('Ctrl Pts',(-6.67560941300006,12.2,-8.21047775800002));
#286201=CARTESIAN_POINT('Ctrl Pts',(-6.67652747900005,12.2,-8.21230089900002));
#286202=CARTESIAN_POINT('Ctrl Pts',(-6.67744703200006,12.2,-8.21413108800002));
#286203=CARTESIAN_POINT('Ctrl Pts',(-6.67836805600006,12.2,-8.21596831500001));
#286204=CARTESIAN_POINT('Ctrl Pts',(-6.67929053300006,12.2,-8.21781257300002));
#286205=CARTESIAN_POINT('Ctrl Pts',(-6.68021444700006,12.2,-8.21966385300002));
#286206=CARTESIAN_POINT('Ctrl Pts',(-6.68113978100005,12.2,-8.22152214800001));
#286207=CARTESIAN_POINT('Ctrl Pts',(-6.68206651900006,12.2,-8.22338745000001));
#286208=CARTESIAN_POINT('Ctrl Pts',(-6.68299464500006,12.2,-8.22525974700002));
#286209=CARTESIAN_POINT('Ctrl Pts',(-6.68392414200006,12.2,-8.22713903600001));
#286210=CARTESIAN_POINT('Ctrl Pts',(-6.68485499200006,12.2,-8.22902530700001));
#286211=CARTESIAN_POINT('Ctrl Pts',(-6.68578718200005,12.2,-8.23091855000002));
#286212=CARTESIAN_POINT('Ctrl Pts',(-6.68672069300006,12.2,-8.23281875900001));
#286213=CARTESIAN_POINT('Ctrl Pts',(-6.68765551100006,12.2,-8.23472592600002));
#286214=CARTESIAN_POINT('Ctrl Pts',(-6.68859161800006,12.2,-8.23664004100002));
#286215=CARTESIAN_POINT('Ctrl Pts',(-6.68952899900006,12.2,-8.23856109700002));
#286216=CARTESIAN_POINT('Ctrl Pts',(-6.69046763700006,12.2,-8.24048908700002));
#286217=CARTESIAN_POINT('Ctrl Pts',(-6.69140751900006,12.2,-8.24242400100001));
#286218=CARTESIAN_POINT('Ctrl Pts',(-6.69234862600006,12.2,-8.24436583300002));
#286219=CARTESIAN_POINT('Ctrl Pts',(-6.69329094300006,12.2,-8.24631457300002));
#286220=CARTESIAN_POINT('Ctrl Pts',(-6.69423445500006,12.2,-8.24827021500001));
#286221=CARTESIAN_POINT('Ctrl Pts',(-6.69517914500006,12.2,-8.25023274900002));
#286222=CARTESIAN_POINT('Ctrl Pts',(-6.69612499800006,12.2,-8.25220216900002));
#286223=CARTESIAN_POINT('Ctrl Pts',(-6.69707199900006,12.2,-8.25417846500001));
#286224=CARTESIAN_POINT('Ctrl Pts',(-6.69802013200006,12.2,-8.25616163100002));
#286225=CARTESIAN_POINT('Ctrl Pts',(-6.69896938100006,12.2,-8.25815165900002));
#286226=CARTESIAN_POINT('Ctrl Pts',(-6.69991973100006,12.2,-8.26014853800002));
#286227=CARTESIAN_POINT('Ctrl Pts',(-6.70087116700006,12.2,-8.26215226500001));
#286228=CARTESIAN_POINT('Ctrl Pts',(-6.70182367300006,12.2,-8.26416282800002));
#286229=CARTESIAN_POINT('Ctrl Pts',(-6.70277723400006,12.2,-8.26618022100002));
#286230=CARTESIAN_POINT('Ctrl Pts',(-6.70373183500006,12.2,-8.26820443600001));
#286231=CARTESIAN_POINT('Ctrl Pts',(-6.70468746000005,12.2,-8.27023546500002));
#286232=CARTESIAN_POINT('Ctrl Pts',(-6.70564409500006,12.2,-8.27227330000002));
#286233=CARTESIAN_POINT('Ctrl Pts',(-6.70660172400006,12.2,-8.27431793400002));
#286234=CARTESIAN_POINT('Ctrl Pts',(-6.70756033200006,12.2,-8.27636935700001));
#286235=CARTESIAN_POINT('Ctrl Pts',(-6.70851990500006,12.2,-8.27842756400001));
#286236=CARTESIAN_POINT('Ctrl Pts',(-6.70948042600005,12.2,-8.28049254600002));
#286237=CARTESIAN_POINT('Ctrl Pts',(-6.71044188300006,12.2,-8.28256429500002));
#286238=CARTESIAN_POINT('Ctrl Pts',(-6.71140426000005,12.2,-8.28464280400001));
#286239=CARTESIAN_POINT('Ctrl Pts',(-6.71236754100006,12.2,-8.28672806400002));
#286240=CARTESIAN_POINT('Ctrl Pts',(-6.71333171300006,12.2,-8.28882006800002));
#286241=CARTESIAN_POINT('Ctrl Pts',(-6.71429675900006,12.2,-8.29091880900001));
#286242=CARTESIAN_POINT('Ctrl Pts',(-6.71526266700006,12.2,-8.29302427800001));
#286243=CARTESIAN_POINT('Ctrl Pts',(-6.71622942200006,12.2,-8.29513646900002));
#286244=CARTESIAN_POINT('Ctrl Pts',(-6.71719700800006,12.2,-8.29725537200002));
#286245=CARTESIAN_POINT('Ctrl Pts',(-6.71816541100006,12.2,-8.29938098200002));
#286246=CARTESIAN_POINT('Ctrl Pts',(-6.71913461600006,12.2,-8.30151328900002));
#286247=CARTESIAN_POINT('Ctrl Pts',(-6.72010461200006,12.2,-8.30365228700002));
#286248=CARTESIAN_POINT('Ctrl Pts',(-6.72107538000006,12.2,-8.30579796800002));
#286249=CARTESIAN_POINT('Ctrl Pts',(-6.72204690900006,12.2,-8.30795032300001));
#286250=CARTESIAN_POINT('Ctrl Pts',(-6.72301918300006,12.2,-8.31010934800002));
#286251=CARTESIAN_POINT('Ctrl Pts',(-6.72399218800006,12.2,-8.31227503100001));
#286252=CARTESIAN_POINT('Ctrl Pts',(-6.72496591100006,12.2,-8.31444736700002));
#286253=CARTESIAN_POINT('Ctrl Pts',(-6.72594033700006,12.2,-8.31662634800002));
#286254=CARTESIAN_POINT('Ctrl Pts',(-6.72691545200006,12.2,-8.31881196600002));
#286255=CARTESIAN_POINT('Ctrl Pts',(-6.72789124200006,12.2,-8.32100421400002));
#286256=CARTESIAN_POINT('Ctrl Pts',(-6.72886769300006,12.2,-8.32320308500002));
#286257=CARTESIAN_POINT('Ctrl Pts',(-6.72984479100006,12.2,-8.32540857000001));
#286258=CARTESIAN_POINT('Ctrl Pts',(-6.73082252300006,12.2,-8.32762066300001));
#286259=CARTESIAN_POINT('Ctrl Pts',(-6.73180087300006,12.2,-8.32983935500001));
#286260=CARTESIAN_POINT('Ctrl Pts',(-6.73277982900006,12.2,-8.33206464000002));
#286261=CARTESIAN_POINT('Ctrl Pts',(-6.73375937800006,12.2,-8.33429650900002));
#286262=CARTESIAN_POINT('Ctrl Pts',(-6.73473950400005,12.2,-8.33653495700002));
#286263=CARTESIAN_POINT('Ctrl Pts',(-6.73572019500006,12.2,-8.33877997400002));
#286264=CARTESIAN_POINT('Ctrl Pts',(-6.73670143700006,12.2,-8.34103155300001));
#286265=CARTESIAN_POINT('Ctrl Pts',(-6.73768321600006,12.2,-8.34328968900002));
#286266=CARTESIAN_POINT('Ctrl Pts',(-6.73866551900006,12.2,-8.34555437100001));
#286267=CARTESIAN_POINT('Ctrl Pts',(-6.73964833200006,12.2,-8.34782559500002));
#286268=CARTESIAN_POINT('Ctrl Pts',(-6.74063164200006,12.2,-8.35010335100002));
#286269=CARTESIAN_POINT('Ctrl Pts',(-6.74161543500006,12.2,-8.35238763300002));
#286270=CARTESIAN_POINT('Ctrl Pts',(-6.74259969900006,12.2,-8.35467843300002));
#286271=CARTESIAN_POINT('Ctrl Pts',(-6.74358442000006,12.2,-8.35697574500001));
#286272=CARTESIAN_POINT('Ctrl Pts',(-6.74456958400006,12.2,-8.35927956000001));
#286273=CARTESIAN_POINT('Ctrl Pts',(-6.74555517700006,12.2,-8.36158987000001));
#286274=CARTESIAN_POINT('Ctrl Pts',(-6.74654118900006,12.2,-8.36390667000002));
#286275=CARTESIAN_POINT('Ctrl Pts',(-6.74752760400006,12.2,-8.36622995200001));
#286276=CARTESIAN_POINT('Ctrl Pts',(-6.74851441000006,12.2,-8.36855970800002));
#286277=CARTESIAN_POINT('Ctrl Pts',(-6.74950159300006,12.2,-8.37089593100002));
#286278=CARTESIAN_POINT('Ctrl Pts',(-6.75048914200006,12.2,-8.37323861500002));
#286279=CARTESIAN_POINT('Ctrl Pts',(-6.75147704200006,12.2,-8.37558775000002));
#286280=CARTESIAN_POINT('Ctrl Pts',(-6.75246528000006,12.2,-8.37794333100002));
#286281=CARTESIAN_POINT('Ctrl Pts',(-6.75345384400006,12.2,-8.38030535000001));
#286282=CARTESIAN_POINT('Ctrl Pts',(-6.75444272200005,12.2,-8.38267380000002));
#286283=CARTESIAN_POINT('Ctrl Pts',(-6.75543189900006,12.2,-8.38504867300001));
#286284=CARTESIAN_POINT('Ctrl Pts',(-6.75642136400006,12.2,-8.38742996300001));
#286285=CARTESIAN_POINT('Ctrl Pts',(-6.75741110400006,12.2,-8.38981766200002));
#286286=CARTESIAN_POINT('Ctrl Pts',(-6.75840110500006,12.2,-8.39221176300001));
#286287=CARTESIAN_POINT('Ctrl Pts',(-6.75939135700006,12.2,-8.39461225900001));
#286288=CARTESIAN_POINT('Ctrl Pts',(-6.76038184400006,12.2,-8.39701914200001));
#286289=CARTESIAN_POINT('Ctrl Pts',(-6.76137255500006,12.2,-8.39943240700002));
#286290=CARTESIAN_POINT('Ctrl Pts',(-6.76236347800006,12.2,-8.40185204500001));
#286291=CARTESIAN_POINT('Ctrl Pts',(-6.76335460000006,12.2,-8.40427804800001));
#286292=CARTESIAN_POINT('Ctrl Pts',(-6.76434590800006,12.2,-8.40671041100002));
#286293=CARTESIAN_POINT('Ctrl Pts',(-6.76533739000006,12.2,-8.40914912700002));
#286294=CARTESIAN_POINT('Ctrl Pts',(-6.76632903400006,12.2,-8.41159418600002));
#286295=CARTESIAN_POINT('Ctrl Pts',(-6.76732082700005,12.2,-8.41404558300002));
#286296=CARTESIAN_POINT('Ctrl Pts',(-6.76831275600006,12.2,-8.41650331100002));
#286297=CARTESIAN_POINT('Ctrl Pts',(-6.76930481100006,12.2,-8.41896736400002));
#286298=CARTESIAN_POINT('Ctrl Pts',(-6.77029697800006,12.2,-8.42143773200002));
#286299=CARTESIAN_POINT('Ctrl Pts',(-6.77128924400006,12.2,-8.42391441000002));
#286300=CARTESIAN_POINT('Ctrl Pts',(-6.77228160000006,12.2,-8.42639739000001));
#286301=CARTESIAN_POINT('Ctrl Pts',(-6.77327403000006,12.2,-8.42888666600001));
#286302=CARTESIAN_POINT('Ctrl Pts',(-6.77426652500006,12.2,-8.43138223000001));
#286303=CARTESIAN_POINT('Ctrl Pts',(-6.77525907000006,12.2,-8.43388407500001));
#286304=CARTESIAN_POINT('Ctrl Pts',(-6.77625165600006,12.2,-8.43639219400002));
#286305=CARTESIAN_POINT('Ctrl Pts',(-6.77724426900006,12.2,-8.43890658100002));
#286306=CARTESIAN_POINT('Ctrl Pts',(-6.77823689800006,12.2,-8.44142722800001));
#286307=CARTESIAN_POINT('Ctrl Pts',(-6.77922953100006,12.2,-8.44395412900001));
#286308=CARTESIAN_POINT('Ctrl Pts',(-6.78022215500006,12.2,-8.44648727600001));
#286309=CARTESIAN_POINT('Ctrl Pts',(-6.78121475800006,12.2,-8.44902666100002));
#286310=CARTESIAN_POINT('Ctrl Pts',(-6.78220733100006,12.2,-8.45157227900001));
#286311=CARTESIAN_POINT('Ctrl Pts',(-6.78319986000006,12.2,-8.45412412300002));
#286312=CARTESIAN_POINT('Ctrl Pts',(-6.78419233200006,12.2,-8.45668218600002));
#286313=CARTESIAN_POINT('Ctrl Pts',(-6.78518473900006,12.2,-8.45924645900002));
#286314=CARTESIAN_POINT('Ctrl Pts',(-6.78617706600006,12.2,-8.46181693800002));
#286315=CARTESIAN_POINT('Ctrl Pts',(-6.78716930300006,12.2,-8.46439361500002));
#286316=CARTESIAN_POINT('Ctrl Pts',(-6.78816143700006,12.2,-8.46697648200001));
#286317=CARTESIAN_POINT('Ctrl Pts',(-6.78915345800006,12.2,-8.46956553300002));
#286318=CARTESIAN_POINT('Ctrl Pts',(-6.79014535300006,12.2,-8.47216076000001));
#286319=CARTESIAN_POINT('Ctrl Pts',(-6.79113711200006,12.2,-8.47476215800001));
#286320=CARTESIAN_POINT('Ctrl Pts',(-6.79212872200006,12.2,-8.47736971900002));
#286321=CARTESIAN_POINT('Ctrl Pts',(-6.79312017300005,12.2,-8.47998343700001));
#286322=CARTESIAN_POINT('Ctrl Pts',(-6.79411145300006,12.2,-8.48260330400001));
#286323=CARTESIAN_POINT('Ctrl Pts',(-6.79510255000006,12.2,-8.48522931400002));
#286324=CARTESIAN_POINT('Ctrl Pts',(-6.79609345300006,12.2,-8.48786145900002));
#286325=CARTESIAN_POINT('Ctrl Pts',(-6.79708415200006,12.2,-8.49049973300002));
#286326=CARTESIAN_POINT('Ctrl Pts',(-6.79807463300006,12.2,-8.49314413000002));
#286327=CARTESIAN_POINT('Ctrl Pts',(-6.79906488700006,12.2,-8.49579464200002));
#286328=CARTESIAN_POINT('Ctrl Pts',(-6.80005490300006,12.2,-8.49845126300002));
#286329=CARTESIAN_POINT('Ctrl Pts',(-6.80104466800006,12.2,-8.50111398400001));
#286330=CARTESIAN_POINT('Ctrl Pts',(-6.80203417100006,12.2,-8.50378280200001));
#286331=CARTESIAN_POINT('Ctrl Pts',(-6.80302340200006,12.2,-8.50645770700002));
#286332=CARTESIAN_POINT('Ctrl Pts',(-6.80401234900006,12.2,-8.50913869300001));
#286333=CARTESIAN_POINT('Ctrl Pts',(-6.80500100400006,12.2,-8.51182575500001));
#286334=CARTESIAN_POINT('Ctrl Pts',(-6.80598935100006,12.2,-8.51451888400002));
#286335=CARTESIAN_POINT('Ctrl Pts',(-6.80697738200006,12.2,-8.51721807500001));
#286336=CARTESIAN_POINT('Ctrl Pts',(-6.80796508500006,12.2,-8.51992331800002));
#286337=CARTESIAN_POINT('Ctrl Pts',(-6.80895244900006,12.2,-8.52263461100002));
#286338=CARTESIAN_POINT('Ctrl Pts',(-6.80993946500006,12.2,-8.52535194300001));
#286339=CARTESIAN_POINT('Ctrl Pts',(-6.81092612100006,12.2,-8.52807531000002));
#286340=CARTESIAN_POINT('Ctrl Pts',(-6.81191240500006,12.2,-8.53080470500002));
#286341=CARTESIAN_POINT('Ctrl Pts',(-6.81289830700006,12.2,-8.53354012000001));
#286342=CARTESIAN_POINT('Ctrl Pts',(-6.81388381700006,12.2,-8.53628154900001));
#286343=CARTESIAN_POINT('Ctrl Pts',(-6.81486892200006,12.2,-8.53902898500002));
#286344=CARTESIAN_POINT('Ctrl Pts',(-6.81585361400006,12.2,-8.54178242200001));
#286345=CARTESIAN_POINT('Ctrl Pts',(-6.81683788100006,12.2,-8.54454185300002));
#286346=CARTESIAN_POINT('Ctrl Pts',(-6.81782171200005,12.2,-8.54730727200002));
#286347=CARTESIAN_POINT('Ctrl Pts',(-6.81880509800005,12.2,-8.55007867000002));
#286348=CARTESIAN_POINT('Ctrl Pts',(-6.81978802600006,12.2,-8.55285604300001));
#286349=CARTESIAN_POINT('Ctrl Pts',(-6.82077048700005,12.2,-8.55563938300002));
#286350=CARTESIAN_POINT('Ctrl Pts',(-6.82175247000006,12.2,-8.55842868400002));
#286351=CARTESIAN_POINT('Ctrl Pts',(-6.82273396500006,12.2,-8.56122393900002));
#286352=CARTESIAN_POINT('Ctrl Pts',(-6.82371496100005,12.2,-8.56402514100001));
#286353=CARTESIAN_POINT('Ctrl Pts',(-6.82469544700006,12.2,-8.56683228400002));
#286354=CARTESIAN_POINT('Ctrl Pts',(-6.82567541400006,12.2,-8.56964536100002));
#286355=CARTESIAN_POINT('Ctrl Pts',(-6.82665485100006,12.2,-8.57246436600001));
#286356=CARTESIAN_POINT('Ctrl Pts',(-6.82763374600006,12.2,-8.57528929200001));
#286357=CARTESIAN_POINT('Ctrl Pts',(-6.82861209100006,12.2,-8.57812013100002));
#286358=CARTESIAN_POINT('Ctrl Pts',(-6.82958987600006,12.2,-8.58095688000001));
#286359=CARTESIAN_POINT('Ctrl Pts',(-6.83056708700006,12.2,-8.58379952900002));
#286360=CARTESIAN_POINT('Ctrl Pts',(-6.83154371800006,12.2,-8.58664807300002));
#286361=CARTESIAN_POINT('Ctrl Pts',(-6.83251975600006,12.2,-8.58950250500002));
#286362=CARTESIAN_POINT('Ctrl Pts',(-6.83349519400006,12.2,-8.59236281800002));
#286363=CARTESIAN_POINT('Ctrl Pts',(-6.83447001700006,12.2,-8.59522900700001));
#286364=CARTESIAN_POINT('Ctrl Pts',(-6.83544421900006,12.2,-8.59810106300002));
#286365=CARTESIAN_POINT('Ctrl Pts',(-6.83641778800006,12.2,-8.60097898100002));
#286366=CARTESIAN_POINT('Ctrl Pts',(-6.83739071400006,12.2,-8.60386275500002));
#286367=CARTESIAN_POINT('Ctrl Pts',(-6.83836298800006,12.2,-8.60675237800002));
#286368=CARTESIAN_POINT('Ctrl Pts',(-6.83933459800006,12.2,-8.60964784300002));
#286369=CARTESIAN_POINT('Ctrl Pts',(-6.84030553600006,12.2,-8.61254914500002));
#286370=CARTESIAN_POINT('Ctrl Pts',(-6.84127579200006,12.2,-8.61545627500002));
#286371=CARTESIAN_POINT('Ctrl Pts',(-6.84224535400006,12.2,-8.61836922800002));
#286372=CARTESIAN_POINT('Ctrl Pts',(-6.84321421300006,12.2,-8.62128799800002));
#286373=CARTESIAN_POINT('Ctrl Pts',(-6.84418236000006,12.2,-8.62421257800002));
#286374=CARTESIAN_POINT('Ctrl Pts',(-6.84514978400006,12.2,-8.62714296000001));
#286375=CARTESIAN_POINT('Ctrl Pts',(-6.84611647700006,12.2,-8.63007914000002));
#286376=CARTESIAN_POINT('Ctrl Pts',(-6.84708242700006,12.2,-8.63302111000002));
#286377=CARTESIAN_POINT('Ctrl Pts',(-6.84804762500006,12.2,-8.63596886400002));
#286378=CARTESIAN_POINT('Ctrl Pts',(-6.84901206200006,12.2,-8.63892239500002));
#286379=CARTESIAN_POINT('Ctrl Pts',(-6.84997572700006,12.2,-8.64188169800002));
#286380=CARTESIAN_POINT('Ctrl Pts',(-6.85093861100006,12.2,-8.64484676500001));
#286381=CARTESIAN_POINT('Ctrl Pts',(-6.85190070400005,12.2,-8.64781759100002));
#286382=CARTESIAN_POINT('Ctrl Pts',(-6.85286199700006,12.2,-8.65079416800001));
#286383=CARTESIAN_POINT('Ctrl Pts',(-6.85382248000006,12.2,-8.65377649100001));
#286384=CARTESIAN_POINT('Ctrl Pts',(-6.85478214300006,12.2,-8.65676455300001));
#286385=CARTESIAN_POINT('Ctrl Pts',(-6.85574097600006,12.2,-8.65975834700001));
#286386=CARTESIAN_POINT('Ctrl Pts',(-6.85669897100006,12.2,-8.66275786700001));
#286387=CARTESIAN_POINT('Ctrl Pts',(-6.85765611700006,12.2,-8.66576310700001));
#286388=CARTESIAN_POINT('Ctrl Pts',(-6.85861240500006,12.2,-8.66877406100001));
#286389=CARTESIAN_POINT('Ctrl Pts',(-6.85956782600006,12.2,-8.67179072200001));
#286390=CARTESIAN_POINT('Ctrl Pts',(-6.86052237000006,12.2,-8.67481308300002));
#286391=CARTESIAN_POINT('Ctrl Pts',(-6.86147602800006,12.2,-8.67784113800001));
#286392=CARTESIAN_POINT('Ctrl Pts',(-6.86242879000006,12.2,-8.68087488200001));
#286393=CARTESIAN_POINT('Ctrl Pts',(-6.86338064600006,12.2,-8.68391430700001));
#286394=CARTESIAN_POINT('Ctrl Pts',(-6.86433158900006,12.2,-8.68695940700002));
#286395=CARTESIAN_POINT('Ctrl Pts',(-6.86528160700006,12.2,-8.69001017600001));
#286396=CARTESIAN_POINT('Ctrl Pts',(-6.86623069200006,12.2,-8.69306660700002));
#286397=CARTESIAN_POINT('Ctrl Pts',(-6.86717883600005,12.2,-8.69612869500001));
#286398=CARTESIAN_POINT('Ctrl Pts',(-6.86812602700006,12.2,-8.69919643300002));
#286399=CARTESIAN_POINT('Ctrl Pts',(-6.86907225800006,12.2,-8.70226981300002));
#286400=CARTESIAN_POINT('Ctrl Pts',(-6.87001751800006,12.2,-8.70534883200002));
#286401=CARTESIAN_POINT('Ctrl Pts',(-6.87096179900006,12.2,-8.70843348100001));
#286402=CARTESIAN_POINT('Ctrl Pts',(-6.87190509000006,12.2,-8.71152375400002));
#286403=CARTESIAN_POINT('Ctrl Pts',(-6.87284738500006,12.2,-8.71461964600002));
#286404=CARTESIAN_POINT('Ctrl Pts',(-6.87378867400006,12.2,-8.71772115000002));
#286405=CARTESIAN_POINT('Ctrl Pts',(-6.87472894500006,12.2,-8.72082826000002));
#286406=CARTESIAN_POINT('Ctrl Pts',(-6.87566819300006,12.2,-8.72394096800001));
#286407=CARTESIAN_POINT('Ctrl Pts',(-6.87660640700006,12.2,-8.72705927100002));
#286408=CARTESIAN_POINT('Ctrl Pts',(-6.87754357700006,12.2,-8.73018316100002));
#286409=CARTESIAN_POINT('Ctrl Pts',(-6.87847969500006,12.2,-8.73331263000001));
#286410=CARTESIAN_POINT('Ctrl Pts',(-6.87941475200006,12.2,-8.73644767400001));
#286411=CARTESIAN_POINT('Ctrl Pts',(-6.88034873900006,12.2,-8.73958828600001));
#286412=CARTESIAN_POINT('Ctrl Pts',(-6.88128164800006,12.2,-8.74273446000002));
#286413=CARTESIAN_POINT('Ctrl Pts',(-6.88221346800006,12.2,-8.74588619000002));
#286414=CARTESIAN_POINT('Ctrl Pts',(-6.88314419200006,12.2,-8.74904347000001));
#286415=CARTESIAN_POINT('Ctrl Pts',(-6.88407381100006,12.2,-8.75220629200001));
#286416=CARTESIAN_POINT('Ctrl Pts',(-6.88500231400006,12.2,-8.75537465100001));
#286417=CARTESIAN_POINT('Ctrl Pts',(-6.88592969500006,12.2,-8.75854854100002));
#286418=CARTESIAN_POINT('Ctrl Pts',(-6.88685594400006,12.2,-8.76172795500001));
#286419=CARTESIAN_POINT('Ctrl Pts',(-6.88778105300006,12.2,-8.76491288800001));
#286420=CARTESIAN_POINT('Ctrl Pts',(-6.88870501100006,12.2,-8.76810333200002));
#286421=CARTESIAN_POINT('Ctrl Pts',(-6.88962781100006,12.2,-8.77129928300001));
#286422=CARTESIAN_POINT('Ctrl Pts',(-6.89054944500006,12.2,-8.77450073400002));
#286423=CARTESIAN_POINT('Ctrl Pts',(-6.89146990300006,12.2,-8.77770767800002));
#286424=CARTESIAN_POINT('Ctrl Pts',(-6.89238917600006,12.2,-8.78092010900002));
#286425=CARTESIAN_POINT('Ctrl Pts',(-6.89330725700006,12.2,-8.78413802100001));
#286426=CARTESIAN_POINT('Ctrl Pts',(-6.89422413500006,12.2,-8.78736140900001));
#286427=CARTESIAN_POINT('Ctrl Pts',(-6.89513980400006,12.2,-8.79059026500002));
#286428=CARTESIAN_POINT('Ctrl Pts',(-6.89605425400006,12.2,-8.79382458400002));
#286429=CARTESIAN_POINT('Ctrl Pts',(-6.89696747600006,12.2,-8.79706435900001));
#286430=CARTESIAN_POINT('Ctrl Pts',(-6.89787946300005,12.2,-8.80030958500001));
#286431=CARTESIAN_POINT('Ctrl Pts',(-6.89879020600006,12.2,-8.80356025400001));
#286432=CARTESIAN_POINT('Ctrl Pts',(-6.89969969600006,12.2,-8.80681636200002));
#286433=CARTESIAN_POINT('Ctrl Pts',(-6.90060792400006,12.2,-8.81007790200002));
#286434=CARTESIAN_POINT('Ctrl Pts',(-6.90151488200006,12.2,-8.81334486800002));
#286435=CARTESIAN_POINT('Ctrl Pts',(-6.90242056300006,12.2,-8.81661725300001));
#286436=CARTESIAN_POINT('Ctrl Pts',(-6.90332495800006,12.2,-8.81989505100002));
#286437=CARTESIAN_POINT('Ctrl Pts',(-6.90422805600006,12.2,-8.82317825800002));
#286438=CARTESIAN_POINT('Ctrl Pts',(-6.90512985200006,12.2,-8.82646686600001));
#286439=CARTESIAN_POINT('Ctrl Pts',(-6.90603033600006,12.2,-8.82976086800002));
#286440=CARTESIAN_POINT('Ctrl Pts',(-6.90692950100006,12.2,-8.83306026000002));
#286441=CARTESIAN_POINT('Ctrl Pts',(-6.90782733600006,12.2,-8.83636503500002));
#286442=CARTESIAN_POINT('Ctrl Pts',(-6.90872383500006,12.2,-8.83967518700001));
#286443=CARTESIAN_POINT('Ctrl Pts',(-6.90961899000006,12.2,-8.84299071000001));
#286444=CARTESIAN_POINT('Ctrl Pts',(-6.91051279100006,12.2,-8.84631159700002));
#286445=CARTESIAN_POINT('Ctrl Pts',(-6.91140523100006,12.2,-8.84963784300002));
#286446=CARTESIAN_POINT('Ctrl Pts',(-6.91229630100006,12.2,-8.85296944200002));
#286447=CARTESIAN_POINT('Ctrl Pts',(-6.91318599400006,12.2,-8.85630638800002));
#286448=CARTESIAN_POINT('Ctrl Pts',(-6.91407430200006,12.2,-8.85964867300002));
#286449=CARTESIAN_POINT('Ctrl Pts',(-6.91496121500006,12.2,-8.86299629400002));
#286450=CARTESIAN_POINT('Ctrl Pts',(-6.91584672600006,12.2,-8.86634924200001));
#286451=CARTESIAN_POINT('Ctrl Pts',(-6.91673082700006,12.2,-8.86970751300002));
#286452=CARTESIAN_POINT('Ctrl Pts',(-6.91761351000006,12.2,-8.87307110000001));
#286453=CARTESIAN_POINT('Ctrl Pts',(-6.91849476600006,12.2,-8.87643999800002));
#286454=CARTESIAN_POINT('Ctrl Pts',(-6.91937458800005,12.2,-8.87981420000001));
#286455=CARTESIAN_POINT('Ctrl Pts',(-6.92025296800006,12.2,-8.88319369900002));
#286456=CARTESIAN_POINT('Ctrl Pts',(-6.92112989800005,12.2,-8.88657849200002));
#286457=CARTESIAN_POINT('Ctrl Pts',(-6.92200536800006,12.2,-8.88996857000001));
#286458=CARTESIAN_POINT('Ctrl Pts',(-6.92287937300006,12.2,-8.89336392900002));
#286459=CARTESIAN_POINT('Ctrl Pts',(-6.92375190400006,12.2,-8.89676456100002));
#286460=CARTESIAN_POINT('Ctrl Pts',(-6.92462295300006,12.2,-8.90017046300001));
#286461=CARTESIAN_POINT('Ctrl Pts',(-6.92549251200006,12.2,-8.90358162500002));
#286462=CARTESIAN_POINT('Ctrl Pts',(-6.92636057200006,12.2,-8.90699804400001));
#286463=CARTESIAN_POINT('Ctrl Pts',(-6.92722712700006,12.2,-8.91041971300002));
#286464=CARTESIAN_POINT('Ctrl Pts',(-6.92809216800006,12.2,-8.91384662700002));
#286465=CARTESIAN_POINT('Ctrl Pts',(-6.92895568900005,12.2,-8.91727877800001));
#286466=CARTESIAN_POINT('Ctrl Pts',(-6.92981767900006,12.2,-8.92071616200001));
#286467=CARTESIAN_POINT('Ctrl Pts',(-6.93067813200006,12.2,-8.92415877200002));
#286468=CARTESIAN_POINT('Ctrl Pts',(-6.93153704100006,12.2,-8.92760660300001));
#286469=CARTESIAN_POINT('Ctrl Pts',(-6.93239439700006,12.2,-8.93105964700002));
#286470=CARTESIAN_POINT('Ctrl Pts',(-6.93325019300006,12.2,-8.93451789900002));
#286471=CARTESIAN_POINT('Ctrl Pts',(-6.93410442200006,12.2,-8.93798135500001));
#286472=CARTESIAN_POINT('Ctrl Pts',(-6.93495707400006,12.2,-8.94145000600002));
#286473=CARTESIAN_POINT('Ctrl Pts',(-6.93580814300006,12.2,-8.94492384900002));
#286474=CARTESIAN_POINT('Ctrl Pts',(-6.93665762200006,12.2,-8.94840287600001));
#286475=CARTESIAN_POINT('Ctrl Pts',(-6.93750550100006,12.2,-8.95188708100001));
#286476=CARTESIAN_POINT('Ctrl Pts',(-6.93835177400006,12.2,-8.95537645900001));
#286477=CARTESIAN_POINT('Ctrl Pts',(-6.93919643300006,12.2,-8.95887100400002));
#286478=CARTESIAN_POINT('Ctrl Pts',(-6.94003947100006,12.2,-8.96237071000002));
#286479=CARTESIAN_POINT('Ctrl Pts',(-6.94088088100006,12.2,-8.96587557000002));
#286480=CARTESIAN_POINT('Ctrl Pts',(-6.94172065300006,12.2,-8.96938558000001));
#286481=CARTESIAN_POINT('Ctrl Pts',(-6.94255878100006,12.2,-8.97290073300002));
#286482=CARTESIAN_POINT('Ctrl Pts',(-6.94339525800006,12.2,-8.97642102300001));
#286483=CARTESIAN_POINT('Ctrl Pts',(-6.94423007700006,12.2,-8.97994644400002));
#286484=CARTESIAN_POINT('Ctrl Pts',(-6.94506322800006,12.2,-8.98347699100002));
#286485=CARTESIAN_POINT('Ctrl Pts',(-6.94589470500006,12.2,-8.98701265600002));
#286486=CARTESIAN_POINT('Ctrl Pts',(-6.94672450200006,12.2,-8.99055343700002));
#286487=CARTESIAN_POINT('Ctrl Pts',(-6.94755260900005,12.2,-8.99409932400001));
#286488=CARTESIAN_POINT('Ctrl Pts',(-6.94837902000006,12.2,-8.99765031300002));
#286489=CARTESIAN_POINT('Ctrl Pts',(-6.94920372700006,12.2,-9.00120639800001));
#286490=CARTESIAN_POINT('Ctrl Pts',(-6.95002672400006,12.2,-9.00476757400002));
#286491=CARTESIAN_POINT('Ctrl Pts',(-6.95084800200005,12.2,-9.00833383300002));
#286492=CARTESIAN_POINT('Ctrl Pts',(-6.95166755500006,12.2,-9.01190517100002));
#286493=CARTESIAN_POINT('Ctrl Pts',(-6.95248537400006,12.2,-9.01548158100002));
#286494=CARTESIAN_POINT('Ctrl Pts',(-6.95330145500006,12.2,-9.01906305900001));
#286495=CARTESIAN_POINT('Ctrl Pts',(-6.95411578700006,12.2,-9.02264959600002));
#286496=CARTESIAN_POINT('Ctrl Pts',(-6.95492836400006,12.2,-9.02624119000001));
#286497=CARTESIAN_POINT('Ctrl Pts',(-6.95573917800006,12.2,-9.02983783100002));
#286498=CARTESIAN_POINT('Ctrl Pts',(-6.95654822400006,12.2,-9.03343951600002));
#286499=CARTESIAN_POINT('Ctrl Pts',(-6.95735549400006,12.2,-9.03704623800002));
#286500=CARTESIAN_POINT('Ctrl Pts',(-6.95816097900006,12.2,-9.04065799200002));
#286501=CARTESIAN_POINT('Ctrl Pts',(-6.95896467400006,12.2,-9.04427477200001));
#286502=CARTESIAN_POINT('Ctrl Pts',(-6.95976657100006,12.2,-9.04789657100002));
#286503=CARTESIAN_POINT('Ctrl Pts',(-6.96056666300006,12.2,-9.05152338500002));
#286504=CARTESIAN_POINT('Ctrl Pts',(-6.96136494300006,12.2,-9.05515520900002));
#286505=CARTESIAN_POINT('Ctrl Pts',(-6.96216140500006,12.2,-9.05879203500002));
#286506=CARTESIAN_POINT('Ctrl Pts',(-6.96295604000006,12.2,-9.06243385600002));
#286507=CARTESIAN_POINT('Ctrl Pts',(-6.96374884000006,12.2,-9.06608066900001));
#286508=CARTESIAN_POINT('Ctrl Pts',(-6.96453980000006,12.2,-9.06973246600002));
#286509=CARTESIAN_POINT('Ctrl Pts',(-6.96532891100006,12.2,-9.07338924200002));
#286510=CARTESIAN_POINT('Ctrl Pts',(-6.96611616800006,12.2,-9.07705099100001));
#286511=CARTESIAN_POINT('Ctrl Pts',(-6.96690156100006,12.2,-9.08071770700002));
#286512=CARTESIAN_POINT('Ctrl Pts',(-6.96768508700006,12.2,-9.08438938500002));
#286513=CARTESIAN_POINT('Ctrl Pts',(-6.96846673800006,12.2,-9.08806602100002));
#286514=CARTESIAN_POINT('Ctrl Pts',(-6.96924650800006,12.2,-9.09174760800001));
#286515=CARTESIAN_POINT('Ctrl Pts',(-6.97002439000006,12.2,-9.09543414100002));
#286516=CARTESIAN_POINT('Ctrl Pts',(-6.97080037900006,12.2,-9.09912561500001));
#286517=CARTESIAN_POINT('Ctrl Pts',(-6.97157446400006,12.2,-9.10282202200002));
#286518=CARTESIAN_POINT('Ctrl Pts',(-6.97234663900006,12.2,-9.10652335600002));
#286519=CARTESIAN_POINT('Ctrl Pts',(-6.97311689200006,12.2,-9.11022960800001));
#286520=CARTESIAN_POINT('Ctrl Pts',(-6.97388521800006,12.2,-9.11394077400002));
#286521=CARTESIAN_POINT('Ctrl Pts',(-6.97465160800006,12.2,-9.11765684500002));
#286522=CARTESIAN_POINT('Ctrl Pts',(-6.97541605700006,12.2,-9.12137781700002));
#286523=CARTESIAN_POINT('Ctrl Pts',(-6.97617855900006,12.2,-9.12510368500002));
#286524=CARTESIAN_POINT('Ctrl Pts',(-6.97693911100006,12.2,-9.12883444900002));
#286525=CARTESIAN_POINT('Ctrl Pts',(-6.97769771300006,12.2,-9.13257010500002));
#286526=CARTESIAN_POINT('Ctrl Pts',(-6.97830303200006,12.2,-9.13556254300002));
#286527=CARTESIAN_POINT('Ctrl Pts',(-6.97875614300006,12.2,-9.13780907300002));
#286528=CARTESIAN_POINT('Ctrl Pts',(-6.97905782800006,12.2,-9.13930773800002));
#286529=CARTESIAN_POINT('Ctrl Pts',(-6.97920857100006,12.2,-9.14005731500002));
#286530=CARTESIAN_POINT('Origin',(-5.66257110645729E-14,15.2,-1.77635683940025E-14));
#286531=CARTESIAN_POINT('',(-5.36127880600006,15.2,-8.88241603200001));
#286532=CARTESIAN_POINT('',(-5.36127880600006,12.2,-8.88241603200001));
#286533=CARTESIAN_POINT('',(-5.36127880600006,15.2,-8.88241603200001));
#286534=CARTESIAN_POINT('Origin',(-5.66257110645729E-14,12.2,-1.77635683940025E-14));
#286535=CARTESIAN_POINT('Origin',(-5.66257110645729E-14,15.2,-1.77635683940025E-14));
#286536=CARTESIAN_POINT('Origin',(-5.66257110645729E-14,15.2,-1.77635683940025E-14));
#286537=CARTESIAN_POINT('',(-5.60740451300005,15.2,-10.040269649));
#286538=CARTESIAN_POINT('',(-5.26939701900006,15.2,-10.221714878));
#286539=CARTESIAN_POINT('Origin',(-5.66257110645729E-14,15.2,-1.77635683940025E-14));
#286540=CARTESIAN_POINT('',(-5.26939701900006,12.2,-10.221714878));
#286541=CARTESIAN_POINT('',(-5.26939701900006,15.2,-10.221714878));
#286542=CARTESIAN_POINT('',(-5.60740451300005,12.2,-10.040269649));
#286543=CARTESIAN_POINT('Origin',(-5.66257110645729E-14,12.2,-1.77635683940025E-14));
#286544=CARTESIAN_POINT('',(-5.60740451300005,15.2,-10.040269649));
#286545=CARTESIAN_POINT('Ctrl Pts',(-5.36127880600006,15.2,-8.88241603200001));
#286546=CARTESIAN_POINT('Ctrl Pts',(-5.36127880600006,11.6,-8.88241603200001));
#286547=CARTESIAN_POINT('Ctrl Pts',(-5.36135574300006,15.2,-8.88257249700001));
#286548=CARTESIAN_POINT('Ctrl Pts',(-5.36135574300006,11.6,-8.88257249700001));
#286549=CARTESIAN_POINT('Ctrl Pts',(-5.36151222900005,15.2,-8.88289093000001));
#286550=CARTESIAN_POINT('Ctrl Pts',(-5.36151222900005,11.6,-8.88289093000001));
#286551=CARTESIAN_POINT('Ctrl Pts',(-5.36174910500006,15.2,-8.88337354800001));
#286552=CARTESIAN_POINT('Ctrl Pts',(-5.36174910500006,11.6,-8.88337354800001));
#286553=CARTESIAN_POINT('Ctrl Pts',(-5.36206771100006,15.2,-8.88402391700001));
#286554=CARTESIAN_POINT('Ctrl Pts',(-5.36206771100006,11.6,-8.88402391700001));
#286555=CARTESIAN_POINT('Ctrl Pts',(-5.36246988000006,15.2,-8.88484693800002));
#286556=CARTESIAN_POINT('Ctrl Pts',(-5.36246988000006,11.6,-8.88484693800002));
#286557=CARTESIAN_POINT('Ctrl Pts',(-5.36287772900006,15.2,-8.88568371000002));
#286558=CARTESIAN_POINT('Ctrl Pts',(-5.36287772900006,11.6,-8.88568371000002));
#286559=CARTESIAN_POINT('Ctrl Pts',(-5.36328889700005,15.2,-8.88652944600001));
#286560=CARTESIAN_POINT('Ctrl Pts',(-5.36328889700005,11.6,-8.88652944600001));
#286561=CARTESIAN_POINT('Ctrl Pts',(-5.36370335800005,15.2,-8.88738413200001));
#286562=CARTESIAN_POINT('Ctrl Pts',(-5.36370335800005,11.6,-8.88738413200001));
#286563=CARTESIAN_POINT('Ctrl Pts',(-5.36412108300006,15.2,-8.88824775000002));
#286564=CARTESIAN_POINT('Ctrl Pts',(-5.36412108300006,11.6,-8.88824775000002));
#286565=CARTESIAN_POINT('Ctrl Pts',(-5.36454204500005,15.2,-8.88912028400001));
#286566=CARTESIAN_POINT('Ctrl Pts',(-5.36454204500005,11.6,-8.88912028400001));
#286567=CARTESIAN_POINT('Ctrl Pts',(-5.36496621600006,15.2,-8.89000172000001));
#286568=CARTESIAN_POINT('Ctrl Pts',(-5.36496621600006,11.6,-8.89000172000001));
#286569=CARTESIAN_POINT('Ctrl Pts',(-5.36539356700006,15.2,-8.89089203900001));
#286570=CARTESIAN_POINT('Ctrl Pts',(-5.36539356700006,11.6,-8.89089203900001));
#286571=CARTESIAN_POINT('Ctrl Pts',(-5.36582407300005,15.2,-8.89179122800002));
#286572=CARTESIAN_POINT('Ctrl Pts',(-5.36582407300005,11.6,-8.89179122800002));
#286573=CARTESIAN_POINT('Ctrl Pts',(-5.36625770500006,15.2,-8.89269926800001));
#286574=CARTESIAN_POINT('Ctrl Pts',(-5.36625770500006,11.6,-8.89269926800001));
#286575=CARTESIAN_POINT('Ctrl Pts',(-5.36669443700006,15.2,-8.89361614500002));
#286576=CARTESIAN_POINT('Ctrl Pts',(-5.36669443700006,11.6,-8.89361614500002));
#286577=CARTESIAN_POINT('Ctrl Pts',(-5.36713424100006,15.2,-8.89454184300002));
#286578=CARTESIAN_POINT('Ctrl Pts',(-5.36713424100006,11.6,-8.89454184300002));
#286579=CARTESIAN_POINT('Ctrl Pts',(-5.36757709000006,15.2,-8.89547634600002));
#286580=CARTESIAN_POINT('Ctrl Pts',(-5.36757709000006,11.6,-8.89547634600002));
#286581=CARTESIAN_POINT('Ctrl Pts',(-5.36802295900006,15.2,-8.89641963800001));
#286582=CARTESIAN_POINT('Ctrl Pts',(-5.36802295900006,11.6,-8.89641963800001));
#286583=CARTESIAN_POINT('Ctrl Pts',(-5.36847181900006,15.2,-8.89737170400002));
#286584=CARTESIAN_POINT('Ctrl Pts',(-5.36847181900006,11.6,-8.89737170400002));
#286585=CARTESIAN_POINT('Ctrl Pts',(-5.36892364700006,15.2,-8.89833252800001));
#286586=CARTESIAN_POINT('Ctrl Pts',(-5.36892364700006,11.6,-8.89833252800001));
#286587=CARTESIAN_POINT('Ctrl Pts',(-5.36937841200006,15.2,-8.89930209500001));
#286588=CARTESIAN_POINT('Ctrl Pts',(-5.36937841200006,11.6,-8.89930209500001));
#286589=CARTESIAN_POINT('Ctrl Pts',(-5.36983609200006,15.2,-8.90028038900001));
#286590=CARTESIAN_POINT('Ctrl Pts',(-5.36983609200006,11.6,-8.90028038900001));
#286591=CARTESIAN_POINT('Ctrl Pts',(-5.37029665900006,15.2,-8.90126739500002));
#286592=CARTESIAN_POINT('Ctrl Pts',(-5.37029665900006,11.6,-8.90126739500002));
#286593=CARTESIAN_POINT('Ctrl Pts',(-5.37076008700006,15.2,-8.90226309800001));
#286594=CARTESIAN_POINT('Ctrl Pts',(-5.37076008700006,11.6,-8.90226309800001));
#286595=CARTESIAN_POINT('Ctrl Pts',(-5.37122635100006,15.2,-8.90326748100001));
#286596=CARTESIAN_POINT('Ctrl Pts',(-5.37122635100006,11.6,-8.90326748100001));
#286597=CARTESIAN_POINT('Ctrl Pts',(-5.37169542500005,15.2,-8.90428053100001));
#286598=CARTESIAN_POINT('Ctrl Pts',(-5.37169542500005,11.6,-8.90428053100001));
#286599=CARTESIAN_POINT('Ctrl Pts',(-5.37216728300006,15.2,-8.90530223200001));
#286600=CARTESIAN_POINT('Ctrl Pts',(-5.37216728300006,11.6,-8.90530223200001));
#286601=CARTESIAN_POINT('Ctrl Pts',(-5.37264189900006,15.2,-8.90633257000001));
#286602=CARTESIAN_POINT('Ctrl Pts',(-5.37264189900006,11.6,-8.90633257000001));
#286603=CARTESIAN_POINT('Ctrl Pts',(-5.37311925100005,15.2,-8.90737152700002));
#286604=CARTESIAN_POINT('Ctrl Pts',(-5.37311925100005,11.6,-8.90737152700002));
#286605=CARTESIAN_POINT('Ctrl Pts',(-5.37359931100006,15.2,-8.90841909100001));
#286606=CARTESIAN_POINT('Ctrl Pts',(-5.37359931100006,11.6,-8.90841909100001));
#286607=CARTESIAN_POINT('Ctrl Pts',(-5.37408205300006,15.2,-8.90947524700002));
#286608=CARTESIAN_POINT('Ctrl Pts',(-5.37408205300006,11.6,-8.90947524700002));
#286609=CARTESIAN_POINT('Ctrl Pts',(-5.37456745500006,15.2,-8.91053997800002));
#286610=CARTESIAN_POINT('Ctrl Pts',(-5.37456745500006,11.6,-8.91053997800002));
#286611=CARTESIAN_POINT('Ctrl Pts',(-5.37505549100006,15.2,-8.91161327200001));
#286612=CARTESIAN_POINT('Ctrl Pts',(-5.37505549100006,11.6,-8.91161327200001));
#286613=CARTESIAN_POINT('Ctrl Pts',(-5.37554613600006,15.2,-8.91269511100001));
#286614=CARTESIAN_POINT('Ctrl Pts',(-5.37554613600006,11.6,-8.91269511100001));
#286615=CARTESIAN_POINT('Ctrl Pts',(-5.37603936500005,15.2,-8.91378548300001));
#286616=CARTESIAN_POINT('Ctrl Pts',(-5.37603936500005,11.6,-8.91378548300001));
#286617=CARTESIAN_POINT('Ctrl Pts',(-5.37653515500006,15.2,-8.91488437200002));
#286618=CARTESIAN_POINT('Ctrl Pts',(-5.37653515500006,11.6,-8.91488437200002));
#286619=CARTESIAN_POINT('Ctrl Pts',(-5.37703348100006,15.2,-8.91599176500002));
#286620=CARTESIAN_POINT('Ctrl Pts',(-5.37703348100006,11.6,-8.91599176500002));
#286621=CARTESIAN_POINT('Ctrl Pts',(-5.37753431800006,15.2,-8.91710764600001));
#286622=CARTESIAN_POINT('Ctrl Pts',(-5.37753431800006,11.6,-8.91710764600001));
#286623=CARTESIAN_POINT('Ctrl Pts',(-5.37803764200006,15.2,-8.91823200100001));
#286624=CARTESIAN_POINT('Ctrl Pts',(-5.37803764200006,11.6,-8.91823200100001));
#286625=CARTESIAN_POINT('Ctrl Pts',(-5.37854343200006,15.2,-8.91936481500002));
#286626=CARTESIAN_POINT('Ctrl Pts',(-5.37854343200006,11.6,-8.91936481500002));
#286627=CARTESIAN_POINT('Ctrl Pts',(-5.37905166000006,15.2,-8.92050607500002));
#286628=CARTESIAN_POINT('Ctrl Pts',(-5.37905166000006,11.6,-8.92050607500002));
#286629=CARTESIAN_POINT('Ctrl Pts',(-5.37956230500006,15.2,-8.92165576600001));
#286630=CARTESIAN_POINT('Ctrl Pts',(-5.37956230500006,11.6,-8.92165576600001));
#286631=CARTESIAN_POINT('Ctrl Pts',(-5.38007534200006,15.2,-8.92281387300002));
#286632=CARTESIAN_POINT('Ctrl Pts',(-5.38007534200006,11.6,-8.92281387300002));
#286633=CARTESIAN_POINT('Ctrl Pts',(-5.38059074800006,15.2,-8.92398038200002));
#286634=CARTESIAN_POINT('Ctrl Pts',(-5.38059074800006,11.6,-8.92398038200002));
#286635=CARTESIAN_POINT('Ctrl Pts',(-5.38110850100006,15.2,-8.92515528100001));
#286636=CARTESIAN_POINT('Ctrl Pts',(-5.38110850100006,11.6,-8.92515528100001));
#286637=CARTESIAN_POINT('Ctrl Pts',(-5.38162857400006,15.2,-8.92633855400002));
#286638=CARTESIAN_POINT('Ctrl Pts',(-5.38162857400006,11.6,-8.92633855400002));
#286639=CARTESIAN_POINT('Ctrl Pts',(-5.38215094700006,15.2,-8.92753018600001));
#286640=CARTESIAN_POINT('Ctrl Pts',(-5.38215094700006,11.6,-8.92753018600001));
#286641=CARTESIAN_POINT('Ctrl Pts',(-5.38267559700006,15.2,-8.92873016600002));
#286642=CARTESIAN_POINT('Ctrl Pts',(-5.38267559700006,11.6,-8.92873016600002));
#286643=CARTESIAN_POINT('Ctrl Pts',(-5.38320250000006,15.2,-8.92993847700001));
#286644=CARTESIAN_POINT('Ctrl Pts',(-5.38320250000006,11.6,-8.92993847700001));
#286645=CARTESIAN_POINT('Ctrl Pts',(-5.38373163200006,15.2,-8.93115510700002));
#286646=CARTESIAN_POINT('Ctrl Pts',(-5.38373163200006,11.6,-8.93115510700002));
#286647=CARTESIAN_POINT('Ctrl Pts',(-5.38426297200005,15.2,-8.93238004100001));
#286648=CARTESIAN_POINT('Ctrl Pts',(-5.38426297200005,11.6,-8.93238004100001));
#286649=CARTESIAN_POINT('Ctrl Pts',(-5.38479649700006,15.2,-8.93361326700001));
#286650=CARTESIAN_POINT('Ctrl Pts',(-5.38479649700006,11.6,-8.93361326700001));
#286651=CARTESIAN_POINT('Ctrl Pts',(-5.38533218400006,15.2,-8.93485477000001));
#286652=CARTESIAN_POINT('Ctrl Pts',(-5.38533218400006,11.6,-8.93485477000001));
#286653=CARTESIAN_POINT('Ctrl Pts',(-5.38587001200006,15.2,-8.93610453600001));
#286654=CARTESIAN_POINT('Ctrl Pts',(-5.38587001200006,11.6,-8.93610453600001));
#286655=CARTESIAN_POINT('Ctrl Pts',(-5.38640995700006,15.2,-8.93736255200002));
#286656=CARTESIAN_POINT('Ctrl Pts',(-5.38640995700006,11.6,-8.93736255200002));
#286657=CARTESIAN_POINT('Ctrl Pts',(-5.38695199800006,15.2,-8.93862880300002));
#286658=CARTESIAN_POINT('Ctrl Pts',(-5.38695199800006,11.6,-8.93862880300002));
#286659=CARTESIAN_POINT('Ctrl Pts',(-5.38749611100005,15.2,-8.93990327800001));
#286660=CARTESIAN_POINT('Ctrl Pts',(-5.38749611100005,11.6,-8.93990327800001));
#286661=CARTESIAN_POINT('Ctrl Pts',(-5.38804227600005,15.2,-8.94118596000002));
#286662=CARTESIAN_POINT('Ctrl Pts',(-5.38804227600005,11.6,-8.94118596000002));
#286663=CARTESIAN_POINT('Ctrl Pts',(-5.38859046900006,15.2,-8.94247684000002));
#286664=CARTESIAN_POINT('Ctrl Pts',(-5.38859046900006,11.6,-8.94247684000002));
#286665=CARTESIAN_POINT('Ctrl Pts',(-5.38914067100006,15.2,-8.94377590100002));
#286666=CARTESIAN_POINT('Ctrl Pts',(-5.38914067100006,11.6,-8.94377590100002));
#286667=CARTESIAN_POINT('Ctrl Pts',(-5.38969285900006,15.2,-8.94508313100001));
#286668=CARTESIAN_POINT('Ctrl Pts',(-5.38969285900006,11.6,-8.94508313100001));
#286669=CARTESIAN_POINT('Ctrl Pts',(-5.39024701000006,15.2,-8.94639851600001));
#286670=CARTESIAN_POINT('Ctrl Pts',(-5.39024701000006,11.6,-8.94639851600001));
#286671=CARTESIAN_POINT('Ctrl Pts',(-5.39080310300006,15.2,-8.94772204400001));
#286672=CARTESIAN_POINT('Ctrl Pts',(-5.39080310300006,11.6,-8.94772204400001));
#286673=CARTESIAN_POINT('Ctrl Pts',(-5.39136111800006,15.2,-8.94905370100001));
#286674=CARTESIAN_POINT('Ctrl Pts',(-5.39136111800006,11.6,-8.94905370100001));
#286675=CARTESIAN_POINT('Ctrl Pts',(-5.39192103300006,15.2,-8.95039347300001));
#286676=CARTESIAN_POINT('Ctrl Pts',(-5.39192103300006,11.6,-8.95039347300001));
#286677=CARTESIAN_POINT('Ctrl Pts',(-5.39248282700005,15.2,-8.95174134800002));
#286678=CARTESIAN_POINT('Ctrl Pts',(-5.39248282700005,11.6,-8.95174134800002));
#286679=CARTESIAN_POINT('Ctrl Pts',(-5.39304647700006,15.2,-8.95309731200001));
#286680=CARTESIAN_POINT('Ctrl Pts',(-5.39304647700006,11.6,-8.95309731200001));
#286681=CARTESIAN_POINT('Ctrl Pts',(-5.39361196500006,15.2,-8.95446135300002));
#286682=CARTESIAN_POINT('Ctrl Pts',(-5.39361196500006,11.6,-8.95446135300002));
#286683=CARTESIAN_POINT('Ctrl Pts',(-5.39417926700006,15.2,-8.95583345700001));
#286684=CARTESIAN_POINT('Ctrl Pts',(-5.39417926700006,11.6,-8.95583345700001));
#286685=CARTESIAN_POINT('Ctrl Pts',(-5.39474836400006,15.2,-8.95721361200001));
#286686=CARTESIAN_POINT('Ctrl Pts',(-5.39474836400006,11.6,-8.95721361200001));
#286687=CARTESIAN_POINT('Ctrl Pts',(-5.39531923500006,15.2,-8.95860180500001));
#286688=CARTESIAN_POINT('Ctrl Pts',(-5.39531923500006,11.6,-8.95860180500001));
#286689=CARTESIAN_POINT('Ctrl Pts',(-5.39589185800006,15.2,-8.95999802100001));
#286690=CARTESIAN_POINT('Ctrl Pts',(-5.39589185800006,11.6,-8.95999802100001));
#286691=CARTESIAN_POINT('Ctrl Pts',(-5.39646621500006,15.2,-8.96140225000002));
#286692=CARTESIAN_POINT('Ctrl Pts',(-5.39646621500006,11.6,-8.96140225000002));
#286693=CARTESIAN_POINT('Ctrl Pts',(-5.39704228400006,15.2,-8.96281447600002));
#286694=CARTESIAN_POINT('Ctrl Pts',(-5.39704228400006,11.6,-8.96281447600002));
#286695=CARTESIAN_POINT('Ctrl Pts',(-5.39762004300006,15.2,-8.96423469000002));
#286696=CARTESIAN_POINT('Ctrl Pts',(-5.39762004300006,11.6,-8.96423469000002));
#286697=CARTESIAN_POINT('Ctrl Pts',(-5.39819947500006,15.2,-8.96566287700002));
#286698=CARTESIAN_POINT('Ctrl Pts',(-5.39819947500006,11.6,-8.96566287700002));
#286699=CARTESIAN_POINT('Ctrl Pts',(-5.39878055600005,15.2,-8.96709902300002));
#286700=CARTESIAN_POINT('Ctrl Pts',(-5.39878055600005,11.6,-8.96709902300002));
#286701=CARTESIAN_POINT('Ctrl Pts',(-5.39936326900006,15.2,-8.96854312000002));
#286702=CARTESIAN_POINT('Ctrl Pts',(-5.39936326900006,11.6,-8.96854312000002));
#286703=CARTESIAN_POINT('Ctrl Pts',(-5.39994759300006,15.2,-8.96999515000001));
#286704=CARTESIAN_POINT('Ctrl Pts',(-5.39994759300006,11.6,-8.96999515000001));
#286705=CARTESIAN_POINT('Ctrl Pts',(-5.40053350800005,15.2,-8.97145510400001));
#286706=CARTESIAN_POINT('Ctrl Pts',(-5.40053350800005,11.6,-8.97145510400001));
#286707=CARTESIAN_POINT('Ctrl Pts',(-5.40112099300006,15.2,-8.97292296800002));
#286708=CARTESIAN_POINT('Ctrl Pts',(-5.40112099300006,11.6,-8.97292296800002));
#286709=CARTESIAN_POINT('Ctrl Pts',(-5.40171003000006,15.2,-8.97439872800001));
#286710=CARTESIAN_POINT('Ctrl Pts',(-5.40171003000006,11.6,-8.97439872800001));
#286711=CARTESIAN_POINT('Ctrl Pts',(-5.40230059700006,15.2,-8.97588237500001));
#286712=CARTESIAN_POINT('Ctrl Pts',(-5.40230059700006,11.6,-8.97588237500001));
#286713=CARTESIAN_POINT('Ctrl Pts',(-5.40289267700006,15.2,-8.97737389500002));
#286714=CARTESIAN_POINT('Ctrl Pts',(-5.40289267700006,11.6,-8.97737389500002));
#286715=CARTESIAN_POINT('Ctrl Pts',(-5.40348624900005,15.2,-8.97887327500002));
#286716=CARTESIAN_POINT('Ctrl Pts',(-5.40348624900005,11.6,-8.97887327500002));
#286717=CARTESIAN_POINT('Ctrl Pts',(-5.40408129300006,15.2,-8.98038050300002));
#286718=CARTESIAN_POINT('Ctrl Pts',(-5.40408129300006,11.6,-8.98038050300002));
#286719=CARTESIAN_POINT('Ctrl Pts',(-5.40467779100006,15.2,-8.98189556700002));
#286720=CARTESIAN_POINT('Ctrl Pts',(-5.40467779100006,11.6,-8.98189556700002));
#286721=CARTESIAN_POINT('Ctrl Pts',(-5.40527572300006,15.2,-8.98341845500001));
#286722=CARTESIAN_POINT('Ctrl Pts',(-5.40527572300006,11.6,-8.98341845500001));
#286723=CARTESIAN_POINT('Ctrl Pts',(-5.40587507000006,15.2,-8.98494915300001));
#286724=CARTESIAN_POINT('Ctrl Pts',(-5.40587507000006,11.6,-8.98494915300001));
#286725=CARTESIAN_POINT('Ctrl Pts',(-5.40647581300005,15.2,-8.98648765100001));
#286726=CARTESIAN_POINT('Ctrl Pts',(-5.40647581300005,11.6,-8.98648765100001));
#286727=CARTESIAN_POINT('Ctrl Pts',(-5.40707793100006,15.2,-8.98803393600001));
#286728=CARTESIAN_POINT('Ctrl Pts',(-5.40707793100006,11.6,-8.98803393600001));
#286729=CARTESIAN_POINT('Ctrl Pts',(-5.40768140800005,15.2,-8.98958799500001));
#286730=CARTESIAN_POINT('Ctrl Pts',(-5.40768140800005,11.6,-8.98958799500001));
#286731=CARTESIAN_POINT('Ctrl Pts',(-5.40828622400006,15.2,-8.99114981800002));
#286732=CARTESIAN_POINT('Ctrl Pts',(-5.40828622400006,11.6,-8.99114981800002));
#286733=CARTESIAN_POINT('Ctrl Pts',(-5.40889235900006,15.2,-8.99271939000002));
#286734=CARTESIAN_POINT('Ctrl Pts',(-5.40889235900006,11.6,-8.99271939000002));
#286735=CARTESIAN_POINT('Ctrl Pts',(-5.40949979600006,15.2,-8.99429670100002));
#286736=CARTESIAN_POINT('Ctrl Pts',(-5.40949979600006,11.6,-8.99429670100002));
#286737=CARTESIAN_POINT('Ctrl Pts',(-5.41010851400006,15.2,-8.99588173800002));
#286738=CARTESIAN_POINT('Ctrl Pts',(-5.41010851400006,11.6,-8.99588173800002));
#286739=CARTESIAN_POINT('Ctrl Pts',(-5.41071849700006,15.2,-8.99747449100002));
#286740=CARTESIAN_POINT('Ctrl Pts',(-5.41071849700006,11.6,-8.99747449100002));
#286741=CARTESIAN_POINT('Ctrl Pts',(-5.41132972500006,15.2,-8.99907494500002));
#286742=CARTESIAN_POINT('Ctrl Pts',(-5.41132972500006,11.6,-8.99907494500002));
#286743=CARTESIAN_POINT('Ctrl Pts',(-5.41194218100006,15.2,-9.00068309100002));
#286744=CARTESIAN_POINT('Ctrl Pts',(-5.41194218100006,11.6,-9.00068309100002));
#286745=CARTESIAN_POINT('Ctrl Pts',(-5.41255584400006,15.2,-9.00229891600001));
#286746=CARTESIAN_POINT('Ctrl Pts',(-5.41255584400006,11.6,-9.00229891600001));
#286747=CARTESIAN_POINT('Ctrl Pts',(-5.41317069800006,15.2,-9.00392240700001));
#286748=CARTESIAN_POINT('Ctrl Pts',(-5.41317069800006,11.6,-9.00392240700001));
#286749=CARTESIAN_POINT('Ctrl Pts',(-5.41378672400006,15.2,-9.00555355400002));
#286750=CARTESIAN_POINT('Ctrl Pts',(-5.41378672400006,11.6,-9.00555355400002));
#286751=CARTESIAN_POINT('Ctrl Pts',(-5.41440390400005,15.2,-9.00719234400002));
#286752=CARTESIAN_POINT('Ctrl Pts',(-5.41440390400005,11.6,-9.00719234400002));
#286753=CARTESIAN_POINT('Ctrl Pts',(-5.41502222100006,15.2,-9.00883876600002));
#286754=CARTESIAN_POINT('Ctrl Pts',(-5.41502222100006,11.6,-9.00883876600002));
#286755=CARTESIAN_POINT('Ctrl Pts',(-5.41564165400006,15.2,-9.01049280800001));
#286756=CARTESIAN_POINT('Ctrl Pts',(-5.41564165400006,11.6,-9.01049280800001));
#286757=CARTESIAN_POINT('Ctrl Pts',(-5.41626218800006,15.2,-9.01215445900002));
#286758=CARTESIAN_POINT('Ctrl Pts',(-5.41626218800006,11.6,-9.01215445900002));
#286759=CARTESIAN_POINT('Ctrl Pts',(-5.41688380400006,15.2,-9.01382370600002));
#286760=CARTESIAN_POINT('Ctrl Pts',(-5.41688380400006,11.6,-9.01382370600002));
#286761=CARTESIAN_POINT('Ctrl Pts',(-5.41750648400006,15.2,-9.01550053800002));
#286762=CARTESIAN_POINT('Ctrl Pts',(-5.41750648400006,11.6,-9.01550053800002));
#286763=CARTESIAN_POINT('Ctrl Pts',(-5.41813021000006,15.2,-9.01718494400002));
#286764=CARTESIAN_POINT('Ctrl Pts',(-5.41813021000006,11.6,-9.01718494400002));
#286765=CARTESIAN_POINT('Ctrl Pts',(-5.41875496600006,15.2,-9.01887691300002));
#286766=CARTESIAN_POINT('Ctrl Pts',(-5.41875496600006,11.6,-9.01887691300002));
#286767=CARTESIAN_POINT('Ctrl Pts',(-5.41938073300006,15.2,-9.02057643200001));
#286768=CARTESIAN_POINT('Ctrl Pts',(-5.41938073300006,11.6,-9.02057643200001));
#286769=CARTESIAN_POINT('Ctrl Pts',(-5.42000749500006,15.2,-9.02228349000002));
#286770=CARTESIAN_POINT('Ctrl Pts',(-5.42000749500006,11.6,-9.02228349000002));
#286771=CARTESIAN_POINT('Ctrl Pts',(-5.42063523200006,15.2,-9.02399807600002));
#286772=CARTESIAN_POINT('Ctrl Pts',(-5.42063523200006,11.6,-9.02399807600002));
#286773=CARTESIAN_POINT('Ctrl Pts',(-5.42126392900006,15.2,-9.02572017700002));
#286774=CARTESIAN_POINT('Ctrl Pts',(-5.42126392900006,11.6,-9.02572017700002));
#286775=CARTESIAN_POINT('Ctrl Pts',(-5.42189356700006,15.2,-9.02744978400002));
#286776=CARTESIAN_POINT('Ctrl Pts',(-5.42189356700006,11.6,-9.02744978400002));
#286777=CARTESIAN_POINT('Ctrl Pts',(-5.42252413200006,15.2,-9.02918688400002));
#286778=CARTESIAN_POINT('Ctrl Pts',(-5.42252413200006,11.6,-9.02918688400002));
#286779=CARTESIAN_POINT('Ctrl Pts',(-5.42315560300006,15.2,-9.03093146700002));
#286780=CARTESIAN_POINT('Ctrl Pts',(-5.42315560300006,11.6,-9.03093146700002));
#286781=CARTESIAN_POINT('Ctrl Pts',(-5.42378796400006,15.2,-9.03268352000002));
#286782=CARTESIAN_POINT('Ctrl Pts',(-5.42378796400006,11.6,-9.03268352000002));
#286783=CARTESIAN_POINT('Ctrl Pts',(-5.42442119900006,15.2,-9.03444303200001));
#286784=CARTESIAN_POINT('Ctrl Pts',(-5.42442119900006,11.6,-9.03444303200001));
#286785=CARTESIAN_POINT('Ctrl Pts',(-5.42505529100006,15.2,-9.03620999300001));
#286786=CARTESIAN_POINT('Ctrl Pts',(-5.42505529100006,11.6,-9.03620999300001));
#286787=CARTESIAN_POINT('Ctrl Pts',(-5.42569022200006,15.2,-9.03798439200001));
#286788=CARTESIAN_POINT('Ctrl Pts',(-5.42569022200006,11.6,-9.03798439200001));
#286789=CARTESIAN_POINT('Ctrl Pts',(-5.42632597500006,15.2,-9.03976621700001));
#286790=CARTESIAN_POINT('Ctrl Pts',(-5.42632597500006,11.6,-9.03976621700001));
#286791=CARTESIAN_POINT('Ctrl Pts',(-5.42696253600006,15.2,-9.04155545600002));
#286792=CARTESIAN_POINT('Ctrl Pts',(-5.42696253600006,11.6,-9.04155545600002));
#286793=CARTESIAN_POINT('Ctrl Pts',(-5.42759988400006,15.2,-9.04335209900001));
#286794=CARTESIAN_POINT('Ctrl Pts',(-5.42759988400006,11.6,-9.04335209900001));
#286795=CARTESIAN_POINT('Ctrl Pts',(-5.42823800600006,15.2,-9.04515613500001));
#286796=CARTESIAN_POINT('Ctrl Pts',(-5.42823800600006,11.6,-9.04515613500001));
#286797=CARTESIAN_POINT('Ctrl Pts',(-5.42887688500006,15.2,-9.04696755200002));
#286798=CARTESIAN_POINT('Ctrl Pts',(-5.42887688500006,11.6,-9.04696755200002));
#286799=CARTESIAN_POINT('Ctrl Pts',(-5.42951650300005,15.2,-9.04878634000001));
#286800=CARTESIAN_POINT('Ctrl Pts',(-5.42951650300005,11.6,-9.04878634000001));
#286801=CARTESIAN_POINT('Ctrl Pts',(-5.43015684400006,15.2,-9.05061248700001));
#286802=CARTESIAN_POINT('Ctrl Pts',(-5.43015684400006,11.6,-9.05061248700001));
#286803=CARTESIAN_POINT('Ctrl Pts',(-5.43079789200006,15.2,-9.05244598400002));
#286804=CARTESIAN_POINT('Ctrl Pts',(-5.43079789200006,11.6,-9.05244598400002));
#286805=CARTESIAN_POINT('Ctrl Pts',(-5.43143963200006,15.2,-9.05428681700002));
#286806=CARTESIAN_POINT('Ctrl Pts',(-5.43143963200006,11.6,-9.05428681700002));
#286807=CARTESIAN_POINT('Ctrl Pts',(-5.43208204500006,15.2,-9.05613497700001));
#286808=CARTESIAN_POINT('Ctrl Pts',(-5.43208204500006,11.6,-9.05613497700001));
#286809=CARTESIAN_POINT('Ctrl Pts',(-5.43272511700006,15.2,-9.05799045400002));
#286810=CARTESIAN_POINT('Ctrl Pts',(-5.43272511700006,11.6,-9.05799045400002));
#286811=CARTESIAN_POINT('Ctrl Pts',(-5.43336883000006,15.2,-9.05985323500002));
#286812=CARTESIAN_POINT('Ctrl Pts',(-5.43336883000006,11.6,-9.05985323500002));
#286813=CARTESIAN_POINT('Ctrl Pts',(-5.43401316900006,15.2,-9.06172331100001));
#286814=CARTESIAN_POINT('Ctrl Pts',(-5.43401316900006,11.6,-9.06172331100001));
#286815=CARTESIAN_POINT('Ctrl Pts',(-5.43465811900006,15.2,-9.06360066900002));
#286816=CARTESIAN_POINT('Ctrl Pts',(-5.43465811900006,11.6,-9.06360066900002));
#286817=CARTESIAN_POINT('Ctrl Pts',(-5.43530366400006,15.2,-9.06548530000002));
#286818=CARTESIAN_POINT('Ctrl Pts',(-5.43530366400006,11.6,-9.06548530000002));
#286819=CARTESIAN_POINT('Ctrl Pts',(-5.43594978500006,15.2,-9.06737719300001));
#286820=CARTESIAN_POINT('Ctrl Pts',(-5.43594978500006,11.6,-9.06737719300001));
#286821=CARTESIAN_POINT('Ctrl Pts',(-5.43659647000006,15.2,-9.06927633700001));
#286822=CARTESIAN_POINT('Ctrl Pts',(-5.43659647000006,11.6,-9.06927633700001));
#286823=CARTESIAN_POINT('Ctrl Pts',(-5.43724370200006,15.2,-9.07118272100002));
#286824=CARTESIAN_POINT('Ctrl Pts',(-5.43724370200006,11.6,-9.07118272100002));
#286825=CARTESIAN_POINT('Ctrl Pts',(-5.43789146400006,15.2,-9.07309633400001));
#286826=CARTESIAN_POINT('Ctrl Pts',(-5.43789146400006,11.6,-9.07309633400001));
#286827=CARTESIAN_POINT('Ctrl Pts',(-5.43853974200006,15.2,-9.07501716600001));
#286828=CARTESIAN_POINT('Ctrl Pts',(-5.43853974200006,11.6,-9.07501716600001));
#286829=CARTESIAN_POINT('Ctrl Pts',(-5.43918852000006,15.2,-9.07694520700002));
#286830=CARTESIAN_POINT('Ctrl Pts',(-5.43918852000006,11.6,-9.07694520700002));
#286831=CARTESIAN_POINT('Ctrl Pts',(-5.43983778200006,15.2,-9.07888044600002));
#286832=CARTESIAN_POINT('Ctrl Pts',(-5.43983778200006,11.6,-9.07888044600002));
#286833=CARTESIAN_POINT('Ctrl Pts',(-5.44048751200005,15.2,-9.08082287200001));
#286834=CARTESIAN_POINT('Ctrl Pts',(-5.44048751200005,11.6,-9.08082287200001));
#286835=CARTESIAN_POINT('Ctrl Pts',(-5.44113769600005,15.2,-9.08277247400001));
#286836=CARTESIAN_POINT('Ctrl Pts',(-5.44113769600005,11.6,-9.08277247400001));
#286837=CARTESIAN_POINT('Ctrl Pts',(-5.44178831900005,15.2,-9.08472924200002));
#286838=CARTESIAN_POINT('Ctrl Pts',(-5.44178831900005,11.6,-9.08472924200002));
#286839=CARTESIAN_POINT('Ctrl Pts',(-5.44243936400005,15.2,-9.08669316600001));
#286840=CARTESIAN_POINT('Ctrl Pts',(-5.44243936400005,11.6,-9.08669316600001));
#286841=CARTESIAN_POINT('Ctrl Pts',(-5.44309081700006,15.2,-9.08866423400001));
#286842=CARTESIAN_POINT('Ctrl Pts',(-5.44309081700006,11.6,-9.08866423400001));
#286843=CARTESIAN_POINT('Ctrl Pts',(-5.44374266300006,15.2,-9.09064243800002));
#286844=CARTESIAN_POINT('Ctrl Pts',(-5.44374266300006,11.6,-9.09064243800002));
#286845=CARTESIAN_POINT('Ctrl Pts',(-5.44439488400006,15.2,-9.09262776600002));
#286846=CARTESIAN_POINT('Ctrl Pts',(-5.44439488400006,11.6,-9.09262776600002));
#286847=CARTESIAN_POINT('Ctrl Pts',(-5.44504746900006,15.2,-9.09462020700002));
#286848=CARTESIAN_POINT('Ctrl Pts',(-5.44504746900006,11.6,-9.09462020700002));
#286849=CARTESIAN_POINT('Ctrl Pts',(-5.44570040100006,15.2,-9.09661975100001));
#286850=CARTESIAN_POINT('Ctrl Pts',(-5.44570040100006,11.6,-9.09661975100001));
#286851=CARTESIAN_POINT('Ctrl Pts',(-5.44635366500006,15.2,-9.09862638900002));
#286852=CARTESIAN_POINT('Ctrl Pts',(-5.44635366500006,11.6,-9.09862638900002));
#286853=CARTESIAN_POINT('Ctrl Pts',(-5.44700724700006,15.2,-9.10064010900001));
#286854=CARTESIAN_POINT('Ctrl Pts',(-5.44700724700006,11.6,-9.10064010900001));
#286855=CARTESIAN_POINT('Ctrl Pts',(-5.44766113200006,15.2,-9.10266090100002));
#286856=CARTESIAN_POINT('Ctrl Pts',(-5.44766113200006,11.6,-9.10266090100002));
#286857=CARTESIAN_POINT('Ctrl Pts',(-5.44831530400006,15.2,-9.10468875600002));
#286858=CARTESIAN_POINT('Ctrl Pts',(-5.44831530400006,11.6,-9.10468875600002));
#286859=CARTESIAN_POINT('Ctrl Pts',(-5.44896974900006,15.2,-9.10672366200002));
#286860=CARTESIAN_POINT('Ctrl Pts',(-5.44896974900006,11.6,-9.10672366200002));
#286861=CARTESIAN_POINT('Ctrl Pts',(-5.44962445200006,15.2,-9.10876561000002));
#286862=CARTESIAN_POINT('Ctrl Pts',(-5.44962445200006,11.6,-9.10876561000002));
#286863=CARTESIAN_POINT('Ctrl Pts',(-5.45027939900006,15.2,-9.11081458800002));
#286864=CARTESIAN_POINT('Ctrl Pts',(-5.45027939900006,11.6,-9.11081458800002));
#286865=CARTESIAN_POINT('Ctrl Pts',(-5.45093457600006,15.2,-9.11287058900001));
#286866=CARTESIAN_POINT('Ctrl Pts',(-5.45093457600006,11.6,-9.11287058900001));
#286867=CARTESIAN_POINT('Ctrl Pts',(-5.45158996700006,15.2,-9.11493360000001));
#286868=CARTESIAN_POINT('Ctrl Pts',(-5.45158996700006,11.6,-9.11493360000001));
#286869=CARTESIAN_POINT('Ctrl Pts',(-5.45224555800006,15.2,-9.11700361100002));
#286870=CARTESIAN_POINT('Ctrl Pts',(-5.45224555800006,11.6,-9.11700361100002));
#286871=CARTESIAN_POINT('Ctrl Pts',(-5.45290133500006,15.2,-9.11908061300002));
#286872=CARTESIAN_POINT('Ctrl Pts',(-5.45290133500006,11.6,-9.11908061300002));
#286873=CARTESIAN_POINT('Ctrl Pts',(-5.45355728400006,15.2,-9.12116459600002));
#286874=CARTESIAN_POINT('Ctrl Pts',(-5.45355728400006,11.6,-9.12116459600002));
#286875=CARTESIAN_POINT('Ctrl Pts',(-5.45421338900006,15.2,-9.12325554900002));
#286876=CARTESIAN_POINT('Ctrl Pts',(-5.45421338900006,11.6,-9.12325554900002));
#286877=CARTESIAN_POINT('Ctrl Pts',(-5.45486963700006,15.2,-9.12535346200002));
#286878=CARTESIAN_POINT('Ctrl Pts',(-5.45486963700006,11.6,-9.12535346200002));
#286879=CARTESIAN_POINT('Ctrl Pts',(-5.45552601400006,15.2,-9.12745832600002));
#286880=CARTESIAN_POINT('Ctrl Pts',(-5.45552601400006,11.6,-9.12745832600002));
#286881=CARTESIAN_POINT('Ctrl Pts',(-5.45618250500006,15.2,-9.12957013000002));
#286882=CARTESIAN_POINT('Ctrl Pts',(-5.45618250500006,11.6,-9.12957013000002));
#286883=CARTESIAN_POINT('Ctrl Pts',(-5.45683909700006,15.2,-9.13168886400002));
#286884=CARTESIAN_POINT('Ctrl Pts',(-5.45683909700006,11.6,-9.13168886400002));
#286885=CARTESIAN_POINT('Ctrl Pts',(-5.45749577500006,15.2,-9.13381451800002));
#286886=CARTESIAN_POINT('Ctrl Pts',(-5.45749577500006,11.6,-9.13381451800002));
#286887=CARTESIAN_POINT('Ctrl Pts',(-5.45815252500006,15.2,-9.13594708400002));
#286888=CARTESIAN_POINT('Ctrl Pts',(-5.45815252500006,11.6,-9.13594708400002));
#286889=CARTESIAN_POINT('Ctrl Pts',(-5.45880933300006,15.2,-9.13808654900001));
#286890=CARTESIAN_POINT('Ctrl Pts',(-5.45880933300006,11.6,-9.13808654900001));
#286891=CARTESIAN_POINT('Ctrl Pts',(-5.45946618600006,15.2,-9.14023290400002));
#286892=CARTESIAN_POINT('Ctrl Pts',(-5.45946618600006,11.6,-9.14023290400002));
#286893=CARTESIAN_POINT('Ctrl Pts',(-5.46012307000006,15.2,-9.14238614000002));
#286894=CARTESIAN_POINT('Ctrl Pts',(-5.46012307000006,11.6,-9.14238614000002));
#286895=CARTESIAN_POINT('Ctrl Pts',(-5.46077997000006,15.2,-9.14454624700002));
#286896=CARTESIAN_POINT('Ctrl Pts',(-5.46077997000006,11.6,-9.14454624700002));
#286897=CARTESIAN_POINT('Ctrl Pts',(-5.46143687300006,15.2,-9.14671321500002));
#286898=CARTESIAN_POINT('Ctrl Pts',(-5.46143687300006,11.6,-9.14671321500002));
#286899=CARTESIAN_POINT('Ctrl Pts',(-5.46209376500006,15.2,-9.14888703300001));
#286900=CARTESIAN_POINT('Ctrl Pts',(-5.46209376500006,11.6,-9.14888703300001));
#286901=CARTESIAN_POINT('Ctrl Pts',(-5.46275063300006,15.2,-9.15106769300002));
#286902=CARTESIAN_POINT('Ctrl Pts',(-5.46275063300006,11.6,-9.15106769300002));
#286903=CARTESIAN_POINT('Ctrl Pts',(-5.46340746300006,15.2,-9.15325518400002));
#286904=CARTESIAN_POINT('Ctrl Pts',(-5.46340746300006,11.6,-9.15325518400002));
#286905=CARTESIAN_POINT('Ctrl Pts',(-5.46406424000006,15.2,-9.15544949700001));
#286906=CARTESIAN_POINT('Ctrl Pts',(-5.46406424000006,11.6,-9.15544949700001));
#286907=CARTESIAN_POINT('Ctrl Pts',(-5.46472095400006,15.2,-9.15765062100002));
#286908=CARTESIAN_POINT('Ctrl Pts',(-5.46472095400006,11.6,-9.15765062100002));
#286909=CARTESIAN_POINT('Ctrl Pts',(-5.46537758800006,15.2,-9.15985854900002));
#286910=CARTESIAN_POINT('Ctrl Pts',(-5.46537758800006,11.6,-9.15985854900002));
#286911=CARTESIAN_POINT('Ctrl Pts',(-5.46603413000006,15.2,-9.16207326700002));
#286912=CARTESIAN_POINT('Ctrl Pts',(-5.46603413000006,11.6,-9.16207326700002));
#286913=CARTESIAN_POINT('Ctrl Pts',(-5.46669056700006,15.2,-9.16429476900002));
#286914=CARTESIAN_POINT('Ctrl Pts',(-5.46669056700006,11.6,-9.16429476900002));
#286915=CARTESIAN_POINT('Ctrl Pts',(-5.46734688500006,15.2,-9.16652304400002));
#286916=CARTESIAN_POINT('Ctrl Pts',(-5.46734688500006,11.6,-9.16652304400002));
#286917=CARTESIAN_POINT('Ctrl Pts',(-5.46800307000006,15.2,-9.16875808200002));
#286918=CARTESIAN_POINT('Ctrl Pts',(-5.46800307000006,11.6,-9.16875808200002));
#286919=CARTESIAN_POINT('Ctrl Pts',(-5.46865911200006,15.2,-9.17099987400002));
#286920=CARTESIAN_POINT('Ctrl Pts',(-5.46865911200006,11.6,-9.17099987400002));
#286921=CARTESIAN_POINT('Ctrl Pts',(-5.46931499300006,15.2,-9.17324841000001));
#286922=CARTESIAN_POINT('Ctrl Pts',(-5.46931499300006,11.6,-9.17324841000001));
#286923=CARTESIAN_POINT('Ctrl Pts',(-5.46997070400006,15.2,-9.17550368100001));
#286924=CARTESIAN_POINT('Ctrl Pts',(-5.46997070400006,11.6,-9.17550368100001));
#286925=CARTESIAN_POINT('Ctrl Pts',(-5.47062622900006,15.2,-9.17776567700002));
#286926=CARTESIAN_POINT('Ctrl Pts',(-5.47062622900006,11.6,-9.17776567700002));
#286927=CARTESIAN_POINT('Ctrl Pts',(-5.47128155700006,15.2,-9.18003438700002));
#286928=CARTESIAN_POINT('Ctrl Pts',(-5.47128155700006,11.6,-9.18003438700002));
#286929=CARTESIAN_POINT('Ctrl Pts',(-5.47193667400006,15.2,-9.18230980400002));
#286930=CARTESIAN_POINT('Ctrl Pts',(-5.47193667400006,11.6,-9.18230980400002));
#286931=CARTESIAN_POINT('Ctrl Pts',(-5.47259156600005,15.2,-9.18459191700002));
#286932=CARTESIAN_POINT('Ctrl Pts',(-5.47259156600005,11.6,-9.18459191700002));
#286933=CARTESIAN_POINT('Ctrl Pts',(-5.47324622200006,15.2,-9.18688071700002));
#286934=CARTESIAN_POINT('Ctrl Pts',(-5.47324622200006,11.6,-9.18688071700002));
#286935=CARTESIAN_POINT('Ctrl Pts',(-5.47390062900006,15.2,-9.18917619500002));
#286936=CARTESIAN_POINT('Ctrl Pts',(-5.47390062900006,11.6,-9.18917619500002));
#286937=CARTESIAN_POINT('Ctrl Pts',(-5.47455477300006,15.2,-9.19147833900002));
#286938=CARTESIAN_POINT('Ctrl Pts',(-5.47455477300006,11.6,-9.19147833900002));
#286939=CARTESIAN_POINT('Ctrl Pts',(-5.47520864000006,15.2,-9.19378714300001));
#286940=CARTESIAN_POINT('Ctrl Pts',(-5.47520864000006,11.6,-9.19378714300001));
#286941=CARTESIAN_POINT('Ctrl Pts',(-5.47586222100006,15.2,-9.19610259600002));
#286942=CARTESIAN_POINT('Ctrl Pts',(-5.47586222100006,11.6,-9.19610259600002));
#286943=CARTESIAN_POINT('Ctrl Pts',(-5.47651550000006,15.2,-9.19842468800002));
#286944=CARTESIAN_POINT('Ctrl Pts',(-5.47651550000006,11.6,-9.19842468800002));
#286945=CARTESIAN_POINT('Ctrl Pts',(-5.47716846700006,15.2,-9.20075341100001));
#286946=CARTESIAN_POINT('Ctrl Pts',(-5.47716846700006,11.6,-9.20075341100001));
#286947=CARTESIAN_POINT('Ctrl Pts',(-5.47782110600005,15.2,-9.20308875400002));
#286948=CARTESIAN_POINT('Ctrl Pts',(-5.47782110600005,11.6,-9.20308875400002));
#286949=CARTESIAN_POINT('Ctrl Pts',(-5.47847340700006,15.2,-9.20543070800001));
#286950=CARTESIAN_POINT('Ctrl Pts',(-5.47847340700006,11.6,-9.20543070800001));
#286951=CARTESIAN_POINT('Ctrl Pts',(-5.47912535700006,15.2,-9.20777926500002));
#286952=CARTESIAN_POINT('Ctrl Pts',(-5.47912535700006,11.6,-9.20777926500002));
#286953=CARTESIAN_POINT('Ctrl Pts',(-5.47977694300006,15.2,-9.21013441500002));
#286954=CARTESIAN_POINT('Ctrl Pts',(-5.47977694300006,11.6,-9.21013441500002));
#286955=CARTESIAN_POINT('Ctrl Pts',(-5.48042815200006,15.2,-9.21249614700002));
#286956=CARTESIAN_POINT('Ctrl Pts',(-5.48042815200006,11.6,-9.21249614700002));
#286957=CARTESIAN_POINT('Ctrl Pts',(-5.48107897400006,15.2,-9.21486445500001));
#286958=CARTESIAN_POINT('Ctrl Pts',(-5.48107897400006,11.6,-9.21486445500001));
#286959=CARTESIAN_POINT('Ctrl Pts',(-5.48172939300006,15.2,-9.21723932700001));
#286960=CARTESIAN_POINT('Ctrl Pts',(-5.48172939300006,11.6,-9.21723932700001));
#286961=CARTESIAN_POINT('Ctrl Pts',(-5.48237940000006,15.2,-9.21962075500002));
#286962=CARTESIAN_POINT('Ctrl Pts',(-5.48237940000006,11.6,-9.21962075500002));
#286963=CARTESIAN_POINT('Ctrl Pts',(-5.48302898100006,15.2,-9.22200872900002));
#286964=CARTESIAN_POINT('Ctrl Pts',(-5.48302898100006,11.6,-9.22200872900002));
#286965=CARTESIAN_POINT('Ctrl Pts',(-5.48367812400006,15.2,-9.22440324100002));
#286966=CARTESIAN_POINT('Ctrl Pts',(-5.48367812400006,11.6,-9.22440324100002));
#286967=CARTESIAN_POINT('Ctrl Pts',(-5.48432681600006,15.2,-9.22680428100002));
#286968=CARTESIAN_POINT('Ctrl Pts',(-5.48432681600006,11.6,-9.22680428100002));
#286969=CARTESIAN_POINT('Ctrl Pts',(-5.48497504600006,15.2,-9.22921183900002));
#286970=CARTESIAN_POINT('Ctrl Pts',(-5.48497504600006,11.6,-9.22921183900002));
#286971=CARTESIAN_POINT('Ctrl Pts',(-5.48562280200006,15.2,-9.23162590700001));
#286972=CARTESIAN_POINT('Ctrl Pts',(-5.48562280200006,11.6,-9.23162590700001));
#286973=CARTESIAN_POINT('Ctrl Pts',(-5.48627007100006,15.2,-9.23404647600002));
#286974=CARTESIAN_POINT('Ctrl Pts',(-5.48627007100006,11.6,-9.23404647600002));
#286975=CARTESIAN_POINT('Ctrl Pts',(-5.48691684200006,15.2,-9.23647353500002));
#286976=CARTESIAN_POINT('Ctrl Pts',(-5.48691684200006,11.6,-9.23647353500002));
#286977=CARTESIAN_POINT('Ctrl Pts',(-5.48756310200006,15.2,-9.23890707800001));
#286978=CARTESIAN_POINT('Ctrl Pts',(-5.48756310200006,11.6,-9.23890707800001));
#286979=CARTESIAN_POINT('Ctrl Pts',(-5.48820883900006,15.2,-9.24134709400001));
#286980=CARTESIAN_POINT('Ctrl Pts',(-5.48820883900006,11.6,-9.24134709400001));
#286981=CARTESIAN_POINT('Ctrl Pts',(-5.48885404200006,15.2,-9.24379357300002));
#286982=CARTESIAN_POINT('Ctrl Pts',(-5.48885404200006,11.6,-9.24379357300002));
#286983=CARTESIAN_POINT('Ctrl Pts',(-5.48949869800006,15.2,-9.24624650800002));
#286984=CARTESIAN_POINT('Ctrl Pts',(-5.48949869800006,11.6,-9.24624650800002));
#286985=CARTESIAN_POINT('Ctrl Pts',(-5.49014279600006,15.2,-9.24870588900001));
#286986=CARTESIAN_POINT('Ctrl Pts',(-5.49014279600006,11.6,-9.24870588900001));
#286987=CARTESIAN_POINT('Ctrl Pts',(-5.49078632300006,15.2,-9.25117170600002));
#286988=CARTESIAN_POINT('Ctrl Pts',(-5.49078632300006,11.6,-9.25117170600002));
#286989=CARTESIAN_POINT('Ctrl Pts',(-5.49142927000006,15.2,-9.25364395200001));
#286990=CARTESIAN_POINT('Ctrl Pts',(-5.49142927000006,11.6,-9.25364395200001));
#286991=CARTESIAN_POINT('Ctrl Pts',(-5.49207162100006,15.2,-9.25612261600002));
#286992=CARTESIAN_POINT('Ctrl Pts',(-5.49207162100006,11.6,-9.25612261600002));
#286993=CARTESIAN_POINT('Ctrl Pts',(-5.49271336800006,15.2,-9.25860769100002));
#286994=CARTESIAN_POINT('Ctrl Pts',(-5.49271336800006,11.6,-9.25860769100002));
#286995=CARTESIAN_POINT('Ctrl Pts',(-5.49335449800005,15.2,-9.26109916700002));
#286996=CARTESIAN_POINT('Ctrl Pts',(-5.49335449800005,11.6,-9.26109916700002));
#286997=CARTESIAN_POINT('Ctrl Pts',(-5.49399499900006,15.2,-9.26359703400001));
#286998=CARTESIAN_POINT('Ctrl Pts',(-5.49399499900006,11.6,-9.26359703400001));
#286999=CARTESIAN_POINT('Ctrl Pts',(-5.49463485900006,15.2,-9.26610128400002));
#287000=CARTESIAN_POINT('Ctrl Pts',(-5.49463485900006,11.6,-9.26610128400002));
#287001=CARTESIAN_POINT('Ctrl Pts',(-5.49527406800006,15.2,-9.26861190900001));
#287002=CARTESIAN_POINT('Ctrl Pts',(-5.49527406800006,11.6,-9.26861190900001));
#287003=CARTESIAN_POINT('Ctrl Pts',(-5.49591261300006,15.2,-9.27112889800001));
#287004=CARTESIAN_POINT('Ctrl Pts',(-5.49591261300006,11.6,-9.27112889800001));
#287005=CARTESIAN_POINT('Ctrl Pts',(-5.49655048300006,15.2,-9.27365224400001));
#287006=CARTESIAN_POINT('Ctrl Pts',(-5.49655048300006,11.6,-9.27365224400001));
#287007=CARTESIAN_POINT('Ctrl Pts',(-5.49718766700006,15.2,-9.27618193800001));
#287008=CARTESIAN_POINT('Ctrl Pts',(-5.49718766700006,11.6,-9.27618193800001));
#287009=CARTESIAN_POINT('Ctrl Pts',(-5.49782415300006,15.2,-9.27871797000002));
#287010=CARTESIAN_POINT('Ctrl Pts',(-5.49782415300006,11.6,-9.27871797000002));
#287011=CARTESIAN_POINT('Ctrl Pts',(-5.49845993000006,15.2,-9.28126033100002));
#287012=CARTESIAN_POINT('Ctrl Pts',(-5.49845993000006,11.6,-9.28126033100002));
#287013=CARTESIAN_POINT('Ctrl Pts',(-5.49909498700006,15.2,-9.28380901500002));
#287014=CARTESIAN_POINT('Ctrl Pts',(-5.49909498700006,11.6,-9.28380901500002));
#287015=CARTESIAN_POINT('Ctrl Pts',(-5.49972931200006,15.2,-9.28636401000002));
#287016=CARTESIAN_POINT('Ctrl Pts',(-5.49972931200006,11.6,-9.28636401000002));
#287017=CARTESIAN_POINT('Ctrl Pts',(-5.50036289400006,15.2,-9.28892530800002));
#287018=CARTESIAN_POINT('Ctrl Pts',(-5.50036289400006,11.6,-9.28892530800002));
#287019=CARTESIAN_POINT('Ctrl Pts',(-5.50099572200006,15.2,-9.29149290000002));
#287020=CARTESIAN_POINT('Ctrl Pts',(-5.50099572200006,11.6,-9.29149290000002));
#287021=CARTESIAN_POINT('Ctrl Pts',(-5.50162778400006,15.2,-9.29406678000002));
#287022=CARTESIAN_POINT('Ctrl Pts',(-5.50162778400006,11.6,-9.29406678000002));
#287023=CARTESIAN_POINT('Ctrl Pts',(-5.50225906900006,15.2,-9.29664693400002));
#287024=CARTESIAN_POINT('Ctrl Pts',(-5.50225906900006,11.6,-9.29664693400002));
#287025=CARTESIAN_POINT('Ctrl Pts',(-5.50288956700006,15.2,-9.29923335800002));
#287026=CARTESIAN_POINT('Ctrl Pts',(-5.50288956700006,11.6,-9.29923335800002));
#287027=CARTESIAN_POINT('Ctrl Pts',(-5.50351926700006,15.2,-9.30182604100001));
#287028=CARTESIAN_POINT('Ctrl Pts',(-5.50351926700006,11.6,-9.30182604100001));
#287029=CARTESIAN_POINT('Ctrl Pts',(-5.50414815600006,15.2,-9.30442497500002));
#287030=CARTESIAN_POINT('Ctrl Pts',(-5.50414815600006,11.6,-9.30442497500002));
#287031=CARTESIAN_POINT('Ctrl Pts',(-5.50477622400006,15.2,-9.30703015100002));
#287032=CARTESIAN_POINT('Ctrl Pts',(-5.50477622400006,11.6,-9.30703015100002));
#287033=CARTESIAN_POINT('Ctrl Pts',(-5.50540346100005,15.2,-9.30964156000002));
#287034=CARTESIAN_POINT('Ctrl Pts',(-5.50540346100005,11.6,-9.30964156000002));
#287035=CARTESIAN_POINT('Ctrl Pts',(-5.50602985400006,15.2,-9.31225919400001));
#287036=CARTESIAN_POINT('Ctrl Pts',(-5.50602985400006,11.6,-9.31225919400001));
#287037=CARTESIAN_POINT('Ctrl Pts',(-5.50665539400006,15.2,-9.31488304500002));
#287038=CARTESIAN_POINT('Ctrl Pts',(-5.50665539400006,11.6,-9.31488304500002));
#287039=CARTESIAN_POINT('Ctrl Pts',(-5.50728006900005,15.2,-9.31751310200001));
#287040=CARTESIAN_POINT('Ctrl Pts',(-5.50728006900005,11.6,-9.31751310200001));
#287041=CARTESIAN_POINT('Ctrl Pts',(-5.50790386900006,15.2,-9.32014935900002));
#287042=CARTESIAN_POINT('Ctrl Pts',(-5.50790386900006,11.6,-9.32014935900002));
#287043=CARTESIAN_POINT('Ctrl Pts',(-5.50852678200005,15.2,-9.32279180500002));
#287044=CARTESIAN_POINT('Ctrl Pts',(-5.50852678200005,11.6,-9.32279180500002));
#287045=CARTESIAN_POINT('Ctrl Pts',(-5.50914879900006,15.2,-9.32544043300001));
#287046=CARTESIAN_POINT('Ctrl Pts',(-5.50914879900006,11.6,-9.32544043300001));
#287047=CARTESIAN_POINT('Ctrl Pts',(-5.50976990800006,15.2,-9.32809523400002));
#287048=CARTESIAN_POINT('Ctrl Pts',(-5.50976990800006,11.6,-9.32809523400002));
#287049=CARTESIAN_POINT('Ctrl Pts',(-5.51039009700006,15.2,-9.33075620000002));
#287050=CARTESIAN_POINT('Ctrl Pts',(-5.51039009700006,11.6,-9.33075620000002));
#287051=CARTESIAN_POINT('Ctrl Pts',(-5.51100935800005,15.2,-9.33342332100001));
#287052=CARTESIAN_POINT('Ctrl Pts',(-5.51100935800005,11.6,-9.33342332100001));
#287053=CARTESIAN_POINT('Ctrl Pts',(-5.51162767900006,15.2,-9.33609659000001));
#287054=CARTESIAN_POINT('Ctrl Pts',(-5.51162767900006,11.6,-9.33609659000001));
#287055=CARTESIAN_POINT('Ctrl Pts',(-5.51224505000006,15.2,-9.33877599700002));
#287056=CARTESIAN_POINT('Ctrl Pts',(-5.51224505000006,11.6,-9.33877599700002));
#287057=CARTESIAN_POINT('Ctrl Pts',(-5.51286145900006,15.2,-9.34146153400001));
#287058=CARTESIAN_POINT('Ctrl Pts',(-5.51286145900006,11.6,-9.34146153400001));
#287059=CARTESIAN_POINT('Ctrl Pts',(-5.51347689600005,15.2,-9.34415319400001));
#287060=CARTESIAN_POINT('Ctrl Pts',(-5.51347689600005,11.6,-9.34415319400001));
#287061=CARTESIAN_POINT('Ctrl Pts',(-5.51409135300006,15.2,-9.34685096600001));
#287062=CARTESIAN_POINT('Ctrl Pts',(-5.51409135300006,11.6,-9.34685096600001));
#287063=CARTESIAN_POINT('Ctrl Pts',(-5.51470481600006,15.2,-9.34955484400002));
#287064=CARTESIAN_POINT('Ctrl Pts',(-5.51470481600006,11.6,-9.34955484400002));
#287065=CARTESIAN_POINT('Ctrl Pts',(-5.51531727600006,15.2,-9.35226481800001));
#287066=CARTESIAN_POINT('Ctrl Pts',(-5.51531727600006,11.6,-9.35226481800001));
#287067=CARTESIAN_POINT('Ctrl Pts',(-5.51592872200006,15.2,-9.35498087900001));
#287068=CARTESIAN_POINT('Ctrl Pts',(-5.51592872200006,11.6,-9.35498087900001));
#287069=CARTESIAN_POINT('Ctrl Pts',(-5.51653914500006,15.2,-9.35770301900002));
#287070=CARTESIAN_POINT('Ctrl Pts',(-5.51653914500006,11.6,-9.35770301900002));
#287071=CARTESIAN_POINT('Ctrl Pts',(-5.51714853300005,15.2,-9.36043123200001));
#287072=CARTESIAN_POINT('Ctrl Pts',(-5.51714853300005,11.6,-9.36043123200001));
#287073=CARTESIAN_POINT('Ctrl Pts',(-5.51775687700006,15.2,-9.36316550500001));
#287074=CARTESIAN_POINT('Ctrl Pts',(-5.51775687700006,11.6,-9.36316550500001));
#287075=CARTESIAN_POINT('Ctrl Pts',(-5.51836416700006,15.2,-9.36590583500001));
#287076=CARTESIAN_POINT('Ctrl Pts',(-5.51836416700006,11.6,-9.36590583500001));
#287077=CARTESIAN_POINT('Ctrl Pts',(-5.51897039000006,15.2,-9.36865220900001));
#287078=CARTESIAN_POINT('Ctrl Pts',(-5.51897039000006,11.6,-9.36865220900001));
#287079=CARTESIAN_POINT('Ctrl Pts',(-5.51957553900006,15.2,-9.37140462000002));
#287080=CARTESIAN_POINT('Ctrl Pts',(-5.51957553900006,11.6,-9.37140462000002));
#287081=CARTESIAN_POINT('Ctrl Pts',(-5.52017960200006,15.2,-9.37416306100002));
#287082=CARTESIAN_POINT('Ctrl Pts',(-5.52017960200006,11.6,-9.37416306100002));
#287083=CARTESIAN_POINT('Ctrl Pts',(-5.52078257000006,15.2,-9.37692752200002));
#287084=CARTESIAN_POINT('Ctrl Pts',(-5.52078257000006,11.6,-9.37692752200002));
#287085=CARTESIAN_POINT('Ctrl Pts',(-5.52138443200006,15.2,-9.37969799600002));
#287086=CARTESIAN_POINT('Ctrl Pts',(-5.52138443200006,11.6,-9.37969799600002));
#287087=CARTESIAN_POINT('Ctrl Pts',(-5.52198517700006,15.2,-9.38247447400002));
#287088=CARTESIAN_POINT('Ctrl Pts',(-5.52198517700006,11.6,-9.38247447400002));
#287089=CARTESIAN_POINT('Ctrl Pts',(-5.52258479700006,15.2,-9.38525694700001));
#287090=CARTESIAN_POINT('Ctrl Pts',(-5.52258479700006,11.6,-9.38525694700001));
#287091=CARTESIAN_POINT('Ctrl Pts',(-5.52318328100006,15.2,-9.38804540800002));
#287092=CARTESIAN_POINT('Ctrl Pts',(-5.52318328100006,11.6,-9.38804540800002));
#287093=CARTESIAN_POINT('Ctrl Pts',(-5.52378061800006,15.2,-9.39083984800002));
#287094=CARTESIAN_POINT('Ctrl Pts',(-5.52378061800006,11.6,-9.39083984800002));
#287095=CARTESIAN_POINT('Ctrl Pts',(-5.52437679900006,15.2,-9.39364025800002));
#287096=CARTESIAN_POINT('Ctrl Pts',(-5.52437679900006,11.6,-9.39364025800002));
#287097=CARTESIAN_POINT('Ctrl Pts',(-5.52497181400006,15.2,-9.39644663300001));
#287098=CARTESIAN_POINT('Ctrl Pts',(-5.52497181400006,11.6,-9.39644663300001));
#287099=CARTESIAN_POINT('Ctrl Pts',(-5.52556565400006,15.2,-9.39925896000002));
#287100=CARTESIAN_POINT('Ctrl Pts',(-5.52556565400006,11.6,-9.39925896000002));
#287101=CARTESIAN_POINT('Ctrl Pts',(-5.52615830800006,15.2,-9.40207723400002));
#287102=CARTESIAN_POINT('Ctrl Pts',(-5.52615830800006,11.6,-9.40207723400002));
#287103=CARTESIAN_POINT('Ctrl Pts',(-5.52674976600006,15.2,-9.40490144500002));
#287104=CARTESIAN_POINT('Ctrl Pts',(-5.52674976600006,11.6,-9.40490144500002));
#287105=CARTESIAN_POINT('Ctrl Pts',(-5.52734001800006,15.2,-9.40773158700001));
#287106=CARTESIAN_POINT('Ctrl Pts',(-5.52734001800006,11.6,-9.40773158700001));
#287107=CARTESIAN_POINT('Ctrl Pts',(-5.52792905500006,15.2,-9.41056764900001));
#287108=CARTESIAN_POINT('Ctrl Pts',(-5.52792905500006,11.6,-9.41056764900001));
#287109=CARTESIAN_POINT('Ctrl Pts',(-5.52851686600006,15.2,-9.41340962500002));
#287110=CARTESIAN_POINT('Ctrl Pts',(-5.52851686600006,11.6,-9.41340962500002));
#287111=CARTESIAN_POINT('Ctrl Pts',(-5.52910344300006,15.2,-9.41625750600002));
#287112=CARTESIAN_POINT('Ctrl Pts',(-5.52910344300006,11.6,-9.41625750600002));
#287113=CARTESIAN_POINT('Ctrl Pts',(-5.52968877600006,15.2,-9.41911128400001));
#287114=CARTESIAN_POINT('Ctrl Pts',(-5.52968877600006,11.6,-9.41911128400001));
#287115=CARTESIAN_POINT('Ctrl Pts',(-5.53027285400006,15.2,-9.42197095100001));
#287116=CARTESIAN_POINT('Ctrl Pts',(-5.53027285400006,11.6,-9.42197095100001));
#287117=CARTESIAN_POINT('Ctrl Pts',(-5.53085566800006,15.2,-9.42483649900002));
#287118=CARTESIAN_POINT('Ctrl Pts',(-5.53085566800006,11.6,-9.42483649900002));
#287119=CARTESIAN_POINT('Ctrl Pts',(-5.53143720800006,15.2,-9.42770791800001));
#287120=CARTESIAN_POINT('Ctrl Pts',(-5.53143720800006,11.6,-9.42770791800001));
#287121=CARTESIAN_POINT('Ctrl Pts',(-5.53201746600006,15.2,-9.43058520200001));
#287122=CARTESIAN_POINT('Ctrl Pts',(-5.53201746600006,11.6,-9.43058520200001));
#287123=CARTESIAN_POINT('Ctrl Pts',(-5.53259643100006,15.2,-9.43346834200002));
#287124=CARTESIAN_POINT('Ctrl Pts',(-5.53259643100006,11.6,-9.43346834200002));
#287125=CARTESIAN_POINT('Ctrl Pts',(-5.53317409300006,15.2,-9.43635733100002));
#287126=CARTESIAN_POINT('Ctrl Pts',(-5.53317409300006,11.6,-9.43635733100002));
#287127=CARTESIAN_POINT('Ctrl Pts',(-5.53375044300005,15.2,-9.43925216000002));
#287128=CARTESIAN_POINT('Ctrl Pts',(-5.53375044300005,11.6,-9.43925216000002));
#287129=CARTESIAN_POINT('Ctrl Pts',(-5.53432547200006,15.2,-9.44215282000001));
#287130=CARTESIAN_POINT('Ctrl Pts',(-5.53432547200006,11.6,-9.44215282000001));
#287131=CARTESIAN_POINT('Ctrl Pts',(-5.53489917000006,15.2,-9.44505930400002));
#287132=CARTESIAN_POINT('Ctrl Pts',(-5.53489917000006,11.6,-9.44505930400002));
#287133=CARTESIAN_POINT('Ctrl Pts',(-5.53547152800006,15.2,-9.44797160400002));
#287134=CARTESIAN_POINT('Ctrl Pts',(-5.53547152800006,11.6,-9.44797160400002));
#287135=CARTESIAN_POINT('Ctrl Pts',(-5.53604253700006,15.2,-9.45088971200001));
#287136=CARTESIAN_POINT('Ctrl Pts',(-5.53604253700006,11.6,-9.45088971200001));
#287137=CARTESIAN_POINT('Ctrl Pts',(-5.53661218600006,15.2,-9.45381362000001));
#287138=CARTESIAN_POINT('Ctrl Pts',(-5.53661218600006,11.6,-9.45381362000001));
#287139=CARTESIAN_POINT('Ctrl Pts',(-5.53718046800006,15.2,-9.45674332000002));
#287140=CARTESIAN_POINT('Ctrl Pts',(-5.53718046800006,11.6,-9.45674332000002));
#287141=CARTESIAN_POINT('Ctrl Pts',(-5.53774737000006,15.2,-9.45967880400002));
#287142=CARTESIAN_POINT('Ctrl Pts',(-5.53774737000006,11.6,-9.45967880400002));
#287143=CARTESIAN_POINT('Ctrl Pts',(-5.53831288800006,15.2,-9.46262006300002));
#287144=CARTESIAN_POINT('Ctrl Pts',(-5.53831288800006,11.6,-9.46262006300002));
#287145=CARTESIAN_POINT('Ctrl Pts',(-5.53887700700006,15.2,-9.46556709000001));
#287146=CARTESIAN_POINT('Ctrl Pts',(-5.53887700700006,11.6,-9.46556709000001));
#287147=CARTESIAN_POINT('Ctrl Pts',(-5.53943972200006,15.2,-9.46851987700001));
#287148=CARTESIAN_POINT('Ctrl Pts',(-5.53943972200006,11.6,-9.46851987700001));
#287149=CARTESIAN_POINT('Ctrl Pts',(-5.54000102100006,15.2,-9.47147841500002));
#287150=CARTESIAN_POINT('Ctrl Pts',(-5.54000102100006,11.6,-9.47147841500002));
#287151=CARTESIAN_POINT('Ctrl Pts',(-5.54056089800006,15.2,-9.47444269800001));
#287152=CARTESIAN_POINT('Ctrl Pts',(-5.54056089800006,11.6,-9.47444269800001));
#287153=CARTESIAN_POINT('Ctrl Pts',(-5.54111934100006,15.2,-9.47741271600002));
#287154=CARTESIAN_POINT('Ctrl Pts',(-5.54111934100006,11.6,-9.47741271600002));
#287155=CARTESIAN_POINT('Ctrl Pts',(-5.54167634100006,15.2,-9.48038846300001));
#287156=CARTESIAN_POINT('Ctrl Pts',(-5.54167634100006,11.6,-9.48038846300001));
#287157=CARTESIAN_POINT('Ctrl Pts',(-5.54223189100005,15.2,-9.48336993000002));
#287158=CARTESIAN_POINT('Ctrl Pts',(-5.54223189100005,11.6,-9.48336993000002));
#287159=CARTESIAN_POINT('Ctrl Pts',(-5.54278597900006,15.2,-9.48635710900002));
#287160=CARTESIAN_POINT('Ctrl Pts',(-5.54278597900006,11.6,-9.48635710900002));
#287161=CARTESIAN_POINT('Ctrl Pts',(-5.54333859900006,15.2,-9.48934999200001));
#287162=CARTESIAN_POINT('Ctrl Pts',(-5.54333859900006,11.6,-9.48934999200001));
#287163=CARTESIAN_POINT('Ctrl Pts',(-5.54388974000006,15.2,-9.49234857200001));
#287164=CARTESIAN_POINT('Ctrl Pts',(-5.54388974000006,11.6,-9.49234857200001));
#287165=CARTESIAN_POINT('Ctrl Pts',(-5.54443939300006,15.2,-9.49535284000002));
#287166=CARTESIAN_POINT('Ctrl Pts',(-5.54443939300006,11.6,-9.49535284000002));
#287167=CARTESIAN_POINT('Ctrl Pts',(-5.54498755000006,15.2,-9.49836278900002));
#287168=CARTESIAN_POINT('Ctrl Pts',(-5.54498755000006,11.6,-9.49836278900002));
#287169=CARTESIAN_POINT('Ctrl Pts',(-5.54553420100006,15.2,-9.50137841100002));
#287170=CARTESIAN_POINT('Ctrl Pts',(-5.54553420100006,11.6,-9.50137841100002));
#287171=CARTESIAN_POINT('Ctrl Pts',(-5.54607933800006,15.2,-9.50439969700002));
#287172=CARTESIAN_POINT('Ctrl Pts',(-5.54607933800006,11.6,-9.50439969700002));
#287173=CARTESIAN_POINT('Ctrl Pts',(-5.54662295300006,15.2,-9.50742664100002));
#287174=CARTESIAN_POINT('Ctrl Pts',(-5.54662295300006,11.6,-9.50742664100002));
#287175=CARTESIAN_POINT('Ctrl Pts',(-5.54716503400006,15.2,-9.51045923400001));
#287176=CARTESIAN_POINT('Ctrl Pts',(-5.54716503400006,11.6,-9.51045923400001));
#287177=CARTESIAN_POINT('Ctrl Pts',(-5.54770557400006,15.2,-9.51349746900001));
#287178=CARTESIAN_POINT('Ctrl Pts',(-5.54770557400006,11.6,-9.51349746900001));
#287179=CARTESIAN_POINT('Ctrl Pts',(-5.54824456500006,15.2,-9.51654133600002));
#287180=CARTESIAN_POINT('Ctrl Pts',(-5.54824456500006,11.6,-9.51654133600002));
#287181=CARTESIAN_POINT('Ctrl Pts',(-5.54878199800006,15.2,-9.51959083100002));
#287182=CARTESIAN_POINT('Ctrl Pts',(-5.54878199800006,11.6,-9.51959083100002));
#287183=CARTESIAN_POINT('Ctrl Pts',(-5.54931786200005,15.2,-9.52264594300001));
#287184=CARTESIAN_POINT('Ctrl Pts',(-5.54931786200005,11.6,-9.52264594300001));
#287185=CARTESIAN_POINT('Ctrl Pts',(-5.54985215100006,15.2,-9.52570666600002));
#287186=CARTESIAN_POINT('Ctrl Pts',(-5.54985215100006,11.6,-9.52570666600002));
#287187=CARTESIAN_POINT('Ctrl Pts',(-5.55038485500006,15.2,-9.52877299000002));
#287188=CARTESIAN_POINT('Ctrl Pts',(-5.55038485500006,11.6,-9.52877299000002));
#287189=CARTESIAN_POINT('Ctrl Pts',(-5.55091596500006,15.2,-9.53184491000002));
#287190=CARTESIAN_POINT('Ctrl Pts',(-5.55091596500006,11.6,-9.53184491000002));
#287191=CARTESIAN_POINT('Ctrl Pts',(-5.55144547200006,15.2,-9.53492241800001));
#287192=CARTESIAN_POINT('Ctrl Pts',(-5.55144547200006,11.6,-9.53492241800001));
#287193=CARTESIAN_POINT('Ctrl Pts',(-5.55197337000005,15.2,-9.53800550400001));
#287194=CARTESIAN_POINT('Ctrl Pts',(-5.55197337000005,11.6,-9.53800550400001));
#287195=CARTESIAN_POINT('Ctrl Pts',(-5.55249964700006,15.2,-9.54109416100002));
#287196=CARTESIAN_POINT('Ctrl Pts',(-5.55249964700006,11.6,-9.54109416100002));
#287197=CARTESIAN_POINT('Ctrl Pts',(-5.55302429700006,15.2,-9.54418838400001));
#287198=CARTESIAN_POINT('Ctrl Pts',(-5.55302429700006,11.6,-9.54418838400001));
#287199=CARTESIAN_POINT('Ctrl Pts',(-5.55354730900006,15.2,-9.54728816200002));
#287200=CARTESIAN_POINT('Ctrl Pts',(-5.55354730900006,11.6,-9.54728816200002));
#287201=CARTESIAN_POINT('Ctrl Pts',(-5.55406867700006,15.2,-9.55039348800002));
#287202=CARTESIAN_POINT('Ctrl Pts',(-5.55406867700006,11.6,-9.55039348800002));
#287203=CARTESIAN_POINT('Ctrl Pts',(-5.55458839100006,15.2,-9.55350435500002));
#287204=CARTESIAN_POINT('Ctrl Pts',(-5.55458839100006,11.6,-9.55350435500002));
#287205=CARTESIAN_POINT('Ctrl Pts',(-5.55510644200006,15.2,-9.55662075600002));
#287206=CARTESIAN_POINT('Ctrl Pts',(-5.55510644200006,11.6,-9.55662075600002));
#287207=CARTESIAN_POINT('Ctrl Pts',(-5.55562282200006,15.2,-9.55974268200002));
#287208=CARTESIAN_POINT('Ctrl Pts',(-5.55562282200006,11.6,-9.55974268200002));
#287209=CARTESIAN_POINT('Ctrl Pts',(-5.55613752400006,15.2,-9.56287012600002));
#287210=CARTESIAN_POINT('Ctrl Pts',(-5.55613752400006,11.6,-9.56287012600002));
#287211=CARTESIAN_POINT('Ctrl Pts',(-5.55665053700006,15.2,-9.56600308000001));
#287212=CARTESIAN_POINT('Ctrl Pts',(-5.55665053700006,11.6,-9.56600308000001));
#287213=CARTESIAN_POINT('Ctrl Pts',(-5.55716185500006,15.2,-9.56914153600002));
#287214=CARTESIAN_POINT('Ctrl Pts',(-5.55716185500006,11.6,-9.56914153600002));
#287215=CARTESIAN_POINT('Ctrl Pts',(-5.55767146700005,15.2,-9.57228548700002));
#287216=CARTESIAN_POINT('Ctrl Pts',(-5.55767146700005,11.6,-9.57228548700002));
#287217=CARTESIAN_POINT('Ctrl Pts',(-5.55817936700006,15.2,-9.57543492600001));
#287218=CARTESIAN_POINT('Ctrl Pts',(-5.55817936700006,11.6,-9.57543492600001));
#287219=CARTESIAN_POINT('Ctrl Pts',(-5.55868554700006,15.2,-9.57858984400002));
#287220=CARTESIAN_POINT('Ctrl Pts',(-5.55868554700006,11.6,-9.57858984400002));
#287221=CARTESIAN_POINT('Ctrl Pts',(-5.55918999600006,15.2,-9.58175023500001));
#287222=CARTESIAN_POINT('Ctrl Pts',(-5.55918999600006,11.6,-9.58175023500001));
#287223=CARTESIAN_POINT('Ctrl Pts',(-5.55969270800006,15.2,-9.58491608900001));
#287224=CARTESIAN_POINT('Ctrl Pts',(-5.55969270800006,11.6,-9.58491608900001));
#287225=CARTESIAN_POINT('Ctrl Pts',(-5.56019367400006,15.2,-9.58808740000002));
#287226=CARTESIAN_POINT('Ctrl Pts',(-5.56019367400006,11.6,-9.58808740000002));
#287227=CARTESIAN_POINT('Ctrl Pts',(-5.56069288500006,15.2,-9.59126416200002));
#287228=CARTESIAN_POINT('Ctrl Pts',(-5.56069288500006,11.6,-9.59126416200002));
#287229=CARTESIAN_POINT('Ctrl Pts',(-5.56119033400006,15.2,-9.59444636500002));
#287230=CARTESIAN_POINT('Ctrl Pts',(-5.56119033400006,11.6,-9.59444636500002));
#287231=CARTESIAN_POINT('Ctrl Pts',(-5.56168601200006,15.2,-9.59763400200002));
#287232=CARTESIAN_POINT('Ctrl Pts',(-5.56168601200006,11.6,-9.59763400200002));
#287233=CARTESIAN_POINT('Ctrl Pts',(-5.56217991100006,15.2,-9.60082706600002));
#287234=CARTESIAN_POINT('Ctrl Pts',(-5.56217991100006,11.6,-9.60082706600002));
#287235=CARTESIAN_POINT('Ctrl Pts',(-5.56267202400006,15.2,-9.60402554800002));
#287236=CARTESIAN_POINT('Ctrl Pts',(-5.56267202400006,11.6,-9.60402554800002));
#287237=CARTESIAN_POINT('Ctrl Pts',(-5.56316234000006,15.2,-9.60722944300001));
#287238=CARTESIAN_POINT('Ctrl Pts',(-5.56316234000006,11.6,-9.60722944300001));
#287239=CARTESIAN_POINT('Ctrl Pts',(-5.56365085400006,15.2,-9.61043874100002));
#287240=CARTESIAN_POINT('Ctrl Pts',(-5.56365085400006,11.6,-9.61043874100002));
#287241=CARTESIAN_POINT('Ctrl Pts',(-5.56413755700006,15.2,-9.61365343600002));
#287242=CARTESIAN_POINT('Ctrl Pts',(-5.56413755700006,11.6,-9.61365343600002));
#287243=CARTESIAN_POINT('Ctrl Pts',(-5.56462243900006,15.2,-9.61687352000002));
#287244=CARTESIAN_POINT('Ctrl Pts',(-5.56462243900006,11.6,-9.61687352000002));
#287245=CARTESIAN_POINT('Ctrl Pts',(-5.56510549500006,15.2,-9.62009898500002));
#287246=CARTESIAN_POINT('Ctrl Pts',(-5.56510549500006,11.6,-9.62009898500002));
#287247=CARTESIAN_POINT('Ctrl Pts',(-5.56558671400006,15.2,-9.62332982500002));
#287248=CARTESIAN_POINT('Ctrl Pts',(-5.56558671400006,11.6,-9.62332982500002));
#287249=CARTESIAN_POINT('Ctrl Pts',(-5.56606609100006,15.2,-9.62656603200001));
#287250=CARTESIAN_POINT('Ctrl Pts',(-5.56606609100006,11.6,-9.62656603200001));
#287251=CARTESIAN_POINT('Ctrl Pts',(-5.56654361600006,15.2,-9.62980759800002));
#287252=CARTESIAN_POINT('Ctrl Pts',(-5.56654361600006,11.6,-9.62980759800002));
#287253=CARTESIAN_POINT('Ctrl Pts',(-5.56701928100006,15.2,-9.63305451500002));
#287254=CARTESIAN_POINT('Ctrl Pts',(-5.56701928100006,11.6,-9.63305451500002));
#287255=CARTESIAN_POINT('Ctrl Pts',(-5.56749308000006,15.2,-9.63630677700002));
#287256=CARTESIAN_POINT('Ctrl Pts',(-5.56749308000006,11.6,-9.63630677700002));
#287257=CARTESIAN_POINT('Ctrl Pts',(-5.56796500300006,15.2,-9.63956437500002));
#287258=CARTESIAN_POINT('Ctrl Pts',(-5.56796500300006,11.6,-9.63956437500002));
#287259=CARTESIAN_POINT('Ctrl Pts',(-5.56843504200006,15.2,-9.64282730200001));
#287260=CARTESIAN_POINT('Ctrl Pts',(-5.56843504200006,11.6,-9.64282730200001));
#287261=CARTESIAN_POINT('Ctrl Pts',(-5.56890319100006,15.2,-9.64609555300001));
#287262=CARTESIAN_POINT('Ctrl Pts',(-5.56890319100006,11.6,-9.64609555300001));
#287263=CARTESIAN_POINT('Ctrl Pts',(-5.56936944100006,15.2,-9.64936911600002));
#287264=CARTESIAN_POINT('Ctrl Pts',(-5.56936944100006,11.6,-9.64936911600002));
#287265=CARTESIAN_POINT('Ctrl Pts',(-5.56983378400006,15.2,-9.65264798800001));
#287266=CARTESIAN_POINT('Ctrl Pts',(-5.56983378400006,11.6,-9.65264798800001));
#287267=CARTESIAN_POINT('Ctrl Pts',(-5.57029621300006,15.2,-9.65593215900001));
#287268=CARTESIAN_POINT('Ctrl Pts',(-5.57029621300006,11.6,-9.65593215900001));
#287269=CARTESIAN_POINT('Ctrl Pts',(-5.57075671900006,15.2,-9.65922162300001));
#287270=CARTESIAN_POINT('Ctrl Pts',(-5.57075671900006,11.6,-9.65922162300001));
#287271=CARTESIAN_POINT('Ctrl Pts',(-5.57121529500006,15.2,-9.66251637100001));
#287272=CARTESIAN_POINT('Ctrl Pts',(-5.57121529500006,11.6,-9.66251637100001));
#287273=CARTESIAN_POINT('Ctrl Pts',(-5.57167193400006,15.2,-9.66581639800001));
#287274=CARTESIAN_POINT('Ctrl Pts',(-5.57167193400006,11.6,-9.66581639800001));
#287275=CARTESIAN_POINT('Ctrl Pts',(-5.57212662700006,15.2,-9.66912169500001));
#287276=CARTESIAN_POINT('Ctrl Pts',(-5.57212662700006,11.6,-9.66912169500001));
#287277=CARTESIAN_POINT('Ctrl Pts',(-5.57257936700006,15.2,-9.67243225400001));
#287278=CARTESIAN_POINT('Ctrl Pts',(-5.57257936700006,11.6,-9.67243225400001));
#287279=CARTESIAN_POINT('Ctrl Pts',(-5.57303014600006,15.2,-9.67574807000001));
#287280=CARTESIAN_POINT('Ctrl Pts',(-5.57303014600006,11.6,-9.67574807000001));
#287281=CARTESIAN_POINT('Ctrl Pts',(-5.57347895600006,15.2,-9.67906913300001));
#287282=CARTESIAN_POINT('Ctrl Pts',(-5.57347895600006,11.6,-9.67906913300001));
#287283=CARTESIAN_POINT('Ctrl Pts',(-5.57392579000005,15.2,-9.68239543700001));
#287284=CARTESIAN_POINT('Ctrl Pts',(-5.57392579000005,11.6,-9.68239543700001));
#287285=CARTESIAN_POINT('Ctrl Pts',(-5.57437064100006,15.2,-9.68572697500001));
#287286=CARTESIAN_POINT('Ctrl Pts',(-5.57437064100006,11.6,-9.68572697500001));
#287287=CARTESIAN_POINT('Ctrl Pts',(-5.57481350100006,15.2,-9.68906373900001));
#287288=CARTESIAN_POINT('Ctrl Pts',(-5.57481350100006,11.6,-9.68906373900001));
#287289=CARTESIAN_POINT('Ctrl Pts',(-5.57525436100006,15.2,-9.69240572200001));
#287290=CARTESIAN_POINT('Ctrl Pts',(-5.57525436100006,11.6,-9.69240572200001));
#287291=CARTESIAN_POINT('Ctrl Pts',(-5.57569321500006,15.2,-9.69575291700002));
#287292=CARTESIAN_POINT('Ctrl Pts',(-5.57569321500006,11.6,-9.69575291700002));
#287293=CARTESIAN_POINT('Ctrl Pts',(-5.57613005500006,15.2,-9.69910531700001));
#287294=CARTESIAN_POINT('Ctrl Pts',(-5.57613005500006,11.6,-9.69910531700001));
#287295=CARTESIAN_POINT('Ctrl Pts',(-5.57656487300005,15.2,-9.70246291300001));
#287296=CARTESIAN_POINT('Ctrl Pts',(-5.57656487300005,11.6,-9.70246291300001));
#287297=CARTESIAN_POINT('Ctrl Pts',(-5.57699766300006,15.2,-9.70582570000001));
#287298=CARTESIAN_POINT('Ctrl Pts',(-5.57699766300006,11.6,-9.70582570000001));
#287299=CARTESIAN_POINT('Ctrl Pts',(-5.57742841600006,15.2,-9.70919366800001));
#287300=CARTESIAN_POINT('Ctrl Pts',(-5.57742841600006,11.6,-9.70919366800001));
#287301=CARTESIAN_POINT('Ctrl Pts',(-5.57785712500006,15.2,-9.71256681200001));
#287302=CARTESIAN_POINT('Ctrl Pts',(-5.57785712500006,11.6,-9.71256681200001));
#287303=CARTESIAN_POINT('Ctrl Pts',(-5.57828378300006,15.2,-9.71594512400001));
#287304=CARTESIAN_POINT('Ctrl Pts',(-5.57828378300006,11.6,-9.71594512400001));
#287305=CARTESIAN_POINT('Ctrl Pts',(-5.57870838200006,15.2,-9.71932859700001));
#287306=CARTESIAN_POINT('Ctrl Pts',(-5.57870838200006,11.6,-9.71932859700001));
#287307=CARTESIAN_POINT('Ctrl Pts',(-5.57913091500006,15.2,-9.72271722400001));
#287308=CARTESIAN_POINT('Ctrl Pts',(-5.57913091500006,11.6,-9.72271722400001));
#287309=CARTESIAN_POINT('Ctrl Pts',(-5.57955137400006,15.2,-9.72611099700002));
#287310=CARTESIAN_POINT('Ctrl Pts',(-5.57955137400006,11.6,-9.72611099700002));
#287311=CARTESIAN_POINT('Ctrl Pts',(-5.57996975300005,15.2,-9.72950991000001));
#287312=CARTESIAN_POINT('Ctrl Pts',(-5.57996975300005,11.6,-9.72950991000001));
#287313=CARTESIAN_POINT('Ctrl Pts',(-5.58038604400006,15.2,-9.73291395500001));
#287314=CARTESIAN_POINT('Ctrl Pts',(-5.58038604400006,11.6,-9.73291395500001));
#287315=CARTESIAN_POINT('Ctrl Pts',(-5.58080023800006,15.2,-9.73632312400001));
#287316=CARTESIAN_POINT('Ctrl Pts',(-5.58080023800006,11.6,-9.73632312400001));
#287317=CARTESIAN_POINT('Ctrl Pts',(-5.58121233100006,15.2,-9.73973741000002));
#287318=CARTESIAN_POINT('Ctrl Pts',(-5.58121233100006,11.6,-9.73973741000002));
#287319=CARTESIAN_POINT('Ctrl Pts',(-5.58162231200006,15.2,-9.74315680800001));
#287320=CARTESIAN_POINT('Ctrl Pts',(-5.58162231200006,11.6,-9.74315680800001));
#287321=CARTESIAN_POINT('Ctrl Pts',(-5.58203017800006,15.2,-9.74658130900002));
#287322=CARTESIAN_POINT('Ctrl Pts',(-5.58203017800006,11.6,-9.74658130900002));
#287323=CARTESIAN_POINT('Ctrl Pts',(-5.58243591800006,15.2,-9.75001090500001));
#287324=CARTESIAN_POINT('Ctrl Pts',(-5.58243591800006,11.6,-9.75001090500001));
#287325=CARTESIAN_POINT('Ctrl Pts',(-5.58283952600005,15.2,-9.75344559000001));
#287326=CARTESIAN_POINT('Ctrl Pts',(-5.58283952600005,11.6,-9.75344559000001));
#287327=CARTESIAN_POINT('Ctrl Pts',(-5.58324099600005,15.2,-9.75688535700001));
#287328=CARTESIAN_POINT('Ctrl Pts',(-5.58324099600005,11.6,-9.75688535700001));
#287329=CARTESIAN_POINT('Ctrl Pts',(-5.58364031900005,15.2,-9.76033019900001));
#287330=CARTESIAN_POINT('Ctrl Pts',(-5.58364031900005,11.6,-9.76033019900001));
#287331=CARTESIAN_POINT('Ctrl Pts',(-5.58403748900006,15.2,-9.76378010900001));
#287332=CARTESIAN_POINT('Ctrl Pts',(-5.58403748900006,11.6,-9.76378010900001));
#287333=CARTESIAN_POINT('Ctrl Pts',(-5.58443250000006,15.2,-9.76723507800001));
#287334=CARTESIAN_POINT('Ctrl Pts',(-5.58443250000006,11.6,-9.76723507800001));
#287335=CARTESIAN_POINT('Ctrl Pts',(-5.58482534200006,15.2,-9.77069510100001));
#287336=CARTESIAN_POINT('Ctrl Pts',(-5.58482534200006,11.6,-9.77069510100001));
#287337=CARTESIAN_POINT('Ctrl Pts',(-5.58521601000006,15.2,-9.77416017100001));
#287338=CARTESIAN_POINT('Ctrl Pts',(-5.58521601000006,11.6,-9.77416017100001));
#287339=CARTESIAN_POINT('Ctrl Pts',(-5.58560449700006,15.2,-9.77763027800002));
#287340=CARTESIAN_POINT('Ctrl Pts',(-5.58560449700006,11.6,-9.77763027800002));
#287341=CARTESIAN_POINT('Ctrl Pts',(-5.58599079400006,15.2,-9.78110541800001));
#287342=CARTESIAN_POINT('Ctrl Pts',(-5.58599079400006,11.6,-9.78110541800001));
#287343=CARTESIAN_POINT('Ctrl Pts',(-5.58637489600006,15.2,-9.78458558300001));
#287344=CARTESIAN_POINT('Ctrl Pts',(-5.58637489600006,11.6,-9.78458558300001));
#287345=CARTESIAN_POINT('Ctrl Pts',(-5.58675679500006,15.2,-9.78807076600001));
#287346=CARTESIAN_POINT('Ctrl Pts',(-5.58675679500006,11.6,-9.78807076600001));
#287347=CARTESIAN_POINT('Ctrl Pts',(-5.58713648300006,15.2,-9.79156095800001));
#287348=CARTESIAN_POINT('Ctrl Pts',(-5.58713648300006,11.6,-9.79156095800001));
#287349=CARTESIAN_POINT('Ctrl Pts',(-5.58751395600006,15.2,-9.79505615600001));
#287350=CARTESIAN_POINT('Ctrl Pts',(-5.58751395600006,11.6,-9.79505615600001));
#287351=CARTESIAN_POINT('Ctrl Pts',(-5.58788920500006,15.2,-9.79855634900001));
#287352=CARTESIAN_POINT('Ctrl Pts',(-5.58788920500006,11.6,-9.79855634900001));
#287353=CARTESIAN_POINT('Ctrl Pts',(-5.58826222200006,15.2,-9.80206153200001));
#287354=CARTESIAN_POINT('Ctrl Pts',(-5.58826222200006,11.6,-9.80206153200001));
#287355=CARTESIAN_POINT('Ctrl Pts',(-5.58863300300006,15.2,-9.80557169700001));
#287356=CARTESIAN_POINT('Ctrl Pts',(-5.58863300300006,11.6,-9.80557169700001));
#287357=CARTESIAN_POINT('Ctrl Pts',(-5.58900153800006,15.2,-9.80908683700001));
#287358=CARTESIAN_POINT('Ctrl Pts',(-5.58900153800006,11.6,-9.80908683700001));
#287359=CARTESIAN_POINT('Ctrl Pts',(-5.58936782300006,15.2,-9.81260694600001));
#287360=CARTESIAN_POINT('Ctrl Pts',(-5.58936782300006,11.6,-9.81260694600001));
#287361=CARTESIAN_POINT('Ctrl Pts',(-5.58973184900006,15.2,-9.81613201700001));
#287362=CARTESIAN_POINT('Ctrl Pts',(-5.58973184900006,11.6,-9.81613201700001));
#287363=CARTESIAN_POINT('Ctrl Pts',(-5.59009361000006,15.2,-9.81966204100001));
#287364=CARTESIAN_POINT('Ctrl Pts',(-5.59009361000006,11.6,-9.81966204100001));
#287365=CARTESIAN_POINT('Ctrl Pts',(-5.59045309900006,15.2,-9.82319701200001));
#287366=CARTESIAN_POINT('Ctrl Pts',(-5.59045309900006,11.6,-9.82319701200001));
#287367=CARTESIAN_POINT('Ctrl Pts',(-5.59081030900006,15.2,-9.82673692500001));
#287368=CARTESIAN_POINT('Ctrl Pts',(-5.59081030900006,11.6,-9.82673692500001));
#287369=CARTESIAN_POINT('Ctrl Pts',(-5.59116523300006,15.2,-9.83028176900001));
#287370=CARTESIAN_POINT('Ctrl Pts',(-5.59116523300006,11.6,-9.83028176900001));
#287371=CARTESIAN_POINT('Ctrl Pts',(-5.59151786600006,15.2,-9.83383154100001));
#287372=CARTESIAN_POINT('Ctrl Pts',(-5.59151786600006,11.6,-9.83383154100001));
#287373=CARTESIAN_POINT('Ctrl Pts',(-5.59186819900006,15.2,-9.83738623200001));
#287374=CARTESIAN_POINT('Ctrl Pts',(-5.59186819900006,11.6,-9.83738623200001));
#287375=CARTESIAN_POINT('Ctrl Pts',(-5.59221622500006,15.2,-9.84094583600001));
#287376=CARTESIAN_POINT('Ctrl Pts',(-5.59221622500006,11.6,-9.84094583600001));
#287377=CARTESIAN_POINT('Ctrl Pts',(-5.59256194100006,15.2,-9.84451034500001));
#287378=CARTESIAN_POINT('Ctrl Pts',(-5.59256194100006,11.6,-9.84451034500001));
#287379=CARTESIAN_POINT('Ctrl Pts',(-5.59290533600006,15.2,-9.84807975100001));
#287380=CARTESIAN_POINT('Ctrl Pts',(-5.59290533600006,11.6,-9.84807975100001));
#287381=CARTESIAN_POINT('Ctrl Pts',(-5.59324640500006,15.2,-9.85165405000001));
#287382=CARTESIAN_POINT('Ctrl Pts',(-5.59324640500006,11.6,-9.85165405000001));
#287383=CARTESIAN_POINT('Ctrl Pts',(-5.59358514100006,15.2,-9.85523323300001));
#287384=CARTESIAN_POINT('Ctrl Pts',(-5.59358514100006,11.6,-9.85523323300001));
#287385=CARTESIAN_POINT('Ctrl Pts',(-5.59392153800006,15.2,-9.85881729400001));
#287386=CARTESIAN_POINT('Ctrl Pts',(-5.59392153800006,11.6,-9.85881729400001));
#287387=CARTESIAN_POINT('Ctrl Pts',(-5.59425559000006,15.2,-9.86240622500001));
#287388=CARTESIAN_POINT('Ctrl Pts',(-5.59425559000006,11.6,-9.86240622500001));
#287389=CARTESIAN_POINT('Ctrl Pts',(-5.59458728700006,15.2,-9.86600002000001));
#287390=CARTESIAN_POINT('Ctrl Pts',(-5.59458728700006,11.6,-9.86600002000001));
#287391=CARTESIAN_POINT('Ctrl Pts',(-5.59491662700006,15.2,-9.86959867100001));
#287392=CARTESIAN_POINT('Ctrl Pts',(-5.59491662700006,11.6,-9.86959867100001));
#287393=CARTESIAN_POINT('Ctrl Pts',(-5.59524360000006,15.2,-9.87320217300001));
#287394=CARTESIAN_POINT('Ctrl Pts',(-5.59524360000006,11.6,-9.87320217300001));
#287395=CARTESIAN_POINT('Ctrl Pts',(-5.59556820200006,15.2,-9.87681051700001));
#287396=CARTESIAN_POINT('Ctrl Pts',(-5.59556820200006,11.6,-9.87681051700001));
#287397=CARTESIAN_POINT('Ctrl Pts',(-5.59589042400006,15.2,-9.88042369800001));
#287398=CARTESIAN_POINT('Ctrl Pts',(-5.59589042400006,11.6,-9.88042369800001));
#287399=CARTESIAN_POINT('Ctrl Pts',(-5.59621026000006,15.2,-9.88404170800001));
#287400=CARTESIAN_POINT('Ctrl Pts',(-5.59621026000006,11.6,-9.88404170800001));
#287401=CARTESIAN_POINT('Ctrl Pts',(-5.59652770400006,15.2,-9.88766454000001));
#287402=CARTESIAN_POINT('Ctrl Pts',(-5.59652770400006,11.6,-9.88766454000001));
#287403=CARTESIAN_POINT('Ctrl Pts',(-5.59684275000006,15.2,-9.89129218700001));
#287404=CARTESIAN_POINT('Ctrl Pts',(-5.59684275000006,11.6,-9.89129218700001));
#287405=CARTESIAN_POINT('Ctrl Pts',(-5.59715539100006,15.2,-9.89492464200001));
#287406=CARTESIAN_POINT('Ctrl Pts',(-5.59715539100006,11.6,-9.89492464200001));
#287407=CARTESIAN_POINT('Ctrl Pts',(-5.59746562000006,15.2,-9.89856190000001));
#287408=CARTESIAN_POINT('Ctrl Pts',(-5.59746562000006,11.6,-9.89856190000001));
#287409=CARTESIAN_POINT('Ctrl Pts',(-5.59777343200006,15.2,-9.90220395300001));
#287410=CARTESIAN_POINT('Ctrl Pts',(-5.59777343200006,11.6,-9.90220395300001));
#287411=CARTESIAN_POINT('Ctrl Pts',(-5.59807881900006,15.2,-9.90585079300001));
#287412=CARTESIAN_POINT('Ctrl Pts',(-5.59807881900006,11.6,-9.90585079300001));
#287413=CARTESIAN_POINT('Ctrl Pts',(-5.59838177600006,15.2,-9.90950241400001));
#287414=CARTESIAN_POINT('Ctrl Pts',(-5.59838177600006,11.6,-9.90950241400001));
#287415=CARTESIAN_POINT('Ctrl Pts',(-5.59868229500006,15.2,-9.91315881000001));
#287416=CARTESIAN_POINT('Ctrl Pts',(-5.59868229500006,11.6,-9.91315881000001));
#287417=CARTESIAN_POINT('Ctrl Pts',(-5.59898037100006,15.2,-9.91681997300001));
#287418=CARTESIAN_POINT('Ctrl Pts',(-5.59898037100006,11.6,-9.91681997300001));
#287419=CARTESIAN_POINT('Ctrl Pts',(-5.59927599700006,15.2,-9.92048589600001));
#287420=CARTESIAN_POINT('Ctrl Pts',(-5.59927599700006,11.6,-9.92048589600001));
#287421=CARTESIAN_POINT('Ctrl Pts',(-5.59956916600005,15.2,-9.92415657400001));
#287422=CARTESIAN_POINT('Ctrl Pts',(-5.59956916600005,11.6,-9.92415657400001));
#287423=CARTESIAN_POINT('Ctrl Pts',(-5.59985987300006,15.2,-9.92783199800001));
#287424=CARTESIAN_POINT('Ctrl Pts',(-5.59985987300006,11.6,-9.92783199800001));
#287425=CARTESIAN_POINT('Ctrl Pts',(-5.60014811000006,15.2,-9.93151216200001));
#287426=CARTESIAN_POINT('Ctrl Pts',(-5.60014811000006,11.6,-9.93151216200001));
#287427=CARTESIAN_POINT('Ctrl Pts',(-5.60043387200006,15.2,-9.93519706000001));
#287428=CARTESIAN_POINT('Ctrl Pts',(-5.60043387200006,11.6,-9.93519706000001));
#287429=CARTESIAN_POINT('Ctrl Pts',(-5.60071715300006,15.2,-9.93888668300001));
#287430=CARTESIAN_POINT('Ctrl Pts',(-5.60071715300006,11.6,-9.93888668300001));
#287431=CARTESIAN_POINT('Ctrl Pts',(-5.60099794600006,15.2,-9.94258102700002));
#287432=CARTESIAN_POINT('Ctrl Pts',(-5.60099794600006,11.6,-9.94258102700002));
#287433=CARTESIAN_POINT('Ctrl Pts',(-5.60127624500006,15.2,-9.94628008400001));
#287434=CARTESIAN_POINT('Ctrl Pts',(-5.60127624500006,11.6,-9.94628008400001));
#287435=CARTESIAN_POINT('Ctrl Pts',(-5.60155204400006,15.2,-9.94998384700001));
#287436=CARTESIAN_POINT('Ctrl Pts',(-5.60155204400006,11.6,-9.94998384700001));
#287437=CARTESIAN_POINT('Ctrl Pts',(-5.60182533700006,15.2,-9.95369231100001));
#287438=CARTESIAN_POINT('Ctrl Pts',(-5.60182533700006,11.6,-9.95369231100001));
#287439=CARTESIAN_POINT('Ctrl Pts',(-5.60209611700006,15.2,-9.95740546800001));
#287440=CARTESIAN_POINT('Ctrl Pts',(-5.60209611700006,11.6,-9.95740546800001));
#287441=CARTESIAN_POINT('Ctrl Pts',(-5.60236437800006,15.2,-9.96112330900001));
#287442=CARTESIAN_POINT('Ctrl Pts',(-5.60236437800006,11.6,-9.96112330900001));
#287443=CARTESIAN_POINT('Ctrl Pts',(-5.60263011400005,15.2,-9.96484583000001));
#287444=CARTESIAN_POINT('Ctrl Pts',(-5.60263011400005,11.6,-9.96484583000001));
#287445=CARTESIAN_POINT('Ctrl Pts',(-5.60289331800006,15.2,-9.96857302300001));
#287446=CARTESIAN_POINT('Ctrl Pts',(-5.60289331800006,11.6,-9.96857302300001));
#287447=CARTESIAN_POINT('Ctrl Pts',(-5.60315398400006,15.2,-9.97230488000001));
#287448=CARTESIAN_POINT('Ctrl Pts',(-5.60315398400006,11.6,-9.97230488000001));
#287449=CARTESIAN_POINT('Ctrl Pts',(-5.60341210500006,15.2,-9.97604139500002));
#287450=CARTESIAN_POINT('Ctrl Pts',(-5.60341210500006,11.6,-9.97604139500002));
#287451=CARTESIAN_POINT('Ctrl Pts',(-5.60366767700006,15.2,-9.97978256300001));
#287452=CARTESIAN_POINT('Ctrl Pts',(-5.60366767700006,11.6,-9.97978256300001));
#287453=CARTESIAN_POINT('Ctrl Pts',(-5.60392069300006,15.2,-9.98352837700001));
#287454=CARTESIAN_POINT('Ctrl Pts',(-5.60392069300006,11.6,-9.98352837700001));
#287455=CARTESIAN_POINT('Ctrl Pts',(-5.60417114800006,15.2,-9.98727882900001));
#287456=CARTESIAN_POINT('Ctrl Pts',(-5.60417114800006,11.6,-9.98727882900001));
#287457=CARTESIAN_POINT('Ctrl Pts',(-5.60441903700006,15.2,-9.99103391600001));
#287458=CARTESIAN_POINT('Ctrl Pts',(-5.60441903700006,11.6,-9.99103391600001));
#287459=CARTESIAN_POINT('Ctrl Pts',(-5.60466435400006,15.2,-9.99479363100001));
#287460=CARTESIAN_POINT('Ctrl Pts',(-5.60466435400006,11.6,-9.99479363100001));
#287461=CARTESIAN_POINT('Ctrl Pts',(-5.60490709200006,15.2,-9.99855796400001));
#287462=CARTESIAN_POINT('Ctrl Pts',(-5.60490709200006,11.6,-9.99855796400001));
#287463=CARTESIAN_POINT('Ctrl Pts',(-5.60514724500006,15.2,-10.002326912));
#287464=CARTESIAN_POINT('Ctrl Pts',(-5.60514724500006,11.6,-10.002326912));
#287465=CARTESIAN_POINT('Ctrl Pts',(-5.60538480400006,15.2,-10.006100463));
#287466=CARTESIAN_POINT('Ctrl Pts',(-5.60538480400006,11.6,-10.006100463));
#287467=CARTESIAN_POINT('Ctrl Pts',(-5.60561976300006,15.2,-10.00987861));
#287468=CARTESIAN_POINT('Ctrl Pts',(-5.60561976300006,11.6,-10.00987861));
#287469=CARTESIAN_POINT('Ctrl Pts',(-5.60585211500006,15.2,-10.013661344));
#287470=CARTESIAN_POINT('Ctrl Pts',(-5.60585211500006,11.6,-10.013661344));
#287471=CARTESIAN_POINT('Ctrl Pts',(-5.60608185300006,15.2,-10.01744866));
#287472=CARTESIAN_POINT('Ctrl Pts',(-5.60608185300006,11.6,-10.01744866));
#287473=CARTESIAN_POINT('Ctrl Pts',(-5.60630897000006,15.2,-10.02124055));
#287474=CARTESIAN_POINT('Ctrl Pts',(-5.60630897000006,11.6,-10.02124055));
#287475=CARTESIAN_POINT('Ctrl Pts',(-5.60653346400006,15.2,-10.025037011));
#287476=CARTESIAN_POINT('Ctrl Pts',(-5.60653346400006,11.6,-10.025037011));
#287477=CARTESIAN_POINT('Ctrl Pts',(-5.60675533300006,15.2,-10.028838039));
#287478=CARTESIAN_POINT('Ctrl Pts',(-5.60675533300006,11.6,-10.028838039));
#287479=CARTESIAN_POINT('Ctrl Pts',(-5.60697457300006,15.2,-10.032643631));
#287480=CARTESIAN_POINT('Ctrl Pts',(-5.60697457300006,11.6,-10.032643631));
#287481=CARTESIAN_POINT('Ctrl Pts',(-5.60714786300006,15.2,-10.035691757));
#287482=CARTESIAN_POINT('Ctrl Pts',(-5.60714786300006,11.6,-10.035691757));
#287483=CARTESIAN_POINT('Ctrl Pts',(-5.60727664800006,15.2,-10.037979904));
#287484=CARTESIAN_POINT('Ctrl Pts',(-5.60727664800006,11.6,-10.037979904));
#287485=CARTESIAN_POINT('Ctrl Pts',(-5.60736197900006,15.2,-10.039506249));
#287486=CARTESIAN_POINT('Ctrl Pts',(-5.60736197900006,11.6,-10.039506249));
#287487=CARTESIAN_POINT('Ctrl Pts',(-5.60740451300005,15.2,-10.040269649));
#287488=CARTESIAN_POINT('Ctrl Pts',(-5.60740451300005,11.6,-10.040269649));
#287489=CARTESIAN_POINT('Ctrl Pts',(-5.36127880600006,15.2,-8.88241603200001));
#287490=CARTESIAN_POINT('Ctrl Pts',(-5.36135574400006,15.2,-8.88257249600001));
#287491=CARTESIAN_POINT('Ctrl Pts',(-5.36151222900005,15.2,-8.88289092900001));
#287492=CARTESIAN_POINT('Ctrl Pts',(-5.36174910400006,15.2,-8.88337354800001));
#287493=CARTESIAN_POINT('Ctrl Pts',(-5.36206771100006,15.2,-8.88402391700001));
#287494=CARTESIAN_POINT('Ctrl Pts',(-5.36246988000006,15.2,-8.88484693800002));
#287495=CARTESIAN_POINT('Ctrl Pts',(-5.36287772900006,15.2,-8.88568371000002));
#287496=CARTESIAN_POINT('Ctrl Pts',(-5.36328889700005,15.2,-8.88652944600001));
#287497=CARTESIAN_POINT('Ctrl Pts',(-5.36370335800005,15.2,-8.88738413200001));
#287498=CARTESIAN_POINT('Ctrl Pts',(-5.36412108300006,15.2,-8.88824775000002));
#287499=CARTESIAN_POINT('Ctrl Pts',(-5.36454204500005,15.2,-8.88912028400001));
#287500=CARTESIAN_POINT('Ctrl Pts',(-5.36496621600006,15.2,-8.89000172000001));
#287501=CARTESIAN_POINT('Ctrl Pts',(-5.36539356700006,15.2,-8.89089203900001));
#287502=CARTESIAN_POINT('Ctrl Pts',(-5.36582407300005,15.2,-8.89179122800002));
#287503=CARTESIAN_POINT('Ctrl Pts',(-5.36625770500006,15.2,-8.89269926800001));
#287504=CARTESIAN_POINT('Ctrl Pts',(-5.36669443700006,15.2,-8.89361614500002));
#287505=CARTESIAN_POINT('Ctrl Pts',(-5.36713424100006,15.2,-8.89454184300002));
#287506=CARTESIAN_POINT('Ctrl Pts',(-5.36757709000006,15.2,-8.89547634600002));
#287507=CARTESIAN_POINT('Ctrl Pts',(-5.36802295900006,15.2,-8.89641963800001));
#287508=CARTESIAN_POINT('Ctrl Pts',(-5.36847181900006,15.2,-8.89737170400002));
#287509=CARTESIAN_POINT('Ctrl Pts',(-5.36892364700006,15.2,-8.89833252800001));
#287510=CARTESIAN_POINT('Ctrl Pts',(-5.36937841200006,15.2,-8.89930209500001));
#287511=CARTESIAN_POINT('Ctrl Pts',(-5.36983609200006,15.2,-8.90028038900001));
#287512=CARTESIAN_POINT('Ctrl Pts',(-5.37029665900006,15.2,-8.90126739500002));
#287513=CARTESIAN_POINT('Ctrl Pts',(-5.37076008700006,15.2,-8.90226309800001));
#287514=CARTESIAN_POINT('Ctrl Pts',(-5.37122635100006,15.2,-8.90326748100001));
#287515=CARTESIAN_POINT('Ctrl Pts',(-5.37169542500005,15.2,-8.90428053100001));
#287516=CARTESIAN_POINT('Ctrl Pts',(-5.37216728300006,15.2,-8.90530223200001));
#287517=CARTESIAN_POINT('Ctrl Pts',(-5.37264189900006,15.2,-8.90633257000001));
#287518=CARTESIAN_POINT('Ctrl Pts',(-5.37311925100005,15.2,-8.90737152700002));
#287519=CARTESIAN_POINT('Ctrl Pts',(-5.37359931100006,15.2,-8.90841909100001));
#287520=CARTESIAN_POINT('Ctrl Pts',(-5.37408205300006,15.2,-8.90947524700002));
#287521=CARTESIAN_POINT('Ctrl Pts',(-5.37456745500006,15.2,-8.91053997800002));
#287522=CARTESIAN_POINT('Ctrl Pts',(-5.37505549100006,15.2,-8.91161327200001));
#287523=CARTESIAN_POINT('Ctrl Pts',(-5.37554613600006,15.2,-8.91269511100001));
#287524=CARTESIAN_POINT('Ctrl Pts',(-5.37603936500005,15.2,-8.91378548300001));
#287525=CARTESIAN_POINT('Ctrl Pts',(-5.37653515500006,15.2,-8.91488437200002));
#287526=CARTESIAN_POINT('Ctrl Pts',(-5.37703348100006,15.2,-8.91599176500002));
#287527=CARTESIAN_POINT('Ctrl Pts',(-5.37753431800006,15.2,-8.91710764600001));
#287528=CARTESIAN_POINT('Ctrl Pts',(-5.37803764200006,15.2,-8.91823200100001));
#287529=CARTESIAN_POINT('Ctrl Pts',(-5.37854343200006,15.2,-8.91936481500002));
#287530=CARTESIAN_POINT('Ctrl Pts',(-5.37905166000006,15.2,-8.92050607500002));
#287531=CARTESIAN_POINT('Ctrl Pts',(-5.37956230500006,15.2,-8.92165576600001));
#287532=CARTESIAN_POINT('Ctrl Pts',(-5.38007534200006,15.2,-8.92281387300002));
#287533=CARTESIAN_POINT('Ctrl Pts',(-5.38059074800006,15.2,-8.92398038200002));
#287534=CARTESIAN_POINT('Ctrl Pts',(-5.38110850100006,15.2,-8.92515528100001));
#287535=CARTESIAN_POINT('Ctrl Pts',(-5.38162857400006,15.2,-8.92633855400002));
#287536=CARTESIAN_POINT('Ctrl Pts',(-5.38215094700006,15.2,-8.92753018600001));
#287537=CARTESIAN_POINT('Ctrl Pts',(-5.38267559700006,15.2,-8.92873016600002));
#287538=CARTESIAN_POINT('Ctrl Pts',(-5.38320250000006,15.2,-8.92993847700001));
#287539=CARTESIAN_POINT('Ctrl Pts',(-5.38373163200006,15.2,-8.93115510700002));
#287540=CARTESIAN_POINT('Ctrl Pts',(-5.38426297200005,15.2,-8.93238004100001));
#287541=CARTESIAN_POINT('Ctrl Pts',(-5.38479649700006,15.2,-8.93361326700001));
#287542=CARTESIAN_POINT('Ctrl Pts',(-5.38533218400006,15.2,-8.93485477000001));
#287543=CARTESIAN_POINT('Ctrl Pts',(-5.38587001200006,15.2,-8.93610453600001));
#287544=CARTESIAN_POINT('Ctrl Pts',(-5.38640995700006,15.2,-8.93736255200002));
#287545=CARTESIAN_POINT('Ctrl Pts',(-5.38695199800006,15.2,-8.93862880300002));
#287546=CARTESIAN_POINT('Ctrl Pts',(-5.38749611100005,15.2,-8.93990327800001));
#287547=CARTESIAN_POINT('Ctrl Pts',(-5.38804227600005,15.2,-8.94118596000002));
#287548=CARTESIAN_POINT('Ctrl Pts',(-5.38859046900006,15.2,-8.94247684000002));
#287549=CARTESIAN_POINT('Ctrl Pts',(-5.38914067100006,15.2,-8.94377590100002));
#287550=CARTESIAN_POINT('Ctrl Pts',(-5.38969285900006,15.2,-8.94508313100001));
#287551=CARTESIAN_POINT('Ctrl Pts',(-5.39024701000006,15.2,-8.94639851600001));
#287552=CARTESIAN_POINT('Ctrl Pts',(-5.39080310300006,15.2,-8.94772204400001));
#287553=CARTESIAN_POINT('Ctrl Pts',(-5.39136111800006,15.2,-8.94905370100001));
#287554=CARTESIAN_POINT('Ctrl Pts',(-5.39192103300006,15.2,-8.95039347300001));
#287555=CARTESIAN_POINT('Ctrl Pts',(-5.39248282700005,15.2,-8.95174134800002));
#287556=CARTESIAN_POINT('Ctrl Pts',(-5.39304647700006,15.2,-8.95309731200001));
#287557=CARTESIAN_POINT('Ctrl Pts',(-5.39361196500006,15.2,-8.95446135300002));
#287558=CARTESIAN_POINT('Ctrl Pts',(-5.39417926700006,15.2,-8.95583345700001));
#287559=CARTESIAN_POINT('Ctrl Pts',(-5.39474836400006,15.2,-8.95721361200001));
#287560=CARTESIAN_POINT('Ctrl Pts',(-5.39531923500006,15.2,-8.95860180500001));
#287561=CARTESIAN_POINT('Ctrl Pts',(-5.39589185800006,15.2,-8.95999802100001));
#287562=CARTESIAN_POINT('Ctrl Pts',(-5.39646621500006,15.2,-8.96140225000002));
#287563=CARTESIAN_POINT('Ctrl Pts',(-5.39704228400006,15.2,-8.96281447600002));
#287564=CARTESIAN_POINT('Ctrl Pts',(-5.39762004300006,15.2,-8.96423469000002));
#287565=CARTESIAN_POINT('Ctrl Pts',(-5.39819947500006,15.2,-8.96566287700002));
#287566=CARTESIAN_POINT('Ctrl Pts',(-5.39878055600005,15.2,-8.96709902300002));
#287567=CARTESIAN_POINT('Ctrl Pts',(-5.39936326900006,15.2,-8.96854312000002));
#287568=CARTESIAN_POINT('Ctrl Pts',(-5.39994759300006,15.2,-8.96999515000001));
#287569=CARTESIAN_POINT('Ctrl Pts',(-5.40053350800005,15.2,-8.97145510400001));
#287570=CARTESIAN_POINT('Ctrl Pts',(-5.40112099300006,15.2,-8.97292296800002));
#287571=CARTESIAN_POINT('Ctrl Pts',(-5.40171003000006,15.2,-8.97439872800001));
#287572=CARTESIAN_POINT('Ctrl Pts',(-5.40230059700006,15.2,-8.97588237500001));
#287573=CARTESIAN_POINT('Ctrl Pts',(-5.40289267700006,15.2,-8.97737389500002));
#287574=CARTESIAN_POINT('Ctrl Pts',(-5.40348624900005,15.2,-8.97887327500002));
#287575=CARTESIAN_POINT('Ctrl Pts',(-5.40408129300006,15.2,-8.98038050300002));
#287576=CARTESIAN_POINT('Ctrl Pts',(-5.40467779100006,15.2,-8.98189556700002));
#287577=CARTESIAN_POINT('Ctrl Pts',(-5.40527572300006,15.2,-8.98341845500001));
#287578=CARTESIAN_POINT('Ctrl Pts',(-5.40587507000006,15.2,-8.98494915300001));
#287579=CARTESIAN_POINT('Ctrl Pts',(-5.40647581300005,15.2,-8.98648765100001));
#287580=CARTESIAN_POINT('Ctrl Pts',(-5.40707793100006,15.2,-8.98803393600001));
#287581=CARTESIAN_POINT('Ctrl Pts',(-5.40768140800005,15.2,-8.98958799500001));
#287582=CARTESIAN_POINT('Ctrl Pts',(-5.40828622400006,15.2,-8.99114981800002));
#287583=CARTESIAN_POINT('Ctrl Pts',(-5.40889235900006,15.2,-8.99271939000002));
#287584=CARTESIAN_POINT('Ctrl Pts',(-5.40949979600006,15.2,-8.99429670100002));
#287585=CARTESIAN_POINT('Ctrl Pts',(-5.41010851400006,15.2,-8.99588173800002));
#287586=CARTESIAN_POINT('Ctrl Pts',(-5.41071849700006,15.2,-8.99747449100002));
#287587=CARTESIAN_POINT('Ctrl Pts',(-5.41132972500006,15.2,-8.99907494500002));
#287588=CARTESIAN_POINT('Ctrl Pts',(-5.41194218100006,15.2,-9.00068309100002));
#287589=CARTESIAN_POINT('Ctrl Pts',(-5.41255584400006,15.2,-9.00229891600001));
#287590=CARTESIAN_POINT('Ctrl Pts',(-5.41317069800006,15.2,-9.00392240700001));
#287591=CARTESIAN_POINT('Ctrl Pts',(-5.41378672400006,15.2,-9.00555355400002));
#287592=CARTESIAN_POINT('Ctrl Pts',(-5.41440390400005,15.2,-9.00719234400002));
#287593=CARTESIAN_POINT('Ctrl Pts',(-5.41502222100006,15.2,-9.00883876600002));
#287594=CARTESIAN_POINT('Ctrl Pts',(-5.41564165400006,15.2,-9.01049280800001));
#287595=CARTESIAN_POINT('Ctrl Pts',(-5.41626218800006,15.2,-9.01215445900002));
#287596=CARTESIAN_POINT('Ctrl Pts',(-5.41688380400006,15.2,-9.01382370600002));
#287597=CARTESIAN_POINT('Ctrl Pts',(-5.41750648400006,15.2,-9.01550053800002));
#287598=CARTESIAN_POINT('Ctrl Pts',(-5.41813021000006,15.2,-9.01718494400002));
#287599=CARTESIAN_POINT('Ctrl Pts',(-5.41875496600006,15.2,-9.01887691300002));
#287600=CARTESIAN_POINT('Ctrl Pts',(-5.41938073300006,15.2,-9.02057643200001));
#287601=CARTESIAN_POINT('Ctrl Pts',(-5.42000749500006,15.2,-9.02228349000002));
#287602=CARTESIAN_POINT('Ctrl Pts',(-5.42063523200006,15.2,-9.02399807600002));
#287603=CARTESIAN_POINT('Ctrl Pts',(-5.42126392900006,15.2,-9.02572017700002));
#287604=CARTESIAN_POINT('Ctrl Pts',(-5.42189356700006,15.2,-9.02744978400002));
#287605=CARTESIAN_POINT('Ctrl Pts',(-5.42252413200006,15.2,-9.02918688400002));
#287606=CARTESIAN_POINT('Ctrl Pts',(-5.42315560300006,15.2,-9.03093146700002));
#287607=CARTESIAN_POINT('Ctrl Pts',(-5.42378796400006,15.2,-9.03268352000002));
#287608=CARTESIAN_POINT('Ctrl Pts',(-5.42442119900006,15.2,-9.03444303200001));
#287609=CARTESIAN_POINT('Ctrl Pts',(-5.42505529100006,15.2,-9.03620999300001));
#287610=CARTESIAN_POINT('Ctrl Pts',(-5.42569022200006,15.2,-9.03798439200001));
#287611=CARTESIAN_POINT('Ctrl Pts',(-5.42632597500006,15.2,-9.03976621700001));
#287612=CARTESIAN_POINT('Ctrl Pts',(-5.42696253600006,15.2,-9.04155545600002));
#287613=CARTESIAN_POINT('Ctrl Pts',(-5.42759988400006,15.2,-9.04335209900001));
#287614=CARTESIAN_POINT('Ctrl Pts',(-5.42823800600006,15.2,-9.04515613500001));
#287615=CARTESIAN_POINT('Ctrl Pts',(-5.42887688500006,15.2,-9.04696755200002));
#287616=CARTESIAN_POINT('Ctrl Pts',(-5.42951650300005,15.2,-9.04878634000001));
#287617=CARTESIAN_POINT('Ctrl Pts',(-5.43015684400006,15.2,-9.05061248700001));
#287618=CARTESIAN_POINT('Ctrl Pts',(-5.43079789200006,15.2,-9.05244598400002));
#287619=CARTESIAN_POINT('Ctrl Pts',(-5.43143963200006,15.2,-9.05428681700002));
#287620=CARTESIAN_POINT('Ctrl Pts',(-5.43208204500006,15.2,-9.05613497700001));
#287621=CARTESIAN_POINT('Ctrl Pts',(-5.43272511700006,15.2,-9.05799045400002));
#287622=CARTESIAN_POINT('Ctrl Pts',(-5.43336883000006,15.2,-9.05985323500002));
#287623=CARTESIAN_POINT('Ctrl Pts',(-5.43401316900006,15.2,-9.06172331100001));
#287624=CARTESIAN_POINT('Ctrl Pts',(-5.43465811900006,15.2,-9.06360066900002));
#287625=CARTESIAN_POINT('Ctrl Pts',(-5.43530366400006,15.2,-9.06548530000002));
#287626=CARTESIAN_POINT('Ctrl Pts',(-5.43594978500006,15.2,-9.06737719300001));
#287627=CARTESIAN_POINT('Ctrl Pts',(-5.43659647000006,15.2,-9.06927633700001));
#287628=CARTESIAN_POINT('Ctrl Pts',(-5.43724370200006,15.2,-9.07118272100002));
#287629=CARTESIAN_POINT('Ctrl Pts',(-5.43789146400006,15.2,-9.07309633400001));
#287630=CARTESIAN_POINT('Ctrl Pts',(-5.43853974200006,15.2,-9.07501716600001));
#287631=CARTESIAN_POINT('Ctrl Pts',(-5.43918852000006,15.2,-9.07694520700002));
#287632=CARTESIAN_POINT('Ctrl Pts',(-5.43983778200006,15.2,-9.07888044600002));
#287633=CARTESIAN_POINT('Ctrl Pts',(-5.44048751200005,15.2,-9.08082287200001));
#287634=CARTESIAN_POINT('Ctrl Pts',(-5.44113769600005,15.2,-9.08277247400001));
#287635=CARTESIAN_POINT('Ctrl Pts',(-5.44178831900005,15.2,-9.08472924200002));
#287636=CARTESIAN_POINT('Ctrl Pts',(-5.44243936400005,15.2,-9.08669316600001));
#287637=CARTESIAN_POINT('Ctrl Pts',(-5.44309081700006,15.2,-9.08866423400001));
#287638=CARTESIAN_POINT('Ctrl Pts',(-5.44374266300006,15.2,-9.09064243800002));
#287639=CARTESIAN_POINT('Ctrl Pts',(-5.44439488400006,15.2,-9.09262776600002));
#287640=CARTESIAN_POINT('Ctrl Pts',(-5.44504746900006,15.2,-9.09462020700002));
#287641=CARTESIAN_POINT('Ctrl Pts',(-5.44570040100006,15.2,-9.09661975100001));
#287642=CARTESIAN_POINT('Ctrl Pts',(-5.44635366500006,15.2,-9.09862638900002));
#287643=CARTESIAN_POINT('Ctrl Pts',(-5.44700724700006,15.2,-9.10064010900001));
#287644=CARTESIAN_POINT('Ctrl Pts',(-5.44766113200006,15.2,-9.10266090100002));
#287645=CARTESIAN_POINT('Ctrl Pts',(-5.44831530400006,15.2,-9.10468875600002));
#287646=CARTESIAN_POINT('Ctrl Pts',(-5.44896974900006,15.2,-9.10672366200002));
#287647=CARTESIAN_POINT('Ctrl Pts',(-5.44962445200006,15.2,-9.10876561000002));
#287648=CARTESIAN_POINT('Ctrl Pts',(-5.45027939900006,15.2,-9.11081458800002));
#287649=CARTESIAN_POINT('Ctrl Pts',(-5.45093457600006,15.2,-9.11287058900001));
#287650=CARTESIAN_POINT('Ctrl Pts',(-5.45158996700006,15.2,-9.11493360000001));
#287651=CARTESIAN_POINT('Ctrl Pts',(-5.45224555800006,15.2,-9.11700361100002));
#287652=CARTESIAN_POINT('Ctrl Pts',(-5.45290133500006,15.2,-9.11908061300002));
#287653=CARTESIAN_POINT('Ctrl Pts',(-5.45355728400006,15.2,-9.12116459600002));
#287654=CARTESIAN_POINT('Ctrl Pts',(-5.45421338900006,15.2,-9.12325554900002));
#287655=CARTESIAN_POINT('Ctrl Pts',(-5.45486963700006,15.2,-9.12535346200002));
#287656=CARTESIAN_POINT('Ctrl Pts',(-5.45552601400006,15.2,-9.12745832600002));
#287657=CARTESIAN_POINT('Ctrl Pts',(-5.45618250500006,15.2,-9.12957013000002));
#287658=CARTESIAN_POINT('Ctrl Pts',(-5.45683909700006,15.2,-9.13168886400002));
#287659=CARTESIAN_POINT('Ctrl Pts',(-5.45749577500006,15.2,-9.13381451800002));
#287660=CARTESIAN_POINT('Ctrl Pts',(-5.45815252500006,15.2,-9.13594708400002));
#287661=CARTESIAN_POINT('Ctrl Pts',(-5.45880933300006,15.2,-9.13808654900001));
#287662=CARTESIAN_POINT('Ctrl Pts',(-5.45946618600006,15.2,-9.14023290400002));
#287663=CARTESIAN_POINT('Ctrl Pts',(-5.46012307000006,15.2,-9.14238614000002));
#287664=CARTESIAN_POINT('Ctrl Pts',(-5.46077997000006,15.2,-9.14454624700002));
#287665=CARTESIAN_POINT('Ctrl Pts',(-5.46143687300006,15.2,-9.14671321500002));
#287666=CARTESIAN_POINT('Ctrl Pts',(-5.46209376500006,15.2,-9.14888703300001));
#287667=CARTESIAN_POINT('Ctrl Pts',(-5.46275063300006,15.2,-9.15106769300002));
#287668=CARTESIAN_POINT('Ctrl Pts',(-5.46340746300006,15.2,-9.15325518400002));
#287669=CARTESIAN_POINT('Ctrl Pts',(-5.46406424000006,15.2,-9.15544949700001));
#287670=CARTESIAN_POINT('Ctrl Pts',(-5.46472095400006,15.2,-9.15765062100002));
#287671=CARTESIAN_POINT('Ctrl Pts',(-5.46537758800006,15.2,-9.15985854900002));
#287672=CARTESIAN_POINT('Ctrl Pts',(-5.46603413000006,15.2,-9.16207326700002));
#287673=CARTESIAN_POINT('Ctrl Pts',(-5.46669056700006,15.2,-9.16429476900002));
#287674=CARTESIAN_POINT('Ctrl Pts',(-5.46734688500006,15.2,-9.16652304400002));
#287675=CARTESIAN_POINT('Ctrl Pts',(-5.46800307000006,15.2,-9.16875808200002));
#287676=CARTESIAN_POINT('Ctrl Pts',(-5.46865911200006,15.2,-9.17099987400002));
#287677=CARTESIAN_POINT('Ctrl Pts',(-5.46931499300006,15.2,-9.17324841000001));
#287678=CARTESIAN_POINT('Ctrl Pts',(-5.46997070400006,15.2,-9.17550368100001));
#287679=CARTESIAN_POINT('Ctrl Pts',(-5.47062622900006,15.2,-9.17776567700002));
#287680=CARTESIAN_POINT('Ctrl Pts',(-5.47128155700006,15.2,-9.18003438700002));
#287681=CARTESIAN_POINT('Ctrl Pts',(-5.47193667400006,15.2,-9.18230980400002));
#287682=CARTESIAN_POINT('Ctrl Pts',(-5.47259156600005,15.2,-9.18459191700002));
#287683=CARTESIAN_POINT('Ctrl Pts',(-5.47324622200006,15.2,-9.18688071700002));
#287684=CARTESIAN_POINT('Ctrl Pts',(-5.47390062900006,15.2,-9.18917619500002));
#287685=CARTESIAN_POINT('Ctrl Pts',(-5.47455477300006,15.2,-9.19147833900002));
#287686=CARTESIAN_POINT('Ctrl Pts',(-5.47520864000006,15.2,-9.19378714300001));
#287687=CARTESIAN_POINT('Ctrl Pts',(-5.47586222100006,15.2,-9.19610259600002));
#287688=CARTESIAN_POINT('Ctrl Pts',(-5.47651550000006,15.2,-9.19842468800002));
#287689=CARTESIAN_POINT('Ctrl Pts',(-5.47716846700006,15.2,-9.20075341100001));
#287690=CARTESIAN_POINT('Ctrl Pts',(-5.47782110600005,15.2,-9.20308875400002));
#287691=CARTESIAN_POINT('Ctrl Pts',(-5.47847340700006,15.2,-9.20543070800001));
#287692=CARTESIAN_POINT('Ctrl Pts',(-5.47912535700006,15.2,-9.20777926500002));
#287693=CARTESIAN_POINT('Ctrl Pts',(-5.47977694300006,15.2,-9.21013441500002));
#287694=CARTESIAN_POINT('Ctrl Pts',(-5.48042815200006,15.2,-9.21249614700002));
#287695=CARTESIAN_POINT('Ctrl Pts',(-5.48107897400006,15.2,-9.21486445500001));
#287696=CARTESIAN_POINT('Ctrl Pts',(-5.48172939300006,15.2,-9.21723932700001));
#287697=CARTESIAN_POINT('Ctrl Pts',(-5.48237940000006,15.2,-9.21962075500002));
#287698=CARTESIAN_POINT('Ctrl Pts',(-5.48302898100006,15.2,-9.22200872900002));
#287699=CARTESIAN_POINT('Ctrl Pts',(-5.48367812400006,15.2,-9.22440324100002));
#287700=CARTESIAN_POINT('Ctrl Pts',(-5.48432681600006,15.2,-9.22680428100002));
#287701=CARTESIAN_POINT('Ctrl Pts',(-5.48497504600006,15.2,-9.22921183900002));
#287702=CARTESIAN_POINT('Ctrl Pts',(-5.48562280200006,15.2,-9.23162590700001));
#287703=CARTESIAN_POINT('Ctrl Pts',(-5.48627007100006,15.2,-9.23404647600002));
#287704=CARTESIAN_POINT('Ctrl Pts',(-5.48691684200006,15.2,-9.23647353500002));
#287705=CARTESIAN_POINT('Ctrl Pts',(-5.48756310200006,15.2,-9.23890707800001));
#287706=CARTESIAN_POINT('Ctrl Pts',(-5.48820883900006,15.2,-9.24134709400001));
#287707=CARTESIAN_POINT('Ctrl Pts',(-5.48885404200006,15.2,-9.24379357300002));
#287708=CARTESIAN_POINT('Ctrl Pts',(-5.48949869800006,15.2,-9.24624650800002));
#287709=CARTESIAN_POINT('Ctrl Pts',(-5.49014279600006,15.2,-9.24870588900001));
#287710=CARTESIAN_POINT('Ctrl Pts',(-5.49078632300006,15.2,-9.25117170600002));
#287711=CARTESIAN_POINT('Ctrl Pts',(-5.49142927000006,15.2,-9.25364395200001));
#287712=CARTESIAN_POINT('Ctrl Pts',(-5.49207162100006,15.2,-9.25612261600002));
#287713=CARTESIAN_POINT('Ctrl Pts',(-5.49271336800006,15.2,-9.25860769100002));
#287714=CARTESIAN_POINT('Ctrl Pts',(-5.49335449800005,15.2,-9.26109916700002));
#287715=CARTESIAN_POINT('Ctrl Pts',(-5.49399499900006,15.2,-9.26359703400001));
#287716=CARTESIAN_POINT('Ctrl Pts',(-5.49463485900006,15.2,-9.26610128400002));
#287717=CARTESIAN_POINT('Ctrl Pts',(-5.49527406800006,15.2,-9.26861190900001));
#287718=CARTESIAN_POINT('Ctrl Pts',(-5.49591261300006,15.2,-9.27112889800001));
#287719=CARTESIAN_POINT('Ctrl Pts',(-5.49655048300006,15.2,-9.27365224400001));
#287720=CARTESIAN_POINT('Ctrl Pts',(-5.49718766700006,15.2,-9.27618193800001));
#287721=CARTESIAN_POINT('Ctrl Pts',(-5.49782415300006,15.2,-9.27871797000002));
#287722=CARTESIAN_POINT('Ctrl Pts',(-5.49845993000006,15.2,-9.28126033100002));
#287723=CARTESIAN_POINT('Ctrl Pts',(-5.49909498700006,15.2,-9.28380901500002));
#287724=CARTESIAN_POINT('Ctrl Pts',(-5.49972931200006,15.2,-9.28636401000002));
#287725=CARTESIAN_POINT('Ctrl Pts',(-5.50036289400006,15.2,-9.28892530800002));
#287726=CARTESIAN_POINT('Ctrl Pts',(-5.50099572200006,15.2,-9.29149290000002));
#287727=CARTESIAN_POINT('Ctrl Pts',(-5.50162778400006,15.2,-9.29406678000002));
#287728=CARTESIAN_POINT('Ctrl Pts',(-5.50225906900006,15.2,-9.29664693400002));
#287729=CARTESIAN_POINT('Ctrl Pts',(-5.50288956700006,15.2,-9.29923335800002));
#287730=CARTESIAN_POINT('Ctrl Pts',(-5.50351926700006,15.2,-9.30182604100001));
#287731=CARTESIAN_POINT('Ctrl Pts',(-5.50414815600006,15.2,-9.30442497500002));
#287732=CARTESIAN_POINT('Ctrl Pts',(-5.50477622400006,15.2,-9.30703015100002));
#287733=CARTESIAN_POINT('Ctrl Pts',(-5.50540346100005,15.2,-9.30964156000002));
#287734=CARTESIAN_POINT('Ctrl Pts',(-5.50602985400006,15.2,-9.31225919400001));
#287735=CARTESIAN_POINT('Ctrl Pts',(-5.50665539400006,15.2,-9.31488304500002));
#287736=CARTESIAN_POINT('Ctrl Pts',(-5.50728006900005,15.2,-9.31751310200001));
#287737=CARTESIAN_POINT('Ctrl Pts',(-5.50790386900006,15.2,-9.32014935900002));
#287738=CARTESIAN_POINT('Ctrl Pts',(-5.50852678200005,15.2,-9.32279180500002));
#287739=CARTESIAN_POINT('Ctrl Pts',(-5.50914879900006,15.2,-9.32544043300001));
#287740=CARTESIAN_POINT('Ctrl Pts',(-5.50976990800006,15.2,-9.32809523400002));
#287741=CARTESIAN_POINT('Ctrl Pts',(-5.51039009700006,15.2,-9.33075620000002));
#287742=CARTESIAN_POINT('Ctrl Pts',(-5.51100935800005,15.2,-9.33342332100001));
#287743=CARTESIAN_POINT('Ctrl Pts',(-5.51162767900006,15.2,-9.33609659000001));
#287744=CARTESIAN_POINT('Ctrl Pts',(-5.51224505000006,15.2,-9.33877599700002));
#287745=CARTESIAN_POINT('Ctrl Pts',(-5.51286145900006,15.2,-9.34146153400001));
#287746=CARTESIAN_POINT('Ctrl Pts',(-5.51347689600005,15.2,-9.34415319400001));
#287747=CARTESIAN_POINT('Ctrl Pts',(-5.51409135300006,15.2,-9.34685096600001));
#287748=CARTESIAN_POINT('Ctrl Pts',(-5.51470481600006,15.2,-9.34955484400002));
#287749=CARTESIAN_POINT('Ctrl Pts',(-5.51531727600006,15.2,-9.35226481800001));
#287750=CARTESIAN_POINT('Ctrl Pts',(-5.51592872200006,15.2,-9.35498087900001));
#287751=CARTESIAN_POINT('Ctrl Pts',(-5.51653914500006,15.2,-9.35770301900002));
#287752=CARTESIAN_POINT('Ctrl Pts',(-5.51714853300005,15.2,-9.36043123200001));
#287753=CARTESIAN_POINT('Ctrl Pts',(-5.51775687700006,15.2,-9.36316550500001));
#287754=CARTESIAN_POINT('Ctrl Pts',(-5.51836416700006,15.2,-9.36590583500001));
#287755=CARTESIAN_POINT('Ctrl Pts',(-5.51897039000006,15.2,-9.36865220900001));
#287756=CARTESIAN_POINT('Ctrl Pts',(-5.51957553900006,15.2,-9.37140462000002));
#287757=CARTESIAN_POINT('Ctrl Pts',(-5.52017960200006,15.2,-9.37416306100002));
#287758=CARTESIAN_POINT('Ctrl Pts',(-5.52078257000006,15.2,-9.37692752200002));
#287759=CARTESIAN_POINT('Ctrl Pts',(-5.52138443200006,15.2,-9.37969799600002));
#287760=CARTESIAN_POINT('Ctrl Pts',(-5.52198517700006,15.2,-9.38247447400002));
#287761=CARTESIAN_POINT('Ctrl Pts',(-5.52258479700006,15.2,-9.38525694700001));
#287762=CARTESIAN_POINT('Ctrl Pts',(-5.52318328100006,15.2,-9.38804540800002));
#287763=CARTESIAN_POINT('Ctrl Pts',(-5.52378061800006,15.2,-9.39083984800002));
#287764=CARTESIAN_POINT('Ctrl Pts',(-5.52437679900006,15.2,-9.39364025800002));
#287765=CARTESIAN_POINT('Ctrl Pts',(-5.52497181400006,15.2,-9.39644663300001));
#287766=CARTESIAN_POINT('Ctrl Pts',(-5.52556565400006,15.2,-9.39925896000002));
#287767=CARTESIAN_POINT('Ctrl Pts',(-5.52615830800006,15.2,-9.40207723400002));
#287768=CARTESIAN_POINT('Ctrl Pts',(-5.52674976600006,15.2,-9.40490144500002));
#287769=CARTESIAN_POINT('Ctrl Pts',(-5.52734001800006,15.2,-9.40773158700001));
#287770=CARTESIAN_POINT('Ctrl Pts',(-5.52792905500006,15.2,-9.41056764900001));
#287771=CARTESIAN_POINT('Ctrl Pts',(-5.52851686600006,15.2,-9.41340962500002));
#287772=CARTESIAN_POINT('Ctrl Pts',(-5.52910344300006,15.2,-9.41625750600002));
#287773=CARTESIAN_POINT('Ctrl Pts',(-5.52968877600006,15.2,-9.41911128400001));
#287774=CARTESIAN_POINT('Ctrl Pts',(-5.53027285400006,15.2,-9.42197095100001));
#287775=CARTESIAN_POINT('Ctrl Pts',(-5.53085566800006,15.2,-9.42483649900002));
#287776=CARTESIAN_POINT('Ctrl Pts',(-5.53143720800006,15.2,-9.42770791800001));
#287777=CARTESIAN_POINT('Ctrl Pts',(-5.53213351757476,15.2,-9.43116065867457));
#287778=CARTESIAN_POINT('Ctrl Pts',(-5.53282788771271,15.2,-9.43462218366274));
#287779=CARTESIAN_POINT('Ctrl Pts',(-5.53352029828741,15.2,-9.43809247833729));
#287780=CARTESIAN_POINT('Ctrl Pts',(-5.53421073242535,15.2,-9.44157152332546));
#287781=CARTESIAN_POINT('Ctrl Pts',(-5.53489917000006,15.2,-9.44505930400002));
#287782=CARTESIAN_POINT('Ctrl Pts',(-5.53547152800006,15.2,-9.44797160400002));
#287783=CARTESIAN_POINT('Ctrl Pts',(-5.53604253700006,15.2,-9.45088971200001));
#287784=CARTESIAN_POINT('Ctrl Pts',(-5.53661218600006,15.2,-9.45381362000001));
#287785=CARTESIAN_POINT('Ctrl Pts',(-5.53718046800006,15.2,-9.45674332000002));
#287786=CARTESIAN_POINT('Ctrl Pts',(-5.53774737000006,15.2,-9.45967880400002));
#287787=CARTESIAN_POINT('Ctrl Pts',(-5.53831288800006,15.2,-9.46262006300002));
#287788=CARTESIAN_POINT('Ctrl Pts',(-5.53887700700006,15.2,-9.46556709000001));
#287789=CARTESIAN_POINT('Ctrl Pts',(-5.53943972200006,15.2,-9.46851987700001));
#287790=CARTESIAN_POINT('Ctrl Pts',(-5.54000102100006,15.2,-9.47147841500002));
#287791=CARTESIAN_POINT('Ctrl Pts',(-5.54056089800006,15.2,-9.47444269800001));
#287792=CARTESIAN_POINT('Ctrl Pts',(-5.54111934100006,15.2,-9.47741271600002));
#287793=CARTESIAN_POINT('Ctrl Pts',(-5.54167634100006,15.2,-9.48038846300001));
#287794=CARTESIAN_POINT('Ctrl Pts',(-5.54223189100005,15.2,-9.48336993000002));
#287795=CARTESIAN_POINT('Ctrl Pts',(-5.54278597900006,15.2,-9.48635710900002));
#287796=CARTESIAN_POINT('Ctrl Pts',(-5.54333859900006,15.2,-9.48934999200001));
#287797=CARTESIAN_POINT('Ctrl Pts',(-5.54388974000006,15.2,-9.49234857200001));
#287798=CARTESIAN_POINT('Ctrl Pts',(-5.54443939300006,15.2,-9.49535284000002));
#287799=CARTESIAN_POINT('Ctrl Pts',(-5.54498755000006,15.2,-9.49836278900002));
#287800=CARTESIAN_POINT('Ctrl Pts',(-5.54553420100006,15.2,-9.50137841100002));
#287801=CARTESIAN_POINT('Ctrl Pts',(-5.54607933800006,15.2,-9.50439969700002));
#287802=CARTESIAN_POINT('Ctrl Pts',(-5.54662295300006,15.2,-9.50742664100002));
#287803=CARTESIAN_POINT('Ctrl Pts',(-5.54716503400006,15.2,-9.51045923400001));
#287804=CARTESIAN_POINT('Ctrl Pts',(-5.54770557400006,15.2,-9.51349746900001));
#287805=CARTESIAN_POINT('Ctrl Pts',(-5.54824456500006,15.2,-9.51654133600002));
#287806=CARTESIAN_POINT('Ctrl Pts',(-5.54878199800006,15.2,-9.51959083100002));
#287807=CARTESIAN_POINT('Ctrl Pts',(-5.54931786200005,15.2,-9.52264594300001));
#287808=CARTESIAN_POINT('Ctrl Pts',(-5.54985215100006,15.2,-9.52570666600002));
#287809=CARTESIAN_POINT('Ctrl Pts',(-5.55038485500006,15.2,-9.52877299000002));
#287810=CARTESIAN_POINT('Ctrl Pts',(-5.55091596500006,15.2,-9.53184491000002));
#287811=CARTESIAN_POINT('Ctrl Pts',(-5.55144547200006,15.2,-9.53492241800001));
#287812=CARTESIAN_POINT('Ctrl Pts',(-5.55197337000005,15.2,-9.53800550400001));
#287813=CARTESIAN_POINT('Ctrl Pts',(-5.55249964700006,15.2,-9.54109416100002));
#287814=CARTESIAN_POINT('Ctrl Pts',(-5.55302429700006,15.2,-9.54418838400001));
#287815=CARTESIAN_POINT('Ctrl Pts',(-5.55354730900006,15.2,-9.54728816200002));
#287816=CARTESIAN_POINT('Ctrl Pts',(-5.55406867700006,15.2,-9.55039348800002));
#287817=CARTESIAN_POINT('Ctrl Pts',(-5.55458839100006,15.2,-9.55350435500002));
#287818=CARTESIAN_POINT('Ctrl Pts',(-5.55510644200006,15.2,-9.55662075600002));
#287819=CARTESIAN_POINT('Ctrl Pts',(-5.55562282200006,15.2,-9.55974268200002));
#287820=CARTESIAN_POINT('Ctrl Pts',(-5.55613752400006,15.2,-9.56287012600002));
#287821=CARTESIAN_POINT('Ctrl Pts',(-5.55665053700006,15.2,-9.56600308000001));
#287822=CARTESIAN_POINT('Ctrl Pts',(-5.55716185500006,15.2,-9.56914153600002));
#287823=CARTESIAN_POINT('Ctrl Pts',(-5.55767146700005,15.2,-9.57228548700002));
#287824=CARTESIAN_POINT('Ctrl Pts',(-5.55817936700006,15.2,-9.57543492600001));
#287825=CARTESIAN_POINT('Ctrl Pts',(-5.55868554700006,15.2,-9.57858984400002));
#287826=CARTESIAN_POINT('Ctrl Pts',(-5.55918999600006,15.2,-9.58175023500001));
#287827=CARTESIAN_POINT('Ctrl Pts',(-5.55969270800006,15.2,-9.58491608900001));
#287828=CARTESIAN_POINT('Ctrl Pts',(-5.56019367400006,15.2,-9.58808740000002));
#287829=CARTESIAN_POINT('Ctrl Pts',(-5.56069288500006,15.2,-9.59126416200002));
#287830=CARTESIAN_POINT('Ctrl Pts',(-5.56119033400006,15.2,-9.59444636500002));
#287831=CARTESIAN_POINT('Ctrl Pts',(-5.56168601200006,15.2,-9.59763400200002));
#287832=CARTESIAN_POINT('Ctrl Pts',(-5.56217991100006,15.2,-9.60082706600002));
#287833=CARTESIAN_POINT('Ctrl Pts',(-5.56267202400006,15.2,-9.60402554800002));
#287834=CARTESIAN_POINT('Ctrl Pts',(-5.56316234000006,15.2,-9.60722944300001));
#287835=CARTESIAN_POINT('Ctrl Pts',(-5.56365085400006,15.2,-9.61043874100002));
#287836=CARTESIAN_POINT('Ctrl Pts',(-5.56413755700006,15.2,-9.61365343600002));
#287837=CARTESIAN_POINT('Ctrl Pts',(-5.56462243900006,15.2,-9.61687352000002));
#287838=CARTESIAN_POINT('Ctrl Pts',(-5.56510549500006,15.2,-9.62009898500002));
#287839=CARTESIAN_POINT('Ctrl Pts',(-5.56558671400006,15.2,-9.62332982500002));
#287840=CARTESIAN_POINT('Ctrl Pts',(-5.56606609100006,15.2,-9.62656603200001));
#287841=CARTESIAN_POINT('Ctrl Pts',(-5.56654361600006,15.2,-9.62980759800002));
#287842=CARTESIAN_POINT('Ctrl Pts',(-5.56701928100006,15.2,-9.63305451500002));
#287843=CARTESIAN_POINT('Ctrl Pts',(-5.56749308000006,15.2,-9.63630677700002));
#287844=CARTESIAN_POINT('Ctrl Pts',(-5.56796500300006,15.2,-9.63956437500002));
#287845=CARTESIAN_POINT('Ctrl Pts',(-5.56843504200006,15.2,-9.64282730200001));
#287846=CARTESIAN_POINT('Ctrl Pts',(-5.56890319100006,15.2,-9.64609555300001));
#287847=CARTESIAN_POINT('Ctrl Pts',(-5.56936944100006,15.2,-9.64936911600002));
#287848=CARTESIAN_POINT('Ctrl Pts',(-5.56983378400006,15.2,-9.65264798800001));
#287849=CARTESIAN_POINT('Ctrl Pts',(-5.57029621300006,15.2,-9.65593215900001));
#287850=CARTESIAN_POINT('Ctrl Pts',(-5.57075671900006,15.2,-9.65922162300001));
#287851=CARTESIAN_POINT('Ctrl Pts',(-5.57121529500006,15.2,-9.66251637100001));
#287852=CARTESIAN_POINT('Ctrl Pts',(-5.57167193400006,15.2,-9.66581639800001));
#287853=CARTESIAN_POINT('Ctrl Pts',(-5.57212662700006,15.2,-9.66912169500001));
#287854=CARTESIAN_POINT('Ctrl Pts',(-5.57257936700006,15.2,-9.67243225400001));
#287855=CARTESIAN_POINT('Ctrl Pts',(-5.57303014600006,15.2,-9.67574807000001));
#287856=CARTESIAN_POINT('Ctrl Pts',(-5.57347895600006,15.2,-9.67906913300001));
#287857=CARTESIAN_POINT('Ctrl Pts',(-5.57392579000005,15.2,-9.68239543700001));
#287858=CARTESIAN_POINT('Ctrl Pts',(-5.57437064100006,15.2,-9.68572697500001));
#287859=CARTESIAN_POINT('Ctrl Pts',(-5.57481350100006,15.2,-9.68906373900001));
#287860=CARTESIAN_POINT('Ctrl Pts',(-5.57525436100006,15.2,-9.69240572200001));
#287861=CARTESIAN_POINT('Ctrl Pts',(-5.57569321500006,15.2,-9.69575291700002));
#287862=CARTESIAN_POINT('Ctrl Pts',(-5.57613005500006,15.2,-9.69910531700001));
#287863=CARTESIAN_POINT('Ctrl Pts',(-5.57656487300005,15.2,-9.70246291300001));
#287864=CARTESIAN_POINT('Ctrl Pts',(-5.57699766300006,15.2,-9.70582570000001));
#287865=CARTESIAN_POINT('Ctrl Pts',(-5.57742841600006,15.2,-9.70919366800001));
#287866=CARTESIAN_POINT('Ctrl Pts',(-5.57785712500006,15.2,-9.71256681200001));
#287867=CARTESIAN_POINT('Ctrl Pts',(-5.57828378300006,15.2,-9.71594512400001));
#287868=CARTESIAN_POINT('Ctrl Pts',(-5.57870838200006,15.2,-9.71932859700001));
#287869=CARTESIAN_POINT('Ctrl Pts',(-5.57913091500006,15.2,-9.72271722400001));
#287870=CARTESIAN_POINT('Ctrl Pts',(-5.57955137400006,15.2,-9.72611099700002));
#287871=CARTESIAN_POINT('Ctrl Pts',(-5.57996975300005,15.2,-9.72950991000001));
#287872=CARTESIAN_POINT('Ctrl Pts',(-5.58038604400006,15.2,-9.73291395500001));
#287873=CARTESIAN_POINT('Ctrl Pts',(-5.58080023800006,15.2,-9.73632312400001));
#287874=CARTESIAN_POINT('Ctrl Pts',(-5.58121233100006,15.2,-9.73973741000002));
#287875=CARTESIAN_POINT('Ctrl Pts',(-5.58162231200006,15.2,-9.74315680800001));
#287876=CARTESIAN_POINT('Ctrl Pts',(-5.58203017800006,15.2,-9.74658130900002));
#287877=CARTESIAN_POINT('Ctrl Pts',(-5.58243591800006,15.2,-9.75001090500001));
#287878=CARTESIAN_POINT('Ctrl Pts',(-5.58283952600005,15.2,-9.75344559000001));
#287879=CARTESIAN_POINT('Ctrl Pts',(-5.58324099600005,15.2,-9.75688535700001));
#287880=CARTESIAN_POINT('Ctrl Pts',(-5.58364031900005,15.2,-9.76033019900001));
#287881=CARTESIAN_POINT('Ctrl Pts',(-5.58403748900006,15.2,-9.76378010900001));
#287882=CARTESIAN_POINT('Ctrl Pts',(-5.58443250000006,15.2,-9.76723507800001));
#287883=CARTESIAN_POINT('Ctrl Pts',(-5.58482534200006,15.2,-9.77069510100001));
#287884=CARTESIAN_POINT('Ctrl Pts',(-5.58521601000006,15.2,-9.77416017100001));
#287885=CARTESIAN_POINT('Ctrl Pts',(-5.58560449700006,15.2,-9.77763027800002));
#287886=CARTESIAN_POINT('Ctrl Pts',(-5.58599079400006,15.2,-9.78110541800001));
#287887=CARTESIAN_POINT('Ctrl Pts',(-5.58637489600006,15.2,-9.78458558300001));
#287888=CARTESIAN_POINT('Ctrl Pts',(-5.58675679500006,15.2,-9.78807076600001));
#287889=CARTESIAN_POINT('Ctrl Pts',(-5.58713648300006,15.2,-9.79156095800001));
#287890=CARTESIAN_POINT('Ctrl Pts',(-5.58751395600006,15.2,-9.79505615600001));
#287891=CARTESIAN_POINT('Ctrl Pts',(-5.58788920500006,15.2,-9.79855634900001));
#287892=CARTESIAN_POINT('Ctrl Pts',(-5.58826222200006,15.2,-9.80206153200001));
#287893=CARTESIAN_POINT('Ctrl Pts',(-5.58863300300006,15.2,-9.80557169700001));
#287894=CARTESIAN_POINT('Ctrl Pts',(-5.58900153800006,15.2,-9.80908683700001));
#287895=CARTESIAN_POINT('Ctrl Pts',(-5.58936782300006,15.2,-9.81260694600001));
#287896=CARTESIAN_POINT('Ctrl Pts',(-5.58973184900006,15.2,-9.81613201700001));
#287897=CARTESIAN_POINT('Ctrl Pts',(-5.59009361000006,15.2,-9.81966204100001));
#287898=CARTESIAN_POINT('Ctrl Pts',(-5.59045309900006,15.2,-9.82319701200001));
#287899=CARTESIAN_POINT('Ctrl Pts',(-5.59081030900006,15.2,-9.82673692500001));
#287900=CARTESIAN_POINT('Ctrl Pts',(-5.59116523300006,15.2,-9.83028176900001));
#287901=CARTESIAN_POINT('Ctrl Pts',(-5.59151786600006,15.2,-9.83383154100001));
#287902=CARTESIAN_POINT('Ctrl Pts',(-5.59186819900006,15.2,-9.83738623200001));
#287903=CARTESIAN_POINT('Ctrl Pts',(-5.59221622500006,15.2,-9.84094583600001));
#287904=CARTESIAN_POINT('Ctrl Pts',(-5.59256194100006,15.2,-9.84451034500001));
#287905=CARTESIAN_POINT('Ctrl Pts',(-5.59290533600006,15.2,-9.84807975100001));
#287906=CARTESIAN_POINT('Ctrl Pts',(-5.59324640500006,15.2,-9.85165405000001));
#287907=CARTESIAN_POINT('Ctrl Pts',(-5.59358514100006,15.2,-9.85523323300001));
#287908=CARTESIAN_POINT('Ctrl Pts',(-5.59392153800006,15.2,-9.85881729400001));
#287909=CARTESIAN_POINT('Ctrl Pts',(-5.59425559000006,15.2,-9.86240622500001));
#287910=CARTESIAN_POINT('Ctrl Pts',(-5.59458728700006,15.2,-9.86600002000001));
#287911=CARTESIAN_POINT('Ctrl Pts',(-5.59491662700006,15.2,-9.86959867100001));
#287912=CARTESIAN_POINT('Ctrl Pts',(-5.59524360000006,15.2,-9.87320217300001));
#287913=CARTESIAN_POINT('Ctrl Pts',(-5.59556820200006,15.2,-9.87681051700001));
#287914=CARTESIAN_POINT('Ctrl Pts',(-5.59589042400006,15.2,-9.88042369800001));
#287915=CARTESIAN_POINT('Ctrl Pts',(-5.59621026000006,15.2,-9.88404170800001));
#287916=CARTESIAN_POINT('Ctrl Pts',(-5.59652770400006,15.2,-9.88766454000001));
#287917=CARTESIAN_POINT('Ctrl Pts',(-5.59684275000006,15.2,-9.89129218700001));
#287918=CARTESIAN_POINT('Ctrl Pts',(-5.59715539100006,15.2,-9.89492464200001));
#287919=CARTESIAN_POINT('Ctrl Pts',(-5.59746562000006,15.2,-9.89856190000001));
#287920=CARTESIAN_POINT('Ctrl Pts',(-5.59777343200006,15.2,-9.90220395300001));
#287921=CARTESIAN_POINT('Ctrl Pts',(-5.59807881900006,15.2,-9.90585079300001));
#287922=CARTESIAN_POINT('Ctrl Pts',(-5.59838177600006,15.2,-9.90950241400001));
#287923=CARTESIAN_POINT('Ctrl Pts',(-5.59868229500006,15.2,-9.91315881000001));
#287924=CARTESIAN_POINT('Ctrl Pts',(-5.59898037100006,15.2,-9.91681997300001));
#287925=CARTESIAN_POINT('Ctrl Pts',(-5.59927599700006,15.2,-9.92048589600001));
#287926=CARTESIAN_POINT('Ctrl Pts',(-5.59956916600005,15.2,-9.92415657400001));
#287927=CARTESIAN_POINT('Ctrl Pts',(-5.59985987300006,15.2,-9.92783199800001));
#287928=CARTESIAN_POINT('Ctrl Pts',(-5.60014811000006,15.2,-9.93151216200001));
#287929=CARTESIAN_POINT('Ctrl Pts',(-5.60043387200006,15.2,-9.93519706000001));
#287930=CARTESIAN_POINT('Ctrl Pts',(-5.60071715300006,15.2,-9.93888668300001));
#287931=CARTESIAN_POINT('Ctrl Pts',(-5.60099794600006,15.2,-9.94258102700002));
#287932=CARTESIAN_POINT('Ctrl Pts',(-5.60127624500006,15.2,-9.94628008400001));
#287933=CARTESIAN_POINT('Ctrl Pts',(-5.60155204400006,15.2,-9.94998384700001));
#287934=CARTESIAN_POINT('Ctrl Pts',(-5.60182533700006,15.2,-9.95369231100001));
#287935=CARTESIAN_POINT('Ctrl Pts',(-5.60209611700006,15.2,-9.95740546800001));
#287936=CARTESIAN_POINT('Ctrl Pts',(-5.60236437800006,15.2,-9.96112330900001));
#287937=CARTESIAN_POINT('Ctrl Pts',(-5.60263011400005,15.2,-9.96484583000001));
#287938=CARTESIAN_POINT('Ctrl Pts',(-5.60289331800006,15.2,-9.96857302300001));
#287939=CARTESIAN_POINT('Ctrl Pts',(-5.60315398400006,15.2,-9.97230488000001));
#287940=CARTESIAN_POINT('Ctrl Pts',(-5.60341210500006,15.2,-9.97604139500002));
#287941=CARTESIAN_POINT('Ctrl Pts',(-5.60366767700006,15.2,-9.97978256300001));
#287942=CARTESIAN_POINT('Ctrl Pts',(-5.60392069300006,15.2,-9.98352837700001));
#287943=CARTESIAN_POINT('Ctrl Pts',(-5.60417114800006,15.2,-9.98727882900001));
#287944=CARTESIAN_POINT('Ctrl Pts',(-5.60441903700006,15.2,-9.99103391600001));
#287945=CARTESIAN_POINT('Ctrl Pts',(-5.60466435400006,15.2,-9.99479363100001));
#287946=CARTESIAN_POINT('Ctrl Pts',(-5.60490709200006,15.2,-9.99855796400001));
#287947=CARTESIAN_POINT('Ctrl Pts',(-5.60514724500006,15.2,-10.002326912));
#287948=CARTESIAN_POINT('Ctrl Pts',(-5.60538480400006,15.2,-10.006100463));
#287949=CARTESIAN_POINT('Ctrl Pts',(-5.60561976300006,15.2,-10.00987861));
#287950=CARTESIAN_POINT('Ctrl Pts',(-5.60585211500006,15.2,-10.013661344));
#287951=CARTESIAN_POINT('Ctrl Pts',(-5.60608185300006,15.2,-10.01744866));
#287952=CARTESIAN_POINT('Ctrl Pts',(-5.60630897000006,15.2,-10.02124055));
#287953=CARTESIAN_POINT('Ctrl Pts',(-5.60653346400006,15.2,-10.025037011));
#287954=CARTESIAN_POINT('Ctrl Pts',(-5.60675533300006,15.2,-10.028838039));
#287955=CARTESIAN_POINT('Ctrl Pts',(-5.60697457300006,15.2,-10.032643631));
#287956=CARTESIAN_POINT('Ctrl Pts',(-5.60714786300006,15.2,-10.035691757));
#287957=CARTESIAN_POINT('Ctrl Pts',(-5.60727664800006,15.2,-10.037979904));
#287958=CARTESIAN_POINT('Ctrl Pts',(-5.60736197900006,15.2,-10.039506249));
#287959=CARTESIAN_POINT('Ctrl Pts',(-5.60740451300005,15.2,-10.040269649));
#287960=CARTESIAN_POINT('Ctrl Pts',(-5.36127880600006,12.2,-8.88241603200001));
#287961=CARTESIAN_POINT('Ctrl Pts',(-5.36135574400006,12.2,-8.88257249600001));
#287962=CARTESIAN_POINT('Ctrl Pts',(-5.36151222900005,12.2,-8.88289092900001));
#287963=CARTESIAN_POINT('Ctrl Pts',(-5.36174910400006,12.2,-8.88337354800001));
#287964=CARTESIAN_POINT('Ctrl Pts',(-5.36206771100006,12.2,-8.88402391700001));
#287965=CARTESIAN_POINT('Ctrl Pts',(-5.36246988000006,12.2,-8.88484693800002));
#287966=CARTESIAN_POINT('Ctrl Pts',(-5.36287772900006,12.2,-8.88568371000002));
#287967=CARTESIAN_POINT('Ctrl Pts',(-5.36328889700005,12.2,-8.88652944600001));
#287968=CARTESIAN_POINT('Ctrl Pts',(-5.36370335800005,12.2,-8.88738413200001));
#287969=CARTESIAN_POINT('Ctrl Pts',(-5.36412108300006,12.2,-8.88824775000002));
#287970=CARTESIAN_POINT('Ctrl Pts',(-5.36454204500005,12.2,-8.88912028400001));
#287971=CARTESIAN_POINT('Ctrl Pts',(-5.36496621600006,12.2,-8.89000172000001));
#287972=CARTESIAN_POINT('Ctrl Pts',(-5.36539356700006,12.2,-8.89089203900001));
#287973=CARTESIAN_POINT('Ctrl Pts',(-5.36582407300005,12.2,-8.89179122800002));
#287974=CARTESIAN_POINT('Ctrl Pts',(-5.36625770500006,12.2,-8.89269926800001));
#287975=CARTESIAN_POINT('Ctrl Pts',(-5.36669443700006,12.2,-8.89361614500002));
#287976=CARTESIAN_POINT('Ctrl Pts',(-5.36713424100006,12.2,-8.89454184300002));
#287977=CARTESIAN_POINT('Ctrl Pts',(-5.36757709000006,12.2,-8.89547634600002));
#287978=CARTESIAN_POINT('Ctrl Pts',(-5.36802295900006,12.2,-8.89641963800001));
#287979=CARTESIAN_POINT('Ctrl Pts',(-5.36847181900006,12.2,-8.89737170400002));
#287980=CARTESIAN_POINT('Ctrl Pts',(-5.36892364700006,12.2,-8.89833252800001));
#287981=CARTESIAN_POINT('Ctrl Pts',(-5.36937841200006,12.2,-8.89930209500001));
#287982=CARTESIAN_POINT('Ctrl Pts',(-5.36983609200006,12.2,-8.90028038900001));
#287983=CARTESIAN_POINT('Ctrl Pts',(-5.37029665900006,12.2,-8.90126739500002));
#287984=CARTESIAN_POINT('Ctrl Pts',(-5.37076008700006,12.2,-8.90226309800001));
#287985=CARTESIAN_POINT('Ctrl Pts',(-5.37122635100006,12.2,-8.90326748100001));
#287986=CARTESIAN_POINT('Ctrl Pts',(-5.37169542500005,12.2,-8.90428053100001));
#287987=CARTESIAN_POINT('Ctrl Pts',(-5.37216728300006,12.2,-8.90530223200001));
#287988=CARTESIAN_POINT('Ctrl Pts',(-5.37264189900006,12.2,-8.90633257000001));
#287989=CARTESIAN_POINT('Ctrl Pts',(-5.37311925100005,12.2,-8.90737152700002));
#287990=CARTESIAN_POINT('Ctrl Pts',(-5.37359931100006,12.2,-8.90841909100001));
#287991=CARTESIAN_POINT('Ctrl Pts',(-5.37408205300006,12.2,-8.90947524700002));
#287992=CARTESIAN_POINT('Ctrl Pts',(-5.37456745500006,12.2,-8.91053997800002));
#287993=CARTESIAN_POINT('Ctrl Pts',(-5.37505549100006,12.2,-8.91161327200001));
#287994=CARTESIAN_POINT('Ctrl Pts',(-5.37554613600006,12.2,-8.91269511100001));
#287995=CARTESIAN_POINT('Ctrl Pts',(-5.37603936500005,12.2,-8.91378548300001));
#287996=CARTESIAN_POINT('Ctrl Pts',(-5.37653515500006,12.2,-8.91488437200002));
#287997=CARTESIAN_POINT('Ctrl Pts',(-5.37703348100006,12.2,-8.91599176500002));
#287998=CARTESIAN_POINT('Ctrl Pts',(-5.37753431800006,12.2,-8.91710764600001));
#287999=CARTESIAN_POINT('Ctrl Pts',(-5.37803764200006,12.2,-8.91823200100001));
#288000=CARTESIAN_POINT('Ctrl Pts',(-5.37854343200006,12.2,-8.91936481500002));
#288001=CARTESIAN_POINT('Ctrl Pts',(-5.37905166000006,12.2,-8.92050607500002));
#288002=CARTESIAN_POINT('Ctrl Pts',(-5.37956230500006,12.2,-8.92165576600001));
#288003=CARTESIAN_POINT('Ctrl Pts',(-5.38007534200006,12.2,-8.92281387300002));
#288004=CARTESIAN_POINT('Ctrl Pts',(-5.38059074800006,12.2,-8.92398038200002));
#288005=CARTESIAN_POINT('Ctrl Pts',(-5.38110850100006,12.2,-8.92515528100001));
#288006=CARTESIAN_POINT('Ctrl Pts',(-5.38162857400006,12.2,-8.92633855400002));
#288007=CARTESIAN_POINT('Ctrl Pts',(-5.38215094700006,12.2,-8.92753018600001));
#288008=CARTESIAN_POINT('Ctrl Pts',(-5.38267559700006,12.2,-8.92873016600002));
#288009=CARTESIAN_POINT('Ctrl Pts',(-5.38320250000006,12.2,-8.92993847700001));
#288010=CARTESIAN_POINT('Ctrl Pts',(-5.38373163200006,12.2,-8.93115510700002));
#288011=CARTESIAN_POINT('Ctrl Pts',(-5.38426297200005,12.2,-8.93238004100001));
#288012=CARTESIAN_POINT('Ctrl Pts',(-5.38479649700006,12.2,-8.93361326700001));
#288013=CARTESIAN_POINT('Ctrl Pts',(-5.38533218400006,12.2,-8.93485477000001));
#288014=CARTESIAN_POINT('Ctrl Pts',(-5.38587001200006,12.2,-8.93610453600001));
#288015=CARTESIAN_POINT('Ctrl Pts',(-5.38640995700006,12.2,-8.93736255200002));
#288016=CARTESIAN_POINT('Ctrl Pts',(-5.38695199800006,12.2,-8.93862880300002));
#288017=CARTESIAN_POINT('Ctrl Pts',(-5.38749611100005,12.2,-8.93990327800001));
#288018=CARTESIAN_POINT('Ctrl Pts',(-5.38804227600005,12.2,-8.94118596000002));
#288019=CARTESIAN_POINT('Ctrl Pts',(-5.38859046900006,12.2,-8.94247684000002));
#288020=CARTESIAN_POINT('Ctrl Pts',(-5.38914067100006,12.2,-8.94377590100002));
#288021=CARTESIAN_POINT('Ctrl Pts',(-5.38969285900006,12.2,-8.94508313100001));
#288022=CARTESIAN_POINT('Ctrl Pts',(-5.39024701000006,12.2,-8.94639851600001));
#288023=CARTESIAN_POINT('Ctrl Pts',(-5.39080310300006,12.2,-8.94772204400001));
#288024=CARTESIAN_POINT('Ctrl Pts',(-5.39136111800006,12.2,-8.94905370100001));
#288025=CARTESIAN_POINT('Ctrl Pts',(-5.39192103300006,12.2,-8.95039347300001));
#288026=CARTESIAN_POINT('Ctrl Pts',(-5.39248282700005,12.2,-8.95174134800002));
#288027=CARTESIAN_POINT('Ctrl Pts',(-5.39304647700006,12.2,-8.95309731200001));
#288028=CARTESIAN_POINT('Ctrl Pts',(-5.39361196500006,12.2,-8.95446135300002));
#288029=CARTESIAN_POINT('Ctrl Pts',(-5.39417926700006,12.2,-8.95583345700001));
#288030=CARTESIAN_POINT('Ctrl Pts',(-5.39474836400006,12.2,-8.95721361200001));
#288031=CARTESIAN_POINT('Ctrl Pts',(-5.39531923500006,12.2,-8.95860180500001));
#288032=CARTESIAN_POINT('Ctrl Pts',(-5.39589185800006,12.2,-8.95999802100001));
#288033=CARTESIAN_POINT('Ctrl Pts',(-5.39646621500006,12.2,-8.96140225000002));
#288034=CARTESIAN_POINT('Ctrl Pts',(-5.39704228400006,12.2,-8.96281447600002));
#288035=CARTESIAN_POINT('Ctrl Pts',(-5.39762004300006,12.2,-8.96423469000002));
#288036=CARTESIAN_POINT('Ctrl Pts',(-5.39819947500006,12.2,-8.96566287700002));
#288037=CARTESIAN_POINT('Ctrl Pts',(-5.39878055600005,12.2,-8.96709902300002));
#288038=CARTESIAN_POINT('Ctrl Pts',(-5.39936326900006,12.2,-8.96854312000002));
#288039=CARTESIAN_POINT('Ctrl Pts',(-5.39994759300006,12.2,-8.96999515000001));
#288040=CARTESIAN_POINT('Ctrl Pts',(-5.40053350800005,12.2,-8.97145510400001));
#288041=CARTESIAN_POINT('Ctrl Pts',(-5.40112099300006,12.2,-8.97292296800002));
#288042=CARTESIAN_POINT('Ctrl Pts',(-5.40171003000006,12.2,-8.97439872800001));
#288043=CARTESIAN_POINT('Ctrl Pts',(-5.40230059700006,12.2,-8.97588237500001));
#288044=CARTESIAN_POINT('Ctrl Pts',(-5.40289267700006,12.2,-8.97737389500002));
#288045=CARTESIAN_POINT('Ctrl Pts',(-5.40348624900005,12.2,-8.97887327500002));
#288046=CARTESIAN_POINT('Ctrl Pts',(-5.40408129300006,12.2,-8.98038050300002));
#288047=CARTESIAN_POINT('Ctrl Pts',(-5.40467779100006,12.2,-8.98189556700002));
#288048=CARTESIAN_POINT('Ctrl Pts',(-5.40527572300006,12.2,-8.98341845500001));
#288049=CARTESIAN_POINT('Ctrl Pts',(-5.40587507000006,12.2,-8.98494915300001));
#288050=CARTESIAN_POINT('Ctrl Pts',(-5.40647581300005,12.2,-8.98648765100001));
#288051=CARTESIAN_POINT('Ctrl Pts',(-5.40707793100006,12.2,-8.98803393600001));
#288052=CARTESIAN_POINT('Ctrl Pts',(-5.40768140800005,12.2,-8.98958799500001));
#288053=CARTESIAN_POINT('Ctrl Pts',(-5.40828622400006,12.2,-8.99114981800002));
#288054=CARTESIAN_POINT('Ctrl Pts',(-5.40889235900006,12.2,-8.99271939000002));
#288055=CARTESIAN_POINT('Ctrl Pts',(-5.40949979600006,12.2,-8.99429670100002));
#288056=CARTESIAN_POINT('Ctrl Pts',(-5.41010851400006,12.2,-8.99588173800002));
#288057=CARTESIAN_POINT('Ctrl Pts',(-5.41071849700006,12.2,-8.99747449100002));
#288058=CARTESIAN_POINT('Ctrl Pts',(-5.41132972500006,12.2,-8.99907494500002));
#288059=CARTESIAN_POINT('Ctrl Pts',(-5.41194218100006,12.2,-9.00068309100002));
#288060=CARTESIAN_POINT('Ctrl Pts',(-5.41255584400006,12.2,-9.00229891600001));
#288061=CARTESIAN_POINT('Ctrl Pts',(-5.41317069800006,12.2,-9.00392240700001));
#288062=CARTESIAN_POINT('Ctrl Pts',(-5.41378672400006,12.2,-9.00555355400002));
#288063=CARTESIAN_POINT('Ctrl Pts',(-5.41440390400005,12.2,-9.00719234400002));
#288064=CARTESIAN_POINT('Ctrl Pts',(-5.41502222100006,12.2,-9.00883876600002));
#288065=CARTESIAN_POINT('Ctrl Pts',(-5.41564165400006,12.2,-9.01049280800001));
#288066=CARTESIAN_POINT('Ctrl Pts',(-5.41626218800006,12.2,-9.01215445900002));
#288067=CARTESIAN_POINT('Ctrl Pts',(-5.41688380400006,12.2,-9.01382370600002));
#288068=CARTESIAN_POINT('Ctrl Pts',(-5.41750648400006,12.2,-9.01550053800002));
#288069=CARTESIAN_POINT('Ctrl Pts',(-5.41813021000006,12.2,-9.01718494400002));
#288070=CARTESIAN_POINT('Ctrl Pts',(-5.41875496600006,12.2,-9.01887691300002));
#288071=CARTESIAN_POINT('Ctrl Pts',(-5.41938073300006,12.2,-9.02057643200001));
#288072=CARTESIAN_POINT('Ctrl Pts',(-5.42000749500006,12.2,-9.02228349000002));
#288073=CARTESIAN_POINT('Ctrl Pts',(-5.42063523200006,12.2,-9.02399807600002));
#288074=CARTESIAN_POINT('Ctrl Pts',(-5.42126392900006,12.2,-9.02572017700002));
#288075=CARTESIAN_POINT('Ctrl Pts',(-5.42189356700006,12.2,-9.02744978400002));
#288076=CARTESIAN_POINT('Ctrl Pts',(-5.42252413200006,12.2,-9.02918688400002));
#288077=CARTESIAN_POINT('Ctrl Pts',(-5.42315560300006,12.2,-9.03093146700002));
#288078=CARTESIAN_POINT('Ctrl Pts',(-5.42378796400006,12.2,-9.03268352000002));
#288079=CARTESIAN_POINT('Ctrl Pts',(-5.42442119900006,12.2,-9.03444303200001));
#288080=CARTESIAN_POINT('Ctrl Pts',(-5.42505529100006,12.2,-9.03620999300001));
#288081=CARTESIAN_POINT('Ctrl Pts',(-5.42569022200006,12.2,-9.03798439200001));
#288082=CARTESIAN_POINT('Ctrl Pts',(-5.42632597500006,12.2,-9.03976621700001));
#288083=CARTESIAN_POINT('Ctrl Pts',(-5.42696253600006,12.2,-9.04155545600002));
#288084=CARTESIAN_POINT('Ctrl Pts',(-5.42759988400006,12.2,-9.04335209900001));
#288085=CARTESIAN_POINT('Ctrl Pts',(-5.42823800600006,12.2,-9.04515613500001));
#288086=CARTESIAN_POINT('Ctrl Pts',(-5.42887688500006,12.2,-9.04696755200002));
#288087=CARTESIAN_POINT('Ctrl Pts',(-5.42951650300005,12.2,-9.04878634000001));
#288088=CARTESIAN_POINT('Ctrl Pts',(-5.43015684400006,12.2,-9.05061248700001));
#288089=CARTESIAN_POINT('Ctrl Pts',(-5.43079789200006,12.2,-9.05244598400002));
#288090=CARTESIAN_POINT('Ctrl Pts',(-5.43143963200006,12.2,-9.05428681700002));
#288091=CARTESIAN_POINT('Ctrl Pts',(-5.43208204500006,12.2,-9.05613497700001));
#288092=CARTESIAN_POINT('Ctrl Pts',(-5.43272511700006,12.2,-9.05799045400002));
#288093=CARTESIAN_POINT('Ctrl Pts',(-5.43336883000006,12.2,-9.05985323500002));
#288094=CARTESIAN_POINT('Ctrl Pts',(-5.43401316900006,12.2,-9.06172331100001));
#288095=CARTESIAN_POINT('Ctrl Pts',(-5.43465811900006,12.2,-9.06360066900002));
#288096=CARTESIAN_POINT('Ctrl Pts',(-5.43530366400006,12.2,-9.06548530000002));
#288097=CARTESIAN_POINT('Ctrl Pts',(-5.43594978500006,12.2,-9.06737719300001));
#288098=CARTESIAN_POINT('Ctrl Pts',(-5.43659647000006,12.2,-9.06927633700001));
#288099=CARTESIAN_POINT('Ctrl Pts',(-5.43724370200006,12.2,-9.07118272100002));
#288100=CARTESIAN_POINT('Ctrl Pts',(-5.43789146400006,12.2,-9.07309633400001));
#288101=CARTESIAN_POINT('Ctrl Pts',(-5.43853974200006,12.2,-9.07501716600001));
#288102=CARTESIAN_POINT('Ctrl Pts',(-5.43918852000006,12.2,-9.07694520700002));
#288103=CARTESIAN_POINT('Ctrl Pts',(-5.43983778200006,12.2,-9.07888044600002));
#288104=CARTESIAN_POINT('Ctrl Pts',(-5.44048751200005,12.2,-9.08082287200001));
#288105=CARTESIAN_POINT('Ctrl Pts',(-5.44113769600005,12.2,-9.08277247400001));
#288106=CARTESIAN_POINT('Ctrl Pts',(-5.44178831900005,12.2,-9.08472924200002));
#288107=CARTESIAN_POINT('Ctrl Pts',(-5.44243936400005,12.2,-9.08669316600001));
#288108=CARTESIAN_POINT('Ctrl Pts',(-5.44309081700006,12.2,-9.08866423400001));
#288109=CARTESIAN_POINT('Ctrl Pts',(-5.44374266300006,12.2,-9.09064243800002));
#288110=CARTESIAN_POINT('Ctrl Pts',(-5.44439488400006,12.2,-9.09262776600002));
#288111=CARTESIAN_POINT('Ctrl Pts',(-5.44504746900006,12.2,-9.09462020700002));
#288112=CARTESIAN_POINT('Ctrl Pts',(-5.44570040100006,12.2,-9.09661975100001));
#288113=CARTESIAN_POINT('Ctrl Pts',(-5.44635366500006,12.2,-9.09862638900002));
#288114=CARTESIAN_POINT('Ctrl Pts',(-5.44700724700006,12.2,-9.10064010900001));
#288115=CARTESIAN_POINT('Ctrl Pts',(-5.44766113200006,12.2,-9.10266090100002));
#288116=CARTESIAN_POINT('Ctrl Pts',(-5.44831530400006,12.2,-9.10468875600002));
#288117=CARTESIAN_POINT('Ctrl Pts',(-5.44896974900006,12.2,-9.10672366200002));
#288118=CARTESIAN_POINT('Ctrl Pts',(-5.44962445200006,12.2,-9.10876561000002));
#288119=CARTESIAN_POINT('Ctrl Pts',(-5.45027939900006,12.2,-9.11081458800002));
#288120=CARTESIAN_POINT('Ctrl Pts',(-5.45093457600006,12.2,-9.11287058900001));
#288121=CARTESIAN_POINT('Ctrl Pts',(-5.45158996700006,12.2,-9.11493360000001));
#288122=CARTESIAN_POINT('Ctrl Pts',(-5.45224555800006,12.2,-9.11700361100002));
#288123=CARTESIAN_POINT('Ctrl Pts',(-5.45290133500006,12.2,-9.11908061300002));
#288124=CARTESIAN_POINT('Ctrl Pts',(-5.45355728400006,12.2,-9.12116459600002));
#288125=CARTESIAN_POINT('Ctrl Pts',(-5.45421338900006,12.2,-9.12325554900002));
#288126=CARTESIAN_POINT('Ctrl Pts',(-5.45486963700006,12.2,-9.12535346200002));
#288127=CARTESIAN_POINT('Ctrl Pts',(-5.45552601400006,12.2,-9.12745832600002));
#288128=CARTESIAN_POINT('Ctrl Pts',(-5.45618250500006,12.2,-9.12957013000002));
#288129=CARTESIAN_POINT('Ctrl Pts',(-5.45683909700006,12.2,-9.13168886400002));
#288130=CARTESIAN_POINT('Ctrl Pts',(-5.45749577500006,12.2,-9.13381451800002));
#288131=CARTESIAN_POINT('Ctrl Pts',(-5.45815252500006,12.2,-9.13594708400002));
#288132=CARTESIAN_POINT('Ctrl Pts',(-5.45880933300006,12.2,-9.13808654900001));
#288133=CARTESIAN_POINT('Ctrl Pts',(-5.45946618600006,12.2,-9.14023290400002));
#288134=CARTESIAN_POINT('Ctrl Pts',(-5.46012307000006,12.2,-9.14238614000002));
#288135=CARTESIAN_POINT('Ctrl Pts',(-5.46077997000006,12.2,-9.14454624700002));
#288136=CARTESIAN_POINT('Ctrl Pts',(-5.46143687300006,12.2,-9.14671321500002));
#288137=CARTESIAN_POINT('Ctrl Pts',(-5.46209376500006,12.2,-9.14888703300001));
#288138=CARTESIAN_POINT('Ctrl Pts',(-5.46275063300006,12.2,-9.15106769300002));
#288139=CARTESIAN_POINT('Ctrl Pts',(-5.46340746300006,12.2,-9.15325518400002));
#288140=CARTESIAN_POINT('Ctrl Pts',(-5.46406424000006,12.2,-9.15544949700001));
#288141=CARTESIAN_POINT('Ctrl Pts',(-5.46472095400006,12.2,-9.15765062100002));
#288142=CARTESIAN_POINT('Ctrl Pts',(-5.46537758800006,12.2,-9.15985854900002));
#288143=CARTESIAN_POINT('Ctrl Pts',(-5.46603413000006,12.2,-9.16207326700002));
#288144=CARTESIAN_POINT('Ctrl Pts',(-5.46669056700006,12.2,-9.16429476900002));
#288145=CARTESIAN_POINT('Ctrl Pts',(-5.46734688500006,12.2,-9.16652304400002));
#288146=CARTESIAN_POINT('Ctrl Pts',(-5.46800307000006,12.2,-9.16875808200002));
#288147=CARTESIAN_POINT('Ctrl Pts',(-5.46865911200006,12.2,-9.17099987400002));
#288148=CARTESIAN_POINT('Ctrl Pts',(-5.46931499300006,12.2,-9.17324841000001));
#288149=CARTESIAN_POINT('Ctrl Pts',(-5.46997070400006,12.2,-9.17550368100001));
#288150=CARTESIAN_POINT('Ctrl Pts',(-5.47062622900006,12.2,-9.17776567700002));
#288151=CARTESIAN_POINT('Ctrl Pts',(-5.47128155700006,12.2,-9.18003438700002));
#288152=CARTESIAN_POINT('Ctrl Pts',(-5.47193667400006,12.2,-9.18230980400002));
#288153=CARTESIAN_POINT('Ctrl Pts',(-5.47259156600005,12.2,-9.18459191700002));
#288154=CARTESIAN_POINT('Ctrl Pts',(-5.47324622200006,12.2,-9.18688071700002));
#288155=CARTESIAN_POINT('Ctrl Pts',(-5.47390062900006,12.2,-9.18917619500002));
#288156=CARTESIAN_POINT('Ctrl Pts',(-5.47455477300006,12.2,-9.19147833900002));
#288157=CARTESIAN_POINT('Ctrl Pts',(-5.47520864000006,12.2,-9.19378714300001));
#288158=CARTESIAN_POINT('Ctrl Pts',(-5.47586222100006,12.2,-9.19610259600002));
#288159=CARTESIAN_POINT('Ctrl Pts',(-5.47651550000006,12.2,-9.19842468800002));
#288160=CARTESIAN_POINT('Ctrl Pts',(-5.47716846700006,12.2,-9.20075341100001));
#288161=CARTESIAN_POINT('Ctrl Pts',(-5.47782110600005,12.2,-9.20308875400002));
#288162=CARTESIAN_POINT('Ctrl Pts',(-5.47847340700006,12.2,-9.20543070800001));
#288163=CARTESIAN_POINT('Ctrl Pts',(-5.47912535700006,12.2,-9.20777926500002));
#288164=CARTESIAN_POINT('Ctrl Pts',(-5.47977694300006,12.2,-9.21013441500002));
#288165=CARTESIAN_POINT('Ctrl Pts',(-5.48042815200006,12.2,-9.21249614700002));
#288166=CARTESIAN_POINT('Ctrl Pts',(-5.48107897400006,12.2,-9.21486445500001));
#288167=CARTESIAN_POINT('Ctrl Pts',(-5.48172939300006,12.2,-9.21723932700001));
#288168=CARTESIAN_POINT('Ctrl Pts',(-5.48237940000006,12.2,-9.21962075500002));
#288169=CARTESIAN_POINT('Ctrl Pts',(-5.48302898100006,12.2,-9.22200872900002));
#288170=CARTESIAN_POINT('Ctrl Pts',(-5.48367812400006,12.2,-9.22440324100002));
#288171=CARTESIAN_POINT('Ctrl Pts',(-5.48432681600006,12.2,-9.22680428100002));
#288172=CARTESIAN_POINT('Ctrl Pts',(-5.48497504600006,12.2,-9.22921183900002));
#288173=CARTESIAN_POINT('Ctrl Pts',(-5.48562280200006,12.2,-9.23162590700001));
#288174=CARTESIAN_POINT('Ctrl Pts',(-5.48627007100006,12.2,-9.23404647600002));
#288175=CARTESIAN_POINT('Ctrl Pts',(-5.48691684200006,12.2,-9.23647353500002));
#288176=CARTESIAN_POINT('Ctrl Pts',(-5.48756310200006,12.2,-9.23890707800001));
#288177=CARTESIAN_POINT('Ctrl Pts',(-5.48820883900006,12.2,-9.24134709400001));
#288178=CARTESIAN_POINT('Ctrl Pts',(-5.48885404200006,12.2,-9.24379357300002));
#288179=CARTESIAN_POINT('Ctrl Pts',(-5.48949869800006,12.2,-9.24624650800002));
#288180=CARTESIAN_POINT('Ctrl Pts',(-5.49014279600006,12.2,-9.24870588900001));
#288181=CARTESIAN_POINT('Ctrl Pts',(-5.49078632300006,12.2,-9.25117170600002));
#288182=CARTESIAN_POINT('Ctrl Pts',(-5.49142927000006,12.2,-9.25364395200001));
#288183=CARTESIAN_POINT('Ctrl Pts',(-5.49207162100006,12.2,-9.25612261600002));
#288184=CARTESIAN_POINT('Ctrl Pts',(-5.49271336800006,12.2,-9.25860769100002));
#288185=CARTESIAN_POINT('Ctrl Pts',(-5.49335449800005,12.2,-9.26109916700002));
#288186=CARTESIAN_POINT('Ctrl Pts',(-5.49399499900006,12.2,-9.26359703400001));
#288187=CARTESIAN_POINT('Ctrl Pts',(-5.49463485900006,12.2,-9.26610128400002));
#288188=CARTESIAN_POINT('Ctrl Pts',(-5.49527406800006,12.2,-9.26861190900001));
#288189=CARTESIAN_POINT('Ctrl Pts',(-5.49591261300006,12.2,-9.27112889800001));
#288190=CARTESIAN_POINT('Ctrl Pts',(-5.49655048300006,12.2,-9.27365224400001));
#288191=CARTESIAN_POINT('Ctrl Pts',(-5.49718766700006,12.2,-9.27618193800001));
#288192=CARTESIAN_POINT('Ctrl Pts',(-5.49782415300006,12.2,-9.27871797000002));
#288193=CARTESIAN_POINT('Ctrl Pts',(-5.49845993000006,12.2,-9.28126033100002));
#288194=CARTESIAN_POINT('Ctrl Pts',(-5.49909498700006,12.2,-9.28380901500002));
#288195=CARTESIAN_POINT('Ctrl Pts',(-5.49972931200006,12.2,-9.28636401000002));
#288196=CARTESIAN_POINT('Ctrl Pts',(-5.50036289400006,12.2,-9.28892530800002));
#288197=CARTESIAN_POINT('Ctrl Pts',(-5.50099572200006,12.2,-9.29149290000002));
#288198=CARTESIAN_POINT('Ctrl Pts',(-5.50162778400006,12.2,-9.29406678000002));
#288199=CARTESIAN_POINT('Ctrl Pts',(-5.50225906900006,12.2,-9.29664693400002));
#288200=CARTESIAN_POINT('Ctrl Pts',(-5.50288956700006,12.2,-9.29923335800002));
#288201=CARTESIAN_POINT('Ctrl Pts',(-5.50351926700006,12.2,-9.30182604100001));
#288202=CARTESIAN_POINT('Ctrl Pts',(-5.50414815600006,12.2,-9.30442497500002));
#288203=CARTESIAN_POINT('Ctrl Pts',(-5.50477622400006,12.2,-9.30703015100002));
#288204=CARTESIAN_POINT('Ctrl Pts',(-5.50540346100005,12.2,-9.30964156000002));
#288205=CARTESIAN_POINT('Ctrl Pts',(-5.50602985400006,12.2,-9.31225919400001));
#288206=CARTESIAN_POINT('Ctrl Pts',(-5.50665539400006,12.2,-9.31488304500002));
#288207=CARTESIAN_POINT('Ctrl Pts',(-5.50728006900005,12.2,-9.31751310200001));
#288208=CARTESIAN_POINT('Ctrl Pts',(-5.50790386900006,12.2,-9.32014935900002));
#288209=CARTESIAN_POINT('Ctrl Pts',(-5.50852678200005,12.2,-9.32279180500002));
#288210=CARTESIAN_POINT('Ctrl Pts',(-5.50914879900006,12.2,-9.32544043300001));
#288211=CARTESIAN_POINT('Ctrl Pts',(-5.50976990800006,12.2,-9.32809523400002));
#288212=CARTESIAN_POINT('Ctrl Pts',(-5.51039009700006,12.2,-9.33075620000002));
#288213=CARTESIAN_POINT('Ctrl Pts',(-5.51100935800005,12.2,-9.33342332100001));
#288214=CARTESIAN_POINT('Ctrl Pts',(-5.51162767900006,12.2,-9.33609659000001));
#288215=CARTESIAN_POINT('Ctrl Pts',(-5.51224505000006,12.2,-9.33877599700002));
#288216=CARTESIAN_POINT('Ctrl Pts',(-5.51286145900006,12.2,-9.34146153400001));
#288217=CARTESIAN_POINT('Ctrl Pts',(-5.51347689600005,12.2,-9.34415319400001));
#288218=CARTESIAN_POINT('Ctrl Pts',(-5.51409135300006,12.2,-9.34685096600001));
#288219=CARTESIAN_POINT('Ctrl Pts',(-5.51470481600006,12.2,-9.34955484400002));
#288220=CARTESIAN_POINT('Ctrl Pts',(-5.51531727600006,12.2,-9.35226481800001));
#288221=CARTESIAN_POINT('Ctrl Pts',(-5.51592872200006,12.2,-9.35498087900001));
#288222=CARTESIAN_POINT('Ctrl Pts',(-5.51653914500006,12.2,-9.35770301900002));
#288223=CARTESIAN_POINT('Ctrl Pts',(-5.51714853300005,12.2,-9.36043123200001));
#288224=CARTESIAN_POINT('Ctrl Pts',(-5.51775687700006,12.2,-9.36316550500001));
#288225=CARTESIAN_POINT('Ctrl Pts',(-5.51836416700006,12.2,-9.36590583500001));
#288226=CARTESIAN_POINT('Ctrl Pts',(-5.51897039000006,12.2,-9.36865220900001));
#288227=CARTESIAN_POINT('Ctrl Pts',(-5.51957553900006,12.2,-9.37140462000002));
#288228=CARTESIAN_POINT('Ctrl Pts',(-5.52017960200006,12.2,-9.37416306100002));
#288229=CARTESIAN_POINT('Ctrl Pts',(-5.52078257000006,12.2,-9.37692752200002));
#288230=CARTESIAN_POINT('Ctrl Pts',(-5.52138443200006,12.2,-9.37969799600002));
#288231=CARTESIAN_POINT('Ctrl Pts',(-5.52198517700006,12.2,-9.38247447400002));
#288232=CARTESIAN_POINT('Ctrl Pts',(-5.52258479700006,12.2,-9.38525694700001));
#288233=CARTESIAN_POINT('Ctrl Pts',(-5.52318328100006,12.2,-9.38804540800002));
#288234=CARTESIAN_POINT('Ctrl Pts',(-5.52378061800006,12.2,-9.39083984800002));
#288235=CARTESIAN_POINT('Ctrl Pts',(-5.52437679900006,12.2,-9.39364025800002));
#288236=CARTESIAN_POINT('Ctrl Pts',(-5.52497181400006,12.2,-9.39644663300001));
#288237=CARTESIAN_POINT('Ctrl Pts',(-5.52556565400006,12.2,-9.39925896000002));
#288238=CARTESIAN_POINT('Ctrl Pts',(-5.52615830800006,12.2,-9.40207723400002));
#288239=CARTESIAN_POINT('Ctrl Pts',(-5.52674976600006,12.2,-9.40490144500002));
#288240=CARTESIAN_POINT('Ctrl Pts',(-5.52734001800006,12.2,-9.40773158700001));
#288241=CARTESIAN_POINT('Ctrl Pts',(-5.52792905500006,12.2,-9.41056764900001));
#288242=CARTESIAN_POINT('Ctrl Pts',(-5.52851686600006,12.2,-9.41340962500002));
#288243=CARTESIAN_POINT('Ctrl Pts',(-5.52910344300006,12.2,-9.41625750600002));
#288244=CARTESIAN_POINT('Ctrl Pts',(-5.52968877600006,12.2,-9.41911128400001));
#288245=CARTESIAN_POINT('Ctrl Pts',(-5.53027285400006,12.2,-9.42197095100001));
#288246=CARTESIAN_POINT('Ctrl Pts',(-5.53085566800006,12.2,-9.42483649900002));
#288247=CARTESIAN_POINT('Ctrl Pts',(-5.53143720800006,12.2,-9.42770791800001));
#288248=CARTESIAN_POINT('Ctrl Pts',(-5.53213351757476,12.2,-9.43116065867457));
#288249=CARTESIAN_POINT('Ctrl Pts',(-5.53282788771271,12.2,-9.43462218366274));
#288250=CARTESIAN_POINT('Ctrl Pts',(-5.53352029828741,12.2,-9.43809247833729));
#288251=CARTESIAN_POINT('Ctrl Pts',(-5.53421073242535,12.2,-9.44157152332546));
#288252=CARTESIAN_POINT('Ctrl Pts',(-5.53489917000006,12.2,-9.44505930400002));
#288253=CARTESIAN_POINT('Ctrl Pts',(-5.53547152800006,12.2,-9.44797160400002));
#288254=CARTESIAN_POINT('Ctrl Pts',(-5.53604253700006,12.2,-9.45088971200001));
#288255=CARTESIAN_POINT('Ctrl Pts',(-5.53661218600006,12.2,-9.45381362000001));
#288256=CARTESIAN_POINT('Ctrl Pts',(-5.53718046800006,12.2,-9.45674332000002));
#288257=CARTESIAN_POINT('Ctrl Pts',(-5.53774737000006,12.2,-9.45967880400002));
#288258=CARTESIAN_POINT('Ctrl Pts',(-5.53831288800006,12.2,-9.46262006300002));
#288259=CARTESIAN_POINT('Ctrl Pts',(-5.53887700700006,12.2,-9.46556709000001));
#288260=CARTESIAN_POINT('Ctrl Pts',(-5.53943972200006,12.2,-9.46851987700001));
#288261=CARTESIAN_POINT('Ctrl Pts',(-5.54000102100006,12.2,-9.47147841500002));
#288262=CARTESIAN_POINT('Ctrl Pts',(-5.54056089800006,12.2,-9.47444269800001));
#288263=CARTESIAN_POINT('Ctrl Pts',(-5.54111934100006,12.2,-9.47741271600002));
#288264=CARTESIAN_POINT('Ctrl Pts',(-5.54167634100006,12.2,-9.48038846300001));
#288265=CARTESIAN_POINT('Ctrl Pts',(-5.54223189100005,12.2,-9.48336993000002));
#288266=CARTESIAN_POINT('Ctrl Pts',(-5.54278597900006,12.2,-9.48635710900002));
#288267=CARTESIAN_POINT('Ctrl Pts',(-5.54333859900006,12.2,-9.48934999200001));
#288268=CARTESIAN_POINT('Ctrl Pts',(-5.54388974000006,12.2,-9.49234857200001));
#288269=CARTESIAN_POINT('Ctrl Pts',(-5.54443939300006,12.2,-9.49535284000002));
#288270=CARTESIAN_POINT('Ctrl Pts',(-5.54498755000006,12.2,-9.49836278900002));
#288271=CARTESIAN_POINT('Ctrl Pts',(-5.54553420100006,12.2,-9.50137841100002));
#288272=CARTESIAN_POINT('Ctrl Pts',(-5.54607933800006,12.2,-9.50439969700002));
#288273=CARTESIAN_POINT('Ctrl Pts',(-5.54662295300006,12.2,-9.50742664100002));
#288274=CARTESIAN_POINT('Ctrl Pts',(-5.54716503400006,12.2,-9.51045923400001));
#288275=CARTESIAN_POINT('Ctrl Pts',(-5.54770557400006,12.2,-9.51349746900001));
#288276=CARTESIAN_POINT('Ctrl Pts',(-5.54824456500006,12.2,-9.51654133600002));
#288277=CARTESIAN_POINT('Ctrl Pts',(-5.54878199800006,12.2,-9.51959083100002));
#288278=CARTESIAN_POINT('Ctrl Pts',(-5.54931786200005,12.2,-9.52264594300001));
#288279=CARTESIAN_POINT('Ctrl Pts',(-5.54985215100006,12.2,-9.52570666600002));
#288280=CARTESIAN_POINT('Ctrl Pts',(-5.55038485500006,12.2,-9.52877299000002));
#288281=CARTESIAN_POINT('Ctrl Pts',(-5.55091596500006,12.2,-9.53184491000002));
#288282=CARTESIAN_POINT('Ctrl Pts',(-5.55144547200006,12.2,-9.53492241800001));
#288283=CARTESIAN_POINT('Ctrl Pts',(-5.55197337000005,12.2,-9.53800550400001));
#288284=CARTESIAN_POINT('Ctrl Pts',(-5.55249964700006,12.2,-9.54109416100002));
#288285=CARTESIAN_POINT('Ctrl Pts',(-5.55302429700006,12.2,-9.54418838400001));
#288286=CARTESIAN_POINT('Ctrl Pts',(-5.55354730900006,12.2,-9.54728816200002));
#288287=CARTESIAN_POINT('Ctrl Pts',(-5.55406867700006,12.2,-9.55039348800002));
#288288=CARTESIAN_POINT('Ctrl Pts',(-5.55458839100006,12.2,-9.55350435500002));
#288289=CARTESIAN_POINT('Ctrl Pts',(-5.55510644200006,12.2,-9.55662075600002));
#288290=CARTESIAN_POINT('Ctrl Pts',(-5.55562282200006,12.2,-9.55974268200002));
#288291=CARTESIAN_POINT('Ctrl Pts',(-5.55613752400006,12.2,-9.56287012600002));
#288292=CARTESIAN_POINT('Ctrl Pts',(-5.55665053700006,12.2,-9.56600308000001));
#288293=CARTESIAN_POINT('Ctrl Pts',(-5.55716185500006,12.2,-9.56914153600002));
#288294=CARTESIAN_POINT('Ctrl Pts',(-5.55767146700005,12.2,-9.57228548700002));
#288295=CARTESIAN_POINT('Ctrl Pts',(-5.55817936700006,12.2,-9.57543492600001));
#288296=CARTESIAN_POINT('Ctrl Pts',(-5.55868554700006,12.2,-9.57858984400002));
#288297=CARTESIAN_POINT('Ctrl Pts',(-5.55918999600006,12.2,-9.58175023500001));
#288298=CARTESIAN_POINT('Ctrl Pts',(-5.55969270800006,12.2,-9.58491608900001));
#288299=CARTESIAN_POINT('Ctrl Pts',(-5.56019367400006,12.2,-9.58808740000002));
#288300=CARTESIAN_POINT('Ctrl Pts',(-5.56069288500006,12.2,-9.59126416200002));
#288301=CARTESIAN_POINT('Ctrl Pts',(-5.56119033400006,12.2,-9.59444636500002));
#288302=CARTESIAN_POINT('Ctrl Pts',(-5.56168601200006,12.2,-9.59763400200002));
#288303=CARTESIAN_POINT('Ctrl Pts',(-5.56217991100006,12.2,-9.60082706600002));
#288304=CARTESIAN_POINT('Ctrl Pts',(-5.56267202400006,12.2,-9.60402554800002));
#288305=CARTESIAN_POINT('Ctrl Pts',(-5.56316234000006,12.2,-9.60722944300001));
#288306=CARTESIAN_POINT('Ctrl Pts',(-5.56365085400006,12.2,-9.61043874100002));
#288307=CARTESIAN_POINT('Ctrl Pts',(-5.56413755700006,12.2,-9.61365343600002));
#288308=CARTESIAN_POINT('Ctrl Pts',(-5.56462243900006,12.2,-9.61687352000002));
#288309=CARTESIAN_POINT('Ctrl Pts',(-5.56510549500006,12.2,-9.62009898500002));
#288310=CARTESIAN_POINT('Ctrl Pts',(-5.56558671400006,12.2,-9.62332982500002));
#288311=CARTESIAN_POINT('Ctrl Pts',(-5.56606609100006,12.2,-9.62656603200001));
#288312=CARTESIAN_POINT('Ctrl Pts',(-5.56654361600006,12.2,-9.62980759800002));
#288313=CARTESIAN_POINT('Ctrl Pts',(-5.56701928100006,12.2,-9.63305451500002));
#288314=CARTESIAN_POINT('Ctrl Pts',(-5.56749308000006,12.2,-9.63630677700002));
#288315=CARTESIAN_POINT('Ctrl Pts',(-5.56796500300006,12.2,-9.63956437500002));
#288316=CARTESIAN_POINT('Ctrl Pts',(-5.56843504200006,12.2,-9.64282730200001));
#288317=CARTESIAN_POINT('Ctrl Pts',(-5.56890319100006,12.2,-9.64609555300001));
#288318=CARTESIAN_POINT('Ctrl Pts',(-5.56936944100006,12.2,-9.64936911600002));
#288319=CARTESIAN_POINT('Ctrl Pts',(-5.56983378400006,12.2,-9.65264798800001));
#288320=CARTESIAN_POINT('Ctrl Pts',(-5.57029621300006,12.2,-9.65593215900001));
#288321=CARTESIAN_POINT('Ctrl Pts',(-5.57075671900006,12.2,-9.65922162300001));
#288322=CARTESIAN_POINT('Ctrl Pts',(-5.57121529500006,12.2,-9.66251637100001));
#288323=CARTESIAN_POINT('Ctrl Pts',(-5.57167193400006,12.2,-9.66581639800001));
#288324=CARTESIAN_POINT('Ctrl Pts',(-5.57212662700006,12.2,-9.66912169500001));
#288325=CARTESIAN_POINT('Ctrl Pts',(-5.57257936700006,12.2,-9.67243225400001));
#288326=CARTESIAN_POINT('Ctrl Pts',(-5.57303014600006,12.2,-9.67574807000001));
#288327=CARTESIAN_POINT('Ctrl Pts',(-5.57347895600006,12.2,-9.67906913300001));
#288328=CARTESIAN_POINT('Ctrl Pts',(-5.57392579000005,12.2,-9.68239543700001));
#288329=CARTESIAN_POINT('Ctrl Pts',(-5.57437064100006,12.2,-9.68572697500001));
#288330=CARTESIAN_POINT('Ctrl Pts',(-5.57481350100006,12.2,-9.68906373900001));
#288331=CARTESIAN_POINT('Ctrl Pts',(-5.57525436100006,12.2,-9.69240572200001));
#288332=CARTESIAN_POINT('Ctrl Pts',(-5.57569321500006,12.2,-9.69575291700002));
#288333=CARTESIAN_POINT('Ctrl Pts',(-5.57613005500006,12.2,-9.69910531700001));
#288334=CARTESIAN_POINT('Ctrl Pts',(-5.57656487300005,12.2,-9.70246291300001));
#288335=CARTESIAN_POINT('Ctrl Pts',(-5.57699766300006,12.2,-9.70582570000001));
#288336=CARTESIAN_POINT('Ctrl Pts',(-5.57742841600006,12.2,-9.70919366800001));
#288337=CARTESIAN_POINT('Ctrl Pts',(-5.57785712500006,12.2,-9.71256681200001));
#288338=CARTESIAN_POINT('Ctrl Pts',(-5.57828378300006,12.2,-9.71594512400001));
#288339=CARTESIAN_POINT('Ctrl Pts',(-5.57870838200006,12.2,-9.71932859700001));
#288340=CARTESIAN_POINT('Ctrl Pts',(-5.57913091500006,12.2,-9.72271722400001));
#288341=CARTESIAN_POINT('Ctrl Pts',(-5.57955137400006,12.2,-9.72611099700002));
#288342=CARTESIAN_POINT('Ctrl Pts',(-5.57996975300005,12.2,-9.72950991000001));
#288343=CARTESIAN_POINT('Ctrl Pts',(-5.58038604400006,12.2,-9.73291395500001));
#288344=CARTESIAN_POINT('Ctrl Pts',(-5.58080023800006,12.2,-9.73632312400001));
#288345=CARTESIAN_POINT('Ctrl Pts',(-5.58121233100006,12.2,-9.73973741000002));
#288346=CARTESIAN_POINT('Ctrl Pts',(-5.58162231200006,12.2,-9.74315680800001));
#288347=CARTESIAN_POINT('Ctrl Pts',(-5.58203017800006,12.2,-9.74658130900002));
#288348=CARTESIAN_POINT('Ctrl Pts',(-5.58243591800006,12.2,-9.75001090500001));
#288349=CARTESIAN_POINT('Ctrl Pts',(-5.58283952600005,12.2,-9.75344559000001));
#288350=CARTESIAN_POINT('Ctrl Pts',(-5.58324099600005,12.2,-9.75688535700001));
#288351=CARTESIAN_POINT('Ctrl Pts',(-5.58364031900005,12.2,-9.76033019900001));
#288352=CARTESIAN_POINT('Ctrl Pts',(-5.58403748900006,12.2,-9.76378010900001));
#288353=CARTESIAN_POINT('Ctrl Pts',(-5.58443250000006,12.2,-9.76723507800001));
#288354=CARTESIAN_POINT('Ctrl Pts',(-5.58482534200006,12.2,-9.77069510100001));
#288355=CARTESIAN_POINT('Ctrl Pts',(-5.58521601000006,12.2,-9.77416017100001));
#288356=CARTESIAN_POINT('Ctrl Pts',(-5.58560449700006,12.2,-9.77763027800002));
#288357=CARTESIAN_POINT('Ctrl Pts',(-5.58599079400006,12.2,-9.78110541800001));
#288358=CARTESIAN_POINT('Ctrl Pts',(-5.58637489600006,12.2,-9.78458558300001));
#288359=CARTESIAN_POINT('Ctrl Pts',(-5.58675679500006,12.2,-9.78807076600001));
#288360=CARTESIAN_POINT('Ctrl Pts',(-5.58713648300006,12.2,-9.79156095800001));
#288361=CARTESIAN_POINT('Ctrl Pts',(-5.58751395600006,12.2,-9.79505615600001));
#288362=CARTESIAN_POINT('Ctrl Pts',(-5.58788920500006,12.2,-9.79855634900001));
#288363=CARTESIAN_POINT('Ctrl Pts',(-5.58826222200006,12.2,-9.80206153200001));
#288364=CARTESIAN_POINT('Ctrl Pts',(-5.58863300300006,12.2,-9.80557169700001));
#288365=CARTESIAN_POINT('Ctrl Pts',(-5.58900153800006,12.2,-9.80908683700001));
#288366=CARTESIAN_POINT('Ctrl Pts',(-5.58936782300006,12.2,-9.81260694600001));
#288367=CARTESIAN_POINT('Ctrl Pts',(-5.58973184900006,12.2,-9.81613201700001));
#288368=CARTESIAN_POINT('Ctrl Pts',(-5.59009361000006,12.2,-9.81966204100001));
#288369=CARTESIAN_POINT('Ctrl Pts',(-5.59045309900006,12.2,-9.82319701200001));
#288370=CARTESIAN_POINT('Ctrl Pts',(-5.59081030900006,12.2,-9.82673692500001));
#288371=CARTESIAN_POINT('Ctrl Pts',(-5.59116523300006,12.2,-9.83028176900001));
#288372=CARTESIAN_POINT('Ctrl Pts',(-5.59151786600006,12.2,-9.83383154100001));
#288373=CARTESIAN_POINT('Ctrl Pts',(-5.59186819900006,12.2,-9.83738623200001));
#288374=CARTESIAN_POINT('Ctrl Pts',(-5.59221622500006,12.2,-9.84094583600001));
#288375=CARTESIAN_POINT('Ctrl Pts',(-5.59256194100006,12.2,-9.84451034500001));
#288376=CARTESIAN_POINT('Ctrl Pts',(-5.59290533600006,12.2,-9.84807975100001));
#288377=CARTESIAN_POINT('Ctrl Pts',(-5.59324640500006,12.2,-9.85165405000001));
#288378=CARTESIAN_POINT('Ctrl Pts',(-5.59358514100006,12.2,-9.85523323300001));
#288379=CARTESIAN_POINT('Ctrl Pts',(-5.59392153800006,12.2,-9.85881729400001));
#288380=CARTESIAN_POINT('Ctrl Pts',(-5.59425559000006,12.2,-9.86240622500001));
#288381=CARTESIAN_POINT('Ctrl Pts',(-5.59458728700006,12.2,-9.86600002000001));
#288382=CARTESIAN_POINT('Ctrl Pts',(-5.59491662700006,12.2,-9.86959867100001));
#288383=CARTESIAN_POINT('Ctrl Pts',(-5.59524360000006,12.2,-9.87320217300001));
#288384=CARTESIAN_POINT('Ctrl Pts',(-5.59556820200006,12.2,-9.87681051700001));
#288385=CARTESIAN_POINT('Ctrl Pts',(-5.59589042400006,12.2,-9.88042369800001));
#288386=CARTESIAN_POINT('Ctrl Pts',(-5.59621026000006,12.2,-9.88404170800001));
#288387=CARTESIAN_POINT('Ctrl Pts',(-5.59652770400006,12.2,-9.88766454000001));
#288388=CARTESIAN_POINT('Ctrl Pts',(-5.59684275000006,12.2,-9.89129218700001));
#288389=CARTESIAN_POINT('Ctrl Pts',(-5.59715539100006,12.2,-9.89492464200001));
#288390=CARTESIAN_POINT('Ctrl Pts',(-5.59746562000006,12.2,-9.89856190000001));
#288391=CARTESIAN_POINT('Ctrl Pts',(-5.59777343200006,12.2,-9.90220395300001));
#288392=CARTESIAN_POINT('Ctrl Pts',(-5.59807881900006,12.2,-9.90585079300001));
#288393=CARTESIAN_POINT('Ctrl Pts',(-5.59838177600006,12.2,-9.90950241400001));
#288394=CARTESIAN_POINT('Ctrl Pts',(-5.59868229500006,12.2,-9.91315881000001));
#288395=CARTESIAN_POINT('Ctrl Pts',(-5.59898037100006,12.2,-9.91681997300001));
#288396=CARTESIAN_POINT('Ctrl Pts',(-5.59927599700006,12.2,-9.92048589600001));
#288397=CARTESIAN_POINT('Ctrl Pts',(-5.59956916600005,12.2,-9.92415657400001));
#288398=CARTESIAN_POINT('Ctrl Pts',(-5.59985987300006,12.2,-9.92783199800001));
#288399=CARTESIAN_POINT('Ctrl Pts',(-5.60014811000006,12.2,-9.93151216200001));
#288400=CARTESIAN_POINT('Ctrl Pts',(-5.60043387200006,12.2,-9.93519706000001));
#288401=CARTESIAN_POINT('Ctrl Pts',(-5.60071715300006,12.2,-9.93888668300001));
#288402=CARTESIAN_POINT('Ctrl Pts',(-5.60099794600006,12.2,-9.94258102700002));
#288403=CARTESIAN_POINT('Ctrl Pts',(-5.60127624500006,12.2,-9.94628008400001));
#288404=CARTESIAN_POINT('Ctrl Pts',(-5.60155204400006,12.2,-9.94998384700001));
#288405=CARTESIAN_POINT('Ctrl Pts',(-5.60182533700006,12.2,-9.95369231100001));
#288406=CARTESIAN_POINT('Ctrl Pts',(-5.60209611700006,12.2,-9.95740546800001));
#288407=CARTESIAN_POINT('Ctrl Pts',(-5.60236437800006,12.2,-9.96112330900001));
#288408=CARTESIAN_POINT('Ctrl Pts',(-5.60263011400005,12.2,-9.96484583000001));
#288409=CARTESIAN_POINT('Ctrl Pts',(-5.60289331800006,12.2,-9.96857302300001));
#288410=CARTESIAN_POINT('Ctrl Pts',(-5.60315398400006,12.2,-9.97230488000001));
#288411=CARTESIAN_POINT('Ctrl Pts',(-5.60341210500006,12.2,-9.97604139500002));
#288412=CARTESIAN_POINT('Ctrl Pts',(-5.60366767700006,12.2,-9.97978256300001));
#288413=CARTESIAN_POINT('Ctrl Pts',(-5.60392069300006,12.2,-9.98352837700001));
#288414=CARTESIAN_POINT('Ctrl Pts',(-5.60417114800006,12.2,-9.98727882900001));
#288415=CARTESIAN_POINT('Ctrl Pts',(-5.60441903700006,12.2,-9.99103391600001));
#288416=CARTESIAN_POINT('Ctrl Pts',(-5.60466435400006,12.2,-9.99479363100001));
#288417=CARTESIAN_POINT('Ctrl Pts',(-5.60490709200006,12.2,-9.99855796400001));
#288418=CARTESIAN_POINT('Ctrl Pts',(-5.60514724500006,12.2,-10.002326912));
#288419=CARTESIAN_POINT('Ctrl Pts',(-5.60538480400006,12.2,-10.006100463));
#288420=CARTESIAN_POINT('Ctrl Pts',(-5.60561976300006,12.2,-10.00987861));
#288421=CARTESIAN_POINT('Ctrl Pts',(-5.60585211500006,12.2,-10.013661344));
#288422=CARTESIAN_POINT('Ctrl Pts',(-5.60608185300006,12.2,-10.01744866));
#288423=CARTESIAN_POINT('Ctrl Pts',(-5.60630897000006,12.2,-10.02124055));
#288424=CARTESIAN_POINT('Ctrl Pts',(-5.60653346400006,12.2,-10.025037011));
#288425=CARTESIAN_POINT('Ctrl Pts',(-5.60675533300006,12.2,-10.028838039));
#288426=CARTESIAN_POINT('Ctrl Pts',(-5.60697457300006,12.2,-10.032643631));
#288427=CARTESIAN_POINT('Ctrl Pts',(-5.60714786300006,12.2,-10.035691757));
#288428=CARTESIAN_POINT('Ctrl Pts',(-5.60727664800006,12.2,-10.037979904));
#288429=CARTESIAN_POINT('Ctrl Pts',(-5.60736197900006,12.2,-10.039506249));
#288430=CARTESIAN_POINT('Ctrl Pts',(-5.60740451300005,12.2,-10.040269649));
#288431=CARTESIAN_POINT('Ctrl Pts',(-5.26939701900006,15.2,-10.221714879));
#288432=CARTESIAN_POINT('Ctrl Pts',(-5.26939701900006,11.6,-10.221714879));
#288433=CARTESIAN_POINT('Ctrl Pts',(-5.26878426900006,15.2,-10.221257574));
#288434=CARTESIAN_POINT('Ctrl Pts',(-5.26878426900006,11.6,-10.221257574));
#288435=CARTESIAN_POINT('Ctrl Pts',(-5.26755929400006,15.2,-10.220343));
#288436=CARTESIAN_POINT('Ctrl Pts',(-5.26755929400006,11.6,-10.220343));
#288437=CARTESIAN_POINT('Ctrl Pts',(-5.26572340900006,15.2,-10.218971238));
#288438=CARTESIAN_POINT('Ctrl Pts',(-5.26572340900006,11.6,-10.218971238));
#288439=CARTESIAN_POINT('Ctrl Pts',(-5.26327871600006,15.2,-10.217142421));
#288440=CARTESIAN_POINT('Ctrl Pts',(-5.26327871600006,11.6,-10.217142421));
#288441=CARTESIAN_POINT('Ctrl Pts',(-5.26022810600006,15.2,-10.214856731));
#288442=CARTESIAN_POINT('Ctrl Pts',(-5.26022810600006,11.6,-10.214856731));
#288443=CARTESIAN_POINT('Ctrl Pts',(-5.25718275200005,15.2,-10.212571373));
#288444=CARTESIAN_POINT('Ctrl Pts',(-5.25718275200005,11.6,-10.212571373));
#288445=CARTESIAN_POINT('Ctrl Pts',(-5.25414265600006,15.2,-10.210286352));
#288446=CARTESIAN_POINT('Ctrl Pts',(-5.25414265600006,11.6,-10.210286352));
#288447=CARTESIAN_POINT('Ctrl Pts',(-5.25110781900006,15.2,-10.208001669));
#288448=CARTESIAN_POINT('Ctrl Pts',(-5.25110781900006,11.6,-10.208001669));
#288449=CARTESIAN_POINT('Ctrl Pts',(-5.24807824200006,15.2,-10.20571733));
#288450=CARTESIAN_POINT('Ctrl Pts',(-5.24807824200006,11.6,-10.20571733));
#288451=CARTESIAN_POINT('Ctrl Pts',(-5.24505392700005,15.2,-10.203433345));
#288452=CARTESIAN_POINT('Ctrl Pts',(-5.24505392700005,11.6,-10.203433345));
#288453=CARTESIAN_POINT('Ctrl Pts',(-5.24203487700006,15.2,-10.20114972));
#288454=CARTESIAN_POINT('Ctrl Pts',(-5.24203487700006,11.6,-10.20114972));
#288455=CARTESIAN_POINT('Ctrl Pts',(-5.23902109500006,15.2,-10.198866468));
#288456=CARTESIAN_POINT('Ctrl Pts',(-5.23902109500006,11.6,-10.198866468));
#288457=CARTESIAN_POINT('Ctrl Pts',(-5.23601258300006,15.2,-10.1965836));
#288458=CARTESIAN_POINT('Ctrl Pts',(-5.23601258300006,11.6,-10.1965836));
#288459=CARTESIAN_POINT('Ctrl Pts',(-5.23300934400006,15.2,-10.194301125));
#288460=CARTESIAN_POINT('Ctrl Pts',(-5.23300934400006,11.6,-10.194301125));
#288461=CARTESIAN_POINT('Ctrl Pts',(-5.23001138100006,15.2,-10.192019055));
#288462=CARTESIAN_POINT('Ctrl Pts',(-5.23001138100006,11.6,-10.192019055));
#288463=CARTESIAN_POINT('Ctrl Pts',(-5.22701869500006,15.2,-10.189737398));
#288464=CARTESIAN_POINT('Ctrl Pts',(-5.22701869500006,11.6,-10.189737398));
#288465=CARTESIAN_POINT('Ctrl Pts',(-5.22403128900006,15.2,-10.187456162));
#288466=CARTESIAN_POINT('Ctrl Pts',(-5.22403128900006,11.6,-10.187456162));
#288467=CARTESIAN_POINT('Ctrl Pts',(-5.22104916700005,15.2,-10.185175356));
#288468=CARTESIAN_POINT('Ctrl Pts',(-5.22104916700005,11.6,-10.185175356));
#288469=CARTESIAN_POINT('Ctrl Pts',(-5.21807232800006,15.2,-10.182894987));
#288470=CARTESIAN_POINT('Ctrl Pts',(-5.21807232800006,11.6,-10.182894987));
#288471=CARTESIAN_POINT('Ctrl Pts',(-5.21510077500006,15.2,-10.180615064));
#288472=CARTESIAN_POINT('Ctrl Pts',(-5.21510077500006,11.6,-10.180615064));
#288473=CARTESIAN_POINT('Ctrl Pts',(-5.21213451000006,15.2,-10.178335595));
#288474=CARTESIAN_POINT('Ctrl Pts',(-5.21213451000006,11.6,-10.178335595));
#288475=CARTESIAN_POINT('Ctrl Pts',(-5.20917353600006,15.2,-10.176056588));
#288476=CARTESIAN_POINT('Ctrl Pts',(-5.20917353600006,11.6,-10.176056588));
#288477=CARTESIAN_POINT('Ctrl Pts',(-5.20621785500006,15.2,-10.173778052));
#288478=CARTESIAN_POINT('Ctrl Pts',(-5.20621785500006,11.6,-10.173778052));
#288479=CARTESIAN_POINT('Ctrl Pts',(-5.20326747000006,15.2,-10.171499997));
#288480=CARTESIAN_POINT('Ctrl Pts',(-5.20326747000006,11.6,-10.171499997));
#288481=CARTESIAN_POINT('Ctrl Pts',(-5.20032238000006,15.2,-10.169222432));
#288482=CARTESIAN_POINT('Ctrl Pts',(-5.20032238000006,11.6,-10.169222432));
#288483=CARTESIAN_POINT('Ctrl Pts',(-5.19738259200006,15.2,-10.166945366));
#288484=CARTESIAN_POINT('Ctrl Pts',(-5.19738259200006,11.6,-10.166945366));
#288485=CARTESIAN_POINT('Ctrl Pts',(-5.19444810400006,15.2,-10.164668808));
#288486=CARTESIAN_POINT('Ctrl Pts',(-5.19444810400006,11.6,-10.164668808));
#288487=CARTESIAN_POINT('Ctrl Pts',(-5.19151892100005,15.2,-10.162392768));
#288488=CARTESIAN_POINT('Ctrl Pts',(-5.19151892100005,11.6,-10.162392768));
#288489=CARTESIAN_POINT('Ctrl Pts',(-5.18859504500006,15.2,-10.160117253));
#288490=CARTESIAN_POINT('Ctrl Pts',(-5.18859504500006,11.6,-10.160117253));
#288491=CARTESIAN_POINT('Ctrl Pts',(-5.18567647700006,15.2,-10.157842273));
#288492=CARTESIAN_POINT('Ctrl Pts',(-5.18567647700006,11.6,-10.157842273));
#288493=CARTESIAN_POINT('Ctrl Pts',(-5.18276322000006,15.2,-10.155567837));
#288494=CARTESIAN_POINT('Ctrl Pts',(-5.18276322000006,11.6,-10.155567837));
#288495=CARTESIAN_POINT('Ctrl Pts',(-5.17985527400006,15.2,-10.153293954));
#288496=CARTESIAN_POINT('Ctrl Pts',(-5.17985527400006,11.6,-10.153293954));
#288497=CARTESIAN_POINT('Ctrl Pts',(-5.17695264500006,15.2,-10.151020632));
#288498=CARTESIAN_POINT('Ctrl Pts',(-5.17695264500006,11.6,-10.151020632));
#288499=CARTESIAN_POINT('Ctrl Pts',(-5.17405533300006,15.2,-10.14874788));
#288500=CARTESIAN_POINT('Ctrl Pts',(-5.17405533300006,11.6,-10.14874788));
#288501=CARTESIAN_POINT('Ctrl Pts',(-5.17116333900006,15.2,-10.146475708));
#288502=CARTESIAN_POINT('Ctrl Pts',(-5.17116333900006,11.6,-10.146475708));
#288503=CARTESIAN_POINT('Ctrl Pts',(-5.16827666700006,15.2,-10.144204125));
#288504=CARTESIAN_POINT('Ctrl Pts',(-5.16827666700006,11.6,-10.144204125));
#288505=CARTESIAN_POINT('Ctrl Pts',(-5.16539531900006,15.2,-10.14193314));
#288506=CARTESIAN_POINT('Ctrl Pts',(-5.16539531900006,11.6,-10.14193314));
#288507=CARTESIAN_POINT('Ctrl Pts',(-5.16251929700006,15.2,-10.139662761));
#288508=CARTESIAN_POINT('Ctrl Pts',(-5.16251929700006,11.6,-10.139662761));
#288509=CARTESIAN_POINT('Ctrl Pts',(-5.15964860300006,15.2,-10.137392999));
#288510=CARTESIAN_POINT('Ctrl Pts',(-5.15964860300006,11.6,-10.137392999));
#288511=CARTESIAN_POINT('Ctrl Pts',(-5.15678323800006,15.2,-10.135123862));
#288512=CARTESIAN_POINT('Ctrl Pts',(-5.15678323800006,11.6,-10.135123862));
#288513=CARTESIAN_POINT('Ctrl Pts',(-5.15392320700006,15.2,-10.132855359));
#288514=CARTESIAN_POINT('Ctrl Pts',(-5.15392320700006,11.6,-10.132855359));
#288515=CARTESIAN_POINT('Ctrl Pts',(-5.15106851000006,15.2,-10.130587501));
#288516=CARTESIAN_POINT('Ctrl Pts',(-5.15106851000006,11.6,-10.130587501));
#288517=CARTESIAN_POINT('Ctrl Pts',(-5.14821915000006,15.2,-10.128320294));
#288518=CARTESIAN_POINT('Ctrl Pts',(-5.14821915000006,11.6,-10.128320294));
#288519=CARTESIAN_POINT('Ctrl Pts',(-5.14537512800006,15.2,-10.12605375));
#288520=CARTESIAN_POINT('Ctrl Pts',(-5.14537512800006,11.6,-10.12605375));
#288521=CARTESIAN_POINT('Ctrl Pts',(-5.14253644700006,15.2,-10.123787877));
#288522=CARTESIAN_POINT('Ctrl Pts',(-5.14253644700006,11.6,-10.123787877));
#288523=CARTESIAN_POINT('Ctrl Pts',(-5.13970311000006,15.2,-10.121522683));
#288524=CARTESIAN_POINT('Ctrl Pts',(-5.13970311000006,11.6,-10.121522683));
#288525=CARTESIAN_POINT('Ctrl Pts',(-5.13687511700006,15.2,-10.119258181));
#288526=CARTESIAN_POINT('Ctrl Pts',(-5.13687511700006,11.6,-10.119258181));
#288527=CARTESIAN_POINT('Ctrl Pts',(-5.13405247200006,15.2,-10.116994376));
#288528=CARTESIAN_POINT('Ctrl Pts',(-5.13405247200006,11.6,-10.116994376));
#288529=CARTESIAN_POINT('Ctrl Pts',(-5.13123517700006,15.2,-10.11473128));
#288530=CARTESIAN_POINT('Ctrl Pts',(-5.13123517700006,11.6,-10.11473128));
#288531=CARTESIAN_POINT('Ctrl Pts',(-5.12842323300006,15.2,-10.112468901));
#288532=CARTESIAN_POINT('Ctrl Pts',(-5.12842323300006,11.6,-10.112468901));
#288533=CARTESIAN_POINT('Ctrl Pts',(-5.12561664200006,15.2,-10.11020725));
#288534=CARTESIAN_POINT('Ctrl Pts',(-5.12561664200006,11.6,-10.11020725));
#288535=CARTESIAN_POINT('Ctrl Pts',(-5.12281540700006,15.2,-10.107946335));
#288536=CARTESIAN_POINT('Ctrl Pts',(-5.12281540700006,11.6,-10.107946335));
#288537=CARTESIAN_POINT('Ctrl Pts',(-5.12001953100006,15.2,-10.105686165));
#288538=CARTESIAN_POINT('Ctrl Pts',(-5.12001953100006,11.6,-10.105686165));
#288539=CARTESIAN_POINT('Ctrl Pts',(-5.11722901500006,15.2,-10.10342675));
#288540=CARTESIAN_POINT('Ctrl Pts',(-5.11722901500006,11.6,-10.10342675));
#288541=CARTESIAN_POINT('Ctrl Pts',(-5.11444386000006,15.2,-10.1011681));
#288542=CARTESIAN_POINT('Ctrl Pts',(-5.11444386000006,11.6,-10.1011681));
#288543=CARTESIAN_POINT('Ctrl Pts',(-5.11166407000006,15.2,-10.098910223));
#288544=CARTESIAN_POINT('Ctrl Pts',(-5.11166407000006,11.6,-10.098910223));
#288545=CARTESIAN_POINT('Ctrl Pts',(-5.10888964600006,15.2,-10.09665313));
#288546=CARTESIAN_POINT('Ctrl Pts',(-5.10888964600006,11.6,-10.09665313));
#288547=CARTESIAN_POINT('Ctrl Pts',(-5.10612059000006,15.2,-10.094396829));
#288548=CARTESIAN_POINT('Ctrl Pts',(-5.10612059000006,11.6,-10.094396829));
#288549=CARTESIAN_POINT('Ctrl Pts',(-5.10335690600006,15.2,-10.092141331));
#288550=CARTESIAN_POINT('Ctrl Pts',(-5.10335690600006,11.6,-10.092141331));
#288551=CARTESIAN_POINT('Ctrl Pts',(-5.10059859200005,15.2,-10.089886644));
#288552=CARTESIAN_POINT('Ctrl Pts',(-5.10059859200005,11.6,-10.089886644));
#288553=CARTESIAN_POINT('Ctrl Pts',(-5.09784565500006,15.2,-10.087632779));
#288554=CARTESIAN_POINT('Ctrl Pts',(-5.09784565500006,11.6,-10.087632779));
#288555=CARTESIAN_POINT('Ctrl Pts',(-5.09509809400006,15.2,-10.085379743));
#288556=CARTESIAN_POINT('Ctrl Pts',(-5.09509809400006,11.6,-10.085379743));
#288557=CARTESIAN_POINT('Ctrl Pts',(-5.09235591200006,15.2,-10.083127549));
#288558=CARTESIAN_POINT('Ctrl Pts',(-5.09235591200006,11.6,-10.083127549));
#288559=CARTESIAN_POINT('Ctrl Pts',(-5.08961911100006,15.2,-10.080876204));
#288560=CARTESIAN_POINT('Ctrl Pts',(-5.08961911100006,11.6,-10.080876204));
#288561=CARTESIAN_POINT('Ctrl Pts',(-5.08688769200006,15.2,-10.078625719));
#288562=CARTESIAN_POINT('Ctrl Pts',(-5.08688769200006,11.6,-10.078625719));
#288563=CARTESIAN_POINT('Ctrl Pts',(-5.08416165800006,15.2,-10.076376102));
#288564=CARTESIAN_POINT('Ctrl Pts',(-5.08416165800006,11.6,-10.076376102));
#288565=CARTESIAN_POINT('Ctrl Pts',(-5.08144101200006,15.2,-10.074127365));
#288566=CARTESIAN_POINT('Ctrl Pts',(-5.08144101200006,11.6,-10.074127365));
#288567=CARTESIAN_POINT('Ctrl Pts',(-5.07872575400006,15.2,-10.071879516));
#288568=CARTESIAN_POINT('Ctrl Pts',(-5.07872575400006,11.6,-10.071879516));
#288569=CARTESIAN_POINT('Ctrl Pts',(-5.07601588800005,15.2,-10.069632565));
#288570=CARTESIAN_POINT('Ctrl Pts',(-5.07601588800005,11.6,-10.069632565));
#288571=CARTESIAN_POINT('Ctrl Pts',(-5.07331141500006,15.2,-10.067386522));
#288572=CARTESIAN_POINT('Ctrl Pts',(-5.07331141500006,11.6,-10.067386522));
#288573=CARTESIAN_POINT('Ctrl Pts',(-5.07061233700006,15.2,-10.065141396));
#288574=CARTESIAN_POINT('Ctrl Pts',(-5.07061233700006,11.6,-10.065141396));
#288575=CARTESIAN_POINT('Ctrl Pts',(-5.06791865700006,15.2,-10.062897196));
#288576=CARTESIAN_POINT('Ctrl Pts',(-5.06791865700006,11.6,-10.062897196));
#288577=CARTESIAN_POINT('Ctrl Pts',(-5.06523037500005,15.2,-10.060653935));
#288578=CARTESIAN_POINT('Ctrl Pts',(-5.06523037500005,11.6,-10.060653935));
#288579=CARTESIAN_POINT('Ctrl Pts',(-5.06254749600005,15.2,-10.05841162));
#288580=CARTESIAN_POINT('Ctrl Pts',(-5.06254749600005,11.6,-10.05841162));
#288581=CARTESIAN_POINT('Ctrl Pts',(-5.05987001900006,15.2,-10.05617026));
#288582=CARTESIAN_POINT('Ctrl Pts',(-5.05987001900006,11.6,-10.05617026));
#288583=CARTESIAN_POINT('Ctrl Pts',(-5.05719794700005,15.2,-10.053929867));
#288584=CARTESIAN_POINT('Ctrl Pts',(-5.05719794700005,11.6,-10.053929867));
#288585=CARTESIAN_POINT('Ctrl Pts',(-5.05453128300006,15.2,-10.051690451));
#288586=CARTESIAN_POINT('Ctrl Pts',(-5.05453128300006,11.6,-10.051690451));
#288587=CARTESIAN_POINT('Ctrl Pts',(-5.05187002900006,15.2,-10.049452021));
#288588=CARTESIAN_POINT('Ctrl Pts',(-5.05187002900006,11.6,-10.049452021));
#288589=CARTESIAN_POINT('Ctrl Pts',(-5.04921418500006,15.2,-10.047214585));
#288590=CARTESIAN_POINT('Ctrl Pts',(-5.04921418500006,11.6,-10.047214585));
#288591=CARTESIAN_POINT('Ctrl Pts',(-5.04656375500006,15.2,-10.044978156));
#288592=CARTESIAN_POINT('Ctrl Pts',(-5.04656375500006,11.6,-10.044978156));
#288593=CARTESIAN_POINT('Ctrl Pts',(-5.04391874100006,15.2,-10.042742742));
#288594=CARTESIAN_POINT('Ctrl Pts',(-5.04391874100006,11.6,-10.042742742));
#288595=CARTESIAN_POINT('Ctrl Pts',(-5.04127914400006,15.2,-10.040508355));
#288596=CARTESIAN_POINT('Ctrl Pts',(-5.04127914400006,11.6,-10.040508355));
#288597=CARTESIAN_POINT('Ctrl Pts',(-5.03864496600006,15.2,-10.038275001));
#288598=CARTESIAN_POINT('Ctrl Pts',(-5.03864496600006,11.6,-10.038275001));
#288599=CARTESIAN_POINT('Ctrl Pts',(-5.03601621000006,15.2,-10.036042694));
#288600=CARTESIAN_POINT('Ctrl Pts',(-5.03601621000006,11.6,-10.036042694));
#288601=CARTESIAN_POINT('Ctrl Pts',(-5.03339287600006,15.2,-10.033811442));
#288602=CARTESIAN_POINT('Ctrl Pts',(-5.03339287600006,11.6,-10.033811442));
#288603=CARTESIAN_POINT('Ctrl Pts',(-5.03077496800006,15.2,-10.031581256));
#288604=CARTESIAN_POINT('Ctrl Pts',(-5.03077496800006,11.6,-10.031581256));
#288605=CARTESIAN_POINT('Ctrl Pts',(-5.02816248700006,15.2,-10.029352144));
#288606=CARTESIAN_POINT('Ctrl Pts',(-5.02816248700006,11.6,-10.029352144));
#288607=CARTESIAN_POINT('Ctrl Pts',(-5.02555543600006,15.2,-10.027124119));
#288608=CARTESIAN_POINT('Ctrl Pts',(-5.02555543600006,11.6,-10.027124119));
#288609=CARTESIAN_POINT('Ctrl Pts',(-5.02295381500006,15.2,-10.024897189));
#288610=CARTESIAN_POINT('Ctrl Pts',(-5.02295381500006,11.6,-10.024897189));
#288611=CARTESIAN_POINT('Ctrl Pts',(-5.02035762800006,15.2,-10.022671365));
#288612=CARTESIAN_POINT('Ctrl Pts',(-5.02035762800006,11.6,-10.022671365));
#288613=CARTESIAN_POINT('Ctrl Pts',(-5.01776687500006,15.2,-10.020446656));
#288614=CARTESIAN_POINT('Ctrl Pts',(-5.01776687500006,11.6,-10.020446656));
#288615=CARTESIAN_POINT('Ctrl Pts',(-5.01518156100006,15.2,-10.018223073));
#288616=CARTESIAN_POINT('Ctrl Pts',(-5.01518156100006,11.6,-10.018223073));
#288617=CARTESIAN_POINT('Ctrl Pts',(-5.01260168500006,15.2,-10.016000626));
#288618=CARTESIAN_POINT('Ctrl Pts',(-5.01260168500006,11.6,-10.016000626));
#288619=CARTESIAN_POINT('Ctrl Pts',(-5.01002724900006,15.2,-10.013779325));
#288620=CARTESIAN_POINT('Ctrl Pts',(-5.01002724900006,11.6,-10.013779325));
#288621=CARTESIAN_POINT('Ctrl Pts',(-5.00745825700006,15.2,-10.011559181));
#288622=CARTESIAN_POINT('Ctrl Pts',(-5.00745825700006,11.6,-10.011559181));
#288623=CARTESIAN_POINT('Ctrl Pts',(-5.00489470900006,15.2,-10.009340204));
#288624=CARTESIAN_POINT('Ctrl Pts',(-5.00489470900006,11.6,-10.009340204));
#288625=CARTESIAN_POINT('Ctrl Pts',(-5.00233660800006,15.2,-10.007122403));
#288626=CARTESIAN_POINT('Ctrl Pts',(-5.00233660800006,11.6,-10.007122403));
#288627=CARTESIAN_POINT('Ctrl Pts',(-4.99978395600006,15.2,-10.004905789));
#288628=CARTESIAN_POINT('Ctrl Pts',(-4.99978395600006,11.6,-10.004905789));
#288629=CARTESIAN_POINT('Ctrl Pts',(-4.99723675400006,15.2,-10.002690373));
#288630=CARTESIAN_POINT('Ctrl Pts',(-4.99723675400006,11.6,-10.002690373));
#288631=CARTESIAN_POINT('Ctrl Pts',(-4.99469500400005,15.2,-10.000476165));
#288632=CARTESIAN_POINT('Ctrl Pts',(-4.99469500400005,11.6,-10.000476165));
#288633=CARTESIAN_POINT('Ctrl Pts',(-4.99215870900006,15.2,-9.99826317500001));
#288634=CARTESIAN_POINT('Ctrl Pts',(-4.99215870900006,11.6,-9.99826317500001));
#288635=CARTESIAN_POINT('Ctrl Pts',(-4.98962787100006,15.2,-9.99605141200002));
#288636=CARTESIAN_POINT('Ctrl Pts',(-4.98962787100006,11.6,-9.99605141200002));
#288637=CARTESIAN_POINT('Ctrl Pts',(-4.98710249000006,15.2,-9.99384088900001));
#288638=CARTESIAN_POINT('Ctrl Pts',(-4.98710249000006,11.6,-9.99384088900001));
#288639=CARTESIAN_POINT('Ctrl Pts',(-4.98458257000006,15.2,-9.99163161400001));
#288640=CARTESIAN_POINT('Ctrl Pts',(-4.98458257000006,11.6,-9.99163161400001));
#288641=CARTESIAN_POINT('Ctrl Pts',(-4.98206811000006,15.2,-9.98942360000001));
#288642=CARTESIAN_POINT('Ctrl Pts',(-4.98206811000006,11.6,-9.98942360000001));
#288643=CARTESIAN_POINT('Ctrl Pts',(-4.97955911600005,15.2,-9.98721685500001));
#288644=CARTESIAN_POINT('Ctrl Pts',(-4.97955911600005,11.6,-9.98721685500001));
#288645=CARTESIAN_POINT('Ctrl Pts',(-4.97705558700006,15.2,-9.98501139100001));
#288646=CARTESIAN_POINT('Ctrl Pts',(-4.97705558700006,11.6,-9.98501139100001));
#288647=CARTESIAN_POINT('Ctrl Pts',(-4.97455752500006,15.2,-9.98280721700001));
#288648=CARTESIAN_POINT('Ctrl Pts',(-4.97455752500006,11.6,-9.98280721700001));
#288649=CARTESIAN_POINT('Ctrl Pts',(-4.97206493300006,15.2,-9.98060434500001));
#288650=CARTESIAN_POINT('Ctrl Pts',(-4.97206493300006,11.6,-9.98060434500001));
#288651=CARTESIAN_POINT('Ctrl Pts',(-4.96957781200006,15.2,-9.97840278500002));
#288652=CARTESIAN_POINT('Ctrl Pts',(-4.96957781200006,11.6,-9.97840278500002));
#288653=CARTESIAN_POINT('Ctrl Pts',(-4.96709616400006,15.2,-9.97620254700001));
#288654=CARTESIAN_POINT('Ctrl Pts',(-4.96709616400006,11.6,-9.97620254700001));
#288655=CARTESIAN_POINT('Ctrl Pts',(-4.96461999100006,15.2,-9.97400364200001));
#288656=CARTESIAN_POINT('Ctrl Pts',(-4.96461999100006,11.6,-9.97400364200001));
#288657=CARTESIAN_POINT('Ctrl Pts',(-4.96214929500006,15.2,-9.97180608100001));
#288658=CARTESIAN_POINT('Ctrl Pts',(-4.96214929500006,11.6,-9.97180608100001));
#288659=CARTESIAN_POINT('Ctrl Pts',(-4.95968407800006,15.2,-9.96960987400001));
#288660=CARTESIAN_POINT('Ctrl Pts',(-4.95968407800006,11.6,-9.96960987400001));
#288661=CARTESIAN_POINT('Ctrl Pts',(-4.95722434300006,15.2,-9.96741503200001));
#288662=CARTESIAN_POINT('Ctrl Pts',(-4.95722434300006,11.6,-9.96741503200001));
#288663=CARTESIAN_POINT('Ctrl Pts',(-4.95477008900005,15.2,-9.96522156500001));
#288664=CARTESIAN_POINT('Ctrl Pts',(-4.95477008900005,11.6,-9.96522156500001));
#288665=CARTESIAN_POINT('Ctrl Pts',(-4.95232131800006,15.2,-9.96302948500001));
#288666=CARTESIAN_POINT('Ctrl Pts',(-4.95232131800006,11.6,-9.96302948500001));
#288667=CARTESIAN_POINT('Ctrl Pts',(-4.94987803400006,15.2,-9.96083880100001));
#288668=CARTESIAN_POINT('Ctrl Pts',(-4.94987803400006,11.6,-9.96083880100001));
#288669=CARTESIAN_POINT('Ctrl Pts',(-4.94744023900005,15.2,-9.95864952500001));
#288670=CARTESIAN_POINT('Ctrl Pts',(-4.94744023900005,11.6,-9.95864952500001));
#288671=CARTESIAN_POINT('Ctrl Pts',(-4.94500793300006,15.2,-9.95646166800001));
#288672=CARTESIAN_POINT('Ctrl Pts',(-4.94500793300006,11.6,-9.95646166800001));
#288673=CARTESIAN_POINT('Ctrl Pts',(-4.94258111800006,15.2,-9.95427523900001));
#288674=CARTESIAN_POINT('Ctrl Pts',(-4.94258111800006,11.6,-9.95427523900001));
#288675=CARTESIAN_POINT('Ctrl Pts',(-4.94015979700006,15.2,-9.95209025100001));
#288676=CARTESIAN_POINT('Ctrl Pts',(-4.94015979700006,11.6,-9.95209025100001));
#288677=CARTESIAN_POINT('Ctrl Pts',(-4.93774397100006,15.2,-9.94990671400001));
#288678=CARTESIAN_POINT('Ctrl Pts',(-4.93774397100006,11.6,-9.94990671400001));
#288679=CARTESIAN_POINT('Ctrl Pts',(-4.93533364100006,15.2,-9.94772463800001));
#288680=CARTESIAN_POINT('Ctrl Pts',(-4.93533364100006,11.6,-9.94772463800001));
#288681=CARTESIAN_POINT('Ctrl Pts',(-4.93292881100006,15.2,-9.94554403400001));
#288682=CARTESIAN_POINT('Ctrl Pts',(-4.93292881100006,11.6,-9.94554403400001));
#288683=CARTESIAN_POINT('Ctrl Pts',(-4.93052948000006,15.2,-9.94336491400001));
#288684=CARTESIAN_POINT('Ctrl Pts',(-4.93052948000006,11.6,-9.94336491400001));
#288685=CARTESIAN_POINT('Ctrl Pts',(-4.92813565300006,15.2,-9.94118728700001));
#288686=CARTESIAN_POINT('Ctrl Pts',(-4.92813565300006,11.6,-9.94118728700001));
#288687=CARTESIAN_POINT('Ctrl Pts',(-4.92574732900006,15.2,-9.93901116700001));
#288688=CARTESIAN_POINT('Ctrl Pts',(-4.92574732900006,11.6,-9.93901116700001));
#288689=CARTESIAN_POINT('Ctrl Pts',(-4.92336451200006,15.2,-9.93683656100002));
#288690=CARTESIAN_POINT('Ctrl Pts',(-4.92336451200006,11.6,-9.93683656100002));
#288691=CARTESIAN_POINT('Ctrl Pts',(-4.92098720200006,15.2,-9.93466348400001));
#288692=CARTESIAN_POINT('Ctrl Pts',(-4.92098720200006,11.6,-9.93466348400001));
#288693=CARTESIAN_POINT('Ctrl Pts',(-4.91861540100006,15.2,-9.93249194400001));
#288694=CARTESIAN_POINT('Ctrl Pts',(-4.91861540100006,11.6,-9.93249194400001));
#288695=CARTESIAN_POINT('Ctrl Pts',(-4.91624911200006,15.2,-9.93032195400001));
#288696=CARTESIAN_POINT('Ctrl Pts',(-4.91624911200006,11.6,-9.93032195400001));
#288697=CARTESIAN_POINT('Ctrl Pts',(-4.91388833500006,15.2,-9.92815352500001));
#288698=CARTESIAN_POINT('Ctrl Pts',(-4.91388833500006,11.6,-9.92815352500001));
#288699=CARTESIAN_POINT('Ctrl Pts',(-4.91153307300006,15.2,-9.92598666500001));
#288700=CARTESIAN_POINT('Ctrl Pts',(-4.91153307300006,11.6,-9.92598666500001));
#288701=CARTESIAN_POINT('Ctrl Pts',(-4.90918332700006,15.2,-9.92382138900001));
#288702=CARTESIAN_POINT('Ctrl Pts',(-4.90918332700006,11.6,-9.92382138900001));
#288703=CARTESIAN_POINT('Ctrl Pts',(-4.90683910000006,15.2,-9.92165770600001));
#288704=CARTESIAN_POINT('Ctrl Pts',(-4.90683910000006,11.6,-9.92165770600001));
#288705=CARTESIAN_POINT('Ctrl Pts',(-4.90450039200006,15.2,-9.91949562800001));
#288706=CARTESIAN_POINT('Ctrl Pts',(-4.90450039200006,11.6,-9.91949562800001));
#288707=CARTESIAN_POINT('Ctrl Pts',(-4.90216720600006,15.2,-9.91733516600001));
#288708=CARTESIAN_POINT('Ctrl Pts',(-4.90216720600006,11.6,-9.91733516600001));
#288709=CARTESIAN_POINT('Ctrl Pts',(-4.89983954300006,15.2,-9.91517633000001));
#288710=CARTESIAN_POINT('Ctrl Pts',(-4.89983954300006,11.6,-9.91517633000001));
#288711=CARTESIAN_POINT('Ctrl Pts',(-4.89751740600005,15.2,-9.91301913400001));
#288712=CARTESIAN_POINT('Ctrl Pts',(-4.89751740600005,11.6,-9.91301913400001));
#288713=CARTESIAN_POINT('Ctrl Pts',(-4.89520079400006,15.2,-9.91086358600001));
#288714=CARTESIAN_POINT('Ctrl Pts',(-4.89520079400006,11.6,-9.91086358600001));
#288715=CARTESIAN_POINT('Ctrl Pts',(-4.89288971100006,15.2,-9.90870970000001));
#288716=CARTESIAN_POINT('Ctrl Pts',(-4.89288971100006,11.6,-9.90870970000001));
#288717=CARTESIAN_POINT('Ctrl Pts',(-4.89058415900006,15.2,-9.90655748600001));
#288718=CARTESIAN_POINT('Ctrl Pts',(-4.89058415900006,11.6,-9.90655748600001));
#288719=CARTESIAN_POINT('Ctrl Pts',(-4.88828413900006,15.2,-9.90440695500001));
#288720=CARTESIAN_POINT('Ctrl Pts',(-4.88828413900006,11.6,-9.90440695500001));
#288721=CARTESIAN_POINT('Ctrl Pts',(-4.88598965300006,15.2,-9.90225811900001));
#288722=CARTESIAN_POINT('Ctrl Pts',(-4.88598965300006,11.6,-9.90225811900001));
#288723=CARTESIAN_POINT('Ctrl Pts',(-4.88370070000006,15.2,-9.90011099000001));
#288724=CARTESIAN_POINT('Ctrl Pts',(-4.88370070000006,11.6,-9.90011099000001));
#288725=CARTESIAN_POINT('Ctrl Pts',(-4.88141728600006,15.2,-9.89796557800001));
#288726=CARTESIAN_POINT('Ctrl Pts',(-4.88141728600006,11.6,-9.89796557800001));
#288727=CARTESIAN_POINT('Ctrl Pts',(-4.87913941000006,15.2,-9.89582189400001));
#288728=CARTESIAN_POINT('Ctrl Pts',(-4.87913941000006,11.6,-9.89582189400001));
#288729=CARTESIAN_POINT('Ctrl Pts',(-4.87686707400006,15.2,-9.89367995200001));
#288730=CARTESIAN_POINT('Ctrl Pts',(-4.87686707400006,11.6,-9.89367995200001));
#288731=CARTESIAN_POINT('Ctrl Pts',(-4.87460028000006,15.2,-9.89153976100001));
#288732=CARTESIAN_POINT('Ctrl Pts',(-4.87460028000006,11.6,-9.89153976100001));
#288733=CARTESIAN_POINT('Ctrl Pts',(-4.87233903000006,15.2,-9.88940133400001));
#288734=CARTESIAN_POINT('Ctrl Pts',(-4.87233903000006,11.6,-9.88940133400001));
#288735=CARTESIAN_POINT('Ctrl Pts',(-4.87008332400006,15.2,-9.88726468300001));
#288736=CARTESIAN_POINT('Ctrl Pts',(-4.87008332400006,11.6,-9.88726468300001));
#288737=CARTESIAN_POINT('Ctrl Pts',(-4.86783316600006,15.2,-9.88512981700001));
#288738=CARTESIAN_POINT('Ctrl Pts',(-4.86783316600006,11.6,-9.88512981700001));
#288739=CARTESIAN_POINT('Ctrl Pts',(-4.86558855600006,15.2,-9.88299675100001));
#288740=CARTESIAN_POINT('Ctrl Pts',(-4.86558855600006,11.6,-9.88299675100001));
#288741=CARTESIAN_POINT('Ctrl Pts',(-4.86334949700006,15.2,-9.88086549300001));
#288742=CARTESIAN_POINT('Ctrl Pts',(-4.86334949700006,11.6,-9.88086549300001));
#288743=CARTESIAN_POINT('Ctrl Pts',(-4.86111598900006,15.2,-9.87873605700001));
#288744=CARTESIAN_POINT('Ctrl Pts',(-4.86111598900006,11.6,-9.87873605700001));
#288745=CARTESIAN_POINT('Ctrl Pts',(-4.85888803500006,15.2,-9.87660845400001));
#288746=CARTESIAN_POINT('Ctrl Pts',(-4.85888803500006,11.6,-9.87660845400001));
#288747=CARTESIAN_POINT('Ctrl Pts',(-4.85666563600006,15.2,-9.87448269700001));
#288748=CARTESIAN_POINT('Ctrl Pts',(-4.85666563600006,11.6,-9.87448269700001));
#288749=CARTESIAN_POINT('Ctrl Pts',(-4.85444879300006,15.2,-9.87235879500002));
#288750=CARTESIAN_POINT('Ctrl Pts',(-4.85444879300006,11.6,-9.87235879500002));
#288751=CARTESIAN_POINT('Ctrl Pts',(-4.85223750900006,15.2,-9.87023676200001));
#288752=CARTESIAN_POINT('Ctrl Pts',(-4.85223750900006,11.6,-9.87023676200001));
#288753=CARTESIAN_POINT('Ctrl Pts',(-4.85003178500006,15.2,-9.86811660900001));
#288754=CARTESIAN_POINT('Ctrl Pts',(-4.85003178500006,11.6,-9.86811660900001));
#288755=CARTESIAN_POINT('Ctrl Pts',(-4.84783162200006,15.2,-9.86599834800001));
#288756=CARTESIAN_POINT('Ctrl Pts',(-4.84783162200006,11.6,-9.86599834800001));
#288757=CARTESIAN_POINT('Ctrl Pts',(-4.84563702200006,15.2,-9.86388199100001));
#288758=CARTESIAN_POINT('Ctrl Pts',(-4.84563702200006,11.6,-9.86388199100001));
#288759=CARTESIAN_POINT('Ctrl Pts',(-4.84344798800006,15.2,-9.86176755000001));
#288760=CARTESIAN_POINT('Ctrl Pts',(-4.84344798800006,11.6,-9.86176755000001));
#288761=CARTESIAN_POINT('Ctrl Pts',(-4.84126451900006,15.2,-9.85965503500001));
#288762=CARTESIAN_POINT('Ctrl Pts',(-4.84126451900006,11.6,-9.85965503500001));
#288763=CARTESIAN_POINT('Ctrl Pts',(-4.83908661800006,15.2,-9.85754446000001));
#288764=CARTESIAN_POINT('Ctrl Pts',(-4.83908661800006,11.6,-9.85754446000001));
#288765=CARTESIAN_POINT('Ctrl Pts',(-4.83691428700006,15.2,-9.85543583700001));
#288766=CARTESIAN_POINT('Ctrl Pts',(-4.83691428700006,11.6,-9.85543583700001));
#288767=CARTESIAN_POINT('Ctrl Pts',(-4.83474752500006,15.2,-9.85332917600001));
#288768=CARTESIAN_POINT('Ctrl Pts',(-4.83474752500006,11.6,-9.85332917600001));
#288769=CARTESIAN_POINT('Ctrl Pts',(-4.83258633700006,15.2,-9.85122449100001));
#288770=CARTESIAN_POINT('Ctrl Pts',(-4.83258633700006,11.6,-9.85122449100001));
#288771=CARTESIAN_POINT('Ctrl Pts',(-4.83043072400006,15.2,-9.84912179400001));
#288772=CARTESIAN_POINT('Ctrl Pts',(-4.83043072400006,11.6,-9.84912179400001));
#288773=CARTESIAN_POINT('Ctrl Pts',(-4.82828068600006,15.2,-9.84702109500001));
#288774=CARTESIAN_POINT('Ctrl Pts',(-4.82828068600006,11.6,-9.84702109500001));
#288775=CARTESIAN_POINT('Ctrl Pts',(-4.82613622400006,15.2,-9.84492240900001));
#288776=CARTESIAN_POINT('Ctrl Pts',(-4.82613622400006,11.6,-9.84492240900001));
#288777=CARTESIAN_POINT('Ctrl Pts',(-4.82399734200006,15.2,-9.84282574600002));
#288778=CARTESIAN_POINT('Ctrl Pts',(-4.82399734200006,11.6,-9.84282574600002));
#288779=CARTESIAN_POINT('Ctrl Pts',(-4.82186404000006,15.2,-9.84073111800001));
#288780=CARTESIAN_POINT('Ctrl Pts',(-4.82186404000006,11.6,-9.84073111800001));
#288781=CARTESIAN_POINT('Ctrl Pts',(-4.81973632000006,15.2,-9.83863853800001));
#288782=CARTESIAN_POINT('Ctrl Pts',(-4.81973632000006,11.6,-9.83863853800001));
#288783=CARTESIAN_POINT('Ctrl Pts',(-4.81761418300006,15.2,-9.83654801900001));
#288784=CARTESIAN_POINT('Ctrl Pts',(-4.81761418300006,11.6,-9.83654801900001));
#288785=CARTESIAN_POINT('Ctrl Pts',(-4.81549763100006,15.2,-9.83445957100001));
#288786=CARTESIAN_POINT('Ctrl Pts',(-4.81549763100006,11.6,-9.83445957100001));
#288787=CARTESIAN_POINT('Ctrl Pts',(-4.81338666500006,15.2,-9.83237320800001));
#288788=CARTESIAN_POINT('Ctrl Pts',(-4.81338666500006,11.6,-9.83237320800001));
#288789=CARTESIAN_POINT('Ctrl Pts',(-4.81128128700006,15.2,-9.83028894200001));
#288790=CARTESIAN_POINT('Ctrl Pts',(-4.81128128700006,11.6,-9.83028894200001));
#288791=CARTESIAN_POINT('Ctrl Pts',(-4.80918149800006,15.2,-9.82820678400001));
#288792=CARTESIAN_POINT('Ctrl Pts',(-4.80918149800006,11.6,-9.82820678400001));
#288793=CARTESIAN_POINT('Ctrl Pts',(-4.80708730100006,15.2,-9.82612674900001));
#288794=CARTESIAN_POINT('Ctrl Pts',(-4.80708730100006,11.6,-9.82612674900001));
#288795=CARTESIAN_POINT('Ctrl Pts',(-4.80499869400006,15.2,-9.82404884800001));
#288796=CARTESIAN_POINT('Ctrl Pts',(-4.80499869400006,11.6,-9.82404884800001));
#288797=CARTESIAN_POINT('Ctrl Pts',(-4.80291568400006,15.2,-9.82197309300001));
#288798=CARTESIAN_POINT('Ctrl Pts',(-4.80291568400006,11.6,-9.82197309300001));
#288799=CARTESIAN_POINT('Ctrl Pts',(-4.80083826700006,15.2,-9.81989949600001));
#288800=CARTESIAN_POINT('Ctrl Pts',(-4.80083826700006,11.6,-9.81989949600001));
#288801=CARTESIAN_POINT('Ctrl Pts',(-4.79876644700005,15.2,-9.81782807100001));
#288802=CARTESIAN_POINT('Ctrl Pts',(-4.79876644700005,11.6,-9.81782807100001));
#288803=CARTESIAN_POINT('Ctrl Pts',(-4.79670022500006,15.2,-9.81575882900001));
#288804=CARTESIAN_POINT('Ctrl Pts',(-4.79670022500006,11.6,-9.81575882900001));
#288805=CARTESIAN_POINT('Ctrl Pts',(-4.79463960400006,15.2,-9.81369178300001));
#288806=CARTESIAN_POINT('Ctrl Pts',(-4.79463960400006,11.6,-9.81369178300001));
#288807=CARTESIAN_POINT('Ctrl Pts',(-4.79258458200006,15.2,-9.81162694600001));
#288808=CARTESIAN_POINT('Ctrl Pts',(-4.79258458200006,11.6,-9.81162694600001));
#288809=CARTESIAN_POINT('Ctrl Pts',(-4.79053516300006,15.2,-9.80956433100001));
#288810=CARTESIAN_POINT('Ctrl Pts',(-4.79053516300006,11.6,-9.80956433100001));
#288811=CARTESIAN_POINT('Ctrl Pts',(-4.78849134900006,15.2,-9.80750394900001));
#288812=CARTESIAN_POINT('Ctrl Pts',(-4.78849134900006,11.6,-9.80750394900001));
#288813=CARTESIAN_POINT('Ctrl Pts',(-4.78645314000006,15.2,-9.80544581400001));
#288814=CARTESIAN_POINT('Ctrl Pts',(-4.78645314000006,11.6,-9.80544581400001));
#288815=CARTESIAN_POINT('Ctrl Pts',(-4.78442053800006,15.2,-9.80338993800001));
#288816=CARTESIAN_POINT('Ctrl Pts',(-4.78442053800006,11.6,-9.80338993800001));
#288817=CARTESIAN_POINT('Ctrl Pts',(-4.78239354400006,15.2,-9.80133633400001));
#288818=CARTESIAN_POINT('Ctrl Pts',(-4.78239354400006,11.6,-9.80133633400001));
#288819=CARTESIAN_POINT('Ctrl Pts',(-4.78037215900006,15.2,-9.79928501500001));
#288820=CARTESIAN_POINT('Ctrl Pts',(-4.78037215900006,11.6,-9.79928501500001));
#288821=CARTESIAN_POINT('Ctrl Pts',(-4.77835638600006,15.2,-9.79723599300001));
#288822=CARTESIAN_POINT('Ctrl Pts',(-4.77835638600006,11.6,-9.79723599300001));
#288823=CARTESIAN_POINT('Ctrl Pts',(-4.77634622500006,15.2,-9.79518928200001));
#288824=CARTESIAN_POINT('Ctrl Pts',(-4.77634622500006,11.6,-9.79518928200001));
#288825=CARTESIAN_POINT('Ctrl Pts',(-4.77434167800006,15.2,-9.79314489300001));
#288826=CARTESIAN_POINT('Ctrl Pts',(-4.77434167800006,11.6,-9.79314489300001));
#288827=CARTESIAN_POINT('Ctrl Pts',(-4.77234274700006,15.2,-9.79110284100001));
#288828=CARTESIAN_POINT('Ctrl Pts',(-4.77234274700006,11.6,-9.79110284100001));
#288829=CARTESIAN_POINT('Ctrl Pts',(-4.77034943200006,15.2,-9.78906313800001));
#288830=CARTESIAN_POINT('Ctrl Pts',(-4.77034943200006,11.6,-9.78906313800001));
#288831=CARTESIAN_POINT('Ctrl Pts',(-4.76836173400006,15.2,-9.78702579500001));
#288832=CARTESIAN_POINT('Ctrl Pts',(-4.76836173400006,11.6,-9.78702579500001));
#288833=CARTESIAN_POINT('Ctrl Pts',(-4.76637965600006,15.2,-9.78499082800001));
#288834=CARTESIAN_POINT('Ctrl Pts',(-4.76637965600006,11.6,-9.78499082800001));
#288835=CARTESIAN_POINT('Ctrl Pts',(-4.76440319900005,15.2,-9.78295824900002));
#288836=CARTESIAN_POINT('Ctrl Pts',(-4.76440319900005,11.6,-9.78295824900002));
#288837=CARTESIAN_POINT('Ctrl Pts',(-4.76243236400006,15.2,-9.78092807100001));
#288838=CARTESIAN_POINT('Ctrl Pts',(-4.76243236400006,11.6,-9.78092807100001));
#288839=CARTESIAN_POINT('Ctrl Pts',(-4.76046715200006,15.2,-9.77890030500001));
#288840=CARTESIAN_POINT('Ctrl Pts',(-4.76046715200006,11.6,-9.77890030500001));
#288841=CARTESIAN_POINT('Ctrl Pts',(-4.75850756600006,15.2,-9.77687496700001));
#288842=CARTESIAN_POINT('Ctrl Pts',(-4.75850756600006,11.6,-9.77687496700001));
#288843=CARTESIAN_POINT('Ctrl Pts',(-4.75655360400006,15.2,-9.77485207000001));
#288844=CARTESIAN_POINT('Ctrl Pts',(-4.75655360400006,11.6,-9.77485207000001));
#288845=CARTESIAN_POINT('Ctrl Pts',(-4.75460527100006,15.2,-9.77283162500001));
#288846=CARTESIAN_POINT('Ctrl Pts',(-4.75460527100006,11.6,-9.77283162500001));
#288847=CARTESIAN_POINT('Ctrl Pts',(-4.75266256600006,15.2,-9.77081364600001));
#288848=CARTESIAN_POINT('Ctrl Pts',(-4.75266256600006,11.6,-9.77081364600001));
#288849=CARTESIAN_POINT('Ctrl Pts',(-4.75072549100005,15.2,-9.76879814700001));
#288850=CARTESIAN_POINT('Ctrl Pts',(-4.75072549100005,11.6,-9.76879814700001));
#288851=CARTESIAN_POINT('Ctrl Pts',(-4.74879404800006,15.2,-9.76678514200001));
#288852=CARTESIAN_POINT('Ctrl Pts',(-4.74879404800006,11.6,-9.76678514200001));
#288853=CARTESIAN_POINT('Ctrl Pts',(-4.74686823700006,15.2,-9.76477464200001));
#288854=CARTESIAN_POINT('Ctrl Pts',(-4.74686823700006,11.6,-9.76477464200001));
#288855=CARTESIAN_POINT('Ctrl Pts',(-4.74494806000005,15.2,-9.76276666100001));
#288856=CARTESIAN_POINT('Ctrl Pts',(-4.74494806000005,11.6,-9.76276666100001));
#288857=CARTESIAN_POINT('Ctrl Pts',(-4.74303351900006,15.2,-9.76076121400001));
#288858=CARTESIAN_POINT('Ctrl Pts',(-4.74303351900006,11.6,-9.76076121400001));
#288859=CARTESIAN_POINT('Ctrl Pts',(-4.74112461300006,15.2,-9.75875831300001));
#288860=CARTESIAN_POINT('Ctrl Pts',(-4.74112461300006,11.6,-9.75875831300001));
#288861=CARTESIAN_POINT('Ctrl Pts',(-4.73922134700006,15.2,-9.75675797100001));
#288862=CARTESIAN_POINT('Ctrl Pts',(-4.73922134700006,11.6,-9.75675797100001));
#288863=CARTESIAN_POINT('Ctrl Pts',(-4.73732371800006,15.2,-9.75476020200001));
#288864=CARTESIAN_POINT('Ctrl Pts',(-4.73732371800006,11.6,-9.75476020200001));
#288865=CARTESIAN_POINT('Ctrl Pts',(-4.73543173000006,15.2,-9.75276502000001));
#288866=CARTESIAN_POINT('Ctrl Pts',(-4.73543173000006,11.6,-9.75276502000001));
#288867=CARTESIAN_POINT('Ctrl Pts',(-4.73354538400006,15.2,-9.75077243800001));
#288868=CARTESIAN_POINT('Ctrl Pts',(-4.73354538400006,11.6,-9.75077243800001));
#288869=CARTESIAN_POINT('Ctrl Pts',(-4.73166468000006,15.2,-9.74878247000001));
#288870=CARTESIAN_POINT('Ctrl Pts',(-4.73166468000006,11.6,-9.74878247000001));
#288871=CARTESIAN_POINT('Ctrl Pts',(-4.72978962100005,15.2,-9.74679512800001));
#288872=CARTESIAN_POINT('Ctrl Pts',(-4.72978962100005,11.6,-9.74679512800001));
#288873=CARTESIAN_POINT('Ctrl Pts',(-4.72792020700005,15.2,-9.74481042800001));
#288874=CARTESIAN_POINT('Ctrl Pts',(-4.72792020700005,11.6,-9.74481042800001));
#288875=CARTESIAN_POINT('Ctrl Pts',(-4.72605643800006,15.2,-9.74282838300001));
#288876=CARTESIAN_POINT('Ctrl Pts',(-4.72605643800006,11.6,-9.74282838300001));
#288877=CARTESIAN_POINT('Ctrl Pts',(-4.72419831900006,15.2,-9.74084900500001));
#288878=CARTESIAN_POINT('Ctrl Pts',(-4.72419831900006,11.6,-9.74084900500001));
#288879=CARTESIAN_POINT('Ctrl Pts',(-4.72234584800006,15.2,-9.73887231000001));
#288880=CARTESIAN_POINT('Ctrl Pts',(-4.72234584800006,11.6,-9.73887231000001));
#288881=CARTESIAN_POINT('Ctrl Pts',(-4.72049902600006,15.2,-9.73689831000001));
#288882=CARTESIAN_POINT('Ctrl Pts',(-4.72049902600006,11.6,-9.73689831000001));
#288883=CARTESIAN_POINT('Ctrl Pts',(-4.71865785700006,15.2,-9.73492702100001));
#288884=CARTESIAN_POINT('Ctrl Pts',(-4.71865785700006,11.6,-9.73492702100001));
#288885=CARTESIAN_POINT('Ctrl Pts',(-4.71682234000006,15.2,-9.73295845400001));
#288886=CARTESIAN_POINT('Ctrl Pts',(-4.71682234000006,11.6,-9.73295845400001));
#288887=CARTESIAN_POINT('Ctrl Pts',(-4.71499247600006,15.2,-9.73099262400001));
#288888=CARTESIAN_POINT('Ctrl Pts',(-4.71499247600006,11.6,-9.73099262400001));
#288889=CARTESIAN_POINT('Ctrl Pts',(-4.71316826800006,15.2,-9.72902954600001));
#288890=CARTESIAN_POINT('Ctrl Pts',(-4.71316826800006,11.6,-9.72902954600001));
#288891=CARTESIAN_POINT('Ctrl Pts',(-4.71134971600006,15.2,-9.72706923300001));
#288892=CARTESIAN_POINT('Ctrl Pts',(-4.71134971600006,11.6,-9.72706923300001));
#288893=CARTESIAN_POINT('Ctrl Pts',(-4.70953682100006,15.2,-9.72511169900001));
#288894=CARTESIAN_POINT('Ctrl Pts',(-4.70953682100006,11.6,-9.72511169900001));
#288895=CARTESIAN_POINT('Ctrl Pts',(-4.70772958400006,15.2,-9.72315696000001));
#288896=CARTESIAN_POINT('Ctrl Pts',(-4.70772958400006,11.6,-9.72315696000001));
#288897=CARTESIAN_POINT('Ctrl Pts',(-4.70592800700006,15.2,-9.72120502600001));
#288898=CARTESIAN_POINT('Ctrl Pts',(-4.70592800700006,11.6,-9.72120502600001));
#288899=CARTESIAN_POINT('Ctrl Pts',(-4.70413209100006,15.2,-9.71925591500001));
#288900=CARTESIAN_POINT('Ctrl Pts',(-4.70413209100006,11.6,-9.71925591500001));
#288901=CARTESIAN_POINT('Ctrl Pts',(-4.70234183600006,15.2,-9.71730963800001));
#288902=CARTESIAN_POINT('Ctrl Pts',(-4.70234183600006,11.6,-9.71730963800001));
#288903=CARTESIAN_POINT('Ctrl Pts',(-4.70055724400006,15.2,-9.71536621100001));
#288904=CARTESIAN_POINT('Ctrl Pts',(-4.70055724400006,11.6,-9.71536621100001));
#288905=CARTESIAN_POINT('Ctrl Pts',(-4.69877831600006,15.2,-9.71342564900001));
#288906=CARTESIAN_POINT('Ctrl Pts',(-4.69877831600006,11.6,-9.71342564900001));
#288907=CARTESIAN_POINT('Ctrl Pts',(-4.69700505400006,15.2,-9.71148796400001));
#288908=CARTESIAN_POINT('Ctrl Pts',(-4.69700505400006,11.6,-9.71148796400001));
#288909=CARTESIAN_POINT('Ctrl Pts',(-4.69523745700006,15.2,-9.70955317200001));
#288910=CARTESIAN_POINT('Ctrl Pts',(-4.69523745700006,11.6,-9.70955317200001));
#288911=CARTESIAN_POINT('Ctrl Pts',(-4.69347552900006,15.2,-9.70762128700001));
#288912=CARTESIAN_POINT('Ctrl Pts',(-4.69347552900006,11.6,-9.70762128700001));
#288913=CARTESIAN_POINT('Ctrl Pts',(-4.69171926900006,15.2,-9.70569232300001));
#288914=CARTESIAN_POINT('Ctrl Pts',(-4.69171926900006,11.6,-9.70569232300001));
#288915=CARTESIAN_POINT('Ctrl Pts',(-4.68996867800006,15.2,-9.70376629500001));
#288916=CARTESIAN_POINT('Ctrl Pts',(-4.68996867800006,11.6,-9.70376629500001));
#288917=CARTESIAN_POINT('Ctrl Pts',(-4.68822375800006,15.2,-9.70184321600001));
#288918=CARTESIAN_POINT('Ctrl Pts',(-4.68822375800006,11.6,-9.70184321600001));
#288919=CARTESIAN_POINT('Ctrl Pts',(-4.68648450900006,15.2,-9.69992310200001));
#288920=CARTESIAN_POINT('Ctrl Pts',(-4.68648450900006,11.6,-9.69992310200001));
#288921=CARTESIAN_POINT('Ctrl Pts',(-4.68475093300006,15.2,-9.69800596700001));
#288922=CARTESIAN_POINT('Ctrl Pts',(-4.68475093300006,11.6,-9.69800596700001));
#288923=CARTESIAN_POINT('Ctrl Pts',(-4.68302303100006,15.2,-9.69609182500001));
#288924=CARTESIAN_POINT('Ctrl Pts',(-4.68302303100006,11.6,-9.69609182500001));
#288925=CARTESIAN_POINT('Ctrl Pts',(-4.68130080400006,15.2,-9.69418069300001));
#288926=CARTESIAN_POINT('Ctrl Pts',(-4.68130080400006,11.6,-9.69418069300001));
#288927=CARTESIAN_POINT('Ctrl Pts',(-4.67958425200006,15.2,-9.69227258200001));
#288928=CARTESIAN_POINT('Ctrl Pts',(-4.67958425200006,11.6,-9.69227258200001));
#288929=CARTESIAN_POINT('Ctrl Pts',(-4.67787337700006,15.2,-9.69036751000001));
#288930=CARTESIAN_POINT('Ctrl Pts',(-4.67787337700006,11.6,-9.69036751000001));
#288931=CARTESIAN_POINT('Ctrl Pts',(-4.67616818100006,15.2,-9.68846548900001));
#288932=CARTESIAN_POINT('Ctrl Pts',(-4.67616818100006,11.6,-9.68846548900001));
#288933=CARTESIAN_POINT('Ctrl Pts',(-4.67446866400006,15.2,-9.68656653500001));
#288934=CARTESIAN_POINT('Ctrl Pts',(-4.67446866400006,11.6,-9.68656653500001));
#288935=CARTESIAN_POINT('Ctrl Pts',(-4.67277482600006,15.2,-9.68467066400001));
#288936=CARTESIAN_POINT('Ctrl Pts',(-4.67277482600006,11.6,-9.68467066400001));
#288937=CARTESIAN_POINT('Ctrl Pts',(-4.67108666900006,15.2,-9.68277788900001));
#288938=CARTESIAN_POINT('Ctrl Pts',(-4.67108666900006,11.6,-9.68277788900001));
#288939=CARTESIAN_POINT('Ctrl Pts',(-4.66940419400006,15.2,-9.68088822600001));
#288940=CARTESIAN_POINT('Ctrl Pts',(-4.66940419400006,11.6,-9.68088822600001));
#288941=CARTESIAN_POINT('Ctrl Pts',(-4.66772740200006,15.2,-9.67900168900002));
#288942=CARTESIAN_POINT('Ctrl Pts',(-4.66772740200006,11.6,-9.67900168900002));
#288943=CARTESIAN_POINT('Ctrl Pts',(-4.66605629400005,15.2,-9.67711829300001));
#288944=CARTESIAN_POINT('Ctrl Pts',(-4.66605629400005,11.6,-9.67711829300001));
#288945=CARTESIAN_POINT('Ctrl Pts',(-4.66439087100006,15.2,-9.67523805500001));
#288946=CARTESIAN_POINT('Ctrl Pts',(-4.66439087100006,11.6,-9.67523805500001));
#288947=CARTESIAN_POINT('Ctrl Pts',(-4.66273113300006,15.2,-9.67336098700001));
#288948=CARTESIAN_POINT('Ctrl Pts',(-4.66273113300006,11.6,-9.67336098700001));
#288949=CARTESIAN_POINT('Ctrl Pts',(-4.66107708300005,15.2,-9.67148710700001));
#288950=CARTESIAN_POINT('Ctrl Pts',(-4.66107708300005,11.6,-9.67148710700001));
#288951=CARTESIAN_POINT('Ctrl Pts',(-4.65942871900006,15.2,-9.66961642800001));
#288952=CARTESIAN_POINT('Ctrl Pts',(-4.65942871900006,11.6,-9.66961642800001));
#288953=CARTESIAN_POINT('Ctrl Pts',(-4.65778604600006,15.2,-9.66774896500001));
#288954=CARTESIAN_POINT('Ctrl Pts',(-4.65778604600006,11.6,-9.66774896500001));
#288955=CARTESIAN_POINT('Ctrl Pts',(-4.65614906000006,15.2,-9.66588473600001));
#288956=CARTESIAN_POINT('Ctrl Pts',(-4.65614906000006,11.6,-9.66588473600001));
#288957=CARTESIAN_POINT('Ctrl Pts',(-4.65451776600006,15.2,-9.66402375300001));
#288958=CARTESIAN_POINT('Ctrl Pts',(-4.65451776600006,11.6,-9.66402375300001));
#288959=CARTESIAN_POINT('Ctrl Pts',(-4.65289216200006,15.2,-9.66216603400001));
#288960=CARTESIAN_POINT('Ctrl Pts',(-4.65289216200006,11.6,-9.66216603400001));
#288961=CARTESIAN_POINT('Ctrl Pts',(-4.65127225200006,15.2,-9.66031159200002));
#288962=CARTESIAN_POINT('Ctrl Pts',(-4.65127225200006,11.6,-9.66031159200002));
#288963=CARTESIAN_POINT('Ctrl Pts',(-4.64965803500006,15.2,-9.65846044500001));
#288964=CARTESIAN_POINT('Ctrl Pts',(-4.64965803500006,11.6,-9.65846044500001));
#288965=CARTESIAN_POINT('Ctrl Pts',(-4.64804951100006,15.2,-9.65661260600001));
#288966=CARTESIAN_POINT('Ctrl Pts',(-4.64804951100006,11.6,-9.65661260600001));
#288967=CARTESIAN_POINT('Ctrl Pts',(-4.64644668200005,15.2,-9.65476809100001));
#288968=CARTESIAN_POINT('Ctrl Pts',(-4.64644668200005,11.6,-9.65476809100001));
#288969=CARTESIAN_POINT('Ctrl Pts',(-4.64484955000006,15.2,-9.65292691600001));
#288970=CARTESIAN_POINT('Ctrl Pts',(-4.64484955000006,11.6,-9.65292691600001));
#288971=CARTESIAN_POINT('Ctrl Pts',(-4.64325811300006,15.2,-9.65108909800002));
#288972=CARTESIAN_POINT('Ctrl Pts',(-4.64325811300006,11.6,-9.65108909800002));
#288973=CARTESIAN_POINT('Ctrl Pts',(-4.64167237400006,15.2,-9.64925464900002));
#288974=CARTESIAN_POINT('Ctrl Pts',(-4.64167237400006,11.6,-9.64925464900002));
#288975=CARTESIAN_POINT('Ctrl Pts',(-4.64009233400006,15.2,-9.64742358800001));
#288976=CARTESIAN_POINT('Ctrl Pts',(-4.64009233400006,11.6,-9.64742358800001));
#288977=CARTESIAN_POINT('Ctrl Pts',(-4.63851799300006,15.2,-9.64559593000001));
#288978=CARTESIAN_POINT('Ctrl Pts',(-4.63851799300006,11.6,-9.64559593000001));
#288979=CARTESIAN_POINT('Ctrl Pts',(-4.63694935100006,15.2,-9.64377169000001));
#288980=CARTESIAN_POINT('Ctrl Pts',(-4.63694935100006,11.6,-9.64377169000001));
#288981=CARTESIAN_POINT('Ctrl Pts',(-4.63538641100006,15.2,-9.64195088400002));
#288982=CARTESIAN_POINT('Ctrl Pts',(-4.63538641100006,11.6,-9.64195088400002));
#288983=CARTESIAN_POINT('Ctrl Pts',(-4.63382917200006,15.2,-9.64013352800002));
#288984=CARTESIAN_POINT('Ctrl Pts',(-4.63382917200006,11.6,-9.64013352800002));
#288985=CARTESIAN_POINT('Ctrl Pts',(-4.63227763500006,15.2,-9.63831963700001));
#288986=CARTESIAN_POINT('Ctrl Pts',(-4.63227763500006,11.6,-9.63831963700001));
#288987=CARTESIAN_POINT('Ctrl Pts',(-4.63073180200006,15.2,-9.63650922900002));
#288988=CARTESIAN_POINT('Ctrl Pts',(-4.63073180200006,11.6,-9.63650922900002));
#288989=CARTESIAN_POINT('Ctrl Pts',(-4.62919167300006,15.2,-9.63470231700001));
#288990=CARTESIAN_POINT('Ctrl Pts',(-4.62919167300006,11.6,-9.63470231700001));
#288991=CARTESIAN_POINT('Ctrl Pts',(-4.62765724900006,15.2,-9.63289892000001));
#288992=CARTESIAN_POINT('Ctrl Pts',(-4.62765724900006,11.6,-9.63289892000001));
#288993=CARTESIAN_POINT('Ctrl Pts',(-4.62612853000006,15.2,-9.63109905300002));
#288994=CARTESIAN_POINT('Ctrl Pts',(-4.62612853000006,11.6,-9.63109905300002));
#288995=CARTESIAN_POINT('Ctrl Pts',(-4.62460551700006,15.2,-9.62930273200002));
#288996=CARTESIAN_POINT('Ctrl Pts',(-4.62460551700006,11.6,-9.62930273200002));
#288997=CARTESIAN_POINT('Ctrl Pts',(-4.62308821200006,15.2,-9.62750997300001));
#288998=CARTESIAN_POINT('Ctrl Pts',(-4.62308821200006,11.6,-9.62750997300001));
#288999=CARTESIAN_POINT('Ctrl Pts',(-4.62157661300005,15.2,-9.62572079200001));
#289000=CARTESIAN_POINT('Ctrl Pts',(-4.62157661300005,11.6,-9.62572079200001));
#289001=CARTESIAN_POINT('Ctrl Pts',(-4.62007072500006,15.2,-9.62393520600001));
#289002=CARTESIAN_POINT('Ctrl Pts',(-4.62007072500006,11.6,-9.62393520600001));
#289003=CARTESIAN_POINT('Ctrl Pts',(-4.61857054400006,15.2,-9.62215323100001));
#289004=CARTESIAN_POINT('Ctrl Pts',(-4.61857054400006,11.6,-9.62215323100001));
#289005=CARTESIAN_POINT('Ctrl Pts',(-4.61707607400006,15.2,-9.62037488300002));
#289006=CARTESIAN_POINT('Ctrl Pts',(-4.61707607400006,11.6,-9.62037488300002));
#289007=CARTESIAN_POINT('Ctrl Pts',(-4.61558731500006,15.2,-9.61860017900002));
#289008=CARTESIAN_POINT('Ctrl Pts',(-4.61558731500006,11.6,-9.61860017900002));
#289009=CARTESIAN_POINT('Ctrl Pts',(-4.61410426600006,15.2,-9.61682913500002));
#289010=CARTESIAN_POINT('Ctrl Pts',(-4.61410426600006,11.6,-9.61682913500002));
#289011=CARTESIAN_POINT('Ctrl Pts',(-4.61262692900006,15.2,-9.61506176800001));
#289012=CARTESIAN_POINT('Ctrl Pts',(-4.61262692900006,11.6,-9.61506176800001));
#289013=CARTESIAN_POINT('Ctrl Pts',(-4.61115530500006,15.2,-9.61329809500001));
#289014=CARTESIAN_POINT('Ctrl Pts',(-4.61115530500006,11.6,-9.61329809500001));
#289015=CARTESIAN_POINT('Ctrl Pts',(-4.60968939500006,15.2,-9.61153813100001));
#289016=CARTESIAN_POINT('Ctrl Pts',(-4.60968939500006,11.6,-9.61153813100001));
#289017=CARTESIAN_POINT('Ctrl Pts',(-4.60822919900005,15.2,-9.60978189400001));
#289018=CARTESIAN_POINT('Ctrl Pts',(-4.60822919900005,11.6,-9.60978189400001));
#289019=CARTESIAN_POINT('Ctrl Pts',(-4.60677471800006,15.2,-9.60802939900002));
#289020=CARTESIAN_POINT('Ctrl Pts',(-4.60677471800006,11.6,-9.60802939900002));
#289021=CARTESIAN_POINT('Ctrl Pts',(-4.60532595100006,15.2,-9.60628066500002));
#289022=CARTESIAN_POINT('Ctrl Pts',(-4.60532595100006,11.6,-9.60628066500002));
#289023=CARTESIAN_POINT('Ctrl Pts',(-4.60388290000005,15.2,-9.60453570900001));
#289024=CARTESIAN_POINT('Ctrl Pts',(-4.60388290000005,11.6,-9.60453570900001));
#289025=CARTESIAN_POINT('Ctrl Pts',(-4.60244556700006,15.2,-9.60279454500002));
#289026=CARTESIAN_POINT('Ctrl Pts',(-4.60244556700006,11.6,-9.60279454500002));
#289027=CARTESIAN_POINT('Ctrl Pts',(-4.60101394900006,15.2,-9.60105719300002));
#289028=CARTESIAN_POINT('Ctrl Pts',(-4.60101394900006,11.6,-9.60105719300002));
#289029=CARTESIAN_POINT('Ctrl Pts',(-4.59958805000006,15.2,-9.59932366700002));
#289030=CARTESIAN_POINT('Ctrl Pts',(-4.59958805000006,11.6,-9.59932366700002));
#289031=CARTESIAN_POINT('Ctrl Pts',(-4.59816786800006,15.2,-9.59759398700001));
#289032=CARTESIAN_POINT('Ctrl Pts',(-4.59816786800006,11.6,-9.59759398700001));
#289033=CARTESIAN_POINT('Ctrl Pts',(-4.59675340700006,15.2,-9.59586816800002));
#289034=CARTESIAN_POINT('Ctrl Pts',(-4.59675340700006,11.6,-9.59586816800002));
#289035=CARTESIAN_POINT('Ctrl Pts',(-4.59534466400005,15.2,-9.59414622900002));
#289036=CARTESIAN_POINT('Ctrl Pts',(-4.59534466400005,11.6,-9.59414622900002));
#289037=CARTESIAN_POINT('Ctrl Pts',(-4.59394164100006,15.2,-9.59242818500002));
#289038=CARTESIAN_POINT('Ctrl Pts',(-4.59394164100006,11.6,-9.59242818500002));
#289039=CARTESIAN_POINT('Ctrl Pts',(-4.59254434000006,15.2,-9.59071405400002));
#289040=CARTESIAN_POINT('Ctrl Pts',(-4.59254434000006,11.6,-9.59071405400002));
#289041=CARTESIAN_POINT('Ctrl Pts',(-4.59115275800006,15.2,-9.58900385500002));
#289042=CARTESIAN_POINT('Ctrl Pts',(-4.59115275800006,11.6,-9.58900385500002));
#289043=CARTESIAN_POINT('Ctrl Pts',(-4.58976689900005,15.2,-9.58729760200002));
#289044=CARTESIAN_POINT('Ctrl Pts',(-4.58976689900005,11.6,-9.58729760200002));
#289045=CARTESIAN_POINT('Ctrl Pts',(-4.58838676200005,15.2,-9.58559531600002));
#289046=CARTESIAN_POINT('Ctrl Pts',(-4.58838676200005,11.6,-9.58559531600002));
#289047=CARTESIAN_POINT('Ctrl Pts',(-4.58701234700006,15.2,-9.58389701100002));
#289048=CARTESIAN_POINT('Ctrl Pts',(-4.58701234700006,11.6,-9.58389701100002));
#289049=CARTESIAN_POINT('Ctrl Pts',(-4.58564365600005,15.2,-9.58220270700001));
#289050=CARTESIAN_POINT('Ctrl Pts',(-4.58564365600005,11.6,-9.58220270700001));
#289051=CARTESIAN_POINT('Ctrl Pts',(-4.58428068800006,15.2,-9.58051242200002));
#289052=CARTESIAN_POINT('Ctrl Pts',(-4.58428068800006,11.6,-9.58051242200002));
#289053=CARTESIAN_POINT('Ctrl Pts',(-4.58292344400006,15.2,-9.57882617100001));
#289054=CARTESIAN_POINT('Ctrl Pts',(-4.58292344400006,11.6,-9.57882617100001));
#289055=CARTESIAN_POINT('Ctrl Pts',(-4.58157192500006,15.2,-9.57714397300002));
#289056=CARTESIAN_POINT('Ctrl Pts',(-4.58157192500006,11.6,-9.57714397300002));
#289057=CARTESIAN_POINT('Ctrl Pts',(-4.58022613100006,15.2,-9.57546584700001));
#289058=CARTESIAN_POINT('Ctrl Pts',(-4.58022613100006,11.6,-9.57546584700001));
#289059=CARTESIAN_POINT('Ctrl Pts',(-4.57888606300005,15.2,-9.57379180900002));
#289060=CARTESIAN_POINT('Ctrl Pts',(-4.57888606300005,11.6,-9.57379180900002));
#289061=CARTESIAN_POINT('Ctrl Pts',(-4.57755172000006,15.2,-9.57212187800002));
#289062=CARTESIAN_POINT('Ctrl Pts',(-4.57755172000006,11.6,-9.57212187800002));
#289063=CARTESIAN_POINT('Ctrl Pts',(-4.57622310400006,15.2,-9.57045607000002));
#289064=CARTESIAN_POINT('Ctrl Pts',(-4.57622310400006,11.6,-9.57045607000002));
#289065=CARTESIAN_POINT('Ctrl Pts',(-4.57490021400006,15.2,-9.56879440500002));
#289066=CARTESIAN_POINT('Ctrl Pts',(-4.57490021400006,11.6,-9.56879440500002));
#289067=CARTESIAN_POINT('Ctrl Pts',(-4.57358305300006,15.2,-9.56713690100001));
#289068=CARTESIAN_POINT('Ctrl Pts',(-4.57358305300006,11.6,-9.56713690100001));
#289069=CARTESIAN_POINT('Ctrl Pts',(-4.57227161800006,15.2,-9.56548357500001));
#289070=CARTESIAN_POINT('Ctrl Pts',(-4.57227161800006,11.6,-9.56548357500001));
#289071=CARTESIAN_POINT('Ctrl Pts',(-4.57096591100006,15.2,-9.56383444500002));
#289072=CARTESIAN_POINT('Ctrl Pts',(-4.57096591100006,11.6,-9.56383444500002));
#289073=CARTESIAN_POINT('Ctrl Pts',(-4.56966593300006,15.2,-9.56218953000001));
#289074=CARTESIAN_POINT('Ctrl Pts',(-4.56966593300006,11.6,-9.56218953000001));
#289075=CARTESIAN_POINT('Ctrl Pts',(-4.56837168400006,15.2,-9.56054884700002));
#289076=CARTESIAN_POINT('Ctrl Pts',(-4.56837168400006,11.6,-9.56054884700002));
#289077=CARTESIAN_POINT('Ctrl Pts',(-4.56708316400006,15.2,-9.55891241700002));
#289078=CARTESIAN_POINT('Ctrl Pts',(-4.56708316400006,11.6,-9.55891241700002));
#289079=CARTESIAN_POINT('Ctrl Pts',(-4.56580037200006,15.2,-9.55728025600001));
#289080=CARTESIAN_POINT('Ctrl Pts',(-4.56580037200006,11.6,-9.55728025600001));
#289081=CARTESIAN_POINT('Ctrl Pts',(-4.56452331100006,15.2,-9.55565238200002));
#289082=CARTESIAN_POINT('Ctrl Pts',(-4.56452331100006,11.6,-9.55565238200002));
#289083=CARTESIAN_POINT('Ctrl Pts',(-4.56325198000005,15.2,-9.55402881600002));
#289084=CARTESIAN_POINT('Ctrl Pts',(-4.56325198000005,11.6,-9.55402881600002));
#289085=CARTESIAN_POINT('Ctrl Pts',(-4.56198637900005,15.2,-9.55240957400001));
#289086=CARTESIAN_POINT('Ctrl Pts',(-4.56198637900005,11.6,-9.55240957400001));
#289087=CARTESIAN_POINT('Ctrl Pts',(-4.56072650900006,15.2,-9.55079467600001));
#289088=CARTESIAN_POINT('Ctrl Pts',(-4.56072650900006,11.6,-9.55079467600001));
#289089=CARTESIAN_POINT('Ctrl Pts',(-4.55947237000006,15.2,-9.54918414100002));
#289090=CARTESIAN_POINT('Ctrl Pts',(-4.55947237000006,11.6,-9.54918414100002));
#289091=CARTESIAN_POINT('Ctrl Pts',(-4.55822396200006,15.2,-9.54757798600001));
#289092=CARTESIAN_POINT('Ctrl Pts',(-4.55822396200006,11.6,-9.54757798600001));
#289093=CARTESIAN_POINT('Ctrl Pts',(-4.55698128600006,15.2,-9.54597623200002));
#289094=CARTESIAN_POINT('Ctrl Pts',(-4.55698128600006,11.6,-9.54597623200002));
#289095=CARTESIAN_POINT('Ctrl Pts',(-4.55574434200006,15.2,-9.54437889600002));
#289096=CARTESIAN_POINT('Ctrl Pts',(-4.55574434200006,11.6,-9.54437889600002));
#289097=CARTESIAN_POINT('Ctrl Pts',(-4.55451312900006,15.2,-9.54278599800002));
#289098=CARTESIAN_POINT('Ctrl Pts',(-4.55451312900006,11.6,-9.54278599800002));
#289099=CARTESIAN_POINT('Ctrl Pts',(-4.55328764900006,15.2,-9.54119755600002));
#289100=CARTESIAN_POINT('Ctrl Pts',(-4.55328764900006,11.6,-9.54119755600002));
#289101=CARTESIAN_POINT('Ctrl Pts',(-4.55206790200006,15.2,-9.53961359000001));
#289102=CARTESIAN_POINT('Ctrl Pts',(-4.55206790200006,11.6,-9.53961359000001));
#289103=CARTESIAN_POINT('Ctrl Pts',(-4.55085388600006,15.2,-9.53803412000001));
#289104=CARTESIAN_POINT('Ctrl Pts',(-4.55085388600006,11.6,-9.53803412000001));
#289105=CARTESIAN_POINT('Ctrl Pts',(-4.54964560400006,15.2,-9.53645916200001));
#289106=CARTESIAN_POINT('Ctrl Pts',(-4.54964560400006,11.6,-9.53645916200001));
#289107=CARTESIAN_POINT('Ctrl Pts',(-4.54844305500006,15.2,-9.53488873800002));
#289108=CARTESIAN_POINT('Ctrl Pts',(-4.54844305500006,11.6,-9.53488873800002));
#289109=CARTESIAN_POINT('Ctrl Pts',(-4.54724624000006,15.2,-9.53332286700002));
#289110=CARTESIAN_POINT('Ctrl Pts',(-4.54724624000006,11.6,-9.53332286700002));
#289111=CARTESIAN_POINT('Ctrl Pts',(-4.54605515800006,15.2,-9.53176156700002));
#289112=CARTESIAN_POINT('Ctrl Pts',(-4.54605515800006,11.6,-9.53176156700002));
#289113=CARTESIAN_POINT('Ctrl Pts',(-4.54486980900006,15.2,-9.53020485900002));
#289114=CARTESIAN_POINT('Ctrl Pts',(-4.54486980900006,11.6,-9.53020485900002));
#289115=CARTESIAN_POINT('Ctrl Pts',(-4.54369019500006,15.2,-9.52865276200002));
#289116=CARTESIAN_POINT('Ctrl Pts',(-4.54369019500006,11.6,-9.52865276200002));
#289117=CARTESIAN_POINT('Ctrl Pts',(-4.54251631400005,15.2,-9.52710529400001));
#289118=CARTESIAN_POINT('Ctrl Pts',(-4.54251631400005,11.6,-9.52710529400001));
#289119=CARTESIAN_POINT('Ctrl Pts',(-4.54134816700006,15.2,-9.52556247700001));
#289120=CARTESIAN_POINT('Ctrl Pts',(-4.54134816700006,11.6,-9.52556247700001));
#289121=CARTESIAN_POINT('Ctrl Pts',(-4.54018575500006,15.2,-9.52402433000002));
#289122=CARTESIAN_POINT('Ctrl Pts',(-4.54018575500006,11.6,-9.52402433000002));
#289123=CARTESIAN_POINT('Ctrl Pts',(-4.53902907600006,15.2,-9.52249087200002));
#289124=CARTESIAN_POINT('Ctrl Pts',(-4.53902907600006,11.6,-9.52249087200002));
#289125=CARTESIAN_POINT('Ctrl Pts',(-4.53787813200006,15.2,-9.52096212300001));
#289126=CARTESIAN_POINT('Ctrl Pts',(-4.53787813200006,11.6,-9.52096212300001));
#289127=CARTESIAN_POINT('Ctrl Pts',(-4.53673292200006,15.2,-9.51943810400002));
#289128=CARTESIAN_POINT('Ctrl Pts',(-4.53673292200006,11.6,-9.51943810400002));
#289129=CARTESIAN_POINT('Ctrl Pts',(-4.53559344600006,15.2,-9.51791883400002));
#289130=CARTESIAN_POINT('Ctrl Pts',(-4.53559344600006,11.6,-9.51791883400002));
#289131=CARTESIAN_POINT('Ctrl Pts',(-4.53445970600006,15.2,-9.51640433300001));
#289132=CARTESIAN_POINT('Ctrl Pts',(-4.53445970600006,11.6,-9.51640433300001));
#289133=CARTESIAN_POINT('Ctrl Pts',(-4.53333169900006,15.2,-9.51489462100002));
#289134=CARTESIAN_POINT('Ctrl Pts',(-4.53333169900006,11.6,-9.51489462100002));
#289135=CARTESIAN_POINT('Ctrl Pts',(-4.53220942700006,15.2,-9.51338972000002));
#289136=CARTESIAN_POINT('Ctrl Pts',(-4.53220942700006,11.6,-9.51338972000002));
#289137=CARTESIAN_POINT('Ctrl Pts',(-4.53109289000006,15.2,-9.51188964700002));
#289138=CARTESIAN_POINT('Ctrl Pts',(-4.53109289000006,11.6,-9.51188964700002));
#289139=CARTESIAN_POINT('Ctrl Pts',(-4.52998208700006,15.2,-9.51039442500001));
#289140=CARTESIAN_POINT('Ctrl Pts',(-4.52998208700006,11.6,-9.51039442500001));
#289141=CARTESIAN_POINT('Ctrl Pts',(-4.52887701900006,15.2,-9.50890407300001));
#289142=CARTESIAN_POINT('Ctrl Pts',(-4.52887701900006,11.6,-9.50890407300001));
#289143=CARTESIAN_POINT('Ctrl Pts',(-4.52777768500006,15.2,-9.50741861400001));
#289144=CARTESIAN_POINT('Ctrl Pts',(-4.52777768500006,11.6,-9.50741861400001));
#289145=CARTESIAN_POINT('Ctrl Pts',(-4.52668408500006,15.2,-9.50593806500001));
#289146=CARTESIAN_POINT('Ctrl Pts',(-4.52668408500006,11.6,-9.50593806500001));
#289147=CARTESIAN_POINT('Ctrl Pts',(-4.52559622100006,15.2,-9.50446244800002));
#289148=CARTESIAN_POINT('Ctrl Pts',(-4.52559622100006,11.6,-9.50446244800002));
#289149=CARTESIAN_POINT('Ctrl Pts',(-4.52451409000005,15.2,-9.50299178400002));
#289150=CARTESIAN_POINT('Ctrl Pts',(-4.52451409000005,11.6,-9.50299178400002));
#289151=CARTESIAN_POINT('Ctrl Pts',(-4.52343769400006,15.2,-9.50152609400002));
#289152=CARTESIAN_POINT('Ctrl Pts',(-4.52343769400006,11.6,-9.50152609400002));
#289153=CARTESIAN_POINT('Ctrl Pts',(-4.52236703200006,15.2,-9.50006539900001));
#289154=CARTESIAN_POINT('Ctrl Pts',(-4.52236703200006,11.6,-9.50006539900001));
#289155=CARTESIAN_POINT('Ctrl Pts',(-4.52130210400006,15.2,-9.49860971900002));
#289156=CARTESIAN_POINT('Ctrl Pts',(-4.52130210400006,11.6,-9.49860971900002));
#289157=CARTESIAN_POINT('Ctrl Pts',(-4.52024291000006,15.2,-9.49715907500002));
#289158=CARTESIAN_POINT('Ctrl Pts',(-4.52024291000006,11.6,-9.49715907500002));
#289159=CARTESIAN_POINT('Ctrl Pts',(-4.51918944900005,15.2,-9.49571348900001));
#289160=CARTESIAN_POINT('Ctrl Pts',(-4.51918944900005,11.6,-9.49571348900001));
#289161=CARTESIAN_POINT('Ctrl Pts',(-4.51814172300006,15.2,-9.49427298100002));
#289162=CARTESIAN_POINT('Ctrl Pts',(-4.51814172300006,11.6,-9.49427298100002));
#289163=CARTESIAN_POINT('Ctrl Pts',(-4.51709973000006,15.2,-9.49283757300002));
#289164=CARTESIAN_POINT('Ctrl Pts',(-4.51709973000006,11.6,-9.49283757300002));
#289165=CARTESIAN_POINT('Ctrl Pts',(-4.51606347100006,15.2,-9.49140728700002));
#289166=CARTESIAN_POINT('Ctrl Pts',(-4.51606347100006,11.6,-9.49140728700002));
#289167=CARTESIAN_POINT('Ctrl Pts',(-4.51503294500006,15.2,-9.48998214200002));
#289168=CARTESIAN_POINT('Ctrl Pts',(-4.51503294500006,11.6,-9.48998214200002));
#289169=CARTESIAN_POINT('Ctrl Pts',(-4.51400815100006,15.2,-9.48856216300002));
#289170=CARTESIAN_POINT('Ctrl Pts',(-4.51400815100006,11.6,-9.48856216300002));
#289171=CARTESIAN_POINT('Ctrl Pts',(-4.51298909100006,15.2,-9.48714736800002));
#289172=CARTESIAN_POINT('Ctrl Pts',(-4.51298909100006,11.6,-9.48714736800002));
#289173=CARTESIAN_POINT('Ctrl Pts',(-4.51197576300006,15.2,-9.48573778100002));
#289174=CARTESIAN_POINT('Ctrl Pts',(-4.51197576300006,11.6,-9.48573778100002));
#289175=CARTESIAN_POINT('Ctrl Pts',(-4.51096816800006,15.2,-9.48433342200002));
#289176=CARTESIAN_POINT('Ctrl Pts',(-4.51096816800006,11.6,-9.48433342200002));
#289177=CARTESIAN_POINT('Ctrl Pts',(-4.50996630400006,15.2,-9.48293431400002));
#289178=CARTESIAN_POINT('Ctrl Pts',(-4.50996630400006,11.6,-9.48293431400002));
#289179=CARTESIAN_POINT('Ctrl Pts',(-4.50897017100006,15.2,-9.48154047900001));
#289180=CARTESIAN_POINT('Ctrl Pts',(-4.50897017100006,11.6,-9.48154047900001));
#289181=CARTESIAN_POINT('Ctrl Pts',(-4.50797977200006,15.2,-9.48015193800002));
#289182=CARTESIAN_POINT('Ctrl Pts',(-4.50797977200006,11.6,-9.48015193800002));
#289183=CARTESIAN_POINT('Ctrl Pts',(-4.50699510300006,15.2,-9.47876871300002));
#289184=CARTESIAN_POINT('Ctrl Pts',(-4.50699510300006,11.6,-9.47876871300002));
#289185=CARTESIAN_POINT('Ctrl Pts',(-4.50601616600006,15.2,-9.47739082700001));
#289186=CARTESIAN_POINT('Ctrl Pts',(-4.50601616600006,11.6,-9.47739082700001));
#289187=CARTESIAN_POINT('Ctrl Pts',(-4.50504295800005,15.2,-9.47601830200002));
#289188=CARTESIAN_POINT('Ctrl Pts',(-4.50504295800005,11.6,-9.47601830200002));
#289189=CARTESIAN_POINT('Ctrl Pts',(-4.50407548200006,15.2,-9.47465116000001));
#289190=CARTESIAN_POINT('Ctrl Pts',(-4.50407548200006,11.6,-9.47465116000001));
#289191=CARTESIAN_POINT('Ctrl Pts',(-4.50311373400006,15.2,-9.47328942300001));
#289192=CARTESIAN_POINT('Ctrl Pts',(-4.50311373400006,11.6,-9.47328942300001));
#289193=CARTESIAN_POINT('Ctrl Pts',(-4.50215771700006,15.2,-9.47193311300002));
#289194=CARTESIAN_POINT('Ctrl Pts',(-4.50215771700006,11.6,-9.47193311300002));
#289195=CARTESIAN_POINT('Ctrl Pts',(-4.50120742900006,15.2,-9.47058225500001));
#289196=CARTESIAN_POINT('Ctrl Pts',(-4.50120742900006,11.6,-9.47058225500001));
#289197=CARTESIAN_POINT('Ctrl Pts',(-4.50026286900005,15.2,-9.46923686900002));
#289198=CARTESIAN_POINT('Ctrl Pts',(-4.50026286900005,11.6,-9.46923686900002));
#289199=CARTESIAN_POINT('Ctrl Pts',(-4.49932403800006,15.2,-9.46789697900002));
#289200=CARTESIAN_POINT('Ctrl Pts',(-4.49932403800006,11.6,-9.46789697900002));
#289201=CARTESIAN_POINT('Ctrl Pts',(-4.49839093600006,15.2,-9.46656260700001));
#289202=CARTESIAN_POINT('Ctrl Pts',(-4.49839093600006,11.6,-9.46656260700001));
#289203=CARTESIAN_POINT('Ctrl Pts',(-4.49746356100006,15.2,-9.46523377700002));
#289204=CARTESIAN_POINT('Ctrl Pts',(-4.49746356100006,11.6,-9.46523377700002));
#289205=CARTESIAN_POINT('Ctrl Pts',(-4.49654191300006,15.2,-9.46391051100001));
#289206=CARTESIAN_POINT('Ctrl Pts',(-4.49654191300006,11.6,-9.46391051100001));
#289207=CARTESIAN_POINT('Ctrl Pts',(-4.49562599200005,15.2,-9.46259283300002));
#289208=CARTESIAN_POINT('Ctrl Pts',(-4.49562599200005,11.6,-9.46259283300002));
#289209=CARTESIAN_POINT('Ctrl Pts',(-4.49471579600006,15.2,-9.46128076400001));
#289210=CARTESIAN_POINT('Ctrl Pts',(-4.49471579600006,11.6,-9.46128076400001));
#289211=CARTESIAN_POINT('Ctrl Pts',(-4.49381132700006,15.2,-9.45997433000001));
#289212=CARTESIAN_POINT('Ctrl Pts',(-4.49381132700006,11.6,-9.45997433000001));
#289213=CARTESIAN_POINT('Ctrl Pts',(-4.49291258300006,15.2,-9.45867355200001));
#289214=CARTESIAN_POINT('Ctrl Pts',(-4.49291258300006,11.6,-9.45867355200001));
#289215=CARTESIAN_POINT('Ctrl Pts',(-4.49201956400006,15.2,-9.45737845500001));
#289216=CARTESIAN_POINT('Ctrl Pts',(-4.49201956400006,11.6,-9.45737845500001));
#289217=CARTESIAN_POINT('Ctrl Pts',(-4.49113226700006,15.2,-9.45608906200002));
#289218=CARTESIAN_POINT('Ctrl Pts',(-4.49113226700006,11.6,-9.45608906200002));
#289219=CARTESIAN_POINT('Ctrl Pts',(-4.49025069600006,15.2,-9.45480539600002));
#289220=CARTESIAN_POINT('Ctrl Pts',(-4.49025069600006,11.6,-9.45480539600002));
#289221=CARTESIAN_POINT('Ctrl Pts',(-4.48937484700005,15.2,-9.45352748200002));
#289222=CARTESIAN_POINT('Ctrl Pts',(-4.48937484700005,11.6,-9.45352748200002));
#289223=CARTESIAN_POINT('Ctrl Pts',(-4.48850472100006,15.2,-9.45225534300001));
#289224=CARTESIAN_POINT('Ctrl Pts',(-4.48850472100006,11.6,-9.45225534300001));
#289225=CARTESIAN_POINT('Ctrl Pts',(-4.48764031700006,15.2,-9.45098900300002));
#289226=CARTESIAN_POINT('Ctrl Pts',(-4.48764031700006,11.6,-9.45098900300002));
#289227=CARTESIAN_POINT('Ctrl Pts',(-4.48678163300006,15.2,-9.44972848600001));
#289228=CARTESIAN_POINT('Ctrl Pts',(-4.48678163300006,11.6,-9.44972848600001));
#289229=CARTESIAN_POINT('Ctrl Pts',(-4.48592867100006,15.2,-9.44847381600002));
#289230=CARTESIAN_POINT('Ctrl Pts',(-4.48592867100006,11.6,-9.44847381600002));
#289231=CARTESIAN_POINT('Ctrl Pts',(-4.48508142900006,15.2,-9.44722501600002));
#289232=CARTESIAN_POINT('Ctrl Pts',(-4.48508142900006,11.6,-9.44722501600002));
#289233=CARTESIAN_POINT('Ctrl Pts',(-4.48423990500006,15.2,-9.44598211300002));
#289234=CARTESIAN_POINT('Ctrl Pts',(-4.48423990500006,11.6,-9.44598211300002));
#289235=CARTESIAN_POINT('Ctrl Pts',(-4.48340410100006,15.2,-9.44474512900002));
#289236=CARTESIAN_POINT('Ctrl Pts',(-4.48340410100006,11.6,-9.44474512900002));
#289237=CARTESIAN_POINT('Ctrl Pts',(-4.48257401400006,15.2,-9.44351408900001));
#289238=CARTESIAN_POINT('Ctrl Pts',(-4.48257401400006,11.6,-9.44351408900001));
#289239=CARTESIAN_POINT('Ctrl Pts',(-4.48174964500006,15.2,-9.44228901900001));
#289240=CARTESIAN_POINT('Ctrl Pts',(-4.48174964500006,11.6,-9.44228901900001));
#289241=CARTESIAN_POINT('Ctrl Pts',(-4.48093099200006,15.2,-9.44106994200002));
#289242=CARTESIAN_POINT('Ctrl Pts',(-4.48093099200006,11.6,-9.44106994200002));
#289243=CARTESIAN_POINT('Ctrl Pts',(-4.48011805500006,15.2,-9.43985688200002));
#289244=CARTESIAN_POINT('Ctrl Pts',(-4.48011805500006,11.6,-9.43985688200002));
#289245=CARTESIAN_POINT('Ctrl Pts',(-4.47931083300006,15.2,-9.43864986700002));
#289246=CARTESIAN_POINT('Ctrl Pts',(-4.47931083300006,11.6,-9.43864986700002));
#289247=CARTESIAN_POINT('Ctrl Pts',(-4.47850932400006,15.2,-9.43744891900002));
#289248=CARTESIAN_POINT('Ctrl Pts',(-4.47850932400006,11.6,-9.43744891900002));
#289249=CARTESIAN_POINT('Ctrl Pts',(-4.47771353000006,15.2,-9.43625406500002));
#289250=CARTESIAN_POINT('Ctrl Pts',(-4.47771353000006,11.6,-9.43625406500002));
#289251=CARTESIAN_POINT('Ctrl Pts',(-4.47692344800006,15.2,-9.43506533000001));
#289252=CARTESIAN_POINT('Ctrl Pts',(-4.47692344800006,11.6,-9.43506533000001));
#289253=CARTESIAN_POINT('Ctrl Pts',(-4.47613907800006,15.2,-9.43388273700002));
#289254=CARTESIAN_POINT('Ctrl Pts',(-4.47613907800006,11.6,-9.43388273700002));
#289255=CARTESIAN_POINT('Ctrl Pts',(-4.47536041800006,15.2,-9.43270631400001));
#289256=CARTESIAN_POINT('Ctrl Pts',(-4.47536041800006,11.6,-9.43270631400001));
#289257=CARTESIAN_POINT('Ctrl Pts',(-4.47458747000006,15.2,-9.43153608600002));
#289258=CARTESIAN_POINT('Ctrl Pts',(-4.47458747000006,11.6,-9.43153608600002));
#289259=CARTESIAN_POINT('Ctrl Pts',(-4.47382023000006,15.2,-9.43037207700002));
#289260=CARTESIAN_POINT('Ctrl Pts',(-4.47382023000006,11.6,-9.43037207700002));
#289261=CARTESIAN_POINT('Ctrl Pts',(-4.47305869800006,15.2,-9.42921431400002));
#289262=CARTESIAN_POINT('Ctrl Pts',(-4.47305869800006,11.6,-9.42921431400002));
#289263=CARTESIAN_POINT('Ctrl Pts',(-4.47230287400005,15.2,-9.42806282400002));
#289264=CARTESIAN_POINT('Ctrl Pts',(-4.47230287400005,11.6,-9.42806282400002));
#289265=CARTESIAN_POINT('Ctrl Pts',(-4.47155275700006,15.2,-9.42691763000001));
#289266=CARTESIAN_POINT('Ctrl Pts',(-4.47155275700006,11.6,-9.42691763000001));
#289267=CARTESIAN_POINT('Ctrl Pts',(-4.47080834500006,15.2,-9.42577876000002));
#289268=CARTESIAN_POINT('Ctrl Pts',(-4.47080834500006,11.6,-9.42577876000002));
#289269=CARTESIAN_POINT('Ctrl Pts',(-4.47006963800006,15.2,-9.42464624100002));
#289270=CARTESIAN_POINT('Ctrl Pts',(-4.47006963800006,11.6,-9.42464624100002));
#289271=CARTESIAN_POINT('Ctrl Pts',(-4.46933663400006,15.2,-9.42352009700001));
#289272=CARTESIAN_POINT('Ctrl Pts',(-4.46933663400006,11.6,-9.42352009700001));
#289273=CARTESIAN_POINT('Ctrl Pts',(-4.46860933200006,15.2,-9.42240035600001));
#289274=CARTESIAN_POINT('Ctrl Pts',(-4.46860933200006,11.6,-9.42240035600001));
#289275=CARTESIAN_POINT('Ctrl Pts',(-4.46788773300006,15.2,-9.42128704400002));
#289276=CARTESIAN_POINT('Ctrl Pts',(-4.46788773300006,11.6,-9.42128704400002));
#289277=CARTESIAN_POINT('Ctrl Pts',(-4.46717183400006,15.2,-9.42018018700002));
#289278=CARTESIAN_POINT('Ctrl Pts',(-4.46717183400006,11.6,-9.42018018700002));
#289279=CARTESIAN_POINT('Ctrl Pts',(-4.46646163400006,15.2,-9.41907981300002));
#289280=CARTESIAN_POINT('Ctrl Pts',(-4.46646163400006,11.6,-9.41907981300002));
#289281=CARTESIAN_POINT('Ctrl Pts',(-4.46575713300006,15.2,-9.41798594700002));
#289282=CARTESIAN_POINT('Ctrl Pts',(-4.46575713300006,11.6,-9.41798594700002));
#289283=CARTESIAN_POINT('Ctrl Pts',(-4.46505833000006,15.2,-9.41689861800001));
#289284=CARTESIAN_POINT('Ctrl Pts',(-4.46505833000006,11.6,-9.41689861800001));
#289285=CARTESIAN_POINT('Ctrl Pts',(-4.46436522200006,15.2,-9.41581785200002));
#289286=CARTESIAN_POINT('Ctrl Pts',(-4.46436522200006,11.6,-9.41581785200002));
#289287=CARTESIAN_POINT('Ctrl Pts',(-4.46367781000006,15.2,-9.41474367700001));
#289288=CARTESIAN_POINT('Ctrl Pts',(-4.46367781000006,11.6,-9.41474367700001));
#289289=CARTESIAN_POINT('Ctrl Pts',(-4.46299609100006,15.2,-9.41367611900001));
#289290=CARTESIAN_POINT('Ctrl Pts',(-4.46299609100006,11.6,-9.41367611900001));
#289291=CARTESIAN_POINT('Ctrl Pts',(-4.46232006500006,15.2,-9.41261520700002));
#289292=CARTESIAN_POINT('Ctrl Pts',(-4.46232006500006,11.6,-9.41261520700002));
#289293=CARTESIAN_POINT('Ctrl Pts',(-4.46164973200006,15.2,-9.41156096600002));
#289294=CARTESIAN_POINT('Ctrl Pts',(-4.46164973200006,11.6,-9.41156096600002));
#289295=CARTESIAN_POINT('Ctrl Pts',(-4.46098508800006,15.2,-9.41051342700002));
#289296=CARTESIAN_POINT('Ctrl Pts',(-4.46098508800006,11.6,-9.41051342700002));
#289297=CARTESIAN_POINT('Ctrl Pts',(-4.46032613400006,15.2,-9.40947261400002));
#289298=CARTESIAN_POINT('Ctrl Pts',(-4.46032613400006,11.6,-9.40947261400002));
#289299=CARTESIAN_POINT('Ctrl Pts',(-4.45967286700006,15.2,-9.40843855900001));
#289300=CARTESIAN_POINT('Ctrl Pts',(-4.45967286700006,11.6,-9.40843855900001));
#289301=CARTESIAN_POINT('Ctrl Pts',(-4.45902528800006,15.2,-9.40741128800001));
#289302=CARTESIAN_POINT('Ctrl Pts',(-4.45902528800006,11.6,-9.40741128800001));
#289303=CARTESIAN_POINT('Ctrl Pts',(-4.45838339400006,15.2,-9.40639082900002));
#289304=CARTESIAN_POINT('Ctrl Pts',(-4.45838339400006,11.6,-9.40639082900002));
#289305=CARTESIAN_POINT('Ctrl Pts',(-4.45774718400005,15.2,-9.40537720900002));
#289306=CARTESIAN_POINT('Ctrl Pts',(-4.45774718400005,11.6,-9.40537720900002));
#289307=CARTESIAN_POINT('Ctrl Pts',(-4.45711665600006,15.2,-9.40437046000002));
#289308=CARTESIAN_POINT('Ctrl Pts',(-4.45711665600006,11.6,-9.40437046000002));
#289309=CARTESIAN_POINT('Ctrl Pts',(-4.45649181000006,15.2,-9.40337060700001));
#289310=CARTESIAN_POINT('Ctrl Pts',(-4.45649181000006,11.6,-9.40337060700001));
#289311=CARTESIAN_POINT('Ctrl Pts',(-4.45587264400006,15.2,-9.40237768200002));
#289312=CARTESIAN_POINT('Ctrl Pts',(-4.45587264400006,11.6,-9.40237768200002));
#289313=CARTESIAN_POINT('Ctrl Pts',(-4.45525915700006,15.2,-9.40139171100002));
#289314=CARTESIAN_POINT('Ctrl Pts',(-4.45525915700006,11.6,-9.40139171100002));
#289315=CARTESIAN_POINT('Ctrl Pts',(-4.45465134800005,15.2,-9.40041272500002));
#289316=CARTESIAN_POINT('Ctrl Pts',(-4.45465134800005,11.6,-9.40041272500002));
#289317=CARTESIAN_POINT('Ctrl Pts',(-4.45404921300006,15.2,-9.39944075100002));
#289318=CARTESIAN_POINT('Ctrl Pts',(-4.45404921300006,11.6,-9.39944075100002));
#289319=CARTESIAN_POINT('Ctrl Pts',(-4.45345275400006,15.2,-9.39847582000001));
#289320=CARTESIAN_POINT('Ctrl Pts',(-4.45345275400006,11.6,-9.39847582000001));
#289321=CARTESIAN_POINT('Ctrl Pts',(-4.45286196800006,15.2,-9.39751796000002));
#289322=CARTESIAN_POINT('Ctrl Pts',(-4.45286196800006,11.6,-9.39751796000002));
#289323=CARTESIAN_POINT('Ctrl Pts',(-4.45227685400006,15.2,-9.39656720200002));
#289324=CARTESIAN_POINT('Ctrl Pts',(-4.45227685400006,11.6,-9.39656720200002));
#289325=CARTESIAN_POINT('Ctrl Pts',(-4.45169740800006,15.2,-9.39562357400002));
#289326=CARTESIAN_POINT('Ctrl Pts',(-4.45169740800006,11.6,-9.39562357400002));
#289327=CARTESIAN_POINT('Ctrl Pts',(-4.45112363200006,15.2,-9.39468710800002));
#289328=CARTESIAN_POINT('Ctrl Pts',(-4.45112363200006,11.6,-9.39468710800002));
#289329=CARTESIAN_POINT('Ctrl Pts',(-4.45055552300006,15.2,-9.39375783100001));
#289330=CARTESIAN_POINT('Ctrl Pts',(-4.45055552300006,11.6,-9.39375783100001));
#289331=CARTESIAN_POINT('Ctrl Pts',(-4.44999307900006,15.2,-9.39283577600002));
#289332=CARTESIAN_POINT('Ctrl Pts',(-4.44999307900006,11.6,-9.39283577600002));
#289333=CARTESIAN_POINT('Ctrl Pts',(-4.44943629900005,15.2,-9.39192097100002));
#289334=CARTESIAN_POINT('Ctrl Pts',(-4.44943629900005,11.6,-9.39192097100002));
#289335=CARTESIAN_POINT('Ctrl Pts',(-4.44888518000006,15.2,-9.39101344800001));
#289336=CARTESIAN_POINT('Ctrl Pts',(-4.44888518000006,11.6,-9.39101344800001));
#289337=CARTESIAN_POINT('Ctrl Pts',(-4.44833972300006,15.2,-9.39011323500001));
#289338=CARTESIAN_POINT('Ctrl Pts',(-4.44833972300006,11.6,-9.39011323500001));
#289339=CARTESIAN_POINT('Ctrl Pts',(-4.44779992500006,15.2,-9.38922036500001));
#289340=CARTESIAN_POINT('Ctrl Pts',(-4.44779992500006,11.6,-9.38922036500001));
#289341=CARTESIAN_POINT('Ctrl Pts',(-4.44726578300005,15.2,-9.38833486800002));
#289342=CARTESIAN_POINT('Ctrl Pts',(-4.44726578300005,11.6,-9.38833486800002));
#289343=CARTESIAN_POINT('Ctrl Pts',(-4.44673729800006,15.2,-9.38745677600001));
#289344=CARTESIAN_POINT('Ctrl Pts',(-4.44673729800006,11.6,-9.38745677600001));
#289345=CARTESIAN_POINT('Ctrl Pts',(-4.44621446600006,15.2,-9.38658611800001));
#289346=CARTESIAN_POINT('Ctrl Pts',(-4.44621446600006,11.6,-9.38658611800001));
#289347=CARTESIAN_POINT('Ctrl Pts',(-4.44569728500006,15.2,-9.38572292700002));
#289348=CARTESIAN_POINT('Ctrl Pts',(-4.44569728500006,11.6,-9.38572292700002));
#289349=CARTESIAN_POINT('Ctrl Pts',(-4.44518575600005,15.2,-9.38486723300001));
#289350=CARTESIAN_POINT('Ctrl Pts',(-4.44518575600005,11.6,-9.38486723300001));
#289351=CARTESIAN_POINT('Ctrl Pts',(-4.44467987500006,15.2,-9.38401906800001));
#289352=CARTESIAN_POINT('Ctrl Pts',(-4.44467987500006,11.6,-9.38401906800001));
#289353=CARTESIAN_POINT('Ctrl Pts',(-4.44417964000006,15.2,-9.38317846500002));
#289354=CARTESIAN_POINT('Ctrl Pts',(-4.44417964000006,11.6,-9.38317846500002));
#289355=CARTESIAN_POINT('Ctrl Pts',(-4.44368505200006,15.2,-9.38234545400002));
#289356=CARTESIAN_POINT('Ctrl Pts',(-4.44368505200006,11.6,-9.38234545400002));
#289357=CARTESIAN_POINT('Ctrl Pts',(-4.44319610500005,15.2,-9.38152006800001));
#289358=CARTESIAN_POINT('Ctrl Pts',(-4.44319610500005,11.6,-9.38152006800001));
#289359=CARTESIAN_POINT('Ctrl Pts',(-4.44271280000006,15.2,-9.38070233800002));
#289360=CARTESIAN_POINT('Ctrl Pts',(-4.44271280000006,11.6,-9.38070233800002));
#289361=CARTESIAN_POINT('Ctrl Pts',(-4.44223513400006,15.2,-9.37989229800002));
#289362=CARTESIAN_POINT('Ctrl Pts',(-4.44223513400006,11.6,-9.37989229800002));
#289363=CARTESIAN_POINT('Ctrl Pts',(-4.44176310600006,15.2,-9.37908998100001));
#289364=CARTESIAN_POINT('Ctrl Pts',(-4.44176310600006,11.6,-9.37908998100001));
#289365=CARTESIAN_POINT('Ctrl Pts',(-4.44129939900006,15.2,-9.37829999200002));
#289366=CARTESIAN_POINT('Ctrl Pts',(-4.44129939900006,11.6,-9.37829999200002));
#289367=CARTESIAN_POINT('Ctrl Pts',(-4.44093341100006,15.2,-9.37767505700002));
#289368=CARTESIAN_POINT('Ctrl Pts',(-4.44093341100006,11.6,-9.37767505700002));
#289369=CARTESIAN_POINT('Ctrl Pts',(-4.44066207100006,15.2,-9.37721094100001));
#289370=CARTESIAN_POINT('Ctrl Pts',(-4.44066207100006,11.6,-9.37721094100001));
#289371=CARTESIAN_POINT('Ctrl Pts',(-4.44048314800006,15.2,-9.37690455300002));
#289372=CARTESIAN_POINT('Ctrl Pts',(-4.44048314800006,11.6,-9.37690455300002));
#289373=CARTESIAN_POINT('Ctrl Pts',(-4.44039525800005,15.2,-9.37675396700002));
#289374=CARTESIAN_POINT('Ctrl Pts',(-4.44039525800005,11.6,-9.37675396700002));
#289375=CARTESIAN_POINT('',(-4.44039525809517,12.2,-9.3767539665342));
#289376=CARTESIAN_POINT('',(-4.44039525809517,15.2,-9.3767539665342));
#289377=CARTESIAN_POINT('',(-4.44039525800005,12.2,-9.37675396600002));
#289378=CARTESIAN_POINT('Ctrl Pts',(-5.26939701852072,12.2,-10.2217148786423));
#289379=CARTESIAN_POINT('Ctrl Pts',(-5.26633327357192,12.2,-10.2194283574115));
#289380=CARTESIAN_POINT('Ctrl Pts',(-5.26327740215982,12.2,-10.2171423379557));
#289381=CARTESIAN_POINT('Ctrl Pts',(-5.26022942034972,12.2,-10.2148568142835));
#289382=CARTESIAN_POINT('Ctrl Pts',(-5.25718143853964,12.2,-10.2125712906113));
#289383=CARTESIAN_POINT('Ctrl Pts',(-5.25414134151229,12.2,-10.2102862658399));
#289384=CARTESIAN_POINT('Ctrl Pts',(-5.25110913459507,12.2,-10.2080017554753));
#289385=CARTESIAN_POINT('Ctrl Pts',(-5.24807692767784,12.2,-10.2057172451108));
#289386=CARTESIAN_POINT('Ctrl Pts',(-5.2450526103324,12.2,-10.2034332511482));
#289387=CARTESIAN_POINT('Ctrl Pts',(-5.24203619464925,12.2,-10.2011498137311));
#289388=CARTESIAN_POINT('Ctrl Pts',(-5.23901977841812,12.2,-10.1988663758992));
#289389=CARTESIAN_POINT('Ctrl Pts',(-5.23601126359756,12.2,-10.1965834977174));
#289390=CARTESIAN_POINT('Ctrl Pts',(-5.23301066232921,12.2,-10.1943012257191));
#289391=CARTESIAN_POINT('Ctrl Pts',(-5.23001006160596,12.2,-10.1920189541355));
#289392=CARTESIAN_POINT('Ctrl Pts',(-5.227017373399,12.2,-10.1897372894851));
#289393=CARTESIAN_POINT('Ctrl Pts',(-5.22403260963313,12.2,-10.1874562692347));
#289394=CARTESIAN_POINT('Ctrl Pts',(-5.22104784586726,12.2,-10.1851752489843));
#289395=CARTESIAN_POINT('Ctrl Pts',(-5.21807100570288,12.2,-10.1828948727588));
#289396=CARTESIAN_POINT('Ctrl Pts',(-5.21510209700565,12.2,-10.1806151774979));
#289397=CARTESIAN_POINT('Ctrl Pts',(-5.21114355225578,12.2,-10.1775755839549));
#289398=CARTESIAN_POINT('Ctrl Pts',(-5.20719911047275,12.2,-10.1745371987484));
#289399=CARTESIAN_POINT('Ctrl Pts',(-5.20326879445928,12.2,-10.1715001199966));
#289400=CARTESIAN_POINT('Ctrl Pts',(-5.20032105677979,12.2,-10.1692223104154));
#289401=CARTESIAN_POINT('Ctrl Pts',(-5.1973812652192,12.2,-10.1669452356012));
#289402=CARTESIAN_POINT('Ctrl Pts',(-5.19444942958587,12.2,-10.1646689369788));
#289403=CARTESIAN_POINT('Ctrl Pts',(-5.19151759448515,12.2,-10.1623926387699));
#289404=CARTESIAN_POINT('Ctrl Pts',(-5.18859371667566,12.2,-10.1601171159194));
#289405=CARTESIAN_POINT('Ctrl Pts',(-5.1856778044073,12.2,-10.1578424087521));
#289406=CARTESIAN_POINT('Ctrl Pts',(-5.18276189213894,12.2,-10.1555677015848));
#289407=CARTESIAN_POINT('Ctrl Pts',(-5.17985394462181,12.2,-10.1532938106423));
#289408=CARTESIAN_POINT('Ctrl Pts',(-5.17695397425571,12.2,-10.1510207745063));
#289409=CARTESIAN_POINT('Ctrl Pts',(-5.17405400388961,12.2,-10.1487477383702));
#289410=CARTESIAN_POINT('Ctrl Pts',(-5.1711620077443,12.2,-10.1464755577132));
#289411=CARTESIAN_POINT('Ctrl Pts',(-5.16827799800262,12.2,-10.1442042744937));
#289412=CARTESIAN_POINT('Ctrl Pts',(-5.16539398826094,12.2,-10.1419329912743));
#289413=CARTESIAN_POINT('Ctrl Pts',(-5.16251796474257,12.2,-10.139662604215));
#289414=CARTESIAN_POINT('Ctrl Pts',(-5.15964993559609,12.2,-10.1373931555057));
#289415=CARTESIAN_POINT('Ctrl Pts',(-5.1567819064496,12.2,-10.1351237067964));
#289416=CARTESIAN_POINT('Ctrl Pts',(-5.15392187308588,12.2,-10.1328551959621));
#289417=CARTESIAN_POINT('Ctrl Pts',(-5.15106984485508,12.2,-10.1305876642943));
#289418=CARTESIAN_POINT('Ctrl Pts',(-5.14821781610616,12.2,-10.1283201322146));
#289419=CARTESIAN_POINT('Ctrl Pts',(-5.14537379164283,12.2,-10.1260535792519));
#289420=CARTESIAN_POINT('Ctrl Pts',(-5.14253778235676,12.2,-10.1237880462978));
#289421=CARTESIAN_POINT('Ctrl Pts',(-5.13875643750067,12.2,-10.1207673363783));
#289422=CARTESIAN_POINT('Ctrl Pts',(-5.13498934030452,12.2,-10.1177484413219));
#289423=CARTESIAN_POINT('Ctrl Pts',(-5.13123651476089,12.2,-10.1147314592771));
#289424=CARTESIAN_POINT('Ctrl Pts',(-5.12842189547534,12.2,-10.1124687226407));
#289425=CARTESIAN_POINT('Ctrl Pts',(-5.12561530227086,12.2,-10.1102070631311));
#289426=CARTESIAN_POINT('Ctrl Pts',(-5.12281674703851,12.2,-10.1079465215048));
#289427=CARTESIAN_POINT('Ctrl Pts',(-5.12001819180616,12.2,-10.1056859798785));
#289428=CARTESIAN_POINT('Ctrl Pts',(-5.11722767402325,12.2,-10.1034265563937));
#289429=CARTESIAN_POINT('Ctrl Pts',(-5.11444520183159,12.2,-10.1011682937673));
#289430=CARTESIAN_POINT('Ctrl Pts',(-5.11166272913444,12.2,-10.0989100307306));
#289431=CARTESIAN_POINT('Ctrl Pts',(-5.10888830266455,12.2,-10.0966529282692));
#289432=CARTESIAN_POINT('Ctrl Pts',(-5.10612193234694,12.2,-10.0943970292332));
#289433=CARTESIAN_POINT('Ctrl Pts',(-5.10335556253188,12.2,-10.092141130607));
#289434=CARTESIAN_POINT('Ctrl Pts',(-5.10059724754973,12.2,-10.0898864356391));
#289435=CARTESIAN_POINT('Ctrl Pts',(-5.09784699873369,12.2,-10.0876329860544));
#289436=CARTESIAN_POINT('Ctrl Pts',(-5.09509674991765,12.2,-10.0853795364697));
#289437=CARTESIAN_POINT('Ctrl Pts',(-5.09235456626056,12.2,-10.0831273331097));
#289438=CARTESIAN_POINT('Ctrl Pts',(-5.08962045651418,12.2,-10.080876418973));
#289439=CARTESIAN_POINT('Ctrl Pts',(-5.08688634676781,12.2,-10.0786255048362));
#289440=CARTESIAN_POINT('Ctrl Pts',(-5.08416031078277,12.2,-10.0763758791973));
#289441=CARTESIAN_POINT('Ctrl Pts',(-5.0814423590358,12.2,-10.0741275870187));
#289442=CARTESIAN_POINT('Ctrl Pts',(-5.07872440728883,12.2,-10.0718792948402));
#289443=CARTESIAN_POINT('Ctrl Pts',(-5.07601453924716,12.2,-10.0696323351633));
#289444=CARTESIAN_POINT('Ctrl Pts',(-5.07331276405296,12.2,-10.0673867514948));
#289445=CARTESIAN_POINT('Ctrl Pts',(-5.06971039680015,12.2,-10.0643926396648));
#289446=CARTESIAN_POINT('Ctrl Pts',(-5.0661224169907,12.2,-10.0614009741934));
#289447=CARTESIAN_POINT('Ctrl Pts',(-5.06254884624133,12.2,-10.0584118585307));
#289448=CARTESIAN_POINT('Ctrl Pts',(-5.05986866842275,12.2,-10.0561700219872));
#289449=CARTESIAN_POINT('Ctrl Pts',(-5.05719659431286,12.2,-10.0539296197101));
#289450=CARTESIAN_POINT('Ctrl Pts',(-5.05453263548092,12.2,-10.0516906974896));
#289451=CARTESIAN_POINT('Ctrl Pts',(-5.05186867664897,12.2,-10.0494517752691));
#289452=CARTESIAN_POINT('Ctrl Pts',(-5.04921283078493,12.2,-10.047214330381));
#289453=CARTESIAN_POINT('Ctrl Pts',(-5.04656510899407,12.2,-10.0449784097854));
#289454=CARTESIAN_POINT('Ctrl Pts',(-5.04391738720321,12.2,-10.0427424891898));
#289455=CARTESIAN_POINT('Ctrl Pts',(-5.04127778854206,12.2,-10.0405080924457));
#289456=CARTESIAN_POINT('Ctrl Pts',(-5.03864632176197,12.2,-10.0382752629434));
#289457=CARTESIAN_POINT('Ctrl Pts',(-5.03601485498187,12.2,-10.0360424334411));
#289458=CARTESIAN_POINT('Ctrl Pts',(-5.03339151957621,12.2,-10.0338111730719));
#289459=CARTESIAN_POINT('Ctrl Pts',(-5.03077632533678,12.2,-10.0315815250277));
#289460=CARTESIAN_POINT('Ctrl Pts',(-5.02816113062226,12.2,-10.0293518765785));
#289461=CARTESIAN_POINT('Ctrl Pts',(-5.02555407711005,12.2,-10.027123841488));
#289462=CARTESIAN_POINT('Ctrl Pts',(-5.02295517290011,12.2,-10.024897464998));
#289463=CARTESIAN_POINT('Ctrl Pts',(-5.02035626916231,12.2,-10.0226710889124));
#289464=CARTESIAN_POINT('Ctrl Pts',(-5.01776551501798,12.2,-10.0204463707667));
#289465=CARTESIAN_POINT('Ctrl Pts',(-5.0151829200254,12.2,-10.0182233565699));
#289466=CARTESIAN_POINT('Ctrl Pts',(-5.01260032503283,12.2,-10.0160003423732));
#289467=CARTESIAN_POINT('Ctrl Pts',(-5.01002588752645,12.2,-10.0137790321273));
#289468=CARTESIAN_POINT('Ctrl Pts',(-5.00745961774541,12.2,-10.0115594724998));
#289469=CARTESIAN_POINT('Ctrl Pts',(-5.00489334796437,12.2,-10.0093399128722));
#289470=CARTESIAN_POINT('Ctrl Pts',(-5.00233524529068,12.2,-10.0071221025362));
#289471=CARTESIAN_POINT('Ctrl Pts',(-4.99978531850833,12.2,-10.0049060884917));
#289472=CARTESIAN_POINT('Ctrl Pts',(-4.99723539172598,12.2,-10.0026900744472));
#289473=CARTESIAN_POINT('Ctrl Pts',(-4.99469363983496,12.2,-10.0004758575276));
#289474=CARTESIAN_POINT('Ctrl Pts',(-4.99216007350963,12.2,-9.99826348202451));
#289475=CARTESIAN_POINT('Ctrl Pts',(-4.9896265071843,12.2,-9.9960511065214));
#289476=CARTESIAN_POINT('Ctrl Pts',(-4.98710112537234,12.2,-9.99384057329098));
#289477=CARTESIAN_POINT('Ctrl Pts',(-4.98458393554543,12.2,-9.99163192963567));
#289478=CARTESIAN_POINT('Ctrl Pts',(-4.98206674571852,12.2,-9.98942328598036));
#289479=CARTESIAN_POINT('Ctrl Pts',(-4.97955774950544,12.2,-9.98721653205081));
#289480=CARTESIAN_POINT('Ctrl Pts',(-4.97705695430351,12.2,-9.98501171400565));
#289481=CARTESIAN_POINT('Ctrl Pts',(-4.97288896214887,12.2,-9.98133701713021));
#289482=CARTESIAN_POINT('Ctrl Pts',(-4.96874375134696,12.2,-9.97766769867996));
#289483=CARTESIAN_POINT('Ctrl Pts',(-4.96462136078907,12.2,-9.97400397847075));
#289484=CARTESIAN_POINT('Ctrl Pts',(-4.96132344816302,12.2,-9.97107300214364));
#289485=CARTESIAN_POINT('Ctrl Pts',(-4.95804014295738,12.2,-9.96814560872895));
#289486=CARTESIAN_POINT('Ctrl Pts',(-4.95477145976444,12.2,-9.96522191172301));
#289487=CARTESIAN_POINT('Ctrl Pts',(-4.95150277701685,12.2,-9.96229821511542));
#289488=CARTESIAN_POINT('Ctrl Pts',(-4.94824871974687,12.2,-9.95937821471655));
#289489=CARTESIAN_POINT('Ctrl Pts',(-4.94500930628799,12.2,-9.95646202551013));
#289490=CARTESIAN_POINT('Ctrl Pts',(-4.94176989238772,12.2,-9.95354583590638));
#289491=CARTESIAN_POINT('Ctrl Pts',(-4.93854512263328,12.2,-9.9506334582224));
#289492=CARTESIAN_POINT('Ctrl Pts',(-4.93533501595833,12.2,-9.94772500600833));
#289493=CARTESIAN_POINT('Ctrl Pts',(-4.93212490928337,12.2,-9.94481655379425));
#289494=CARTESIAN_POINT('Ctrl Pts',(-4.92892946581291,12.2,-9.94191202802787));
#289495=CARTESIAN_POINT('Ctrl Pts',(-4.92574870519662,12.2,-9.93901154509243));
#289496=CARTESIAN_POINT('Ctrl Pts',(-4.92256794501371,12.2,-9.93611106255218));
#289497=CARTESIAN_POINT('Ctrl Pts',(-4.91940186695056,12.2,-9.93321462228146));
#289498=CARTESIAN_POINT('Ctrl Pts',(-4.91625049002715,12.2,-9.93032234422697));
#289499=CARTESIAN_POINT('Ctrl Pts',(-4.91309911267437,12.2,-9.92743006577841));
#289500=CARTESIAN_POINT('Ctrl Pts',(-4.90996243593322,12.2,-9.92454194631578));
#289501=CARTESIAN_POINT('Ctrl Pts',(-4.90684047926456,12.2,-9.92165810677015));
#289502=CARTESIAN_POINT('Ctrl Pts',(-4.90371852302128,12.2,-9.91877426761745));
#289503=CARTESIAN_POINT('Ctrl Pts',(-4.90061128645942,12.2,-9.91589470749476));
#289504=CARTESIAN_POINT('Ctrl Pts',(-4.89751878754462,12.2,-9.91301954628508));
#289505=CARTESIAN_POINT('Ctrl Pts',(-4.89365316358509,12.2,-9.90942559447918));
#289506=CARTESIAN_POINT('Ctrl Pts',(-4.88981056848061,12.2,-9.90583851505712));
#289507=CARTESIAN_POINT('Ctrl Pts',(-4.88599103631042,12.2,-9.90225854573528));
#289508=CARTESIAN_POINT('Ctrl Pts',(-4.88293541040773,12.2,-9.89939457012172));
#289509=CARTESIAN_POINT('Ctrl Pts',(-4.8798945456131,12.2,-9.8965351435828));
#289510=CARTESIAN_POINT('Ctrl Pts',(-4.87686845900524,12.2,-9.89368038931658));
#289511=CARTESIAN_POINT('Ctrl Pts',(-4.87384237280968,12.2,-9.89082563543931));
#289512=CARTESIAN_POINT('Ctrl Pts',(-4.87083106485943,12.2,-9.88797555366423));
#289513=CARTESIAN_POINT('Ctrl Pts',(-4.86783455327011,12.2,-9.88513026717431));
#289514=CARTESIAN_POINT('Ctrl Pts',(-4.86483804127251,12.2,-9.88228498029672));
#289515=CARTESIAN_POINT('Ctrl Pts',(-4.86185632551708,12.2,-9.8794444874621));
#289516=CARTESIAN_POINT('Ctrl Pts',(-4.85888942331956,12.2,-9.87660891505523));
#289517=CARTESIAN_POINT('Ctrl Pts',(-4.85592252152629,12.2,-9.8737733430347));
#289518=CARTESIAN_POINT('Ctrl Pts',(-4.85297043309277,12.2,-9.87094269000036));
#289519=CARTESIAN_POINT('Ctrl Pts',(-4.8500331754986,12.2,-9.86811708223104));
#289520=CARTESIAN_POINT('Ctrl Pts',(-4.84709591750422,12.2,-9.86529147407672));
#289521=CARTESIAN_POINT('Ctrl Pts',(-4.84417349063382,12.2,-9.8624709117952));
#289522=CARTESIAN_POINT('Ctrl Pts',(-4.84126591075411,12.2,-9.85965551975322));
#289523=CARTESIAN_POINT('Ctrl Pts',(-4.83835833127056,12.2,-9.85684012809482));
#289524=CARTESIAN_POINT('Ctrl Pts',(-4.83546559825624,12.2,-9.85402990832429));
#289525=CARTESIAN_POINT('Ctrl Pts',(-4.8325877312122,12.2,-9.85122498844193));
#289526=CARTESIAN_POINT('Ctrl Pts',(-4.82970986377605,12.2,-9.84842006817742));
#289527=CARTESIAN_POINT('Ctrl Pts',(-4.82684685973839,12.2,-9.84562044753249));
#289528=CARTESIAN_POINT('Ctrl Pts',(-4.82399873701473,12.2,-9.84282625475642));
#289529=CARTESIAN_POINT('Ctrl Pts',(-4.82115061467911,12.2,-9.84003206236106));
#289530=CARTESIAN_POINT('Ctrl Pts',(-4.81831737290693,12.2,-9.83724329835031));
#289531=CARTESIAN_POINT('Ctrl Pts',(-4.81549902796914,12.2,-9.83446009268838));
#289532=CARTESIAN_POINT('Ctrl Pts',(-4.81268068264735,12.2,-9.83167688664724));
#289533=CARTESIAN_POINT('Ctrl Pts',(-4.80987723444919,12.2,-9.82889923871495));
#289534=CARTESIAN_POINT('Ctrl Pts',(-4.80708869857499,12.2,-9.82612728250832));
#289535=CARTESIAN_POINT('Ctrl Pts',(-4.8043001627008,12.2,-9.8233553263017));
#289536=CARTESIAN_POINT('Ctrl Pts',(-4.80152654065889,12.2,-9.82058905979851));
#289537=CARTESIAN_POINT('Ctrl Pts',(-4.79876784606562,12.2,-9.81782861631532));
#289538=CARTESIAN_POINT('Ctrl Pts',(-4.79600915184822,12.2,-9.81506817320825));
#289539=CARTESIAN_POINT('Ctrl Pts',(-4.79326538591345,12.2,-9.81231355234244));
#289540=CARTESIAN_POINT('Ctrl Pts',(-4.79053656423519,12.2,-9.80956488927686));
#289541=CARTESIAN_POINT('Ctrl Pts',(-4.78780774218513,12.2,-9.80681622583677));
#289542=CARTESIAN_POINT('Ctrl Pts',(-4.78509386508208,12.2,-9.80407351888719));
#289543=CARTESIAN_POINT('Ctrl Pts',(-4.7823949458254,12.2,-9.80133690479422));
#289544=CARTESIAN_POINT('Ctrl Pts',(-4.77969602693645,12.2,-9.7986002910741));
#289545=CARTESIAN_POINT('Ctrl Pts',(-4.77701206720667,12.2,-9.79586976972545));
#289546=CARTESIAN_POINT('Ctrl Pts',(-4.77434308220166,12.2,-9.79314547744776));
#289547=CARTESIAN_POINT('Ctrl Pts',(-4.771674096833,12.2,-9.79042118479888));
#289548=CARTESIAN_POINT('Ctrl Pts',(-4.76902008436373,12.2,-9.78770312084202));
#289549=CARTESIAN_POINT('Ctrl Pts',(-4.76638106086714,12.2,-9.78499142461487));
#289550=CARTESIAN_POINT('Ctrl Pts',(-4.76374203773012,12.2,-9.7822797287572));
#289551=CARTESIAN_POINT('Ctrl Pts',(-4.76111800389278,12.2,-9.77957439923381));
#289552=CARTESIAN_POINT('Ctrl Pts',(-4.75850897227176,12.2,-9.77687557745401));
#289553=CARTESIAN_POINT('Ctrl Pts',(-4.75589994029526,12.2,-9.7741767553065));
#289554=CARTESIAN_POINT('Ctrl Pts',(-4.7533059108011,12.2,-9.77148443834587));
#289555=CARTESIAN_POINT('Ctrl Pts',(-4.75072689877264,12.2,-9.7687987702555));
#289556=CARTESIAN_POINT('Ctrl Pts',(-4.74750313391277,12.2,-9.7654416853255));
#289557=CARTESIAN_POINT('Ctrl Pts',(-4.74430283258282,12.2,-9.76209498649535));
#289558=CARTESIAN_POINT('Ctrl Pts',(-4.74112602256463,12.2,-9.75875895237109));
#289559=CARTESIAN_POINT('Ctrl Pts',(-4.73858457475785,12.2,-9.75609012528987));
#289560=CARTESIAN_POINT('Ctrl Pts',(-4.73605816102612,12.2,-9.75342812337273));
#289561=CARTESIAN_POINT('Ctrl Pts',(-4.73354679473044,12.2,-9.75077309170043));
#289562=CARTESIAN_POINT('Ctrl Pts',(-4.73103542809259,12.2,-9.74811805966639));
#289563=CARTESIAN_POINT('Ctrl Pts',(-4.72853910887321,12.2,-9.74546999682206));
#289564=CARTESIAN_POINT('Ctrl Pts',(-4.72605785023896,12.2,-9.74282904956749));
#289565=CARTESIAN_POINT('Ctrl Pts',(-4.72357659194279,12.2,-9.74018810267274));
#289566=CARTESIAN_POINT('Ctrl Pts',(-4.72111039429581,12.2,-9.73755427105384));
#289567=CARTESIAN_POINT('Ctrl Pts',(-4.71865927037242,12.2,-9.73492770191449));
#289568=CARTESIAN_POINT('Ctrl Pts',(-4.71620814611507,12.2,-9.73230113241728));
#289569=CARTESIAN_POINT('Ctrl Pts',(-4.71377209473874,12.2,-9.72968182402841));
#289570=CARTESIAN_POINT('Ctrl Pts',(-4.71135113005222,12.2,-9.7270699275532));
#289571=CARTESIAN_POINT('Ctrl Pts',(-4.70893016569556,12.2,-9.72445803143386));
#289572=CARTESIAN_POINT('Ctrl Pts',(-4.70652428701922,12.2,-9.72185354758805));
#289573=CARTESIAN_POINT('Ctrl Pts',(-4.70413350665756,12.2,-9.71925662396625));
#289574=CARTESIAN_POINT('Ctrl Pts',(-4.70174272597016,12.2,-9.71665969999061));
#289575=CARTESIAN_POINT('Ctrl Pts',(-4.69936704292938,12.2,-9.71407033705063));
#289576=CARTESIAN_POINT('Ctrl Pts',(-4.69700647029006,12.2,-9.71148868723156));
#289577=CARTESIAN_POINT('Ctrl Pts',(-4.69464589797236,12.2,-9.70890703776424));
#289578=CARTESIAN_POINT('Ctrl Pts',(-4.69230043648095,12.2,-9.70633310220778));
#289579=CARTESIAN_POINT('Ctrl Pts',(-4.68997009611436,12.2,-9.70376703269454));
#289580=CARTESIAN_POINT('Ctrl Pts',(-4.68763975543026,12.2,-9.70120096283167));
#289581=CARTESIAN_POINT('Ctrl Pts',(-4.68532453581146,12.2,-9.69864275870007));
#289582=CARTESIAN_POINT('Ctrl Pts',(-4.68302444974166,12.2,-9.69609257744998));
#289583=CARTESIAN_POINT('Ctrl Pts',(-4.68072436367186,12.2,-9.69354239619989));
#289584=CARTESIAN_POINT('Ctrl Pts',(-4.67843940916771,12.2,-9.69100023702849));
#289585=CARTESIAN_POINT('Ctrl Pts',(-4.67616960037889,12.2,-9.68846625533568));
#289586=CARTESIAN_POINT('Ctrl Pts',(-4.67389979189934,12.2,-9.68593227398813));
#289587=CARTESIAN_POINT('Ctrl Pts',(-4.67164512580088,12.2,-9.68340647237124));
#289588=CARTESIAN_POINT('Ctrl Pts',(-4.66940561475152,12.2,-9.68088900751003));
#289589=CARTESIAN_POINT('Ctrl Pts',(-4.66716610339703,12.2,-9.67837154230581));
#289590=CARTESIAN_POINT('Ctrl Pts',(-4.66494174666043,12.2,-9.67586241396267));
#289591=CARTESIAN_POINT('Ctrl Pts',(-4.66273255459713,12.2,-9.67336178354946));
#289592=CARTESIAN_POINT('Ctrl Pts',(-4.65997106466851,12.2,-9.67023599570333));
#289593=CARTESIAN_POINT('Ctrl Pts',(-4.65723326972084,12.2,-9.66712348473242));
#289594=CARTESIAN_POINT('Ctrl Pts',(-4.654519188195,12.2,-9.66402456855298));
#289595=CARTESIAN_POINT('Ctrl Pts',(-4.651805106965,12.2,-9.66092565271133));
#289596=CARTESIAN_POINT('Ctrl Pts',(-4.64911474044341,12.2,-9.65784033211808));
#289597=CARTESIAN_POINT('Ctrl Pts',(-4.64644810656547,12.2,-9.65476892641006));
#289598=CARTESIAN_POINT('Ctrl Pts',(-4.64378147239686,12.2,-9.65169752036726));
#289599=CARTESIAN_POINT('Ctrl Pts',(-4.64113857041119,12.2,-9.64864003108809));
#289600=CARTESIAN_POINT('Ctrl Pts',(-4.63851941811759,12.2,-9.64559678490637));
#289601=CARTESIAN_POINT('Ctrl Pts',(-4.63590026582398,12.2,-9.64255353872465));
#289602=CARTESIAN_POINT('Ctrl Pts',(-4.6333048632772,12.2,-9.63952453455656));
#289603=CARTESIAN_POINT('Ctrl Pts',(-4.63073322834471,12.2,-9.63651010344427));
#289604=CARTESIAN_POINT('Ctrl Pts',(-4.62764726625754,12.2,-9.63289278591239));
#289605=CARTESIAN_POINT('Ctrl Pts',(-4.62459552761305,12.2,-9.62929645501804));
#289606=CARTESIAN_POINT('Ctrl Pts',(-4.62157804038318,12.2,-9.62572169039588));
#289607=CARTESIAN_POINT('Ctrl Pts',(-4.61906346782865,12.2,-9.62274272003977));
#289608=CARTESIAN_POINT('Ctrl Pts',(-4.61657268179206,12.2,-9.61977872733529));
#289609=CARTESIAN_POINT('Ctrl Pts',(-4.61410569366899,12.2,-9.61683005386429));
#289610=CARTESIAN_POINT('Ctrl Pts',(-4.61163870554591,12.2,-9.6138813803933));
#289611=CARTESIAN_POINT('Ctrl Pts',(-4.60919551947046,12.2,-9.6109480271837));
#289612=CARTESIAN_POINT('Ctrl Pts',(-4.60677614620855,12.2,-9.60803033885168));
#289613=CARTESIAN_POINT('Ctrl Pts',(-4.60435677321034,12.2,-9.60511265083768));
#289614=CARTESIAN_POINT('Ctrl Pts',(-4.60196121338143,12.2,-9.60221063109198));
#289615=CARTESIAN_POINT('Ctrl Pts',(-4.59958947961023,12.2,-9.5993246288358));
#289616=CARTESIAN_POINT('Ctrl Pts',(-4.59721774558051,12.2,-9.59643862626505));
#289617=CARTESIAN_POINT('Ctrl Pts',(-4.59486983921152,12.2,-9.5935686433746));
#289618=CARTESIAN_POINT('Ctrl Pts',(-4.59254577011232,12.2,-9.59071503733156));
#289619=CARTESIAN_POINT('Ctrl Pts',(-4.59022170101313,12.2,-9.58786143128853));
#289620=CARTESIAN_POINT('Ctrl Pts',(-4.58792146964639,12.2,-9.58502420073619));
#289621=CARTESIAN_POINT('Ctrl Pts',(-4.585645087031,12.2,-9.58220371205245));
#289622=CARTESIAN_POINT('Ctrl Pts',(-4.58336870441562,12.2,-9.57938322336871));
#289623=CARTESIAN_POINT('Ctrl Pts',(-4.58111617018602,12.2,-9.57657947431099));
#289624=CARTESIAN_POINT('Ctrl Pts',(-4.5788874944209,12.2,-9.57379283590732));
#289625=CARTESIAN_POINT('Ctrl Pts',(-4.57665881865576,12.2,-9.57100619750366));
#289626=CARTESIAN_POINT('Ctrl Pts',(-4.57445400159402,12.2,-9.56823666828653));
#289627=CARTESIAN_POINT('Ctrl Pts',(-4.57227305013444,12.2,-9.56548462418839));
#289628=CARTESIAN_POINT('Ctrl Pts',(-4.57009209867486,12.2,-9.56273258009026));
#289629=CARTESIAN_POINT('Ctrl Pts',(-4.56793501542203,12.2,-9.55999802091383));
#289630=CARTESIAN_POINT('Ctrl Pts',(-4.56580180471783,12.2,-9.55728132777645));
#289631=CARTESIAN_POINT('Ctrl Pts',(-4.56366859401363,12.2,-9.55456463463907));
#289632=CARTESIAN_POINT('Ctrl Pts',(-4.5615592585222,12.2,-9.55186580839441));
#289633=CARTESIAN_POINT('Ctrl Pts',(-4.55947380275833,12.2,-9.5491852360333));
#289634=CARTESIAN_POINT('Ctrl Pts',(-4.55738834699444,12.2,-9.54650466367219));
#289635=CARTESIAN_POINT('Ctrl Pts',(-4.55532677154696,12.2,-9.54384234556603));
#289636=CARTESIAN_POINT('Ctrl Pts',(-4.55328908223222,12.2,-9.54119867499853));
#289637=CARTESIAN_POINT('Ctrl Pts',(-4.55084385514338,12.2,-9.53802627043278));
#289638=CARTESIAN_POINT('Ctrl Pts',(-4.54843302214482,12.2,-9.53488071970793));
#289639=CARTESIAN_POINT('Ctrl Pts',(-4.54605659139632,12.2,-9.53176271515335));
#289640=CARTESIAN_POINT('Ctrl Pts',(-4.54368016043197,12.2,-9.52864471031555));
#289641=CARTESIAN_POINT('Ctrl Pts',(-4.54133813251356,12.2,-9.52555425267282));
#289642=CARTESIAN_POINT('Ctrl Pts',(-4.53903050947347,12.2,-9.52249204892452));
#289643=CARTESIAN_POINT('Ctrl Pts',(-4.53672288664299,12.2,-9.51942984545438));
#289644=CARTESIAN_POINT('Ctrl Pts',(-4.53444966962028,12.2,-9.51639589744254));
#289645=CARTESIAN_POINT('Ctrl Pts',(-4.5322108606198,12.2,-9.51339092688632));
#289646=CARTESIAN_POINT('Ctrl Pts',(-4.52997205161932,12.2,-9.51038595633012));
#289647=CARTESIAN_POINT('Ctrl Pts',(-4.52776764941607,12.2,-9.50740996380491));
#289648=CARTESIAN_POINT('Ctrl Pts',(-4.52559765441008,12.2,-9.50446368641068));
#289649=CARTESIAN_POINT('Ctrl Pts',(-4.5234276594041,12.2,-9.50151740901644));
#289650=CARTESIAN_POINT('Ctrl Pts',(-4.5212920698717,12.2,-9.49860084922844));
#289651=CARTESIAN_POINT('Ctrl Pts',(-4.5191908829457,12.2,-9.49571475883122));
#289652=CARTESIAN_POINT('Ctrl Pts',(-4.51708969582884,12.2,-9.49282866817185));
#289653=CARTESIAN_POINT('Ctrl Pts',(-4.51502291210698,12.2,-9.48997304829872));
#289654=CARTESIAN_POINT('Ctrl Pts',(-4.51299052391437,12.2,-9.48714866981283));
#289655=CARTESIAN_POINT('Ctrl Pts',(-4.51095813590639,12.2,-9.48432429158348));
#289656=CARTESIAN_POINT('Ctrl Pts',(-4.50896014198021,12.2,-9.48153115490518));
#289657=CARTESIAN_POINT('Ctrl Pts',(-4.50699653595922,12.2,-9.47877004774288));
#289658=CARTESIAN_POINT('Ctrl Pts',(-4.50503292993824,12.2,-9.47600894058059));
#289659=CARTESIAN_POINT('Ctrl Pts',(-4.50310370915668,12.2,-9.47327986356477));
#289660=CARTESIAN_POINT('Ctrl Pts',(-4.50120886122321,12.2,-9.47058362332719));
#289661=CARTESIAN_POINT('Ctrl Pts',(-4.49931401311762,12.2,-9.46788738284471));
#289662=CARTESIAN_POINT('Ctrl Pts',(-4.49745354028197,12.2,-9.46522397837363));
#289663=CARTESIAN_POINT('Ctrl Pts',(-4.49562742318395,12.2,-9.46259423514845));
#289664=CARTESIAN_POINT('Ctrl Pts',(-4.49380130625181,12.2,-9.45996449216213));
#289665=CARTESIAN_POINT('Ctrl Pts',(-4.49200954673666,12.2,-9.45736840990308));
#289666=CARTESIAN_POINT('Ctrl Pts',(-4.49025212654247,12.2,-9.45480683398446));
#289667=CARTESIAN_POINT('Ctrl Pts',(-4.48849470634826,12.2,-9.45224525806583));
#289668=CARTESIAN_POINT('Ctrl Pts',(-4.4867716246584,12.2,-9.44971818930846));
#289669=CARTESIAN_POINT('Ctrl Pts',(-4.48508285871741,12.2,-9.44722649047989));
#289670=CARTESIAN_POINT('Ctrl Pts',(-4.48339409262302,12.2,-9.444734791425));
#289671=CARTESIAN_POINT('Ctrl Pts',(-4.48173964300225,12.2,-9.44227846404994));
#289672=CARTESIAN_POINT('Ctrl Pts',(-4.48011948358502,12.2,-9.43985839296593));
#289673=CARTESIAN_POINT('Ctrl Pts',(-4.47849932431494,12.2,-9.43743832210177));
#289674=CARTESIAN_POINT('Ctrl Pts',(-4.47691345406029,12.2,-9.43505450957303));
#289675=CARTESIAN_POINT('Ctrl Pts',(-4.47536184594999,12.2,-9.43270786274161));
#289676=CARTESIAN_POINT('Ctrl Pts',(-4.47355163639402,12.2,-9.42997010796286));
#289677=CARTESIAN_POINT('Ctrl Pts',(-4.47178806018459,12.2,-9.42728293651277));
#289678=CARTESIAN_POINT('Ctrl Pts',(-4.47007106361604,12.2,-9.42464783456488));
#289679=CARTESIAN_POINT('Ctrl Pts',(-4.46859935234796,12.2,-9.42238917586963));
#289680=CARTESIAN_POINT('Ctrl Pts',(-4.46716186176567,12.2,-9.42016877156237));
#289681=CARTESIAN_POINT('Ctrl Pts',(-4.46575855748332,12.2,-9.41798758122494));
#289682=CARTESIAN_POINT('Ctrl Pts',(-4.46435525320098,12.2,-9.41580639088751));
#289683=CARTESIAN_POINT('Ctrl Pts',(-4.46298613169106,12.2,-9.41366441709268));
#289684=CARTESIAN_POINT('Ctrl Pts',(-4.46165115442089,12.2,-9.41156264164503));
#289685=CARTESIAN_POINT('Ctrl Pts',(-4.46031617702945,12.2,-9.40946086600647));
#289686=CARTESIAN_POINT('Ctrl Pts',(-4.45901534261198,12.2,-9.40739929082871));
#289687=CARTESIAN_POINT('Ctrl Pts',(-4.4577486043786,12.2,-9.4053789264714));
#289688=CARTESIAN_POINT('Ctrl Pts',(-4.45648186626027,12.2,-9.40335856229759));
#289689=CARTESIAN_POINT('Ctrl Pts',(-4.45524922600296,12.2,-9.40137941174577));
#289690=CARTESIAN_POINT('Ctrl Pts',(-4.4540506319578,12.2,-9.39944251172409));
#289691=CARTESIAN_POINT('Ctrl Pts',(-4.45285203791264,12.2,-9.39750561170241));
#289692=CARTESIAN_POINT('Ctrl Pts',(-4.4516874925305,12.2,-9.39561096341066));
#289693=CARTESIAN_POINT('Ctrl Pts',(-4.45055693932009,12.2,-9.39375963655935));
#289694=CARTESIAN_POINT('Ctrl Pts',(-4.44942638600698,12.2,-9.39190830953989));
#289695=CARTESIAN_POINT('Ctrl Pts',(-4.44832982439813,12.2,-9.3901003030425));
#289696=CARTESIAN_POINT('Ctrl Pts',(-4.44726719709251,12.2,-9.38833671903271));
#289697=CARTESIAN_POINT('Ctrl Pts',(-4.44620456988342,12.2,-9.38657313518314));
#289698=CARTESIAN_POINT('Ctrl Pts',(-4.44517587501664,12.2,-9.38485397162112));
#289699=CARTESIAN_POINT('Ctrl Pts',(-4.44418105163759,12.2,-9.38318036293392));
#289700=CARTESIAN_POINT('Ctrl Pts',(-4.44285939486153,12.2,-9.38095691673382));
#289701=CARTESIAN_POINT('Ctrl Pts',(-4.4415975258323,12.2,-9.3788138680557));
#289702=CARTESIAN_POINT('Ctrl Pts',(-4.44039525800005,12.2,-9.37675396700002));
#289703=CARTESIAN_POINT('Ctrl Pts',(-4.44039525800005,15.2,-9.37675396700002));
#289704=CARTESIAN_POINT('Ctrl Pts',(-4.44129587306896,15.2,-9.37829703243141));
#289705=CARTESIAN_POINT('Ctrl Pts',(-4.44222992933227,15.2,-9.37988675705661));
#289706=CARTESIAN_POINT('Ctrl Pts',(-4.44319751536069,15.2,-9.38152198184585));
#289707=CARTESIAN_POINT('Ctrl Pts',(-4.44416976757804,15.2,-9.38316509251559));
#289708=CARTESIAN_POINT('Ctrl Pts',(-4.44517586568178,15.2,-9.3848541409591));
#289709=CARTESIAN_POINT('Ctrl Pts',(-4.44621587887569,15.2,-9.38658798489277));
#289710=CARTESIAN_POINT('Ctrl Pts',(-4.44725589197513,15.2,-9.38832182866894));
#289711=CARTESIAN_POINT('Ctrl Pts',(-4.4483298151569,15.2,-9.3901004685328));
#289712=CARTESIAN_POINT('Ctrl Pts',(-4.44943771428333,15.2,-9.3919227914666));
#289713=CARTESIAN_POINT('Ctrl Pts',(-4.45054561340975,15.2,-9.39374511440041));
#289714=CARTESIAN_POINT('Ctrl Pts',(-4.45168748543062,15.2,-9.39561112218358));
#289715=CARTESIAN_POINT('Ctrl Pts',(-4.45286338586133,15.2,-9.39751973529041));
#289716=CARTESIAN_POINT('Ctrl Pts',(-4.45403928639883,15.2,-9.39942834857061));
#289717=CARTESIAN_POINT('Ctrl Pts',(-4.45524921782382,15.2,-9.40137956588904));
#289718=CARTESIAN_POINT('Ctrl Pts',(-4.45649323014394,15.2,-9.40337233916716));
#289719=CARTESIAN_POINT('Ctrl Pts',(-4.45773724235106,15.2,-9.40536511226427));
#289720=CARTESIAN_POINT('Ctrl Pts',(-4.4590153346589,15.2,-9.40739944035009));
#289721=CARTESIAN_POINT('Ctrl Pts',(-4.46032755578393,15.2,-9.40947430345089));
#289722=CARTESIAN_POINT('Ctrl Pts',(-4.46163977690896,15.2,-9.41154916655169));
#289723=CARTESIAN_POINT('Ctrl Pts',(-4.46298612577653,15.2,-9.41366456319599));
#289724=CARTESIAN_POINT('Ctrl Pts',(-4.46436664589157,15.2,-9.415819499616));
#289725=CARTESIAN_POINT('Ctrl Pts',(-4.46574716613199,15.2,-9.41797443623173));
#289726=CARTESIAN_POINT('Ctrl Pts',(-4.46716185662663,15.2,-9.42016891470236));
#289727=CARTESIAN_POINT('Ctrl Pts',(-4.4686107578746,15.2,-9.42240196349335));
#289728=CARTESIAN_POINT('Ctrl Pts',(-4.47005965899096,15.2,-9.42463501208151));
#289729=CARTESIAN_POINT('Ctrl Pts',(-4.47154276904483,15.2,-9.4269066335916));
#289730=CARTESIAN_POINT('Ctrl Pts',(-4.4730601250745,15.2,-9.42921588234262));
#289731=CARTESIAN_POINT('Ctrl Pts',(-4.47457748110417,15.2,-9.43152513109366));
#289732=CARTESIAN_POINT('Ctrl Pts',(-4.47612908174782,15.2,-9.43387200969173));
#289733=CARTESIAN_POINT('Ctrl Pts',(-4.47771495793871,15.2,-9.43625559460353));
#289734=CARTESIAN_POINT('Ctrl Pts',(-4.47930083412959,15.2,-9.43863917951534));
#289735=CARTESIAN_POINT('Ctrl Pts',(-4.48092098727379,15.2,-9.44105947538224));
#289736=CARTESIAN_POINT('Ctrl Pts',(-4.48257544329467,15.2,-9.44351558120724));
#289737=CARTESIAN_POINT('Ctrl Pts',(-4.48422989946583,15.2,-9.44597168725533));
#289738=CARTESIAN_POINT('Ctrl Pts',(-4.48591865903198,15.2,-9.44846360574858));
#289739=CARTESIAN_POINT('Ctrl Pts',(-4.48764174712739,15.2,-9.45099045888782));
#289740=CARTESIAN_POINT('Ctrl Pts',(-4.48936483506628,15.2,-9.45351731179754));
#289741=CARTESIAN_POINT('Ctrl Pts',(-4.49112225103122,15.2,-9.4560791013147));
#289742=CARTESIAN_POINT('Ctrl Pts',(-4.49291401422419,15.2,-9.45867497223211));
#289743=CARTESIAN_POINT('Ctrl Pts',(-4.49470577741715,15.2,-9.46127084314952));
#289744=CARTESIAN_POINT('Ctrl Pts',(-4.49653189046714,15.2,-9.46390079412535));
#289745=CARTESIAN_POINT('Ctrl Pts',(-4.49839236756388,15.2,-9.46656399219301));
#289746=CARTESIAN_POINT('Ctrl Pts',(-4.50025284482961,15.2,-9.46922719050256));
#289747=CARTESIAN_POINT('Ctrl Pts',(-4.50214768997363,15.2,-9.47192363591533));
#289748=CARTESIAN_POINT('Ctrl Pts',(-4.50407691416362,15.2,-9.47465251139882));
#289749=CARTESIAN_POINT('Ctrl Pts',(-4.50600613817835,15.2,-9.47738138663443));
#289750=CARTESIAN_POINT('Ctrl Pts',(-4.50796974008769,15.2,-9.48014269291256));
#289751=CARTESIAN_POINT('Ctrl Pts',(-4.50996773677409,15.2,-9.48293563224036));
#289752=CARTESIAN_POINT('Ctrl Pts',(-4.51196573346048,15.2,-9.48572857156816));
#289753=CARTESIAN_POINT('Ctrl Pts',(-4.51399811893549,15.2,-9.48855314476124));
#289754=CARTESIAN_POINT('Ctrl Pts',(-4.51606490402472,15.2,-9.49140857198872));
#289755=CARTESIAN_POINT('Ctrl Pts',(-4.51813168930169,15.2,-9.49426399947558));
#289756=CARTESIAN_POINT('Ctrl Pts',(-4.52023287548161,15.2,-9.49715028115079));
#289757=CARTESIAN_POINT('Ctrl Pts',(-4.52236846570667,15.2,-9.50006665304049));
#289758=CARTESIAN_POINT('Ctrl Pts',(-4.52450405573775,15.2,-9.50298302466529));
#289759=CARTESIAN_POINT('Ctrl Pts',(-4.52667405050507,15.2,-9.50592948864139));
#289760=CARTESIAN_POINT('Ctrl Pts',(-4.52887845250833,15.2,-9.50890529619996));
#289761=CARTESIAN_POINT('Ctrl Pts',(-4.53108285451158,15.2,-9.51188110375853));
#289762=CARTESIAN_POINT('Ctrl Pts',(-4.5333216636262,15.2,-9.5148862582502));
#289763=CARTESIAN_POINT('Ctrl Pts',(-4.53559487973851,15.2,-9.51792002595656));
#289764=CARTESIAN_POINT('Ctrl Pts',(-4.53786809605731,15.2,-9.52095379393847));
#289765=CARTESIAN_POINT('Ctrl Pts',(-4.54017571979194,15.2,-9.52401617530812));
#289766=CARTESIAN_POINT('Ctrl Pts',(-4.54251774775529,15.2,-9.52710645706181));
#289767=CARTESIAN_POINT('Ctrl Pts',(-4.54485977550589,15.2,-9.5301967385348));
#289768=CARTESIAN_POINT('Ctrl Pts',(-4.54723620634433,15.2,-9.533314916993));
#289769=CARTESIAN_POINT('Ctrl Pts',(-4.54964703726776,15.2,-9.5364602954764));
#289770=CARTESIAN_POINT('Ctrl Pts',(-4.55205786819119,15.2,-9.5396056739598));
#289771=CARTESIAN_POINT('Ctrl Pts',(-4.55450309886493,15.2,-9.54277824955146));
#289772=CARTESIAN_POINT('Ctrl Pts',(-4.55698271885667,15.2,-9.54597733635073));
#289773=CARTESIAN_POINT('Ctrl Pts',(-4.55904906892486,15.2,-9.54864324211365));
#289774=CARTESIAN_POINT('Ctrl Pts',(-4.5611393024409,15.2,-9.55132755935761));
#289775=CARTESIAN_POINT('Ctrl Pts',(-4.56325341237021,15.2,-9.55402989685668));
#289776=CARTESIAN_POINT('Ctrl Pts',(-4.56536752229952,15.2,-9.55673223435573));
#289777=CARTESIAN_POINT('Ctrl Pts',(-4.56750550940575,15.2,-9.559452592325));
#289778=CARTESIAN_POINT('Ctrl Pts',(-4.56966736524882,15.2,-9.56219058803181));
#289779=CARTESIAN_POINT('Ctrl Pts',(-4.57182922109189,15.2,-9.56492858373862));
#289780=CARTESIAN_POINT('Ctrl Pts',(-4.57401494733888,15.2,-9.56768421420552));
#289781=CARTESIAN_POINT('Ctrl Pts',(-4.57622453553333,15.2,-9.5704571057333));
#289782=CARTESIAN_POINT('Ctrl Pts',(-4.57843412372777,15.2,-9.57322999726108));
#289783=CARTESIAN_POINT('Ctrl Pts',(-4.58066757280202,15.2,-9.57602014604425));
#289784=CARTESIAN_POINT('Ctrl Pts',(-4.5829248752429,15.2,-9.57882718425151));
#289785=CARTESIAN_POINT('Ctrl Pts',(-4.58518217768378,15.2,-9.58163422245876));
#289786=CARTESIAN_POINT('Ctrl Pts',(-4.58746333292187,15.2,-9.58445814714054));
#289787=CARTESIAN_POINT('Ctrl Pts',(-4.58976832965921,15.2,-9.5872985938775));
#289788=CARTESIAN_POINT('Ctrl Pts',(-4.59207332639657,15.2,-9.59013904061447));
#289789=CARTESIAN_POINT('Ctrl Pts',(-4.59440216662497,15.2,-9.59299600884825));
#289790=CARTESIAN_POINT('Ctrl Pts',(-4.59675483669568,15.2,-9.59586913815465));
#289791=CARTESIAN_POINT('Ctrl Pts',(-4.59910750676638,15.2,-9.59874226746106));
#289792=CARTESIAN_POINT('Ctrl Pts',(-4.60148400954602,15.2,-9.60163155960212));
#289793=CARTESIAN_POINT('Ctrl Pts',(-4.60388432973706,15.2,-9.60453665738727));
#289794=CARTESIAN_POINT('Ctrl Pts',(-4.60676471386164,15.2,-9.60802277460278));
#289795=CARTESIAN_POINT('Ctrl Pts',(-4.60967939652379,15.2,-9.61153165427825));
#289796=CARTESIAN_POINT('Ctrl Pts',(-4.61262835724999,15.2,-9.61506269148331));
#289797=CARTESIAN_POINT('Ctrl Pts',(-4.61508582461112,15.2,-9.61800522259443));
#289798=CARTESIAN_POINT('Ctrl Pts',(-4.61756709430659,15.2,-9.62096314346027));
#289799=CARTESIAN_POINT('Ctrl Pts',(-4.62007215181803,15.2,-9.6239361087516));
#289800=CARTESIAN_POINT('Ctrl Pts',(-4.62307822072255,15.2,-9.62750366697158));
#289801=CARTESIAN_POINT('Ctrl Pts',(-4.62611854627076,15.2,-9.63109288948539));
#289802=CARTESIAN_POINT('Ctrl Pts',(-4.62919309907425,15.2,-9.63470319551998));
#289803=CARTESIAN_POINT('Ctrl Pts',(-4.63175522650357,15.2,-9.63771178399145));
#289804=CARTESIAN_POINT('Ctrl Pts',(-4.6343411247696,15.2,-9.64073501219105));
#289805=CARTESIAN_POINT('Ctrl Pts',(-4.63695077629614,15.2,-9.64377254830142));
#289806=CARTESIAN_POINT('Ctrl Pts',(-4.63956042782267,15.2,-9.64681008441177));
#289807=CARTESIAN_POINT('Ctrl Pts',(-4.64219383285538,15.2,-9.64986192952252));
#289808=CARTESIAN_POINT('Ctrl Pts',(-4.64485097361803,15.2,-9.65292775500789));
#289809=CARTESIAN_POINT('Ctrl Pts',(-4.64750811438069,15.2,-9.65599358049328));
#289810=CARTESIAN_POINT('Ctrl Pts',(-4.65018899065296,15.2,-9.65907338792872));
#289811=CARTESIAN_POINT('Ctrl Pts',(-4.65289358545686,15.2,-9.66216685328996));
#289812=CARTESIAN_POINT('Ctrl Pts',(-4.65559818026076,15.2,-9.66526031865121));
#289813=CARTESIAN_POINT('Ctrl Pts',(-4.65832649309999,15.2,-9.66836744337775));
#289814=CARTESIAN_POINT('Ctrl Pts',(-4.66107850455832,15.2,-9.67148790726664));
#289815=CARTESIAN_POINT('Ctrl Pts',(-4.66328011384498,15.2,-9.6739842785138));
#289816=CARTESIAN_POINT('Ctrl Pts',(-4.66549689001951,15.2,-9.67648918765086));
#289817=CARTESIAN_POINT('Ctrl Pts',(-4.66772882336492,15.2,-9.67900247467757));
#289818=CARTESIAN_POINT('Ctrl Pts',(-4.66996075640623,15.2,-9.68151576136185));
#289819=CARTESIAN_POINT('Ctrl Pts',(-4.67220784738428,15.2,-9.68403742419639));
#289820=CARTESIAN_POINT('Ctrl Pts',(-4.67447008376513,15.2,-9.68656730572326));
#289821=CARTESIAN_POINT('Ctrl Pts',(-4.6767323204542,15.2,-9.68909718759483));
#289822=CARTESIAN_POINT('Ctrl Pts',(-4.67900970379279,15.2,-9.69163528819614));
#289823=CARTESIAN_POINT('Ctrl Pts',(-4.6813022231415,15.2,-9.69418144872462));
#289824=CARTESIAN_POINT('Ctrl Pts',(-4.68359474217786,15.2,-9.69672760890619));
#289825=CARTESIAN_POINT('Ctrl Pts',(-4.68590239654558,15.2,-9.69928183023391));
#289826=CARTESIAN_POINT('Ctrl Pts',(-4.68822517557692,15.2,-9.70184395702393));
#289827=CARTESIAN_POINT('Ctrl Pts',(-4.69054795492474,15.2,-9.70440608416305));
#289828=CARTESIAN_POINT('Ctrl Pts',(-4.69288585780274,15.2,-9.70697611574302));
#289829=CARTESIAN_POINT('Ctrl Pts',(-4.69523887454985,15.2,-9.70955389912408));
#289830=CARTESIAN_POINT('Ctrl Pts',(-4.69759189097635,15.2,-9.7121316821539));
#289831=CARTESIAN_POINT('Ctrl Pts',(-4.69996002057612,15.2,-9.71471721621443));
#289832=CARTESIAN_POINT('Ctrl Pts',(-4.70234325154698,15.2,-9.71731035027974));
#289833=CARTESIAN_POINT('Ctrl Pts',(-4.70472648284255,15.2,-9.71990348469834));
#289834=CARTESIAN_POINT('Ctrl Pts',(-4.70712481440659,15.2,-9.72250421721508));
#289835=CARTESIAN_POINT('Ctrl Pts',(-4.70953823570577,15.2,-9.72511239791327));
#289836=CARTESIAN_POINT('Ctrl Pts',(-4.71195165667613,15.2,-9.72772057825609));
#289837=CARTESIAN_POINT('Ctrl Pts',(-4.71438016588005,15.2,-9.73033620828677));
#289838=CARTESIAN_POINT('Ctrl Pts',(-4.71682375291217,15.2,-9.73295913786943));
#289839=CARTESIAN_POINT('Ctrl Pts',(-4.71926734027724,15.2,-9.73558206780946));
#289840=CARTESIAN_POINT('Ctrl Pts',(-4.72172600436934,15.2,-9.73821229534368));
#289841=CARTESIAN_POINT('Ctrl Pts',(-4.72419973122737,15.2,-9.74084967593232));
#289842=CARTESIAN_POINT('Ctrl Pts',(-4.72667345774834,15.2,-9.74348705616163));
#289843=CARTESIAN_POINT('Ctrl Pts',(-4.72916224918853,15.2,-9.74613158787284));
#289844=CARTESIAN_POINT('Ctrl Pts',(-4.73166609081563,15.2,-9.7487831260998));
#289845=CARTESIAN_POINT('Ctrl Pts',(-4.73416993278388,15.2,-9.75143466468803));
#289846=CARTESIAN_POINT('Ctrl Pts',(-4.73668882621595,15.2,-9.75409320831662));
#289847=CARTESIAN_POINT('Ctrl Pts',(-4.73922275631006,15.2,-9.7567586142518));
#289848=CARTESIAN_POINT('Ctrl Pts',(-4.74175668605892,15.2,-9.75942401982382));
#289849=CARTESIAN_POINT('Ctrl Pts',(-4.74430565351416,15.2,-9.76209628581778));
#289850=CARTESIAN_POINT('Ctrl Pts',(-4.74686964508079,15.2,-9.76477527132031));
#289851=CARTESIAN_POINT('Ctrl Pts',(-4.74943363699677,15.2,-9.76745425718785));
#289852=CARTESIAN_POINT('Ctrl Pts',(-4.75201265260585,15.2,-9.77013996024215));
#289853=CARTESIAN_POINT('Ctrl Pts',(-4.75460667802499,15.2,-9.77283224149999));
#289854=CARTESIAN_POINT('Ctrl Pts',(-4.75720070344414,15.2,-9.77552452275782));
#289855=CARTESIAN_POINT('Ctrl Pts',(-4.75980973894005,15.2,-9.77822337983588));
#289856=CARTESIAN_POINT('Ctrl Pts',(-4.7624337701957,15.2,-9.78092867448397));
#289857=CARTESIAN_POINT('Ctrl Pts',(-4.76505780109382,15.2,-9.78363396876347));
#289858=CARTESIAN_POINT('Ctrl Pts',(-4.76769682802537,15.2,-9.78634569908302));
#289859=CARTESIAN_POINT('Ctrl Pts',(-4.77035083626486,15.2,-9.7890637280398));
#289860=CARTESIAN_POINT('Ctrl Pts',(-4.77300484486595,15.2,-9.79178175736693));
#289861=CARTESIAN_POINT('Ctrl Pts',(-4.77567383341881,15.2,-9.79450608374421));
#289862=CARTESIAN_POINT('Ctrl Pts',(-4.7783577894555,15.2,-9.79723657117143));
#289863=CARTESIAN_POINT('Ctrl Pts',(-4.7810417451265,15.2,-9.79996705822662));
#289864=CARTESIAN_POINT('Ctrl Pts',(-4.78374066790945,15.2,-9.80270370614766));
#289865=CARTESIAN_POINT('Ctrl Pts',(-4.78645454151995,15.2,-9.80544637853417));
#289866=CARTESIAN_POINT('Ctrl Pts',(-4.78984688381039,15.2,-9.80887471929756));
#289867=CARTESIAN_POINT('Ctrl Pts',(-4.793262589427,15.2,-9.81231247312136));
#289868=CARTESIAN_POINT('Ctrl Pts',(-4.79670162520646,15.2,-9.81575937799811));
#289869=CARTESIAN_POINT('Ctrl Pts',(-4.79945285397997,15.2,-9.81851690204981));
#289870=CARTESIAN_POINT('Ctrl Pts',(-4.80221901562662,15.2,-9.82128028213457));
#289871=CARTESIAN_POINT('Ctrl Pts',(-4.80500009361305,15.2,-9.82404938495274));
#289872=CARTESIAN_POINT('Ctrl Pts',(-4.80778117122055,15.2,-9.82681848739362));
#289873=CARTESIAN_POINT('Ctrl Pts',(-4.81057716615944,15.2,-9.82959331418652));
#289874=CARTESIAN_POINT('Ctrl Pts',(-4.81338806176202,15.2,-9.83237373201441));
#289875=CARTESIAN_POINT('Ctrl Pts',(-4.81619895774758,15.2,-9.83515415022114));
#289876=CARTESIAN_POINT('Ctrl Pts',(-4.81902475443926,15.2,-9.83794015955746));
#289877=CARTESIAN_POINT('Ctrl Pts',(-4.82186543590395,15.2,-9.84073163040508));
#289878=CARTESIAN_POINT('Ctrl Pts',(-4.82470611698159,15.2,-9.84352310087235));
#289879=CARTESIAN_POINT('Ctrl Pts',(-4.827561683815,15.2,-9.84632003093095));
#289880=CARTESIAN_POINT('Ctrl Pts',(-4.83043211752381,15.2,-9.84912229331263));
#289881=CARTESIAN_POINT('Ctrl Pts',(-4.83330255162373,15.2,-9.85192455607611));
#289882=CARTESIAN_POINT('Ctrl Pts',(-4.83618785594209,15.2,-9.85473215061525));
#289883=CARTESIAN_POINT('Ctrl Pts',(-4.83908801071222,15.2,-9.85754494821332));
#289884=CARTESIAN_POINT('Ctrl Pts',(-4.84198816508721,15.2,-9.86035774542816));
#289885=CARTESIAN_POINT('Ctrl Pts',(-4.84490317079812,15.2,-9.8631757464364));
#289886=CARTESIAN_POINT('Ctrl Pts',(-4.84783301227931,15.2,-9.86599882353843));
#289887=CARTESIAN_POINT('Ctrl Pts',(-4.85076285415969,15.2,-9.86882190102509));
#289888=CARTESIAN_POINT('Ctrl Pts',(-4.85370753039946,15.2,-9.87165005590408));
#289889=CARTESIAN_POINT('Ctrl Pts',(-4.85666702501868,15.2,-9.87448316079359));
#289890=CARTESIAN_POINT('Ctrl Pts',(-4.85962651923467,15.2,-9.87731626529708));
#289891=CARTESIAN_POINT('Ctrl Pts',(-4.86260083098215,15.2,-9.88015432137363));
#289892=CARTESIAN_POINT('Ctrl Pts',(-4.86558994323629,15.2,-9.88299720258519));
#289893=CARTESIAN_POINT('Ctrl Pts',(-4.86857905589768,15.2,-9.88584008418408));
#289894=CARTESIAN_POINT('Ctrl Pts',(-4.87158296992992,15.2,-9.8886877912251));
#289895=CARTESIAN_POINT('Ctrl Pts',(-4.87460166598333,15.2,-9.89154020199166));
#289896=CARTESIAN_POINT('Ctrl Pts',(-4.87837503584443,15.2,-9.89510571525555));
#289897=CARTESIAN_POINT('Ctrl Pts',(-4.88217150414023,15.2,-9.89867857641345));
#289898=CARTESIAN_POINT('Ctrl Pts',(-4.88599103631042,15.2,-9.90225854573528));
#289899=CARTESIAN_POINT('Ctrl Pts',(-4.88904666179677,15.2,-9.90512252095861));
#289900=CARTESIAN_POINT('Ctrl Pts',(-4.89211704631597,15.2,-9.90799104656559));
#289901=CARTESIAN_POINT('Ctrl Pts',(-4.89520217572892,15.2,-9.91086400099694));
#289902=CARTESIAN_POINT('Ctrl Pts',(-4.89828730556222,15.2,-9.91373695581972));
#289903=CARTESIAN_POINT('Ctrl Pts',(-4.90138717653582,15.2,-9.91661433966796));
#289904=CARTESIAN_POINT('Ctrl Pts',(-4.90450177248333,15.2,-9.91949603199166));
#289905=CARTESIAN_POINT('Ctrl Pts',(-4.90761636843084,15.2,-9.92237772431537));
#289906=CARTESIAN_POINT('Ctrl Pts',(-4.91074568829676,15.2,-9.92526372623405));
#289907=CARTESIAN_POINT('Ctrl Pts',(-4.91388971424739,15.2,-9.92815391778088));
#289908=CARTESIAN_POINT('Ctrl Pts',(-4.91703373976965,15.2,-9.93104410893392));
#289909=CARTESIAN_POINT('Ctrl Pts',(-4.92019247112068,15.2,-9.93393848935794));
#289910=CARTESIAN_POINT('Ctrl Pts',(-4.92336588876451,15.2,-9.93683694318969));
#289911=CARTESIAN_POINT('Ctrl Pts',(-4.92733266114358,15.2,-9.94046001077558));
#289912=CARTESIAN_POINT('Ctrl Pts',(-4.93132238283334,15.2,-9.94408944093889));
#289913=CARTESIAN_POINT('Ctrl Pts',(-4.93533501595833,15.2,-9.94772500600833));
#289914=CARTESIAN_POINT('Ctrl Pts',(-4.93854512263327,15.2,-9.95063345822239));
#289915=CARTESIAN_POINT('Ctrl Pts',(-4.94176989238772,15.2,-9.95354583590637));
#289916=CARTESIAN_POINT('Ctrl Pts',(-4.94500930628798,15.2,-9.95646202551013));
#289917=CARTESIAN_POINT('Ctrl Pts',(-4.94824871974687,15.2,-9.95937821471655));
#289918=CARTESIAN_POINT('Ctrl Pts',(-4.95150277701686,15.2,-9.96229821511542));
#289919=CARTESIAN_POINT('Ctrl Pts',(-4.95477145976444,15.2,-9.96522191172301));
#289920=CARTESIAN_POINT('Ctrl Pts',(-4.95804014295737,15.2,-9.96814560872894));
#289921=CARTESIAN_POINT('Ctrl Pts',(-4.96132344816353,15.2,-9.9710730021441));
#289922=CARTESIAN_POINT('Ctrl Pts',(-4.96462136078921,15.2,-9.97400397847088));
#289923=CARTESIAN_POINT('Ctrl Pts',(-4.96791927296556,15.2,-9.97693495439831));
#289924=CARTESIAN_POINT('Ctrl Pts',(-4.97123179003945,15.2,-9.97986951303868));
#289925=CARTESIAN_POINT('Ctrl Pts',(-4.97455889221133,15.2,-9.98280754224305));
#289926=CARTESIAN_POINT('Ctrl Pts',(-4.97705421895357,15.2,-9.9850110642464));
#289927=CARTESIAN_POINT('Ctrl Pts',(-4.97955774913085,15.2,-9.98721653815976));
#289928=CARTESIAN_POINT('Ctrl Pts',(-4.98206947595579,15.2,-9.98942391685628));
#289929=CARTESIAN_POINT('Ctrl Pts',(-4.98625568748279,15.2,-9.99310288148416));
#289930=CARTESIAN_POINT('Ctrl Pts',(-4.99046466364678,15.2,-9.99678713890346));
#289931=CARTESIAN_POINT('Ctrl Pts',(-4.99469636746505,15.2,-10.0004764692504));
#289932=CARTESIAN_POINT('Ctrl Pts',(-4.99723538966376,15.2,-10.0026900673782));
#289933=CARTESIAN_POINT('Ctrl Pts',(-4.99978259340357,15.2,-10.0049054927641));
#289934=CARTESIAN_POINT('Ctrl Pts',(-5.0023379696846,15.2,-10.0071226992667));
#289935=CARTESIAN_POINT('Ctrl Pts',(-5.00489334642986,15.2,-10.009339906172));
#289936=CARTESIAN_POINT('Ctrl Pts',(-5.0074568963191,15.2,-10.0115588927778));
#289937=CARTESIAN_POINT('Ctrl Pts',(-5.01002861052731,15.2,-10.0137796147258));
#289938=CARTESIAN_POINT('Ctrl Pts',(-5.0143147997842,15.2,-10.0174808170311));
#289939=CARTESIAN_POINT('Ctrl Pts',(-5.01862366698522,15.2,-10.0211868384584));
#289940=CARTESIAN_POINT('Ctrl Pts',(-5.02295517290012,15.2,-10.024897464998));
#289941=CARTESIAN_POINT('Ctrl Pts',(-5.02555407711004,15.2,-10.027123841488));
#289942=CARTESIAN_POINT('Ctrl Pts',(-5.02816113062227,15.2,-10.0293518765785));
#289943=CARTESIAN_POINT('Ctrl Pts',(-5.03077632533679,15.2,-10.0315815250277));
#289944=CARTESIAN_POINT('Ctrl Pts',(-5.03339151957621,15.2,-10.0338111730719));
#289945=CARTESIAN_POINT('Ctrl Pts',(-5.03601485498186,15.2,-10.0360424334411));
#289946=CARTESIAN_POINT('Ctrl Pts',(-5.03864632176197,15.2,-10.0382752629434));
#289947=CARTESIAN_POINT('Ctrl Pts',(-5.04127778854207,15.2,-10.0405080924458));
#289948=CARTESIAN_POINT('Ctrl Pts',(-5.04391738720321,15.2,-10.0427424891898));
#289949=CARTESIAN_POINT('Ctrl Pts',(-5.04656510899407,15.2,-10.0449784097854));
#289950=CARTESIAN_POINT('Ctrl Pts',(-5.04921283078493,15.2,-10.0472143303809));
#289951=CARTESIAN_POINT('Ctrl Pts',(-5.05186867664898,15.2,-10.0494517752692));
#289952=CARTESIAN_POINT('Ctrl Pts',(-5.05453263548092,15.2,-10.0516906974896));
#289953=CARTESIAN_POINT('Ctrl Pts',(-5.05719659431285,15.2,-10.0539296197101));
#289954=CARTESIAN_POINT('Ctrl Pts',(-5.05986866842276,15.2,-10.0561700219872));
#289955=CARTESIAN_POINT('Ctrl Pts',(-5.06254884624133,15.2,-10.0584118585307));
#289956=CARTESIAN_POINT('Ctrl Pts',(-5.0652290240599,15.2,-10.0606536950741));
#289957=CARTESIAN_POINT('Ctrl Pts',(-5.06791730711127,15.2,-10.0628969650424));
#289958=CARTESIAN_POINT('Ctrl Pts',(-5.07061368588719,15.2,-10.065141627044));
#289959=CARTESIAN_POINT('Ctrl Pts',(-5.07331006515296,15.2,-10.0673862894534));
#289960=CARTESIAN_POINT('Ctrl Pts',(-5.07601454037935,15.2,-10.0696323414965));
#289961=CARTESIAN_POINT('Ctrl Pts',(-5.07872710256635,15.2,-10.0718797409899));
#289962=CARTESIAN_POINT('Ctrl Pts',(-5.08143966426057,15.2,-10.0741271400751));
#289963=CARTESIAN_POINT('Ctrl Pts',(-5.08416031248991,15.2,-10.0763758862712));
#289964=CARTESIAN_POINT('Ctrl Pts',(-5.08688903877802,15.2,-10.0786259364687));
#289965=CARTESIAN_POINT('Ctrl Pts',(-5.08961776506613,15.2,-10.0808759866661));
#289966=CARTESIAN_POINT('Ctrl Pts',(-5.09235456784836,15.2,-10.0831273396106));
#289967=CARTESIAN_POINT('Ctrl Pts',(-5.09509943904099,15.2,-10.0853799536956));
#289968=CARTESIAN_POINT('Ctrl Pts',(-5.09784431023363,15.2,-10.0876325677805));
#289969=CARTESIAN_POINT('Ctrl Pts',(-5.10059724988364,15.2,-10.0898864421486));
#289970=CARTESIAN_POINT('Ctrl Pts',(-5.103358248575,15.2,-10.092141533775));
#289971=CARTESIAN_POINT('Ctrl Pts',(-5.10611924726635,15.2,-10.0943966254014));
#289972=CARTESIAN_POINT('Ctrl Pts',(-5.10888830443237,15.2,-10.0966529346028));
#289973=CARTESIAN_POINT('Ctrl Pts',(-5.11166541120576,15.2,-10.098910418729));
#289974=CARTESIAN_POINT('Ctrl Pts',(-5.11444251797916,15.2,-10.1011679028552));
#289975=CARTESIAN_POINT('Ctrl Pts',(-5.11722767457701,15.2,-10.103426561673));
#289976=CARTESIAN_POINT('Ctrl Pts',(-5.12002087039109,15.2,-10.1056863532574));
#289977=CARTESIAN_POINT('Ctrl Pts',(-5.1228140667126,15.2,-10.1079461452523));
#289978=CARTESIAN_POINT('Ctrl Pts',(-5.12561530416972,15.2,-10.1102070689309));
#289979=CARTESIAN_POINT('Ctrl Pts',(-5.12842457187077,15.2,-10.1124690834681));
#289980=CARTESIAN_POINT('Ctrl Pts',(-5.13123383906146,15.2,-10.1147310975944));
#289981=CARTESIAN_POINT('Ctrl Pts',(-5.13405113574062,15.2,-10.1169942029238));
#289982=CARTESIAN_POINT('Ctrl Pts',(-5.13687645453005,15.2,-10.1192583557464));
#289983=CARTESIAN_POINT('Ctrl Pts',(-5.13970177331947,15.2,-10.121522508569));
#289984=CARTESIAN_POINT('Ctrl Pts',(-5.14253511241238,15.2,-10.1237877102459));
#289985=CARTESIAN_POINT('Ctrl Pts',(-5.14537646355984,15.2,-10.126053917997));
#289986=CARTESIAN_POINT('Ctrl Pts',(-5.14821781470731,15.2,-10.1283201257481));
#289987=CARTESIAN_POINT('Ctrl Pts',(-5.15106717675381,15.2,-10.1305873404991));
#289988=CARTESIAN_POINT('Ctrl Pts',(-5.15392454052499,15.2,-10.1328555202083));
#289989=CARTESIAN_POINT('Ctrl Pts',(-5.15678190429618,15.2,-10.1351236999176));
#289990=CARTESIAN_POINT('Ctrl Pts',(-5.1596472709087,15.2,-10.1373928453518));
#289991=CARTESIAN_POINT('Ctrl Pts',(-5.16252062867861,15.2,-10.1396629149776));
#289992=CARTESIAN_POINT('Ctrl Pts',(-5.16539398644852,15.2,-10.1419329846034));
#289993=CARTESIAN_POINT('Ctrl Pts',(-5.16827533613595,15.2,-10.1442039780296));
#289994=CARTESIAN_POINT('Ctrl Pts',(-5.1711646689244,15.2,-10.1464758548105));
#289995=CARTESIAN_POINT('Ctrl Pts',(-5.17405400171285,15.2,-10.1487477315913));
#289996=CARTESIAN_POINT('Ctrl Pts',(-5.17695131542331,15.2,-10.1510204920538));
#289997=CARTESIAN_POINT('Ctrl Pts',(-5.17985660256666,15.2,-10.1532940937627));
#289998=CARTESIAN_POINT('Ctrl Pts',(-5.18276189023779,15.2,-10.1555676958847));
#289999=CARTESIAN_POINT('Ctrl Pts',(-5.18567515039454,15.2,-10.1578421401986));
#290000=CARTESIAN_POINT('Ctrl Pts',(-5.1885963726535,15.2,-10.1601173872377));
#290001=CARTESIAN_POINT('Ctrl Pts',(-5.19151759438178,15.2,-10.1623926338635));
#290002=CARTESIAN_POINT('Ctrl Pts',(-5.19444677960963,15.2,-10.1646686821308));
#290003=CARTESIAN_POINT('Ctrl Pts',(-5.19738391737861,15.2,-10.1669454932565));
#290004=CARTESIAN_POINT('Ctrl Pts',(-5.20130010089273,15.2,-10.1699812412862));
#290005=CARTESIAN_POINT('Ctrl Pts',(-5.2052304224238,15.2,-10.1730183444697));
#290006=CARTESIAN_POINT('Ctrl Pts',(-5.20917485868605,15.2,-10.1760567053175));
#290007=CARTESIAN_POINT('Ctrl Pts',(-5.21213318601711,15.2,-10.1783354760568));
#290008=CARTESIAN_POINT('Ctrl Pts',(-5.21509945316077,15.2,-10.1806149527859));
#290009=CARTESIAN_POINT('Ctrl Pts',(-5.2180736488433,15.2,-10.1828950979946));
#290010=CARTESIAN_POINT('Ctrl Pts',(-5.22104784506614,15.2,-10.1851752436176));
#290011=CARTESIAN_POINT('Ctrl Pts',(-5.22402996951621,15.2,-10.1874560576324));
#290012=CARTESIAN_POINT('Ctrl Pts',(-5.22702001566017,15.2,-10.1897375037557));
#290013=CARTESIAN_POINT('Ctrl Pts',(-5.2310067429468,15.2,-10.1927794312294));
#290014=CARTESIAN_POINT('Ctrl Pts',(-5.2350075501205,15.2,-10.1958224850945));
#290015=CARTESIAN_POINT('Ctrl Pts',(-5.23902241218025,15.2,-10.1988665637345));
#290016=CARTESIAN_POINT('Ctrl Pts',(-5.24203355886183,15.2,-10.2011496228182));
#290017=CARTESIAN_POINT('Ctrl Pts',(-5.24505261109078,15.2,-10.2034332566604));
#290018=CARTESIAN_POINT('Ctrl Pts',(-5.24807955692278,15.2,-10.2057174180248));
#290019=CARTESIAN_POINT('Ctrl Pts',(-5.25110650275477,15.2,-10.2080015793892));
#290020=CARTESIAN_POINT('Ctrl Pts',(-5.25414134106499,15.2,-10.2102862675516));
#290021=CARTESIAN_POINT('Ctrl Pts',(-5.25718406582836,15.2,-10.2125714567185));
#290022=CARTESIAN_POINT('Ctrl Pts',(-5.26124103254804,15.2,-10.2156183758845));
#290023=CARTESIAN_POINT('Ctrl Pts',(-5.2653120248846,15.2,-10.218666183391));
#290024=CARTESIAN_POINT('Ctrl Pts',(-5.26939701852072,15.2,-10.2217148786423));
#290025=CARTESIAN_POINT('Origin',(-5.66257110645729E-14,15.2,-1.77635683940025E-14));
#290026=CARTESIAN_POINT('',(-4.04260911704029,15.2,-9.55499537042844));
#290027=CARTESIAN_POINT('',(-4.04260911704029,12.2,-9.55499537042844));
#290028=CARTESIAN_POINT('',(-4.04260911700006,15.2,-9.55499537000001));
#290029=CARTESIAN_POINT('Origin',(-5.66257110645729E-14,12.2,-1.77635683940025E-14));
#290030=CARTESIAN_POINT('Origin',(-5.66257110645729E-14,15.2,-1.77635683940025E-14));
#290031=CARTESIAN_POINT('Origin',(-5.66257110645729E-14,15.2,-1.77635683940025E-14));
#290032=CARTESIAN_POINT('',(-4.12144986800006,15.2,-10.736091047));
#290033=CARTESIAN_POINT('',(-3.76106045600006,15.2,-10.867585944));
#290034=CARTESIAN_POINT('Origin',(-5.66257110645729E-14,15.2,-1.77635683940025E-14));
#290035=CARTESIAN_POINT('',(-3.76106045600006,12.2,-10.867585944));
#290036=CARTESIAN_POINT('',(-3.76106045600006,15.2,-10.867585944));
#290037=CARTESIAN_POINT('',(-4.12144986800006,12.2,-10.736091047));
#290038=CARTESIAN_POINT('Origin',(-5.66257110645729E-14,12.2,-1.77635683940025E-14));
#290039=CARTESIAN_POINT('',(-4.12144986800006,15.2,-10.736091047));
#290040=CARTESIAN_POINT('Ctrl Pts',(-3.76106045600006,15.2,-10.867585944));
#290041=CARTESIAN_POINT('Ctrl Pts',(-3.76106045600006,11.6,-10.867585944));
#290042=CARTESIAN_POINT('Ctrl Pts',(-3.76051902400006,15.2,-10.867046091));
#290043=CARTESIAN_POINT('Ctrl Pts',(-3.76051902400006,11.6,-10.867046091));
#290044=CARTESIAN_POINT('Ctrl Pts',(-3.75943667400006,15.2,-10.865966493));
#290045=CARTESIAN_POINT('Ctrl Pts',(-3.75943667400006,11.6,-10.865966493));
#290046=CARTESIAN_POINT('Ctrl Pts',(-3.75781469800006,15.2,-10.864347421));
#290047=CARTESIAN_POINT('Ctrl Pts',(-3.75781469800006,11.6,-10.864347421));
#290048=CARTESIAN_POINT('Ctrl Pts',(-3.75565515700006,15.2,-10.862189303));
#290049=CARTESIAN_POINT('Ctrl Pts',(-3.75565515700006,11.6,-10.862189303));
#290050=CARTESIAN_POINT('Ctrl Pts',(-3.75296088400006,15.2,-10.85949273));
#290051=CARTESIAN_POINT('Ctrl Pts',(-3.75296088400006,11.6,-10.85949273));
#290052=CARTESIAN_POINT('Ctrl Pts',(-3.75027176800006,15.2,-10.856797236));
#290053=CARTESIAN_POINT('Ctrl Pts',(-3.75027176800006,11.6,-10.856797236));
#290054=CARTESIAN_POINT('Ctrl Pts',(-3.74758780900006,15.2,-10.854102821));
#290055=CARTESIAN_POINT('Ctrl Pts',(-3.74758780900006,11.6,-10.854102821));
#290056=CARTESIAN_POINT('Ctrl Pts',(-3.74490900600006,15.2,-10.851409491));
#290057=CARTESIAN_POINT('Ctrl Pts',(-3.74490900600006,11.6,-10.851409491));
#290058=CARTESIAN_POINT('Ctrl Pts',(-3.74223536200006,15.2,-10.848717249));
#290059=CARTESIAN_POINT('Ctrl Pts',(-3.74223536200006,11.6,-10.848717249));
#290060=CARTESIAN_POINT('Ctrl Pts',(-3.73956687400006,15.2,-10.846026106));
#290061=CARTESIAN_POINT('Ctrl Pts',(-3.73956687400006,11.6,-10.846026106));
#290062=CARTESIAN_POINT('Ctrl Pts',(-3.73690354800006,15.2,-10.843336071));
#290063=CARTESIAN_POINT('Ctrl Pts',(-3.73690354800006,11.6,-10.843336071));
#290064=CARTESIAN_POINT('Ctrl Pts',(-3.73424538200006,15.2,-10.840647153));
#290065=CARTESIAN_POINT('Ctrl Pts',(-3.73424538200006,11.6,-10.840647153));
#290066=CARTESIAN_POINT('Ctrl Pts',(-3.73159237800006,15.2,-10.837959365));
#290067=CARTESIAN_POINT('Ctrl Pts',(-3.73159237800006,11.6,-10.837959365));
#290068=CARTESIAN_POINT('Ctrl Pts',(-3.72894453900006,15.2,-10.835272718));
#290069=CARTESIAN_POINT('Ctrl Pts',(-3.72894453900006,11.6,-10.835272718));
#290070=CARTESIAN_POINT('Ctrl Pts',(-3.72630186200006,15.2,-10.832587221));
#290071=CARTESIAN_POINT('Ctrl Pts',(-3.72630186200006,11.6,-10.832587221));
#290072=CARTESIAN_POINT('Ctrl Pts',(-3.72366435200005,15.2,-10.829902884));
#290073=CARTESIAN_POINT('Ctrl Pts',(-3.72366435200005,11.6,-10.829902884));
#290074=CARTESIAN_POINT('Ctrl Pts',(-3.72103200800006,15.2,-10.827219715));
#290075=CARTESIAN_POINT('Ctrl Pts',(-3.72103200800006,11.6,-10.827219715));
#290076=CARTESIAN_POINT('Ctrl Pts',(-3.71840483000006,15.2,-10.824537725));
#290077=CARTESIAN_POINT('Ctrl Pts',(-3.71840483000006,11.6,-10.824537725));
#290078=CARTESIAN_POINT('Ctrl Pts',(-3.71578282100006,15.2,-10.821856919));
#290079=CARTESIAN_POINT('Ctrl Pts',(-3.71578282100006,11.6,-10.821856919));
#290080=CARTESIAN_POINT('Ctrl Pts',(-3.71316598200006,15.2,-10.819177306));
#290081=CARTESIAN_POINT('Ctrl Pts',(-3.71316598200006,11.6,-10.819177306));
#290082=CARTESIAN_POINT('Ctrl Pts',(-3.71055431200006,15.2,-10.816498895));
#290083=CARTESIAN_POINT('Ctrl Pts',(-3.71055431200006,11.6,-10.816498895));
#290084=CARTESIAN_POINT('Ctrl Pts',(-3.70794781300006,15.2,-10.813821694));
#290085=CARTESIAN_POINT('Ctrl Pts',(-3.70794781300006,11.6,-10.813821694));
#290086=CARTESIAN_POINT('Ctrl Pts',(-3.70534648600006,15.2,-10.811145713));
#290087=CARTESIAN_POINT('Ctrl Pts',(-3.70534648600006,11.6,-10.811145713));
#290088=CARTESIAN_POINT('Ctrl Pts',(-3.70275033200006,15.2,-10.808470962));
#290089=CARTESIAN_POINT('Ctrl Pts',(-3.70275033200006,11.6,-10.808470962));
#290090=CARTESIAN_POINT('Ctrl Pts',(-3.70015935100006,15.2,-10.805797449));
#290091=CARTESIAN_POINT('Ctrl Pts',(-3.70015935100006,11.6,-10.805797449));
#290092=CARTESIAN_POINT('Ctrl Pts',(-3.69757354500006,15.2,-10.803125185));
#290093=CARTESIAN_POINT('Ctrl Pts',(-3.69757354500006,11.6,-10.803125185));
#290094=CARTESIAN_POINT('Ctrl Pts',(-3.69499291500006,15.2,-10.800454178));
#290095=CARTESIAN_POINT('Ctrl Pts',(-3.69499291500006,11.6,-10.800454178));
#290096=CARTESIAN_POINT('Ctrl Pts',(-3.69241746100006,15.2,-10.797784438));
#290097=CARTESIAN_POINT('Ctrl Pts',(-3.69241746100006,11.6,-10.797784438));
#290098=CARTESIAN_POINT('Ctrl Pts',(-3.68984718500006,15.2,-10.795115973));
#290099=CARTESIAN_POINT('Ctrl Pts',(-3.68984718500006,11.6,-10.795115973));
#290100=CARTESIAN_POINT('Ctrl Pts',(-3.68728208700006,15.2,-10.792448794));
#290101=CARTESIAN_POINT('Ctrl Pts',(-3.68728208700006,11.6,-10.792448794));
#290102=CARTESIAN_POINT('Ctrl Pts',(-3.68472216800006,15.2,-10.789782909));
#290103=CARTESIAN_POINT('Ctrl Pts',(-3.68472216800006,11.6,-10.789782909));
#290104=CARTESIAN_POINT('Ctrl Pts',(-3.68216742900006,15.2,-10.787118327));
#290105=CARTESIAN_POINT('Ctrl Pts',(-3.68216742900006,11.6,-10.787118327));
#290106=CARTESIAN_POINT('Ctrl Pts',(-3.67961787200006,15.2,-10.784455056));
#290107=CARTESIAN_POINT('Ctrl Pts',(-3.67961787200006,11.6,-10.784455056));
#290108=CARTESIAN_POINT('Ctrl Pts',(-3.67707349600006,15.2,-10.781793107));
#290109=CARTESIAN_POINT('Ctrl Pts',(-3.67707349600006,11.6,-10.781793107));
#290110=CARTESIAN_POINT('Ctrl Pts',(-3.67453430300006,15.2,-10.779132489));
#290111=CARTESIAN_POINT('Ctrl Pts',(-3.67453430300006,11.6,-10.779132489));
#290112=CARTESIAN_POINT('Ctrl Pts',(-3.67200029300006,15.2,-10.776473212));
#290113=CARTESIAN_POINT('Ctrl Pts',(-3.67200029300006,11.6,-10.776473212));
#290114=CARTESIAN_POINT('Ctrl Pts',(-3.66947146800006,15.2,-10.773815283));
#290115=CARTESIAN_POINT('Ctrl Pts',(-3.66947146800006,11.6,-10.773815283));
#290116=CARTESIAN_POINT('Ctrl Pts',(-3.66694782800006,15.2,-10.771158713));
#290117=CARTESIAN_POINT('Ctrl Pts',(-3.66694782800006,11.6,-10.771158713));
#290118=CARTESIAN_POINT('Ctrl Pts',(-3.66442937500006,15.2,-10.768503511));
#290119=CARTESIAN_POINT('Ctrl Pts',(-3.66442937500006,11.6,-10.768503511));
#290120=CARTESIAN_POINT('Ctrl Pts',(-3.66191610700006,15.2,-10.765849687));
#290121=CARTESIAN_POINT('Ctrl Pts',(-3.66191610700006,11.6,-10.765849687));
#290122=CARTESIAN_POINT('Ctrl Pts',(-3.65940802900006,15.2,-10.76319725));
#290123=CARTESIAN_POINT('Ctrl Pts',(-3.65940802900006,11.6,-10.76319725));
#290124=CARTESIAN_POINT('Ctrl Pts',(-3.65690513800006,15.2,-10.760546209));
#290125=CARTESIAN_POINT('Ctrl Pts',(-3.65690513800006,11.6,-10.760546209));
#290126=CARTESIAN_POINT('Ctrl Pts',(-3.65440743700006,15.2,-10.757896573));
#290127=CARTESIAN_POINT('Ctrl Pts',(-3.65440743700006,11.6,-10.757896573));
#290128=CARTESIAN_POINT('Ctrl Pts',(-3.65191492700006,15.2,-10.755248352));
#290129=CARTESIAN_POINT('Ctrl Pts',(-3.65191492700006,11.6,-10.755248352));
#290130=CARTESIAN_POINT('Ctrl Pts',(-3.64942760700006,15.2,-10.752601556));
#290131=CARTESIAN_POINT('Ctrl Pts',(-3.64942760700006,11.6,-10.752601556));
#290132=CARTESIAN_POINT('Ctrl Pts',(-3.64694547900006,15.2,-10.749956194));
#290133=CARTESIAN_POINT('Ctrl Pts',(-3.64694547900006,11.6,-10.749956194));
#290134=CARTESIAN_POINT('Ctrl Pts',(-3.64446854400006,15.2,-10.747312274));
#290135=CARTESIAN_POINT('Ctrl Pts',(-3.64446854400006,11.6,-10.747312274));
#290136=CARTESIAN_POINT('Ctrl Pts',(-3.64199680200006,15.2,-10.744669809));
#290137=CARTESIAN_POINT('Ctrl Pts',(-3.64199680200006,11.6,-10.744669809));
#290138=CARTESIAN_POINT('Ctrl Pts',(-3.63953025500006,15.2,-10.742028805));
#290139=CARTESIAN_POINT('Ctrl Pts',(-3.63953025500006,11.6,-10.742028805));
#290140=CARTESIAN_POINT('Ctrl Pts',(-3.63706890200006,15.2,-10.739389272));
#290141=CARTESIAN_POINT('Ctrl Pts',(-3.63706890200006,11.6,-10.739389272));
#290142=CARTESIAN_POINT('Ctrl Pts',(-3.63461274600006,15.2,-10.736751221));
#290143=CARTESIAN_POINT('Ctrl Pts',(-3.63461274600006,11.6,-10.736751221));
#290144=CARTESIAN_POINT('Ctrl Pts',(-3.63216178500006,15.2,-10.734114661));
#290145=CARTESIAN_POINT('Ctrl Pts',(-3.63216178500006,11.6,-10.734114661));
#290146=CARTESIAN_POINT('Ctrl Pts',(-3.62971602300005,15.2,-10.731479603));
#290147=CARTESIAN_POINT('Ctrl Pts',(-3.62971602300005,11.6,-10.731479603));
#290148=CARTESIAN_POINT('Ctrl Pts',(-3.62727545800006,15.2,-10.728846054));
#290149=CARTESIAN_POINT('Ctrl Pts',(-3.62727545800006,11.6,-10.728846054));
#290150=CARTESIAN_POINT('Ctrl Pts',(-3.62484009100006,15.2,-10.726214024));
#290151=CARTESIAN_POINT('Ctrl Pts',(-3.62484009100006,11.6,-10.726214024));
#290152=CARTESIAN_POINT('Ctrl Pts',(-3.62240992500006,15.2,-10.723583524));
#290153=CARTESIAN_POINT('Ctrl Pts',(-3.62240992500006,11.6,-10.723583524));
#290154=CARTESIAN_POINT('Ctrl Pts',(-3.61998495800006,15.2,-10.720954563));
#290155=CARTESIAN_POINT('Ctrl Pts',(-3.61998495800006,11.6,-10.720954563));
#290156=CARTESIAN_POINT('Ctrl Pts',(-3.61756519300005,15.2,-10.71832715));
#290157=CARTESIAN_POINT('Ctrl Pts',(-3.61756519300005,11.6,-10.71832715));
#290158=CARTESIAN_POINT('Ctrl Pts',(-3.61515062900006,15.2,-10.715701296));
#290159=CARTESIAN_POINT('Ctrl Pts',(-3.61515062900006,11.6,-10.715701296));
#290160=CARTESIAN_POINT('Ctrl Pts',(-3.61274126800006,15.2,-10.713077011));
#290161=CARTESIAN_POINT('Ctrl Pts',(-3.61274126800006,11.6,-10.713077011));
#290162=CARTESIAN_POINT('Ctrl Pts',(-3.61033711000006,15.2,-10.710454301));
#290163=CARTESIAN_POINT('Ctrl Pts',(-3.61033711000006,11.6,-10.710454301));
#290164=CARTESIAN_POINT('Ctrl Pts',(-3.60793815500006,15.2,-10.707833181));
#290165=CARTESIAN_POINT('Ctrl Pts',(-3.60793815500006,11.6,-10.707833181));
#290166=CARTESIAN_POINT('Ctrl Pts',(-3.60554440400006,15.2,-10.705213657));
#290167=CARTESIAN_POINT('Ctrl Pts',(-3.60554440400006,11.6,-10.705213657));
#290168=CARTESIAN_POINT('Ctrl Pts',(-3.60315586000006,15.2,-10.70259574));
#290169=CARTESIAN_POINT('Ctrl Pts',(-3.60315586000006,11.6,-10.70259574));
#290170=CARTESIAN_POINT('Ctrl Pts',(-3.60077252100006,15.2,-10.699979441));
#290171=CARTESIAN_POINT('Ctrl Pts',(-3.60077252100006,11.6,-10.699979441));
#290172=CARTESIAN_POINT('Ctrl Pts',(-3.59839438800006,15.2,-10.697364767));
#290173=CARTESIAN_POINT('Ctrl Pts',(-3.59839438800006,11.6,-10.697364767));
#290174=CARTESIAN_POINT('Ctrl Pts',(-3.59602146300006,15.2,-10.69475173));
#290175=CARTESIAN_POINT('Ctrl Pts',(-3.59602146300006,11.6,-10.69475173));
#290176=CARTESIAN_POINT('Ctrl Pts',(-3.59365374500006,15.2,-10.692140339));
#290177=CARTESIAN_POINT('Ctrl Pts',(-3.59365374500006,11.6,-10.692140339));
#290178=CARTESIAN_POINT('Ctrl Pts',(-3.59129123600006,15.2,-10.689530605));
#290179=CARTESIAN_POINT('Ctrl Pts',(-3.59129123600006,11.6,-10.689530605));
#290180=CARTESIAN_POINT('Ctrl Pts',(-3.58893393500006,15.2,-10.686922536));
#290181=CARTESIAN_POINT('Ctrl Pts',(-3.58893393500006,11.6,-10.686922536));
#290182=CARTESIAN_POINT('Ctrl Pts',(-3.58658184600006,15.2,-10.684316144));
#290183=CARTESIAN_POINT('Ctrl Pts',(-3.58658184600006,11.6,-10.684316144));
#290184=CARTESIAN_POINT('Ctrl Pts',(-3.58423496600006,15.2,-10.681711437));
#290185=CARTESIAN_POINT('Ctrl Pts',(-3.58423496600006,11.6,-10.681711437));
#290186=CARTESIAN_POINT('Ctrl Pts',(-3.58189329600005,15.2,-10.679108426));
#290187=CARTESIAN_POINT('Ctrl Pts',(-3.58189329600005,11.6,-10.679108426));
#290188=CARTESIAN_POINT('Ctrl Pts',(-3.57955683800006,15.2,-10.67650712));
#290189=CARTESIAN_POINT('Ctrl Pts',(-3.57955683800006,11.6,-10.67650712));
#290190=CARTESIAN_POINT('Ctrl Pts',(-3.57722559400006,15.2,-10.67390753));
#290191=CARTESIAN_POINT('Ctrl Pts',(-3.57722559400006,11.6,-10.67390753));
#290192=CARTESIAN_POINT('Ctrl Pts',(-3.57489956100006,15.2,-10.671309667));
#290193=CARTESIAN_POINT('Ctrl Pts',(-3.57489956100006,11.6,-10.671309667));
#290194=CARTESIAN_POINT('Ctrl Pts',(-3.57257874200006,15.2,-10.668713538));
#290195=CARTESIAN_POINT('Ctrl Pts',(-3.57257874200006,11.6,-10.668713538));
#290196=CARTESIAN_POINT('Ctrl Pts',(-3.57026313700006,15.2,-10.666119155));
#290197=CARTESIAN_POINT('Ctrl Pts',(-3.57026313700006,11.6,-10.666119155));
#290198=CARTESIAN_POINT('Ctrl Pts',(-3.56795274700006,15.2,-10.663526528));
#290199=CARTESIAN_POINT('Ctrl Pts',(-3.56795274700006,11.6,-10.663526528));
#290200=CARTESIAN_POINT('Ctrl Pts',(-3.56564757100006,15.2,-10.660935667));
#290201=CARTESIAN_POINT('Ctrl Pts',(-3.56564757100006,11.6,-10.660935667));
#290202=CARTESIAN_POINT('Ctrl Pts',(-3.56334761200006,15.2,-10.658346582));
#290203=CARTESIAN_POINT('Ctrl Pts',(-3.56334761200006,11.6,-10.658346582));
#290204=CARTESIAN_POINT('Ctrl Pts',(-3.56105286900006,15.2,-10.655759283));
#290205=CARTESIAN_POINT('Ctrl Pts',(-3.56105286900006,11.6,-10.655759283));
#290206=CARTESIAN_POINT('Ctrl Pts',(-3.55876334100006,15.2,-10.65317378));
#290207=CARTESIAN_POINT('Ctrl Pts',(-3.55876334100006,11.6,-10.65317378));
#290208=CARTESIAN_POINT('Ctrl Pts',(-3.55647903300006,15.2,-10.650590083));
#290209=CARTESIAN_POINT('Ctrl Pts',(-3.55647903300006,11.6,-10.650590083));
#290210=CARTESIAN_POINT('Ctrl Pts',(-3.55419994100005,15.2,-10.648008202));
#290211=CARTESIAN_POINT('Ctrl Pts',(-3.55419994100005,11.6,-10.648008202));
#290212=CARTESIAN_POINT('Ctrl Pts',(-3.55192606900006,15.2,-10.645428149));
#290213=CARTESIAN_POINT('Ctrl Pts',(-3.55192606900006,11.6,-10.645428149));
#290214=CARTESIAN_POINT('Ctrl Pts',(-3.54965741500005,15.2,-10.642849932));
#290215=CARTESIAN_POINT('Ctrl Pts',(-3.54965741500005,11.6,-10.642849932));
#290216=CARTESIAN_POINT('Ctrl Pts',(-3.54739398000006,15.2,-10.640273563));
#290217=CARTESIAN_POINT('Ctrl Pts',(-3.54739398000006,11.6,-10.640273563));
#290218=CARTESIAN_POINT('Ctrl Pts',(-3.54513576600006,15.2,-10.63769905));
#290219=CARTESIAN_POINT('Ctrl Pts',(-3.54513576600006,11.6,-10.63769905));
#290220=CARTESIAN_POINT('Ctrl Pts',(-3.54288277300006,15.2,-10.635126405));
#290221=CARTESIAN_POINT('Ctrl Pts',(-3.54288277300006,11.6,-10.635126405));
#290222=CARTESIAN_POINT('Ctrl Pts',(-3.54063499900006,15.2,-10.632555638));
#290223=CARTESIAN_POINT('Ctrl Pts',(-3.54063499900006,11.6,-10.632555638));
#290224=CARTESIAN_POINT('Ctrl Pts',(-3.53839244700006,15.2,-10.62998676));
#290225=CARTESIAN_POINT('Ctrl Pts',(-3.53839244700006,11.6,-10.62998676));
#290226=CARTESIAN_POINT('Ctrl Pts',(-3.53615511800006,15.2,-10.627419779));
#290227=CARTESIAN_POINT('Ctrl Pts',(-3.53615511800006,11.6,-10.627419779));
#290228=CARTESIAN_POINT('Ctrl Pts',(-3.53392301000006,15.2,-10.624854708));
#290229=CARTESIAN_POINT('Ctrl Pts',(-3.53392301000006,11.6,-10.624854708));
#290230=CARTESIAN_POINT('Ctrl Pts',(-3.53169612600006,15.2,-10.622291556));
#290231=CARTESIAN_POINT('Ctrl Pts',(-3.53169612600006,11.6,-10.622291556));
#290232=CARTESIAN_POINT('Ctrl Pts',(-3.52947446500006,15.2,-10.619730333));
#290233=CARTESIAN_POINT('Ctrl Pts',(-3.52947446500006,11.6,-10.619730333));
#290234=CARTESIAN_POINT('Ctrl Pts',(-3.52725802800006,15.2,-10.617171052));
#290235=CARTESIAN_POINT('Ctrl Pts',(-3.52725802800006,11.6,-10.617171052));
#290236=CARTESIAN_POINT('Ctrl Pts',(-3.52504681500006,15.2,-10.614613719));
#290237=CARTESIAN_POINT('Ctrl Pts',(-3.52504681500006,11.6,-10.614613719));
#290238=CARTESIAN_POINT('Ctrl Pts',(-3.52284082700006,15.2,-10.612058348));
#290239=CARTESIAN_POINT('Ctrl Pts',(-3.52284082700006,11.6,-10.612058348));
#290240=CARTESIAN_POINT('Ctrl Pts',(-3.52064006300006,15.2,-10.609504949));
#290241=CARTESIAN_POINT('Ctrl Pts',(-3.52064006300006,11.6,-10.609504949));
#290242=CARTESIAN_POINT('Ctrl Pts',(-3.51844452500006,15.2,-10.606953531));
#290243=CARTESIAN_POINT('Ctrl Pts',(-3.51844452500006,11.6,-10.606953531));
#290244=CARTESIAN_POINT('Ctrl Pts',(-3.51625421300006,15.2,-10.604404105));
#290245=CARTESIAN_POINT('Ctrl Pts',(-3.51625421300006,11.6,-10.604404105));
#290246=CARTESIAN_POINT('Ctrl Pts',(-3.51406912700006,15.2,-10.601856682));
#290247=CARTESIAN_POINT('Ctrl Pts',(-3.51406912700006,11.6,-10.601856682));
#290248=CARTESIAN_POINT('Ctrl Pts',(-3.51188926800006,15.2,-10.599311274));
#290249=CARTESIAN_POINT('Ctrl Pts',(-3.51188926800006,11.6,-10.599311274));
#290250=CARTESIAN_POINT('Ctrl Pts',(-3.50971463700006,15.2,-10.596767888));
#290251=CARTESIAN_POINT('Ctrl Pts',(-3.50971463700006,11.6,-10.596767888));
#290252=CARTESIAN_POINT('Ctrl Pts',(-3.50754523300006,15.2,-10.594226538));
#290253=CARTESIAN_POINT('Ctrl Pts',(-3.50754523300006,11.6,-10.594226538));
#290254=CARTESIAN_POINT('Ctrl Pts',(-3.50538105600006,15.2,-10.591687232));
#290255=CARTESIAN_POINT('Ctrl Pts',(-3.50538105600006,11.6,-10.591687232));
#290256=CARTESIAN_POINT('Ctrl Pts',(-3.50322210700006,15.2,-10.589149983));
#290257=CARTESIAN_POINT('Ctrl Pts',(-3.50322210700006,11.6,-10.589149983));
#290258=CARTESIAN_POINT('Ctrl Pts',(-3.50106838800006,15.2,-10.586614801));
#290259=CARTESIAN_POINT('Ctrl Pts',(-3.50106838800006,11.6,-10.586614801));
#290260=CARTESIAN_POINT('Ctrl Pts',(-3.49891989700006,15.2,-10.584081695));
#290261=CARTESIAN_POINT('Ctrl Pts',(-3.49891989700006,11.6,-10.584081695));
#290262=CARTESIAN_POINT('Ctrl Pts',(-3.49677663600006,15.2,-10.581550677));
#290263=CARTESIAN_POINT('Ctrl Pts',(-3.49677663600006,11.6,-10.581550677));
#290264=CARTESIAN_POINT('Ctrl Pts',(-3.49463860300005,15.2,-10.579021757));
#290265=CARTESIAN_POINT('Ctrl Pts',(-3.49463860300005,11.6,-10.579021757));
#290266=CARTESIAN_POINT('Ctrl Pts',(-3.49250580100006,15.2,-10.576494948));
#290267=CARTESIAN_POINT('Ctrl Pts',(-3.49250580100006,11.6,-10.576494948));
#290268=CARTESIAN_POINT('Ctrl Pts',(-3.49037822900006,15.2,-10.573970258));
#290269=CARTESIAN_POINT('Ctrl Pts',(-3.49037822900006,11.6,-10.573970258));
#290270=CARTESIAN_POINT('Ctrl Pts',(-3.48825588700006,15.2,-10.571447699));
#290271=CARTESIAN_POINT('Ctrl Pts',(-3.48825588700006,11.6,-10.571447699));
#290272=CARTESIAN_POINT('Ctrl Pts',(-3.48613877700005,15.2,-10.568927282));
#290273=CARTESIAN_POINT('Ctrl Pts',(-3.48613877700005,11.6,-10.568927282));
#290274=CARTESIAN_POINT('Ctrl Pts',(-3.48402689800006,15.2,-10.566409018));
#290275=CARTESIAN_POINT('Ctrl Pts',(-3.48402689800006,11.6,-10.566409018));
#290276=CARTESIAN_POINT('Ctrl Pts',(-3.48192025100006,15.2,-10.563892917));
#290277=CARTESIAN_POINT('Ctrl Pts',(-3.48192025100006,11.6,-10.563892917));
#290278=CARTESIAN_POINT('Ctrl Pts',(-3.47981883400006,15.2,-10.56137899));
#290279=CARTESIAN_POINT('Ctrl Pts',(-3.47981883400006,11.6,-10.56137899));
#290280=CARTESIAN_POINT('Ctrl Pts',(-3.47772265000006,15.2,-10.558867249));
#290281=CARTESIAN_POINT('Ctrl Pts',(-3.47772265000006,11.6,-10.558867249));
#290282=CARTESIAN_POINT('Ctrl Pts',(-3.47563169800006,15.2,-10.556357703));
#290283=CARTESIAN_POINT('Ctrl Pts',(-3.47563169800006,11.6,-10.556357703));
#290284=CARTESIAN_POINT('Ctrl Pts',(-3.47354597800006,15.2,-10.553850365));
#290285=CARTESIAN_POINT('Ctrl Pts',(-3.47354597800006,11.6,-10.553850365));
#290286=CARTESIAN_POINT('Ctrl Pts',(-3.47146549200006,15.2,-10.551345245));
#290287=CARTESIAN_POINT('Ctrl Pts',(-3.47146549200006,11.6,-10.551345245));
#290288=CARTESIAN_POINT('Ctrl Pts',(-3.46939023800005,15.2,-10.548842353));
#290289=CARTESIAN_POINT('Ctrl Pts',(-3.46939023800005,11.6,-10.548842353));
#290290=CARTESIAN_POINT('Ctrl Pts',(-3.46732021800006,15.2,-10.546341702));
#290291=CARTESIAN_POINT('Ctrl Pts',(-3.46732021800006,11.6,-10.546341702));
#290292=CARTESIAN_POINT('Ctrl Pts',(-3.46525543000006,15.2,-10.543843302));
#290293=CARTESIAN_POINT('Ctrl Pts',(-3.46525543000006,11.6,-10.543843302));
#290294=CARTESIAN_POINT('Ctrl Pts',(-3.46319587600005,15.2,-10.541347163));
#290295=CARTESIAN_POINT('Ctrl Pts',(-3.46319587600005,11.6,-10.541347163));
#290296=CARTESIAN_POINT('Ctrl Pts',(-3.46114155700006,15.2,-10.538853298));
#290297=CARTESIAN_POINT('Ctrl Pts',(-3.46114155700006,11.6,-10.538853298));
#290298=CARTESIAN_POINT('Ctrl Pts',(-3.45909247200006,15.2,-10.536361717));
#290299=CARTESIAN_POINT('Ctrl Pts',(-3.45909247200006,11.6,-10.536361717));
#290300=CARTESIAN_POINT('Ctrl Pts',(-3.45704862000006,15.2,-10.533872432));
#290301=CARTESIAN_POINT('Ctrl Pts',(-3.45704862000006,11.6,-10.533872432));
#290302=CARTESIAN_POINT('Ctrl Pts',(-3.45501000300006,15.2,-10.531385453));
#290303=CARTESIAN_POINT('Ctrl Pts',(-3.45501000300006,11.6,-10.531385453));
#290304=CARTESIAN_POINT('Ctrl Pts',(-3.45297662200006,15.2,-10.528900792));
#290305=CARTESIAN_POINT('Ctrl Pts',(-3.45297662200006,11.6,-10.528900792));
#290306=CARTESIAN_POINT('Ctrl Pts',(-3.45094847400006,15.2,-10.52641846));
#290307=CARTESIAN_POINT('Ctrl Pts',(-3.45094847400006,11.6,-10.52641846));
#290308=CARTESIAN_POINT('Ctrl Pts',(-3.44892556100006,15.2,-10.523938468));
#290309=CARTESIAN_POINT('Ctrl Pts',(-3.44892556100006,11.6,-10.523938468));
#290310=CARTESIAN_POINT('Ctrl Pts',(-3.44690788300006,15.2,-10.521460828));
#290311=CARTESIAN_POINT('Ctrl Pts',(-3.44690788300006,11.6,-10.521460828));
#290312=CARTESIAN_POINT('Ctrl Pts',(-3.44489544100006,15.2,-10.518985549));
#290313=CARTESIAN_POINT('Ctrl Pts',(-3.44489544100006,11.6,-10.518985549));
#290314=CARTESIAN_POINT('Ctrl Pts',(-3.44288823300006,15.2,-10.516512646));
#290315=CARTESIAN_POINT('Ctrl Pts',(-3.44288823300006,11.6,-10.516512646));
#290316=CARTESIAN_POINT('Ctrl Pts',(-3.44088626200006,15.2,-10.514042127));
#290317=CARTESIAN_POINT('Ctrl Pts',(-3.44088626200006,11.6,-10.514042127));
#290318=CARTESIAN_POINT('Ctrl Pts',(-3.43888952500006,15.2,-10.511574004));
#290319=CARTESIAN_POINT('Ctrl Pts',(-3.43888952500006,11.6,-10.511574004));
#290320=CARTESIAN_POINT('Ctrl Pts',(-3.43689802500006,15.2,-10.50910829));
#290321=CARTESIAN_POINT('Ctrl Pts',(-3.43689802500006,11.6,-10.50910829));
#290322=CARTESIAN_POINT('Ctrl Pts',(-3.43491176000006,15.2,-10.506644995));
#290323=CARTESIAN_POINT('Ctrl Pts',(-3.43491176000006,11.6,-10.506644995));
#290324=CARTESIAN_POINT('Ctrl Pts',(-3.43293073100006,15.2,-10.504184131));
#290325=CARTESIAN_POINT('Ctrl Pts',(-3.43293073100006,11.6,-10.504184131));
#290326=CARTESIAN_POINT('Ctrl Pts',(-3.43095493700006,15.2,-10.501725709));
#290327=CARTESIAN_POINT('Ctrl Pts',(-3.43095493700006,11.6,-10.501725709));
#290328=CARTESIAN_POINT('Ctrl Pts',(-3.42898438100006,15.2,-10.49926974));
#290329=CARTESIAN_POINT('Ctrl Pts',(-3.42898438100006,11.6,-10.49926974));
#290330=CARTESIAN_POINT('Ctrl Pts',(-3.42701905900006,15.2,-10.496816237));
#290331=CARTESIAN_POINT('Ctrl Pts',(-3.42701905900006,11.6,-10.496816237));
#290332=CARTESIAN_POINT('Ctrl Pts',(-3.42505897400006,15.2,-10.49436521));
#290333=CARTESIAN_POINT('Ctrl Pts',(-3.42505897400006,11.6,-10.49436521));
#290334=CARTESIAN_POINT('Ctrl Pts',(-3.42310412600006,15.2,-10.491916672));
#290335=CARTESIAN_POINT('Ctrl Pts',(-3.42310412600006,11.6,-10.491916672));
#290336=CARTESIAN_POINT('Ctrl Pts',(-3.42115451300006,15.2,-10.489470633));
#290337=CARTESIAN_POINT('Ctrl Pts',(-3.42115451300006,11.6,-10.489470633));
#290338=CARTESIAN_POINT('Ctrl Pts',(-3.41921013600006,15.2,-10.487027105));
#290339=CARTESIAN_POINT('Ctrl Pts',(-3.41921013600006,11.6,-10.487027105));
#290340=CARTESIAN_POINT('Ctrl Pts',(-3.41727099700006,15.2,-10.484586099));
#290341=CARTESIAN_POINT('Ctrl Pts',(-3.41727099700006,11.6,-10.484586099));
#290342=CARTESIAN_POINT('Ctrl Pts',(-3.41533709200006,15.2,-10.482147629));
#290343=CARTESIAN_POINT('Ctrl Pts',(-3.41533709200006,11.6,-10.482147629));
#290344=CARTESIAN_POINT('Ctrl Pts',(-3.41340842400006,15.2,-10.479711705));
#290345=CARTESIAN_POINT('Ctrl Pts',(-3.41340842400006,11.6,-10.479711705));
#290346=CARTESIAN_POINT('Ctrl Pts',(-3.41148499200005,15.2,-10.477278338));
#290347=CARTESIAN_POINT('Ctrl Pts',(-3.41148499200005,11.6,-10.477278338));
#290348=CARTESIAN_POINT('Ctrl Pts',(-3.40956679600006,15.2,-10.474847542));
#290349=CARTESIAN_POINT('Ctrl Pts',(-3.40956679600006,11.6,-10.474847542));
#290350=CARTESIAN_POINT('Ctrl Pts',(-3.40765383700006,15.2,-10.472419327));
#290351=CARTESIAN_POINT('Ctrl Pts',(-3.40765383700006,11.6,-10.472419327));
#290352=CARTESIAN_POINT('Ctrl Pts',(-3.40574611300006,15.2,-10.469993704));
#290353=CARTESIAN_POINT('Ctrl Pts',(-3.40574611300006,11.6,-10.469993704));
#290354=CARTESIAN_POINT('Ctrl Pts',(-3.40384362600005,15.2,-10.467570686));
#290355=CARTESIAN_POINT('Ctrl Pts',(-3.40384362600005,11.6,-10.467570686));
#290356=CARTESIAN_POINT('Ctrl Pts',(-3.40194637500006,15.2,-10.465150285));
#290357=CARTESIAN_POINT('Ctrl Pts',(-3.40194637500006,11.6,-10.465150285));
#290358=CARTESIAN_POINT('Ctrl Pts',(-3.40005435900005,15.2,-10.462732513));
#290359=CARTESIAN_POINT('Ctrl Pts',(-3.40005435900005,11.6,-10.462732513));
#290360=CARTESIAN_POINT('Ctrl Pts',(-3.39816757900006,15.2,-10.46031738));
#290361=CARTESIAN_POINT('Ctrl Pts',(-3.39816757900006,11.6,-10.46031738));
#290362=CARTESIAN_POINT('Ctrl Pts',(-3.39628603500006,15.2,-10.457904901));
#290363=CARTESIAN_POINT('Ctrl Pts',(-3.39628603500006,11.6,-10.457904901));
#290364=CARTESIAN_POINT('Ctrl Pts',(-3.39440972600006,15.2,-10.455495085));
#290365=CARTESIAN_POINT('Ctrl Pts',(-3.39440972600006,11.6,-10.455495085));
#290366=CARTESIAN_POINT('Ctrl Pts',(-3.39253865400006,15.2,-10.453087944));
#290367=CARTESIAN_POINT('Ctrl Pts',(-3.39253865400006,11.6,-10.453087944));
#290368=CARTESIAN_POINT('Ctrl Pts',(-3.39067281600005,15.2,-10.450683493));
#290369=CARTESIAN_POINT('Ctrl Pts',(-3.39067281600005,11.6,-10.450683493));
#290370=CARTESIAN_POINT('Ctrl Pts',(-3.38881221500006,15.2,-10.448281741));
#290371=CARTESIAN_POINT('Ctrl Pts',(-3.38881221500006,11.6,-10.448281741));
#290372=CARTESIAN_POINT('Ctrl Pts',(-3.38695684800005,15.2,-10.4458827));
#290373=CARTESIAN_POINT('Ctrl Pts',(-3.38695684800005,11.6,-10.4458827));
#290374=CARTESIAN_POINT('Ctrl Pts',(-3.38510671600006,15.2,-10.443486385));
#290375=CARTESIAN_POINT('Ctrl Pts',(-3.38510671600006,11.6,-10.443486385));
#290376=CARTESIAN_POINT('Ctrl Pts',(-3.38326181900006,15.2,-10.441092805));
#290377=CARTESIAN_POINT('Ctrl Pts',(-3.38326181900006,11.6,-10.441092805));
#290378=CARTESIAN_POINT('Ctrl Pts',(-3.38142215600006,15.2,-10.438701973));
#290379=CARTESIAN_POINT('Ctrl Pts',(-3.38142215600006,11.6,-10.438701973));
#290380=CARTESIAN_POINT('Ctrl Pts',(-3.37958772900006,15.2,-10.436313902));
#290381=CARTESIAN_POINT('Ctrl Pts',(-3.37958772900006,11.6,-10.436313902));
#290382=CARTESIAN_POINT('Ctrl Pts',(-3.37775853500006,15.2,-10.433928604));
#290383=CARTESIAN_POINT('Ctrl Pts',(-3.37775853500006,11.6,-10.433928604));
#290384=CARTESIAN_POINT('Ctrl Pts',(-3.37593457600006,15.2,-10.43154609));
#290385=CARTESIAN_POINT('Ctrl Pts',(-3.37593457600006,11.6,-10.43154609));
#290386=CARTESIAN_POINT('Ctrl Pts',(-3.37411585100006,15.2,-10.429166373));
#290387=CARTESIAN_POINT('Ctrl Pts',(-3.37411585100006,11.6,-10.429166373));
#290388=CARTESIAN_POINT('Ctrl Pts',(-3.37230235900006,15.2,-10.426789465));
#290389=CARTESIAN_POINT('Ctrl Pts',(-3.37230235900006,11.6,-10.426789465));
#290390=CARTESIAN_POINT('Ctrl Pts',(-3.37049410100006,15.2,-10.424415378));
#290391=CARTESIAN_POINT('Ctrl Pts',(-3.37049410100006,11.6,-10.424415378));
#290392=CARTESIAN_POINT('Ctrl Pts',(-3.36869107700006,15.2,-10.422044126));
#290393=CARTESIAN_POINT('Ctrl Pts',(-3.36869107700006,11.6,-10.422044126));
#290394=CARTESIAN_POINT('Ctrl Pts',(-3.36689328500006,15.2,-10.419675719));
#290395=CARTESIAN_POINT('Ctrl Pts',(-3.36689328500006,11.6,-10.419675719));
#290396=CARTESIAN_POINT('Ctrl Pts',(-3.36510072600006,15.2,-10.41731017));
#290397=CARTESIAN_POINT('Ctrl Pts',(-3.36510072600006,11.6,-10.41731017));
#290398=CARTESIAN_POINT('Ctrl Pts',(-3.36331340000006,15.2,-10.414947492));
#290399=CARTESIAN_POINT('Ctrl Pts',(-3.36331340000006,11.6,-10.414947492));
#290400=CARTESIAN_POINT('Ctrl Pts',(-3.36153130500006,15.2,-10.412587698));
#290401=CARTESIAN_POINT('Ctrl Pts',(-3.36153130500006,11.6,-10.412587698));
#290402=CARTESIAN_POINT('Ctrl Pts',(-3.35975444300006,15.2,-10.410230799));
#290403=CARTESIAN_POINT('Ctrl Pts',(-3.35975444300006,11.6,-10.410230799));
#290404=CARTESIAN_POINT('Ctrl Pts',(-3.35798281300006,15.2,-10.407876808));
#290405=CARTESIAN_POINT('Ctrl Pts',(-3.35798281300006,11.6,-10.407876808));
#290406=CARTESIAN_POINT('Ctrl Pts',(-3.35621641500006,15.2,-10.405525737));
#290407=CARTESIAN_POINT('Ctrl Pts',(-3.35621641500006,11.6,-10.405525737));
#290408=CARTESIAN_POINT('Ctrl Pts',(-3.35445524700006,15.2,-10.403177599));
#290409=CARTESIAN_POINT('Ctrl Pts',(-3.35445524700006,11.6,-10.403177599));
#290410=CARTESIAN_POINT('Ctrl Pts',(-3.35269931000005,15.2,-10.400832408));
#290411=CARTESIAN_POINT('Ctrl Pts',(-3.35269931000005,11.6,-10.400832408));
#290412=CARTESIAN_POINT('Ctrl Pts',(-3.35094860200006,15.2,-10.398490174));
#290413=CARTESIAN_POINT('Ctrl Pts',(-3.35094860200006,11.6,-10.398490174));
#290414=CARTESIAN_POINT('Ctrl Pts',(-3.34920312700006,15.2,-10.39615091));
#290415=CARTESIAN_POINT('Ctrl Pts',(-3.34920312700006,11.6,-10.39615091));
#290416=CARTESIAN_POINT('Ctrl Pts',(-3.34746288000006,15.2,-10.393814631));
#290417=CARTESIAN_POINT('Ctrl Pts',(-3.34746288000006,11.6,-10.393814631));
#290418=CARTESIAN_POINT('Ctrl Pts',(-3.34572786200006,15.2,-10.391481347));
#290419=CARTESIAN_POINT('Ctrl Pts',(-3.34572786200006,11.6,-10.391481347));
#290420=CARTESIAN_POINT('Ctrl Pts',(-3.34399807300006,15.2,-10.389151072));
#290421=CARTESIAN_POINT('Ctrl Pts',(-3.34399807300006,11.6,-10.389151072));
#290422=CARTESIAN_POINT('Ctrl Pts',(-3.34227351400005,15.2,-10.386823819));
#290423=CARTESIAN_POINT('Ctrl Pts',(-3.34227351400005,11.6,-10.386823819));
#290424=CARTESIAN_POINT('Ctrl Pts',(-3.34055418200006,15.2,-10.384499599));
#290425=CARTESIAN_POINT('Ctrl Pts',(-3.34055418200006,11.6,-10.384499599));
#290426=CARTESIAN_POINT('Ctrl Pts',(-3.33884007800005,15.2,-10.382178426));
#290427=CARTESIAN_POINT('Ctrl Pts',(-3.33884007800005,11.6,-10.382178426));
#290428=CARTESIAN_POINT('Ctrl Pts',(-3.33713120200006,15.2,-10.379860314));
#290429=CARTESIAN_POINT('Ctrl Pts',(-3.33713120200006,11.6,-10.379860314));
#290430=CARTESIAN_POINT('Ctrl Pts',(-3.33542755300006,15.2,-10.377545273));
#290431=CARTESIAN_POINT('Ctrl Pts',(-3.33542755300006,11.6,-10.377545273));
#290432=CARTESIAN_POINT('Ctrl Pts',(-3.33372912900006,15.2,-10.375233318));
#290433=CARTESIAN_POINT('Ctrl Pts',(-3.33372912900006,11.6,-10.375233318));
#290434=CARTESIAN_POINT('Ctrl Pts',(-3.33203593200006,15.2,-10.372924463));
#290435=CARTESIAN_POINT('Ctrl Pts',(-3.33203593200006,11.6,-10.372924463));
#290436=CARTESIAN_POINT('Ctrl Pts',(-3.33034796100006,15.2,-10.370618717));
#290437=CARTESIAN_POINT('Ctrl Pts',(-3.33034796100006,11.6,-10.370618717));
#290438=CARTESIAN_POINT('Ctrl Pts',(-3.32866521500006,15.2,-10.368316097));
#290439=CARTESIAN_POINT('Ctrl Pts',(-3.32866521500006,11.6,-10.368316097));
#290440=CARTESIAN_POINT('Ctrl Pts',(-3.32698769400006,15.2,-10.366016613));
#290441=CARTESIAN_POINT('Ctrl Pts',(-3.32698769400006,11.6,-10.366016613));
#290442=CARTESIAN_POINT('Ctrl Pts',(-3.32531539700006,15.2,-10.36372028));
#290443=CARTESIAN_POINT('Ctrl Pts',(-3.32531539700006,11.6,-10.36372028));
#290444=CARTESIAN_POINT('Ctrl Pts',(-3.32364832400006,15.2,-10.36142711));
#290445=CARTESIAN_POINT('Ctrl Pts',(-3.32364832400006,11.6,-10.36142711));
#290446=CARTESIAN_POINT('Ctrl Pts',(-3.32198647300006,15.2,-10.359137116));
#290447=CARTESIAN_POINT('Ctrl Pts',(-3.32198647300006,11.6,-10.359137116));
#290448=CARTESIAN_POINT('Ctrl Pts',(-3.32032984600006,15.2,-10.356850314));
#290449=CARTESIAN_POINT('Ctrl Pts',(-3.32032984600006,11.6,-10.356850314));
#290450=CARTESIAN_POINT('Ctrl Pts',(-3.31867844000006,15.2,-10.354566711));
#290451=CARTESIAN_POINT('Ctrl Pts',(-3.31867844000006,11.6,-10.354566711));
#290452=CARTESIAN_POINT('Ctrl Pts',(-3.31703225600006,15.2,-10.352286326));
#290453=CARTESIAN_POINT('Ctrl Pts',(-3.31703225600006,11.6,-10.352286326));
#290454=CARTESIAN_POINT('Ctrl Pts',(-3.31539129200006,15.2,-10.35000917));
#290455=CARTESIAN_POINT('Ctrl Pts',(-3.31539129200006,11.6,-10.35000917));
#290456=CARTESIAN_POINT('Ctrl Pts',(-3.31375555000006,15.2,-10.347735256));
#290457=CARTESIAN_POINT('Ctrl Pts',(-3.31375555000006,11.6,-10.347735256));
#290458=CARTESIAN_POINT('Ctrl Pts',(-3.31212502800006,15.2,-10.345464598));
#290459=CARTESIAN_POINT('Ctrl Pts',(-3.31212502800006,11.6,-10.345464598));
#290460=CARTESIAN_POINT('Ctrl Pts',(-3.31049972400006,15.2,-10.343197208));
#290461=CARTESIAN_POINT('Ctrl Pts',(-3.31049972400006,11.6,-10.343197208));
#290462=CARTESIAN_POINT('Ctrl Pts',(-3.30887963900006,15.2,-10.340933101));
#290463=CARTESIAN_POINT('Ctrl Pts',(-3.30887963900006,11.6,-10.340933101));
#290464=CARTESIAN_POINT('Ctrl Pts',(-3.30726477200006,15.2,-10.338672289));
#290465=CARTESIAN_POINT('Ctrl Pts',(-3.30726477200006,11.6,-10.338672289));
#290466=CARTESIAN_POINT('Ctrl Pts',(-3.30565512200006,15.2,-10.336414787));
#290467=CARTESIAN_POINT('Ctrl Pts',(-3.30565512200006,11.6,-10.336414787));
#290468=CARTESIAN_POINT('Ctrl Pts',(-3.30405069000005,15.2,-10.334160607));
#290469=CARTESIAN_POINT('Ctrl Pts',(-3.30405069000005,11.6,-10.334160607));
#290470=CARTESIAN_POINT('Ctrl Pts',(-3.30245147400006,15.2,-10.331909762));
#290471=CARTESIAN_POINT('Ctrl Pts',(-3.30245147400006,11.6,-10.331909762));
#290472=CARTESIAN_POINT('Ctrl Pts',(-3.30085747200005,15.2,-10.329662267));
#290473=CARTESIAN_POINT('Ctrl Pts',(-3.30085747200005,11.6,-10.329662267));
#290474=CARTESIAN_POINT('Ctrl Pts',(-3.29926868600006,15.2,-10.327418135));
#290475=CARTESIAN_POINT('Ctrl Pts',(-3.29926868600006,11.6,-10.327418135));
#290476=CARTESIAN_POINT('Ctrl Pts',(-3.29768511500005,15.2,-10.32517738));
#290477=CARTESIAN_POINT('Ctrl Pts',(-3.29768511500005,11.6,-10.32517738));
#290478=CARTESIAN_POINT('Ctrl Pts',(-3.29610675600006,15.2,-10.322940015));
#290479=CARTESIAN_POINT('Ctrl Pts',(-3.29610675600006,11.6,-10.322940015));
#290480=CARTESIAN_POINT('Ctrl Pts',(-3.29453360900006,15.2,-10.320706053));
#290481=CARTESIAN_POINT('Ctrl Pts',(-3.29453360900006,11.6,-10.320706053));
#290482=CARTESIAN_POINT('Ctrl Pts',(-3.29296567600006,15.2,-10.318475508));
#290483=CARTESIAN_POINT('Ctrl Pts',(-3.29296567600006,11.6,-10.318475508));
#290484=CARTESIAN_POINT('Ctrl Pts',(-3.29140295200005,15.2,-10.316248395));
#290485=CARTESIAN_POINT('Ctrl Pts',(-3.29140295200005,11.6,-10.316248395));
#290486=CARTESIAN_POINT('Ctrl Pts',(-3.28984544000006,15.2,-10.314024727));
#290487=CARTESIAN_POINT('Ctrl Pts',(-3.28984544000006,11.6,-10.314024727));
#290488=CARTESIAN_POINT('Ctrl Pts',(-3.28829313800005,15.2,-10.311804517));
#290489=CARTESIAN_POINT('Ctrl Pts',(-3.28829313800005,11.6,-10.311804517));
#290490=CARTESIAN_POINT('Ctrl Pts',(-3.28674604500006,15.2,-10.309587781));
#290491=CARTESIAN_POINT('Ctrl Pts',(-3.28674604500006,11.6,-10.309587781));
#290492=CARTESIAN_POINT('Ctrl Pts',(-3.28520415900006,15.2,-10.307374529));
#290493=CARTESIAN_POINT('Ctrl Pts',(-3.28520415900006,11.6,-10.307374529));
#290494=CARTESIAN_POINT('Ctrl Pts',(-3.28366748200006,15.2,-10.305164778));
#290495=CARTESIAN_POINT('Ctrl Pts',(-3.28366748200006,11.6,-10.305164778));
#290496=CARTESIAN_POINT('Ctrl Pts',(-3.28213601000006,15.2,-10.302958542));
#290497=CARTESIAN_POINT('Ctrl Pts',(-3.28213601000006,11.6,-10.302958542));
#290498=CARTESIAN_POINT('Ctrl Pts',(-3.28060974500006,15.2,-10.300755833));
#290499=CARTESIAN_POINT('Ctrl Pts',(-3.28060974500006,11.6,-10.300755833));
#290500=CARTESIAN_POINT('Ctrl Pts',(-3.27908868500006,15.2,-10.298556667));
#290501=CARTESIAN_POINT('Ctrl Pts',(-3.27908868500006,11.6,-10.298556667));
#290502=CARTESIAN_POINT('Ctrl Pts',(-3.27757282800006,15.2,-10.296361056));
#290503=CARTESIAN_POINT('Ctrl Pts',(-3.27757282800006,11.6,-10.296361056));
#290504=CARTESIAN_POINT('Ctrl Pts',(-3.27606217500006,15.2,-10.294169016));
#290505=CARTESIAN_POINT('Ctrl Pts',(-3.27606217500006,11.6,-10.294169016));
#290506=CARTESIAN_POINT('Ctrl Pts',(-3.27455672400006,15.2,-10.291980559));
#290507=CARTESIAN_POINT('Ctrl Pts',(-3.27455672400006,11.6,-10.291980559));
#290508=CARTESIAN_POINT('Ctrl Pts',(-3.27305647500005,15.2,-10.289795701));
#290509=CARTESIAN_POINT('Ctrl Pts',(-3.27305647500005,11.6,-10.289795701));
#290510=CARTESIAN_POINT('Ctrl Pts',(-3.27156142600006,15.2,-10.287614455));
#290511=CARTESIAN_POINT('Ctrl Pts',(-3.27156142600006,11.6,-10.287614455));
#290512=CARTESIAN_POINT('Ctrl Pts',(-3.27007157800006,15.2,-10.285436836));
#290513=CARTESIAN_POINT('Ctrl Pts',(-3.27007157800006,11.6,-10.285436836));
#290514=CARTESIAN_POINT('Ctrl Pts',(-3.26858692800006,15.2,-10.283262857));
#290515=CARTESIAN_POINT('Ctrl Pts',(-3.26858692800006,11.6,-10.283262857));
#290516=CARTESIAN_POINT('Ctrl Pts',(-3.26710747700006,15.2,-10.281092534));
#290517=CARTESIAN_POINT('Ctrl Pts',(-3.26710747700006,11.6,-10.281092534));
#290518=CARTESIAN_POINT('Ctrl Pts',(-3.26563322100006,15.2,-10.27892588));
#290519=CARTESIAN_POINT('Ctrl Pts',(-3.26563322100006,11.6,-10.27892588));
#290520=CARTESIAN_POINT('Ctrl Pts',(-3.26416416300006,15.2,-10.27676291));
#290521=CARTESIAN_POINT('Ctrl Pts',(-3.26416416300006,11.6,-10.27676291));
#290522=CARTESIAN_POINT('Ctrl Pts',(-3.26270029800006,15.2,-10.274603638));
#290523=CARTESIAN_POINT('Ctrl Pts',(-3.26270029800006,11.6,-10.274603638));
#290524=CARTESIAN_POINT('Ctrl Pts',(-3.26124162800005,15.2,-10.272448079));
#290525=CARTESIAN_POINT('Ctrl Pts',(-3.26124162800005,11.6,-10.272448079));
#290526=CARTESIAN_POINT('Ctrl Pts',(-3.25978815100005,15.2,-10.270296247));
#290527=CARTESIAN_POINT('Ctrl Pts',(-3.25978815100005,11.6,-10.270296247));
#290528=CARTESIAN_POINT('Ctrl Pts',(-3.25833986600006,15.2,-10.268148155));
#290529=CARTESIAN_POINT('Ctrl Pts',(-3.25833986600006,11.6,-10.268148155));
#290530=CARTESIAN_POINT('Ctrl Pts',(-3.25689677300006,15.2,-10.266003821));
#290531=CARTESIAN_POINT('Ctrl Pts',(-3.25689677300006,11.6,-10.266003821));
#290532=CARTESIAN_POINT('Ctrl Pts',(-3.25545886800006,15.2,-10.263863257));
#290533=CARTESIAN_POINT('Ctrl Pts',(-3.25545886800006,11.6,-10.263863257));
#290534=CARTESIAN_POINT('Ctrl Pts',(-3.25402615400006,15.2,-10.261726477));
#290535=CARTESIAN_POINT('Ctrl Pts',(-3.25402615400006,11.6,-10.261726477));
#290536=CARTESIAN_POINT('Ctrl Pts',(-3.25259862700006,15.2,-10.259593499));
#290537=CARTESIAN_POINT('Ctrl Pts',(-3.25259862700006,11.6,-10.259593499));
#290538=CARTESIAN_POINT('Ctrl Pts',(-3.25117628700006,15.2,-10.257464333));
#290539=CARTESIAN_POINT('Ctrl Pts',(-3.25117628700006,11.6,-10.257464333));
#290540=CARTESIAN_POINT('Ctrl Pts',(-3.24975913200006,15.2,-10.255338999));
#290541=CARTESIAN_POINT('Ctrl Pts',(-3.24975913200006,11.6,-10.255338999));
#290542=CARTESIAN_POINT('Ctrl Pts',(-3.24834716300006,15.2,-10.253217507));
#290543=CARTESIAN_POINT('Ctrl Pts',(-3.24834716300006,11.6,-10.253217507));
#290544=CARTESIAN_POINT('Ctrl Pts',(-3.24694037600006,15.2,-10.251099874));
#290545=CARTESIAN_POINT('Ctrl Pts',(-3.24694037600006,11.6,-10.251099874));
#290546=CARTESIAN_POINT('Ctrl Pts',(-3.24553877200006,15.2,-10.248986116));
#290547=CARTESIAN_POINT('Ctrl Pts',(-3.24553877200006,11.6,-10.248986116));
#290548=CARTESIAN_POINT('Ctrl Pts',(-3.24414235000006,15.2,-10.246876246));
#290549=CARTESIAN_POINT('Ctrl Pts',(-3.24414235000006,11.6,-10.246876246));
#290550=CARTESIAN_POINT('Ctrl Pts',(-3.24275110800006,15.2,-10.244770278));
#290551=CARTESIAN_POINT('Ctrl Pts',(-3.24275110800006,11.6,-10.244770278));
#290552=CARTESIAN_POINT('Ctrl Pts',(-3.24136504400005,15.2,-10.24266823));
#290553=CARTESIAN_POINT('Ctrl Pts',(-3.24136504400005,11.6,-10.24266823));
#290554=CARTESIAN_POINT('Ctrl Pts',(-3.23998415800005,15.2,-10.240570114));
#290555=CARTESIAN_POINT('Ctrl Pts',(-3.23998415800005,11.6,-10.240570114));
#290556=CARTESIAN_POINT('Ctrl Pts',(-3.23860844900006,15.2,-10.238475947));
#290557=CARTESIAN_POINT('Ctrl Pts',(-3.23860844900006,11.6,-10.238475947));
#290558=CARTESIAN_POINT('Ctrl Pts',(-3.23723791500006,15.2,-10.236385744));
#290559=CARTESIAN_POINT('Ctrl Pts',(-3.23723791500006,11.6,-10.236385744));
#290560=CARTESIAN_POINT('Ctrl Pts',(-3.23587255600006,15.2,-10.23429952));
#290561=CARTESIAN_POINT('Ctrl Pts',(-3.23587255600006,11.6,-10.23429952));
#290562=CARTESIAN_POINT('Ctrl Pts',(-3.23451236800006,15.2,-10.232217289));
#290563=CARTESIAN_POINT('Ctrl Pts',(-3.23451236800006,11.6,-10.232217289));
#290564=CARTESIAN_POINT('Ctrl Pts',(-3.23315735400006,15.2,-10.230139067));
#290565=CARTESIAN_POINT('Ctrl Pts',(-3.23315735400006,11.6,-10.230139067));
#290566=CARTESIAN_POINT('Ctrl Pts',(-3.23180750800006,15.2,-10.228064869));
#290567=CARTESIAN_POINT('Ctrl Pts',(-3.23180750800006,11.6,-10.228064869));
#290568=CARTESIAN_POINT('Ctrl Pts',(-3.23046283300005,15.2,-10.225994712));
#290569=CARTESIAN_POINT('Ctrl Pts',(-3.23046283300005,11.6,-10.225994712));
#290570=CARTESIAN_POINT('Ctrl Pts',(-3.22912332500006,15.2,-10.223928608));
#290571=CARTESIAN_POINT('Ctrl Pts',(-3.22912332500006,11.6,-10.223928608));
#290572=CARTESIAN_POINT('Ctrl Pts',(-3.22778898300006,15.2,-10.221866575));
#290573=CARTESIAN_POINT('Ctrl Pts',(-3.22778898300006,11.6,-10.221866575));
#290574=CARTESIAN_POINT('Ctrl Pts',(-3.22645980800006,15.2,-10.219808628));
#290575=CARTESIAN_POINT('Ctrl Pts',(-3.22645980800006,11.6,-10.219808628));
#290576=CARTESIAN_POINT('Ctrl Pts',(-3.22513579500006,15.2,-10.217754781));
#290577=CARTESIAN_POINT('Ctrl Pts',(-3.22513579500006,11.6,-10.217754781));
#290578=CARTESIAN_POINT('Ctrl Pts',(-3.22381694500006,15.2,-10.215705052));
#290579=CARTESIAN_POINT('Ctrl Pts',(-3.22381694500006,11.6,-10.215705052));
#290580=CARTESIAN_POINT('Ctrl Pts',(-3.22250325700006,15.2,-10.213659454));
#290581=CARTESIAN_POINT('Ctrl Pts',(-3.22250325700006,11.6,-10.213659454));
#290582=CARTESIAN_POINT('Ctrl Pts',(-3.22119472800006,15.2,-10.211618003));
#290583=CARTESIAN_POINT('Ctrl Pts',(-3.22119472800006,11.6,-10.211618003));
#290584=CARTESIAN_POINT('Ctrl Pts',(-3.21989135700006,15.2,-10.209580717));
#290585=CARTESIAN_POINT('Ctrl Pts',(-3.21989135700006,11.6,-10.209580717));
#290586=CARTESIAN_POINT('Ctrl Pts',(-3.21859314300006,15.2,-10.207547609));
#290587=CARTESIAN_POINT('Ctrl Pts',(-3.21859314300006,11.6,-10.207547609));
#290588=CARTESIAN_POINT('Ctrl Pts',(-3.21730008400006,15.2,-10.205518696));
#290589=CARTESIAN_POINT('Ctrl Pts',(-3.21730008400006,11.6,-10.205518696));
#290590=CARTESIAN_POINT('Ctrl Pts',(-3.21601218000006,15.2,-10.203493994));
#290591=CARTESIAN_POINT('Ctrl Pts',(-3.21601218000006,11.6,-10.203493994));
#290592=CARTESIAN_POINT('Ctrl Pts',(-3.21472942800006,15.2,-10.201473517));
#290593=CARTESIAN_POINT('Ctrl Pts',(-3.21472942800006,11.6,-10.201473517));
#290594=CARTESIAN_POINT('Ctrl Pts',(-3.21345182800005,15.2,-10.199457283));
#290595=CARTESIAN_POINT('Ctrl Pts',(-3.21345182800005,11.6,-10.199457283));
#290596=CARTESIAN_POINT('Ctrl Pts',(-3.21217937800006,15.2,-10.197445307));
#290597=CARTESIAN_POINT('Ctrl Pts',(-3.21217937800006,11.6,-10.197445307));
#290598=CARTESIAN_POINT('Ctrl Pts',(-3.21091207400006,15.2,-10.195437604));
#290599=CARTESIAN_POINT('Ctrl Pts',(-3.21091207400006,11.6,-10.195437604));
#290600=CARTESIAN_POINT('Ctrl Pts',(-3.20964991900006,15.2,-10.193434192));
#290601=CARTESIAN_POINT('Ctrl Pts',(-3.20964991900006,11.6,-10.193434192));
#290602=CARTESIAN_POINT('Ctrl Pts',(-3.20839290700006,15.2,-10.191435085));
#290603=CARTESIAN_POINT('Ctrl Pts',(-3.20839290700006,11.6,-10.191435085));
#290604=CARTESIAN_POINT('Ctrl Pts',(-3.20714104000006,15.2,-10.189440301));
#290605=CARTESIAN_POINT('Ctrl Pts',(-3.20714104000006,11.6,-10.189440301));
#290606=CARTESIAN_POINT('Ctrl Pts',(-3.20589431500005,15.2,-10.187449854));
#290607=CARTESIAN_POINT('Ctrl Pts',(-3.20589431500005,11.6,-10.187449854));
#290608=CARTESIAN_POINT('Ctrl Pts',(-3.20465273000006,15.2,-10.185463762));
#290609=CARTESIAN_POINT('Ctrl Pts',(-3.20465273000006,11.6,-10.185463762));
#290610=CARTESIAN_POINT('Ctrl Pts',(-3.20341628400006,15.2,-10.18348204));
#290611=CARTESIAN_POINT('Ctrl Pts',(-3.20341628400006,11.6,-10.18348204));
#290612=CARTESIAN_POINT('Ctrl Pts',(-3.20218497500006,15.2,-10.181504705));
#290613=CARTESIAN_POINT('Ctrl Pts',(-3.20218497500006,11.6,-10.181504705));
#290614=CARTESIAN_POINT('Ctrl Pts',(-3.20095880100005,15.2,-10.179531773));
#290615=CARTESIAN_POINT('Ctrl Pts',(-3.20095880100005,11.6,-10.179531773));
#290616=CARTESIAN_POINT('Ctrl Pts',(-3.19973776200006,15.2,-10.17756326));
#290617=CARTESIAN_POINT('Ctrl Pts',(-3.19973776200006,11.6,-10.17756326));
#290618=CARTESIAN_POINT('Ctrl Pts',(-3.19852185400006,15.2,-10.175599183));
#290619=CARTESIAN_POINT('Ctrl Pts',(-3.19852185400006,11.6,-10.175599183));
#290620=CARTESIAN_POINT('Ctrl Pts',(-3.19731107800005,15.2,-10.173639558));
#290621=CARTESIAN_POINT('Ctrl Pts',(-3.19731107800005,11.6,-10.173639558));
#290622=CARTESIAN_POINT('Ctrl Pts',(-3.19610543000006,15.2,-10.171684403));
#290623=CARTESIAN_POINT('Ctrl Pts',(-3.19610543000006,11.6,-10.171684403));
#290624=CARTESIAN_POINT('Ctrl Pts',(-3.19490490900006,15.2,-10.169733732));
#290625=CARTESIAN_POINT('Ctrl Pts',(-3.19490490900006,11.6,-10.169733732));
#290626=CARTESIAN_POINT('Ctrl Pts',(-3.19370951400006,15.2,-10.167787564));
#290627=CARTESIAN_POINT('Ctrl Pts',(-3.19370951400006,11.6,-10.167787564));
#290628=CARTESIAN_POINT('Ctrl Pts',(-3.19251924200006,15.2,-10.165845913));
#290629=CARTESIAN_POINT('Ctrl Pts',(-3.19251924200006,11.6,-10.165845913));
#290630=CARTESIAN_POINT('Ctrl Pts',(-3.19133409400005,15.2,-10.163908798));
#290631=CARTESIAN_POINT('Ctrl Pts',(-3.19133409400005,11.6,-10.163908798));
#290632=CARTESIAN_POINT('Ctrl Pts',(-3.19015406500006,15.2,-10.161976234));
#290633=CARTESIAN_POINT('Ctrl Pts',(-3.19015406500006,11.6,-10.161976234));
#290634=CARTESIAN_POINT('Ctrl Pts',(-3.18897915400006,15.2,-10.16004824));
#290635=CARTESIAN_POINT('Ctrl Pts',(-3.18897915400006,11.6,-10.16004824));
#290636=CARTESIAN_POINT('Ctrl Pts',(-3.18780936000006,15.2,-10.15812483));
#290637=CARTESIAN_POINT('Ctrl Pts',(-3.18780936000006,11.6,-10.15812483));
#290638=CARTESIAN_POINT('Ctrl Pts',(-3.18664468100006,15.2,-10.156206023));
#290639=CARTESIAN_POINT('Ctrl Pts',(-3.18664468100006,11.6,-10.156206023));
#290640=CARTESIAN_POINT('Ctrl Pts',(-3.18548511400006,15.2,-10.154291835));
#290641=CARTESIAN_POINT('Ctrl Pts',(-3.18548511400006,11.6,-10.154291835));
#290642=CARTESIAN_POINT('Ctrl Pts',(-3.18433065900006,15.2,-10.152382284));
#290643=CARTESIAN_POINT('Ctrl Pts',(-3.18433065900006,11.6,-10.152382284));
#290644=CARTESIAN_POINT('Ctrl Pts',(-3.18318131200006,15.2,-10.150477386));
#290645=CARTESIAN_POINT('Ctrl Pts',(-3.18318131200006,11.6,-10.150477386));
#290646=CARTESIAN_POINT('Ctrl Pts',(-3.18203707300006,15.2,-10.148577159));
#290647=CARTESIAN_POINT('Ctrl Pts',(-3.18203707300006,11.6,-10.148577159));
#290648=CARTESIAN_POINT('Ctrl Pts',(-3.18089794000006,15.2,-10.146681619));
#290649=CARTESIAN_POINT('Ctrl Pts',(-3.18089794000006,11.6,-10.146681619));
#290650=CARTESIAN_POINT('Ctrl Pts',(-3.17976391000005,15.2,-10.144790784));
#290651=CARTESIAN_POINT('Ctrl Pts',(-3.17976391000005,11.6,-10.144790784));
#290652=CARTESIAN_POINT('Ctrl Pts',(-3.17863498200006,15.2,-10.14290467));
#290653=CARTESIAN_POINT('Ctrl Pts',(-3.17863498200006,11.6,-10.14290467));
#290654=CARTESIAN_POINT('Ctrl Pts',(-3.17751115300006,15.2,-10.141023296));
#290655=CARTESIAN_POINT('Ctrl Pts',(-3.17751115300006,11.6,-10.141023296));
#290656=CARTESIAN_POINT('Ctrl Pts',(-3.17639242200006,15.2,-10.139146679));
#290657=CARTESIAN_POINT('Ctrl Pts',(-3.17639242200006,11.6,-10.139146679));
#290658=CARTESIAN_POINT('Ctrl Pts',(-3.17527878700006,15.2,-10.137274836));
#290659=CARTESIAN_POINT('Ctrl Pts',(-3.17527878700006,11.6,-10.137274836));
#290660=CARTESIAN_POINT('Ctrl Pts',(-3.17417024500006,15.2,-10.135407784));
#290661=CARTESIAN_POINT('Ctrl Pts',(-3.17417024500006,11.6,-10.135407784));
#290662=CARTESIAN_POINT('Ctrl Pts',(-3.17306679400006,15.2,-10.133545541));
#290663=CARTESIAN_POINT('Ctrl Pts',(-3.17306679400006,11.6,-10.133545541));
#290664=CARTESIAN_POINT('Ctrl Pts',(-3.17196843400006,15.2,-10.131688125));
#290665=CARTESIAN_POINT('Ctrl Pts',(-3.17196843400006,11.6,-10.131688125));
#290666=CARTESIAN_POINT('Ctrl Pts',(-3.17087516000006,15.2,-10.129835552));
#290667=CARTESIAN_POINT('Ctrl Pts',(-3.17087516000006,11.6,-10.129835552));
#290668=CARTESIAN_POINT('Ctrl Pts',(-3.16978697200006,15.2,-10.127987842));
#290669=CARTESIAN_POINT('Ctrl Pts',(-3.16978697200006,11.6,-10.127987842));
#290670=CARTESIAN_POINT('Ctrl Pts',(-3.16870386700006,15.2,-10.126145011));
#290671=CARTESIAN_POINT('Ctrl Pts',(-3.16870386700006,11.6,-10.126145011));
#290672=CARTESIAN_POINT('Ctrl Pts',(-3.16762584300006,15.2,-10.124307078));
#290673=CARTESIAN_POINT('Ctrl Pts',(-3.16762584300006,11.6,-10.124307078));
#290674=CARTESIAN_POINT('Ctrl Pts',(-3.16655289900006,15.2,-10.12247406));
#290675=CARTESIAN_POINT('Ctrl Pts',(-3.16655289900006,11.6,-10.12247406));
#290676=CARTESIAN_POINT('Ctrl Pts',(-3.16548503100006,15.2,-10.120645974));
#290677=CARTESIAN_POINT('Ctrl Pts',(-3.16548503100006,11.6,-10.120645974));
#290678=CARTESIAN_POINT('Ctrl Pts',(-3.16442223700005,15.2,-10.11882284));
#290679=CARTESIAN_POINT('Ctrl Pts',(-3.16442223700005,11.6,-10.11882284));
#290680=CARTESIAN_POINT('Ctrl Pts',(-3.16336451700006,15.2,-10.117004674));
#290681=CARTESIAN_POINT('Ctrl Pts',(-3.16336451700006,11.6,-10.117004674));
#290682=CARTESIAN_POINT('Ctrl Pts',(-3.16231186600006,15.2,-10.115191495));
#290683=CARTESIAN_POINT('Ctrl Pts',(-3.16231186600006,11.6,-10.115191495));
#290684=CARTESIAN_POINT('Ctrl Pts',(-3.16126428300006,15.2,-10.113383323));
#290685=CARTESIAN_POINT('Ctrl Pts',(-3.16126428300006,11.6,-10.113383323));
#290686=CARTESIAN_POINT('Ctrl Pts',(-3.16022176700006,15.2,-10.111580173));
#290687=CARTESIAN_POINT('Ctrl Pts',(-3.16022176700006,11.6,-10.111580173));
#290688=CARTESIAN_POINT('Ctrl Pts',(-3.15918431400006,15.2,-10.109782065));
#290689=CARTESIAN_POINT('Ctrl Pts',(-3.15918431400006,11.6,-10.109782065));
#290690=CARTESIAN_POINT('Ctrl Pts',(-3.15815192200006,15.2,-10.107989016));
#290691=CARTESIAN_POINT('Ctrl Pts',(-3.15815192200006,11.6,-10.107989016));
#290692=CARTESIAN_POINT('Ctrl Pts',(-3.15712458900005,15.2,-10.106201046));
#290693=CARTESIAN_POINT('Ctrl Pts',(-3.15712458900005,11.6,-10.106201046));
#290694=CARTESIAN_POINT('Ctrl Pts',(-3.15610231200006,15.2,-10.104418172));
#290695=CARTESIAN_POINT('Ctrl Pts',(-3.15610231200006,11.6,-10.104418172));
#290696=CARTESIAN_POINT('Ctrl Pts',(-3.15508508900006,15.2,-10.102640413));
#290697=CARTESIAN_POINT('Ctrl Pts',(-3.15508508900006,11.6,-10.102640413));
#290698=CARTESIAN_POINT('Ctrl Pts',(-3.15407291900006,15.2,-10.100867788));
#290699=CARTESIAN_POINT('Ctrl Pts',(-3.15407291900006,11.6,-10.100867788));
#290700=CARTESIAN_POINT('Ctrl Pts',(-3.15306579800006,15.2,-10.099100315));
#290701=CARTESIAN_POINT('Ctrl Pts',(-3.15306579800006,11.6,-10.099100315));
#290702=CARTESIAN_POINT('Ctrl Pts',(-3.15206372300006,15.2,-10.097338012));
#290703=CARTESIAN_POINT('Ctrl Pts',(-3.15206372300006,11.6,-10.097338012));
#290704=CARTESIAN_POINT('Ctrl Pts',(-3.15106669400006,15.2,-10.0955809));
#290705=CARTESIAN_POINT('Ctrl Pts',(-3.15106669400006,11.6,-10.0955809));
#290706=CARTESIAN_POINT('Ctrl Pts',(-3.15007470600006,15.2,-10.093828995));
#290707=CARTESIAN_POINT('Ctrl Pts',(-3.15007470600006,11.6,-10.093828995));
#290708=CARTESIAN_POINT('Ctrl Pts',(-3.14908775900005,15.2,-10.092082318));
#290709=CARTESIAN_POINT('Ctrl Pts',(-3.14908775900005,11.6,-10.092082318));
#290710=CARTESIAN_POINT('Ctrl Pts',(-3.14810584800005,15.2,-10.090340886));
#290711=CARTESIAN_POINT('Ctrl Pts',(-3.14810584800005,11.6,-10.090340886));
#290712=CARTESIAN_POINT('Ctrl Pts',(-3.14712897200006,15.2,-10.088604719));
#290713=CARTESIAN_POINT('Ctrl Pts',(-3.14712897200006,11.6,-10.088604719));
#290714=CARTESIAN_POINT('Ctrl Pts',(-3.14615712900005,15.2,-10.086873836));
#290715=CARTESIAN_POINT('Ctrl Pts',(-3.14615712900005,11.6,-10.086873836));
#290716=CARTESIAN_POINT('Ctrl Pts',(-3.14519031500006,15.2,-10.085148257));
#290717=CARTESIAN_POINT('Ctrl Pts',(-3.14519031500006,11.6,-10.085148257));
#290718=CARTESIAN_POINT('Ctrl Pts',(-3.14422852800006,15.2,-10.083427999));
#290719=CARTESIAN_POINT('Ctrl Pts',(-3.14422852800006,11.6,-10.083427999));
#290720=CARTESIAN_POINT('Ctrl Pts',(-3.14327176600006,15.2,-10.081713082));
#290721=CARTESIAN_POINT('Ctrl Pts',(-3.14327176600006,11.6,-10.081713082));
#290722=CARTESIAN_POINT('Ctrl Pts',(-3.14232002500006,15.2,-10.080003527));
#290723=CARTESIAN_POINT('Ctrl Pts',(-3.14232002500006,11.6,-10.080003527));
#290724=CARTESIAN_POINT('Ctrl Pts',(-3.14137330400006,15.2,-10.078299351));
#290725=CARTESIAN_POINT('Ctrl Pts',(-3.14137330400006,11.6,-10.078299351));
#290726=CARTESIAN_POINT('Ctrl Pts',(-3.14043159900006,15.2,-10.076600574));
#290727=CARTESIAN_POINT('Ctrl Pts',(-3.14043159900006,11.6,-10.076600574));
#290728=CARTESIAN_POINT('Ctrl Pts',(-3.13949490800006,15.2,-10.074907216));
#290729=CARTESIAN_POINT('Ctrl Pts',(-3.13949490800006,11.6,-10.074907216));
#290730=CARTESIAN_POINT('Ctrl Pts',(-3.13856322800006,15.2,-10.073219295));
#290731=CARTESIAN_POINT('Ctrl Pts',(-3.13856322800006,11.6,-10.073219295));
#290732=CARTESIAN_POINT('Ctrl Pts',(-3.13763655600006,15.2,-10.071536834));
#290733=CARTESIAN_POINT('Ctrl Pts',(-3.13763655600006,11.6,-10.071536834));
#290734=CARTESIAN_POINT('Ctrl Pts',(-3.13671489000006,15.2,-10.06985985));
#290735=CARTESIAN_POINT('Ctrl Pts',(-3.13671489000006,11.6,-10.06985985));
#290736=CARTESIAN_POINT('Ctrl Pts',(-3.13579822800006,15.2,-10.068188363));
#290737=CARTESIAN_POINT('Ctrl Pts',(-3.13579822800006,11.6,-10.068188363));
#290738=CARTESIAN_POINT('Ctrl Pts',(-3.13488656600006,15.2,-10.066522391));
#290739=CARTESIAN_POINT('Ctrl Pts',(-3.13488656600006,11.6,-10.066522391));
#290740=CARTESIAN_POINT('Ctrl Pts',(-3.13397990100006,15.2,-10.064861958));
#290741=CARTESIAN_POINT('Ctrl Pts',(-3.13397990100006,11.6,-10.064861958));
#290742=CARTESIAN_POINT('Ctrl Pts',(-3.13307823000006,15.2,-10.063207081));
#290743=CARTESIAN_POINT('Ctrl Pts',(-3.13307823000006,11.6,-10.063207081));
#290744=CARTESIAN_POINT('Ctrl Pts',(-3.13218155100006,15.2,-10.061557781));
#290745=CARTESIAN_POINT('Ctrl Pts',(-3.13218155100006,11.6,-10.061557781));
#290746=CARTESIAN_POINT('Ctrl Pts',(-3.13128986000006,15.2,-10.059914078));
#290747=CARTESIAN_POINT('Ctrl Pts',(-3.13128986000006,11.6,-10.059914078));
#290748=CARTESIAN_POINT('Ctrl Pts',(-3.13040315600006,15.2,-10.058275991));
#290749=CARTESIAN_POINT('Ctrl Pts',(-3.13040315600006,11.6,-10.058275991));
#290750=CARTESIAN_POINT('Ctrl Pts',(-3.12952143500006,15.2,-10.056643542));
#290751=CARTESIAN_POINT('Ctrl Pts',(-3.12952143500006,11.6,-10.056643542));
#290752=CARTESIAN_POINT('Ctrl Pts',(-3.12864469400005,15.2,-10.055016749));
#290753=CARTESIAN_POINT('Ctrl Pts',(-3.12864469400005,11.6,-10.055016749));
#290754=CARTESIAN_POINT('Ctrl Pts',(-3.12777293000006,15.2,-10.053395635));
#290755=CARTESIAN_POINT('Ctrl Pts',(-3.12777293000006,11.6,-10.053395635));
#290756=CARTESIAN_POINT('Ctrl Pts',(-3.12690614000006,15.2,-10.051780219));
#290757=CARTESIAN_POINT('Ctrl Pts',(-3.12690614000006,11.6,-10.051780219));
#290758=CARTESIAN_POINT('Ctrl Pts',(-3.12604432200006,15.2,-10.050170521));
#290759=CARTESIAN_POINT('Ctrl Pts',(-3.12604432200006,11.6,-10.050170521));
#290760=CARTESIAN_POINT('Ctrl Pts',(-3.12518747100006,15.2,-10.048566563));
#290761=CARTESIAN_POINT('Ctrl Pts',(-3.12518747100006,11.6,-10.048566563));
#290762=CARTESIAN_POINT('Ctrl Pts',(-3.12433558500006,15.2,-10.046968363));
#290763=CARTESIAN_POINT('Ctrl Pts',(-3.12433558500006,11.6,-10.046968363));
#290764=CARTESIAN_POINT('Ctrl Pts',(-3.12348866200006,15.2,-10.045375945));
#290765=CARTESIAN_POINT('Ctrl Pts',(-3.12348866200006,11.6,-10.045375945));
#290766=CARTESIAN_POINT('Ctrl Pts',(-3.12264669700005,15.2,-10.043789328));
#290767=CARTESIAN_POINT('Ctrl Pts',(-3.12264669700005,11.6,-10.043789328));
#290768=CARTESIAN_POINT('Ctrl Pts',(-3.12180968800006,15.2,-10.042208533));
#290769=CARTESIAN_POINT('Ctrl Pts',(-3.12180968800006,11.6,-10.042208533));
#290770=CARTESIAN_POINT('Ctrl Pts',(-3.12097763100006,15.2,-10.04063358));
#290771=CARTESIAN_POINT('Ctrl Pts',(-3.12097763100006,11.6,-10.04063358));
#290772=CARTESIAN_POINT('Ctrl Pts',(-3.12015052400006,15.2,-10.039064492));
#290773=CARTESIAN_POINT('Ctrl Pts',(-3.12015052400006,11.6,-10.039064492));
#290774=CARTESIAN_POINT('Ctrl Pts',(-3.11932836300006,15.2,-10.037501288));
#290775=CARTESIAN_POINT('Ctrl Pts',(-3.11932836300006,11.6,-10.037501288));
#290776=CARTESIAN_POINT('Ctrl Pts',(-3.11851114600006,15.2,-10.035943992));
#290777=CARTESIAN_POINT('Ctrl Pts',(-3.11851114600006,11.6,-10.035943992));
#290778=CARTESIAN_POINT('Ctrl Pts',(-3.11769886800006,15.2,-10.034392621));
#290779=CARTESIAN_POINT('Ctrl Pts',(-3.11769886800006,11.6,-10.034392621));
#290780=CARTESIAN_POINT('Ctrl Pts',(-3.11689152600006,15.2,-10.0328472));
#290781=CARTESIAN_POINT('Ctrl Pts',(-3.11689152600006,11.6,-10.0328472));
#290782=CARTESIAN_POINT('Ctrl Pts',(-3.11608911700006,15.2,-10.031307748));
#290783=CARTESIAN_POINT('Ctrl Pts',(-3.11608911700006,11.6,-10.031307748));
#290784=CARTESIAN_POINT('Ctrl Pts',(-3.11529163900006,15.2,-10.029774289));
#290785=CARTESIAN_POINT('Ctrl Pts',(-3.11529163900006,11.6,-10.029774289));
#290786=CARTESIAN_POINT('Ctrl Pts',(-3.11449908600005,15.2,-10.028246842));
#290787=CARTESIAN_POINT('Ctrl Pts',(-3.11449908600005,11.6,-10.028246842));
#290788=CARTESIAN_POINT('Ctrl Pts',(-3.11371145700006,15.2,-10.026725429));
#290789=CARTESIAN_POINT('Ctrl Pts',(-3.11371145700006,11.6,-10.026725429));
#290790=CARTESIAN_POINT('Ctrl Pts',(-3.11292874800006,15.2,-10.025210073));
#290791=CARTESIAN_POINT('Ctrl Pts',(-3.11292874800006,11.6,-10.025210073));
#290792=CARTESIAN_POINT('Ctrl Pts',(-3.11215095500006,15.2,-10.023700794));
#290793=CARTESIAN_POINT('Ctrl Pts',(-3.11215095500006,11.6,-10.023700794));
#290794=CARTESIAN_POINT('Ctrl Pts',(-3.11137807500006,15.2,-10.022197616));
#290795=CARTESIAN_POINT('Ctrl Pts',(-3.11137807500006,11.6,-10.022197616));
#290796=CARTESIAN_POINT('Ctrl Pts',(-3.11061010400006,15.2,-10.020700559));
#290797=CARTESIAN_POINT('Ctrl Pts',(-3.11061010400006,11.6,-10.020700559));
#290798=CARTESIAN_POINT('Ctrl Pts',(-3.10984704000006,15.2,-10.019209646));
#290799=CARTESIAN_POINT('Ctrl Pts',(-3.10984704000006,11.6,-10.019209646));
#290800=CARTESIAN_POINT('Ctrl Pts',(-3.10908887700006,15.2,-10.017724898));
#290801=CARTESIAN_POINT('Ctrl Pts',(-3.10908887700006,11.6,-10.017724898));
#290802=CARTESIAN_POINT('Ctrl Pts',(-3.10833561300006,15.2,-10.016246339));
#290803=CARTESIAN_POINT('Ctrl Pts',(-3.10833561300006,11.6,-10.016246339));
#290804=CARTESIAN_POINT('Ctrl Pts',(-3.10758724500006,15.2,-10.01477399));
#290805=CARTESIAN_POINT('Ctrl Pts',(-3.10758724500006,11.6,-10.01477399));
#290806=CARTESIAN_POINT('Ctrl Pts',(-3.10684376800006,15.2,-10.013307874));
#290807=CARTESIAN_POINT('Ctrl Pts',(-3.10684376800006,11.6,-10.013307874));
#290808=CARTESIAN_POINT('Ctrl Pts',(-3.10610518000006,15.2,-10.011848012));
#290809=CARTESIAN_POINT('Ctrl Pts',(-3.10610518000006,11.6,-10.011848012));
#290810=CARTESIAN_POINT('Ctrl Pts',(-3.10537147600006,15.2,-10.010394429));
#290811=CARTESIAN_POINT('Ctrl Pts',(-3.10537147600006,11.6,-10.010394429));
#290812=CARTESIAN_POINT('Ctrl Pts',(-3.10464265200005,15.2,-10.008947144));
#290813=CARTESIAN_POINT('Ctrl Pts',(-3.10464265200005,11.6,-10.008947144));
#290814=CARTESIAN_POINT('Ctrl Pts',(-3.10391870600006,15.2,-10.007506182));
#290815=CARTESIAN_POINT('Ctrl Pts',(-3.10391870600006,11.6,-10.007506182));
#290816=CARTESIAN_POINT('Ctrl Pts',(-3.10319963300006,15.2,-10.006071567));
#290817=CARTESIAN_POINT('Ctrl Pts',(-3.10319963300006,11.6,-10.006071567));
#290818=CARTESIAN_POINT('Ctrl Pts',(-3.10248542800006,15.2,-10.004643319));
#290819=CARTESIAN_POINT('Ctrl Pts',(-3.10248542800006,11.6,-10.004643319));
#290820=CARTESIAN_POINT('Ctrl Pts',(-3.10177609000006,15.2,-10.003221464));
#290821=CARTESIAN_POINT('Ctrl Pts',(-3.10177609000006,11.6,-10.003221464));
#290822=CARTESIAN_POINT('Ctrl Pts',(-3.10107161400006,15.2,-10.001806021));
#290823=CARTESIAN_POINT('Ctrl Pts',(-3.10107161400006,11.6,-10.001806021));
#290824=CARTESIAN_POINT('Ctrl Pts',(-3.10037199600006,15.2,-10.000397016));
#290825=CARTESIAN_POINT('Ctrl Pts',(-3.10037199600006,11.6,-10.000397016));
#290826=CARTESIAN_POINT('Ctrl Pts',(-3.09967723200006,15.2,-9.99899447200001));
#290827=CARTESIAN_POINT('Ctrl Pts',(-3.09967723200006,11.6,-9.99899447200001));
#290828=CARTESIAN_POINT('Ctrl Pts',(-3.09898731800006,15.2,-9.99759841200001));
#290829=CARTESIAN_POINT('Ctrl Pts',(-3.09898731800006,11.6,-9.99759841200001));
#290830=CARTESIAN_POINT('Ctrl Pts',(-3.09830225000006,15.2,-9.99620885900001));
#290831=CARTESIAN_POINT('Ctrl Pts',(-3.09830225000006,11.6,-9.99620885900001));
#290832=CARTESIAN_POINT('Ctrl Pts',(-3.09762202400006,15.2,-9.99482583600001));
#290833=CARTESIAN_POINT('Ctrl Pts',(-3.09762202400006,11.6,-9.99482583600001));
#290834=CARTESIAN_POINT('Ctrl Pts',(-3.09694663700005,15.2,-9.99344936800002));
#290835=CARTESIAN_POINT('Ctrl Pts',(-3.09694663700005,11.6,-9.99344936800002));
#290836=CARTESIAN_POINT('Ctrl Pts',(-3.09627608500006,15.2,-9.99207947800001));
#290837=CARTESIAN_POINT('Ctrl Pts',(-3.09627608500006,11.6,-9.99207947800001));
#290838=CARTESIAN_POINT('Ctrl Pts',(-3.09561036200006,15.2,-9.99071618900001));
#290839=CARTESIAN_POINT('Ctrl Pts',(-3.09561036200006,11.6,-9.99071618900001));
#290840=CARTESIAN_POINT('Ctrl Pts',(-3.09494946600006,15.2,-9.98935952600001));
#290841=CARTESIAN_POINT('Ctrl Pts',(-3.09494946600006,11.6,-9.98935952600001));
#290842=CARTESIAN_POINT('Ctrl Pts',(-3.09429339200006,15.2,-9.98800951200001));
#290843=CARTESIAN_POINT('Ctrl Pts',(-3.09429339200006,11.6,-9.98800951200001));
#290844=CARTESIAN_POINT('Ctrl Pts',(-3.09364213600006,15.2,-9.98666617100001));
#290845=CARTESIAN_POINT('Ctrl Pts',(-3.09364213600006,11.6,-9.98666617100001));
#290846=CARTESIAN_POINT('Ctrl Pts',(-3.09299569400005,15.2,-9.98532952800001));
#290847=CARTESIAN_POINT('Ctrl Pts',(-3.09299569400005,11.6,-9.98532952800001));
#290848=CARTESIAN_POINT('Ctrl Pts',(-3.09235406100006,15.2,-9.98399960700001));
#290849=CARTESIAN_POINT('Ctrl Pts',(-3.09235406100006,11.6,-9.98399960700001));
#290850=CARTESIAN_POINT('Ctrl Pts',(-3.09171723400006,15.2,-9.98267643200001));
#290851=CARTESIAN_POINT('Ctrl Pts',(-3.09171723400006,11.6,-9.98267643200001));
#290852=CARTESIAN_POINT('Ctrl Pts',(-3.09108520700006,15.2,-9.98136002700001));
#290853=CARTESIAN_POINT('Ctrl Pts',(-3.09108520700006,11.6,-9.98136002700001));
#290854=CARTESIAN_POINT('Ctrl Pts',(-3.09045797700006,15.2,-9.98005041700001));
#290855=CARTESIAN_POINT('Ctrl Pts',(-3.09045797700006,11.6,-9.98005041700001));
#290856=CARTESIAN_POINT('Ctrl Pts',(-3.08983554000006,15.2,-9.97874762700001));
#290857=CARTESIAN_POINT('Ctrl Pts',(-3.08983554000006,11.6,-9.97874762700001));
#290858=CARTESIAN_POINT('Ctrl Pts',(-3.08921789100005,15.2,-9.97745168100001));
#290859=CARTESIAN_POINT('Ctrl Pts',(-3.08921789100005,11.6,-9.97745168100001));
#290860=CARTESIAN_POINT('Ctrl Pts',(-3.08860502600006,15.2,-9.97616260400001));
#290861=CARTESIAN_POINT('Ctrl Pts',(-3.08860502600006,11.6,-9.97616260400001));
#290862=CARTESIAN_POINT('Ctrl Pts',(-3.08799694000006,15.2,-9.97488042200001));
#290863=CARTESIAN_POINT('Ctrl Pts',(-3.08799694000006,11.6,-9.97488042200001));
#290864=CARTESIAN_POINT('Ctrl Pts',(-3.08739362900006,15.2,-9.97360515800001));
#290865=CARTESIAN_POINT('Ctrl Pts',(-3.08739362900006,11.6,-9.97360515800001));
#290866=CARTESIAN_POINT('Ctrl Pts',(-3.08679508800005,15.2,-9.97233683800001));
#290867=CARTESIAN_POINT('Ctrl Pts',(-3.08679508800005,11.6,-9.97233683800001));
#290868=CARTESIAN_POINT('Ctrl Pts',(-3.08620131400006,15.2,-9.97107548900001));
#290869=CARTESIAN_POINT('Ctrl Pts',(-3.08620131400006,11.6,-9.97107548900001));
#290870=CARTESIAN_POINT('Ctrl Pts',(-3.08561230000006,15.2,-9.96982113300001));
#290871=CARTESIAN_POINT('Ctrl Pts',(-3.08561230000006,11.6,-9.96982113300001));
#290872=CARTESIAN_POINT('Ctrl Pts',(-3.08502804400006,15.2,-9.96857379800001));
#290873=CARTESIAN_POINT('Ctrl Pts',(-3.08502804400006,11.6,-9.96857379800001));
#290874=CARTESIAN_POINT('Ctrl Pts',(-3.08444854000005,15.2,-9.96733350900001));
#290875=CARTESIAN_POINT('Ctrl Pts',(-3.08444854000005,11.6,-9.96733350900001));
#290876=CARTESIAN_POINT('Ctrl Pts',(-3.08387378200006,15.2,-9.96610029000001));
#290877=CARTESIAN_POINT('Ctrl Pts',(-3.08387378200006,11.6,-9.96610029000001));
#290878=CARTESIAN_POINT('Ctrl Pts',(-3.08330376800006,15.2,-9.96487416900001));
#290879=CARTESIAN_POINT('Ctrl Pts',(-3.08330376800006,11.6,-9.96487416900001));
#290880=CARTESIAN_POINT('Ctrl Pts',(-3.08273849300006,15.2,-9.96365517000001));
#290881=CARTESIAN_POINT('Ctrl Pts',(-3.08273849300006,11.6,-9.96365517000001));
#290882=CARTESIAN_POINT('Ctrl Pts',(-3.08217795000005,15.2,-9.96244332100001));
#290883=CARTESIAN_POINT('Ctrl Pts',(-3.08217795000005,11.6,-9.96244332100001));
#290884=CARTESIAN_POINT('Ctrl Pts',(-3.08162213700006,15.2,-9.96123864600001));
#290885=CARTESIAN_POINT('Ctrl Pts',(-3.08162213700006,11.6,-9.96123864600001));
#290886=CARTESIAN_POINT('Ctrl Pts',(-3.08107104600006,15.2,-9.96004117200001));
#290887=CARTESIAN_POINT('Ctrl Pts',(-3.08107104600006,11.6,-9.96004117200001));
#290888=CARTESIAN_POINT('Ctrl Pts',(-3.08052467500006,15.2,-9.95885092700002));
#290889=CARTESIAN_POINT('Ctrl Pts',(-3.08052467500006,11.6,-9.95885092700002));
#290890=CARTESIAN_POINT('Ctrl Pts',(-3.07998301800006,15.2,-9.95766793500001));
#290891=CARTESIAN_POINT('Ctrl Pts',(-3.07998301800006,11.6,-9.95766793500001));
#290892=CARTESIAN_POINT('Ctrl Pts',(-3.07944607000006,15.2,-9.95649222300001));
#290893=CARTESIAN_POINT('Ctrl Pts',(-3.07944607000006,11.6,-9.95649222300001));
#290894=CARTESIAN_POINT('Ctrl Pts',(-3.07891382700006,15.2,-9.95532381800001));
#290895=CARTESIAN_POINT('Ctrl Pts',(-3.07891382700006,11.6,-9.95532381800001));
#290896=CARTESIAN_POINT('Ctrl Pts',(-3.07838628300006,15.2,-9.95416274700001));
#290897=CARTESIAN_POINT('Ctrl Pts',(-3.07838628300006,11.6,-9.95416274700001));
#290898=CARTESIAN_POINT('Ctrl Pts',(-3.07786343200006,15.2,-9.95300903700001));
#290899=CARTESIAN_POINT('Ctrl Pts',(-3.07786343200006,11.6,-9.95300903700001));
#290900=CARTESIAN_POINT('Ctrl Pts',(-3.07734527100005,15.2,-9.95186271400001));
#290901=CARTESIAN_POINT('Ctrl Pts',(-3.07734527100005,11.6,-9.95186271400001));
#290902=CARTESIAN_POINT('Ctrl Pts',(-3.07683179400006,15.2,-9.95072380600002));
#290903=CARTESIAN_POINT('Ctrl Pts',(-3.07683179400006,11.6,-9.95072380600002));
#290904=CARTESIAN_POINT('Ctrl Pts',(-3.07632299600006,15.2,-9.94959234000001));
#290905=CARTESIAN_POINT('Ctrl Pts',(-3.07632299600006,11.6,-9.94959234000001));
#290906=CARTESIAN_POINT('Ctrl Pts',(-3.07581887200006,15.2,-9.94846834300001));
#290907=CARTESIAN_POINT('Ctrl Pts',(-3.07581887200006,11.6,-9.94846834300001));
#290908=CARTESIAN_POINT('Ctrl Pts',(-3.07531941600006,15.2,-9.94735184300001));
#290909=CARTESIAN_POINT('Ctrl Pts',(-3.07531941600006,11.6,-9.94735184300001));
#290910=CARTESIAN_POINT('Ctrl Pts',(-3.07482462400006,15.2,-9.94624286700001));
#290911=CARTESIAN_POINT('Ctrl Pts',(-3.07482462400006,11.6,-9.94624286700001));
#290912=CARTESIAN_POINT('Ctrl Pts',(-3.07433449000006,15.2,-9.94514144400001));
#290913=CARTESIAN_POINT('Ctrl Pts',(-3.07433449000006,11.6,-9.94514144400001));
#290914=CARTESIAN_POINT('Ctrl Pts',(-3.07384900800006,15.2,-9.94404760000001));
#290915=CARTESIAN_POINT('Ctrl Pts',(-3.07384900800006,11.6,-9.94404760000001));
#290916=CARTESIAN_POINT('Ctrl Pts',(-3.07336817400006,15.2,-9.94296136400001));
#290917=CARTESIAN_POINT('Ctrl Pts',(-3.07336817400006,11.6,-9.94296136400001));
#290918=CARTESIAN_POINT('Ctrl Pts',(-3.07289198200006,15.2,-9.94188276500001));
#290919=CARTESIAN_POINT('Ctrl Pts',(-3.07289198200006,11.6,-9.94188276500001));
#290920=CARTESIAN_POINT('Ctrl Pts',(-3.07242042600006,15.2,-9.94081182900001));
#290921=CARTESIAN_POINT('Ctrl Pts',(-3.07242042600006,11.6,-9.94081182900001));
#290922=CARTESIAN_POINT('Ctrl Pts',(-3.07195350200006,15.2,-9.93974858600001));
#290923=CARTESIAN_POINT('Ctrl Pts',(-3.07195350200006,11.6,-9.93974858600001));
#290924=CARTESIAN_POINT('Ctrl Pts',(-3.07149120300005,15.2,-9.93869306300001));
#290925=CARTESIAN_POINT('Ctrl Pts',(-3.07149120300005,11.6,-9.93869306300001));
#290926=CARTESIAN_POINT('Ctrl Pts',(-3.07103352500006,15.2,-9.93764529100002));
#290927=CARTESIAN_POINT('Ctrl Pts',(-3.07103352500006,11.6,-9.93764529100002));
#290928=CARTESIAN_POINT('Ctrl Pts',(-3.07058046000006,15.2,-9.93660529500001));
#290929=CARTESIAN_POINT('Ctrl Pts',(-3.07058046000006,11.6,-9.93660529500001));
#290930=CARTESIAN_POINT('Ctrl Pts',(-3.07013200500006,15.2,-9.93557310800002));
#290931=CARTESIAN_POINT('Ctrl Pts',(-3.07013200500006,11.6,-9.93557310800002));
#290932=CARTESIAN_POINT('Ctrl Pts',(-3.06968815300006,15.2,-9.93454875700001));
#290933=CARTESIAN_POINT('Ctrl Pts',(-3.06968815300006,11.6,-9.93454875700001));
#290934=CARTESIAN_POINT('Ctrl Pts',(-3.06924889800006,15.2,-9.93353227000001));
#290935=CARTESIAN_POINT('Ctrl Pts',(-3.06924889800006,11.6,-9.93353227000001));
#290936=CARTESIAN_POINT('Ctrl Pts',(-3.06881423500006,15.2,-9.93252367900001));
#290937=CARTESIAN_POINT('Ctrl Pts',(-3.06881423500006,11.6,-9.93252367900001));
#290938=CARTESIAN_POINT('Ctrl Pts',(-3.06838415800006,15.2,-9.93152301000001));
#290939=CARTESIAN_POINT('Ctrl Pts',(-3.06838415800006,11.6,-9.93152301000001));
#290940=CARTESIAN_POINT('Ctrl Pts',(-3.06795866100006,15.2,-9.93053029600001));
#290941=CARTESIAN_POINT('Ctrl Pts',(-3.06795866100006,11.6,-9.93053029600001));
#290942=CARTESIAN_POINT('Ctrl Pts',(-3.06753773900006,15.2,-9.92954556400001));
#290943=CARTESIAN_POINT('Ctrl Pts',(-3.06753773900006,11.6,-9.92954556400001));
#290944=CARTESIAN_POINT('Ctrl Pts',(-3.06712138400006,15.2,-9.92856884600001));
#290945=CARTESIAN_POINT('Ctrl Pts',(-3.06712138400006,11.6,-9.92856884600001));
#290946=CARTESIAN_POINT('Ctrl Pts',(-3.06670959200006,15.2,-9.92760017000001));
#290947=CARTESIAN_POINT('Ctrl Pts',(-3.06670959200006,11.6,-9.92760017000001));
#290948=CARTESIAN_POINT('Ctrl Pts',(-3.06630235700006,15.2,-9.92663956700001));
#290949=CARTESIAN_POINT('Ctrl Pts',(-3.06630235700006,11.6,-9.92663956700001));
#290950=CARTESIAN_POINT('Ctrl Pts',(-3.06589967200006,15.2,-9.92568706800001));
#290951=CARTESIAN_POINT('Ctrl Pts',(-3.06589967200006,11.6,-9.92568706800001));
#290952=CARTESIAN_POINT('Ctrl Pts',(-3.06550153000006,15.2,-9.92474270100001));
#290953=CARTESIAN_POINT('Ctrl Pts',(-3.06550153000006,11.6,-9.92474270100001));
#290954=CARTESIAN_POINT('Ctrl Pts',(-3.06510792800006,15.2,-9.92380649800001));
#290955=CARTESIAN_POINT('Ctrl Pts',(-3.06510792800006,11.6,-9.92380649800001));
#290956=CARTESIAN_POINT('Ctrl Pts',(-3.06471885700006,15.2,-9.92287849000001));
#290957=CARTESIAN_POINT('Ctrl Pts',(-3.06471885700006,11.6,-9.92287849000001));
#290958=CARTESIAN_POINT('Ctrl Pts',(-3.06433431200006,15.2,-9.92195870800001));
#290959=CARTESIAN_POINT('Ctrl Pts',(-3.06433431200006,11.6,-9.92195870800001));
#290960=CARTESIAN_POINT('Ctrl Pts',(-3.06395428700006,15.2,-9.92104718300001));
#290961=CARTESIAN_POINT('Ctrl Pts',(-3.06395428700006,11.6,-9.92104718300001));
#290962=CARTESIAN_POINT('Ctrl Pts',(-3.06357877400006,15.2,-9.92014394500002));
#290963=CARTESIAN_POINT('Ctrl Pts',(-3.06357877400006,11.6,-9.92014394500002));
#290964=CARTESIAN_POINT('Ctrl Pts',(-3.06320776900006,15.2,-9.91924902500001));
#290965=CARTESIAN_POINT('Ctrl Pts',(-3.06320776900006,11.6,-9.91924902500001));
#290966=CARTESIAN_POINT('Ctrl Pts',(-3.06284126400006,15.2,-9.91836245500001));
#290967=CARTESIAN_POINT('Ctrl Pts',(-3.06284126400006,11.6,-9.91836245500001));
#290968=CARTESIAN_POINT('Ctrl Pts',(-3.06247925300006,15.2,-9.91748426800001));
#290969=CARTESIAN_POINT('Ctrl Pts',(-3.06247925300006,11.6,-9.91748426800001));
#290970=CARTESIAN_POINT('Ctrl Pts',(-3.06212173000006,15.2,-9.91661449400001));
#290971=CARTESIAN_POINT('Ctrl Pts',(-3.06212173000006,11.6,-9.91661449400001));
#290972=CARTESIAN_POINT('Ctrl Pts',(-3.06176868800006,15.2,-9.91575316500001));
#290973=CARTESIAN_POINT('Ctrl Pts',(-3.06176868800006,11.6,-9.91575316500001));
#290974=CARTESIAN_POINT('Ctrl Pts',(-3.06142212800005,15.2,-9.91490522700001));
#290975=CARTESIAN_POINT('Ctrl Pts',(-3.06142212800005,11.6,-9.91490522700001));
#290976=CARTESIAN_POINT('Ctrl Pts',(-3.06114880300006,15.2,-9.91423456700001));
#290977=CARTESIAN_POINT('Ctrl Pts',(-3.06114880300006,11.6,-9.91423456700001));
#290978=CARTESIAN_POINT('Ctrl Pts',(-3.06094627500006,15.2,-9.91373655900001));
#290979=CARTESIAN_POINT('Ctrl Pts',(-3.06094627500006,11.6,-9.91373655900001));
#290980=CARTESIAN_POINT('Ctrl Pts',(-3.06081277600006,15.2,-9.91340782600002));
#290981=CARTESIAN_POINT('Ctrl Pts',(-3.06081277600006,11.6,-9.91340782600002));
#290982=CARTESIAN_POINT('Ctrl Pts',(-3.06074721300006,15.2,-9.91324626500001));
#290983=CARTESIAN_POINT('Ctrl Pts',(-3.06074721300006,11.6,-9.91324626500001));
#290984=CARTESIAN_POINT('',(-3.06074721303514,12.2,-9.91324626444698));
#290985=CARTESIAN_POINT('',(-3.06074721303514,15.2,-9.91324626444698));
#290986=CARTESIAN_POINT('',(-3.06074721300006,12.2,-9.91324626400001));
#290987=CARTESIAN_POINT('Ctrl Pts',(-3.76106045600006,12.2,-10.867585944));
#290988=CARTESIAN_POINT('Ctrl Pts',(-3.75835329800824,12.2,-10.8648866810023));
#290989=CARTESIAN_POINT('Ctrl Pts',(-3.75565386775155,12.2,-10.8621890332137));
#290990=CARTESIAN_POINT('Ctrl Pts',(-3.75296217351105,12.2,-10.8594930000052));
#290991=CARTESIAN_POINT('Ctrl Pts',(-3.75027047927055,12.2,-10.8567969667966));
#290992=CARTESIAN_POINT('Ctrl Pts',(-3.74758651975522,12.2,-10.8541025490412));
#290993=CARTESIAN_POINT('Ctrl Pts',(-3.74491029621786,12.2,-10.8514097635877));
#290994=CARTESIAN_POINT('Ctrl Pts',(-3.74223407268051,12.2,-10.8487169781341));
#290995=CARTESIAN_POINT('Ctrl Pts',(-3.73956558451776,12.2,-10.8460258263555));
#290996=CARTESIAN_POINT('Ctrl Pts',(-3.73690483861338,12.2,-10.8433363508696));
#290997=CARTESIAN_POINT('Ctrl Pts',(-3.73424409222563,12.2,-10.8406468748952));
#290998=CARTESIAN_POINT('Ctrl Pts',(-3.73159108729007,12.2,-10.8379590765212));
#290999=CARTESIAN_POINT('Ctrl Pts',(-3.72894582899001,12.2,-10.8352730049228));
#291000=CARTESIAN_POINT('Ctrl Pts',(-3.72630057117051,12.2,-10.8325869338123));
#291001=CARTESIAN_POINT('Ctrl Pts',(-3.72366306001726,12.2,-10.8299025881433));
#291002=CARTESIAN_POINT('Ctrl Pts',(-3.72103329923849,12.2,-10.8272200094076));
#291003=CARTESIAN_POINT('Ctrl Pts',(-3.7175269516927,12.2,-10.8236432379225));
#291004=CARTESIAN_POINT('Ctrl Pts',(-3.7140343843038,12.2,-10.8200696049215));
#291005=CARTESIAN_POINT('Ctrl Pts',(-3.71055560524654,12.2,-10.8164991980348));
#291006=CARTESIAN_POINT('Ctrl Pts',(-3.7070768257153,12.2,-10.8129287906616));
#291007=CARTESIAN_POINT('Ctrl Pts',(-3.70361183581352,12.2,-10.8093616114055));
#291008=CARTESIAN_POINT('Ctrl Pts',(-3.70016064445966,12.2,-10.8057977609337));
#291009=CARTESIAN_POINT('Ctrl Pts',(-3.69757225117938,12.2,-10.8031248733226));
#291010=CARTESIAN_POINT('Ctrl Pts',(-3.69499162030653,12.2,-10.8004538583864));
#291011=CARTESIAN_POINT('Ctrl Pts',(-3.69241875548333,12.2,-10.797784756775));
#291012=CARTESIAN_POINT('Ctrl Pts',(-3.68984589066014,12.2,-10.7951156551636));
#291013=CARTESIAN_POINT('Ctrl Pts',(-3.68728079206997,12.2,-10.7924484677272));
#291014=CARTESIAN_POINT('Ctrl Pts',(-3.68472346328722,12.2,-10.7897832350322));
#291015=CARTESIAN_POINT('Ctrl Pts',(-3.68216613450446,12.2,-10.7871180023372));
#291016=CARTESIAN_POINT('Ctrl Pts',(-3.67961657667738,12.2,-10.7844547230181));
#291017=CARTESIAN_POINT('Ctrl Pts',(-3.67707479222519,12.2,-10.7817934402733));
#291018=CARTESIAN_POINT('Ctrl Pts',(-3.67453300777299,12.2,-10.7791321575284));
#291019=CARTESIAN_POINT('Ctrl Pts',(-3.67199899714333,12.2,-10.776472871883));
#291020=CARTESIAN_POINT('Ctrl Pts',(-3.66947276481739,12.2,-10.7738156233126));
#291021=CARTESIAN_POINT('Ctrl Pts',(-3.66694653203252,12.2,-10.7711583742595));
#291022=CARTESIAN_POINT('Ctrl Pts',(-3.66442807716651,12.2,-10.7685031633069));
#291023=CARTESIAN_POINT('Ctrl Pts',(-3.66191740388602,12.2,-10.7658500331716));
#291024=CARTESIAN_POINT('Ctrl Pts',(-3.65940673106163,12.2,-10.7631969035183));
#291025=CARTESIAN_POINT('Ctrl Pts',(-3.65690383987016,12.2,-10.7605458540315));
#291026=CARTESIAN_POINT('Ctrl Pts',(-3.6544087344615,12.2,-10.7578969264613));
#291027=CARTESIAN_POINT('Ctrl Pts',(-3.65191362905284,12.2,-10.7552479988911));
#291028=CARTESIAN_POINT('Ctrl Pts',(-3.64942630861889,12.2,-10.7526011945802));
#291029=CARTESIAN_POINT('Ctrl Pts',(-3.64694677723942,12.2,-10.7499565545393));
#291030=CARTESIAN_POINT('Ctrl Pts',(-3.64446724585995,12.2,-10.7473119144984));
#291031=CARTESIAN_POINT('Ctrl Pts',(-3.64199550337394,12.2,-10.7446694403018));
#291032=CARTESIAN_POINT('Ctrl Pts',(-3.63953155353558,12.2,-10.7420291727607));
#291033=CARTESIAN_POINT('Ctrl Pts',(-3.63706760369721,12.2,-10.7393889052197));
#291034=CARTESIAN_POINT('Ctrl Pts',(-3.63461144629539,12.2,-10.7367508449084));
#291035=CARTESIAN_POINT('Ctrl Pts',(-3.632163084967,12.2,-10.734115036754));
#291036=CARTESIAN_POINT('Ctrl Pts',(-3.62889860289929,12.2,-10.7306006255622));
#291037=CARTESIAN_POINT('Ctrl Pts',(-3.62564797998048,12.2,-10.7270902149876));
#291038=CARTESIAN_POINT('Ctrl Pts',(-3.62241122452719,12.2,-10.7235839084634));
#291039=CARTESIAN_POINT('Ctrl Pts',(-3.61998365815773,12.2,-10.7209541788091));
#291040=CARTESIAN_POINT('Ctrl Pts',(-3.61756389206236,12.2,-10.7183267569546));
#291041=CARTESIAN_POINT('Ctrl Pts',(-3.61515192973333,12.2,-10.7157016882167));
#291042=CARTESIAN_POINT('Ctrl Pts',(-3.6127399674043,12.2,-10.7130766194787));
#291043=CARTESIAN_POINT('Ctrl Pts',(-3.61033580902495,12.2,-10.710453901524));
#291044=CARTESIAN_POINT('Ctrl Pts',(-3.607939456278,12.2,-10.7078335803273));
#291045=CARTESIAN_POINT('Ctrl Pts',(-3.60554310353106,12.2,-10.7052132591306));
#291046=CARTESIAN_POINT('Ctrl Pts',(-3.60315455887737,12.2,-10.702595333542));
#291047=CARTESIAN_POINT('Ctrl Pts',(-3.60077382296903,12.2,-10.6999798477977));
#291048=CARTESIAN_POINT('Ctrl Pts',(-3.59839308706069,12.2,-10.6973643620535));
#291049=CARTESIAN_POINT('Ctrl Pts',(-3.59602016111406,12.2,-10.6947513154079));
#291050=CARTESIAN_POINT('Ctrl Pts',(-3.5936550477406,12.2,-10.6921407537941));
#291051=CARTESIAN_POINT('Ctrl Pts',(-3.59128993393748,12.2,-10.689530191706));
#291052=CARTESIAN_POINT('Ctrl Pts',(-3.58893263269488,12.2,-10.6869221137937));
#291053=CARTESIAN_POINT('Ctrl Pts',(-3.58658314777116,12.2,-10.684316564707));
#291054=CARTESIAN_POINT('Ctrl Pts',(-3.58423366327425,12.2,-10.6817110160937));
#291055=CARTESIAN_POINT('Ctrl Pts',(-3.58189199216026,12.2,-10.6791079957052));
#291056=CARTESIAN_POINT('Ctrl Pts',(-3.57955814120407,12.2,-10.6765075487166));
#291057=CARTESIAN_POINT('Ctrl Pts',(-3.57722429024789,12.2,-10.673907101728));
#291058=CARTESIAN_POINT('Ctrl Pts',(-3.57489825739083,12.2,-10.6713092294818));
#291059=CARTESIAN_POINT('Ctrl Pts',(-3.57258004550623,12.2,-10.668713974481));
#291060=CARTESIAN_POINT('Ctrl Pts',(-3.57026183362163,12.2,-10.6661187194802));
#291061=CARTESIAN_POINT('Ctrl Pts',(-3.56795144256226,12.2,-10.6635260830867));
#291062=CARTESIAN_POINT('Ctrl Pts',(-3.56564887521876,12.2,-10.6609361110023));
#291063=CARTESIAN_POINT('Ctrl Pts',(-3.56334630787527,12.2,-10.658346138918));
#291064=CARTESIAN_POINT('Ctrl Pts',(-3.56105156405033,12.2,-10.6557588308548));
#291065=CARTESIAN_POINT('Ctrl Pts',(-3.55876464617441,12.2,-10.6531742317818));
#291066=CARTESIAN_POINT('Ctrl Pts',(-3.55647772829848,12.2,-10.6505896327088));
#291067=CARTESIAN_POINT('Ctrl Pts',(-3.55419863698036,12.2,-10.6480077426689));
#291068=CARTESIAN_POINT('Ctrl Pts',(-3.55192737402014,12.2,-10.6454286085956));
#291069=CARTESIAN_POINT('Ctrl Pts',(-3.54965611064731,12.2,-10.6428494740537));
#291070=CARTESIAN_POINT('Ctrl Pts',(-3.5473926746517,12.2,-10.6402730948793));
#291071=CARTESIAN_POINT('Ctrl Pts',(-3.54513707074162,12.2,-10.6376995164223));
#291072=CARTESIAN_POINT('Ctrl Pts',(-3.54288146724131,12.2,-10.6351259384329));
#291073=CARTESIAN_POINT('Ctrl Pts',(-3.54063369286298,12.2,-10.6325551624545));
#291074=CARTESIAN_POINT('Ctrl Pts',(-3.5383937522917,12.2,-10.6299872337948));
#291075=CARTESIAN_POINT('Ctrl Pts',(-3.53615381172042,12.2,-10.6274193051352));
#291076=CARTESIAN_POINT('Ctrl Pts',(-3.53392170394285,12.2,-10.6248542244441));
#291077=CARTESIAN_POINT('Ctrl Pts',(-3.53169743152436,12.2,-10.6222920379958));
#291078=CARTESIAN_POINT('Ctrl Pts',(-3.52947315910586,12.2,-10.6197298515475));
#291079=CARTESIAN_POINT('Ctrl Pts',(-3.52725672165308,12.2,-10.6171705603738));
#291080=CARTESIAN_POINT('Ctrl Pts',(-3.52504812123333,12.2,-10.6146142094667));
#291081=CARTESIAN_POINT('Ctrl Pts',(-3.52136712039999,12.2,-10.6103536244667));
#291082=CARTESIAN_POINT('Ctrl Pts',(-3.51770788779226,12.2,-10.6061012102392));
#291083=CARTESIAN_POINT('Ctrl Pts',(-3.51407043374802,12.2,-10.601857185706));
#291084=CARTESIAN_POINT('Ctrl Pts',(-3.51188796140077,12.2,-10.5993107710786));
#291085=CARTESIAN_POINT('Ctrl Pts',(-3.50971333014979,12.2,-10.5967673760882));
#291086=CARTESIAN_POINT('Ctrl Pts',(-3.5075465397603,12.2,-10.594227049044));
#291087=CARTESIAN_POINT('Ctrl Pts',(-3.50465748564524,12.2,-10.5908399460106));
#291088=CARTESIAN_POINT('Ctrl Pts',(-3.50178237215338,12.2,-10.5874582980592));
#291089=CARTESIAN_POINT('Ctrl Pts',(-3.49892120399887,12.2,-10.5840822164313));
#291090=CARTESIAN_POINT('Ctrl Pts',(-3.4960600362342,12.2,-10.5807061352635));
#291091=CARTESIAN_POINT('Ctrl Pts',(-3.49321281240659,12.2,-10.577335622131));
#291092=CARTESIAN_POINT('Ctrl Pts',(-3.49037953674842,12.2,-10.5739707910168));
#291093=CARTESIAN_POINT('Ctrl Pts',(-3.48754626070421,12.2,-10.5706059594441));
#291094=CARTESIAN_POINT('Ctrl Pts',(-3.48472693437094,12.2,-10.5672468110938));
#291095=CARTESIAN_POINT('Ctrl Pts',(-3.48192155813467,12.2,-10.5638934600218));
#291096=CARTESIAN_POINT('Ctrl Pts',(-3.47911618228063,12.2,-10.5605401094067));
#291097=CARTESIAN_POINT('Ctrl Pts',(-3.47632475713438,12.2,-10.557192557056));
#291098=CARTESIAN_POINT('Ctrl Pts',(-3.47354728669386,12.2,-10.5538509197732));
#291099=CARTESIAN_POINT('Ctrl Pts',(-3.47076981587491,12.2,-10.5505092820352));
#291100=CARTESIAN_POINT('Ctrl Pts',(-3.46800629958263,12.2,-10.5471735585728));
#291101=CARTESIAN_POINT('Ctrl Pts',(-3.46525673826702,12.2,-10.5438438670028));
#291102=CARTESIAN_POINT('Ctrl Pts',(-3.46250717732603,12.2,-10.5405141758866));
#291103=CARTESIAN_POINT('Ctrl Pts',(-3.4597715748847,12.2,-10.5371905170043));
#291104=CARTESIAN_POINT('Ctrl Pts',(-3.45704992913667,12.2,-10.5338730089981));
#291105=CARTESIAN_POINT('Ctrl Pts',(-3.45432828301782,12.2,-10.5305555005399));
#291106=CARTESIAN_POINT('Ctrl Pts',(-3.45162059696194,12.2,-10.5272441427179));
#291107=CARTESIAN_POINT('Ctrl Pts',(-3.44892686953825,12.2,-10.5239390557049));
#291108=CARTESIAN_POINT('Ctrl Pts',(-3.44623314248158,12.2,-10.5206339691421));
#291109=CARTESIAN_POINT('Ctrl Pts',(-3.44355337610269,12.2,-10.5173351528892));
#291110=CARTESIAN_POINT('Ctrl Pts',(-3.44088757098587,12.2,-10.5140427265466));
#291111=CARTESIAN_POINT('Ctrl Pts',(-3.43822176550583,12.2,-10.5107502997554));
#291112=CARTESIAN_POINT('Ctrl Pts',(-3.43556992182613,12.2,-10.5074642644691));
#291113=CARTESIAN_POINT('Ctrl Pts',(-3.43293203978154,12.2,-10.5041847414978));
#291114=CARTESIAN_POINT('Ctrl Pts',(-3.43029415809635,12.2,-10.5009052189732));
#291115=CARTESIAN_POINT('Ctrl Pts',(-3.42767023889257,12.2,-10.4976322078816));
#291116=CARTESIAN_POINT('Ctrl Pts',(-3.42506028366007,12.2,-10.494365832759));
#291117=CARTESIAN_POINT('Ctrl Pts',(-3.42245032807196,12.2,-10.4910994571915));
#291118=CARTESIAN_POINT('Ctrl Pts',(-3.41985433508793,12.2,-10.4878397158106));
#291119=CARTESIAN_POINT('Ctrl Pts',(-3.41727230555833,12.2,-10.4845867329667));
#291120=CARTESIAN_POINT('Ctrl Pts',(-3.41469027602873,12.2,-10.4813337501227));
#291121=CARTESIAN_POINT('Ctrl Pts',(-3.41212220833408,12.2,-10.4780875264045));
#291122=CARTESIAN_POINT('Ctrl Pts',(-3.40956810480741,12.2,-10.4748481867287));
#291123=CARTESIAN_POINT('Ctrl Pts',(-3.40701400162875,12.2,-10.4716088474942));
#291124=CARTESIAN_POINT('Ctrl Pts',(-3.4044738615734,12.2,-10.468376389431));
#291125=CARTESIAN_POINT('Ctrl Pts',(-3.40194768376839,12.2,-10.4651509422355));
#291126=CARTESIAN_POINT('Ctrl Pts',(-3.39942150561919,12.2,-10.4619254946006));
#291127=CARTESIAN_POINT('Ctrl Pts',(-3.39690928899016,12.2,-10.4587070565909));
#291128=CARTESIAN_POINT('Ctrl Pts',(-3.39441103479988,12.2,-10.4554957532499));
#291129=CARTESIAN_POINT('Ctrl Pts',(-3.39191278094997,12.2,-10.4522844503465));
#291130=CARTESIAN_POINT('Ctrl Pts',(-3.38942848935381,12.2,-10.4490802841172));
#291131=CARTESIAN_POINT('Ctrl Pts',(-3.38695815694375,12.2,-10.4458833817114));
#291132=CARTESIAN_POINT('Ctrl Pts',(-3.3844878241971,12.2,-10.44268647887));
#291133=CARTESIAN_POINT('Ctrl Pts',(-3.38203145127989,12.2,-10.4394968398767));
#291134=CARTESIAN_POINT('Ctrl Pts',(-3.37958903709213,12.2,-10.4363145949816));
#291135=CARTESIAN_POINT('Ctrl Pts',(-3.37714662323716,12.2,-10.43313235052));
#291136=CARTESIAN_POINT('Ctrl Pts',(-3.37471816771099,12.2,-10.4299574991818));
#291137=CARTESIAN_POINT('Ctrl Pts',(-3.3723036678421,12.2,-10.4267901707263));
#291138=CARTESIAN_POINT('Ctrl Pts',(-3.36988916764423,12.2,-10.4236228418392));
#291139=CARTESIAN_POINT('Ctrl Pts',(-3.36748862427863,12.2,-10.4204630375525));
#291140=CARTESIAN_POINT('Ctrl Pts',(-3.36510203403836,12.2,-10.4173108874924));
#291141=CARTESIAN_POINT('Ctrl Pts',(-3.36271544412327,12.2,-10.4141587378617));
#291142=CARTESIAN_POINT('Ctrl Pts',(-3.36034280662203,12.2,-10.4110142448766));
#291143=CARTESIAN_POINT('Ctrl Pts',(-3.35798412136899,12.2,-10.4078775385212));
#291144=CARTESIAN_POINT('Ctrl Pts',(-3.35562543579457,12.2,-10.4047408317383));
#291145=CARTESIAN_POINT('Ctrl Pts',(-3.3532806990332,12.2,-10.4016119138099));
#291146=CARTESIAN_POINT('Ctrl Pts',(-3.35094991017341,12.2,-10.3984909165145));
#291147=CARTESIAN_POINT('Ctrl Pts',(-3.3486191216312,12.2,-10.3953699196444));
#291148=CARTESIAN_POINT('Ctrl Pts',(-3.34630227943413,12.2,-10.3922568450713));
#291149=CARTESIAN_POINT('Ctrl Pts',(-3.3439993808432,12.2,-10.389151827991));
#291150=CARTESIAN_POINT('Ctrl Pts',(-3.34169648193849,12.2,-10.3860468104876));
#291151=CARTESIAN_POINT('Ctrl Pts',(-3.33940752569898,12.2,-10.3829498492378));
#291152=CARTESIAN_POINT('Ctrl Pts',(-3.33713250874166,12.2,-10.3798610817916));
#291153=CARTESIAN_POINT('Ctrl Pts',(-3.33485749178434,12.2,-10.3767723143455));
#291154=CARTESIAN_POINT('Ctrl Pts',(-3.3325964117342,12.2,-10.3736917406059));
#291155=CARTESIAN_POINT('Ctrl Pts',(-3.33034926689093,12.2,-10.3706194979393));
#291156=CARTESIAN_POINT('Ctrl Pts',(-3.32810212235384,12.2,-10.3675472556913));
#291157=CARTESIAN_POINT('Ctrl Pts',(-3.32586891203021,12.2,-10.3644833448467));
#291158=CARTESIAN_POINT('Ctrl Pts',(-3.32364962953485,12.2,-10.3614279040271));
#291159=CARTESIAN_POINT('Ctrl Pts',(-3.32143034673711,12.2,-10.3583724627911));
#291160=CARTESIAN_POINT('Ctrl Pts',(-3.31922499279305,12.2,-10.3553254922679));
#291161=CARTESIAN_POINT('Ctrl Pts',(-3.31703356067505,12.2,-10.3522871327699));
#291162=CARTESIAN_POINT('Ctrl Pts',(-3.31484212885563,12.2,-10.3492487736858));
#291163=CARTESIAN_POINT('Ctrl Pts',(-3.31266462140105,12.2,-10.3462190252256));
#291164=CARTESIAN_POINT('Ctrl Pts',(-3.31050102891034,12.2,-10.343198028972));
#291165=CARTESIAN_POINT('Ctrl Pts',(-3.30833743612485,12.2,-10.3401770323068));
#291166=CARTESIAN_POINT('Ctrl Pts',(-3.30618775946761,12.2,-10.3371647890883));
#291167=CARTESIAN_POINT('Ctrl Pts',(-3.30405199369016,12.2,-10.3341614403309));
#291168=CARTESIAN_POINT('Ctrl Pts',(-3.30191622820371,12.2,-10.3311580919827));
#291169=CARTESIAN_POINT('Ctrl Pts',(-3.29979437152604,12.2,-10.3281636393895));
#291170=CARTESIAN_POINT('Ctrl Pts',(-3.29768641819746,12.2,-10.3251782277441));
#291171=CARTESIAN_POINT('Ctrl Pts',(-3.29557846458167,12.2,-10.3221928156919));
#291172=CARTESIAN_POINT('Ctrl Pts',(-3.29348441217865,12.2,-10.3192164420575));
#291173=CARTESIAN_POINT('Ctrl Pts',(-3.29140425478841,12.2,-10.3162492560075));
#291174=CARTESIAN_POINT('Ctrl Pts',(-3.28932409768159,12.2,-10.3132820703618));
#291175=CARTESIAN_POINT('Ctrl Pts',(-3.28725783687829,12.2,-10.3103240715044));
#291176=CARTESIAN_POINT('Ctrl Pts',(-3.28520546149789,12.2,-10.3073754046529));
#291177=CARTESIAN_POINT('Ctrl Pts',(-3.28315308583786,12.2,-10.3044267373996));
#291178=CARTESIAN_POINT('Ctrl Pts',(-3.28111459710795,12.2,-10.3014874054807));
#291179=CARTESIAN_POINT('Ctrl Pts',(-3.27908998560962,12.2,-10.2985575555439));
#291180=CARTESIAN_POINT('Ctrl Pts',(-3.27706537438714,12.2,-10.2956277060062));
#291181=CARTESIAN_POINT('Ctrl Pts',(-3.27505464057856,12.2,-10.2927073387));
#291182=CARTESIAN_POINT('Ctrl Pts',(-3.2730577753515,12.2,-10.2897966044926));
#291183=CARTESIAN_POINT('Ctrl Pts',(-3.27106090985235,12.2,-10.2868858698885));
#291184=CARTESIAN_POINT('Ctrl Pts',(-3.26907791397877,12.2,-10.2839847678798));
#291185=CARTESIAN_POINT('Ctrl Pts',(-3.267108775807,12.2,-10.2810934512647));
#291186=CARTESIAN_POINT('Ctrl Pts',(-3.26464735322643,12.2,-10.2774793056927));
#291187=CARTESIAN_POINT('Ctrl Pts',(-3.26220758391863,12.2,-10.2738804496538));
#291188=CARTESIAN_POINT('Ctrl Pts',(-3.25978944885032,12.2,-10.2702971818074));
#291189=CARTESIAN_POINT('Ctrl Pts',(-3.25785494095382,12.2,-10.2674305677646));
#291190=CARTESIAN_POINT('Ctrl Pts',(-3.2559342784962,12.2,-10.2645739314448));
#291191=CARTESIAN_POINT('Ctrl Pts',(-3.25402745109511,12.2,-10.2617274278987));
#291192=CARTESIAN_POINT('Ctrl Pts',(-3.25212062343421,12.2,-10.2588809239648));
#291193=CARTESIAN_POINT('Ctrl Pts',(-3.25022762948462,12.2,-10.2560445534066));
#291194=CARTESIAN_POINT('Ctrl Pts',(-3.24834845854039,12.2,-10.2532184717397));
#291195=CARTESIAN_POINT('Ctrl Pts',(-3.24646928785219,12.2,-10.2503923904579));
#291196=CARTESIAN_POINT('Ctrl Pts',(-3.24460394011389,12.2,-10.2475766005137));
#291197=CARTESIAN_POINT('Ctrl Pts',(-3.2427524028194,12.2,-10.2447712584087));
#291198=CARTESIAN_POINT('Ctrl Pts',(-3.24090086527264,12.2,-10.2419659159214));
#291199=CARTESIAN_POINT('Ctrl Pts',(-3.23906313770495,12.2,-10.2391710219489));
#291200=CARTESIAN_POINT('Ctrl Pts',(-3.23723920871666,12.2,-10.2363867387416));
#291201=CARTESIAN_POINT('Ctrl Pts',(-3.23495929760556,12.2,-10.2329063849222));
#291202=CARTESIAN_POINT('Ctrl Pts',(-3.23270094429777,12.2,-10.229442607397));
#291203=CARTESIAN_POINT('Ctrl Pts',(-3.23046412477379,12.2,-10.2259957252981));
#291204=CARTESIAN_POINT('Ctrl Pts',(-3.2282273052498,12.2,-10.2225488431992));
#291205=CARTESIAN_POINT('Ctrl Pts',(-3.22601201728332,12.2,-10.2191188550371));
#291206=CARTESIAN_POINT('Ctrl Pts',(-3.22381823533999,12.2,-10.2157060845519));
#291207=CARTESIAN_POINT('Ctrl Pts',(-3.22162445339668,12.2,-10.2122933140667));
#291208=CARTESIAN_POINT('Ctrl Pts',(-3.21945217529168,12.2,-10.2088977589283));
#291209=CARTESIAN_POINT('Ctrl Pts',(-3.21730137258447,12.2,-10.2055197485125));
#291210=CARTESIAN_POINT('Ctrl Pts',(-3.21515056987726,12.2,-10.2021417380967));
#291211=CARTESIAN_POINT('Ctrl Pts',(-3.21302124374448,12.2,-10.1987812701083));
#291212=CARTESIAN_POINT('Ctrl Pts',(-3.21091336103728,12.2,-10.1954386764981));
#291213=CARTESIAN_POINT('Ctrl Pts',(-3.20880547833007,12.2,-10.192096082888));
#291214=CARTESIAN_POINT('Ctrl Pts',(-3.20671904064537,12.2,-10.1887713637412));
#291215=CARTESIAN_POINT('Ctrl Pts',(-3.20465401450203,12.2,-10.1854648541329));
#291216=CARTESIAN_POINT('Ctrl Pts',(-3.20258898835869,12.2,-10.1821583445245));
#291217=CARTESIAN_POINT('Ctrl Pts',(-3.2005453735671,12.2,-10.178870044893));
#291218=CARTESIAN_POINT('Ctrl Pts',(-3.19852313669383,12.2,-10.175600295589));
#291219=CARTESIAN_POINT('Ctrl Pts',(-3.19650089982057,12.2,-10.1723305462849));
#291220=CARTESIAN_POINT('Ctrl Pts',(-3.1945000396338,12.2,-10.1690793491812));
#291221=CARTESIAN_POINT('Ctrl Pts',(-3.1925205226911,12.2,-10.1658470465439));
#291222=CARTESIAN_POINT('Ctrl Pts',(-3.19054100596417,12.2,-10.1626147442589));
#291223=CARTESIAN_POINT('Ctrl Pts',(-3.18858283094397,12.2,-10.1594013379767));
#291224=CARTESIAN_POINT('Ctrl Pts',(-3.18664595927835,12.2,-10.1562071781844));
#291225=CARTESIAN_POINT('Ctrl Pts',(-3.18470908740161,12.2,-10.153013018044));
#291226=CARTESIAN_POINT('Ctrl Pts',(-3.18279351879397,12.2,-10.1498381057865));
#291227=CARTESIAN_POINT('Ctrl Pts',(-3.18089921601445,12.2,-10.146682795646));
#291228=CARTESIAN_POINT('Ctrl Pts',(-3.17900491323494,12.2,-10.1435274855055));
#291229=CARTESIAN_POINT('Ctrl Pts',(-3.17713187508126,12.2,-10.1403917776799));
#291230=CARTESIAN_POINT('Ctrl Pts',(-3.17528006047338,12.2,-10.1372760341201));
#291231=CARTESIAN_POINT('Ctrl Pts',(-3.1734282458655,12.2,-10.1341602905602));
#291232=CARTESIAN_POINT('Ctrl Pts',(-3.17159765405846,12.2,-10.1310645103801));
#291233=CARTESIAN_POINT('Ctrl Pts',(-3.1697882428768,12.2,-10.1279890619762));
#291234=CARTESIAN_POINT('Ctrl Pts',(-3.16797883169514,12.2,-10.1249136135724));
#291235=CARTESIAN_POINT('Ctrl Pts',(-3.16619060092236,12.2,-10.1218584964608));
#291236=CARTESIAN_POINT('Ctrl Pts',(-3.16442350557403,12.2,-10.1188240822235));
#291237=CARTESIAN_POINT('Ctrl Pts',(-3.1626564102257,12.2,-10.1157896679863));
#291238=CARTESIAN_POINT('Ctrl Pts',(-3.16091045036994,12.2,-10.1127759580541));
#291239=CARTESIAN_POINT('Ctrl Pts',(-3.15918557925095,12.2,-10.1097833297766));
#291240=CARTESIAN_POINT('Ctrl Pts',(-3.15746070813195,12.2,-10.1067907014991));
#291241=CARTESIAN_POINT('Ctrl Pts',(-3.15575692424444,12.2,-10.1038191551666));
#291242=CARTESIAN_POINT('Ctrl Pts',(-3.15407418125833,12.2,-10.100869076));
#291243=CARTESIAN_POINT('Ctrl Pts',(-3.15239143827223,12.2,-10.0979189968333));
#291244=CARTESIAN_POINT('Ctrl Pts',(-3.1507297334565,12.2,-10.0949903842171));
#291245=CARTESIAN_POINT('Ctrl Pts',(-3.14908901803245,12.2,-10.0920836292734));
#291246=CARTESIAN_POINT('Ctrl Pts',(-3.14712015959512,12.2,-10.0885955234677));
#291247=CARTESIAN_POINT('Ctrl Pts',(-3.14518152472779,12.2,-10.0851388913637));
#291248=CARTESIAN_POINT('Ctrl Pts',(-3.14327302137914,12.2,-10.0817144226534));
#291249=CARTESIAN_POINT('Ctrl Pts',(-3.14136451785714,12.2,-10.078289953632));
#291250=CARTESIAN_POINT('Ctrl Pts',(-3.13948614573056,12.2,-10.0748976450063));
#291251=CARTESIAN_POINT('Ctrl Pts',(-3.13763780729854,12.2,-10.0715382029088));
#291252=CARTESIAN_POINT('Ctrl Pts',(-3.13578946903442,12.2,-10.0681787611164));
#291253=CARTESIAN_POINT('Ctrl Pts',(-3.13397116827805,12.2,-10.0648521796912));
#291254=CARTESIAN_POINT('Ctrl Pts',(-3.13218279792766,12.2,-10.0615591800623));
#291255=CARTESIAN_POINT('Ctrl Pts',(-3.13039442757727,12.2,-10.0582661804334));
#291256=CARTESIAN_POINT('Ctrl Pts',(-3.12863599159116,12.2,-10.0550067590768));
#291257=CARTESIAN_POINT('Ctrl Pts',(-3.12690738306934,12.2,-10.0517816486925));
#291258=CARTESIAN_POINT('Ctrl Pts',(-3.12517877454752,12.2,-10.0485565383082));
#291259=CARTESIAN_POINT('Ctrl Pts',(-3.12347999264,12.2,-10.0453657381733));
#291260=CARTESIAN_POINT('Ctrl Pts',(-3.1218109261986,12.2,-10.0422099938689));
#291261=CARTESIAN_POINT('Ctrl Pts',(-3.12014185960561,12.2,-10.0390542492779));
#291262=CARTESIAN_POINT('Ctrl Pts',(-3.11850251067384,12.2,-10.0359335617069));
#291263=CARTESIAN_POINT('Ctrl Pts',(-3.11689275917073,12.2,-10.0328486921236));
#291264=CARTESIAN_POINT('Ctrl Pts',(-3.11528300781385,12.2,-10.0297638228206));
#291265=CARTESIAN_POINT('Ctrl Pts',(-3.11370285677648,12.2,-10.0267147724556));
#291266=CARTESIAN_POINT('Ctrl Pts',(-3.11215218324238,12.2,-10.023702319218));
#291267=CARTESIAN_POINT('Ctrl Pts',(-3.11060150970829,12.2,-10.0206898659804));
#291268=CARTESIAN_POINT('Ctrl Pts',(-3.10908031346876,12.2,-10.0177140097827));
#291269=CARTESIAN_POINT('Ctrl Pts',(-3.10758846793762,12.2,-10.0147755485536));
#291270=CARTESIAN_POINT('Ctrl Pts',(-3.10609662227098,12.2,-10.0118370870575));
#291271=CARTESIAN_POINT('Ctrl Pts',(-3.10463412853219,12.2,-10.0089360179651));
#291272=CARTESIAN_POINT('Ctrl Pts',(-3.10320084995535,12.2,-10.0060731586441));
#291273=CARTESIAN_POINT('Ctrl Pts',(-3.10176757150868,12.2,-10.0032102995831));
#291274=CARTESIAN_POINT('Ctrl Pts',(-3.10036351212365,12.2,-10.0003856478294));
#291275=CARTESIAN_POINT('Ctrl Pts',(-3.09898852950063,12.2,-9.99760003875121));
#291276=CARTESIAN_POINT('Ctrl Pts',(-3.09761354687761,12.2,-9.99481442967302));
#291277=CARTESIAN_POINT('Ctrl Pts',(-3.09626764235601,12.2,-9.992067861541));
#291278=CARTESIAN_POINT('Ctrl Pts',(-3.0949506716519,12.2,-9.98936118855332));
#291279=CARTESIAN_POINT('Ctrl Pts',(-3.09363370082815,12.2,-9.98665451531976));
#291280=CARTESIAN_POINT('Ctrl Pts',(-3.09234566383313,12.2,-9.98398773660126));
#291281=CARTESIAN_POINT('Ctrl Pts',(-3.09108640611993,12.2,-9.98136172549601));
#291282=CARTESIAN_POINT('Ctrl Pts',(-3.08982714852112,12.2,-9.97873571462928));
#291283=CARTESIAN_POINT('Ctrl Pts',(-3.08859667413966,12.2,-9.97615047349918));
#291284=CARTESIAN_POINT('Ctrl Pts',(-3.08739482151667,12.2,-9.97360689400827));
#291285=CARTESIAN_POINT('Ctrl Pts',(-3.08619296889367,12.2,-9.97106331451735));
#291286=CARTESIAN_POINT('Ctrl Pts',(-3.0850197406864,12.2,-9.96856140040726));
#291287=CARTESIAN_POINT('Ctrl Pts',(-3.08387496808582,12.2,-9.96610206470462));
#291288=CARTESIAN_POINT('Ctrl Pts',(-3.08273019538126,12.2,-9.9636427287786));
#291289=CARTESIAN_POINT('Ctrl Pts',(-3.08161388236379,12.2,-9.96122597289263));
#291290=CARTESIAN_POINT('Ctrl Pts',(-3.08052585338975,12.2,-9.95885274001627));
#291291=CARTESIAN_POINT('Ctrl Pts',(-3.07943782451455,12.2,-9.95647950735548));
#291292=CARTESIAN_POINT('Ctrl Pts',(-3.07837808089167,12.2,-9.95414979408447));
#291293=CARTESIAN_POINT('Ctrl Pts',(-3.07734644200787,12.2,-9.95186456774057));
#291294=CARTESIAN_POINT('Ctrl Pts',(-3.07631480312407,12.2,-9.94957934139665));
#291295=CARTESIAN_POINT('Ctrl Pts',(-3.07531126986906,12.2,-9.94733860123363));
#291296=CARTESIAN_POINT('Ctrl Pts',(-3.07433565306996,12.2,-9.94514333889477));
#291297=CARTESIAN_POINT('Ctrl Pts',(-3.07336003618225,12.2,-9.94294807635649));
#291298=CARTESIAN_POINT('Ctrl Pts',(-3.07241233616466,12.2,-9.9407982909155));
#291299=CARTESIAN_POINT('Ctrl Pts',(-3.0714923581164,12.2,-9.93869500047068));
#291300=CARTESIAN_POINT('Ctrl Pts',(-3.07057238015171,12.2,-9.93659171021692));
#291301=CARTESIAN_POINT('Ctrl Pts',(-3.06968012242037,12.2,-9.9345349144572));
#291302=CARTESIAN_POINT('Ctrl Pts',(-3.06881538145299,12.2,-9.93252565944896));
#291303=CARTESIAN_POINT('Ctrl Pts',(-3.06795064048562,12.2,-9.9305164044407));
#291304=CARTESIAN_POINT('Ctrl Pts',(-3.06711341568285,12.2,-9.92855469009569));
#291305=CARTESIAN_POINT('Ctrl Pts',(-3.06630349454421,12.2,-9.92664159307927));
#291306=CARTESIAN_POINT('Ctrl Pts',(-3.06549357340558,12.2,-9.92472849606284));
#291307=CARTESIAN_POINT('Ctrl Pts',(-3.0647109540901,12.2,-9.9228640128102));
#291308=CARTESIAN_POINT('Ctrl Pts',(-3.0639554151157,12.2,-9.92104925495608));
#291309=CARTESIAN_POINT('Ctrl Pts',(-3.06282573262112,12.2,-9.91833582752322));
#291310=CARTESIAN_POINT('Ctrl Pts',(-3.06175657911663,12.2,-9.91573355507463));
#291311=CARTESIAN_POINT('Ctrl Pts',(-3.06074721300006,12.2,-9.91324626500001));
#291312=CARTESIAN_POINT('Ctrl Pts',(-3.06074721300006,15.2,-9.91324626500001));
#291313=CARTESIAN_POINT('Ctrl Pts',(-3.06141904375483,15.2,-9.91490179706191));
#291314=CARTESIAN_POINT('Ctrl Pts',(-3.06211736679865,15.2,-9.91660826837016));
#291315=CARTESIAN_POINT('Ctrl Pts',(-3.06284238742061,15.2,-9.91836455053259));
#291316=CARTESIAN_POINT('Ctrl Pts',(-3.06357090445848,15.2,-9.92012930237536));
#291317=CARTESIAN_POINT('Ctrl Pts',(-3.06432638660912,15.2,-9.92194434089947));
#291318=CARTESIAN_POINT('Ctrl Pts',(-3.06510906085912,15.2,-9.92380854693038));
#291319=CARTESIAN_POINT('Ctrl Pts',(-3.06589173503803,15.2,-9.92567275279196));
#291320=CARTESIAN_POINT('Ctrl Pts',(-3.06670160281363,15.2,-9.92758612253754));
#291321=CARTESIAN_POINT('Ctrl Pts',(-3.0675388807832,15.2,-9.92954756746627));
#291322=CARTESIAN_POINT('Ctrl Pts',(-3.06837615875278,15.2,-9.931509012395));
#291323=CARTESIAN_POINT('Ctrl Pts',(-3.0692408475782,15.2,-9.93351853336747));
#291324=CARTESIAN_POINT('Ctrl Pts',(-3.07013315567209,15.2,-9.93557506680944));
#291325=CARTESIAN_POINT('Ctrl Pts',(-3.07102546384703,15.2,-9.9376316004382));
#291326=CARTESIAN_POINT('Ctrl Pts',(-3.07194539223311,15.2,-9.93973515056398));
#291327=CARTESIAN_POINT('Ctrl Pts',(-3.07289314111998,15.2,-9.94188468101757));
#291328=CARTESIAN_POINT('Ctrl Pts',(-3.07384088992077,15.2,-9.94403421127591));
#291329=CARTESIAN_POINT('Ctrl Pts',(-3.07481645821564,15.2,-9.94622972489708));
#291330=CARTESIAN_POINT('Ctrl Pts',(-3.07582003901713,15.2,-9.94847021724262));
#291331=CARTESIAN_POINT('Ctrl Pts',(-3.07682361981862,15.2,-9.95071070958816));
#291332=CARTESIAN_POINT('Ctrl Pts',(-3.07785521373208,15.2,-9.95299617995969));
#291333=CARTESIAN_POINT('Ctrl Pts',(-3.07891500169237,15.2,-9.95532565137317));
#291334=CARTESIAN_POINT('Ctrl Pts',(-3.07997478974891,15.2,-9.95765512299823));
#291335=CARTESIAN_POINT('Ctrl Pts',(-3.08106277567559,15.2,-9.96002859490372));
#291336=CARTESIAN_POINT('Ctrl Pts',(-3.08217913257169,15.2,-9.96244511478835));
#291337=CARTESIAN_POINT('Ctrl Pts',(-3.0832954893664,15.2,-9.96486163445348));
#291338=CARTESIAN_POINT('Ctrl Pts',(-3.08444021890545,15.2,-9.9673212018672));
#291339=CARTESIAN_POINT('Ctrl Pts',(-3.08561348953074,15.2,-9.96982288836146));
#291340=CARTESIAN_POINT('Ctrl Pts',(-3.08678676015602,15.2,-9.97232457485573));
#291341=CARTESIAN_POINT('Ctrl Pts',(-3.08798857222068,15.2,-9.97486837946327));
#291342=CARTESIAN_POINT('Ctrl Pts',(-3.08921908692473,15.2,-9.97745339811756));
#291343=CARTESIAN_POINT('Ctrl Pts',(-3.09044960162878,15.2,-9.98003841677186));
#291344=CARTESIAN_POINT('Ctrl Pts',(-3.09170882050837,15.2,-9.98266464830892));
#291345=CARTESIAN_POINT('Ctrl Pts',(-3.09299689612628,15.2,-9.9853312082093));
#291346=CARTESIAN_POINT('Ctrl Pts',(-3.09428497186118,15.2,-9.98799776835189));
#291347=CARTESIAN_POINT('Ctrl Pts',(-3.09560190589886,15.2,-9.99070465833173));
#291348=CARTESIAN_POINT('Ctrl Pts',(-3.09694784580681,15.2,-9.99345101264978));
#291349=CARTESIAN_POINT('Ctrl Pts',(-3.0982937855925,15.2,-9.99619736671838));
#291350=CARTESIAN_POINT('Ctrl Pts',(-3.0996687338774,15.2,-9.99898318664687));
#291351=CARTESIAN_POINT('Ctrl Pts',(-3.10107282849937,15.2,-10.0018076304737));
#291352=CARTESIAN_POINT('Ctrl Pts',(-3.10247692312134,15.2,-10.0046320743005));
#291353=CARTESIAN_POINT('Ctrl Pts',(-3.1039101674124,15.2,-10.0074951390084));
#291354=CARTESIAN_POINT('Ctrl Pts',(-3.10537269585726,15.2,-10.0103960032338));
#291355=CARTESIAN_POINT('Ctrl Pts',(-3.10683522443497,15.2,-10.0132968677226));
#291356=CARTESIAN_POINT('Ctrl Pts',(-3.10832703761551,15.2,-10.0162355300235));
#291357=CARTESIAN_POINT('Ctrl Pts',(-3.10984826536637,15.2,-10.0192111874373));
#291358=CARTESIAN_POINT('Ctrl Pts',(-3.11136949297905,15.2,-10.0221868445808));
#291359=CARTESIAN_POINT('Ctrl Pts',(-3.11292013460792,15.2,-10.0251994943539));
#291360=CARTESIAN_POINT('Ctrl Pts',(-3.11450031697429,15.2,-10.0282483505069));
#291361=CARTESIAN_POINT('Ctrl Pts',(-3.11608049934065,15.2,-10.0312972066599));
#291362=CARTESIAN_POINT('Ctrl Pts',(-3.11769022027456,15.2,-10.034382268134));
#291363=CARTESIAN_POINT('Ctrl Pts',(-3.11932959879632,15.2,-10.0375027646015));
#291364=CARTESIAN_POINT('Ctrl Pts',(-3.12096897746699,15.2,-10.0406232613525));
#291365=CARTESIAN_POINT('Ctrl Pts',(-3.1226380161269,15.2,-10.043779194015));
#291366=CARTESIAN_POINT('Ctrl Pts',(-3.12433682588942,15.2,-10.046969808767));
#291367=CARTESIAN_POINT('Ctrl Pts',(-3.12603563549762,15.2,-10.0501604232292));
#291368=CARTESIAN_POINT('Ctrl Pts',(-3.12776421756389,15.2,-10.0533857175767));
#291369=CARTESIAN_POINT('Ctrl Pts',(-3.12952268,15.2,-10.0566449560416));
#291370=CARTESIAN_POINT('Ctrl Pts',(-3.13128114243611,15.2,-10.0599041945065));
#291371=CARTESIAN_POINT('Ctrl Pts',(-3.13306948755115,15.2,-10.0631973737432));
#291372=CARTESIAN_POINT('Ctrl Pts',(-3.13488781507418,15.2,-10.0665237753699));
#291373=CARTESIAN_POINT('Ctrl Pts',(-3.13670614276237,15.2,-10.0698501772988));
#291374=CARTESIAN_POINT('Ctrl Pts',(-3.13855445617533,15.2,-10.0732097970826));
#291375=CARTESIAN_POINT('Ctrl Pts',(-3.14043285269643,15.2,-10.076601929103));
#291376=CARTESIAN_POINT('Ctrl Pts',(-3.1423112490469,15.2,-10.0799940608154));
#291377=CARTESIAN_POINT('Ctrl Pts',(-3.14421972882912,15.2,-10.0834187031697));
#291378=CARTESIAN_POINT('Ctrl Pts',(-3.14615838626755,15.2,-10.0868751619765));
#291379=CARTESIAN_POINT('Ctrl Pts',(-3.14809704370598,15.2,-10.0903316207834));
#291380=CARTESIAN_POINT('Ctrl Pts',(-3.15006588000679,15.2,-10.0938198977291));
#291381=CARTESIAN_POINT('Ctrl Pts',(-3.15206498434951,15.2,-10.0973393095166));
#291382=CARTESIAN_POINT('Ctrl Pts',(-3.15373090469565,15.2,-10.1002721527794));
#291383=CARTESIAN_POINT('Ctrl Pts',(-3.1554178442173,15.2,-10.1032266189899));
#291384=CARTESIAN_POINT('Ctrl Pts',(-3.15712585289676,15.2,-10.1062023198221));
#291385=CARTESIAN_POINT('Ctrl Pts',(-3.15883386157622,15.2,-10.1091780206544));
#291386=CARTESIAN_POINT('Ctrl Pts',(-3.16056293785227,15.2,-10.1121749566236));
#291387=CARTESIAN_POINT('Ctrl Pts',(-3.16231313299905,15.2,-10.1151927467066));
#291388=CARTESIAN_POINT('Ctrl Pts',(-3.16406332814582,15.2,-10.1182105367897));
#291389=CARTESIAN_POINT('Ctrl Pts',(-3.16583463929444,15.2,-10.1212491832777));
#291390=CARTESIAN_POINT('Ctrl Pts',(-3.167627112975,15.2,-10.12430830675));
#291391=CARTESIAN_POINT('Ctrl Pts',(-3.16941958665556,15.2,-10.1273674302222));
#291392=CARTESIAN_POINT('Ctrl Pts',(-3.17123322385372,15.2,-10.1304470342486));
#291393=CARTESIAN_POINT('Ctrl Pts',(-3.17306806670934,15.2,-10.133546747735));
#291394=CARTESIAN_POINT('Ctrl Pts',(-3.17490290956495,15.2,-10.1366464612213));
#291395=CARTESIAN_POINT('Ctrl Pts',(-3.17675895911068,15.2,-10.1397662843544));
#291396=CARTESIAN_POINT('Ctrl Pts',(-3.17863625688957,15.2,-10.1429058551887));
#291397=CARTESIAN_POINT('Ctrl Pts',(-3.18051355466847,15.2,-10.1460454260231));
#291398=CARTESIAN_POINT('Ctrl Pts',(-3.18241210088013,15.2,-10.1492047423347));
#291399=CARTESIAN_POINT('Ctrl Pts',(-3.18433193615902,15.2,-10.1523834474746));
#291400=CARTESIAN_POINT('Ctrl Pts',(-3.18625177143792,15.2,-10.1555621526145));
#291401=CARTESIAN_POINT('Ctrl Pts',(-3.18819289448948,15.2,-10.1587602472948));
#291402=CARTESIAN_POINT('Ctrl Pts',(-3.19015534472789,15.2,-10.1619773768318));
#291403=CARTESIAN_POINT('Ctrl Pts',(-3.1921177949663,15.2,-10.1651945063689));
#291404=CARTESIAN_POINT('Ctrl Pts',(-3.19410157103831,15.2,-10.1684306717575));
#291405=CARTESIAN_POINT('Ctrl Pts',(-3.19610671201228,15.2,-10.1716855244674));
#291406=CARTESIAN_POINT('Ctrl Pts',(-3.19811185298625,15.2,-10.1749403771773));
#291407=CARTESIAN_POINT('Ctrl Pts',(-3.2001383563939,15.2,-10.1782139192346));
#291408=CARTESIAN_POINT('Ctrl Pts',(-3.20218625903454,15.2,-10.1815058061805));
#291409=CARTESIAN_POINT('Ctrl Pts',(-3.20423416145195,15.2,-10.1847976927677));
#291410=CARTESIAN_POINT('Ctrl Pts',(-3.20630346059506,15.2,-10.1881079253678));
#291411=CARTESIAN_POINT('Ctrl Pts',(-3.20839419293487,15.2,-10.1914361652813));
#291412=CARTESIAN_POINT('Ctrl Pts',(-3.21048492550257,15.2,-10.1947644055576));
#291413=CARTESIAN_POINT('Ctrl Pts',(-3.21259708890046,15.2,-10.1981106537447));
#291414=CARTESIAN_POINT('Ctrl Pts',(-3.21473071570426,15.2,-10.201474577285));
#291415=CARTESIAN_POINT('Ctrl Pts',(-3.21686434250806,15.2,-10.2048385008252));
#291416=CARTESIAN_POINT('Ctrl Pts',(-3.21901943374485,15.2,-10.2082200984179));
#291417=CARTESIAN_POINT('Ctrl Pts',(-3.22119601721531,15.2,-10.2116190437637));
#291418=CARTESIAN_POINT('Ctrl Pts',(-3.22337260068577,15.2,-10.2150179891095));
#291419=CARTESIAN_POINT('Ctrl Pts',(-3.22557067655524,15.2,-10.21843428127));
#291420=CARTESIAN_POINT('Ctrl Pts',(-3.22779027444242,15.2,-10.2218675960931));
#291421=CARTESIAN_POINT('Ctrl Pts',(-3.2300098723296,15.2,-10.2253009109163));
#291422=CARTESIAN_POINT('Ctrl Pts',(-3.23225099273662,15.2,-10.228751249002));
#291423=CARTESIAN_POINT('Ctrl Pts',(-3.23451366127715,15.2,-10.232218291015));
#291424=CARTESIAN_POINT('Ctrl Pts',(-3.23677632981768,15.2,-10.235685333028));
#291425=CARTESIAN_POINT('Ctrl Pts',(-3.23906054660602,15.2,-10.2391690781609));
#291426=CARTESIAN_POINT('Ctrl Pts',(-3.241366338341,15.2,-10.2426692128128));
#291427=CARTESIAN_POINT('Ctrl Pts',(-3.24321097182952,15.2,-10.245469320687));
#291428=CARTESIAN_POINT('Ctrl Pts',(-3.24506941114164,15.2,-10.2482799171166));
#291429=CARTESIAN_POINT('Ctrl Pts',(-3.24694167200509,15.2,-10.2511008431344));
#291430=CARTESIAN_POINT('Ctrl Pts',(-3.24881393261344,15.2,-10.2539217687678));
#291431=CARTESIAN_POINT('Ctrl Pts',(-3.25070001228992,15.2,-10.2567530244174));
#291432=CARTESIAN_POINT('Ctrl Pts',(-3.25259992357815,15.2,-10.2595944518511));
#291433=CARTESIAN_POINT('Ctrl Pts',(-3.25449983512524,15.2,-10.262435879672));
#291434=CARTESIAN_POINT('Ctrl Pts',(-3.25641357846286,15.2,-10.2652874788607));
#291435=CARTESIAN_POINT('Ctrl Pts',(-3.25834116412438,15.2,-10.268149094684));
#291436=CARTESIAN_POINT('Ctrl Pts',(-3.26026874952326,15.2,-10.2710107101174));
#291437=CARTESIAN_POINT('Ctrl Pts',(-3.26221017892137,15.2,-10.2738823411271));
#291438=CARTESIAN_POINT('Ctrl Pts',(-3.26416546102469,15.2,-10.2767638340902));
#291439=CARTESIAN_POINT('Ctrl Pts',(-3.26660956385364,15.2,-10.2803657005886));
#291440=CARTESIAN_POINT('Ctrl Pts',(-3.26907531174968,15.2,-10.283982975941));
#291441=CARTESIAN_POINT('Ctrl Pts',(-3.27156272605412,15.2,-10.2876153614958));
#291442=CARTESIAN_POINT('Ctrl Pts',(-3.27355265760613,15.2,-10.290521270098));
#291443=CARTESIAN_POINT('Ctrl Pts',(-3.27555645564032,15.2,-10.2934368496847));
#291444=CARTESIAN_POINT('Ctrl Pts',(-3.27757412914008,15.2,-10.2963619489559));
#291445=CARTESIAN_POINT('Ctrl Pts',(-3.27959180236493,15.2,-10.2992870478285));
#291446=CARTESIAN_POINT('Ctrl Pts',(-3.28162335029173,15.2,-10.3022216665117));
#291447=CARTESIAN_POINT('Ctrl Pts',(-3.28366878300327,15.2,-10.3051656563062));
#291448=CARTESIAN_POINT('Ctrl Pts',(-3.28571421599351,15.2,-10.3081096465018));
#291449=CARTESIAN_POINT('Ctrl Pts',(-3.28777353306405,15.2,-10.311063007883));
#291450=CARTESIAN_POINT('Ctrl Pts',(-3.28984674267795,15.2,-10.3140255917673));
#291451=CARTESIAN_POINT('Ctrl Pts',(-3.29191995200937,15.2,-10.3169881752479));
#291452=CARTESIAN_POINT('Ctrl Pts',(-3.29400705495745,15.2,-10.3199599823489));
#291453=CARTESIAN_POINT('Ctrl Pts',(-3.29610805867316,15.2,-10.3229408652709));
#291454=CARTESIAN_POINT('Ctrl Pts',(-3.29820906267513,15.2,-10.3259217485991));
#291455=CARTESIAN_POINT('Ctrl Pts',(-3.30032396540905,15.2,-10.3289117075305));
#291456=CARTESIAN_POINT('Ctrl Pts',(-3.30245277753479,15.2,-10.3319105994854));
#291457=CARTESIAN_POINT('Ctrl Pts',(-3.30458158937047,15.2,-10.3349094910316));
#291458=CARTESIAN_POINT('Ctrl Pts',(-3.30672430854734,15.2,-10.3379173133626));
#291459=CARTESIAN_POINT('Ctrl Pts',(-3.3088809431474,15.2,-10.3409339242818));
#291460=CARTESIAN_POINT('Ctrl Pts',(-3.3110375780413,15.2,-10.343950535612));
#291461=CARTESIAN_POINT('Ctrl Pts',(-3.31320812668095,15.2,-10.3469759351763));
#291462=CARTESIAN_POINT('Ctrl Pts',(-3.31539259746666,15.2,-10.3500099805083));
#291463=CARTESIAN_POINT('Ctrl Pts',(-3.31757706825238,15.2,-10.3530440258403));
#291464=CARTESIAN_POINT('Ctrl Pts',(-3.31977546047584,15.2,-10.3560867182011));
#291465=CARTESIAN_POINT('Ctrl Pts',(-3.32198777932005,15.2,-10.3591379144239));
#291466=CARTESIAN_POINT('Ctrl Pts',(-3.32420009786284,15.2,-10.3621891102308));
#291467=CARTESIAN_POINT('Ctrl Pts',(-3.32642634335759,15.2,-10.365248813332));
#291468=CARTESIAN_POINT('Ctrl Pts',(-3.32866652124014,15.2,-10.3683168810396));
#291469=CARTESIAN_POINT('Ctrl Pts',(-3.33090669942791,15.2,-10.3713849491651));
#291470=CARTESIAN_POINT('Ctrl Pts',(-3.33316081086247,15.2,-10.3744613824381));
#291471=CARTESIAN_POINT('Ctrl Pts',(-3.33542885965417,15.2,-10.377546044996));
#291472=CARTESIAN_POINT('Ctrl Pts',(-3.33769690813684,15.2,-10.3806307071335));
#291473=CARTESIAN_POINT('Ctrl Pts',(-3.33997889333993,15.2,-10.3837235966645));
#291474=CARTESIAN_POINT('Ctrl Pts',(-3.34227482059578,15.2,-10.3868245770216));
#291475=CARTESIAN_POINT('Ctrl Pts',(-3.3451447299002,15.2,-10.3907008027848));
#291476=CARTESIAN_POINT('Ctrl Pts',(-3.34803642425746,15.2,-10.3945896701079));
#291477=CARTESIAN_POINT('Ctrl Pts',(-3.35094991017342,15.2,-10.3984909165145));
#291478=CARTESIAN_POINT('Ctrl Pts',(-3.35328069903322,15.2,-10.4016119138099));
#291479=CARTESIAN_POINT('Ctrl Pts',(-3.35562543579456,15.2,-10.4047408317383));
#291480=CARTESIAN_POINT('Ctrl Pts',(-3.35798412136899,15.2,-10.4078775385212));
#291481=CARTESIAN_POINT('Ctrl Pts',(-3.36034280662204,15.2,-10.4110142448766));
#291482=CARTESIAN_POINT('Ctrl Pts',(-3.36271544412326,15.2,-10.4141587378617));
#291483=CARTESIAN_POINT('Ctrl Pts',(-3.36510203403836,15.2,-10.4173108874924));
#291484=CARTESIAN_POINT('Ctrl Pts',(-3.36748862427863,15.2,-10.4204630375525));
#291485=CARTESIAN_POINT('Ctrl Pts',(-3.36988916764422,15.2,-10.4236228418392));
#291486=CARTESIAN_POINT('Ctrl Pts',(-3.3723036678421,15.2,-10.4267901707263));
#291487=CARTESIAN_POINT('Ctrl Pts',(-3.37471816771101,15.2,-10.4299574991818));
#291488=CARTESIAN_POINT('Ctrl Pts',(-3.37714662323717,15.2,-10.43313235052));
#291489=CARTESIAN_POINT('Ctrl Pts',(-3.37958903709213,15.2,-10.4363145949816));
#291490=CARTESIAN_POINT('Ctrl Pts',(-3.38203145127987,15.2,-10.4394968398767));
#291491=CARTESIAN_POINT('Ctrl Pts',(-3.38448782419709,15.2,-10.44268647887));
#291492=CARTESIAN_POINT('Ctrl Pts',(-3.38695815694375,15.2,-10.4458833817114));
#291493=CARTESIAN_POINT('Ctrl Pts',(-3.38942848935382,15.2,-10.4490802841172));
#291494=CARTESIAN_POINT('Ctrl Pts',(-3.39191278094997,15.2,-10.4522844503465));
#291495=CARTESIAN_POINT('Ctrl Pts',(-3.39441103479988,15.2,-10.4554957532499));
#291496=CARTESIAN_POINT('Ctrl Pts',(-3.39690928899017,15.2,-10.4587070565909));
#291497=CARTESIAN_POINT('Ctrl Pts',(-3.39942150561919,15.2,-10.4619254946006));
#291498=CARTESIAN_POINT('Ctrl Pts',(-3.40194768376839,15.2,-10.4651509422355));
#291499=CARTESIAN_POINT('Ctrl Pts',(-3.4044738615734,15.2,-10.468376389431));
#291500=CARTESIAN_POINT('Ctrl Pts',(-3.40701400162874,15.2,-10.4716088474942));
#291501=CARTESIAN_POINT('Ctrl Pts',(-3.40956810480741,15.2,-10.4748481867287));
#291502=CARTESIAN_POINT('Ctrl Pts',(-3.41212220833408,15.2,-10.4780875264045));
#291503=CARTESIAN_POINT('Ctrl Pts',(-3.41469027602872,15.2,-10.4813337501227));
#291504=CARTESIAN_POINT('Ctrl Pts',(-3.41727230555833,15.2,-10.4845867329667));
#291505=CARTESIAN_POINT('Ctrl Pts',(-3.42049984229445,15.2,-10.4886529613));
#291506=CARTESIAN_POINT('Ctrl Pts',(-3.42374919592019,15.2,-10.4927297492725));
#291507=CARTESIAN_POINT('Ctrl Pts',(-3.42702036822679,15.2,-10.4968168560272));
#291508=CARTESIAN_POINT('Ctrl Pts',(-3.42963730585813,15.2,-10.5000865411637));
#291509=CARTESIAN_POINT('Ctrl Pts',(-3.43226820610188,15.2,-10.5033628310851));
#291510=CARTESIAN_POINT('Ctrl Pts',(-3.43491306855091,15.2,-10.5066456022049));
#291511=CARTESIAN_POINT('Ctrl Pts',(-3.4375579313603,15.2,-10.5099283737721));
#291512=CARTESIAN_POINT('Ctrl Pts',(-3.44021675605433,15.2,-10.5132176282981));
#291513=CARTESIAN_POINT('Ctrl Pts',(-3.4428895422,15.2,-10.5165132420333));
#291514=CARTESIAN_POINT('Ctrl Pts',(-3.44556232834566,15.2,-10.5198088557685));
#291515=CARTESIAN_POINT('Ctrl Pts',(-3.44824907580407,15.2,-10.5231108306461));
#291516=CARTESIAN_POINT('Ctrl Pts',(-3.45094978317491,15.2,-10.5264190455492));
#291517=CARTESIAN_POINT('Ctrl Pts',(-3.45365049017777,15.2,-10.5297272600016));
#291518=CARTESIAN_POINT('Ctrl Pts',(-3.45636515587275,15.2,-10.5330417151263));
#291519=CARTESIAN_POINT('Ctrl Pts',(-3.45909378027315,15.2,-10.5363622909811));
#291520=CARTESIAN_POINT('Ctrl Pts',(-3.46250456105248,15.2,-10.5405130111388));
#291521=CARTESIAN_POINT('Ctrl Pts',(-3.46593715146666,15.2,-10.5446732956555));
#291522=CARTESIAN_POINT('Ctrl Pts',(-3.46939154646666,15.2,-10.548842913225));
#291523=CARTESIAN_POINT('Ctrl Pts',(-3.47215506261727,15.2,-10.5521786074623));
#291524=CARTESIAN_POINT('Ctrl Pts',(-3.47493253425562,15.2,-10.5555202747032));
#291525=CARTESIAN_POINT('Ctrl Pts',(-3.47772395846474,15.2,-10.5588677983306));
#291526=CARTESIAN_POINT('Ctrl Pts',(-3.48051538229352,15.2,-10.562215321502));
#291527=CARTESIAN_POINT('Ctrl Pts',(-3.48332075898246,15.2,-10.5655687009987));
#291528=CARTESIAN_POINT('Ctrl Pts',(-3.48614008476475,15.2,-10.5689278202394));
#291529=CARTESIAN_POINT('Ctrl Pts',(-3.48895941093117,15.2,-10.5722869399377));
#291530=CARTESIAN_POINT('Ctrl Pts',(-3.49179268780338,15.2,-10.5756518002418));
#291531=CARTESIAN_POINT('Ctrl Pts',(-3.49463991118219,15.2,-10.5790222852594));
#291532=CARTESIAN_POINT('Ctrl Pts',(-3.49748713417307,15.2,-10.5823927698178));
#291533=CARTESIAN_POINT('Ctrl Pts',(-3.50034830246771,15.2,-10.585768880131));
#291534=CARTESIAN_POINT('Ctrl Pts',(-3.50322341423176,15.2,-10.5891504994653));
#291535=CARTESIAN_POINT('Ctrl Pts',(-3.50537974815274,15.2,-10.5916867140812));
#291536=CARTESIAN_POINT('Ctrl Pts',(-3.50754392576783,15.2,-10.5942260293405));
#291537=CARTESIAN_POINT('Ctrl Pts',(-3.50971594333818,15.2,-10.5967683964581));
#291538=CARTESIAN_POINT('Ctrl Pts',(-3.51333597275363,15.2,-10.6010056751415));
#291539=CARTESIAN_POINT('Ctrl Pts',(-3.5169777843839,15.2,-10.6052514312112));
#291540=CARTESIAN_POINT('Ctrl Pts',(-3.52064136924387,15.2,-10.6095054439885));
#291541=CARTESIAN_POINT('Ctrl Pts',(-3.52283952007998,15.2,-10.6120578515622));
#291542=CARTESIAN_POINT('Ctrl Pts',(-3.5250455086489,15.2,-10.6146132324356));
#291543=CARTESIAN_POINT('Ctrl Pts',(-3.52725933352573,15.2,-10.617171538509));
#291544=CARTESIAN_POINT('Ctrl Pts',(-3.52947315880474,15.2,-10.619729845047));
#291545=CARTESIAN_POINT('Ctrl Pts',(-3.53169482021096,15.2,-10.6222910772359));
#291546=CARTESIAN_POINT('Ctrl Pts',(-3.5339243164527,15.2,-10.6248551883173));
#291547=CARTESIAN_POINT('Ctrl Pts',(-3.53764014257722,15.2,-10.6291287056994));
#291548=CARTESIAN_POINT('Ctrl Pts',(-3.54137773184761,15.2,-10.6334102200849));
#291549=CARTESIAN_POINT('Ctrl Pts',(-3.54513707074162,15.2,-10.6376995164223));
#291550=CARTESIAN_POINT('Ctrl Pts',(-3.5473926746517,15.2,-10.6402730948793));
#291551=CARTESIAN_POINT('Ctrl Pts',(-3.54965611064733,15.2,-10.6428494740537));
#291552=CARTESIAN_POINT('Ctrl Pts',(-3.55192737402014,15.2,-10.6454286085956));
#291553=CARTESIAN_POINT('Ctrl Pts',(-3.55495572449621,15.2,-10.6488674538705));
#291554=CARTESIAN_POINT('Ctrl Pts',(-3.55799799235659,15.2,-10.6523111984448));
#291555=CARTESIAN_POINT('Ctrl Pts',(-3.56105417255029,15.2,-10.6557597317181));
#291556=CARTESIAN_POINT('Ctrl Pts',(-3.56334630779966,15.2,-10.6583461317906));
#291557=CARTESIAN_POINT('Ctrl Pts',(-3.56564626713971,15.2,-10.6609352257969));
#291558=CARTESIAN_POINT('Ctrl Pts',(-3.56795405008691,15.2,-10.6635269689986));
#291559=CARTESIAN_POINT('Ctrl Pts',(-3.57026183303412,15.2,-10.6661187122003));
#291560=CARTESIAN_POINT('Ctrl Pts',(-3.57257743817898,15.2,-10.6687131048619));
#291561=CARTESIAN_POINT('Ctrl Pts',(-3.5749008639685,15.2,-10.6713100999755));
#291562=CARTESIAN_POINT('Ctrl Pts',(-3.57722429018012,15.2,-10.6739070955609));
#291563=CARTESIAN_POINT('Ctrl Pts',(-3.57955553533558,15.2,-10.6765066947887));
#291564=CARTESIAN_POINT('Ctrl Pts',(-3.58189459950992,15.2,-10.6791088528339));
#291565=CARTESIAN_POINT('Ctrl Pts',(-3.58423366325934,15.2,-10.6817110104064));
#291566=CARTESIAN_POINT('Ctrl Pts',(-3.586580543325,15.2,-10.6843157259287));
#291567=CARTESIAN_POINT('Ctrl Pts',(-3.58893523819846,15.2,-10.6869229555009));
#291568=CARTESIAN_POINT('Ctrl Pts',(-3.59128993307192,15.2,-10.689530185073));
#291569=CARTESIAN_POINT('Ctrl Pts',(-3.59365244339414,15.2,-10.6921399284354));
#291570=CARTESIAN_POINT('Ctrl Pts',(-3.59602276477716,15.2,-10.694752141519));
#291571=CARTESIAN_POINT('Ctrl Pts',(-3.59839308616017,15.2,-10.6973643546027));
#291572=CARTESIAN_POINT('Ctrl Pts',(-3.60077121980706,15.2,-10.6999790372975));
#291573=CARTESIAN_POINT('Ctrl Pts',(-3.60315716127284,15.2,-10.7025961444643));
#291574=CARTESIAN_POINT('Ctrl Pts',(-3.60554310273861,15.2,-10.7052132516311));
#291575=CARTESIAN_POINT('Ctrl Pts',(-3.60793685412629,15.2,-10.7078327841097));
#291576=CARTESIAN_POINT('Ctrl Pts',(-3.61033841049669,15.2,-10.7104546981392));
#291577=CARTESIAN_POINT('Ctrl Pts',(-3.6127399668671,15.2,-10.7130766121688));
#291578=CARTESIAN_POINT('Ctrl Pts',(-3.61514932837862,15.2,-10.7157009066398));
#291579=CARTESIAN_POINT('Ctrl Pts',(-3.61756649274807,15.2,-10.7183275391691));
#291580=CARTESIAN_POINT('Ctrl Pts',(-3.61998365755664,15.2,-10.7209541721755));
#291581=CARTESIAN_POINT('Ctrl Pts',(-3.62240862492572,15.2,-10.7235831425075));
#291582=CARTESIAN_POINT('Ctrl Pts',(-3.62484139173869,15.2,-10.7262144070569));
#291583=CARTESIAN_POINT('Ctrl Pts',(-3.62808508008606,15.2,-10.7297227589928));
#291584=CARTESIAN_POINT('Ctrl Pts',(-3.63134263357882,15.2,-10.7332351875448));
#291585=CARTESIAN_POINT('Ctrl Pts',(-3.6346140445327,15.2,-10.7367515934792));
#291586=CARTESIAN_POINT('Ctrl Pts',(-3.63706760285953,15.2,-10.7393888980499));
#291587=CARTESIAN_POINT('Ctrl Pts',(-3.6395289557563,15.2,-10.7420284399032));
#291588=CARTESIAN_POINT('Ctrl Pts',(-3.64199810024736,15.2,-10.7446701737722));
#291589=CARTESIAN_POINT('Ctrl Pts',(-3.64446724473843,15.2,-10.7473119076413));
#291590=CARTESIAN_POINT('Ctrl Pts',(-3.64694418066634,15.2,-10.7499558357196));
#291591=CARTESIAN_POINT('Ctrl Pts',(-3.64942890445001,15.2,-10.7526019139148));
#291592=CARTESIAN_POINT('Ctrl Pts',(-3.65191362868507,15.2,-10.7552479925908));
#291593=CARTESIAN_POINT('Ctrl Pts',(-3.65440613983063,15.2,-10.7578962227423));
#291594=CARTESIAN_POINT('Ctrl Pts',(-3.65690643602841,15.2,-10.7605465608361));
#291595=CARTESIAN_POINT('Ctrl Pts',(-3.65940673177196,15.2,-10.7631968984484));
#291596=CARTESIAN_POINT('Ctrl Pts',(-3.66191481129844,15.2,-10.765849343669));
#291597=CARTESIAN_POINT('Ctrl Pts',(-3.66443067158269,15.2,-10.768503855781));
#291598=CARTESIAN_POINT('Ctrl Pts',(-3.66694653186695,15.2,-10.7711583678931));
#291599=CARTESIAN_POINT('Ctrl Pts',(-3.66947017189941,15.2,-10.7738149468703));
#291600=CARTESIAN_POINT('Ctrl Pts',(-3.67200158923564,15.2,-10.7764735490357));
#291601=CARTESIAN_POINT('Ctrl Pts',(-3.67453300657186,15.2,-10.7791321512012));
#291602=CARTESIAN_POINT('Ctrl Pts',(-3.67707220089537,15.2,-10.7817927773989));
#291603=CARTESIAN_POINT('Ctrl Pts',(-3.67961916727269,15.2,-10.7844553864809));
#291604=CARTESIAN_POINT('Ctrl Pts',(-3.68216613365002,15.2,-10.7871179955629));
#291605=CARTESIAN_POINT('Ctrl Pts',(-3.68472087314793,15.2,-10.7897825860231));
#291606=CARTESIAN_POINT('Ctrl Pts',(-3.68728338147082,15.2,-10.7924491172177));
#291607=CARTESIAN_POINT('Ctrl Pts',(-3.68984588979371,15.2,-10.7951156484123));
#291608=CARTESIAN_POINT('Ctrl Pts',(-3.69241616663272,15.2,-10.7977841214985));
#291609=CARTESIAN_POINT('Ctrl Pts',(-3.69499420845467,15.2,-10.8004544941512));
#291610=CARTESIAN_POINT('Ctrl Pts',(-3.69843159786283,15.2,-10.8040149913449));
#291611=CARTESIAN_POINT('Ctrl Pts',(-3.70188279176162,15.2,-10.8075788666085));
#291612=CARTESIAN_POINT('Ctrl Pts',(-3.70534777924403,15.2,-10.8111460204858));
#291613=CARTESIAN_POINT('Ctrl Pts',(-3.70794651961979,15.2,-10.8138213856507));
#291614=CARTESIAN_POINT('Ctrl Pts',(-3.71055301989745,15.2,-10.8164985952827));
#291615=CARTESIAN_POINT('Ctrl Pts',(-3.71316727427263,15.2,-10.8191776064892));
#291616=CARTESIAN_POINT('Ctrl Pts',(-3.71578152864781,15.2,-10.8218566176957));
#291617=CARTESIAN_POINT('Ctrl Pts',(-3.71840353845971,15.2,-10.8245374306719));
#291618=CARTESIAN_POINT('Ctrl Pts',(-3.72103329923849,15.2,-10.8272200094076));
#291619=CARTESIAN_POINT('Ctrl Pts',(-3.72366306001727,15.2,-10.8299025881434));
#291620=CARTESIAN_POINT('Ctrl Pts',(-3.72630057117052,15.2,-10.8325869338123));
#291621=CARTESIAN_POINT('Ctrl Pts',(-3.72894582899001,15.2,-10.8352730049228));
#291622=CARTESIAN_POINT('Ctrl Pts',(-3.73159108729005,15.2,-10.8379590765212));
#291623=CARTESIAN_POINT('Ctrl Pts',(-3.73424409222563,15.2,-10.8406468748952));
#291624=CARTESIAN_POINT('Ctrl Pts',(-3.73690483861338,15.2,-10.8433363508696));
#291625=CARTESIAN_POINT('Ctrl Pts',(-3.73956558451777,15.2,-10.8460258263555));
#291626=CARTESIAN_POINT('Ctrl Pts',(-3.7422340726805,15.2,-10.8487169781341));
#291627=CARTESIAN_POINT('Ctrl Pts',(-3.74491029621786,15.2,-10.8514097635877));
#291628=CARTESIAN_POINT('Ctrl Pts',(-3.74758651975522,15.2,-10.8541025490412));
#291629=CARTESIAN_POINT('Ctrl Pts',(-3.75027047927055,15.2,-10.8567969667966));
#291630=CARTESIAN_POINT('Ctrl Pts',(-3.75296217351105,15.2,-10.8594930000052));
#291631=CARTESIAN_POINT('Ctrl Pts',(-3.75565386775154,15.2,-10.8621890332137));
#291632=CARTESIAN_POINT('Ctrl Pts',(-3.75835329800824,15.2,-10.8648866810023));
#291633=CARTESIAN_POINT('Ctrl Pts',(-3.76106045600006,15.2,-10.867585944));
#291634=CARTESIAN_POINT('Ctrl Pts',(-4.04260911700006,15.2,-9.55499537100001));
#291635=CARTESIAN_POINT('Ctrl Pts',(-4.04260911700006,11.6,-9.55499537100001));
#291636=CARTESIAN_POINT('Ctrl Pts',(-4.04266300400006,15.2,-9.55516119200002));
#291637=CARTESIAN_POINT('Ctrl Pts',(-4.04266300400006,11.6,-9.55516119200002));
#291638=CARTESIAN_POINT('Ctrl Pts',(-4.04277258000006,15.2,-9.55549865500002));
#291639=CARTESIAN_POINT('Ctrl Pts',(-4.04277258000006,11.6,-9.55549865500002));
#291640=CARTESIAN_POINT('Ctrl Pts',(-4.04293835900006,15.2,-9.55601007100002));
#291641=CARTESIAN_POINT('Ctrl Pts',(-4.04293835900006,11.6,-9.55601007100002));
#291642=CARTESIAN_POINT('Ctrl Pts',(-4.04316116500006,15.2,-9.55669916200002));
#291643=CARTESIAN_POINT('Ctrl Pts',(-4.04316116500006,11.6,-9.55669916200002));
#291644=CARTESIAN_POINT('Ctrl Pts',(-4.04344211400006,15.2,-9.55757104100002));
#291645=CARTESIAN_POINT('Ctrl Pts',(-4.04344211400006,11.6,-9.55757104100002));
#291646=CARTESIAN_POINT('Ctrl Pts',(-4.04372672500006,15.2,-9.55845733800002));
#291647=CARTESIAN_POINT('Ctrl Pts',(-4.04372672500006,11.6,-9.55845733800002));
#291648=CARTESIAN_POINT('Ctrl Pts',(-4.04401334900006,15.2,-9.55935298200002));
#291649=CARTESIAN_POINT('Ctrl Pts',(-4.04401334900006,11.6,-9.55935298200002));
#291650=CARTESIAN_POINT('Ctrl Pts',(-4.04430195600006,15.2,-9.56025795100001));
#291651=CARTESIAN_POINT('Ctrl Pts',(-4.04430195600006,11.6,-9.56025795100001));
#291652=CARTESIAN_POINT('Ctrl Pts',(-4.04459252500006,15.2,-9.56117222800002));
#291653=CARTESIAN_POINT('Ctrl Pts',(-4.04459252500006,11.6,-9.56117222800002));
#291654=CARTESIAN_POINT('Ctrl Pts',(-4.04488502600006,15.2,-9.56209579100002));
#291655=CARTESIAN_POINT('Ctrl Pts',(-4.04488502600006,11.6,-9.56209579100002));
#291656=CARTESIAN_POINT('Ctrl Pts',(-4.04517943800006,15.2,-9.56302862000001));
#291657=CARTESIAN_POINT('Ctrl Pts',(-4.04517943800006,11.6,-9.56302862000001));
#291658=CARTESIAN_POINT('Ctrl Pts',(-4.04547573400006,15.2,-9.56397069600002));
#291659=CARTESIAN_POINT('Ctrl Pts',(-4.04547573400006,11.6,-9.56397069600002));
#291660=CARTESIAN_POINT('Ctrl Pts',(-4.04577389000006,15.2,-9.56492199900002));
#291661=CARTESIAN_POINT('Ctrl Pts',(-4.04577389000006,11.6,-9.56492199900002));
#291662=CARTESIAN_POINT('Ctrl Pts',(-4.04607388100006,15.2,-9.56588250900002));
#291663=CARTESIAN_POINT('Ctrl Pts',(-4.04607388100006,11.6,-9.56588250900002));
#291664=CARTESIAN_POINT('Ctrl Pts',(-4.04637568200005,15.2,-9.56685220700002));
#291665=CARTESIAN_POINT('Ctrl Pts',(-4.04637568200005,11.6,-9.56685220700002));
#291666=CARTESIAN_POINT('Ctrl Pts',(-4.04667926900006,15.2,-9.56783107300001));
#291667=CARTESIAN_POINT('Ctrl Pts',(-4.04667926900006,11.6,-9.56783107300001));
#291668=CARTESIAN_POINT('Ctrl Pts',(-4.04698461700006,15.2,-9.56881908900002));
#291669=CARTESIAN_POINT('Ctrl Pts',(-4.04698461700006,11.6,-9.56881908900002));
#291670=CARTESIAN_POINT('Ctrl Pts',(-4.04729170300006,15.2,-9.56981623200001));
#291671=CARTESIAN_POINT('Ctrl Pts',(-4.04729170300006,11.6,-9.56981623200001));
#291672=CARTESIAN_POINT('Ctrl Pts',(-4.04760050200006,15.2,-9.57082248800001));
#291673=CARTESIAN_POINT('Ctrl Pts',(-4.04760050200006,11.6,-9.57082248800001));
#291674=CARTESIAN_POINT('Ctrl Pts',(-4.04791099000006,15.2,-9.57183783400002));
#291675=CARTESIAN_POINT('Ctrl Pts',(-4.04791099000006,11.6,-9.57183783400002));
#291676=CARTESIAN_POINT('Ctrl Pts',(-4.04822314400006,15.2,-9.57286225100002));
#291677=CARTESIAN_POINT('Ctrl Pts',(-4.04822314400006,11.6,-9.57286225100002));
#291678=CARTESIAN_POINT('Ctrl Pts',(-4.04853693900006,15.2,-9.57389572300002));
#291679=CARTESIAN_POINT('Ctrl Pts',(-4.04853693900006,11.6,-9.57389572300002));
#291680=CARTESIAN_POINT('Ctrl Pts',(-4.04885235200005,15.2,-9.57493822800001));
#291681=CARTESIAN_POINT('Ctrl Pts',(-4.04885235200005,11.6,-9.57493822800001));
#291682=CARTESIAN_POINT('Ctrl Pts',(-4.04916936000006,15.2,-9.57598974800002));
#291683=CARTESIAN_POINT('Ctrl Pts',(-4.04916936000006,11.6,-9.57598974800002));
#291684=CARTESIAN_POINT('Ctrl Pts',(-4.04948794000005,15.2,-9.57705026500001));
#291685=CARTESIAN_POINT('Ctrl Pts',(-4.04948794000005,11.6,-9.57705026500001));
#291686=CARTESIAN_POINT('Ctrl Pts',(-4.04980806700006,15.2,-9.57811976000002));
#291687=CARTESIAN_POINT('Ctrl Pts',(-4.04980806700006,11.6,-9.57811976000002));
#291688=CARTESIAN_POINT('Ctrl Pts',(-4.05012971900006,15.2,-9.57919821400001));
#291689=CARTESIAN_POINT('Ctrl Pts',(-4.05012971900006,11.6,-9.57919821400001));
#291690=CARTESIAN_POINT('Ctrl Pts',(-4.05045287300006,15.2,-9.58028560900001));
#291691=CARTESIAN_POINT('Ctrl Pts',(-4.05045287300006,11.6,-9.58028560900001));
#291692=CARTESIAN_POINT('Ctrl Pts',(-4.05077750600006,15.2,-9.58138192600002));
#291693=CARTESIAN_POINT('Ctrl Pts',(-4.05077750600006,11.6,-9.58138192600002));
#291694=CARTESIAN_POINT('Ctrl Pts',(-4.05110359500005,15.2,-9.58248714700002));
#291695=CARTESIAN_POINT('Ctrl Pts',(-4.05110359500005,11.6,-9.58248714700002));
#291696=CARTESIAN_POINT('Ctrl Pts',(-4.05143111900006,15.2,-9.58360125300001));
#291697=CARTESIAN_POINT('Ctrl Pts',(-4.05143111900006,11.6,-9.58360125300001));
#291698=CARTESIAN_POINT('Ctrl Pts',(-4.05176005200006,15.2,-9.58472422800002));
#291699=CARTESIAN_POINT('Ctrl Pts',(-4.05176005200006,11.6,-9.58472422800002));
#291700=CARTESIAN_POINT('Ctrl Pts',(-4.05209037500006,15.2,-9.58585605000002));
#291701=CARTESIAN_POINT('Ctrl Pts',(-4.05209037500006,11.6,-9.58585605000002));
#291702=CARTESIAN_POINT('Ctrl Pts',(-4.05242206400006,15.2,-9.58699670600001));
#291703=CARTESIAN_POINT('Ctrl Pts',(-4.05242206400006,11.6,-9.58699670600001));
#291704=CARTESIAN_POINT('Ctrl Pts',(-4.05275509600005,15.2,-9.58814617300002));
#291705=CARTESIAN_POINT('Ctrl Pts',(-4.05275509600005,11.6,-9.58814617300002));
#291706=CARTESIAN_POINT('Ctrl Pts',(-4.05308945100006,15.2,-9.58930443500002));
#291707=CARTESIAN_POINT('Ctrl Pts',(-4.05308945100006,11.6,-9.58930443500002));
#291708=CARTESIAN_POINT('Ctrl Pts',(-4.05342510700006,15.2,-9.59047147500002));
#291709=CARTESIAN_POINT('Ctrl Pts',(-4.05342510700006,11.6,-9.59047147500002));
#291710=CARTESIAN_POINT('Ctrl Pts',(-4.05376204000006,15.2,-9.59164727400001));
#291711=CARTESIAN_POINT('Ctrl Pts',(-4.05376204000006,11.6,-9.59164727400001));
#291712=CARTESIAN_POINT('Ctrl Pts',(-4.05410023000006,15.2,-9.59283181500002));
#291713=CARTESIAN_POINT('Ctrl Pts',(-4.05410023000006,11.6,-9.59283181500002));
#291714=CARTESIAN_POINT('Ctrl Pts',(-4.05443965400006,15.2,-9.59402508100002));
#291715=CARTESIAN_POINT('Ctrl Pts',(-4.05443965400006,11.6,-9.59402508100002));
#291716=CARTESIAN_POINT('Ctrl Pts',(-4.05478029100006,15.2,-9.59522705200002));
#291717=CARTESIAN_POINT('Ctrl Pts',(-4.05478029100006,11.6,-9.59522705200002));
#291718=CARTESIAN_POINT('Ctrl Pts',(-4.05512211900006,15.2,-9.59643771300002));
#291719=CARTESIAN_POINT('Ctrl Pts',(-4.05512211900006,11.6,-9.59643771300002));
#291720=CARTESIAN_POINT('Ctrl Pts',(-4.05546511900006,15.2,-9.59765704600001));
#291721=CARTESIAN_POINT('Ctrl Pts',(-4.05546511900006,11.6,-9.59765704600001));
#291722=CARTESIAN_POINT('Ctrl Pts',(-4.05580926700006,15.2,-9.59888503200002));
#291723=CARTESIAN_POINT('Ctrl Pts',(-4.05580926700006,11.6,-9.59888503200002));
#291724=CARTESIAN_POINT('Ctrl Pts',(-4.05615454400006,15.2,-9.60012165500002));
#291725=CARTESIAN_POINT('Ctrl Pts',(-4.05615454400006,11.6,-9.60012165500002));
#291726=CARTESIAN_POINT('Ctrl Pts',(-4.05650092700006,15.2,-9.60136689800001));
#291727=CARTESIAN_POINT('Ctrl Pts',(-4.05650092700006,11.6,-9.60136689800001));
#291728=CARTESIAN_POINT('Ctrl Pts',(-4.05684839700006,15.2,-9.60262074300001));
#291729=CARTESIAN_POINT('Ctrl Pts',(-4.05684839700006,11.6,-9.60262074300001));
#291730=CARTESIAN_POINT('Ctrl Pts',(-4.05719693100006,15.2,-9.60388317400002));
#291731=CARTESIAN_POINT('Ctrl Pts',(-4.05719693100006,11.6,-9.60388317400002));
#291732=CARTESIAN_POINT('Ctrl Pts',(-4.05754650900006,15.2,-9.60515417200002));
#291733=CARTESIAN_POINT('Ctrl Pts',(-4.05754650900006,11.6,-9.60515417200002));
#291734=CARTESIAN_POINT('Ctrl Pts',(-4.05789711200006,15.2,-9.60643372300002));
#291735=CARTESIAN_POINT('Ctrl Pts',(-4.05789711200006,11.6,-9.60643372300002));
#291736=CARTESIAN_POINT('Ctrl Pts',(-4.05824871700006,15.2,-9.60772180700001));
#291737=CARTESIAN_POINT('Ctrl Pts',(-4.05824871700006,11.6,-9.60772180700001));
#291738=CARTESIAN_POINT('Ctrl Pts',(-4.05860130600006,15.2,-9.60901840800001));
#291739=CARTESIAN_POINT('Ctrl Pts',(-4.05860130600006,11.6,-9.60901840800001));
#291740=CARTESIAN_POINT('Ctrl Pts',(-4.05895485700006,15.2,-9.61032351000001));
#291741=CARTESIAN_POINT('Ctrl Pts',(-4.05895485700006,11.6,-9.61032351000001));
#291742=CARTESIAN_POINT('Ctrl Pts',(-4.05930934900006,15.2,-9.61163709600001));
#291743=CARTESIAN_POINT('Ctrl Pts',(-4.05930934900006,11.6,-9.61163709600001));
#291744=CARTESIAN_POINT('Ctrl Pts',(-4.05966476500006,15.2,-9.61295914900001));
#291745=CARTESIAN_POINT('Ctrl Pts',(-4.05966476500006,11.6,-9.61295914900001));
#291746=CARTESIAN_POINT('Ctrl Pts',(-4.06002108100005,15.2,-9.61428965300002));
#291747=CARTESIAN_POINT('Ctrl Pts',(-4.06002108100005,11.6,-9.61428965300002));
#291748=CARTESIAN_POINT('Ctrl Pts',(-4.06037827900006,15.2,-9.61562859000002));
#291749=CARTESIAN_POINT('Ctrl Pts',(-4.06037827900006,11.6,-9.61562859000002));
#291750=CARTESIAN_POINT('Ctrl Pts',(-4.06073634000006,15.2,-9.61697594500002));
#291751=CARTESIAN_POINT('Ctrl Pts',(-4.06073634000006,11.6,-9.61697594500002));
#291752=CARTESIAN_POINT('Ctrl Pts',(-4.06109524300006,15.2,-9.61833170100002));
#291753=CARTESIAN_POINT('Ctrl Pts',(-4.06109524300006,11.6,-9.61833170100002));
#291754=CARTESIAN_POINT('Ctrl Pts',(-4.06145496900006,15.2,-9.61969584100002));
#291755=CARTESIAN_POINT('Ctrl Pts',(-4.06145496900006,11.6,-9.61969584100002));
#291756=CARTESIAN_POINT('Ctrl Pts',(-4.06181549800006,15.2,-9.62106835000002));
#291757=CARTESIAN_POINT('Ctrl Pts',(-4.06181549800006,11.6,-9.62106835000002));
#291758=CARTESIAN_POINT('Ctrl Pts',(-4.06217680900006,15.2,-9.62244921100002));
#291759=CARTESIAN_POINT('Ctrl Pts',(-4.06217680900006,11.6,-9.62244921100002));
#291760=CARTESIAN_POINT('Ctrl Pts',(-4.06253888500006,15.2,-9.62383840700002));
#291761=CARTESIAN_POINT('Ctrl Pts',(-4.06253888500006,11.6,-9.62383840700002));
#291762=CARTESIAN_POINT('Ctrl Pts',(-4.06290170600006,15.2,-9.62523592300002));
#291763=CARTESIAN_POINT('Ctrl Pts',(-4.06290170600006,11.6,-9.62523592300002));
#291764=CARTESIAN_POINT('Ctrl Pts',(-4.06326525200006,15.2,-9.62664174300001));
#291765=CARTESIAN_POINT('Ctrl Pts',(-4.06326525200006,11.6,-9.62664174300001));
#291766=CARTESIAN_POINT('Ctrl Pts',(-4.06362950500006,15.2,-9.62805584900002));
#291767=CARTESIAN_POINT('Ctrl Pts',(-4.06362950500006,11.6,-9.62805584900002));
#291768=CARTESIAN_POINT('Ctrl Pts',(-4.06399444400006,15.2,-9.62947822800002));
#291769=CARTESIAN_POINT('Ctrl Pts',(-4.06399444400006,11.6,-9.62947822800002));
#291770=CARTESIAN_POINT('Ctrl Pts',(-4.06436005300006,15.2,-9.63090886200002));
#291771=CARTESIAN_POINT('Ctrl Pts',(-4.06436005300006,11.6,-9.63090886200002));
#291772=CARTESIAN_POINT('Ctrl Pts',(-4.06472631000006,15.2,-9.63234773600002));
#291773=CARTESIAN_POINT('Ctrl Pts',(-4.06472631000006,11.6,-9.63234773600002));
#291774=CARTESIAN_POINT('Ctrl Pts',(-4.06509319700006,15.2,-9.63379483400002));
#291775=CARTESIAN_POINT('Ctrl Pts',(-4.06509319700006,11.6,-9.63379483400002));
#291776=CARTESIAN_POINT('Ctrl Pts',(-4.06546069800005,15.2,-9.63525013900002));
#291777=CARTESIAN_POINT('Ctrl Pts',(-4.06546069800005,11.6,-9.63525013900002));
#291778=CARTESIAN_POINT('Ctrl Pts',(-4.06582879000006,15.2,-9.63671363800002));
#291779=CARTESIAN_POINT('Ctrl Pts',(-4.06582879000006,11.6,-9.63671363800002));
#291780=CARTESIAN_POINT('Ctrl Pts',(-4.06619745800006,15.2,-9.63818531300002));
#291781=CARTESIAN_POINT('Ctrl Pts',(-4.06619745800006,11.6,-9.63818531300002));
#291782=CARTESIAN_POINT('Ctrl Pts',(-4.06656668200006,15.2,-9.63966514900001));
#291783=CARTESIAN_POINT('Ctrl Pts',(-4.06656668200006,11.6,-9.63966514900001));
#291784=CARTESIAN_POINT('Ctrl Pts',(-4.06693644400006,15.2,-9.64115313000002));
#291785=CARTESIAN_POINT('Ctrl Pts',(-4.06693644400006,11.6,-9.64115313000002));
#291786=CARTESIAN_POINT('Ctrl Pts',(-4.06730672500006,15.2,-9.64264924100002));
#291787=CARTESIAN_POINT('Ctrl Pts',(-4.06730672500006,11.6,-9.64264924100002));
#291788=CARTESIAN_POINT('Ctrl Pts',(-4.06767750700006,15.2,-9.64415346700001));
#291789=CARTESIAN_POINT('Ctrl Pts',(-4.06767750700006,11.6,-9.64415346700001));
#291790=CARTESIAN_POINT('Ctrl Pts',(-4.06804877300006,15.2,-9.64566579300002));
#291791=CARTESIAN_POINT('Ctrl Pts',(-4.06804877300006,11.6,-9.64566579300002));
#291792=CARTESIAN_POINT('Ctrl Pts',(-4.06842050400006,15.2,-9.64718620200001));
#291793=CARTESIAN_POINT('Ctrl Pts',(-4.06842050400006,11.6,-9.64718620200001));
#291794=CARTESIAN_POINT('Ctrl Pts',(-4.06879268100006,15.2,-9.64871467800002));
#291795=CARTESIAN_POINT('Ctrl Pts',(-4.06879268100006,11.6,-9.64871467800002));
#291796=CARTESIAN_POINT('Ctrl Pts',(-4.06916528800005,15.2,-9.65025121000001));
#291797=CARTESIAN_POINT('Ctrl Pts',(-4.06916528800005,11.6,-9.65025121000001));
#291798=CARTESIAN_POINT('Ctrl Pts',(-4.06953830600005,15.2,-9.65179577800001));
#291799=CARTESIAN_POINT('Ctrl Pts',(-4.06953830600005,11.6,-9.65179577800001));
#291800=CARTESIAN_POINT('Ctrl Pts',(-4.06991171800006,15.2,-9.65334837100001));
#291801=CARTESIAN_POINT('Ctrl Pts',(-4.06991171800006,11.6,-9.65334837100001));
#291802=CARTESIAN_POINT('Ctrl Pts',(-4.07028550500006,15.2,-9.65490897100001));
#291803=CARTESIAN_POINT('Ctrl Pts',(-4.07028550500006,11.6,-9.65490897100001));
#291804=CARTESIAN_POINT('Ctrl Pts',(-4.07065965200006,15.2,-9.65647756300001));
#291805=CARTESIAN_POINT('Ctrl Pts',(-4.07065965200006,11.6,-9.65647756300001));
#291806=CARTESIAN_POINT('Ctrl Pts',(-4.07103413900006,15.2,-9.65805413300002));
#291807=CARTESIAN_POINT('Ctrl Pts',(-4.07103413900006,11.6,-9.65805413300002));
#291808=CARTESIAN_POINT('Ctrl Pts',(-4.07140894900006,15.2,-9.65963866700001));
#291809=CARTESIAN_POINT('Ctrl Pts',(-4.07140894900006,11.6,-9.65963866700001));
#291810=CARTESIAN_POINT('Ctrl Pts',(-4.07178406600006,15.2,-9.66123114900001));
#291811=CARTESIAN_POINT('Ctrl Pts',(-4.07178406600006,11.6,-9.66123114900001));
#291812=CARTESIAN_POINT('Ctrl Pts',(-4.07215947000005,15.2,-9.66283156300001));
#291813=CARTESIAN_POINT('Ctrl Pts',(-4.07215947000005,11.6,-9.66283156300001));
#291814=CARTESIAN_POINT('Ctrl Pts',(-4.07253514800006,15.2,-9.66443989500001));
#291815=CARTESIAN_POINT('Ctrl Pts',(-4.07253514800006,11.6,-9.66443989500001));
#291816=CARTESIAN_POINT('Ctrl Pts',(-4.07291107900006,15.2,-9.66605613100001));
#291817=CARTESIAN_POINT('Ctrl Pts',(-4.07291107900006,11.6,-9.66605613100001));
#291818=CARTESIAN_POINT('Ctrl Pts',(-4.07328724700006,15.2,-9.66768025600001));
#291819=CARTESIAN_POINT('Ctrl Pts',(-4.07328724700006,11.6,-9.66768025600001));
#291820=CARTESIAN_POINT('Ctrl Pts',(-4.07366363600006,15.2,-9.66931225500001));
#291821=CARTESIAN_POINT('Ctrl Pts',(-4.07366363600006,11.6,-9.66931225500001));
#291822=CARTESIAN_POINT('Ctrl Pts',(-4.07404022800006,15.2,-9.67095211400001));
#291823=CARTESIAN_POINT('Ctrl Pts',(-4.07404022800006,11.6,-9.67095211400001));
#291824=CARTESIAN_POINT('Ctrl Pts',(-4.07441700700006,15.2,-9.67259981700001));
#291825=CARTESIAN_POINT('Ctrl Pts',(-4.07441700700006,11.6,-9.67259981700001));
#291826=CARTESIAN_POINT('Ctrl Pts',(-4.07479395600006,15.2,-9.67425535100001));
#291827=CARTESIAN_POINT('Ctrl Pts',(-4.07479395600006,11.6,-9.67425535100001));
#291828=CARTESIAN_POINT('Ctrl Pts',(-4.07517105700006,15.2,-9.67591870100001));
#291829=CARTESIAN_POINT('Ctrl Pts',(-4.07517105700006,11.6,-9.67591870100001));
#291830=CARTESIAN_POINT('Ctrl Pts',(-4.07554829600006,15.2,-9.67758985300001));
#291831=CARTESIAN_POINT('Ctrl Pts',(-4.07554829600006,11.6,-9.67758985300001));
#291832=CARTESIAN_POINT('Ctrl Pts',(-4.07592565400006,15.2,-9.67926879100001));
#291833=CARTESIAN_POINT('Ctrl Pts',(-4.07592565400006,11.6,-9.67926879100001));
#291834=CARTESIAN_POINT('Ctrl Pts',(-4.07630311600006,15.2,-9.68095550200001));
#291835=CARTESIAN_POINT('Ctrl Pts',(-4.07630311600006,11.6,-9.68095550200001));
#291836=CARTESIAN_POINT('Ctrl Pts',(-4.07668066500006,15.2,-9.68264997100001));
#291837=CARTESIAN_POINT('Ctrl Pts',(-4.07668066500006,11.6,-9.68264997100001));
#291838=CARTESIAN_POINT('Ctrl Pts',(-4.07705828300006,15.2,-9.68435218600001));
#291839=CARTESIAN_POINT('Ctrl Pts',(-4.07705828300006,11.6,-9.68435218600001));
#291840=CARTESIAN_POINT('Ctrl Pts',(-4.07743595800006,15.2,-9.68606212900001));
#291841=CARTESIAN_POINT('Ctrl Pts',(-4.07743595800006,11.6,-9.68606212900001));
#291842=CARTESIAN_POINT('Ctrl Pts',(-4.07781367000006,15.2,-9.68777978900001));
#291843=CARTESIAN_POINT('Ctrl Pts',(-4.07781367000006,11.6,-9.68777978900001));
#291844=CARTESIAN_POINT('Ctrl Pts',(-4.07819140400006,15.2,-9.68950514900001));
#291845=CARTESIAN_POINT('Ctrl Pts',(-4.07819140400006,11.6,-9.68950514900001));
#291846=CARTESIAN_POINT('Ctrl Pts',(-4.07856914400006,15.2,-9.69123819800001));
#291847=CARTESIAN_POINT('Ctrl Pts',(-4.07856914400006,11.6,-9.69123819800001));
#291848=CARTESIAN_POINT('Ctrl Pts',(-4.07894687300006,15.2,-9.69297892000001));
#291849=CARTESIAN_POINT('Ctrl Pts',(-4.07894687300006,11.6,-9.69297892000001));
#291850=CARTESIAN_POINT('Ctrl Pts',(-4.07932457800006,15.2,-9.69472730100001));
#291851=CARTESIAN_POINT('Ctrl Pts',(-4.07932457800006,11.6,-9.69472730100001));
#291852=CARTESIAN_POINT('Ctrl Pts',(-4.07970224000006,15.2,-9.69648332900001));
#291853=CARTESIAN_POINT('Ctrl Pts',(-4.07970224000006,11.6,-9.69648332900001));
#291854=CARTESIAN_POINT('Ctrl Pts',(-4.08007984400006,15.2,-9.69824698600001));
#291855=CARTESIAN_POINT('Ctrl Pts',(-4.08007984400006,11.6,-9.69824698600001));
#291856=CARTESIAN_POINT('Ctrl Pts',(-4.08045737600006,15.2,-9.70001826300001));
#291857=CARTESIAN_POINT('Ctrl Pts',(-4.08045737600006,11.6,-9.70001826300001));
#291858=CARTESIAN_POINT('Ctrl Pts',(-4.08083481800006,15.2,-9.70179714300001));
#291859=CARTESIAN_POINT('Ctrl Pts',(-4.08083481800006,11.6,-9.70179714300001));
#291860=CARTESIAN_POINT('Ctrl Pts',(-4.08121215500006,15.2,-9.70358361200001));
#291861=CARTESIAN_POINT('Ctrl Pts',(-4.08121215500006,11.6,-9.70358361200001));
#291862=CARTESIAN_POINT('Ctrl Pts',(-4.08158937200006,15.2,-9.70537765900001));
#291863=CARTESIAN_POINT('Ctrl Pts',(-4.08158937200006,11.6,-9.70537765900001));
#291864=CARTESIAN_POINT('Ctrl Pts',(-4.08196645300006,15.2,-9.70717926800001));
#291865=CARTESIAN_POINT('Ctrl Pts',(-4.08196645300006,11.6,-9.70717926800001));
#291866=CARTESIAN_POINT('Ctrl Pts',(-4.08234338400006,15.2,-9.70898842600001));
#291867=CARTESIAN_POINT('Ctrl Pts',(-4.08234338400006,11.6,-9.70898842600001));
#291868=CARTESIAN_POINT('Ctrl Pts',(-4.08272014700006,15.2,-9.71080511800001));
#291869=CARTESIAN_POINT('Ctrl Pts',(-4.08272014700006,11.6,-9.71080511800001));
#291870=CARTESIAN_POINT('Ctrl Pts',(-4.08309672900006,15.2,-9.71262933200001));
#291871=CARTESIAN_POINT('Ctrl Pts',(-4.08309672900006,11.6,-9.71262933200001));
#291872=CARTESIAN_POINT('Ctrl Pts',(-4.08347311300005,15.2,-9.71446105500001));
#291873=CARTESIAN_POINT('Ctrl Pts',(-4.08347311300005,11.6,-9.71446105500001));
#291874=CARTESIAN_POINT('Ctrl Pts',(-4.08384928600006,15.2,-9.71630027200001));
#291875=CARTESIAN_POINT('Ctrl Pts',(-4.08384928600006,11.6,-9.71630027200001));
#291876=CARTESIAN_POINT('Ctrl Pts',(-4.08422523100006,15.2,-9.71814696900001));
#291877=CARTESIAN_POINT('Ctrl Pts',(-4.08422523100006,11.6,-9.71814696900001));
#291878=CARTESIAN_POINT('Ctrl Pts',(-4.08460093300006,15.2,-9.72000113500001));
#291879=CARTESIAN_POINT('Ctrl Pts',(-4.08460093300006,11.6,-9.72000113500001));
#291880=CARTESIAN_POINT('Ctrl Pts',(-4.08497637900005,15.2,-9.72186275400001));
#291881=CARTESIAN_POINT('Ctrl Pts',(-4.08497637900005,11.6,-9.72186275400001));
#291882=CARTESIAN_POINT('Ctrl Pts',(-4.08535155300005,15.2,-9.72373181400001));
#291883=CARTESIAN_POINT('Ctrl Pts',(-4.08535155300005,11.6,-9.72373181400001));
#291884=CARTESIAN_POINT('Ctrl Pts',(-4.08572643900006,15.2,-9.72560830200001));
#291885=CARTESIAN_POINT('Ctrl Pts',(-4.08572643900006,11.6,-9.72560830200001));
#291886=CARTESIAN_POINT('Ctrl Pts',(-4.08610102200006,15.2,-9.72749220300001));
#291887=CARTESIAN_POINT('Ctrl Pts',(-4.08610102200006,11.6,-9.72749220300001));
#291888=CARTESIAN_POINT('Ctrl Pts',(-4.08647528900006,15.2,-9.72938350500001));
#291889=CARTESIAN_POINT('Ctrl Pts',(-4.08647528900006,11.6,-9.72938350500001));
#291890=CARTESIAN_POINT('Ctrl Pts',(-4.08684922500006,15.2,-9.73128219600001));
#291891=CARTESIAN_POINT('Ctrl Pts',(-4.08684922500006,11.6,-9.73128219600001));
#291892=CARTESIAN_POINT('Ctrl Pts',(-4.08722281500006,15.2,-9.73318826000001));
#291893=CARTESIAN_POINT('Ctrl Pts',(-4.08722281500006,11.6,-9.73318826000001));
#291894=CARTESIAN_POINT('Ctrl Pts',(-4.08759604300006,15.2,-9.73510168500001));
#291895=CARTESIAN_POINT('Ctrl Pts',(-4.08759604300006,11.6,-9.73510168500001));
#291896=CARTESIAN_POINT('Ctrl Pts',(-4.08796889700006,15.2,-9.73702246000001));
#291897=CARTESIAN_POINT('Ctrl Pts',(-4.08796889700006,11.6,-9.73702246000001));
#291898=CARTESIAN_POINT('Ctrl Pts',(-4.08834136200006,15.2,-9.73895056800002));
#291899=CARTESIAN_POINT('Ctrl Pts',(-4.08834136200006,11.6,-9.73895056800002));
#291900=CARTESIAN_POINT('Ctrl Pts',(-4.08871342100006,15.2,-9.74088599900002));
#291901=CARTESIAN_POINT('Ctrl Pts',(-4.08871342100006,11.6,-9.74088599900002));
#291902=CARTESIAN_POINT('Ctrl Pts',(-4.08908506300006,15.2,-9.74282873800002));
#291903=CARTESIAN_POINT('Ctrl Pts',(-4.08908506300006,11.6,-9.74282873800002));
#291904=CARTESIAN_POINT('Ctrl Pts',(-4.08945627200006,15.2,-9.74477877400002));
#291905=CARTESIAN_POINT('Ctrl Pts',(-4.08945627200006,11.6,-9.74477877400002));
#291906=CARTESIAN_POINT('Ctrl Pts',(-4.08982703500006,15.2,-9.74673609300002));
#291907=CARTESIAN_POINT('Ctrl Pts',(-4.08982703500006,11.6,-9.74673609300002));
#291908=CARTESIAN_POINT('Ctrl Pts',(-4.09019733600006,15.2,-9.74870068100001));
#291909=CARTESIAN_POINT('Ctrl Pts',(-4.09019733600006,11.6,-9.74870068100001));
#291910=CARTESIAN_POINT('Ctrl Pts',(-4.09056716200006,15.2,-9.75067252700001));
#291911=CARTESIAN_POINT('Ctrl Pts',(-4.09056716200006,11.6,-9.75067252700001));
#291912=CARTESIAN_POINT('Ctrl Pts',(-4.09093649900006,15.2,-9.75265161800001));
#291913=CARTESIAN_POINT('Ctrl Pts',(-4.09093649900006,11.6,-9.75265161800001));
#291914=CARTESIAN_POINT('Ctrl Pts',(-4.09130533200006,15.2,-9.75463794000001));
#291915=CARTESIAN_POINT('Ctrl Pts',(-4.09130533200006,11.6,-9.75463794000001));
#291916=CARTESIAN_POINT('Ctrl Pts',(-4.09167364900005,15.2,-9.75663148100001));
#291917=CARTESIAN_POINT('Ctrl Pts',(-4.09167364900005,11.6,-9.75663148100001));
#291918=CARTESIAN_POINT('Ctrl Pts',(-4.09204143300006,15.2,-9.75863222700001));
#291919=CARTESIAN_POINT('Ctrl Pts',(-4.09204143300006,11.6,-9.75863222700001));
#291920=CARTESIAN_POINT('Ctrl Pts',(-4.09240867400006,15.2,-9.76064016800001));
#291921=CARTESIAN_POINT('Ctrl Pts',(-4.09240867400006,11.6,-9.76064016800001));
#291922=CARTESIAN_POINT('Ctrl Pts',(-4.09277535500006,15.2,-9.76265528900001));
#291923=CARTESIAN_POINT('Ctrl Pts',(-4.09277535500006,11.6,-9.76265528900001));
#291924=CARTESIAN_POINT('Ctrl Pts',(-4.09314146500006,15.2,-9.76467757800001));
#291925=CARTESIAN_POINT('Ctrl Pts',(-4.09314146500006,11.6,-9.76467757800001));
#291926=CARTESIAN_POINT('Ctrl Pts',(-4.09350698800006,15.2,-9.76670702200001));
#291927=CARTESIAN_POINT('Ctrl Pts',(-4.09350698800006,11.6,-9.76670702200001));
#291928=CARTESIAN_POINT('Ctrl Pts',(-4.09387191000006,15.2,-9.76874360900001));
#291929=CARTESIAN_POINT('Ctrl Pts',(-4.09387191000006,11.6,-9.76874360900001));
#291930=CARTESIAN_POINT('Ctrl Pts',(-4.09423622000006,15.2,-9.77078732700001));
#291931=CARTESIAN_POINT('Ctrl Pts',(-4.09423622000006,11.6,-9.77078732700001));
#291932=CARTESIAN_POINT('Ctrl Pts',(-4.09459990200006,15.2,-9.77283816200002));
#291933=CARTESIAN_POINT('Ctrl Pts',(-4.09459990200006,11.6,-9.77283816200002));
#291934=CARTESIAN_POINT('Ctrl Pts',(-4.09496294500006,15.2,-9.77489610300001));
#291935=CARTESIAN_POINT('Ctrl Pts',(-4.09496294500006,11.6,-9.77489610300001));
#291936=CARTESIAN_POINT('Ctrl Pts',(-4.09532533400006,15.2,-9.77696113700001));
#291937=CARTESIAN_POINT('Ctrl Pts',(-4.09532533400006,11.6,-9.77696113700001));
#291938=CARTESIAN_POINT('Ctrl Pts',(-4.09568705400006,15.2,-9.77903325100001));
#291939=CARTESIAN_POINT('Ctrl Pts',(-4.09568705400006,11.6,-9.77903325100001));
#291940=CARTESIAN_POINT('Ctrl Pts',(-4.09604809600006,15.2,-9.78111243300001));
#291941=CARTESIAN_POINT('Ctrl Pts',(-4.09604809600006,11.6,-9.78111243300001));
#291942=CARTESIAN_POINT('Ctrl Pts',(-4.09640844200006,15.2,-9.78319867000001));
#291943=CARTESIAN_POINT('Ctrl Pts',(-4.09640844200006,11.6,-9.78319867000001));
#291944=CARTESIAN_POINT('Ctrl Pts',(-4.09676808300006,15.2,-9.78529195200001));
#291945=CARTESIAN_POINT('Ctrl Pts',(-4.09676808300006,11.6,-9.78529195200001));
#291946=CARTESIAN_POINT('Ctrl Pts',(-4.09712700200005,15.2,-9.78739226400001));
#291947=CARTESIAN_POINT('Ctrl Pts',(-4.09712700200005,11.6,-9.78739226400001));
#291948=CARTESIAN_POINT('Ctrl Pts',(-4.09748518900006,15.2,-9.78949959400001));
#291949=CARTESIAN_POINT('Ctrl Pts',(-4.09748518900006,11.6,-9.78949959400001));
#291950=CARTESIAN_POINT('Ctrl Pts',(-4.09784262900006,15.2,-9.79161393200001));
#291951=CARTESIAN_POINT('Ctrl Pts',(-4.09784262900006,11.6,-9.79161393200001));
#291952=CARTESIAN_POINT('Ctrl Pts',(-4.09819930900006,15.2,-9.79373526400001));
#291953=CARTESIAN_POINT('Ctrl Pts',(-4.09819930900006,11.6,-9.79373526400001));
#291954=CARTESIAN_POINT('Ctrl Pts',(-4.09855521800006,15.2,-9.79586357800001));
#291955=CARTESIAN_POINT('Ctrl Pts',(-4.09855521800006,11.6,-9.79586357800001));
#291956=CARTESIAN_POINT('Ctrl Pts',(-4.09891034100006,15.2,-9.79799886300001));
#291957=CARTESIAN_POINT('Ctrl Pts',(-4.09891034100006,11.6,-9.79799886300001));
#291958=CARTESIAN_POINT('Ctrl Pts',(-4.09926466500006,15.2,-9.80014110500001));
#291959=CARTESIAN_POINT('Ctrl Pts',(-4.09926466500006,11.6,-9.80014110500001));
#291960=CARTESIAN_POINT('Ctrl Pts',(-4.09961817900006,15.2,-9.80229029300001));
#291961=CARTESIAN_POINT('Ctrl Pts',(-4.09961817900006,11.6,-9.80229029300001));
#291962=CARTESIAN_POINT('Ctrl Pts',(-4.09997086900006,15.2,-9.80444641500001));
#291963=CARTESIAN_POINT('Ctrl Pts',(-4.09997086900006,11.6,-9.80444641500001));
#291964=CARTESIAN_POINT('Ctrl Pts',(-4.10032272300006,15.2,-9.80660945800001));
#291965=CARTESIAN_POINT('Ctrl Pts',(-4.10032272300006,11.6,-9.80660945800001));
#291966=CARTESIAN_POINT('Ctrl Pts',(-4.10067372700006,15.2,-9.80877941200001));
#291967=CARTESIAN_POINT('Ctrl Pts',(-4.10067372700006,11.6,-9.80877941200001));
#291968=CARTESIAN_POINT('Ctrl Pts',(-4.10102386900006,15.2,-9.81095626300001));
#291969=CARTESIAN_POINT('Ctrl Pts',(-4.10102386900006,11.6,-9.81095626300001));
#291970=CARTESIAN_POINT('Ctrl Pts',(-4.10137313800006,15.2,-9.81314000000001));
#291971=CARTESIAN_POINT('Ctrl Pts',(-4.10137313800006,11.6,-9.81314000000001));
#291972=CARTESIAN_POINT('Ctrl Pts',(-4.10172152000006,15.2,-9.81533061200001));
#291973=CARTESIAN_POINT('Ctrl Pts',(-4.10172152000006,11.6,-9.81533061200001));
#291974=CARTESIAN_POINT('Ctrl Pts',(-4.10206900100006,15.2,-9.81752808500001));
#291975=CARTESIAN_POINT('Ctrl Pts',(-4.10206900100006,11.6,-9.81752808500001));
#291976=CARTESIAN_POINT('Ctrl Pts',(-4.10241557100006,15.2,-9.81973240900001));
#291977=CARTESIAN_POINT('Ctrl Pts',(-4.10241557100006,11.6,-9.81973240900001));
#291978=CARTESIAN_POINT('Ctrl Pts',(-4.10276121600006,15.2,-9.82194357100001));
#291979=CARTESIAN_POINT('Ctrl Pts',(-4.10276121600006,11.6,-9.82194357100001));
#291980=CARTESIAN_POINT('Ctrl Pts',(-4.10310592400006,15.2,-9.82416156000001));
#291981=CARTESIAN_POINT('Ctrl Pts',(-4.10310592400006,11.6,-9.82416156000001));
#291982=CARTESIAN_POINT('Ctrl Pts',(-4.10344968400006,15.2,-9.82638636200001));
#291983=CARTESIAN_POINT('Ctrl Pts',(-4.10344968400006,11.6,-9.82638636200001));
#291984=CARTESIAN_POINT('Ctrl Pts',(-4.10379248300006,15.2,-9.82861797000002));
#291985=CARTESIAN_POINT('Ctrl Pts',(-4.10379248300006,11.6,-9.82861797000002));
#291986=CARTESIAN_POINT('Ctrl Pts',(-4.10413430800006,15.2,-9.83085636800001));
#291987=CARTESIAN_POINT('Ctrl Pts',(-4.10413430800006,11.6,-9.83085636800001));
#291988=CARTESIAN_POINT('Ctrl Pts',(-4.10447514700006,15.2,-9.83310154500001));
#291989=CARTESIAN_POINT('Ctrl Pts',(-4.10447514700006,11.6,-9.83310154500001));
#291990=CARTESIAN_POINT('Ctrl Pts',(-4.10481498900006,15.2,-9.83535349100001));
#291991=CARTESIAN_POINT('Ctrl Pts',(-4.10481498900006,11.6,-9.83535349100001));
#291992=CARTESIAN_POINT('Ctrl Pts',(-4.10515382100006,15.2,-9.83761219400001));
#291993=CARTESIAN_POINT('Ctrl Pts',(-4.10515382100006,11.6,-9.83761219400001));
#291994=CARTESIAN_POINT('Ctrl Pts',(-4.10549163100006,15.2,-9.83987764100001));
#291995=CARTESIAN_POINT('Ctrl Pts',(-4.10549163100006,11.6,-9.83987764100001));
#291996=CARTESIAN_POINT('Ctrl Pts',(-4.10582840600005,15.2,-9.84214982100001));
#291997=CARTESIAN_POINT('Ctrl Pts',(-4.10582840600005,11.6,-9.84214982100001));
#291998=CARTESIAN_POINT('Ctrl Pts',(-4.10616413700006,15.2,-9.84442872300001));
#291999=CARTESIAN_POINT('Ctrl Pts',(-4.10616413700006,11.6,-9.84442872300001));
#292000=CARTESIAN_POINT('Ctrl Pts',(-4.10649880900006,15.2,-9.84671433500001));
#292001=CARTESIAN_POINT('Ctrl Pts',(-4.10649880900006,11.6,-9.84671433500001));
#292002=CARTESIAN_POINT('Ctrl Pts',(-4.10683241100006,15.2,-9.84900664600001));
#292003=CARTESIAN_POINT('Ctrl Pts',(-4.10683241100006,11.6,-9.84900664600001));
#292004=CARTESIAN_POINT('Ctrl Pts',(-4.10716493300006,15.2,-9.85130564400001));
#292005=CARTESIAN_POINT('Ctrl Pts',(-4.10716493300006,11.6,-9.85130564400001));
#292006=CARTESIAN_POINT('Ctrl Pts',(-4.10749636000006,15.2,-9.85361131800001));
#292007=CARTESIAN_POINT('Ctrl Pts',(-4.10749636000006,11.6,-9.85361131800001));
#292008=CARTESIAN_POINT('Ctrl Pts',(-4.10782668300006,15.2,-9.85592365600001));
#292009=CARTESIAN_POINT('Ctrl Pts',(-4.10782668300006,11.6,-9.85592365600001));
#292010=CARTESIAN_POINT('Ctrl Pts',(-4.10815588900006,15.2,-9.85824264700001));
#292011=CARTESIAN_POINT('Ctrl Pts',(-4.10815588900006,11.6,-9.85824264700001));
#292012=CARTESIAN_POINT('Ctrl Pts',(-4.10848396700006,15.2,-9.86056827900001));
#292013=CARTESIAN_POINT('Ctrl Pts',(-4.10848396700006,11.6,-9.86056827900001));
#292014=CARTESIAN_POINT('Ctrl Pts',(-4.10881090400006,15.2,-9.86290054200001));
#292015=CARTESIAN_POINT('Ctrl Pts',(-4.10881090400006,11.6,-9.86290054200001));
#292016=CARTESIAN_POINT('Ctrl Pts',(-4.10913669000006,15.2,-9.86523942300001));
#292017=CARTESIAN_POINT('Ctrl Pts',(-4.10913669000006,11.6,-9.86523942300001));
#292018=CARTESIAN_POINT('Ctrl Pts',(-4.10946131400006,15.2,-9.86758491300001));
#292019=CARTESIAN_POINT('Ctrl Pts',(-4.10946131400006,11.6,-9.86758491300001));
#292020=CARTESIAN_POINT('Ctrl Pts',(-4.10978476100006,15.2,-9.86993699800001));
#292021=CARTESIAN_POINT('Ctrl Pts',(-4.10978476100006,11.6,-9.86993699800001));
#292022=CARTESIAN_POINT('Ctrl Pts',(-4.11010702400006,15.2,-9.87229566900002));
#292023=CARTESIAN_POINT('Ctrl Pts',(-4.11010702400006,11.6,-9.87229566900002));
#292024=CARTESIAN_POINT('Ctrl Pts',(-4.11042808900006,15.2,-9.87466091300002));
#292025=CARTESIAN_POINT('Ctrl Pts',(-4.11042808900006,11.6,-9.87466091300002));
#292026=CARTESIAN_POINT('Ctrl Pts',(-4.11074794500006,15.2,-9.87703272000001));
#292027=CARTESIAN_POINT('Ctrl Pts',(-4.11074794500006,11.6,-9.87703272000001));
#292028=CARTESIAN_POINT('Ctrl Pts',(-4.11106658100006,15.2,-9.87941107800001));
#292029=CARTESIAN_POINT('Ctrl Pts',(-4.11106658100006,11.6,-9.87941107800001));
#292030=CARTESIAN_POINT('Ctrl Pts',(-4.11138398500006,15.2,-9.88179597800001));
#292031=CARTESIAN_POINT('Ctrl Pts',(-4.11138398500006,11.6,-9.88179597800001));
#292032=CARTESIAN_POINT('Ctrl Pts',(-4.11170014700006,15.2,-9.88418740500001));
#292033=CARTESIAN_POINT('Ctrl Pts',(-4.11170014700006,11.6,-9.88418740500001));
#292034=CARTESIAN_POINT('Ctrl Pts',(-4.11201505600006,15.2,-9.88658535100001));
#292035=CARTESIAN_POINT('Ctrl Pts',(-4.11201505600006,11.6,-9.88658535100001));
#292036=CARTESIAN_POINT('Ctrl Pts',(-4.11232869800005,15.2,-9.88898980400001));
#292037=CARTESIAN_POINT('Ctrl Pts',(-4.11232869800005,11.6,-9.88898980400001));
#292038=CARTESIAN_POINT('Ctrl Pts',(-4.11264106500006,15.2,-9.89140075300002));
#292039=CARTESIAN_POINT('Ctrl Pts',(-4.11264106500006,11.6,-9.89140075300002));
#292040=CARTESIAN_POINT('Ctrl Pts',(-4.11295214400006,15.2,-9.89381818800001));
#292041=CARTESIAN_POINT('Ctrl Pts',(-4.11295214400006,11.6,-9.89381818800001));
#292042=CARTESIAN_POINT('Ctrl Pts',(-4.11326192500006,15.2,-9.89624209500001));
#292043=CARTESIAN_POINT('Ctrl Pts',(-4.11326192500006,11.6,-9.89624209500001));
#292044=CARTESIAN_POINT('Ctrl Pts',(-4.11357039600006,15.2,-9.89867246600001));
#292045=CARTESIAN_POINT('Ctrl Pts',(-4.11357039600006,11.6,-9.89867246600001));
#292046=CARTESIAN_POINT('Ctrl Pts',(-4.11387754700006,15.2,-9.90110928800001));
#292047=CARTESIAN_POINT('Ctrl Pts',(-4.11387754700006,11.6,-9.90110928800001));
#292048=CARTESIAN_POINT('Ctrl Pts',(-4.11418336800006,15.2,-9.90355255300001));
#292049=CARTESIAN_POINT('Ctrl Pts',(-4.11418336800006,11.6,-9.90355255300001));
#292050=CARTESIAN_POINT('Ctrl Pts',(-4.11448784500006,15.2,-9.90600224700001));
#292051=CARTESIAN_POINT('Ctrl Pts',(-4.11448784500006,11.6,-9.90600224700001));
#292052=CARTESIAN_POINT('Ctrl Pts',(-4.11479097000006,15.2,-9.90845836000001));
#292053=CARTESIAN_POINT('Ctrl Pts',(-4.11479097000006,11.6,-9.90845836000001));
#292054=CARTESIAN_POINT('Ctrl Pts',(-4.11509273200005,15.2,-9.91092088100001));
#292055=CARTESIAN_POINT('Ctrl Pts',(-4.11509273200005,11.6,-9.91092088100001));
#292056=CARTESIAN_POINT('Ctrl Pts',(-4.11539311800006,15.2,-9.91338980100001));
#292057=CARTESIAN_POINT('Ctrl Pts',(-4.11539311800006,11.6,-9.91338980100001));
#292058=CARTESIAN_POINT('Ctrl Pts',(-4.11569211900006,15.2,-9.91586510600001));
#292059=CARTESIAN_POINT('Ctrl Pts',(-4.11569211900006,11.6,-9.91586510600001));
#292060=CARTESIAN_POINT('Ctrl Pts',(-4.11598972300006,15.2,-9.91834678800001));
#292061=CARTESIAN_POINT('Ctrl Pts',(-4.11598972300006,11.6,-9.91834678800001));
#292062=CARTESIAN_POINT('Ctrl Pts',(-4.11628592200006,15.2,-9.92083483500001));
#292063=CARTESIAN_POINT('Ctrl Pts',(-4.11628592200006,11.6,-9.92083483500001));
#292064=CARTESIAN_POINT('Ctrl Pts',(-4.11658070300006,15.2,-9.92332923600001));
#292065=CARTESIAN_POINT('Ctrl Pts',(-4.11658070300006,11.6,-9.92332923600001));
#292066=CARTESIAN_POINT('Ctrl Pts',(-4.11687405500006,15.2,-9.92582998100001));
#292067=CARTESIAN_POINT('Ctrl Pts',(-4.11687405500006,11.6,-9.92582998100001));
#292068=CARTESIAN_POINT('Ctrl Pts',(-4.11716597000006,15.2,-9.92833705900001));
#292069=CARTESIAN_POINT('Ctrl Pts',(-4.11716597000006,11.6,-9.92833705900001));
#292070=CARTESIAN_POINT('Ctrl Pts',(-4.11745643400006,15.2,-9.93085045900001));
#292071=CARTESIAN_POINT('Ctrl Pts',(-4.11745643400006,11.6,-9.93085045900001));
#292072=CARTESIAN_POINT('Ctrl Pts',(-4.11774544000005,15.2,-9.93337017000002));
#292073=CARTESIAN_POINT('Ctrl Pts',(-4.11774544000005,11.6,-9.93337017000002));
#292074=CARTESIAN_POINT('Ctrl Pts',(-4.11803297600006,15.2,-9.93589618200001));
#292075=CARTESIAN_POINT('Ctrl Pts',(-4.11803297600006,11.6,-9.93589618200001));
#292076=CARTESIAN_POINT('Ctrl Pts',(-4.11831903100006,15.2,-9.93842848500002));
#292077=CARTESIAN_POINT('Ctrl Pts',(-4.11831903100006,11.6,-9.93842848500002));
#292078=CARTESIAN_POINT('Ctrl Pts',(-4.11860359500006,15.2,-9.94096706700001));
#292079=CARTESIAN_POINT('Ctrl Pts',(-4.11860359500006,11.6,-9.94096706700001));
#292080=CARTESIAN_POINT('Ctrl Pts',(-4.11888665800006,15.2,-9.94351191900001));
#292081=CARTESIAN_POINT('Ctrl Pts',(-4.11888665800006,11.6,-9.94351191900001));
#292082=CARTESIAN_POINT('Ctrl Pts',(-4.11916821000006,15.2,-9.94606302900001));
#292083=CARTESIAN_POINT('Ctrl Pts',(-4.11916821000006,11.6,-9.94606302900001));
#292084=CARTESIAN_POINT('Ctrl Pts',(-4.11944823900006,15.2,-9.94862038700001));
#292085=CARTESIAN_POINT('Ctrl Pts',(-4.11944823900006,11.6,-9.94862038700001));
#292086=CARTESIAN_POINT('Ctrl Pts',(-4.11972673700006,15.2,-9.95118398200001));
#292087=CARTESIAN_POINT('Ctrl Pts',(-4.11972673700006,11.6,-9.95118398200001));
#292088=CARTESIAN_POINT('Ctrl Pts',(-4.12000369300006,15.2,-9.95375380500001));
#292089=CARTESIAN_POINT('Ctrl Pts',(-4.12000369300006,11.6,-9.95375380500001));
#292090=CARTESIAN_POINT('Ctrl Pts',(-4.12027909600006,15.2,-9.95632984300001));
#292091=CARTESIAN_POINT('Ctrl Pts',(-4.12027909600006,11.6,-9.95632984300001));
#292092=CARTESIAN_POINT('Ctrl Pts',(-4.12055293700006,15.2,-9.95891208800001));
#292093=CARTESIAN_POINT('Ctrl Pts',(-4.12055293700006,11.6,-9.95891208800001));
#292094=CARTESIAN_POINT('Ctrl Pts',(-4.12082520500006,15.2,-9.96150052900001));
#292095=CARTESIAN_POINT('Ctrl Pts',(-4.12082520500006,11.6,-9.96150052900001));
#292096=CARTESIAN_POINT('Ctrl Pts',(-4.12109589100006,15.2,-9.96409515500001));
#292097=CARTESIAN_POINT('Ctrl Pts',(-4.12109589100006,11.6,-9.96409515500001));
#292098=CARTESIAN_POINT('Ctrl Pts',(-4.12136498300006,15.2,-9.96669595500001));
#292099=CARTESIAN_POINT('Ctrl Pts',(-4.12136498300006,11.6,-9.96669595500001));
#292100=CARTESIAN_POINT('Ctrl Pts',(-4.12163247300006,15.2,-9.96930291900001));
#292101=CARTESIAN_POINT('Ctrl Pts',(-4.12163247300006,11.6,-9.96930291900001));
#292102=CARTESIAN_POINT('Ctrl Pts',(-4.12189835100006,15.2,-9.97191603900001));
#292103=CARTESIAN_POINT('Ctrl Pts',(-4.12189835100006,11.6,-9.97191603900001));
#292104=CARTESIAN_POINT('Ctrl Pts',(-4.12216260500006,15.2,-9.97453530100001));
#292105=CARTESIAN_POINT('Ctrl Pts',(-4.12216260500006,11.6,-9.97453530100001));
#292106=CARTESIAN_POINT('Ctrl Pts',(-4.12242522800006,15.2,-9.97716069700001));
#292107=CARTESIAN_POINT('Ctrl Pts',(-4.12242522800006,11.6,-9.97716069700001));
#292108=CARTESIAN_POINT('Ctrl Pts',(-4.12268620700006,15.2,-9.97979221700001));
#292109=CARTESIAN_POINT('Ctrl Pts',(-4.12268620700006,11.6,-9.97979221700001));
#292110=CARTESIAN_POINT('Ctrl Pts',(-4.12294553500006,15.2,-9.98242984900001));
#292111=CARTESIAN_POINT('Ctrl Pts',(-4.12294553500006,11.6,-9.98242984900001));
#292112=CARTESIAN_POINT('Ctrl Pts',(-4.12320320100005,15.2,-9.98507358300001));
#292113=CARTESIAN_POINT('Ctrl Pts',(-4.12320320100005,11.6,-9.98507358300001));
#292114=CARTESIAN_POINT('Ctrl Pts',(-4.12345919400006,15.2,-9.98772340900001));
#292115=CARTESIAN_POINT('Ctrl Pts',(-4.12345919400006,11.6,-9.98772340900001));
#292116=CARTESIAN_POINT('Ctrl Pts',(-4.12371350700006,15.2,-9.99037931800001));
#292117=CARTESIAN_POINT('Ctrl Pts',(-4.12371350700006,11.6,-9.99037931800001));
#292118=CARTESIAN_POINT('Ctrl Pts',(-4.12396612900006,15.2,-9.99304129900001));
#292119=CARTESIAN_POINT('Ctrl Pts',(-4.12396612900006,11.6,-9.99304129900001));
#292120=CARTESIAN_POINT('Ctrl Pts',(-4.12421704900006,15.2,-9.99570934200001));
#292121=CARTESIAN_POINT('Ctrl Pts',(-4.12421704900006,11.6,-9.99570934200001));
#292122=CARTESIAN_POINT('Ctrl Pts',(-4.12446625800006,15.2,-9.99838343600001));
#292123=CARTESIAN_POINT('Ctrl Pts',(-4.12446625800006,11.6,-9.99838343600001));
#292124=CARTESIAN_POINT('Ctrl Pts',(-4.12471374800006,15.2,-10.001063571));
#292125=CARTESIAN_POINT('Ctrl Pts',(-4.12471374800006,11.6,-10.001063571));
#292126=CARTESIAN_POINT('Ctrl Pts',(-4.12495950800006,15.2,-10.003749738));
#292127=CARTESIAN_POINT('Ctrl Pts',(-4.12495950800006,11.6,-10.003749738));
#292128=CARTESIAN_POINT('Ctrl Pts',(-4.12520352900006,15.2,-10.006441926));
#292129=CARTESIAN_POINT('Ctrl Pts',(-4.12520352900006,11.6,-10.006441926));
#292130=CARTESIAN_POINT('Ctrl Pts',(-4.12544580000006,15.2,-10.009140125));
#292131=CARTESIAN_POINT('Ctrl Pts',(-4.12544580000006,11.6,-10.009140125));
#292132=CARTESIAN_POINT('Ctrl Pts',(-4.12568631400006,15.2,-10.011844324));
#292133=CARTESIAN_POINT('Ctrl Pts',(-4.12568631400006,11.6,-10.011844324));
#292134=CARTESIAN_POINT('Ctrl Pts',(-4.12592506000006,15.2,-10.014554516));
#292135=CARTESIAN_POINT('Ctrl Pts',(-4.12592506000006,11.6,-10.014554516));
#292136=CARTESIAN_POINT('Ctrl Pts',(-4.12616203000006,15.2,-10.017270688));
#292137=CARTESIAN_POINT('Ctrl Pts',(-4.12616203000006,11.6,-10.017270688));
#292138=CARTESIAN_POINT('Ctrl Pts',(-4.12639721200006,15.2,-10.019992831));
#292139=CARTESIAN_POINT('Ctrl Pts',(-4.12639721200006,11.6,-10.019992831));
#292140=CARTESIAN_POINT('Ctrl Pts',(-4.12663059900006,15.2,-10.022720935));
#292141=CARTESIAN_POINT('Ctrl Pts',(-4.12663059900006,11.6,-10.022720935));
#292142=CARTESIAN_POINT('Ctrl Pts',(-4.12686218000006,15.2,-10.02545499));
#292143=CARTESIAN_POINT('Ctrl Pts',(-4.12686218000006,11.6,-10.02545499));
#292144=CARTESIAN_POINT('Ctrl Pts',(-4.12709194700006,15.2,-10.028194986));
#292145=CARTESIAN_POINT('Ctrl Pts',(-4.12709194700006,11.6,-10.028194986));
#292146=CARTESIAN_POINT('Ctrl Pts',(-4.12731989100006,15.2,-10.030940913));
#292147=CARTESIAN_POINT('Ctrl Pts',(-4.12731989100006,11.6,-10.030940913));
#292148=CARTESIAN_POINT('Ctrl Pts',(-4.12754600100006,15.2,-10.03369276));
#292149=CARTESIAN_POINT('Ctrl Pts',(-4.12754600100006,11.6,-10.03369276));
#292150=CARTESIAN_POINT('Ctrl Pts',(-4.12777027000006,15.2,-10.036450519));
#292151=CARTESIAN_POINT('Ctrl Pts',(-4.12777027000006,11.6,-10.036450519));
#292152=CARTESIAN_POINT('Ctrl Pts',(-4.12799268700006,15.2,-10.03921418));
#292153=CARTESIAN_POINT('Ctrl Pts',(-4.12799268700006,11.6,-10.03921418));
#292154=CARTESIAN_POINT('Ctrl Pts',(-4.12821324300006,15.2,-10.041983733));
#292155=CARTESIAN_POINT('Ctrl Pts',(-4.12821324300006,11.6,-10.041983733));
#292156=CARTESIAN_POINT('Ctrl Pts',(-4.12843193000006,15.2,-10.044759166));
#292157=CARTESIAN_POINT('Ctrl Pts',(-4.12843193000006,11.6,-10.044759166));
#292158=CARTESIAN_POINT('Ctrl Pts',(-4.12864873900006,15.2,-10.047540471));
#292159=CARTESIAN_POINT('Ctrl Pts',(-4.12864873900006,11.6,-10.047540471));
#292160=CARTESIAN_POINT('Ctrl Pts',(-4.12886366000006,15.2,-10.050327639));
#292161=CARTESIAN_POINT('Ctrl Pts',(-4.12886366000006,11.6,-10.050327639));
#292162=CARTESIAN_POINT('Ctrl Pts',(-4.12907668400006,15.2,-10.053120659));
#292163=CARTESIAN_POINT('Ctrl Pts',(-4.12907668400006,11.6,-10.053120659));
#292164=CARTESIAN_POINT('Ctrl Pts',(-4.12928780200006,15.2,-10.055919521));
#292165=CARTESIAN_POINT('Ctrl Pts',(-4.12928780200006,11.6,-10.055919521));
#292166=CARTESIAN_POINT('Ctrl Pts',(-4.12949700600006,15.2,-10.058724216));
#292167=CARTESIAN_POINT('Ctrl Pts',(-4.12949700600006,11.6,-10.058724216));
#292168=CARTESIAN_POINT('Ctrl Pts',(-4.12970428600006,15.2,-10.061534734));
#292169=CARTESIAN_POINT('Ctrl Pts',(-4.12970428600006,11.6,-10.061534734));
#292170=CARTESIAN_POINT('Ctrl Pts',(-4.12990963400006,15.2,-10.064351065));
#292171=CARTESIAN_POINT('Ctrl Pts',(-4.12990963400006,11.6,-10.064351065));
#292172=CARTESIAN_POINT('Ctrl Pts',(-4.13011304000006,15.2,-10.067173199));
#292173=CARTESIAN_POINT('Ctrl Pts',(-4.13011304000006,11.6,-10.067173199));
#292174=CARTESIAN_POINT('Ctrl Pts',(-4.13031449600005,15.2,-10.070001127));
#292175=CARTESIAN_POINT('Ctrl Pts',(-4.13031449600005,11.6,-10.070001127));
#292176=CARTESIAN_POINT('Ctrl Pts',(-4.13051399200006,15.2,-10.07283484));
#292177=CARTESIAN_POINT('Ctrl Pts',(-4.13051399200006,11.6,-10.07283484));
#292178=CARTESIAN_POINT('Ctrl Pts',(-4.13071152200006,15.2,-10.075674326));
#292179=CARTESIAN_POINT('Ctrl Pts',(-4.13071152200006,11.6,-10.075674326));
#292180=CARTESIAN_POINT('Ctrl Pts',(-4.13090707400006,15.2,-10.078519577));
#292181=CARTESIAN_POINT('Ctrl Pts',(-4.13090707400006,11.6,-10.078519577));
#292182=CARTESIAN_POINT('Ctrl Pts',(-4.13110064100006,15.2,-10.081370584));
#292183=CARTESIAN_POINT('Ctrl Pts',(-4.13110064100006,11.6,-10.081370584));
#292184=CARTESIAN_POINT('Ctrl Pts',(-4.13129221500006,15.2,-10.084227336));
#292185=CARTESIAN_POINT('Ctrl Pts',(-4.13129221500006,11.6,-10.084227336));
#292186=CARTESIAN_POINT('Ctrl Pts',(-4.13148178500006,15.2,-10.087089824));
#292187=CARTESIAN_POINT('Ctrl Pts',(-4.13148178500006,11.6,-10.087089824));
#292188=CARTESIAN_POINT('Ctrl Pts',(-4.13166934400006,15.2,-10.089958038));
#292189=CARTESIAN_POINT('Ctrl Pts',(-4.13166934400006,11.6,-10.089958038));
#292190=CARTESIAN_POINT('Ctrl Pts',(-4.13185488300006,15.2,-10.09283197));
#292191=CARTESIAN_POINT('Ctrl Pts',(-4.13185488300006,11.6,-10.09283197));
#292192=CARTESIAN_POINT('Ctrl Pts',(-4.13203839300006,15.2,-10.095711608));
#292193=CARTESIAN_POINT('Ctrl Pts',(-4.13203839300006,11.6,-10.095711608));
#292194=CARTESIAN_POINT('Ctrl Pts',(-4.13221986700006,15.2,-10.098596944));
#292195=CARTESIAN_POINT('Ctrl Pts',(-4.13221986700006,11.6,-10.098596944));
#292196=CARTESIAN_POINT('Ctrl Pts',(-4.13239929400006,15.2,-10.101487969));
#292197=CARTESIAN_POINT('Ctrl Pts',(-4.13239929400006,11.6,-10.101487969));
#292198=CARTESIAN_POINT('Ctrl Pts',(-4.13257666800006,15.2,-10.104384672));
#292199=CARTESIAN_POINT('Ctrl Pts',(-4.13257666800006,11.6,-10.104384672));
#292200=CARTESIAN_POINT('Ctrl Pts',(-4.13275197800006,15.2,-10.107287044));
#292201=CARTESIAN_POINT('Ctrl Pts',(-4.13275197800006,11.6,-10.107287044));
#292202=CARTESIAN_POINT('Ctrl Pts',(-4.13292521800006,15.2,-10.110195076));
#292203=CARTESIAN_POINT('Ctrl Pts',(-4.13292521800006,11.6,-10.110195076));
#292204=CARTESIAN_POINT('Ctrl Pts',(-4.13309637800006,15.2,-10.113108759));
#292205=CARTESIAN_POINT('Ctrl Pts',(-4.13309637800006,11.6,-10.113108759));
#292206=CARTESIAN_POINT('Ctrl Pts',(-4.13326545000006,15.2,-10.116028082));
#292207=CARTESIAN_POINT('Ctrl Pts',(-4.13326545000006,11.6,-10.116028082));
#292208=CARTESIAN_POINT('Ctrl Pts',(-4.13343242600006,15.2,-10.118953036));
#292209=CARTESIAN_POINT('Ctrl Pts',(-4.13343242600006,11.6,-10.118953036));
#292210=CARTESIAN_POINT('Ctrl Pts',(-4.13359729700006,15.2,-10.121883613));
#292211=CARTESIAN_POINT('Ctrl Pts',(-4.13359729700006,11.6,-10.121883613));
#292212=CARTESIAN_POINT('Ctrl Pts',(-4.13376005400006,15.2,-10.124819802));
#292213=CARTESIAN_POINT('Ctrl Pts',(-4.13376005400006,11.6,-10.124819802));
#292214=CARTESIAN_POINT('Ctrl Pts',(-4.13392069200006,15.2,-10.127761595));
#292215=CARTESIAN_POINT('Ctrl Pts',(-4.13392069200006,11.6,-10.127761595));
#292216=CARTESIAN_POINT('Ctrl Pts',(-4.13407919800005,15.2,-10.130708982));
#292217=CARTESIAN_POINT('Ctrl Pts',(-4.13407919800005,11.6,-10.130708982));
#292218=CARTESIAN_POINT('Ctrl Pts',(-4.13423556800006,15.2,-10.133661953));
#292219=CARTESIAN_POINT('Ctrl Pts',(-4.13423556800006,11.6,-10.133661953));
#292220=CARTESIAN_POINT('Ctrl Pts',(-4.13438979000006,15.2,-10.136620499));
#292221=CARTESIAN_POINT('Ctrl Pts',(-4.13438979000006,11.6,-10.136620499));
#292222=CARTESIAN_POINT('Ctrl Pts',(-4.13454185900005,15.2,-10.139584612));
#292223=CARTESIAN_POINT('Ctrl Pts',(-4.13454185900005,11.6,-10.139584612));
#292224=CARTESIAN_POINT('Ctrl Pts',(-4.13469176500006,15.2,-10.142554281));
#292225=CARTESIAN_POINT('Ctrl Pts',(-4.13469176500006,11.6,-10.142554281));
#292226=CARTESIAN_POINT('Ctrl Pts',(-4.13483950100006,15.2,-10.145529497));
#292227=CARTESIAN_POINT('Ctrl Pts',(-4.13483950100006,11.6,-10.145529497));
#292228=CARTESIAN_POINT('Ctrl Pts',(-4.13498505800006,15.2,-10.148510251));
#292229=CARTESIAN_POINT('Ctrl Pts',(-4.13498505800006,11.6,-10.148510251));
#292230=CARTESIAN_POINT('Ctrl Pts',(-4.13512842900006,15.2,-10.151496534));
#292231=CARTESIAN_POINT('Ctrl Pts',(-4.13512842900006,11.6,-10.151496534));
#292232=CARTESIAN_POINT('Ctrl Pts',(-4.13526960400006,15.2,-10.154488337));
#292233=CARTESIAN_POINT('Ctrl Pts',(-4.13526960400006,11.6,-10.154488337));
#292234=CARTESIAN_POINT('Ctrl Pts',(-4.13540857600006,15.2,-10.15748565));
#292235=CARTESIAN_POINT('Ctrl Pts',(-4.13540857600006,11.6,-10.15748565));
#292236=CARTESIAN_POINT('Ctrl Pts',(-4.13554533800006,15.2,-10.160488466));
#292237=CARTESIAN_POINT('Ctrl Pts',(-4.13554533800006,11.6,-10.160488466));
#292238=CARTESIAN_POINT('Ctrl Pts',(-4.13567988100006,15.2,-10.163496771));
#292239=CARTESIAN_POINT('Ctrl Pts',(-4.13567988100006,11.6,-10.163496771));
#292240=CARTESIAN_POINT('Ctrl Pts',(-4.13581219700006,15.2,-10.16651056));
#292241=CARTESIAN_POINT('Ctrl Pts',(-4.13581219700006,11.6,-10.16651056));
#292242=CARTESIAN_POINT('Ctrl Pts',(-4.13594227700006,15.2,-10.169529823));
#292243=CARTESIAN_POINT('Ctrl Pts',(-4.13594227700006,11.6,-10.169529823));
#292244=CARTESIAN_POINT('Ctrl Pts',(-4.13607011600006,15.2,-10.17255455));
#292245=CARTESIAN_POINT('Ctrl Pts',(-4.13607011600006,11.6,-10.17255455));
#292246=CARTESIAN_POINT('Ctrl Pts',(-4.13619570300006,15.2,-10.175584733));
#292247=CARTESIAN_POINT('Ctrl Pts',(-4.13619570300006,11.6,-10.175584733));
#292248=CARTESIAN_POINT('Ctrl Pts',(-4.13631903200006,15.2,-10.178620362));
#292249=CARTESIAN_POINT('Ctrl Pts',(-4.13631903200006,11.6,-10.178620362));
#292250=CARTESIAN_POINT('Ctrl Pts',(-4.13644009500006,15.2,-10.181661427));
#292251=CARTESIAN_POINT('Ctrl Pts',(-4.13644009500006,11.6,-10.181661427));
#292252=CARTESIAN_POINT('Ctrl Pts',(-4.13655888400006,15.2,-10.184707922));
#292253=CARTESIAN_POINT('Ctrl Pts',(-4.13655888400006,11.6,-10.184707922));
#292254=CARTESIAN_POINT('Ctrl Pts',(-4.13667539100006,15.2,-10.187759834));
#292255=CARTESIAN_POINT('Ctrl Pts',(-4.13667539100006,11.6,-10.187759834));
#292256=CARTESIAN_POINT('Ctrl Pts',(-4.13678960800006,15.2,-10.190817158));
#292257=CARTESIAN_POINT('Ctrl Pts',(-4.13678960800006,11.6,-10.190817158));
#292258=CARTESIAN_POINT('Ctrl Pts',(-4.13690152700006,15.2,-10.193879881));
#292259=CARTESIAN_POINT('Ctrl Pts',(-4.13690152700006,11.6,-10.193879881));
#292260=CARTESIAN_POINT('Ctrl Pts',(-4.13701114100006,15.2,-10.196947997));
#292261=CARTESIAN_POINT('Ctrl Pts',(-4.13701114100006,11.6,-10.196947997));
#292262=CARTESIAN_POINT('Ctrl Pts',(-4.13711844300006,15.2,-10.200021495));
#292263=CARTESIAN_POINT('Ctrl Pts',(-4.13711844300006,11.6,-10.200021495));
#292264=CARTESIAN_POINT('Ctrl Pts',(-4.13722342400006,15.2,-10.203100366));
#292265=CARTESIAN_POINT('Ctrl Pts',(-4.13722342400006,11.6,-10.203100366));
#292266=CARTESIAN_POINT('Ctrl Pts',(-4.13732607700006,15.2,-10.206184603));
#292267=CARTESIAN_POINT('Ctrl Pts',(-4.13732607700006,11.6,-10.206184603));
#292268=CARTESIAN_POINT('Ctrl Pts',(-4.13742639400006,15.2,-10.209274195));
#292269=CARTESIAN_POINT('Ctrl Pts',(-4.13742639400006,11.6,-10.209274195));
#292270=CARTESIAN_POINT('Ctrl Pts',(-4.13752436800006,15.2,-10.212369135));
#292271=CARTESIAN_POINT('Ctrl Pts',(-4.13752436800006,11.6,-10.212369135));
#292272=CARTESIAN_POINT('Ctrl Pts',(-4.13761999100006,15.2,-10.215469411));
#292273=CARTESIAN_POINT('Ctrl Pts',(-4.13761999100006,11.6,-10.215469411));
#292274=CARTESIAN_POINT('Ctrl Pts',(-4.13771325500006,15.2,-10.218575018));
#292275=CARTESIAN_POINT('Ctrl Pts',(-4.13771325500006,11.6,-10.218575018));
#292276=CARTESIAN_POINT('Ctrl Pts',(-4.13780415300006,15.2,-10.221685943));
#292277=CARTESIAN_POINT('Ctrl Pts',(-4.13780415300006,11.6,-10.221685943));
#292278=CARTESIAN_POINT('Ctrl Pts',(-4.13789267800006,15.2,-10.224802181));
#292279=CARTESIAN_POINT('Ctrl Pts',(-4.13789267800006,11.6,-10.224802181));
#292280=CARTESIAN_POINT('Ctrl Pts',(-4.13797882100006,15.2,-10.22792372));
#292281=CARTESIAN_POINT('Ctrl Pts',(-4.13797882100006,11.6,-10.22792372));
#292282=CARTESIAN_POINT('Ctrl Pts',(-4.13806257600006,15.2,-10.231050552));
#292283=CARTESIAN_POINT('Ctrl Pts',(-4.13806257600006,11.6,-10.231050552));
#292284=CARTESIAN_POINT('Ctrl Pts',(-4.13814393400005,15.2,-10.234182669));
#292285=CARTESIAN_POINT('Ctrl Pts',(-4.13814393400005,11.6,-10.234182669));
#292286=CARTESIAN_POINT('Ctrl Pts',(-4.13822289000006,15.2,-10.237320063));
#292287=CARTESIAN_POINT('Ctrl Pts',(-4.13822289000006,11.6,-10.237320063));
#292288=CARTESIAN_POINT('Ctrl Pts',(-4.13829943500006,15.2,-10.240462721));
#292289=CARTESIAN_POINT('Ctrl Pts',(-4.13829943500006,11.6,-10.240462721));
#292290=CARTESIAN_POINT('Ctrl Pts',(-4.13837356100006,15.2,-10.243610638));
#292291=CARTESIAN_POINT('Ctrl Pts',(-4.13837356100006,11.6,-10.243610638));
#292292=CARTESIAN_POINT('Ctrl Pts',(-4.13844526300006,15.2,-10.246763805));
#292293=CARTESIAN_POINT('Ctrl Pts',(-4.13844526300006,11.6,-10.246763805));
#292294=CARTESIAN_POINT('Ctrl Pts',(-4.13851453100006,15.2,-10.249922211));
#292295=CARTESIAN_POINT('Ctrl Pts',(-4.13851453100006,11.6,-10.249922211));
#292296=CARTESIAN_POINT('Ctrl Pts',(-4.13858135900006,15.2,-10.253085849));
#292297=CARTESIAN_POINT('Ctrl Pts',(-4.13858135900006,11.6,-10.253085849));
#292298=CARTESIAN_POINT('Ctrl Pts',(-4.13864573900006,15.2,-10.25625471));
#292299=CARTESIAN_POINT('Ctrl Pts',(-4.13864573900006,11.6,-10.25625471));
#292300=CARTESIAN_POINT('Ctrl Pts',(-4.13870766600006,15.2,-10.259428784));
#292301=CARTESIAN_POINT('Ctrl Pts',(-4.13870766600006,11.6,-10.259428784));
#292302=CARTESIAN_POINT('Ctrl Pts',(-4.13876712900006,15.2,-10.262608063));
#292303=CARTESIAN_POINT('Ctrl Pts',(-4.13876712900006,11.6,-10.262608063));
#292304=CARTESIAN_POINT('Ctrl Pts',(-4.13882412400006,15.2,-10.265792539));
#292305=CARTESIAN_POINT('Ctrl Pts',(-4.13882412400006,11.6,-10.265792539));
#292306=CARTESIAN_POINT('Ctrl Pts',(-4.13887864300006,15.2,-10.268982202));
#292307=CARTESIAN_POINT('Ctrl Pts',(-4.13887864300006,11.6,-10.268982202));
#292308=CARTESIAN_POINT('Ctrl Pts',(-4.13893067800006,15.2,-10.272177045));
#292309=CARTESIAN_POINT('Ctrl Pts',(-4.13893067800006,11.6,-10.272177045));
#292310=CARTESIAN_POINT('Ctrl Pts',(-4.13898022300006,15.2,-10.275377057));
#292311=CARTESIAN_POINT('Ctrl Pts',(-4.13898022300006,11.6,-10.275377057));
#292312=CARTESIAN_POINT('Ctrl Pts',(-4.13902726900006,15.2,-10.278582232));
#292313=CARTESIAN_POINT('Ctrl Pts',(-4.13902726900006,11.6,-10.278582232));
#292314=CARTESIAN_POINT('Ctrl Pts',(-4.13907181100006,15.2,-10.28179256));
#292315=CARTESIAN_POINT('Ctrl Pts',(-4.13907181100006,11.6,-10.28179256));
#292316=CARTESIAN_POINT('Ctrl Pts',(-4.13911384100006,15.2,-10.28500803));
#292317=CARTESIAN_POINT('Ctrl Pts',(-4.13911384100006,11.6,-10.28500803));
#292318=CARTESIAN_POINT('Ctrl Pts',(-4.13915335200006,15.2,-10.288228637));
#292319=CARTESIAN_POINT('Ctrl Pts',(-4.13915335200006,11.6,-10.288228637));
#292320=CARTESIAN_POINT('Ctrl Pts',(-4.13919033700005,15.2,-10.291454371));
#292321=CARTESIAN_POINT('Ctrl Pts',(-4.13919033700005,11.6,-10.291454371));
#292322=CARTESIAN_POINT('Ctrl Pts',(-4.13922478800006,15.2,-10.294685224));
#292323=CARTESIAN_POINT('Ctrl Pts',(-4.13922478800006,11.6,-10.294685224));
#292324=CARTESIAN_POINT('Ctrl Pts',(-4.13925670000006,15.2,-10.297921185));
#292325=CARTESIAN_POINT('Ctrl Pts',(-4.13925670000006,11.6,-10.297921185));
#292326=CARTESIAN_POINT('Ctrl Pts',(-4.13928606500006,15.2,-10.301162248));
#292327=CARTESIAN_POINT('Ctrl Pts',(-4.13928606500006,11.6,-10.301162248));
#292328=CARTESIAN_POINT('Ctrl Pts',(-4.13931287600006,15.2,-10.304408403));
#292329=CARTESIAN_POINT('Ctrl Pts',(-4.13931287600006,11.6,-10.304408403));
#292330=CARTESIAN_POINT('Ctrl Pts',(-4.13933712500006,15.2,-10.307659642));
#292331=CARTESIAN_POINT('Ctrl Pts',(-4.13933712500006,11.6,-10.307659642));
#292332=CARTESIAN_POINT('Ctrl Pts',(-4.13935880700006,15.2,-10.310915957));
#292333=CARTESIAN_POINT('Ctrl Pts',(-4.13935880700006,11.6,-10.310915957));
#292334=CARTESIAN_POINT('Ctrl Pts',(-4.13937791400006,15.2,-10.314177337));
#292335=CARTESIAN_POINT('Ctrl Pts',(-4.13937791400006,11.6,-10.314177337));
#292336=CARTESIAN_POINT('Ctrl Pts',(-4.13939443900006,15.2,-10.317443776));
#292337=CARTESIAN_POINT('Ctrl Pts',(-4.13939443900006,11.6,-10.317443776));
#292338=CARTESIAN_POINT('Ctrl Pts',(-4.13940837600006,15.2,-10.320715266));
#292339=CARTESIAN_POINT('Ctrl Pts',(-4.13940837600006,11.6,-10.320715266));
#292340=CARTESIAN_POINT('Ctrl Pts',(-4.13941971700006,15.2,-10.323991796));
#292341=CARTESIAN_POINT('Ctrl Pts',(-4.13941971700006,11.6,-10.323991796));
#292342=CARTESIAN_POINT('Ctrl Pts',(-4.13942845700006,15.2,-10.327273358));
#292343=CARTESIAN_POINT('Ctrl Pts',(-4.13942845700006,11.6,-10.327273358));
#292344=CARTESIAN_POINT('Ctrl Pts',(-4.13943458800006,15.2,-10.330559945));
#292345=CARTESIAN_POINT('Ctrl Pts',(-4.13943458800006,11.6,-10.330559945));
#292346=CARTESIAN_POINT('Ctrl Pts',(-4.13943810200006,15.2,-10.333851548));
#292347=CARTESIAN_POINT('Ctrl Pts',(-4.13943810200006,11.6,-10.333851548));
#292348=CARTESIAN_POINT('Ctrl Pts',(-4.13943899400006,15.2,-10.337148156));
#292349=CARTESIAN_POINT('Ctrl Pts',(-4.13943899400006,11.6,-10.337148156));
#292350=CARTESIAN_POINT('Ctrl Pts',(-4.13943725800006,15.2,-10.340449765));
#292351=CARTESIAN_POINT('Ctrl Pts',(-4.13943725800006,11.6,-10.340449765));
#292352=CARTESIAN_POINT('Ctrl Pts',(-4.13943288500006,15.2,-10.343756364));
#292353=CARTESIAN_POINT('Ctrl Pts',(-4.13943288500006,11.6,-10.343756364));
#292354=CARTESIAN_POINT('Ctrl Pts',(-4.13942587000006,15.2,-10.347067944));
#292355=CARTESIAN_POINT('Ctrl Pts',(-4.13942587000006,11.6,-10.347067944));
#292356=CARTESIAN_POINT('Ctrl Pts',(-4.13941620600006,15.2,-10.350384497));
#292357=CARTESIAN_POINT('Ctrl Pts',(-4.13941620600006,11.6,-10.350384497));
#292358=CARTESIAN_POINT('Ctrl Pts',(-4.13940388500006,15.2,-10.353706015));
#292359=CARTESIAN_POINT('Ctrl Pts',(-4.13940388500006,11.6,-10.353706015));
#292360=CARTESIAN_POINT('Ctrl Pts',(-4.13938890200006,15.2,-10.357032491));
#292361=CARTESIAN_POINT('Ctrl Pts',(-4.13938890200006,11.6,-10.357032491));
#292362=CARTESIAN_POINT('Ctrl Pts',(-4.13937125000006,15.2,-10.360363914));
#292363=CARTESIAN_POINT('Ctrl Pts',(-4.13937125000006,11.6,-10.360363914));
#292364=CARTESIAN_POINT('Ctrl Pts',(-4.13935092200005,15.2,-10.363700277));
#292365=CARTESIAN_POINT('Ctrl Pts',(-4.13935092200005,11.6,-10.363700277));
#292366=CARTESIAN_POINT('Ctrl Pts',(-4.13932791200006,15.2,-10.367041572));
#292367=CARTESIAN_POINT('Ctrl Pts',(-4.13932791200006,11.6,-10.367041572));
#292368=CARTESIAN_POINT('Ctrl Pts',(-4.13930221300006,15.2,-10.370387789));
#292369=CARTESIAN_POINT('Ctrl Pts',(-4.13930221300006,11.6,-10.370387789));
#292370=CARTESIAN_POINT('Ctrl Pts',(-4.13927381800006,15.2,-10.373738921));
#292371=CARTESIAN_POINT('Ctrl Pts',(-4.13927381800006,11.6,-10.373738921));
#292372=CARTESIAN_POINT('Ctrl Pts',(-4.13924272200005,15.2,-10.37709496));
#292373=CARTESIAN_POINT('Ctrl Pts',(-4.13924272200005,11.6,-10.37709496));
#292374=CARTESIAN_POINT('Ctrl Pts',(-4.13920891800006,15.2,-10.380455896));
#292375=CARTESIAN_POINT('Ctrl Pts',(-4.13920891800006,11.6,-10.380455896));
#292376=CARTESIAN_POINT('Ctrl Pts',(-4.13917239900006,15.2,-10.383821723));
#292377=CARTESIAN_POINT('Ctrl Pts',(-4.13917239900006,11.6,-10.383821723));
#292378=CARTESIAN_POINT('Ctrl Pts',(-4.13913315700006,15.2,-10.38719243));
#292379=CARTESIAN_POINT('Ctrl Pts',(-4.13913315700006,11.6,-10.38719243));
#292380=CARTESIAN_POINT('Ctrl Pts',(-4.13909119000006,15.2,-10.390568011));
#292381=CARTESIAN_POINT('Ctrl Pts',(-4.13909119000006,11.6,-10.390568011));
#292382=CARTESIAN_POINT('Ctrl Pts',(-4.13904648600006,15.2,-10.393948456));
#292383=CARTESIAN_POINT('Ctrl Pts',(-4.13904648600006,11.6,-10.393948456));
#292384=CARTESIAN_POINT('Ctrl Pts',(-4.13899904400005,15.2,-10.397333758));
#292385=CARTESIAN_POINT('Ctrl Pts',(-4.13899904400005,11.6,-10.397333758));
#292386=CARTESIAN_POINT('Ctrl Pts',(-4.13894885300006,15.2,-10.400723908));
#292387=CARTESIAN_POINT('Ctrl Pts',(-4.13894885300006,11.6,-10.400723908));
#292388=CARTESIAN_POINT('Ctrl Pts',(-4.13889591000006,15.2,-10.404118899));
#292389=CARTESIAN_POINT('Ctrl Pts',(-4.13889591000006,11.6,-10.404118899));
#292390=CARTESIAN_POINT('Ctrl Pts',(-4.13884020700006,15.2,-10.407518722));
#292391=CARTESIAN_POINT('Ctrl Pts',(-4.13884020700006,11.6,-10.407518722));
#292392=CARTESIAN_POINT('Ctrl Pts',(-4.13878173800006,15.2,-10.410923367));
#292393=CARTESIAN_POINT('Ctrl Pts',(-4.13878173800006,11.6,-10.410923367));
#292394=CARTESIAN_POINT('Ctrl Pts',(-4.13872049700006,15.2,-10.414332828));
#292395=CARTESIAN_POINT('Ctrl Pts',(-4.13872049700006,11.6,-10.414332828));
#292396=CARTESIAN_POINT('Ctrl Pts',(-4.13865647700006,15.2,-10.417747096));
#292397=CARTESIAN_POINT('Ctrl Pts',(-4.13865647700006,11.6,-10.417747096));
#292398=CARTESIAN_POINT('Ctrl Pts',(-4.13858967300006,15.2,-10.421166163));
#292399=CARTESIAN_POINT('Ctrl Pts',(-4.13858967300006,11.6,-10.421166163));
#292400=CARTESIAN_POINT('Ctrl Pts',(-4.13852007700005,15.2,-10.424590021));
#292401=CARTESIAN_POINT('Ctrl Pts',(-4.13852007700005,11.6,-10.424590021));
#292402=CARTESIAN_POINT('Ctrl Pts',(-4.13844768400006,15.2,-10.428018661));
#292403=CARTESIAN_POINT('Ctrl Pts',(-4.13844768400006,11.6,-10.428018661));
#292404=CARTESIAN_POINT('Ctrl Pts',(-4.13837248800006,15.2,-10.431452076));
#292405=CARTESIAN_POINT('Ctrl Pts',(-4.13837248800006,11.6,-10.431452076));
#292406=CARTESIAN_POINT('Ctrl Pts',(-4.13829448200006,15.2,-10.434890257));
#292407=CARTESIAN_POINT('Ctrl Pts',(-4.13829448200006,11.6,-10.434890257));
#292408=CARTESIAN_POINT('Ctrl Pts',(-4.13821365900006,15.2,-10.438333197));
#292409=CARTESIAN_POINT('Ctrl Pts',(-4.13821365900006,11.6,-10.438333197));
#292410=CARTESIAN_POINT('Ctrl Pts',(-4.13813001600006,15.2,-10.441780886));
#292411=CARTESIAN_POINT('Ctrl Pts',(-4.13813001600006,11.6,-10.441780886));
#292412=CARTESIAN_POINT('Ctrl Pts',(-4.13804354400006,15.2,-10.445233317));
#292413=CARTESIAN_POINT('Ctrl Pts',(-4.13804354400006,11.6,-10.445233317));
#292414=CARTESIAN_POINT('Ctrl Pts',(-4.13795423700006,15.2,-10.448690482));
#292415=CARTESIAN_POINT('Ctrl Pts',(-4.13795423700006,11.6,-10.448690482));
#292416=CARTESIAN_POINT('Ctrl Pts',(-4.13786209100006,15.2,-10.452152372));
#292417=CARTESIAN_POINT('Ctrl Pts',(-4.13786209100006,11.6,-10.452152372));
#292418=CARTESIAN_POINT('Ctrl Pts',(-4.13776709800006,15.2,-10.45561898));
#292419=CARTESIAN_POINT('Ctrl Pts',(-4.13776709800006,11.6,-10.45561898));
#292420=CARTESIAN_POINT('Ctrl Pts',(-4.13766925200005,15.2,-10.459090298));
#292421=CARTESIAN_POINT('Ctrl Pts',(-4.13766925200005,11.6,-10.459090298));
#292422=CARTESIAN_POINT('Ctrl Pts',(-4.13756854800006,15.2,-10.462566317));
#292423=CARTESIAN_POINT('Ctrl Pts',(-4.13756854800006,11.6,-10.462566317));
#292424=CARTESIAN_POINT('Ctrl Pts',(-4.13746498000005,15.2,-10.466047029));
#292425=CARTESIAN_POINT('Ctrl Pts',(-4.13746498000005,11.6,-10.466047029));
#292426=CARTESIAN_POINT('Ctrl Pts',(-4.13735854100006,15.2,-10.469532426));
#292427=CARTESIAN_POINT('Ctrl Pts',(-4.13735854100006,11.6,-10.469532426));
#292428=CARTESIAN_POINT('Ctrl Pts',(-4.13724922400006,15.2,-10.473022501));
#292429=CARTESIAN_POINT('Ctrl Pts',(-4.13724922400006,11.6,-10.473022501));
#292430=CARTESIAN_POINT('Ctrl Pts',(-4.13713702600006,15.2,-10.476517244));
#292431=CARTESIAN_POINT('Ctrl Pts',(-4.13713702600006,11.6,-10.476517244));
#292432=CARTESIAN_POINT('Ctrl Pts',(-4.13702193900006,15.2,-10.480016649));
#292433=CARTESIAN_POINT('Ctrl Pts',(-4.13702193900006,11.6,-10.480016649));
#292434=CARTESIAN_POINT('Ctrl Pts',(-4.13690395800006,15.2,-10.483520708));
#292435=CARTESIAN_POINT('Ctrl Pts',(-4.13690395800006,11.6,-10.483520708));
#292436=CARTESIAN_POINT('Ctrl Pts',(-4.13678307500006,15.2,-10.487029411));
#292437=CARTESIAN_POINT('Ctrl Pts',(-4.13678307500006,11.6,-10.487029411));
#292438=CARTESIAN_POINT('Ctrl Pts',(-4.13665928800006,15.2,-10.490542752));
#292439=CARTESIAN_POINT('Ctrl Pts',(-4.13665928800006,11.6,-10.490542752));
#292440=CARTESIAN_POINT('Ctrl Pts',(-4.13653258700006,15.2,-10.494060721));
#292441=CARTESIAN_POINT('Ctrl Pts',(-4.13653258700006,11.6,-10.494060721));
#292442=CARTESIAN_POINT('Ctrl Pts',(-4.13640296900006,15.2,-10.497583313));
#292443=CARTESIAN_POINT('Ctrl Pts',(-4.13640296900006,11.6,-10.497583313));
#292444=CARTESIAN_POINT('Ctrl Pts',(-4.13627042600006,15.2,-10.501110517));
#292445=CARTESIAN_POINT('Ctrl Pts',(-4.13627042600006,11.6,-10.501110517));
#292446=CARTESIAN_POINT('Ctrl Pts',(-4.13613495400006,15.2,-10.504642327));
#292447=CARTESIAN_POINT('Ctrl Pts',(-4.13613495400006,11.6,-10.504642327));
#292448=CARTESIAN_POINT('Ctrl Pts',(-4.13599654700006,15.2,-10.508178734));
#292449=CARTESIAN_POINT('Ctrl Pts',(-4.13599654700006,11.6,-10.508178734));
#292450=CARTESIAN_POINT('Ctrl Pts',(-4.13585519800006,15.2,-10.51171973));
#292451=CARTESIAN_POINT('Ctrl Pts',(-4.13585519800006,11.6,-10.51171973));
#292452=CARTESIAN_POINT('Ctrl Pts',(-4.13571090200006,15.2,-10.515265307));
#292453=CARTESIAN_POINT('Ctrl Pts',(-4.13571090200006,11.6,-10.515265307));
#292454=CARTESIAN_POINT('Ctrl Pts',(-4.13556365200006,15.2,-10.518815459));
#292455=CARTESIAN_POINT('Ctrl Pts',(-4.13556365200006,11.6,-10.518815459));
#292456=CARTESIAN_POINT('Ctrl Pts',(-4.13541344500006,15.2,-10.522370176));
#292457=CARTESIAN_POINT('Ctrl Pts',(-4.13541344500006,11.6,-10.522370176));
#292458=CARTESIAN_POINT('Ctrl Pts',(-4.13526027300006,15.2,-10.525929452));
#292459=CARTESIAN_POINT('Ctrl Pts',(-4.13526027300006,11.6,-10.525929452));
#292460=CARTESIAN_POINT('Ctrl Pts',(-4.13510413100005,15.2,-10.529493276));
#292461=CARTESIAN_POINT('Ctrl Pts',(-4.13510413100005,11.6,-10.529493276));
#292462=CARTESIAN_POINT('Ctrl Pts',(-4.13494501300006,15.2,-10.533061643));
#292463=CARTESIAN_POINT('Ctrl Pts',(-4.13494501300006,11.6,-10.533061643));
#292464=CARTESIAN_POINT('Ctrl Pts',(-4.13478291300006,15.2,-10.536634544));
#292465=CARTESIAN_POINT('Ctrl Pts',(-4.13478291300006,11.6,-10.536634544));
#292466=CARTESIAN_POINT('Ctrl Pts',(-4.13461782600006,15.2,-10.540211971));
#292467=CARTESIAN_POINT('Ctrl Pts',(-4.13461782600006,11.6,-10.540211971));
#292468=CARTESIAN_POINT('Ctrl Pts',(-4.13444974700006,15.2,-10.543793918));
#292469=CARTESIAN_POINT('Ctrl Pts',(-4.13444974700006,11.6,-10.543793918));
#292470=CARTESIAN_POINT('Ctrl Pts',(-4.13427866800006,15.2,-10.547380374));
#292471=CARTESIAN_POINT('Ctrl Pts',(-4.13427866800006,11.6,-10.547380374));
#292472=CARTESIAN_POINT('Ctrl Pts',(-4.13410458600006,15.2,-10.550971334));
#292473=CARTESIAN_POINT('Ctrl Pts',(-4.13410458600006,11.6,-10.550971334));
#292474=CARTESIAN_POINT('Ctrl Pts',(-4.13392749300006,15.2,-10.554566788));
#292475=CARTESIAN_POINT('Ctrl Pts',(-4.13392749300006,11.6,-10.554566788));
#292476=CARTESIAN_POINT('Ctrl Pts',(-4.13374738600006,15.2,-10.558166729));
#292477=CARTESIAN_POINT('Ctrl Pts',(-4.13374738600006,11.6,-10.558166729));
#292478=CARTESIAN_POINT('Ctrl Pts',(-4.13356425900006,15.2,-10.561771151));
#292479=CARTESIAN_POINT('Ctrl Pts',(-4.13356425900006,11.6,-10.561771151));
#292480=CARTESIAN_POINT('Ctrl Pts',(-4.13337810400006,15.2,-10.565380043));
#292481=CARTESIAN_POINT('Ctrl Pts',(-4.13337810400006,11.6,-10.565380043));
#292482=CARTESIAN_POINT('Ctrl Pts',(-4.13318891700006,15.2,-10.568993399));
#292483=CARTESIAN_POINT('Ctrl Pts',(-4.13318891700006,11.6,-10.568993399));
#292484=CARTESIAN_POINT('Ctrl Pts',(-4.13299669400006,15.2,-10.572611212));
#292485=CARTESIAN_POINT('Ctrl Pts',(-4.13299669400006,11.6,-10.572611212));
#292486=CARTESIAN_POINT('Ctrl Pts',(-4.13280142700006,15.2,-10.576233472));
#292487=CARTESIAN_POINT('Ctrl Pts',(-4.13280142700006,11.6,-10.576233472));
#292488=CARTESIAN_POINT('Ctrl Pts',(-4.13260311100006,15.2,-10.579860172));
#292489=CARTESIAN_POINT('Ctrl Pts',(-4.13260311100006,11.6,-10.579860172));
#292490=CARTESIAN_POINT('Ctrl Pts',(-4.13240174200006,15.2,-10.583491306));
#292491=CARTESIAN_POINT('Ctrl Pts',(-4.13240174200006,11.6,-10.583491306));
#292492=CARTESIAN_POINT('Ctrl Pts',(-4.13219731300006,15.2,-10.587126866));
#292493=CARTESIAN_POINT('Ctrl Pts',(-4.13219731300006,11.6,-10.587126866));
#292494=CARTESIAN_POINT('Ctrl Pts',(-4.13198981900006,15.2,-10.590766842));
#292495=CARTESIAN_POINT('Ctrl Pts',(-4.13198981900006,11.6,-10.590766842));
#292496=CARTESIAN_POINT('Ctrl Pts',(-4.13177925500006,15.2,-10.594411227));
#292497=CARTESIAN_POINT('Ctrl Pts',(-4.13177925500006,11.6,-10.594411227));
#292498=CARTESIAN_POINT('Ctrl Pts',(-4.13156561600006,15.2,-10.598060015));
#292499=CARTESIAN_POINT('Ctrl Pts',(-4.13156561600006,11.6,-10.598060015));
#292500=CARTESIAN_POINT('Ctrl Pts',(-4.13134889500006,15.2,-10.601713197));
#292501=CARTESIAN_POINT('Ctrl Pts',(-4.13134889500006,11.6,-10.601713197));
#292502=CARTESIAN_POINT('Ctrl Pts',(-4.13112908800006,15.2,-10.605370765));
#292503=CARTESIAN_POINT('Ctrl Pts',(-4.13112908800006,11.6,-10.605370765));
#292504=CARTESIAN_POINT('Ctrl Pts',(-4.13090618900006,15.2,-10.609032712));
#292505=CARTESIAN_POINT('Ctrl Pts',(-4.13090618900006,11.6,-10.609032712));
#292506=CARTESIAN_POINT('Ctrl Pts',(-4.13068019400006,15.2,-10.61269903));
#292507=CARTESIAN_POINT('Ctrl Pts',(-4.13068019400006,11.6,-10.61269903));
#292508=CARTESIAN_POINT('Ctrl Pts',(-4.13045109500006,15.2,-10.616369712));
#292509=CARTESIAN_POINT('Ctrl Pts',(-4.13045109500006,11.6,-10.616369712));
#292510=CARTESIAN_POINT('Ctrl Pts',(-4.13021888800006,15.2,-10.62004475));
#292511=CARTESIAN_POINT('Ctrl Pts',(-4.13021888800006,11.6,-10.62004475));
#292512=CARTESIAN_POINT('Ctrl Pts',(-4.12998356800006,15.2,-10.623724135));
#292513=CARTESIAN_POINT('Ctrl Pts',(-4.12998356800006,11.6,-10.623724135));
#292514=CARTESIAN_POINT('Ctrl Pts',(-4.12974513000006,15.2,-10.627407861));
#292515=CARTESIAN_POINT('Ctrl Pts',(-4.12974513000006,11.6,-10.627407861));
#292516=CARTESIAN_POINT('Ctrl Pts',(-4.12950356800006,15.2,-10.63109592));
#292517=CARTESIAN_POINT('Ctrl Pts',(-4.12950356800006,11.6,-10.63109592));
#292518=CARTESIAN_POINT('Ctrl Pts',(-4.12925887700006,15.2,-10.634788304));
#292519=CARTESIAN_POINT('Ctrl Pts',(-4.12925887700006,11.6,-10.634788304));
#292520=CARTESIAN_POINT('Ctrl Pts',(-4.12901105200006,15.2,-10.638485006));
#292521=CARTESIAN_POINT('Ctrl Pts',(-4.12901105200006,11.6,-10.638485006));
#292522=CARTESIAN_POINT('Ctrl Pts',(-4.12876008700006,15.2,-10.642186017));
#292523=CARTESIAN_POINT('Ctrl Pts',(-4.12876008700006,11.6,-10.642186017));
#292524=CARTESIAN_POINT('Ctrl Pts',(-4.12850597800006,15.2,-10.645891333));
#292525=CARTESIAN_POINT('Ctrl Pts',(-4.12850597800006,11.6,-10.645891333));
#292526=CARTESIAN_POINT('Ctrl Pts',(-4.12824872100006,15.2,-10.649600942));
#292527=CARTESIAN_POINT('Ctrl Pts',(-4.12824872100006,11.6,-10.649600942));
#292528=CARTESIAN_POINT('Ctrl Pts',(-4.12798830800006,15.2,-10.65331484));
#292529=CARTESIAN_POINT('Ctrl Pts',(-4.12798830800006,11.6,-10.65331484));
#292530=CARTESIAN_POINT('Ctrl Pts',(-4.12772473400006,15.2,-10.657033017));
#292531=CARTESIAN_POINT('Ctrl Pts',(-4.12772473400006,11.6,-10.657033017));
#292532=CARTESIAN_POINT('Ctrl Pts',(-4.12745799500006,15.2,-10.660755466));
#292533=CARTESIAN_POINT('Ctrl Pts',(-4.12745799500006,11.6,-10.660755466));
#292534=CARTESIAN_POINT('Ctrl Pts',(-4.12718808600006,15.2,-10.664482179));
#292535=CARTESIAN_POINT('Ctrl Pts',(-4.12718808600006,11.6,-10.664482179));
#292536=CARTESIAN_POINT('Ctrl Pts',(-4.12691499900006,15.2,-10.668213148));
#292537=CARTESIAN_POINT('Ctrl Pts',(-4.12691499900006,11.6,-10.668213148));
#292538=CARTESIAN_POINT('Ctrl Pts',(-4.12663873100006,15.2,-10.671948366));
#292539=CARTESIAN_POINT('Ctrl Pts',(-4.12663873100006,11.6,-10.671948366));
#292540=CARTESIAN_POINT('Ctrl Pts',(-4.12635927800006,15.2,-10.675687825));
#292541=CARTESIAN_POINT('Ctrl Pts',(-4.12635927800006,11.6,-10.675687825));
#292542=CARTESIAN_POINT('Ctrl Pts',(-4.12607663400006,15.2,-10.67943152));
#292543=CARTESIAN_POINT('Ctrl Pts',(-4.12607663400006,11.6,-10.67943152));
#292544=CARTESIAN_POINT('Ctrl Pts',(-4.12579079500006,15.2,-10.683179442));
#292545=CARTESIAN_POINT('Ctrl Pts',(-4.12579079500006,11.6,-10.683179442));
#292546=CARTESIAN_POINT('Ctrl Pts',(-4.12550175600006,15.2,-10.686931586));
#292547=CARTESIAN_POINT('Ctrl Pts',(-4.12550175600006,11.6,-10.686931586));
#292548=CARTESIAN_POINT('Ctrl Pts',(-4.12520951300006,15.2,-10.690687943));
#292549=CARTESIAN_POINT('Ctrl Pts',(-4.12520951300006,11.6,-10.690687943));
#292550=CARTESIAN_POINT('Ctrl Pts',(-4.12491405900006,15.2,-10.694448508));
#292551=CARTESIAN_POINT('Ctrl Pts',(-4.12491405900006,11.6,-10.694448508));
#292552=CARTESIAN_POINT('Ctrl Pts',(-4.12461539100006,15.2,-10.698213269));
#292553=CARTESIAN_POINT('Ctrl Pts',(-4.12461539100006,11.6,-10.698213269));
#292554=CARTESIAN_POINT('Ctrl Pts',(-4.12431350000006,15.2,-10.701982219));
#292555=CARTESIAN_POINT('Ctrl Pts',(-4.12431350000006,11.6,-10.701982219));
#292556=CARTESIAN_POINT('Ctrl Pts',(-4.12400838200006,15.2,-10.705755349));
#292557=CARTESIAN_POINT('Ctrl Pts',(-4.12400838200006,11.6,-10.705755349));
#292558=CARTESIAN_POINT('Ctrl Pts',(-4.12370002800006,15.2,-10.709532648));
#292559=CARTESIAN_POINT('Ctrl Pts',(-4.12370002800006,11.6,-10.709532648));
#292560=CARTESIAN_POINT('Ctrl Pts',(-4.12338843600006,15.2,-10.713314109));
#292561=CARTESIAN_POINT('Ctrl Pts',(-4.12338843600006,11.6,-10.713314109));
#292562=CARTESIAN_POINT('Ctrl Pts',(-4.12307360000006,15.2,-10.717099725));
#292563=CARTESIAN_POINT('Ctrl Pts',(-4.12307360000006,11.6,-10.717099725));
#292564=CARTESIAN_POINT('Ctrl Pts',(-4.12275551700006,15.2,-10.720889492));
#292565=CARTESIAN_POINT('Ctrl Pts',(-4.12275551700006,11.6,-10.720889492));
#292566=CARTESIAN_POINT('Ctrl Pts',(-4.12243418400006,15.2,-10.724683406));
#292567=CARTESIAN_POINT('Ctrl Pts',(-4.12243418400006,11.6,-10.724683406));
#292568=CARTESIAN_POINT('Ctrl Pts',(-4.12210960100006,15.2,-10.728481464));
#292569=CARTESIAN_POINT('Ctrl Pts',(-4.12210960100006,11.6,-10.728481464));
#292570=CARTESIAN_POINT('Ctrl Pts',(-4.12184733300006,15.2,-10.731523226));
#292571=CARTESIAN_POINT('Ctrl Pts',(-4.12184733300006,11.6,-10.731523226));
#292572=CARTESIAN_POINT('Ctrl Pts',(-4.12164917000006,15.2,-10.733806411));
#292573=CARTESIAN_POINT('Ctrl Pts',(-4.12164917000006,11.6,-10.733806411));
#292574=CARTESIAN_POINT('Ctrl Pts',(-4.12151641000006,15.2,-10.735329364));
#292575=CARTESIAN_POINT('Ctrl Pts',(-4.12151641000006,11.6,-10.735329364));
#292576=CARTESIAN_POINT('Ctrl Pts',(-4.12144986800006,15.2,-10.736091047));
#292577=CARTESIAN_POINT('Ctrl Pts',(-4.12144986800006,11.6,-10.736091047));
#292578=CARTESIAN_POINT('Ctrl Pts',(-4.04260911700006,15.2,-9.55499537100001));
#292579=CARTESIAN_POINT('Ctrl Pts',(-4.04316130262144,15.2,-9.55669455581129));
#292580=CARTESIAN_POINT('Ctrl Pts',(-4.04372605423532,15.2,-9.55844976611691));
#292581=CARTESIAN_POINT('Ctrl Pts',(-4.04430244636191,15.2,-9.56026027775997));
#292582=CARTESIAN_POINT('Ctrl Pts',(-4.04488161814269,15.2,-9.56207952060535));
#292583=CARTESIAN_POINT('Ctrl Pts',(-4.04547254558646,15.2,-9.56395460122364));
#292584=CARTESIAN_POINT('Ctrl Pts',(-4.04607433356661,15.2,-9.56588480617844));
#292585=CARTESIAN_POINT('Ctrl Pts',(-4.0466761214921,15.2,-9.56781501095792));
#292586=CARTESIAN_POINT('Ctrl Pts',(-4.047288768506,15.2,-9.5698003417657));
#292587=CARTESIAN_POINT('Ctrl Pts',(-4.04791140648337,15.2,-9.57184010177491));
#292588=CARTESIAN_POINT('Ctrl Pts',(-4.04853404446074,15.2,-9.57387986178411));
#292589=CARTESIAN_POINT('Ctrl Pts',(-4.04916667292143,15.1999999999999,
-9.57597405360779));
#292590=CARTESIAN_POINT('Ctrl Pts',(-4.04980844817965,15.2,-9.5781219995506));
#292591=CARTESIAN_POINT('Ctrl Pts',(-4.05045022349616,15.2,-9.58026994568851));
#292592=CARTESIAN_POINT('Ctrl Pts',(-4.05110114707708,15.2,-9.58247164586089));
#292593=CARTESIAN_POINT('Ctrl Pts',(-4.05176039953023,15.2,-9.5847264400707));
#292594=CARTESIAN_POINT('Ctrl Pts',(-4.0524196519235,15.2,-9.5869812340757));
#292595=CARTESIAN_POINT('Ctrl Pts',(-4.05308723483013,15.2,-9.58928912240923));
#292596=CARTESIAN_POINT('Ctrl Pts',(-4.05376235422535,15.2,-9.591649459501));
#292597=CARTESIAN_POINT('Ctrl Pts',(-4.05443747362059,15.2,-9.59400979659278));
#292598=CARTESIAN_POINT('Ctrl Pts',(-4.0551201277045,15.2,-9.59642258494927));
#292599=CARTESIAN_POINT('Ctrl Pts',(-4.05580954917917,15.2,-9.59888719110749));
#292600=CARTESIAN_POINT('Ctrl Pts',(-4.05649897071645,15.2,-9.60135179748957));
#292601=CARTESIAN_POINT('Ctrl Pts',(-4.05719515799624,15.2,-9.6038682244197));
#292602=CARTESIAN_POINT('Ctrl Pts',(-4.05789736261825,15.2,-9.60643585656314));
#292603=CARTESIAN_POINT('Ctrl Pts',(-4.05859956717648,15.2,-9.60900348847334));
#292604=CARTESIAN_POINT('Ctrl Pts',(-4.05930779063964,15.2,-9.61162232326542));
#292605=CARTESIAN_POINT('Ctrl Pts',(-4.06002130153062,15.2,-9.61429176142062));
#292606=CARTESIAN_POINT('Ctrl Pts',(-4.06073481242159,15.2,-9.61696119957584));
#292607=CARTESIAN_POINT('Ctrl Pts',(-4.06145361629545,15.2,-9.61968124038532));
#292608=CARTESIAN_POINT('Ctrl Pts',(-4.06217700018564,15.2,-9.62245129461584));
#292609=CARTESIAN_POINT('Ctrl Pts',(-4.06290038407583,15.2,-9.62522134884637));
#292610=CARTESIAN_POINT('Ctrl Pts',(-4.0636283523138,15.2,-9.6280414163698));
#292611=CARTESIAN_POINT('Ctrl Pts',(-4.06436021495361,15.2,-9.63091092167883));
#292612=CARTESIAN_POINT('Ctrl Pts',(-4.0650920776599,15.2,-9.63378042724854));
#292613=CARTESIAN_POINT('Ctrl Pts',(-4.06582783357492,15.2,-9.63669937083966));
#292614=CARTESIAN_POINT('Ctrl Pts',(-4.066566816532,15.2,-9.63966718542021));
#292615=CARTESIAN_POINT('Ctrl Pts',(-4.06730579942196,15.2,-9.64263499973116));
#292616=CARTESIAN_POINT('Ctrl Pts',(-4.06804800741506,15.2,-9.64565168660443));
#292617=CARTESIAN_POINT('Ctrl Pts',(-4.06879278847472,15.2,-9.64871669192355));
#292618=CARTESIAN_POINT('Ctrl Pts',(-4.06953756953436,15.2,-9.65178169724266));
#292619=CARTESIAN_POINT('Ctrl Pts',(-4.07028492545407,15.2,-9.65489502225683));
#292620=CARTESIAN_POINT('Ctrl Pts',(-4.07103421967672,15.2,-9.65805612363872));
#292621=CARTESIAN_POINT('Ctrl Pts',(-4.07178351396743,15.2,-9.66121722530775));
#292622=CARTESIAN_POINT('Ctrl Pts',(-4.07253474806667,15.2,-9.66442610292308));
#292623=CARTESIAN_POINT('Ctrl Pts',(-4.07328730227441,15.2,-9.66768222468592));
#292624=CARTESIAN_POINT('Ctrl Pts',(-4.07403985641379,15.2,-9.67093834615299));
#292625=CARTESIAN_POINT('Ctrl Pts',(-4.07479373164037,15.2,-9.67424171204671));
#292626=CARTESIAN_POINT('Ctrl Pts',(-4.07554832578305,15.2,-9.67759179952341));
#292627=CARTESIAN_POINT('Ctrl Pts',(-4.07630291992571,15.2,-9.68094188700013));
#292628=CARTESIAN_POINT('Ctrl Pts',(-4.07705823202017,15.2,-9.68433869613623));
#292629=CARTESIAN_POINT('Ctrl Pts',(-4.07781367540938,15.2,-9.68778171367465));
#292630=CARTESIAN_POINT('Ctrl Pts',(-4.07856911886721,15.2,-9.69122473152583));
#292631=CARTESIAN_POINT('Ctrl Pts',(-4.07932469262759,15.2,-9.69471395907011));
#292632=CARTESIAN_POINT('Ctrl Pts',(-4.08007982603977,15.2,-9.69824889127534));
#292633=CARTESIAN_POINT('Ctrl Pts',(-4.08083495938337,15.2,-9.70178382315949));
#292634=CARTESIAN_POINT('Ctrl Pts',(-4.08158965065244,15.2,-9.70536446190666));
#292635=CARTESIAN_POINT('Ctrl Pts',(-4.08234334204173,15.2,-9.70899030952492));
#292636=CARTESIAN_POINT('Ctrl Pts',(-4.0832226487082,15.2,-9.71322046529913));
#292637=CARTESIAN_POINT('Ctrl Pts',(-4.08410059079317,15.2,-9.7175121579116));
#292638=CARTESIAN_POINT('Ctrl Pts',(-4.08497631107267,15.2,-9.72186461460261));
#292639=CARTESIAN_POINT('Ctrl Pts',(-4.08572692841613,15.2,-9.72559529157269));
#292640=CARTESIAN_POINT('Ctrl Pts',(-4.08647590889386,15.2,-9.7293706133137));
#292641=CARTESIAN_POINT('Ctrl Pts',(-4.08722272453339,15.2,-9.73319010025826));
#292642=CARTESIAN_POINT('Ctrl Pts',(-4.08809400949141,15.2,-9.73764616859154));
#292643=CARTESIAN_POINT('Ctrl Pts',(-4.08896234769306,15.2,-9.74216235461556));
#292644=CARTESIAN_POINT('Ctrl Pts',(-4.08982691959674,15.2,-9.74673791065444));
#292645=CARTESIAN_POINT('Ctrl Pts',(-4.0904444709469,15.2,-9.75000616491704));
#292646=CARTESIAN_POINT('Ctrl Pts',(-4.09106010026381,15.2,-9.75330471188287));
#292647=CARTESIAN_POINT('Ctrl Pts',(-4.09167351588863,15.2,-9.75663328271865));
#292648=CARTESIAN_POINT('Ctrl Pts',(-4.09228693151345,15.2,-9.75996185355443));
#292649=CARTESIAN_POINT('Ctrl Pts',(-4.09289813542433,15.2,-9.76332045069072));
#292650=CARTESIAN_POINT('Ctrl Pts',(-4.09350683785468,15.2,-9.76670880819314));
#292651=CARTESIAN_POINT('Ctrl Pts',(-4.09411554021868,15.2,-9.77009716532623));
#292652=CARTESIAN_POINT('Ctrl Pts',(-4.09472174428668,15.2,-9.77351528533831));
#292653=CARTESIAN_POINT('Ctrl Pts',(-4.09532516672113,15.2,-9.77696290655733));
#292654=CARTESIAN_POINT('Ctrl Pts',(-4.09592858922136,15.2,-9.78041052815213));
#292655=CARTESIAN_POINT('Ctrl Pts',(-4.09652923228276,15.2,-9.78388765125482));
#292656=CARTESIAN_POINT('Ctrl Pts',(-4.09712681888023,15.2,-9.78739401805798));
#292657=CARTESIAN_POINT('Ctrl Pts',(-4.09784392283627,15.2,-9.7916016584511));
#292658=CARTESIAN_POINT('Ctrl Pts',(-4.0985566265532,15.2,-9.79585141337281));
#292659=CARTESIAN_POINT('Ctrl Pts',(-4.09926446254353,15.2,-9.80014284190685));
#292660=CARTESIAN_POINT('Ctrl Pts',(-4.09985432583665,15.2,-9.80371903215698));
#292661=CARTESIAN_POINT('Ctrl Pts',(-4.10044081003771,15.2,-9.80732416316734));
#292662=CARTESIAN_POINT('Ctrl Pts',(-4.1010236508013,15.2,-9.81095798497526));
#292663=CARTESIAN_POINT('Ctrl Pts',(-4.1016064915649,15.2,-9.81459180678317));
#292664=CARTESIAN_POINT('Ctrl Pts',(-4.10218568926452,15.2,-9.81825432077486));
#292665=CARTESIAN_POINT('Ctrl Pts',(-4.10276098183365,15.2,-9.82194527820773));
#292666=CARTESIAN_POINT('Ctrl Pts',(-4.10333627434006,15.2,-9.8256362352383));
#292667=CARTESIAN_POINT('Ctrl Pts',(-4.10390766522069,15.2,-9.82935563618167));
#292668=CARTESIAN_POINT('Ctrl Pts',(-4.1044748976592,15.2,-9.8331032367431));
#292669=CARTESIAN_POINT('Ctrl Pts',(-4.10504213015955,15.2,-9.83685083771302));
#292670=CARTESIAN_POINT('Ctrl Pts',(-4.10560520484884,15.2,-9.8406266399436));
#292671=CARTESIAN_POINT('Ctrl Pts',(-4.10616387221033,15.2,-9.84443040001075));
#292672=CARTESIAN_POINT('Ctrl Pts',(-4.1067225395718,15.2,-9.84823416007791));
#292673=CARTESIAN_POINT('Ctrl Pts',(-4.10727679784181,15.2,-9.85206587936669));
#292674=CARTESIAN_POINT('Ctrl Pts',(-4.10782640370292,15.2,-9.85592531879368));
#292675=CARTESIAN_POINT('Ctrl Pts',(-4.10859585192046,15.2,-9.86132853407562));
#292676=CARTESIAN_POINT('Ctrl Pts',(-4.10935617761061,15.2,-9.86678608025856));
#292677=CARTESIAN_POINT('Ctrl Pts',(-4.11010672452507,15.2,-9.87229731227494));
#292678=CARTESIAN_POINT('Ctrl Pts',(-4.11064282945563,15.2,-9.87623390651106));
#292679=CARTESIAN_POINT('Ctrl Pts',(-4.11117394296118,15.2,-9.88019789193882));
#292680=CARTESIAN_POINT('Ctrl Pts',(-4.11169983372507,15.2,-9.88418903471661));
#292681=CARTESIAN_POINT('Ctrl Pts',(-4.11222572448896,15.2,-9.88818017749438));
#292682=CARTESIAN_POINT('Ctrl Pts',(-4.11274638904247,15.2,-9.89219848073369));
#292683=CARTESIAN_POINT('Ctrl Pts',(-4.11326159751702,15.2,-9.89624371096049));
#292684=CARTESIAN_POINT('Ctrl Pts',(-4.11377680599157,15.2,-9.90028894118728));
#292685=CARTESIAN_POINT('Ctrl Pts',(-4.1142865584333,15.2,-9.90436110200566));
#292686=CARTESIAN_POINT('Ctrl Pts',(-4.11479062926633,15.2,-9.90845996228484));
#292687=CARTESIAN_POINT('Ctrl Pts',(-4.11529470009938,15.2,-9.91255882256402));
#292688=CARTESIAN_POINT('Ctrl Pts',(-4.11579308588255,15.2,-9.91668438523692));
#292689=CARTESIAN_POINT('Ctrl Pts',(-4.11628556754891,15.2,-9.92083642377998));
#292690=CARTESIAN_POINT('Ctrl Pts',(-4.11667955284979,15.2,-9.92415805434289));
#292691=CARTESIAN_POINT('Ctrl Pts',(-4.11706975713649,15.2,-9.92749663021293));
#292692=CARTESIAN_POINT('Ctrl Pts',(-4.11745606940233,15.2,-9.93085203627149));
#292693=CARTESIAN_POINT('Ctrl Pts',(-4.1178423817208,15.2,-9.93420744278723));
#292694=CARTESIAN_POINT('Ctrl Pts',(-4.11822480287172,15.2,-9.93757967973302));
#292695=CARTESIAN_POINT('Ctrl Pts',(-4.11860321978097,15.2,-9.94096863475215));
#292696=CARTESIAN_POINT('Ctrl Pts',(-4.11898163663866,15.2,-9.94435758930954));
#292697=CARTESIAN_POINT('Ctrl Pts',(-4.11935605002493,15.2,-9.94776326124409));
#292698=CARTESIAN_POINT('Ctrl Pts',(-4.11972635143953,15.2,-9.95118553840708));
#292699=CARTESIAN_POINT('Ctrl Pts',(-4.12009665290458,15.2,-9.95460781603635));
#292700=CARTESIAN_POINT('Ctrl Pts',(-4.1204628412873,15.2,-9.95804669827047));
#292701=CARTESIAN_POINT('Ctrl Pts',(-4.12082480947532,15.2,-9.9615020752523));
#292702=CARTESIAN_POINT('Ctrl Pts',(-4.12118677761402,15.2,-9.96495745176335));
#292703=CARTESIAN_POINT('Ctrl Pts',(-4.12154452473462,15.2,-9.96842932082201));
#292704=CARTESIAN_POINT('Ctrl Pts',(-4.12189794498395,15.2,-9.97191757397963));
#292705=CARTESIAN_POINT('Ctrl Pts',(-4.12225136528143,15.2,-9.97540582761253));
#292706=CARTESIAN_POINT('Ctrl Pts',(-4.12260045803685,15.2,-9.9789104647525));
#292707=CARTESIAN_POINT('Ctrl Pts',(-4.12294511950007,15.2,-9.98243137449994));
#292708=CARTESIAN_POINT('Ctrl Pts',(-4.1232897809633,15.2,-9.98595228424738));
#292709=CARTESIAN_POINT('Ctrl Pts',(-4.12363000999824,15.2,-9.9894894667106));
#292710=CARTESIAN_POINT('Ctrl Pts',(-4.12396570357162,15.2,-9.99304281507259));
#292711=CARTESIAN_POINT('Ctrl Pts',(-4.12430139709927,15.2,-9.99659616295044));
#292712=CARTESIAN_POINT('Ctrl Pts',(-4.12463255370282,15.2,-10.0001656746994));
#292713=CARTESIAN_POINT('Ctrl Pts',(-4.12495907323319,15.2,-10.0037512432558));
#292714=CARTESIAN_POINT('Ctrl Pts',(-4.12528559280803,15.2,-10.0073368123008));
#292715=CARTESIAN_POINT('Ctrl Pts',(-4.12560747311291,15.2,-10.0109384366482));
#292716=CARTESIAN_POINT('Ctrl Pts',(-4.12592461601859,15.2,-10.0145560116248));
#292717=CARTESIAN_POINT('Ctrl Pts',(-4.1263210446291,15.2,-10.019077980099));
#292718=CARTESIAN_POINT('Ctrl Pts',(-4.12671006683948,15.2,-10.0236248682959));
#292719=CARTESIAN_POINT('Ctrl Pts',(-4.1270914912833,15.2,-10.0281964693396));
#292720=CARTESIAN_POINT('Ctrl Pts',(-4.12739663081341,15.2,-10.0318537498756));
#292721=CARTESIAN_POINT('Ctrl Pts',(-4.1276969073921,15.2,-10.0355268451545));
#292722=CARTESIAN_POINT('Ctrl Pts',(-4.12799222175821,15.2,-10.0392156529808));
#292723=CARTESIAN_POINT('Ctrl Pts',(-4.12828753616455,15.2,-10.0429044613096));
#292724=CARTESIAN_POINT('Ctrl Pts',(-4.12857789011502,15.2,-10.0466089782455));
#292725=CARTESIAN_POINT('Ctrl Pts',(-4.12886318579672,15.2,-10.0503291026165));
#292726=CARTESIAN_POINT('Ctrl Pts',(-4.12921980537941,15.2,-10.0549792578269));
#292727=CARTESIAN_POINT('Ctrl Pts',(-4.12956852147862,15.2,-10.059653796857));
#292728=CARTESIAN_POINT('Ctrl Pts',(-4.12990914856129,15.2,-10.0643525163729));
#292729=CARTESIAN_POINT('Ctrl Pts',(-4.13018165020515,15.2,-10.0681114916783));
#292730=CARTESIAN_POINT('Ctrl Pts',(-4.13044897395067,15.2,-10.0718859438095));
#292731=CARTESIAN_POINT('Ctrl Pts',(-4.13071102754156,15.2,-10.075675767239));
#292732=CARTESIAN_POINT('Ctrl Pts',(-4.13097308116816,15.2,-10.079465591185));
#292733=CARTESIAN_POINT('Ctrl Pts',(-4.13122986381692,15.2,-10.0832707889315));
#292734=CARTESIAN_POINT('Ctrl Pts',(-4.13148128227451,15.2,-10.0870912561413));
#292735=CARTESIAN_POINT('Ctrl Pts',(-4.13173270069786,15.2,-10.0909117228305));
#292736=CARTESIAN_POINT('Ctrl Pts',(-4.13197875556911,15.2,-10.0947474600122));
#292737=CARTESIAN_POINT('Ctrl Pts',(-4.13221935527202,15.2,-10.0985983659186));
#292738=CARTESIAN_POINT('Ctrl Pts',(-4.13245995500772,15.2,-10.1024492723497));
#292739=CARTESIAN_POINT('Ctrl Pts',(-4.13269509902653,15.2,-10.1063153466676));
#292740=CARTESIAN_POINT('Ctrl Pts',(-4.13292469805003,15.2,-10.1101964892966));
#292741=CARTESIAN_POINT('Ctrl Pts',(-4.13315429704225,15.2,-10.1140776313967));
#292742=CARTESIAN_POINT('Ctrl Pts',(-4.1333783506441,15.2,-10.1179738397483));
#292743=CARTESIAN_POINT('Ctrl Pts',(-4.1335967685155,15.2,-10.1218850157054));
#292744=CARTESIAN_POINT('Ctrl Pts',(-4.13392439536725,15.2,-10.1277517804403));
#292745=CARTESIAN_POINT('Ctrl Pts',(-4.13423934470908,15.2,-10.1336522210044));
#292746=CARTESIAN_POINT('Ctrl Pts',(-4.13454131830799,15.2,-10.1395860016634));
#292747=CARTESIAN_POINT('Ctrl Pts',(-4.13474263401316,15.2,-10.1435418548971));
#292748=CARTESIAN_POINT('Ctrl Pts',(-4.13493818365069,15.2,-10.1475125246855));
#292749=CARTESIAN_POINT('Ctrl Pts',(-4.13512788002495,15.2,-10.1514979139889));
#292750=CARTESIAN_POINT('Ctrl Pts',(-4.13531757642506,15.2,-10.1554833038353));
#292751=CARTESIAN_POINT('Ctrl Pts',(-4.13550141920619,15.2,-10.1594834138944));
#292752=CARTESIAN_POINT('Ctrl Pts',(-4.13567932427083,15.2,-10.1634981426147));
#292753=CARTESIAN_POINT('Ctrl Pts',(-4.13590170558952,15.2,-10.1685165532416));
#292754=CARTESIAN_POINT('Ctrl Pts',(-4.1361148066386,15.2,-10.1735578111382));
#292755=CARTESIAN_POINT('Ctrl Pts',(-4.13631846552672,15.2,-10.1786217216957));
#292756=CARTESIAN_POINT('Ctrl Pts',(-4.13652212441483,15.2,-10.1836856322531));
#292757=CARTESIAN_POINT('Ctrl Pts',(-4.1367163409139,15.2,-10.1887721985553));
#292758=CARTESIAN_POINT('Ctrl Pts',(-4.13690095077422,15.2,-10.1938812298766));
#292759=CARTESIAN_POINT('Ctrl Pts',(-4.13704863865041,15.2,-10.1979684545994));
#292760=CARTESIAN_POINT('Ctrl Pts',(-4.13719018051875,15.2,-10.2020700570983));
#292761=CARTESIAN_POINT('Ctrl Pts',(-4.13732549300832,15.2,-10.2061859417805));
#292762=CARTESIAN_POINT('Ctrl Pts',(-4.13746080551633,15.2,-10.2103018270235));
#292763=CARTESIAN_POINT('Ctrl Pts',(-4.13758988962521,15.2,-10.2144319943503));
#292764=CARTESIAN_POINT('Ctrl Pts',(-4.13771266352015,15.2,-10.2185763482442));
#292765=CARTESIAN_POINT('Ctrl Pts',(-4.13786613088045,15.2,-10.2237567903293));
#292766=CARTESIAN_POINT('Ctrl Pts',(-4.13800973945726,15.2,-10.2289593978482));
#292767=CARTESIAN_POINT('Ctrl Pts',(-4.13814333348422,15.2,-10.2341839888917));
#292768=CARTESIAN_POINT('Ctrl Pts',(-4.13825020869705,15.2,-10.2383636613848));
#292769=CARTESIAN_POINT('Ctrl Pts',(-4.13835067542947,15.2,-10.242557400772));
#292770=CARTESIAN_POINT('Ctrl Pts',(-4.13844465453335,15.2,-10.2467651147804));
#292771=CARTESIAN_POINT('Ctrl Pts',(-4.13853863365003,15.2,-10.2509728293621));
#292772=CARTESIAN_POINT('Ctrl Pts',(-4.13862612423457,15.2,-10.2551945179324));
#292773=CARTESIAN_POINT('Ctrl Pts',(-4.13870705007164,15.2,-10.2594300859425));
#292774=CARTESIAN_POINT('Ctrl Pts',(-4.13880820736247,15.2,-10.2647245456665));
#292775=CARTESIAN_POINT('Ctrl Pts',(-4.13889910676701,15.2,-10.2700406936908));
#292776=CARTESIAN_POINT('Ctrl Pts',(-4.13897959829394,15.2,-10.2753783484148));
#292777=CARTESIAN_POINT('Ctrl Pts',(-4.13904399151022,15.2,-10.2796484718449));
#292778=CARTESIAN_POINT('Ctrl Pts',(-4.13910172399563,15.2,-10.2839323594289));
#292779=CARTESIAN_POINT('Ctrl Pts',(-4.13915272049171,15.2,-10.2882299187637));
#292780=CARTESIAN_POINT('Ctrl Pts',(-4.13920371699475,15.2,-10.2925274786841));
#292781=CARTESIAN_POINT('Ctrl Pts',(-4.13924797666319,15.2,-10.2968387104866));
#292782=CARTESIAN_POINT('Ctrl Pts',(-4.13928542649787,15.2,-10.3011635217237));
#292783=CARTESIAN_POINT('Ctrl Pts',(-4.13932287632744,15.2,-10.3054883323715));
#292784=CARTESIAN_POINT('Ctrl Pts',(-4.13935351456345,15.2,-10.3098267231787));
#292785=CARTESIAN_POINT('Ctrl Pts',(-4.13937726850641,15.2,-10.3141786013777));
#292786=CARTESIAN_POINT('Ctrl Pts',(-4.1394010224526,15.2,-10.3185304801695));
#292787=CARTESIAN_POINT('Ctrl Pts',(-4.13941789163994,15.2,-10.3228958492991));
#292788=CARTESIAN_POINT('Ctrl Pts',(-4.13942780475148,15.2,-10.3272746148687));
#292789=CARTESIAN_POINT('Ctrl Pts',(-4.13943771786167,15.2,-10.3316533798418));
#292790=CARTESIAN_POINT('Ctrl Pts',(-4.13944067222733,15.2,-10.3360455416287));
#292791=CARTESIAN_POINT('Ctrl Pts',(-4.13943659878368,15.2,-10.3404510121566));
#292792=CARTESIAN_POINT('Ctrl Pts',(-4.13943252533948,15.2,-10.3448564832847));
#292793=CARTESIAN_POINT('Ctrl Pts',(-4.13942142281665,15.2,-10.3492752595867));
#292794=CARTESIAN_POINT('Ctrl Pts',(-4.13940321948186,15.2,-10.3537072548291));
#292795=CARTESIAN_POINT('Ctrl Pts',(-4.13938046531462,15.2,-10.3592472485802));
#292796=CARTESIAN_POINT('Ctrl Pts',(-4.13934661818118,15.2,-10.3648078949844));
#292797=CARTESIAN_POINT('Ctrl Pts',(-4.13930153901148,15.2,-10.3703890183896));
#292798=CARTESIAN_POINT('Ctrl Pts',(-4.13927449151064,15.2,-10.3737376923111));
#292799=CARTESIAN_POINT('Ctrl Pts',(-4.13924340136193,15.2,-10.3770937384049));
#292800=CARTESIAN_POINT('Ctrl Pts',(-4.13920823923785,15.2,-10.380457119075));
#292801=CARTESIAN_POINT('Ctrl Pts',(-4.13917307711377,15.2,-10.3838204997451));
#292802=CARTESIAN_POINT('Ctrl Pts',(-4.13913384188185,15.2,-10.387191214856));
#292803=CARTESIAN_POINT('Ctrl Pts',(-4.13909050584175,15.2,-10.390569227025));
#292804=CARTESIAN_POINT('Ctrl Pts',(-4.13903272444971,15.2,-10.3950732436593));
#292805=CARTESIAN_POINT('Ctrl Pts',(-4.13896765145405,15.2,-10.3995902325396));
#292806=CARTESIAN_POINT('Ctrl Pts',(-4.13889522000491,15.2,-10.4041201077323));
#292807=CARTESIAN_POINT('Ctrl Pts',(-4.13884089642298,15.2,-10.4075175138181));
#292808=CARTESIAN_POINT('Ctrl Pts',(-4.13878243325593,15.2,-10.4109221665795));
#292809=CARTESIAN_POINT('Ctrl Pts',(-4.13871980225459,15.2,-10.4143340304185));
#292810=CARTESIAN_POINT('Ctrl Pts',(-4.13865717125326,15.2,-10.4177458942574));
#292811=CARTESIAN_POINT('Ctrl Pts',(-4.13859037269006,15.2,-10.4211649686807));
#292812=CARTESIAN_POINT('Ctrl Pts',(-4.13851937773394,15.2,-10.4245912168902));
#292813=CARTESIAN_POINT('Ctrl Pts',(-4.13844838277782,15.2,-10.4280174650997));
#292814=CARTESIAN_POINT('Ctrl Pts',(-4.1383731926972,15.2,-10.4314508870583));
#292815=CARTESIAN_POINT('Ctrl Pts',(-4.13829377778342,15.2,-10.434891446725));
#292816=CARTESIAN_POINT('Ctrl Pts',(-4.13821436286964,15.2,-10.4383320063916));
#292817=CARTESIAN_POINT('Ctrl Pts',(-4.13813072518937,15.2,-10.4417797029497));
#292818=CARTESIAN_POINT('Ctrl Pts',(-4.13804283527626,15.2,-10.4452345001152));
#292819=CARTESIAN_POINT('Ctrl Pts',(-4.13792564871481,15.2,-10.4498408967543));
#292820=CARTESIAN_POINT('Ctrl Pts',(-4.13780090476477,15.2,-10.45445991639));
#292821=CARTESIAN_POINT('Ctrl Pts',(-4.1376685374725,15.2,-10.4590914739304));
#292822=CARTESIAN_POINT('Ctrl Pts',(-4.13756926201232,15.2,-10.4625651417702));
#292823=CARTESIAN_POINT('Ctrl Pts',(-4.13746569993471,15.2,-10.4660458606897));
#292824=CARTESIAN_POINT('Ctrl Pts',(-4.13735782152159,15.2,-10.4695335958552));
#292825=CARTESIAN_POINT('Ctrl Pts',(-4.13724994310846,15.2,-10.4730213310208));
#292826=CARTESIAN_POINT('Ctrl Pts',(-4.13713775001252,15.2,-10.4765160813605));
#292827=CARTESIAN_POINT('Ctrl Pts',(-4.13702121547509,15.2,-10.4800178124833));
#292828=CARTESIAN_POINT('Ctrl Pts',(-4.13686583607773,15.2,-10.4846867877378));
#292829=CARTESIAN_POINT('Ctrl Pts',(-4.13670273763503,15.2,-10.4893681707659));
#292830=CARTESIAN_POINT('Ctrl Pts',(-4.13653185768048,15.2,-10.4940618774674));
#292831=CARTESIAN_POINT('Ctrl Pts',(-4.1364036977262,15.2,-10.4975821571738));
#292832=CARTESIAN_POINT('Ctrl Pts',(-4.13627116025926,15.2,-10.5011093691015));
#292833=CARTESIAN_POINT('Ctrl Pts',(-4.13613422021522,15.2,-10.5046434769421));
#292834=CARTESIAN_POINT('Ctrl Pts',(-4.13599728017117,15.2,-10.5081775847828));
#292835=CARTESIAN_POINT('Ctrl Pts',(-4.13585593692921,15.2,-10.5117185873984));
#292836=CARTESIAN_POINT('Ctrl Pts',(-4.13571016351746,15.2,-10.5152664511035));
#292837=CARTESIAN_POINT('Ctrl Pts',(-4.1355643901057,15.2,-10.5188143148085));
#292838=CARTESIAN_POINT('Ctrl Pts',(-4.13541418794447,15.2,-10.522369039846));
#292839=CARTESIAN_POINT('Ctrl Pts',(-4.13525953049176,15.2,-10.52593058905));
#292840=CARTESIAN_POINT('Ctrl Pts',(-4.13505332053607,15.2,-10.5306793217532));
#292841=CARTESIAN_POINT('Ctrl Pts',(-4.13483918934058,15.2,-10.5354401864218));
#292842=CARTESIAN_POINT('Ctrl Pts',(-4.13461707793877,15.2,-10.5402131017387));
#292843=CARTESIAN_POINT('Ctrl Pts',(-4.13445049440254,15.2,-10.5437927879012));
#292844=CARTESIAN_POINT('Ctrl Pts',(-4.13427942122489,15.2,-10.547379251755));
#292845=CARTESIAN_POINT('Ctrl Pts',(-4.13410383327254,15.2,-10.5509724579167));
#292846=CARTESIAN_POINT('Ctrl Pts',(-4.13392824532019,15.2,-10.5545656640784));
#292847=CARTESIAN_POINT('Ctrl Pts',(-4.1337481435274,15.2,-10.5581656123679));
#292848=CARTESIAN_POINT('Ctrl Pts',(-4.13356350203325,15.2,-10.5617722685449));
#292849=CARTESIAN_POINT('Ctrl Pts',(-4.1333788605391,15.2,-10.565378924722));
#292850=CARTESIAN_POINT('Ctrl Pts',(-4.13318967856075,15.2,-10.5689922880951));
#292851=CARTESIAN_POINT('Ctrl Pts',(-4.13299593302526,15.2,-10.5726123237717));
#292852=CARTESIAN_POINT('Ctrl Pts',(-4.13267302378771,15.2,-10.5786457167852));
#292853=CARTESIAN_POINT('Ctrl Pts',(-4.1323374338612,15.2,-10.5846976443278));
#292854=CARTESIAN_POINT('Ctrl Pts',(-4.13198905150009,15.2,-10.5907679442583));
#292855=CARTESIAN_POINT('Ctrl Pts',(-4.13171034559601,15.2,-10.5956241844674));
#292856=CARTESIAN_POINT('Ctrl Pts',(-4.13142345287431,15.2,-10.600492184439));
#292857=CARTESIAN_POINT('Ctrl Pts',(-4.1311283149685,15.2,-10.6053718605395));
#292858=CARTESIAN_POINT('Ctrl Pts',(-4.13090696155924,15.2,-10.6090316172824));
#292859=CARTESIAN_POINT('Ctrl Pts',(-4.13068097132577,15.2,-10.6126979423598));
#292860=CARTESIAN_POINT('Ctrl Pts',(-4.13045031794709,15.2,-10.6163708017023));
#292861=CARTESIAN_POINT('Ctrl Pts',(-4.1302196645684,15.2,-10.6200436610448));
#292862=CARTESIAN_POINT('Ctrl Pts',(-4.12998434943221,15.2,-10.6237230529518));
#292863=CARTESIAN_POINT('Ctrl Pts',(-4.12974434898218,15.2,-10.6274089446518));
#292864=CARTESIAN_POINT('Ctrl Pts',(-4.12950434853216,15.2,-10.6310948363518));
#292865=CARTESIAN_POINT('Ctrl Pts',(-4.12925966242436,15.2,-10.6347872274677));
#292866=CARTESIAN_POINT('Ctrl Pts',(-4.12901026701676,15.2,-10.6384860832916));
#292867=CARTESIAN_POINT('Ctrl Pts',(-4.12859460798898,15.2,-10.6446508432222));
#292868=CARTESIAN_POINT('Ctrl Pts',(-4.12816587086856,15.2,-10.6508335643418));
#292869=CARTESIAN_POINT('Ctrl Pts',(-4.12772394274151,15.2,-10.657034084995));
#292870=CARTESIAN_POINT('Ctrl Pts',(-4.12745878587492,15.2,-10.6607543972518));
#292871=CARTESIAN_POINT('Ctrl Pts',(-4.12718888152492,15.2,-10.664481117482));
#292872=CARTESIAN_POINT('Ctrl Pts',(-4.126914203742,15.2,-10.6682142102382));
#292873=CARTESIAN_POINT('Ctrl Pts',(-4.12663952595909,15.2,-10.6719473029945));
#292874=CARTESIAN_POINT('Ctrl Pts',(-4.12636007713692,15.2,-10.6756867685951));
#292875=CARTESIAN_POINT('Ctrl Pts',(-4.12607583527266,15.2,-10.6794325763751));
#292876=CARTESIAN_POINT('Ctrl Pts',(-4.1257915934084,15.2,-10.6831783841551));
#292877=CARTESIAN_POINT('Ctrl Pts',(-4.12550255925281,15.2,-10.6869305339681));
#292878=CARTESIAN_POINT('Ctrl Pts',(-4.12520871034748,15.2,-10.6906889941223));
#292879=CARTESIAN_POINT('Ctrl Pts',(-4.12491486138876,15.2,-10.6944474549593));
#292880=CARTESIAN_POINT('Ctrl Pts',(-4.12461619822869,15.2,-10.6982122250898));
#292881=CARTESIAN_POINT('Ctrl Pts',(-4.12431269314226,15.2,-10.7019832648054));
#292882=CARTESIAN_POINT('Ctrl Pts',(-4.12400918811096,15.2,-10.7057543038359));
#292883=CARTESIAN_POINT('Ctrl Pts',(-4.12370083934428,15.2,-10.7095316104131));
#292884=CARTESIAN_POINT('Ctrl Pts',(-4.12338762496444,15.2,-10.713315148507));
#292885=CARTESIAN_POINT('Ctrl Pts',(-4.12307441058461,15.2,-10.717098686601));
#292886=CARTESIAN_POINT('Ctrl Pts',(-4.12275632951957,15.2,-10.7208884566915));
#292887=CARTESIAN_POINT('Ctrl Pts',(-4.12243337144829,15.2,-10.7246844424413));
#292888=CARTESIAN_POINT('Ctrl Pts',(-4.12211041337701,15.2,-10.7284804281911));
#292889=CARTESIAN_POINT('Ctrl Pts',(-4.1217825780605,15.2,-10.7322826313081));
#292890=CARTESIAN_POINT('Ctrl Pts',(-4.12144986800006,15.2,-10.736091047));
#292891=CARTESIAN_POINT('Ctrl Pts',(-4.04260911700006,12.2,-9.55499537100001));
#292892=CARTESIAN_POINT('Ctrl Pts',(-4.04316130262144,12.2,-9.55669455581129));
#292893=CARTESIAN_POINT('Ctrl Pts',(-4.04372605423532,12.2,-9.55844976611691));
#292894=CARTESIAN_POINT('Ctrl Pts',(-4.04430244636191,12.2,-9.56026027775997));
#292895=CARTESIAN_POINT('Ctrl Pts',(-4.04488161814269,12.2,-9.56207952060535));
#292896=CARTESIAN_POINT('Ctrl Pts',(-4.04547254558646,12.2,-9.56395460122364));
#292897=CARTESIAN_POINT('Ctrl Pts',(-4.04607433356661,12.2,-9.56588480617844));
#292898=CARTESIAN_POINT('Ctrl Pts',(-4.0466761214921,12.2,-9.56781501095792));
#292899=CARTESIAN_POINT('Ctrl Pts',(-4.047288768506,12.2,-9.5698003417657));
#292900=CARTESIAN_POINT('Ctrl Pts',(-4.04791140648337,12.2,-9.57184010177491));
#292901=CARTESIAN_POINT('Ctrl Pts',(-4.04853404446074,12.2,-9.57387986178411));
#292902=CARTESIAN_POINT('Ctrl Pts',(-4.04916667292143,12.2,-9.57597405360779));
#292903=CARTESIAN_POINT('Ctrl Pts',(-4.04980844817965,12.2,-9.5781219995506));
#292904=CARTESIAN_POINT('Ctrl Pts',(-4.05045022349616,12.2,-9.58026994568851));
#292905=CARTESIAN_POINT('Ctrl Pts',(-4.05110114707708,12.2,-9.58247164586089));
#292906=CARTESIAN_POINT('Ctrl Pts',(-4.05176039953023,12.2,-9.5847264400707));
#292907=CARTESIAN_POINT('Ctrl Pts',(-4.0524196519235,12.2,-9.5869812340757));
#292908=CARTESIAN_POINT('Ctrl Pts',(-4.05308723483013,12.2,-9.58928912240923));
#292909=CARTESIAN_POINT('Ctrl Pts',(-4.05376235422535,12.2,-9.591649459501));
#292910=CARTESIAN_POINT('Ctrl Pts',(-4.05443747362059,12.2,-9.59400979659278));
#292911=CARTESIAN_POINT('Ctrl Pts',(-4.0551201277045,12.2,-9.59642258494927));
#292912=CARTESIAN_POINT('Ctrl Pts',(-4.05580954917917,12.2,-9.59888719110749));
#292913=CARTESIAN_POINT('Ctrl Pts',(-4.05649897071645,12.2,-9.60135179748957));
#292914=CARTESIAN_POINT('Ctrl Pts',(-4.05719515799624,12.2,-9.6038682244197));
#292915=CARTESIAN_POINT('Ctrl Pts',(-4.05789736261825,12.2,-9.60643585656314));
#292916=CARTESIAN_POINT('Ctrl Pts',(-4.05859956717648,12.2,-9.60900348847334));
#292917=CARTESIAN_POINT('Ctrl Pts',(-4.05930779063965,12.2,-9.61162232326542));
#292918=CARTESIAN_POINT('Ctrl Pts',(-4.06002130153062,12.2,-9.61429176142063));
#292919=CARTESIAN_POINT('Ctrl Pts',(-4.0607348124216,12.2,-9.61696119957584));
#292920=CARTESIAN_POINT('Ctrl Pts',(-4.06145361629545,12.2,-9.61968124038532));
#292921=CARTESIAN_POINT('Ctrl Pts',(-4.06217700018564,12.2,-9.62245129461584));
#292922=CARTESIAN_POINT('Ctrl Pts',(-4.06290038407583,12.2,-9.62522134884637));
#292923=CARTESIAN_POINT('Ctrl Pts',(-4.0636283523138,12.2,-9.6280414163698));
#292924=CARTESIAN_POINT('Ctrl Pts',(-4.06436021495361,12.2,-9.63091092167883));
#292925=CARTESIAN_POINT('Ctrl Pts',(-4.0650920776599,12.2,-9.63378042724854));
#292926=CARTESIAN_POINT('Ctrl Pts',(-4.06582783357492,12.2,-9.63669937083967));
#292927=CARTESIAN_POINT('Ctrl Pts',(-4.066566816532,12.2,-9.63966718542021));
#292928=CARTESIAN_POINT('Ctrl Pts',(-4.06730579942196,12.2,-9.64263499973117));
#292929=CARTESIAN_POINT('Ctrl Pts',(-4.06804800741506,12.2,-9.64565168660443));
#292930=CARTESIAN_POINT('Ctrl Pts',(-4.06879278847471,12.2,-9.64871669192354));
#292931=CARTESIAN_POINT('Ctrl Pts',(-4.06953756953436,12.2,-9.65178169724265));
#292932=CARTESIAN_POINT('Ctrl Pts',(-4.07028492545407,12.2,-9.65489502225683));
#292933=CARTESIAN_POINT('Ctrl Pts',(-4.07103421967672,12.2,-9.65805612363872));
#292934=CARTESIAN_POINT('Ctrl Pts',(-4.07178351396743,12.2,-9.66121722530775));
#292935=CARTESIAN_POINT('Ctrl Pts',(-4.07253474806667,12.2,-9.66442610292308));
#292936=CARTESIAN_POINT('Ctrl Pts',(-4.07328730227441,12.2,-9.66768222468592));
#292937=CARTESIAN_POINT('Ctrl Pts',(-4.07403985641379,12.2,-9.67093834615299));
#292938=CARTESIAN_POINT('Ctrl Pts',(-4.07479373164037,12.2,-9.6742417120467));
#292939=CARTESIAN_POINT('Ctrl Pts',(-4.07554832578304,12.2,-9.6775917995234));
#292940=CARTESIAN_POINT('Ctrl Pts',(-4.07630291992571,12.2,-9.68094188700012));
#292941=CARTESIAN_POINT('Ctrl Pts',(-4.07705823202017,12.2,-9.68433869613623));
#292942=CARTESIAN_POINT('Ctrl Pts',(-4.07781367540938,12.2,-9.68778171367465));
#292943=CARTESIAN_POINT('Ctrl Pts',(-4.07856911886721,12.2,-9.69122473152582));
#292944=CARTESIAN_POINT('Ctrl Pts',(-4.07932469262759,12.2,-9.6947139590701));
#292945=CARTESIAN_POINT('Ctrl Pts',(-4.08007982603977,12.2,-9.69824889127533));
#292946=CARTESIAN_POINT('Ctrl Pts',(-4.08083495938336,12.2,-9.70178382315948));
#292947=CARTESIAN_POINT('Ctrl Pts',(-4.08158965065244,12.2,-9.70536446190665));
#292948=CARTESIAN_POINT('Ctrl Pts',(-4.08234334204172,12.2,-9.70899030952491));
#292949=CARTESIAN_POINT('Ctrl Pts',(-4.08309703343101,12.2,-9.71261615714318));
#292950=CARTESIAN_POINT('Ctrl Pts',(-4.08384972330873,12.2,-9.71628721520919));
#292951=CARTESIAN_POINT('Ctrl Pts',(-4.08460086890239,12.2,-9.72000299792392));
#292952=CARTESIAN_POINT('Ctrl Pts',(-4.08535201456428,12.2,-9.72371878097617));
#292953=CARTESIAN_POINT('Ctrl Pts',(-4.08610161511594,12.2,-9.72747928682096));
#292954=CARTESIAN_POINT('Ctrl Pts',(-4.08684913857321,12.2,-9.73128403969801));
#292955=CARTESIAN_POINT('Ctrl Pts',(-4.08759666196258,12.2,-9.73508879222945));
#292956=CARTESIAN_POINT('Ctrl Pts',(-4.08834210621569,12.2,-9.7389377894337));
#292957=CARTESIAN_POINT('Ctrl Pts',(-4.0890849547754,12.2,-9.74283056222672));
#292958=CARTESIAN_POINT('Ctrl Pts',(-4.08982780333511,12.2,-9.74672333501973));
#292959=CARTESIAN_POINT('Ctrl Pts',(-4.09056805536152,12.2,-9.75065988382971));
#292960=CARTESIAN_POINT('Ctrl Pts',(-4.09130520291821,12.2,-9.75463974451655));
#292961=CARTESIAN_POINT('Ctrl Pts',(-4.09191949257109,12.2,-9.75795629520942));
#292962=CARTESIAN_POINT('Ctrl Pts',(-4.09253162614338,12.2,-9.76130292410865));
#292963=CARTESIAN_POINT('Ctrl Pts',(-4.09314131822684,12.2,-9.76467936653764));
#292964=CARTESIAN_POINT('Ctrl Pts',(-4.0937510103103,12.2,-9.76805580896661));
#292965=CARTESIAN_POINT('Ctrl Pts',(-4.09435825691365,12.2,-9.77146206553812));
#292966=CARTESIAN_POINT('Ctrl Pts',(-4.09496278149974,12.2,-9.77489787624809));
#292967=CARTESIAN_POINT('Ctrl Pts',(-4.09556730608582,12.2,-9.77833368695805));
#292968=CARTESIAN_POINT('Ctrl Pts',(-4.0961691044334,12.2,-9.78179904973328));
#292969=CARTESIAN_POINT('Ctrl Pts',(-4.0967679025584,12.2,-9.78529370952493));
#292970=CARTESIAN_POINT('Ctrl Pts',(-4.09736670068339,12.2,-9.78878836931659));
#292971=CARTESIAN_POINT('Ctrl Pts',(-4.09796249679215,12.2,-9.79231232328012));
#292972=CARTESIAN_POINT('Ctrl Pts',(-4.09855502151705,12.2,-9.79586532072688));
#292973=CARTESIAN_POINT('Ctrl Pts',(-4.09914754624196,12.2,-9.79941831817364));
#292974=CARTESIAN_POINT('Ctrl Pts',(-4.09973679736076,12.2,-9.80300035678474));
#292975=CARTESIAN_POINT('Ctrl Pts',(-4.10032251055502,12.2,-9.80661118595292));
#292976=CARTESIAN_POINT('Ctrl Pts',(-4.10090822374928,12.2,-9.81022201512111));
#292977=CARTESIAN_POINT('Ctrl Pts',(-4.10149039908807,12.2,-9.81386163539408));
#292978=CARTESIAN_POINT('Ctrl Pts',(-4.10206877325454,12.2,-9.81752979796501));
#292979=CARTESIAN_POINT('Ctrl Pts',(-4.102647147421,12.2,-9.82119796053593));
#292980=CARTESIAN_POINT('Ctrl Pts',(-4.10322172128251,12.2,-9.82489466466107));
#292981=CARTESIAN_POINT('Ctrl Pts',(-4.10379223957461,12.2,-9.82861966797413));
#292982=CARTESIAN_POINT('Ctrl Pts',(-4.10436275786672,12.2,-9.83234467128718));
#292983=CARTESIAN_POINT('Ctrl Pts',(-4.10492921971839,12.2,-9.8360979704367));
#292984=CARTESIAN_POINT('Ctrl Pts',(-4.10549137235693,12.2,-9.83987932474456));
#292985=CARTESIAN_POINT('Ctrl Pts',(-4.10605352499546,12.2,-9.84366067905241));
#292986=CARTESIAN_POINT('Ctrl Pts',(-4.10661137020614,12.2,-9.84747008842182));
#292987=CARTESIAN_POINT('Ctrl Pts',(-4.10716465937244,12.2,-9.85130731349353));
#292988=CARTESIAN_POINT('Ctrl Pts',(-4.10771794847843,12.2,-9.855144538147));
#292989=CARTESIAN_POINT('Ctrl Pts',(-4.10826668185449,12.2,-9.85900957797845));
#292990=CARTESIAN_POINT('Ctrl Pts',(-4.10881061617059,12.2,-9.86290219602413));
#292991=CARTESIAN_POINT('Ctrl Pts',(-4.10946333745663,12.2,-9.86757333844268));
#292992=CARTESIAN_POINT('Ctrl Pts',(-4.1101091499087,12.2,-9.87228419452342));
#292993=CARTESIAN_POINT('Ctrl Pts',(-4.1107476400265,12.2,-9.87703435803399));
#292994=CARTESIAN_POINT('Ctrl Pts',(-4.11127971509568,12.2,-9.88099282741039));
#292995=CARTESIAN_POINT('Ctrl Pts',(-4.11180670653443,12.2,-9.88497859472781));
#292996=CARTESIAN_POINT('Ctrl Pts',(-4.11232837924249,12.2,-9.88899142827089));
#292997=CARTESIAN_POINT('Ctrl Pts',(-4.11285005195055,12.2,-9.89300426181397));
#292998=CARTESIAN_POINT('Ctrl Pts',(-4.11336640616755,12.2,-9.8970441613282));
#292999=CARTESIAN_POINT('Ctrl Pts',(-4.11387721452601,12.2,-9.90111089917212));
#293000=CARTESIAN_POINT('Ctrl Pts',(-4.11438802288448,12.2,-9.90517763701604));
#293001=CARTESIAN_POINT('Ctrl Pts',(-4.11489328408254,12.2,-9.90927121186446));
#293002=CARTESIAN_POINT('Ctrl Pts',(-4.1153927717904,12.2,-9.91339139783888));
#293003=CARTESIAN_POINT('Ctrl Pts',(-4.11579236192403,12.2,-9.91668754634894));
#293004=CARTESIAN_POINT('Ctrl Pts',(-4.11618825816368,12.2,-9.92000072582621));
#293005=CARTESIAN_POINT('Ctrl Pts',(-4.11658034574298,12.2,-9.92333082171954));
#293006=CARTESIAN_POINT('Ctrl Pts',(-4.11697243337571,12.2,-9.92666091806659));
#293007=CARTESIAN_POINT('Ctrl Pts',(-4.1173607124688,12.2,-9.93000793116309));
#293008=CARTESIAN_POINT('Ctrl Pts',(-4.11774507256416,12.2,-9.93337174573815));
#293009=CARTESIAN_POINT('Ctrl Pts',(-4.11812943260715,12.2,-9.9367355598549));
#293010=CARTESIAN_POINT('Ctrl Pts',(-4.11850987145533,12.2,-9.94011617674009));
#293011=CARTESIAN_POINT('Ctrl Pts',(-4.1188862802026,12.2,-9.94351348323904));
#293012=CARTESIAN_POINT('Ctrl Pts',(-4.11926268900115,12.2,-9.94691079020087));
#293013=CARTESIAN_POINT('Ctrl Pts',(-4.11963506655479,12.2,-9.95032478605084));
#293014=CARTESIAN_POINT('Ctrl Pts',(-4.1200033047968,12.2,-9.95375535907222));
#293015=CARTESIAN_POINT('Ctrl Pts',(-4.12037154298865,12.2,-9.95718593162619));
#293016=CARTESIAN_POINT('Ctrl Pts',(-4.12073564160335,12.2,-9.96063308195066));
#293017=CARTESIAN_POINT('Ctrl Pts',(-4.12109549248117,12.2,-9.96409669800578));
#293018=CARTESIAN_POINT('Ctrl Pts',(-4.12145534340801,12.2,-9.96756031453283));
#293019=CARTESIAN_POINT('Ctrl Pts',(-4.12181094698766,12.2,-9.97104039691098));
#293020=CARTESIAN_POINT('Ctrl Pts',(-4.12216219722875,12.2,-9.97453683476927));
#293021=CARTESIAN_POINT('Ctrl Pts',(-4.12251344742197,12.2,-9.97803327215117));
#293022=CARTESIAN_POINT('Ctrl Pts',(-4.12286034442162,12.2,-9.98154606677697));
#293023=CARTESIAN_POINT('Ctrl Pts',(-4.12320278272741,12.2,-9.98507510543128));
#293024=CARTESIAN_POINT('Ctrl Pts',(-4.12354522107987,12.2,-9.98860414456644));
#293025=CARTESIAN_POINT('Ctrl Pts',(-4.12388320285007,12.2,-9.99214943105037));
#293026=CARTESIAN_POINT('Ctrl Pts',(-4.12421662125863,12.2,-9.99571085476071));
#293027=CARTESIAN_POINT('Ctrl Pts',(-4.12455003962177,12.2,-9.99927227798581));
#293028=CARTESIAN_POINT('Ctrl Pts',(-4.12487889783976,12.2,-10.0028498382828));
#293029=CARTESIAN_POINT('Ctrl Pts',(-4.1252030914804,12.2,-10.0064434281541));
#293030=CARTESIAN_POINT('Ctrl Pts',(-4.12552728516521,12.2,-10.010037018515));
#293031=CARTESIAN_POINT('Ctrl Pts',(-4.12584681608015,12.2,-10.0136466382662));
#293032=CARTESIAN_POINT('Ctrl Pts',(-4.12616158304174,12.2,-10.0172721807416));
#293033=CARTESIAN_POINT('Ctrl Pts',(-4.12647635000334,12.2,-10.020897723217));
#293034=CARTESIAN_POINT('Ctrl Pts',(-4.12678635171161,12.2,-10.0245391883053));
#293035=CARTESIAN_POINT('Ctrl Pts',(-4.1270914912833,12.2,-10.0281964693396));
#293036=CARTESIAN_POINT('Ctrl Pts',(-4.12739663081341,12.2,-10.0318537498756));
#293037=CARTESIAN_POINT('Ctrl Pts',(-4.1276969073921,12.2,-10.0355268451545));
#293038=CARTESIAN_POINT('Ctrl Pts',(-4.12799222175821,12.2,-10.0392156529808));
#293039=CARTESIAN_POINT('Ctrl Pts',(-4.12828753616455,12.2,-10.0429044613096));
#293040=CARTESIAN_POINT('Ctrl Pts',(-4.12857789011502,12.2,-10.0466089782455));
#293041=CARTESIAN_POINT('Ctrl Pts',(-4.12886318579672,12.2,-10.0503291026165));
#293042=CARTESIAN_POINT('Ctrl Pts',(-4.12914848143955,12.2,-10.0540492264807));
#293043=CARTESIAN_POINT('Ctrl Pts',(-4.12942871864969,12.2,-10.0577849556955));
#293044=CARTESIAN_POINT('Ctrl Pts',(-4.12970380296087,12.2,-10.0615361869434));
#293045=CARTESIAN_POINT('Ctrl Pts',(-4.12997888730953,12.2,-10.0652874187024));
#293046=CARTESIAN_POINT('Ctrl Pts',(-4.13024881746126,12.2,-10.0690541518802));
#293047=CARTESIAN_POINT('Ctrl Pts',(-4.13051350048845,12.2,-10.0728362838322));
#293048=CARTESIAN_POINT('Ctrl Pts',(-4.13077818347958,12.2,-10.0766184152688));
#293049=CARTESIAN_POINT('Ctrl Pts',(-4.13103761903301,12.2,-10.0804159443817));
#293050=CARTESIAN_POINT('Ctrl Pts',(-4.13129171401259,12.2,-10.0842287696801));
#293051=CARTESIAN_POINT('Ctrl Pts',(-4.13154580902679,12.2,-10.088041595498));
#293052=CARTESIAN_POINT('Ctrl Pts',(-4.13179456230701,12.2,-10.09186971754));
#293053=CARTESIAN_POINT('Ctrl Pts',(-4.13203788398658,12.2,-10.095713032806));
#293054=CARTESIAN_POINT('Ctrl Pts',(-4.13228120563301,12.2,-10.0995563475483));
#293055=CARTESIAN_POINT('Ctrl Pts',(-4.13251909466213,12.2,-10.1034148568957));
#293056=CARTESIAN_POINT('Ctrl Pts',(-4.132751460433,12.2,-10.107288458438));
#293057=CARTESIAN_POINT('Ctrl Pts',(-4.13298382623553,12.2,-10.1111620605079));
#293058=CARTESIAN_POINT('Ctrl Pts',(-4.13321066942309,12.2,-10.1150507555527));
#293059=CARTESIAN_POINT('Ctrl Pts',(-4.13343189976811,12.2,-10.1189544420442));
#293060=CARTESIAN_POINT('Ctrl Pts',(-4.13365313008299,12.2,-10.1228581280039));
#293061=CARTESIAN_POINT('Ctrl Pts',(-4.13386874747122,12.2,-10.1267768067438));
#293062=CARTESIAN_POINT('Ctrl Pts',(-4.13407866389909,12.2,-10.1307103773652));
#293063=CARTESIAN_POINT('Ctrl Pts',(-4.13428858035556,12.2,-10.1346439485225));
#293064=CARTESIAN_POINT('Ctrl Pts',(-4.13449279536074,12.2,-10.138592411852));
#293065=CARTESIAN_POINT('Ctrl Pts',(-4.13469122248355,12.2,-10.1425556677527));
#293066=CARTESIAN_POINT('Ctrl Pts',(-4.13488964957932,12.2,-10.1465189231134));
#293067=CARTESIAN_POINT('Ctrl Pts',(-4.13508228934532,12.2,-10.1504969711445));
#293068=CARTESIAN_POINT('Ctrl Pts',(-4.13526905321954,12.2,-10.1544897138722));
#293069=CARTESIAN_POINT('Ctrl Pts',(-4.13545581711921,12.2,-10.1584824571438));
#293070=CARTESIAN_POINT('Ctrl Pts',(-4.13563670813499,12.2,-10.1624898947252));
#293071=CARTESIAN_POINT('Ctrl Pts',(-4.13581163803341,12.2,-10.1665119285));
#293072=CARTESIAN_POINT('Ctrl Pts',(-4.13598656793184,12.2,-10.1705339622747));
#293073=CARTESIAN_POINT('Ctrl Pts',(-4.13615553840734,12.2,-10.1745705930289));
#293074=CARTESIAN_POINT('Ctrl Pts',(-4.13631846552672,12.2,-10.1786217216956));
#293075=CARTESIAN_POINT('Ctrl Pts',(-4.13648139262389,12.2,-10.1826728498104));
#293076=CARTESIAN_POINT('Ctrl Pts',(-4.13663827700795,12.2,-10.1867384775316));
#293077=CARTESIAN_POINT('Ctrl Pts',(-4.13678903349603,12.2,-10.1908185074749));
#293078=CARTESIAN_POINT('Ctrl Pts',(-4.13693979000465,12.2,-10.1948985379741));
#293079=CARTESIAN_POINT('Ctrl Pts',(-4.13708442016454,12.2,-10.1989929699658));
#293080=CARTESIAN_POINT('Ctrl Pts',(-4.1372228420118,12.2,-10.2031017080629));
#293081=CARTESIAN_POINT('Ctrl Pts',(-4.13736126384019,12.2,-10.2072104456002));
#293082=CARTESIAN_POINT('Ctrl Pts',(-4.13749347742461,12.2,-10.211333489351));
#293083=CARTESIAN_POINT('Ctrl Pts',(-4.13761940124806,12.2,-10.2154707433452));
#293084=CARTESIAN_POINT('Ctrl Pts',(-4.13774532508867,12.2,-10.2196079979031));
#293085=CARTESIAN_POINT('Ctrl Pts',(-4.13786495947852,12.2,-10.2237594635849));
#293086=CARTESIAN_POINT('Ctrl Pts',(-4.13797822398428,12.2,-10.2279250435906));
#293087=CARTESIAN_POINT('Ctrl Pts',(-4.1380914884746,12.2,-10.2320906230288));
#293088=CARTESIAN_POINT('Ctrl Pts',(-4.13819838365199,12.2,-10.2362703193538));
#293089=CARTESIAN_POINT('Ctrl Pts',(-4.13829883026047,12.2,-10.2404640351082));
#293090=CARTESIAN_POINT('Ctrl Pts',(-4.13842438853133,12.2,-10.2457061802296));
#293091=CARTESIAN_POINT('Ctrl Pts',(-4.13853987097038,12.2,-10.2509702350055));
#293092=CARTESIAN_POINT('Ctrl Pts',(-4.13864512569314,12.2,-10.2562560129211));
#293093=CARTESIAN_POINT('Ctrl Pts',(-4.13872932947593,12.2,-10.260484635484));
#293094=CARTESIAN_POINT('Ctrl Pts',(-4.13880698679683,12.2,-10.2647271607485));
#293095=CARTESIAN_POINT('Ctrl Pts',(-4.13887802202249,12.2,-10.2689834973147));
#293096=CARTESIAN_POINT('Ctrl Pts',(-4.13894905723848,12.2,-10.273239833301));
#293097=CARTESIAN_POINT('Ctrl Pts',(-4.13901346916792,12.2,-10.2775099806213));
#293098=CARTESIAN_POINT('Ctrl Pts',(-4.139071183,12.2,-10.2817938449284));
#293099=CARTESIAN_POINT('Ctrl Pts',(-4.13912889683995,12.2,-10.2860777098192));
#293100=CARTESIAN_POINT('Ctrl Pts',(-4.13917991194888,12.2,-10.2903752927694));
#293101=CARTESIAN_POINT('Ctrl Pts',(-4.13922415322864,12.2,-10.2946865013942));
#293102=CARTESIAN_POINT('Ctrl Pts',(-4.13926839450235,12.2,-10.2989977094316));
#293103=CARTESIAN_POINT('Ctrl Pts',(-4.13930586327743,12.2,-10.3033225423439));
#293104=CARTESIAN_POINT('Ctrl Pts',(-4.13933648322007,12.2,-10.3076609102656));
#293105=CARTESIAN_POINT('Ctrl Pts',(-4.13936710316689,12.2,-10.3119992787785));
#293106=CARTESIAN_POINT('Ctrl Pts',(-4.13939087574634,12.2,-10.316351180159));
#293107=CARTESIAN_POINT('Ctrl Pts',(-4.13940772702509,12.2,-10.3207165260279));
#293108=CARTESIAN_POINT('Ctrl Pts',(-4.13942457830155,12.2,-10.325081871302));
#293109=CARTESIAN_POINT('Ctrl Pts',(-4.13943450976857,12.2,-10.3294606591173));
#293110=CARTESIAN_POINT('Ctrl Pts',(-4.13943744649127,12.2,-10.3338527985902));
#293111=CARTESIAN_POINT('Ctrl Pts',(-4.13944038321436,12.2,-10.3382449386615));
#293112=CARTESIAN_POINT('Ctrl Pts',(-4.13943632790903,12.2,-10.3426504325647));
#293113=CARTESIAN_POINT('Ctrl Pts',(-4.13942520774175,12.2,-10.34706918725));
#293114=CARTESIAN_POINT('Ctrl Pts',(-4.13941408757448,12.2,-10.3514879419352));
#293115=CARTESIAN_POINT('Ctrl Pts',(-4.13939590172861,12.2,-10.3559199596415));
#293116=CARTESIAN_POINT('Ctrl Pts',(-4.13937058100427,12.2,-10.3603651497184));
#293117=CARTESIAN_POINT('Ctrl Pts',(-4.13935159046275,12.2,-10.3636990419733));
#293118=CARTESIAN_POINT('Ctrl Pts',(-4.13932858651232,12.2,-10.3670403444681));
#293119=CARTESIAN_POINT('Ctrl Pts',(-4.13930153901148,12.2,-10.3703890183896));
#293120=CARTESIAN_POINT('Ctrl Pts',(-4.13926547567867,12.2,-10.3748539167488));
#293121=CARTESIAN_POINT('Ctrl Pts',(-4.13922222618843,12.2,-10.3793319213204));
#293122=CARTESIAN_POINT('Ctrl Pts',(-4.13917171830415,12.2,-10.3838229426746));
#293123=CARTESIAN_POINT('Ctrl Pts',(-4.13912121041298,12.2,-10.3883139646407));
#293124=CARTESIAN_POINT('Ctrl Pts',(-4.13906344625983,12.2,-10.3928180030279));
#293125=CARTESIAN_POINT('Ctrl Pts',(-4.13899835681136,12.2,-10.397334970386));
#293126=CARTESIAN_POINT('Ctrl Pts',(-4.13894953972944,12.2,-10.4007226955969));
#293127=CARTESIAN_POINT('Ctrl Pts',(-4.13889660199824,12.2,-10.4041176943112));
#293128=CARTESIAN_POINT('Ctrl Pts',(-4.13883951550003,12.2,-10.4075199275364));
#293129=CARTESIAN_POINT('Ctrl Pts',(-4.1387443713329,12.2,-10.4131903164511));
#293130=CARTESIAN_POINT('Ctrl Pts',(-4.13863770266511,12.2,-10.4188808030003));
#293131=CARTESIAN_POINT('Ctrl Pts',(-4.13851937773394,12.2,-10.4245912168902));
#293132=CARTESIAN_POINT('Ctrl Pts',(-4.13844838277782,12.2,-10.4280174650997));
#293133=CARTESIAN_POINT('Ctrl Pts',(-4.1383731926972,12.2,-10.4314508870583));
#293134=CARTESIAN_POINT('Ctrl Pts',(-4.13829377778342,12.2,-10.434891446725));
#293135=CARTESIAN_POINT('Ctrl Pts',(-4.13821436286964,12.2,-10.4383320063916));
#293136=CARTESIAN_POINT('Ctrl Pts',(-4.13813072518937,12.2,-10.4417797029497));
#293137=CARTESIAN_POINT('Ctrl Pts',(-4.13804283527626,12.2,-10.4452345001152));
#293138=CARTESIAN_POINT('Ctrl Pts',(-4.13795494536316,12.2,-10.4486892972807));
#293139=CARTESIAN_POINT('Ctrl Pts',(-4.13786280473618,12.2,-10.4521511944824));
#293140=CARTESIAN_POINT('Ctrl Pts',(-4.13776638477703,12.2,-10.4556201568205));
#293141=CARTESIAN_POINT('Ctrl Pts',(-4.13766996481788,12.2,-10.4590891191587));
#293142=CARTESIAN_POINT('Ctrl Pts',(-4.13756926635191,12.2,-10.4625651457515));
#293143=CARTESIAN_POINT('Ctrl Pts',(-4.13746426227297,12.2,-10.466048199499));
#293144=CARTESIAN_POINT('Ctrl Pts',(-4.13735925817497,12.2,-10.4695312538792));
#293145=CARTESIAN_POINT('Ctrl Pts',(-4.13724994680908,12.2,-10.4730213363198));
#293146=CARTESIAN_POINT('Ctrl Pts',(-4.13713630375031,12.2,-10.4765184102457));
#293147=CARTESIAN_POINT('Ctrl Pts',(-4.13702266071218,12.2,-10.4800154835362));
#293148=CARTESIAN_POINT('Ctrl Pts',(-4.13690468441595,12.2,-10.4835195496431));
#293149=CARTESIAN_POINT('Ctrl Pts',(-4.13678234892001,12.2,-10.4870305708495));
#293150=CARTESIAN_POINT('Ctrl Pts',(-4.13666001342408,12.2,-10.4905415920558));
#293151=CARTESIAN_POINT('Ctrl Pts',(-4.13653331877915,12.2,-10.4940595688652));
#293152=CARTESIAN_POINT('Ctrl Pts',(-4.1364022377833,12.2,-10.4975844660448));
#293153=CARTESIAN_POINT('Ctrl Pts',(-4.13627115678745,12.2,-10.5011093632245));
#293154=CARTESIAN_POINT('Ctrl Pts',(-4.13613569001241,12.2,-10.504641180526));
#293155=CARTESIAN_POINT('Ctrl Pts',(-4.13599581151688,12.2,-10.5081798812467));
#293156=CARTESIAN_POINT('Ctrl Pts',(-4.13585593302135,12.2,-10.5117185819676));
#293157=CARTESIAN_POINT('Ctrl Pts',(-4.1357116416771,12.2,-10.5152641661925));
#293158=CARTESIAN_POINT('Ctrl Pts',(-4.13556291272456,12.2,-10.5188165998962));
#293159=CARTESIAN_POINT('Ctrl Pts',(-4.13541418377201,12.2,-10.5223690335999));
#293160=CARTESIAN_POINT('Ctrl Pts',(-4.13526101752811,12.2,-10.5259283161531));
#293161=CARTESIAN_POINT('Ctrl Pts',(-4.13510338703445,12.2,-10.5294944109392));
#293162=CARTESIAN_POINT('Ctrl Pts',(-4.13494575651215,12.2,-10.5330605063732));
#293163=CARTESIAN_POINT('Ctrl Pts',(-4.13478366150526,12.2,-10.5366334149258));
#293164=CARTESIAN_POINT('Ctrl Pts',(-4.13461707793877,12.2,-10.5402131017387));
#293165=CARTESIAN_POINT('Ctrl Pts',(-4.13445049440254,12.2,-10.5437927879012));
#293166=CARTESIAN_POINT('Ctrl Pts',(-4.13427942122489,12.2,-10.547379251755));
#293167=CARTESIAN_POINT('Ctrl Pts',(-4.13410383327254,12.2,-10.5509724579167));
#293168=CARTESIAN_POINT('Ctrl Pts',(-4.13392824532019,12.2,-10.5545656640784));
#293169=CARTESIAN_POINT('Ctrl Pts',(-4.1337481435274,12.2,-10.5581656123679));
#293170=CARTESIAN_POINT('Ctrl Pts',(-4.13356350203325,12.2,-10.5617722685449));
#293171=CARTESIAN_POINT('Ctrl Pts',(-4.1333788605391,12.2,-10.565378924722));
#293172=CARTESIAN_POINT('Ctrl Pts',(-4.13318967856075,12.2,-10.5689922880951));
#293173=CARTESIAN_POINT('Ctrl Pts',(-4.13299593302526,12.2,-10.5726123237717));
#293174=CARTESIAN_POINT('Ctrl Pts',(-4.13280218748977,12.2,-10.5762323594483));
#293175=CARTESIAN_POINT('Ctrl Pts',(-4.13260387653102,12.2,-10.57985906597));
#293176=CARTESIAN_POINT('Ctrl Pts',(-4.13240097703879,12.2,-10.5834924120874));
#293177=CARTESIAN_POINT('Ctrl Pts',(-4.13219807754657,12.2,-10.5871257582048));
#293178=CARTESIAN_POINT('Ctrl Pts',(-4.13199058827132,12.2,-10.5907657411884));
#293179=CARTESIAN_POINT('Ctrl Pts',(-4.13177848627966,12.2,-10.59441232693));
#293180=CARTESIAN_POINT('Ctrl Pts',(-4.13156638424946,12.2,-10.5980589133341));
#293181=CARTESIAN_POINT('Ctrl Pts',(-4.13134966841797,12.2,-10.6017121031317));
#293182=CARTESIAN_POINT('Ctrl Pts',(-4.1311283149685,12.2,-10.6053718605395));
#293183=CARTESIAN_POINT('Ctrl Pts',(-4.13090696155924,12.2,-10.6090316172824));
#293184=CARTESIAN_POINT('Ctrl Pts',(-4.13068097132577,12.2,-10.6126979423598));
#293185=CARTESIAN_POINT('Ctrl Pts',(-4.13045031794708,12.2,-10.6163708017023));
#293186=CARTESIAN_POINT('Ctrl Pts',(-4.1302196645684,12.2,-10.6200436610448));
#293187=CARTESIAN_POINT('Ctrl Pts',(-4.12998434943221,12.2,-10.6237230529518));
#293188=CARTESIAN_POINT('Ctrl Pts',(-4.12974434898218,12.2,-10.6274089446518));
#293189=CARTESIAN_POINT('Ctrl Pts',(-4.12950434853216,12.2,-10.6310948363518));
#293190=CARTESIAN_POINT('Ctrl Pts',(-4.12925966242436,12.2,-10.6347872274677));
#293191=CARTESIAN_POINT('Ctrl Pts',(-4.12901026701676,12.2,-10.6384860832916));
#293192=CARTESIAN_POINT('Ctrl Pts',(-4.12876087160915,12.2,-10.6421849391156));
#293193=CARTESIAN_POINT('Ctrl Pts',(-4.12850676758507,12.2,-10.6458902610143));
#293194=CARTESIAN_POINT('Ctrl Pts',(-4.12824793205322,12.2,-10.6496020137955));
#293195=CARTESIAN_POINT('Ctrl Pts',(-4.12781653948446,12.2,-10.6557882686557));
#293196=CARTESIAN_POINT('Ctrl Pts',(-4.12737200006349,12.2,-10.6619923887517));
#293197=CARTESIAN_POINT('Ctrl Pts',(-4.126914203742,12.2,-10.6682142102382));
#293198=CARTESIAN_POINT('Ctrl Pts',(-4.12663952595909,12.2,-10.6719473029945));
#293199=CARTESIAN_POINT('Ctrl Pts',(-4.12636007713692,12.2,-10.6756867685951));
#293200=CARTESIAN_POINT('Ctrl Pts',(-4.12607583527266,12.2,-10.6794325763751));
#293201=CARTESIAN_POINT('Ctrl Pts',(-4.12569684608589,12.2,-10.6844269872021));
#293202=CARTESIAN_POINT('Ctrl Pts',(-4.12530933743978,12.2,-10.6894326742333));
#293203=CARTESIAN_POINT('Ctrl Pts',(-4.12491325541763,12.2,-10.6944495574519));
#293204=CARTESIAN_POINT('Ctrl Pts',(-4.124616193928,12.2,-10.6982122195241));
#293205=CARTESIAN_POINT('Ctrl Pts',(-4.12431430950675,12.2,-10.7019811776567));
#293206=CARTESIAN_POINT('Ctrl Pts',(-4.12400757305814,12.2,-10.7057563912867));
#293207=CARTESIAN_POINT('Ctrl Pts',(-4.12370083660954,12.2,-10.7095316049168));
#293208=CARTESIAN_POINT('Ctrl Pts',(-4.12338924799029,12.2,-10.7133130717003));
#293209=CARTESIAN_POINT('Ctrl Pts',(-4.12307278825038,12.2,-10.7171007627465));
#293210=CARTESIAN_POINT('Ctrl Pts',(-4.12254535533135,12.2,-10.7234135813863));
#293211=CARTESIAN_POINT('Ctrl Pts',(-4.12200438478762,12.2,-10.7297436872829));
#293212=CARTESIAN_POINT('Ctrl Pts',(-4.12144986800006,12.2,-10.736091047));
#293213=CARTESIAN_POINT('Origin',(-5.66257110645729E-14,15.2,-1.77635683940025E-14));
#293214=CARTESIAN_POINT('',(-2.64164356403319,15.2,-10.0330625574592));
#293215=CARTESIAN_POINT('',(-2.64164356403319,12.2,-10.0330625574592));
#293216=CARTESIAN_POINT('',(-2.64164356400005,15.2,-10.033062557));
#293217=CARTESIAN_POINT('Origin',(-5.66257110645729E-14,12.2,-1.77635683940025E-14));
#293218=CARTESIAN_POINT('Origin',(-5.66257110645729E-14,15.2,-1.77635683940025E-14));
#293219=CARTESIAN_POINT('Origin',(-5.66257110645729E-14,15.2,-1.77635683940025E-14));
#293220=CARTESIAN_POINT('',(-2.55159439100006,15.2,-11.213356592));
#293221=CARTESIAN_POINT('',(-2.17615954800006,15.2,-11.292224299));
#293222=CARTESIAN_POINT('Origin',(-5.66257110645729E-14,15.2,-1.77635683940025E-14));
#293223=CARTESIAN_POINT('',(-2.17615954800006,12.2,-11.292224299));
#293224=CARTESIAN_POINT('',(-2.17615954800006,15.2,-11.292224299));
#293225=CARTESIAN_POINT('',(-2.55159439100006,12.2,-11.213356592));
#293226=CARTESIAN_POINT('Origin',(-5.66257110645729E-14,12.2,-1.77635683940025E-14));
#293227=CARTESIAN_POINT('',(-2.55159439100006,15.2,-11.213356592));
#293228=CARTESIAN_POINT('Ctrl Pts',(-2.64164356400005,15.2,-10.033062558));
#293229=CARTESIAN_POINT('Ctrl Pts',(-2.64164356400005,11.6,-10.033062558));
#293230=CARTESIAN_POINT('Ctrl Pts',(-2.64167330500006,15.2,-10.03323436));
#293231=CARTESIAN_POINT('Ctrl Pts',(-2.64167330500006,11.6,-10.03323436));
#293232=CARTESIAN_POINT('Ctrl Pts',(-2.64173373800006,15.2,-10.033583981));
#293233=CARTESIAN_POINT('Ctrl Pts',(-2.64173373800006,11.6,-10.033583981));
#293234=CARTESIAN_POINT('Ctrl Pts',(-2.64182504800006,15.2,-10.034113785));
#293235=CARTESIAN_POINT('Ctrl Pts',(-2.64182504800006,11.6,-10.034113785));
#293236=CARTESIAN_POINT('Ctrl Pts',(-2.64194752000006,15.2,-10.034827572));
#293237=CARTESIAN_POINT('Ctrl Pts',(-2.64194752000006,11.6,-10.034827572));
#293238=CARTESIAN_POINT('Ctrl Pts',(-2.64210152600006,15.2,-10.03573056));
#293239=CARTESIAN_POINT('Ctrl Pts',(-2.64210152600006,11.6,-10.03573056));
#293240=CARTESIAN_POINT('Ctrl Pts',(-2.64225710800006,15.2,-10.03664834));
#293241=CARTESIAN_POINT('Ctrl Pts',(-2.64225710800006,11.6,-10.03664834));
#293242=CARTESIAN_POINT('Ctrl Pts',(-2.64241335000006,15.2,-10.037575657));
#293243=CARTESIAN_POINT('Ctrl Pts',(-2.64241335000006,11.6,-10.037575657));
#293244=CARTESIAN_POINT('Ctrl Pts',(-2.64257023000006,15.2,-10.038512489));
#293245=CARTESIAN_POINT('Ctrl Pts',(-2.64257023000006,11.6,-10.038512489));
#293246=CARTESIAN_POINT('Ctrl Pts',(-2.64272772500005,15.2,-10.039458811));
#293247=CARTESIAN_POINT('Ctrl Pts',(-2.64272772500005,11.6,-10.039458811));
#293248=CARTESIAN_POINT('Ctrl Pts',(-2.64288581300006,15.2,-10.040414601));
#293249=CARTESIAN_POINT('Ctrl Pts',(-2.64288581300006,11.6,-10.040414601));
#293250=CARTESIAN_POINT('Ctrl Pts',(-2.64304447300006,15.2,-10.041379835));
#293251=CARTESIAN_POINT('Ctrl Pts',(-2.64304447300006,11.6,-10.041379835));
#293252=CARTESIAN_POINT('Ctrl Pts',(-2.64320368100006,15.2,-10.042354489));
#293253=CARTESIAN_POINT('Ctrl Pts',(-2.64320368100006,11.6,-10.042354489));
#293254=CARTESIAN_POINT('Ctrl Pts',(-2.64336341800006,15.2,-10.043338542));
#293255=CARTESIAN_POINT('Ctrl Pts',(-2.64336341800006,11.6,-10.043338542));
#293256=CARTESIAN_POINT('Ctrl Pts',(-2.64352366100006,15.2,-10.044331968));
#293257=CARTESIAN_POINT('Ctrl Pts',(-2.64352366100006,11.6,-10.044331968));
#293258=CARTESIAN_POINT('Ctrl Pts',(-2.64368438700005,15.2,-10.045334746));
#293259=CARTESIAN_POINT('Ctrl Pts',(-2.64368438700005,11.6,-10.045334746));
#293260=CARTESIAN_POINT('Ctrl Pts',(-2.64384557700006,15.2,-10.046346854));
#293261=CARTESIAN_POINT('Ctrl Pts',(-2.64384557700006,11.6,-10.046346854));
#293262=CARTESIAN_POINT('Ctrl Pts',(-2.64400720800006,15.2,-10.047368268));
#293263=CARTESIAN_POINT('Ctrl Pts',(-2.64400720800006,11.6,-10.047368268));
#293264=CARTESIAN_POINT('Ctrl Pts',(-2.64416926000006,15.2,-10.048398967));
#293265=CARTESIAN_POINT('Ctrl Pts',(-2.64416926000006,11.6,-10.048398967));
#293266=CARTESIAN_POINT('Ctrl Pts',(-2.64433171100006,15.2,-10.049438925));
#293267=CARTESIAN_POINT('Ctrl Pts',(-2.64433171100006,11.6,-10.049438925));
#293268=CARTESIAN_POINT('Ctrl Pts',(-2.64449454000005,15.2,-10.050488124));
#293269=CARTESIAN_POINT('Ctrl Pts',(-2.64449454000005,11.6,-10.050488124));
#293270=CARTESIAN_POINT('Ctrl Pts',(-2.64465772700006,15.2,-10.051546539));
#293271=CARTESIAN_POINT('Ctrl Pts',(-2.64465772700006,11.6,-10.051546539));
#293272=CARTESIAN_POINT('Ctrl Pts',(-2.64482124900006,15.2,-10.052614149));
#293273=CARTESIAN_POINT('Ctrl Pts',(-2.64482124900006,11.6,-10.052614149));
#293274=CARTESIAN_POINT('Ctrl Pts',(-2.64498508800005,15.2,-10.05369093));
#293275=CARTESIAN_POINT('Ctrl Pts',(-2.64498508800005,11.6,-10.05369093));
#293276=CARTESIAN_POINT('Ctrl Pts',(-2.64514922300005,15.2,-10.054776863));
#293277=CARTESIAN_POINT('Ctrl Pts',(-2.64514922300005,11.6,-10.054776863));
#293278=CARTESIAN_POINT('Ctrl Pts',(-2.64531363200006,15.2,-10.055871923));
#293279=CARTESIAN_POINT('Ctrl Pts',(-2.64531363200006,11.6,-10.055871923));
#293280=CARTESIAN_POINT('Ctrl Pts',(-2.64547829600006,15.2,-10.056976091));
#293281=CARTESIAN_POINT('Ctrl Pts',(-2.64547829600006,11.6,-10.056976091));
#293282=CARTESIAN_POINT('Ctrl Pts',(-2.64564319300006,15.2,-10.058089344));
#293283=CARTESIAN_POINT('Ctrl Pts',(-2.64564319300006,11.6,-10.058089344));
#293284=CARTESIAN_POINT('Ctrl Pts',(-2.64580830600006,15.2,-10.059211661));
#293285=CARTESIAN_POINT('Ctrl Pts',(-2.64580830600006,11.6,-10.059211661));
#293286=CARTESIAN_POINT('Ctrl Pts',(-2.64597361300006,15.2,-10.060343019));
#293287=CARTESIAN_POINT('Ctrl Pts',(-2.64597361300006,11.6,-10.060343019));
#293288=CARTESIAN_POINT('Ctrl Pts',(-2.64613909300006,15.2,-10.061483397));
#293289=CARTESIAN_POINT('Ctrl Pts',(-2.64613909300006,11.6,-10.061483397));
#293290=CARTESIAN_POINT('Ctrl Pts',(-2.64630472900006,15.2,-10.062632776));
#293291=CARTESIAN_POINT('Ctrl Pts',(-2.64630472900006,11.6,-10.062632776));
#293292=CARTESIAN_POINT('Ctrl Pts',(-2.64647049900006,15.2,-10.063791132));
#293293=CARTESIAN_POINT('Ctrl Pts',(-2.64647049900006,11.6,-10.063791132));
#293294=CARTESIAN_POINT('Ctrl Pts',(-2.64663638300005,15.2,-10.064958444));
#293295=CARTESIAN_POINT('Ctrl Pts',(-2.64663638300005,11.6,-10.064958444));
#293296=CARTESIAN_POINT('Ctrl Pts',(-2.64680236500006,15.2,-10.066134693));
#293297=CARTESIAN_POINT('Ctrl Pts',(-2.64680236500006,11.6,-10.066134693));
#293298=CARTESIAN_POINT('Ctrl Pts',(-2.64696842100005,15.2,-10.067319856));
#293299=CARTESIAN_POINT('Ctrl Pts',(-2.64696842100005,11.6,-10.067319856));
#293300=CARTESIAN_POINT('Ctrl Pts',(-2.64713453500006,15.2,-10.068513912));
#293301=CARTESIAN_POINT('Ctrl Pts',(-2.64713453500006,11.6,-10.068513912));
#293302=CARTESIAN_POINT('Ctrl Pts',(-2.64730068700006,15.2,-10.069716842));
#293303=CARTESIAN_POINT('Ctrl Pts',(-2.64730068700006,11.6,-10.069716842));
#293304=CARTESIAN_POINT('Ctrl Pts',(-2.64746685600006,15.2,-10.070928624));
#293305=CARTESIAN_POINT('Ctrl Pts',(-2.64746685600006,11.6,-10.070928624));
#293306=CARTESIAN_POINT('Ctrl Pts',(-2.64763302600006,15.2,-10.072149237));
#293307=CARTESIAN_POINT('Ctrl Pts',(-2.64763302600006,11.6,-10.072149237));
#293308=CARTESIAN_POINT('Ctrl Pts',(-2.64779917600006,15.2,-10.073378662));
#293309=CARTESIAN_POINT('Ctrl Pts',(-2.64779917600006,11.6,-10.073378662));
#293310=CARTESIAN_POINT('Ctrl Pts',(-2.64796528800006,15.2,-10.074616877));
#293311=CARTESIAN_POINT('Ctrl Pts',(-2.64796528800006,11.6,-10.074616877));
#293312=CARTESIAN_POINT('Ctrl Pts',(-2.64813134300006,15.2,-10.075863863));
#293313=CARTESIAN_POINT('Ctrl Pts',(-2.64813134300006,11.6,-10.075863863));
#293314=CARTESIAN_POINT('Ctrl Pts',(-2.64829732200006,15.2,-10.077119598));
#293315=CARTESIAN_POINT('Ctrl Pts',(-2.64829732200006,11.6,-10.077119598));
#293316=CARTESIAN_POINT('Ctrl Pts',(-2.64846320600005,15.2,-10.078384063));
#293317=CARTESIAN_POINT('Ctrl Pts',(-2.64846320600005,11.6,-10.078384063));
#293318=CARTESIAN_POINT('Ctrl Pts',(-2.64862897800006,15.2,-10.079657237));
#293319=CARTESIAN_POINT('Ctrl Pts',(-2.64862897800006,11.6,-10.079657237));
#293320=CARTESIAN_POINT('Ctrl Pts',(-2.64879462000006,15.2,-10.0809391));
#293321=CARTESIAN_POINT('Ctrl Pts',(-2.64879462000006,11.6,-10.0809391));
#293322=CARTESIAN_POINT('Ctrl Pts',(-2.64896011100006,15.2,-10.082229633));
#293323=CARTESIAN_POINT('Ctrl Pts',(-2.64896011100006,11.6,-10.082229633));
#293324=CARTESIAN_POINT('Ctrl Pts',(-2.64912543500006,15.2,-10.083528816));
#293325=CARTESIAN_POINT('Ctrl Pts',(-2.64912543500006,11.6,-10.083528816));
#293326=CARTESIAN_POINT('Ctrl Pts',(-2.64929057300006,15.2,-10.084836628));
#293327=CARTESIAN_POINT('Ctrl Pts',(-2.64929057300006,11.6,-10.084836628));
#293328=CARTESIAN_POINT('Ctrl Pts',(-2.64945550900006,15.2,-10.086153049));
#293329=CARTESIAN_POINT('Ctrl Pts',(-2.64945550900006,11.6,-10.086153049));
#293330=CARTESIAN_POINT('Ctrl Pts',(-2.64962022200006,15.2,-10.087478061));
#293331=CARTESIAN_POINT('Ctrl Pts',(-2.64962022200006,11.6,-10.087478061));
#293332=CARTESIAN_POINT('Ctrl Pts',(-2.64978469600006,15.2,-10.088811644));
#293333=CARTESIAN_POINT('Ctrl Pts',(-2.64978469600006,11.6,-10.088811644));
#293334=CARTESIAN_POINT('Ctrl Pts',(-2.64994891300006,15.2,-10.090153778));
#293335=CARTESIAN_POINT('Ctrl Pts',(-2.64994891300006,11.6,-10.090153778));
#293336=CARTESIAN_POINT('Ctrl Pts',(-2.65011285400006,15.2,-10.091504443));
#293337=CARTESIAN_POINT('Ctrl Pts',(-2.65011285400006,11.6,-10.091504443));
#293338=CARTESIAN_POINT('Ctrl Pts',(-2.65027650300006,15.2,-10.09286362));
#293339=CARTESIAN_POINT('Ctrl Pts',(-2.65027650300006,11.6,-10.09286362));
#293340=CARTESIAN_POINT('Ctrl Pts',(-2.65043984300006,15.2,-10.09423129));
#293341=CARTESIAN_POINT('Ctrl Pts',(-2.65043984300006,11.6,-10.09423129));
#293342=CARTESIAN_POINT('Ctrl Pts',(-2.65060285500006,15.2,-10.095607434));
#293343=CARTESIAN_POINT('Ctrl Pts',(-2.65060285500006,11.6,-10.095607434));
#293344=CARTESIAN_POINT('Ctrl Pts',(-2.65076552300005,15.2,-10.096992032));
#293345=CARTESIAN_POINT('Ctrl Pts',(-2.65076552300005,11.6,-10.096992032));
#293346=CARTESIAN_POINT('Ctrl Pts',(-2.65092782900005,15.2,-10.098385065));
#293347=CARTESIAN_POINT('Ctrl Pts',(-2.65092782900005,11.6,-10.098385065));
#293348=CARTESIAN_POINT('Ctrl Pts',(-2.65108975500006,15.2,-10.099786515));
#293349=CARTESIAN_POINT('Ctrl Pts',(-2.65108975500006,11.6,-10.099786515));
#293350=CARTESIAN_POINT('Ctrl Pts',(-2.65125128600005,15.2,-10.101196362));
#293351=CARTESIAN_POINT('Ctrl Pts',(-2.65125128600005,11.6,-10.101196362));
#293352=CARTESIAN_POINT('Ctrl Pts',(-2.65141240300005,15.2,-10.102614588));
#293353=CARTESIAN_POINT('Ctrl Pts',(-2.65141240300005,11.6,-10.102614588));
#293354=CARTESIAN_POINT('Ctrl Pts',(-2.65157309100006,15.2,-10.104041173));
#293355=CARTESIAN_POINT('Ctrl Pts',(-2.65157309100006,11.6,-10.104041173));
#293356=CARTESIAN_POINT('Ctrl Pts',(-2.65173333100006,15.2,-10.105476099));
#293357=CARTESIAN_POINT('Ctrl Pts',(-2.65173333100006,11.6,-10.105476099));
#293358=CARTESIAN_POINT('Ctrl Pts',(-2.65189310800006,15.2,-10.106919347));
#293359=CARTESIAN_POINT('Ctrl Pts',(-2.65189310800006,11.6,-10.106919347));
#293360=CARTESIAN_POINT('Ctrl Pts',(-2.65205240400006,15.2,-10.108370899));
#293361=CARTESIAN_POINT('Ctrl Pts',(-2.65205240400006,11.6,-10.108370899));
#293362=CARTESIAN_POINT('Ctrl Pts',(-2.65221120300006,15.2,-10.109830736));
#293363=CARTESIAN_POINT('Ctrl Pts',(-2.65221120300006,11.6,-10.109830736));
#293364=CARTESIAN_POINT('Ctrl Pts',(-2.65236949000006,15.2,-10.11129884));
#293365=CARTESIAN_POINT('Ctrl Pts',(-2.65236949000006,11.6,-10.11129884));
#293366=CARTESIAN_POINT('Ctrl Pts',(-2.65252724700006,15.2,-10.112775192));
#293367=CARTESIAN_POINT('Ctrl Pts',(-2.65252724700006,11.6,-10.112775192));
#293368=CARTESIAN_POINT('Ctrl Pts',(-2.65268445700006,15.2,-10.114259774));
#293369=CARTESIAN_POINT('Ctrl Pts',(-2.65268445700006,11.6,-10.114259774));
#293370=CARTESIAN_POINT('Ctrl Pts',(-2.65284110500006,15.2,-10.115752567));
#293371=CARTESIAN_POINT('Ctrl Pts',(-2.65284110500006,11.6,-10.115752567));
#293372=CARTESIAN_POINT('Ctrl Pts',(-2.65299717300006,15.2,-10.117253555));
#293373=CARTESIAN_POINT('Ctrl Pts',(-2.65299717300006,11.6,-10.117253555));
#293374=CARTESIAN_POINT('Ctrl Pts',(-2.65315264700006,15.2,-10.118762717));
#293375=CARTESIAN_POINT('Ctrl Pts',(-2.65315264700006,11.6,-10.118762717));
#293376=CARTESIAN_POINT('Ctrl Pts',(-2.65330751000006,15.2,-10.120280036));
#293377=CARTESIAN_POINT('Ctrl Pts',(-2.65330751000006,11.6,-10.120280036));
#293378=CARTESIAN_POINT('Ctrl Pts',(-2.65346174600006,15.2,-10.121805494));
#293379=CARTESIAN_POINT('Ctrl Pts',(-2.65346174600006,11.6,-10.121805494));
#293380=CARTESIAN_POINT('Ctrl Pts',(-2.65361534000006,15.2,-10.123339074));
#293381=CARTESIAN_POINT('Ctrl Pts',(-2.65361534000006,11.6,-10.123339074));
#293382=CARTESIAN_POINT('Ctrl Pts',(-2.65376827400006,15.2,-10.124880757));
#293383=CARTESIAN_POINT('Ctrl Pts',(-2.65376827400006,11.6,-10.124880757));
#293384=CARTESIAN_POINT('Ctrl Pts',(-2.65392053400006,15.2,-10.126430526));
#293385=CARTESIAN_POINT('Ctrl Pts',(-2.65392053400006,11.6,-10.126430526));
#293386=CARTESIAN_POINT('Ctrl Pts',(-2.65407210500006,15.2,-10.127988362));
#293387=CARTESIAN_POINT('Ctrl Pts',(-2.65407210500006,11.6,-10.127988362));
#293388=CARTESIAN_POINT('Ctrl Pts',(-2.65422296900006,15.2,-10.129554248));
#293389=CARTESIAN_POINT('Ctrl Pts',(-2.65422296900006,11.6,-10.129554248));
#293390=CARTESIAN_POINT('Ctrl Pts',(-2.65437311200006,15.2,-10.131128167));
#293391=CARTESIAN_POINT('Ctrl Pts',(-2.65437311200006,11.6,-10.131128167));
#293392=CARTESIAN_POINT('Ctrl Pts',(-2.65452251800005,15.2,-10.1327101));
#293393=CARTESIAN_POINT('Ctrl Pts',(-2.65452251800005,11.6,-10.1327101));
#293394=CARTESIAN_POINT('Ctrl Pts',(-2.65467117300005,15.2,-10.134300032));
#293395=CARTESIAN_POINT('Ctrl Pts',(-2.65467117300005,11.6,-10.134300032));
#293396=CARTESIAN_POINT('Ctrl Pts',(-2.65481906000006,15.2,-10.135897942));
#293397=CARTESIAN_POINT('Ctrl Pts',(-2.65481906000006,11.6,-10.135897942));
#293398=CARTESIAN_POINT('Ctrl Pts',(-2.65496616300006,15.2,-10.137503815));
#293399=CARTESIAN_POINT('Ctrl Pts',(-2.65496616300006,11.6,-10.137503815));
#293400=CARTESIAN_POINT('Ctrl Pts',(-2.65511246900005,15.2,-10.139117634));
#293401=CARTESIAN_POINT('Ctrl Pts',(-2.65511246900005,11.6,-10.139117634));
#293402=CARTESIAN_POINT('Ctrl Pts',(-2.65525796200006,15.2,-10.14073938));
#293403=CARTESIAN_POINT('Ctrl Pts',(-2.65525796200006,11.6,-10.14073938));
#293404=CARTESIAN_POINT('Ctrl Pts',(-2.65540262700006,15.2,-10.142369036));
#293405=CARTESIAN_POINT('Ctrl Pts',(-2.65540262700006,11.6,-10.142369036));
#293406=CARTESIAN_POINT('Ctrl Pts',(-2.65554644800006,15.2,-10.144006586));
#293407=CARTESIAN_POINT('Ctrl Pts',(-2.65554644800006,11.6,-10.144006586));
#293408=CARTESIAN_POINT('Ctrl Pts',(-2.65568941100006,15.2,-10.145652013));
#293409=CARTESIAN_POINT('Ctrl Pts',(-2.65568941100006,11.6,-10.145652013));
#293410=CARTESIAN_POINT('Ctrl Pts',(-2.65583150100006,15.2,-10.147305299));
#293411=CARTESIAN_POINT('Ctrl Pts',(-2.65583150100006,11.6,-10.147305299));
#293412=CARTESIAN_POINT('Ctrl Pts',(-2.65597270400006,15.2,-10.148966426));
#293413=CARTESIAN_POINT('Ctrl Pts',(-2.65597270400006,11.6,-10.148966426));
#293414=CARTESIAN_POINT('Ctrl Pts',(-2.65611300400006,15.2,-10.15063538));
#293415=CARTESIAN_POINT('Ctrl Pts',(-2.65611300400006,11.6,-10.15063538));
#293416=CARTESIAN_POINT('Ctrl Pts',(-2.65625238700005,15.2,-10.152312142));
#293417=CARTESIAN_POINT('Ctrl Pts',(-2.65625238700005,11.6,-10.152312142));
#293418=CARTESIAN_POINT('Ctrl Pts',(-2.65639083700006,15.2,-10.153996696));
#293419=CARTESIAN_POINT('Ctrl Pts',(-2.65639083700006,11.6,-10.153996696));
#293420=CARTESIAN_POINT('Ctrl Pts',(-2.65652834300006,15.2,-10.155689024));
#293421=CARTESIAN_POINT('Ctrl Pts',(-2.65652834300006,11.6,-10.155689024));
#293422=CARTESIAN_POINT('Ctrl Pts',(-2.65666488600006,15.2,-10.157389111));
#293423=CARTESIAN_POINT('Ctrl Pts',(-2.65666488600006,11.6,-10.157389111));
#293424=CARTESIAN_POINT('Ctrl Pts',(-2.65680045600006,15.2,-10.159096939));
#293425=CARTESIAN_POINT('Ctrl Pts',(-2.65680045600006,11.6,-10.159096939));
#293426=CARTESIAN_POINT('Ctrl Pts',(-2.65693503500006,15.2,-10.160812491));
#293427=CARTESIAN_POINT('Ctrl Pts',(-2.65693503500006,11.6,-10.160812491));
#293428=CARTESIAN_POINT('Ctrl Pts',(-2.65706861100006,15.2,-10.162535753));
#293429=CARTESIAN_POINT('Ctrl Pts',(-2.65706861100006,11.6,-10.162535753));
#293430=CARTESIAN_POINT('Ctrl Pts',(-2.65720116900006,15.2,-10.164266706));
#293431=CARTESIAN_POINT('Ctrl Pts',(-2.65720116900006,11.6,-10.164266706));
#293432=CARTESIAN_POINT('Ctrl Pts',(-2.65733269400006,15.2,-10.166005334));
#293433=CARTESIAN_POINT('Ctrl Pts',(-2.65733269400006,11.6,-10.166005334));
#293434=CARTESIAN_POINT('Ctrl Pts',(-2.65746317300006,15.2,-10.167751622));
#293435=CARTESIAN_POINT('Ctrl Pts',(-2.65746317300006,11.6,-10.167751622));
#293436=CARTESIAN_POINT('Ctrl Pts',(-2.65759259200005,15.2,-10.169505551));
#293437=CARTESIAN_POINT('Ctrl Pts',(-2.65759259200005,11.6,-10.169505551));
#293438=CARTESIAN_POINT('Ctrl Pts',(-2.65772093700006,15.2,-10.171267108));
#293439=CARTESIAN_POINT('Ctrl Pts',(-2.65772093700006,11.6,-10.171267108));
#293440=CARTESIAN_POINT('Ctrl Pts',(-2.65784819400006,15.2,-10.173036275));
#293441=CARTESIAN_POINT('Ctrl Pts',(-2.65784819400006,11.6,-10.173036275));
#293442=CARTESIAN_POINT('Ctrl Pts',(-2.65797434800006,15.2,-10.174813035));
#293443=CARTESIAN_POINT('Ctrl Pts',(-2.65797434800006,11.6,-10.174813035));
#293444=CARTESIAN_POINT('Ctrl Pts',(-2.65809938700006,15.2,-10.176597374));
#293445=CARTESIAN_POINT('Ctrl Pts',(-2.65809938700006,11.6,-10.176597374));
#293446=CARTESIAN_POINT('Ctrl Pts',(-2.65822329700006,15.2,-10.178389273));
#293447=CARTESIAN_POINT('Ctrl Pts',(-2.65822329700006,11.6,-10.178389273));
#293448=CARTESIAN_POINT('Ctrl Pts',(-2.65834606300006,15.2,-10.18018872));
#293449=CARTESIAN_POINT('Ctrl Pts',(-2.65834606300006,11.6,-10.18018872));
#293450=CARTESIAN_POINT('Ctrl Pts',(-2.65846767200005,15.2,-10.181995694));
#293451=CARTESIAN_POINT('Ctrl Pts',(-2.65846767200005,11.6,-10.181995694));
#293452=CARTESIAN_POINT('Ctrl Pts',(-2.65858811200005,15.2,-10.183810184));
#293453=CARTESIAN_POINT('Ctrl Pts',(-2.65858811200005,11.6,-10.183810184));
#293454=CARTESIAN_POINT('Ctrl Pts',(-2.65870736700006,15.2,-10.185632171));
#293455=CARTESIAN_POINT('Ctrl Pts',(-2.65870736700006,11.6,-10.185632171));
#293456=CARTESIAN_POINT('Ctrl Pts',(-2.65882542500006,15.2,-10.18746164));
#293457=CARTESIAN_POINT('Ctrl Pts',(-2.65882542500006,11.6,-10.18746164));
#293458=CARTESIAN_POINT('Ctrl Pts',(-2.65894227300006,15.2,-10.189298575));
#293459=CARTESIAN_POINT('Ctrl Pts',(-2.65894227300006,11.6,-10.189298575));
#293460=CARTESIAN_POINT('Ctrl Pts',(-2.65905789700006,15.2,-10.191142961));
#293461=CARTESIAN_POINT('Ctrl Pts',(-2.65905789700006,11.6,-10.191142961));
#293462=CARTESIAN_POINT('Ctrl Pts',(-2.65917228200005,15.2,-10.192994781));
#293463=CARTESIAN_POINT('Ctrl Pts',(-2.65917228200005,11.6,-10.192994781));
#293464=CARTESIAN_POINT('Ctrl Pts',(-2.65928541900006,15.2,-10.194854021));
#293465=CARTESIAN_POINT('Ctrl Pts',(-2.65928541900006,11.6,-10.194854021));
#293466=CARTESIAN_POINT('Ctrl Pts',(-2.65939729100006,15.2,-10.196720664));
#293467=CARTESIAN_POINT('Ctrl Pts',(-2.65939729100006,11.6,-10.196720664));
#293468=CARTESIAN_POINT('Ctrl Pts',(-2.65950788700006,15.2,-10.198594695));
#293469=CARTESIAN_POINT('Ctrl Pts',(-2.65950788700006,11.6,-10.198594695));
#293470=CARTESIAN_POINT('Ctrl Pts',(-2.65961719400006,15.2,-10.200476098));
#293471=CARTESIAN_POINT('Ctrl Pts',(-2.65961719400006,11.6,-10.200476098));
#293472=CARTESIAN_POINT('Ctrl Pts',(-2.65972519700005,15.2,-10.202364859));
#293473=CARTESIAN_POINT('Ctrl Pts',(-2.65972519700005,11.6,-10.202364859));
#293474=CARTESIAN_POINT('Ctrl Pts',(-2.65983188500006,15.2,-10.204260961));
#293475=CARTESIAN_POINT('Ctrl Pts',(-2.65983188500006,11.6,-10.204260961));
#293476=CARTESIAN_POINT('Ctrl Pts',(-2.65993724400006,15.2,-10.20616439));
#293477=CARTESIAN_POINT('Ctrl Pts',(-2.65993724400006,11.6,-10.20616439));
#293478=CARTESIAN_POINT('Ctrl Pts',(-2.66004126100006,15.2,-10.208075129));
#293479=CARTESIAN_POINT('Ctrl Pts',(-2.66004126100006,11.6,-10.208075129));
#293480=CARTESIAN_POINT('Ctrl Pts',(-2.66014392500006,15.2,-10.209993165));
#293481=CARTESIAN_POINT('Ctrl Pts',(-2.66014392500006,11.6,-10.209993165));
#293482=CARTESIAN_POINT('Ctrl Pts',(-2.66024522200006,15.2,-10.21191848));
#293483=CARTESIAN_POINT('Ctrl Pts',(-2.66024522200006,11.6,-10.21191848));
#293484=CARTESIAN_POINT('Ctrl Pts',(-2.66034514100005,15.2,-10.213851061));
#293485=CARTESIAN_POINT('Ctrl Pts',(-2.66034514100005,11.6,-10.213851061));
#293486=CARTESIAN_POINT('Ctrl Pts',(-2.66044366600005,15.2,-10.215790891));
#293487=CARTESIAN_POINT('Ctrl Pts',(-2.66044366600005,11.6,-10.215790891));
#293488=CARTESIAN_POINT('Ctrl Pts',(-2.66054078800006,15.2,-10.217737957));
#293489=CARTESIAN_POINT('Ctrl Pts',(-2.66054078800006,11.6,-10.217737957));
#293490=CARTESIAN_POINT('Ctrl Pts',(-2.66063649100006,15.2,-10.219692242));
#293491=CARTESIAN_POINT('Ctrl Pts',(-2.66063649100006,11.6,-10.219692242));
#293492=CARTESIAN_POINT('Ctrl Pts',(-2.66073076600006,15.2,-10.221653734));
#293493=CARTESIAN_POINT('Ctrl Pts',(-2.66073076600006,11.6,-10.221653734));
#293494=CARTESIAN_POINT('Ctrl Pts',(-2.66082359900006,15.2,-10.223622414));
#293495=CARTESIAN_POINT('Ctrl Pts',(-2.66082359900006,11.6,-10.223622414));
#293496=CARTESIAN_POINT('Ctrl Pts',(-2.66091497700006,15.2,-10.225598269));
#293497=CARTESIAN_POINT('Ctrl Pts',(-2.66091497700006,11.6,-10.225598269));
#293498=CARTESIAN_POINT('Ctrl Pts',(-2.66100488900006,15.2,-10.227581285));
#293499=CARTESIAN_POINT('Ctrl Pts',(-2.66100488900006,11.6,-10.227581285));
#293500=CARTESIAN_POINT('Ctrl Pts',(-2.66109332200006,15.2,-10.229571446));
#293501=CARTESIAN_POINT('Ctrl Pts',(-2.66109332200006,11.6,-10.229571446));
#293502=CARTESIAN_POINT('Ctrl Pts',(-2.66118026300005,15.2,-10.231568737));
#293503=CARTESIAN_POINT('Ctrl Pts',(-2.66118026300005,11.6,-10.231568737));
#293504=CARTESIAN_POINT('Ctrl Pts',(-2.66126570200006,15.2,-10.233573145));
#293505=CARTESIAN_POINT('Ctrl Pts',(-2.66126570200006,11.6,-10.233573145));
#293506=CARTESIAN_POINT('Ctrl Pts',(-2.66134962600006,15.2,-10.235584653));
#293507=CARTESIAN_POINT('Ctrl Pts',(-2.66134962600006,11.6,-10.235584653));
#293508=CARTESIAN_POINT('Ctrl Pts',(-2.66143202200006,15.2,-10.237603248));
#293509=CARTESIAN_POINT('Ctrl Pts',(-2.66143202200006,11.6,-10.237603248));
#293510=CARTESIAN_POINT('Ctrl Pts',(-2.66151287900006,15.2,-10.239628914));
#293511=CARTESIAN_POINT('Ctrl Pts',(-2.66151287900006,11.6,-10.239628914));
#293512=CARTESIAN_POINT('Ctrl Pts',(-2.66159218500006,15.2,-10.241661637));
#293513=CARTESIAN_POINT('Ctrl Pts',(-2.66159218500006,11.6,-10.241661637));
#293514=CARTESIAN_POINT('Ctrl Pts',(-2.66166992800006,15.2,-10.243701403));
#293515=CARTESIAN_POINT('Ctrl Pts',(-2.66166992800006,11.6,-10.243701403));
#293516=CARTESIAN_POINT('Ctrl Pts',(-2.66174609500006,15.2,-10.245748197));
#293517=CARTESIAN_POINT('Ctrl Pts',(-2.66174609500006,11.6,-10.245748197));
#293518=CARTESIAN_POINT('Ctrl Pts',(-2.66182067500006,15.2,-10.247802005));
#293519=CARTESIAN_POINT('Ctrl Pts',(-2.66182067500006,11.6,-10.247802005));
#293520=CARTESIAN_POINT('Ctrl Pts',(-2.66189365800006,15.2,-10.249862812));
#293521=CARTESIAN_POINT('Ctrl Pts',(-2.66189365800006,11.6,-10.249862812));
#293522=CARTESIAN_POINT('Ctrl Pts',(-2.66196503000006,15.2,-10.251930603));
#293523=CARTESIAN_POINT('Ctrl Pts',(-2.66196503000006,11.6,-10.251930603));
#293524=CARTESIAN_POINT('Ctrl Pts',(-2.66203478000006,15.2,-10.254005366));
#293525=CARTESIAN_POINT('Ctrl Pts',(-2.66203478000006,11.6,-10.254005366));
#293526=CARTESIAN_POINT('Ctrl Pts',(-2.66210289700005,15.2,-10.256087084));
#293527=CARTESIAN_POINT('Ctrl Pts',(-2.66210289700005,11.6,-10.256087084));
#293528=CARTESIAN_POINT('Ctrl Pts',(-2.66216936800005,15.2,-10.258175744));
#293529=CARTESIAN_POINT('Ctrl Pts',(-2.66216936800005,11.6,-10.258175744));
#293530=CARTESIAN_POINT('Ctrl Pts',(-2.66223418300005,15.2,-10.260271331));
#293531=CARTESIAN_POINT('Ctrl Pts',(-2.66223418300005,11.6,-10.260271331));
#293532=CARTESIAN_POINT('Ctrl Pts',(-2.66229733100006,15.2,-10.262373833));
#293533=CARTESIAN_POINT('Ctrl Pts',(-2.66229733100006,11.6,-10.262373833));
#293534=CARTESIAN_POINT('Ctrl Pts',(-2.66235879800006,15.2,-10.264483233));
#293535=CARTESIAN_POINT('Ctrl Pts',(-2.66235879800006,11.6,-10.264483233));
#293536=CARTESIAN_POINT('Ctrl Pts',(-2.66241857500006,15.2,-10.266599519));
#293537=CARTESIAN_POINT('Ctrl Pts',(-2.66241857500006,11.6,-10.266599519));
#293538=CARTESIAN_POINT('Ctrl Pts',(-2.66247664900006,15.2,-10.268722675));
#293539=CARTESIAN_POINT('Ctrl Pts',(-2.66247664900006,11.6,-10.268722675));
#293540=CARTESIAN_POINT('Ctrl Pts',(-2.66253301000006,15.2,-10.270852689));
#293541=CARTESIAN_POINT('Ctrl Pts',(-2.66253301000006,11.6,-10.270852689));
#293542=CARTESIAN_POINT('Ctrl Pts',(-2.66258764600006,15.2,-10.272989546));
#293543=CARTESIAN_POINT('Ctrl Pts',(-2.66258764600006,11.6,-10.272989546));
#293544=CARTESIAN_POINT('Ctrl Pts',(-2.66264054600006,15.2,-10.275133231));
#293545=CARTESIAN_POINT('Ctrl Pts',(-2.66264054600006,11.6,-10.275133231));
#293546=CARTESIAN_POINT('Ctrl Pts',(-2.66269169900006,15.2,-10.277283732));
#293547=CARTESIAN_POINT('Ctrl Pts',(-2.66269169900006,11.6,-10.277283732));
#293548=CARTESIAN_POINT('Ctrl Pts',(-2.66274109400006,15.2,-10.279441034));
#293549=CARTESIAN_POINT('Ctrl Pts',(-2.66274109400006,11.6,-10.279441034));
#293550=CARTESIAN_POINT('Ctrl Pts',(-2.66278872000006,15.2,-10.281605123));
#293551=CARTESIAN_POINT('Ctrl Pts',(-2.66278872000006,11.6,-10.281605123));
#293552=CARTESIAN_POINT('Ctrl Pts',(-2.66283456500005,15.2,-10.283775986));
#293553=CARTESIAN_POINT('Ctrl Pts',(-2.66283456500005,11.6,-10.283775986));
#293554=CARTESIAN_POINT('Ctrl Pts',(-2.66287862000006,15.2,-10.28595361));
#293555=CARTESIAN_POINT('Ctrl Pts',(-2.66287862000006,11.6,-10.28595361));
#293556=CARTESIAN_POINT('Ctrl Pts',(-2.66292087200006,15.2,-10.288137978));
#293557=CARTESIAN_POINT('Ctrl Pts',(-2.66292087200006,11.6,-10.288137978));
#293558=CARTESIAN_POINT('Ctrl Pts',(-2.66296131100006,15.2,-10.290329079));
#293559=CARTESIAN_POINT('Ctrl Pts',(-2.66296131100006,11.6,-10.290329079));
#293560=CARTESIAN_POINT('Ctrl Pts',(-2.66299992500006,15.2,-10.292526898));
#293561=CARTESIAN_POINT('Ctrl Pts',(-2.66299992500006,11.6,-10.292526898));
#293562=CARTESIAN_POINT('Ctrl Pts',(-2.66303670700006,15.2,-10.294731423));
#293563=CARTESIAN_POINT('Ctrl Pts',(-2.66303670700006,11.6,-10.294731423));
#293564=CARTESIAN_POINT('Ctrl Pts',(-2.66307164100006,15.2,-10.296942639));
#293565=CARTESIAN_POINT('Ctrl Pts',(-2.66307164100006,11.6,-10.296942639));
#293566=CARTESIAN_POINT('Ctrl Pts',(-2.66310472000006,15.2,-10.299160533));
#293567=CARTESIAN_POINT('Ctrl Pts',(-2.66310472000006,11.6,-10.299160533));
#293568=CARTESIAN_POINT('Ctrl Pts',(-2.66313593100006,15.2,-10.301385092));
#293569=CARTESIAN_POINT('Ctrl Pts',(-2.66313593100006,11.6,-10.301385092));
#293570=CARTESIAN_POINT('Ctrl Pts',(-2.66316526600006,15.2,-10.3036163));
#293571=CARTESIAN_POINT('Ctrl Pts',(-2.66316526600006,11.6,-10.3036163));
#293572=CARTESIAN_POINT('Ctrl Pts',(-2.66319271200006,15.2,-10.305854147));
#293573=CARTESIAN_POINT('Ctrl Pts',(-2.66319271200006,11.6,-10.305854147));
#293574=CARTESIAN_POINT('Ctrl Pts',(-2.66321825900006,15.2,-10.308098617));
#293575=CARTESIAN_POINT('Ctrl Pts',(-2.66321825900006,11.6,-10.308098617));
#293576=CARTESIAN_POINT('Ctrl Pts',(-2.66324189700006,15.2,-10.310349696));
#293577=CARTESIAN_POINT('Ctrl Pts',(-2.66324189700006,11.6,-10.310349696));
#293578=CARTESIAN_POINT('Ctrl Pts',(-2.66326361600006,15.2,-10.312607374));
#293579=CARTESIAN_POINT('Ctrl Pts',(-2.66326361600006,11.6,-10.312607374));
#293580=CARTESIAN_POINT('Ctrl Pts',(-2.66328340400006,15.2,-10.314871635));
#293581=CARTESIAN_POINT('Ctrl Pts',(-2.66328340400006,11.6,-10.314871635));
#293582=CARTESIAN_POINT('Ctrl Pts',(-2.66330125200006,15.2,-10.317142467));
#293583=CARTESIAN_POINT('Ctrl Pts',(-2.66330125200006,11.6,-10.317142467));
#293584=CARTESIAN_POINT('Ctrl Pts',(-2.66331714900006,15.2,-10.319419855));
#293585=CARTESIAN_POINT('Ctrl Pts',(-2.66331714900006,11.6,-10.319419855));
#293586=CARTESIAN_POINT('Ctrl Pts',(-2.66333108600006,15.2,-10.321703788));
#293587=CARTESIAN_POINT('Ctrl Pts',(-2.66333108600006,11.6,-10.321703788));
#293588=CARTESIAN_POINT('Ctrl Pts',(-2.66334305100006,15.2,-10.323994252));
#293589=CARTESIAN_POINT('Ctrl Pts',(-2.66334305100006,11.6,-10.323994252));
#293590=CARTESIAN_POINT('Ctrl Pts',(-2.66335303300006,15.2,-10.326291233));
#293591=CARTESIAN_POINT('Ctrl Pts',(-2.66335303300006,11.6,-10.326291233));
#293592=CARTESIAN_POINT('Ctrl Pts',(-2.66336102400006,15.2,-10.328594718));
#293593=CARTESIAN_POINT('Ctrl Pts',(-2.66336102400006,11.6,-10.328594718));
#293594=CARTESIAN_POINT('Ctrl Pts',(-2.66336701400005,15.2,-10.330904695));
#293595=CARTESIAN_POINT('Ctrl Pts',(-2.66336701400005,11.6,-10.330904695));
#293596=CARTESIAN_POINT('Ctrl Pts',(-2.66337099100005,15.2,-10.33322115));
#293597=CARTESIAN_POINT('Ctrl Pts',(-2.66337099100005,11.6,-10.33322115));
#293598=CARTESIAN_POINT('Ctrl Pts',(-2.66337294600006,15.2,-10.33554407));
#293599=CARTESIAN_POINT('Ctrl Pts',(-2.66337294600006,11.6,-10.33554407));
#293600=CARTESIAN_POINT('Ctrl Pts',(-2.66337286800006,15.2,-10.337873443));
#293601=CARTESIAN_POINT('Ctrl Pts',(-2.66337286800006,11.6,-10.337873443));
#293602=CARTESIAN_POINT('Ctrl Pts',(-2.66337074900005,15.2,-10.340209254));
#293603=CARTESIAN_POINT('Ctrl Pts',(-2.66337074900005,11.6,-10.340209254));
#293604=CARTESIAN_POINT('Ctrl Pts',(-2.66336657800006,15.2,-10.342551492));
#293605=CARTESIAN_POINT('Ctrl Pts',(-2.66336657800006,11.6,-10.342551492));
#293606=CARTESIAN_POINT('Ctrl Pts',(-2.66336034400006,15.2,-10.344900143));
#293607=CARTESIAN_POINT('Ctrl Pts',(-2.66336034400006,11.6,-10.344900143));
#293608=CARTESIAN_POINT('Ctrl Pts',(-2.66335203800006,15.2,-10.347255195));
#293609=CARTESIAN_POINT('Ctrl Pts',(-2.66335203800006,11.6,-10.347255195));
#293610=CARTESIAN_POINT('Ctrl Pts',(-2.66334165000006,15.2,-10.349616635));
#293611=CARTESIAN_POINT('Ctrl Pts',(-2.66334165000006,11.6,-10.349616635));
#293612=CARTESIAN_POINT('Ctrl Pts',(-2.66332917200006,15.2,-10.351984448));
#293613=CARTESIAN_POINT('Ctrl Pts',(-2.66332917200006,11.6,-10.351984448));
#293614=CARTESIAN_POINT('Ctrl Pts',(-2.66331459100006,15.2,-10.354358625));
#293615=CARTESIAN_POINT('Ctrl Pts',(-2.66331459100006,11.6,-10.354358625));
#293616=CARTESIAN_POINT('Ctrl Pts',(-2.66329789900006,15.2,-10.35673915));
#293617=CARTESIAN_POINT('Ctrl Pts',(-2.66329789900006,11.6,-10.35673915));
#293618=CARTESIAN_POINT('Ctrl Pts',(-2.66327908700006,15.2,-10.359126011));
#293619=CARTESIAN_POINT('Ctrl Pts',(-2.66327908700006,11.6,-10.359126011));
#293620=CARTESIAN_POINT('Ctrl Pts',(-2.66325814400005,15.2,-10.361519197));
#293621=CARTESIAN_POINT('Ctrl Pts',(-2.66325814400005,11.6,-10.361519197));
#293622=CARTESIAN_POINT('Ctrl Pts',(-2.66323506000006,15.2,-10.363918694));
#293623=CARTESIAN_POINT('Ctrl Pts',(-2.66323506000006,11.6,-10.363918694));
#293624=CARTESIAN_POINT('Ctrl Pts',(-2.66320982800006,15.2,-10.36632449));
#293625=CARTESIAN_POINT('Ctrl Pts',(-2.66320982800006,11.6,-10.36632449));
#293626=CARTESIAN_POINT('Ctrl Pts',(-2.66318243600006,15.2,-10.36873657));
#293627=CARTESIAN_POINT('Ctrl Pts',(-2.66318243600006,11.6,-10.36873657));
#293628=CARTESIAN_POINT('Ctrl Pts',(-2.66315287500006,15.2,-10.371154926));
#293629=CARTESIAN_POINT('Ctrl Pts',(-2.66315287500006,11.6,-10.371154926));
#293630=CARTESIAN_POINT('Ctrl Pts',(-2.66312113600006,15.2,-10.37357954));
#293631=CARTESIAN_POINT('Ctrl Pts',(-2.66312113600006,11.6,-10.37357954));
#293632=CARTESIAN_POINT('Ctrl Pts',(-2.66308721000006,15.2,-10.376010404));
#293633=CARTESIAN_POINT('Ctrl Pts',(-2.66308721000006,11.6,-10.376010404));
#293634=CARTESIAN_POINT('Ctrl Pts',(-2.66305108600006,15.2,-10.378447503));
#293635=CARTESIAN_POINT('Ctrl Pts',(-2.66305108600006,11.6,-10.378447503));
#293636=CARTESIAN_POINT('Ctrl Pts',(-2.66301275600005,15.2,-10.380890826));
#293637=CARTESIAN_POINT('Ctrl Pts',(-2.66301275600005,11.6,-10.380890826));
#293638=CARTESIAN_POINT('Ctrl Pts',(-2.66297221000006,15.2,-10.383340359));
#293639=CARTESIAN_POINT('Ctrl Pts',(-2.66297221000006,11.6,-10.383340359));
#293640=CARTESIAN_POINT('Ctrl Pts',(-2.66292943900006,15.2,-10.38579609));
#293641=CARTESIAN_POINT('Ctrl Pts',(-2.66292943900006,11.6,-10.38579609));
#293642=CARTESIAN_POINT('Ctrl Pts',(-2.66288443400006,15.2,-10.388258008));
#293643=CARTESIAN_POINT('Ctrl Pts',(-2.66288443400006,11.6,-10.388258008));
#293644=CARTESIAN_POINT('Ctrl Pts',(-2.66283718400006,15.2,-10.390726099));
#293645=CARTESIAN_POINT('Ctrl Pts',(-2.66283718400006,11.6,-10.390726099));
#293646=CARTESIAN_POINT('Ctrl Pts',(-2.66278768300006,15.2,-10.393200352));
#293647=CARTESIAN_POINT('Ctrl Pts',(-2.66278768300006,11.6,-10.393200352));
#293648=CARTESIAN_POINT('Ctrl Pts',(-2.66273591900006,15.2,-10.395680753));
#293649=CARTESIAN_POINT('Ctrl Pts',(-2.66273591900006,11.6,-10.395680753));
#293650=CARTESIAN_POINT('Ctrl Pts',(-2.66268188400006,15.2,-10.398167292));
#293651=CARTESIAN_POINT('Ctrl Pts',(-2.66268188400006,11.6,-10.398167292));
#293652=CARTESIAN_POINT('Ctrl Pts',(-2.66262556800006,15.2,-10.400659955));
#293653=CARTESIAN_POINT('Ctrl Pts',(-2.66262556800006,11.6,-10.400659955));
#293654=CARTESIAN_POINT('Ctrl Pts',(-2.66256696400006,15.2,-10.403158731));
#293655=CARTESIAN_POINT('Ctrl Pts',(-2.66256696400006,11.6,-10.403158731));
#293656=CARTESIAN_POINT('Ctrl Pts',(-2.66250606100006,15.2,-10.405663606));
#293657=CARTESIAN_POINT('Ctrl Pts',(-2.66250606100006,11.6,-10.405663606));
#293658=CARTESIAN_POINT('Ctrl Pts',(-2.66244285200006,15.2,-10.40817457));
#293659=CARTESIAN_POINT('Ctrl Pts',(-2.66244285200006,11.6,-10.40817457));
#293660=CARTESIAN_POINT('Ctrl Pts',(-2.66237732500006,15.2,-10.410691609));
#293661=CARTESIAN_POINT('Ctrl Pts',(-2.66237732500006,11.6,-10.410691609));
#293662=CARTESIAN_POINT('Ctrl Pts',(-2.66230947400006,15.2,-10.413214712));
#293663=CARTESIAN_POINT('Ctrl Pts',(-2.66230947400006,11.6,-10.413214712));
#293664=CARTESIAN_POINT('Ctrl Pts',(-2.66223928800006,15.2,-10.415743867));
#293665=CARTESIAN_POINT('Ctrl Pts',(-2.66223928800006,11.6,-10.415743867));
#293666=CARTESIAN_POINT('Ctrl Pts',(-2.66216676000006,15.2,-10.41827906));
#293667=CARTESIAN_POINT('Ctrl Pts',(-2.66216676000006,11.6,-10.41827906));
#293668=CARTESIAN_POINT('Ctrl Pts',(-2.66209187900006,15.2,-10.420820282));
#293669=CARTESIAN_POINT('Ctrl Pts',(-2.66209187900006,11.6,-10.420820282));
#293670=CARTESIAN_POINT('Ctrl Pts',(-2.66201463800006,15.2,-10.423367519));
#293671=CARTESIAN_POINT('Ctrl Pts',(-2.66201463800006,11.6,-10.423367519));
#293672=CARTESIAN_POINT('Ctrl Pts',(-2.66193502800005,15.2,-10.42592076));
#293673=CARTESIAN_POINT('Ctrl Pts',(-2.66193502800005,11.6,-10.42592076));
#293674=CARTESIAN_POINT('Ctrl Pts',(-2.66185304000006,15.2,-10.428479993));
#293675=CARTESIAN_POINT('Ctrl Pts',(-2.66185304000006,11.6,-10.428479993));
#293676=CARTESIAN_POINT('Ctrl Pts',(-2.66176866500006,15.2,-10.431045206));
#293677=CARTESIAN_POINT('Ctrl Pts',(-2.66176866500006,11.6,-10.431045206));
#293678=CARTESIAN_POINT('Ctrl Pts',(-2.66168189500006,15.2,-10.433616386));
#293679=CARTESIAN_POINT('Ctrl Pts',(-2.66168189500006,11.6,-10.433616386));
#293680=CARTESIAN_POINT('Ctrl Pts',(-2.66159272000006,15.2,-10.436193522));
#293681=CARTESIAN_POINT('Ctrl Pts',(-2.66159272000006,11.6,-10.436193522));
#293682=CARTESIAN_POINT('Ctrl Pts',(-2.66150113200006,15.2,-10.438776602));
#293683=CARTESIAN_POINT('Ctrl Pts',(-2.66150113200006,11.6,-10.438776602));
#293684=CARTESIAN_POINT('Ctrl Pts',(-2.66140712500006,15.2,-10.441365614));
#293685=CARTESIAN_POINT('Ctrl Pts',(-2.66140712500006,11.6,-10.441365614));
#293686=CARTESIAN_POINT('Ctrl Pts',(-2.66131068600005,15.2,-10.443960548));
#293687=CARTESIAN_POINT('Ctrl Pts',(-2.66131068600005,11.6,-10.443960548));
#293688=CARTESIAN_POINT('Ctrl Pts',(-2.66121180900006,15.2,-10.446561389));
#293689=CARTESIAN_POINT('Ctrl Pts',(-2.66121180900006,11.6,-10.446561389));
#293690=CARTESIAN_POINT('Ctrl Pts',(-2.66111048600005,15.2,-10.449168128));
#293691=CARTESIAN_POINT('Ctrl Pts',(-2.66111048600005,11.6,-10.449168128));
#293692=CARTESIAN_POINT('Ctrl Pts',(-2.66100670800005,15.2,-10.451780752));
#293693=CARTESIAN_POINT('Ctrl Pts',(-2.66100670800005,11.6,-10.451780752));
#293694=CARTESIAN_POINT('Ctrl Pts',(-2.66090046500006,15.2,-10.45439925));
#293695=CARTESIAN_POINT('Ctrl Pts',(-2.66090046500006,11.6,-10.45439925));
#293696=CARTESIAN_POINT('Ctrl Pts',(-2.66079175100006,15.2,-10.457023609));
#293697=CARTESIAN_POINT('Ctrl Pts',(-2.66079175100006,11.6,-10.457023609));
#293698=CARTESIAN_POINT('Ctrl Pts',(-2.66068055500006,15.2,-10.459653819));
#293699=CARTESIAN_POINT('Ctrl Pts',(-2.66068055500006,11.6,-10.459653819));
#293700=CARTESIAN_POINT('Ctrl Pts',(-2.66056687200006,15.2,-10.462289867));
#293701=CARTESIAN_POINT('Ctrl Pts',(-2.66056687200006,11.6,-10.462289867));
#293702=CARTESIAN_POINT('Ctrl Pts',(-2.66045069100006,15.2,-10.464931742));
#293703=CARTESIAN_POINT('Ctrl Pts',(-2.66045069100006,11.6,-10.464931742));
#293704=CARTESIAN_POINT('Ctrl Pts',(-2.66033200500006,15.2,-10.467579434));
#293705=CARTESIAN_POINT('Ctrl Pts',(-2.66033200500006,11.6,-10.467579434));
#293706=CARTESIAN_POINT('Ctrl Pts',(-2.66021080500006,15.2,-10.470232928));
#293707=CARTESIAN_POINT('Ctrl Pts',(-2.66021080500006,11.6,-10.470232928));
#293708=CARTESIAN_POINT('Ctrl Pts',(-2.66008708400005,15.2,-10.472892215));
#293709=CARTESIAN_POINT('Ctrl Pts',(-2.66008708400005,11.6,-10.472892215));
#293710=CARTESIAN_POINT('Ctrl Pts',(-2.65996083200006,15.2,-10.475557283));
#293711=CARTESIAN_POINT('Ctrl Pts',(-2.65996083200006,11.6,-10.475557283));
#293712=CARTESIAN_POINT('Ctrl Pts',(-2.65983204300006,15.2,-10.47822812));
#293713=CARTESIAN_POINT('Ctrl Pts',(-2.65983204300006,11.6,-10.47822812));
#293714=CARTESIAN_POINT('Ctrl Pts',(-2.65970070700006,15.2,-10.480904716));
#293715=CARTESIAN_POINT('Ctrl Pts',(-2.65970070700006,11.6,-10.480904716));
#293716=CARTESIAN_POINT('Ctrl Pts',(-2.65956681800006,15.2,-10.483587058));
#293717=CARTESIAN_POINT('Ctrl Pts',(-2.65956681800006,11.6,-10.483587058));
#293718=CARTESIAN_POINT('Ctrl Pts',(-2.65943036500006,15.2,-10.486275134));
#293719=CARTESIAN_POINT('Ctrl Pts',(-2.65943036500006,11.6,-10.486275134));
#293720=CARTESIAN_POINT('Ctrl Pts',(-2.65929134200006,15.2,-10.488968935));
#293721=CARTESIAN_POINT('Ctrl Pts',(-2.65929134200006,11.6,-10.488968935));
#293722=CARTESIAN_POINT('Ctrl Pts',(-2.65914974000005,15.2,-10.491668449));
#293723=CARTESIAN_POINT('Ctrl Pts',(-2.65914974000005,11.6,-10.491668449));
#293724=CARTESIAN_POINT('Ctrl Pts',(-2.65900555300006,15.2,-10.494373662));
#293725=CARTESIAN_POINT('Ctrl Pts',(-2.65900555300006,11.6,-10.494373662));
#293726=CARTESIAN_POINT('Ctrl Pts',(-2.65885877000006,15.2,-10.497084566));
#293727=CARTESIAN_POINT('Ctrl Pts',(-2.65885877000006,11.6,-10.497084566));
#293728=CARTESIAN_POINT('Ctrl Pts',(-2.65870938700006,15.2,-10.499801149));
#293729=CARTESIAN_POINT('Ctrl Pts',(-2.65870938700006,11.6,-10.499801149));
#293730=CARTESIAN_POINT('Ctrl Pts',(-2.65855739200005,15.2,-10.502523398));
#293731=CARTESIAN_POINT('Ctrl Pts',(-2.65855739200005,11.6,-10.502523398));
#293732=CARTESIAN_POINT('Ctrl Pts',(-2.65840277900006,15.2,-10.505251303));
#293733=CARTESIAN_POINT('Ctrl Pts',(-2.65840277900006,11.6,-10.505251303));
#293734=CARTESIAN_POINT('Ctrl Pts',(-2.65824554000006,15.2,-10.507984854));
#293735=CARTESIAN_POINT('Ctrl Pts',(-2.65824554000006,11.6,-10.507984854));
#293736=CARTESIAN_POINT('Ctrl Pts',(-2.65808566800006,15.2,-10.510724037));
#293737=CARTESIAN_POINT('Ctrl Pts',(-2.65808566800006,11.6,-10.510724037));
#293738=CARTESIAN_POINT('Ctrl Pts',(-2.65792315500006,15.2,-10.513468843));
#293739=CARTESIAN_POINT('Ctrl Pts',(-2.65792315500006,11.6,-10.513468843));
#293740=CARTESIAN_POINT('Ctrl Pts',(-2.65775799200005,15.2,-10.51621926));
#293741=CARTESIAN_POINT('Ctrl Pts',(-2.65775799200005,11.6,-10.51621926));
#293742=CARTESIAN_POINT('Ctrl Pts',(-2.65759017200006,15.2,-10.518975277));
#293743=CARTESIAN_POINT('Ctrl Pts',(-2.65759017200006,11.6,-10.518975277));
#293744=CARTESIAN_POINT('Ctrl Pts',(-2.65741968700006,15.2,-10.521736883));
#293745=CARTESIAN_POINT('Ctrl Pts',(-2.65741968700006,11.6,-10.521736883));
#293746=CARTESIAN_POINT('Ctrl Pts',(-2.65724653100006,15.2,-10.524504067));
#293747=CARTESIAN_POINT('Ctrl Pts',(-2.65724653100006,11.6,-10.524504067));
#293748=CARTESIAN_POINT('Ctrl Pts',(-2.65707069400006,15.2,-10.527276817));
#293749=CARTESIAN_POINT('Ctrl Pts',(-2.65707069400006,11.6,-10.527276817));
#293750=CARTESIAN_POINT('Ctrl Pts',(-2.65689217000005,15.2,-10.530055124));
#293751=CARTESIAN_POINT('Ctrl Pts',(-2.65689217000005,11.6,-10.530055124));
#293752=CARTESIAN_POINT('Ctrl Pts',(-2.65671095000005,15.2,-10.532838975));
#293753=CARTESIAN_POINT('Ctrl Pts',(-2.65671095000005,11.6,-10.532838975));
#293754=CARTESIAN_POINT('Ctrl Pts',(-2.65652702800006,15.2,-10.535628359));
#293755=CARTESIAN_POINT('Ctrl Pts',(-2.65652702800006,11.6,-10.535628359));
#293756=CARTESIAN_POINT('Ctrl Pts',(-2.65634039600006,15.2,-10.538423267));
#293757=CARTESIAN_POINT('Ctrl Pts',(-2.65634039600006,11.6,-10.538423267));
#293758=CARTESIAN_POINT('Ctrl Pts',(-2.65615104500006,15.2,-10.541223686));
#293759=CARTESIAN_POINT('Ctrl Pts',(-2.65615104500006,11.6,-10.541223686));
#293760=CARTESIAN_POINT('Ctrl Pts',(-2.65595897100006,15.2,-10.544029605));
#293761=CARTESIAN_POINT('Ctrl Pts',(-2.65595897100006,11.6,-10.544029605));
#293762=CARTESIAN_POINT('Ctrl Pts',(-2.65576416300005,15.2,-10.546841016));
#293763=CARTESIAN_POINT('Ctrl Pts',(-2.65576416300005,11.6,-10.546841016));
#293764=CARTESIAN_POINT('Ctrl Pts',(-2.65556661400006,15.2,-10.549657904));
#293765=CARTESIAN_POINT('Ctrl Pts',(-2.65556661400006,11.6,-10.549657904));
#293766=CARTESIAN_POINT('Ctrl Pts',(-2.65536631800006,15.2,-10.552480261));
#293767=CARTESIAN_POINT('Ctrl Pts',(-2.65536631800006,11.6,-10.552480261));
#293768=CARTESIAN_POINT('Ctrl Pts',(-2.65516326800005,15.2,-10.555308075));
#293769=CARTESIAN_POINT('Ctrl Pts',(-2.65516326800005,11.6,-10.555308075));
#293770=CARTESIAN_POINT('Ctrl Pts',(-2.65495745400006,15.2,-10.558141335));
#293771=CARTESIAN_POINT('Ctrl Pts',(-2.65495745400006,11.6,-10.558141335));
#293772=CARTESIAN_POINT('Ctrl Pts',(-2.65474887200006,15.2,-10.560980032));
#293773=CARTESIAN_POINT('Ctrl Pts',(-2.65474887200006,11.6,-10.560980032));
#293774=CARTESIAN_POINT('Ctrl Pts',(-2.65453751300006,15.2,-10.563824152));
#293775=CARTESIAN_POINT('Ctrl Pts',(-2.65453751300006,11.6,-10.563824152));
#293776=CARTESIAN_POINT('Ctrl Pts',(-2.65432336900006,15.2,-10.566673688));
#293777=CARTESIAN_POINT('Ctrl Pts',(-2.65432336900006,11.6,-10.566673688));
#293778=CARTESIAN_POINT('Ctrl Pts',(-2.65410643400006,15.2,-10.569528625));
#293779=CARTESIAN_POINT('Ctrl Pts',(-2.65410643400006,11.6,-10.569528625));
#293780=CARTESIAN_POINT('Ctrl Pts',(-2.65388670100006,15.2,-10.572388956));
#293781=CARTESIAN_POINT('Ctrl Pts',(-2.65388670100006,11.6,-10.572388956));
#293782=CARTESIAN_POINT('Ctrl Pts',(-2.65366416100006,15.2,-10.575254669));
#293783=CARTESIAN_POINT('Ctrl Pts',(-2.65366416100006,11.6,-10.575254669));
#293784=CARTESIAN_POINT('Ctrl Pts',(-2.65343880900006,15.2,-10.578125752));
#293785=CARTESIAN_POINT('Ctrl Pts',(-2.65343880900006,11.6,-10.578125752));
#293786=CARTESIAN_POINT('Ctrl Pts',(-2.65321063600005,15.2,-10.581002197));
#293787=CARTESIAN_POINT('Ctrl Pts',(-2.65321063600005,11.6,-10.581002197));
#293788=CARTESIAN_POINT('Ctrl Pts',(-2.65297963600006,15.2,-10.58388399));
#293789=CARTESIAN_POINT('Ctrl Pts',(-2.65297963600006,11.6,-10.58388399));
#293790=CARTESIAN_POINT('Ctrl Pts',(-2.65274580100006,15.2,-10.586771123));
#293791=CARTESIAN_POINT('Ctrl Pts',(-2.65274580100006,11.6,-10.586771123));
#293792=CARTESIAN_POINT('Ctrl Pts',(-2.65250912600006,15.2,-10.589663585));
#293793=CARTESIAN_POINT('Ctrl Pts',(-2.65250912600006,11.6,-10.589663585));
#293794=CARTESIAN_POINT('Ctrl Pts',(-2.65226960100006,15.2,-10.592561365));
#293795=CARTESIAN_POINT('Ctrl Pts',(-2.65226960100006,11.6,-10.592561365));
#293796=CARTESIAN_POINT('Ctrl Pts',(-2.65202722100006,15.2,-10.595464452));
#293797=CARTESIAN_POINT('Ctrl Pts',(-2.65202722100006,11.6,-10.595464452));
#293798=CARTESIAN_POINT('Ctrl Pts',(-2.65178197900005,15.2,-10.598372836));
#293799=CARTESIAN_POINT('Ctrl Pts',(-2.65178197900005,11.6,-10.598372836));
#293800=CARTESIAN_POINT('Ctrl Pts',(-2.65153386700006,15.2,-10.601286506));
#293801=CARTESIAN_POINT('Ctrl Pts',(-2.65153386700006,11.6,-10.601286506));
#293802=CARTESIAN_POINT('Ctrl Pts',(-2.65128287800006,15.2,-10.604205452));
#293803=CARTESIAN_POINT('Ctrl Pts',(-2.65128287800006,11.6,-10.604205452));
#293804=CARTESIAN_POINT('Ctrl Pts',(-2.65102900700006,15.2,-10.607129663));
#293805=CARTESIAN_POINT('Ctrl Pts',(-2.65102900700006,11.6,-10.607129663));
#293806=CARTESIAN_POINT('Ctrl Pts',(-2.65077224500006,15.2,-10.610059129));
#293807=CARTESIAN_POINT('Ctrl Pts',(-2.65077224500006,11.6,-10.610059129));
#293808=CARTESIAN_POINT('Ctrl Pts',(-2.65051258500006,15.2,-10.61299384));
#293809=CARTESIAN_POINT('Ctrl Pts',(-2.65051258500006,11.6,-10.61299384));
#293810=CARTESIAN_POINT('Ctrl Pts',(-2.65025002300006,15.2,-10.615933785));
#293811=CARTESIAN_POINT('Ctrl Pts',(-2.65025002300006,11.6,-10.615933785));
#293812=CARTESIAN_POINT('Ctrl Pts',(-2.64998454800006,15.2,-10.618878952));
#293813=CARTESIAN_POINT('Ctrl Pts',(-2.64998454800006,11.6,-10.618878952));
#293814=CARTESIAN_POINT('Ctrl Pts',(-2.64971615600006,15.2,-10.621829333));
#293815=CARTESIAN_POINT('Ctrl Pts',(-2.64971615600006,11.6,-10.621829333));
#293816=CARTESIAN_POINT('Ctrl Pts',(-2.64944484000006,15.2,-10.624784916));
#293817=CARTESIAN_POINT('Ctrl Pts',(-2.64944484000006,11.6,-10.624784916));
#293818=CARTESIAN_POINT('Ctrl Pts',(-2.64917059300006,15.2,-10.627745692));
#293819=CARTESIAN_POINT('Ctrl Pts',(-2.64917059300006,11.6,-10.627745692));
#293820=CARTESIAN_POINT('Ctrl Pts',(-2.64889340700006,15.2,-10.63071165));
#293821=CARTESIAN_POINT('Ctrl Pts',(-2.64889340700006,11.6,-10.63071165));
#293822=CARTESIAN_POINT('Ctrl Pts',(-2.64861327700005,15.2,-10.63368278));
#293823=CARTESIAN_POINT('Ctrl Pts',(-2.64861327700005,11.6,-10.63368278));
#293824=CARTESIAN_POINT('Ctrl Pts',(-2.64833019600006,15.2,-10.636659071));
#293825=CARTESIAN_POINT('Ctrl Pts',(-2.64833019600006,11.6,-10.636659071));
#293826=CARTESIAN_POINT('Ctrl Pts',(-2.64804415600006,15.2,-10.639640512));
#293827=CARTESIAN_POINT('Ctrl Pts',(-2.64804415600006,11.6,-10.639640512));
#293828=CARTESIAN_POINT('Ctrl Pts',(-2.64775515200005,15.2,-10.642627095));
#293829=CARTESIAN_POINT('Ctrl Pts',(-2.64775515200005,11.6,-10.642627095));
#293830=CARTESIAN_POINT('Ctrl Pts',(-2.64746317600005,15.2,-10.645618808));
#293831=CARTESIAN_POINT('Ctrl Pts',(-2.64746317600005,11.6,-10.645618808));
#293832=CARTESIAN_POINT('Ctrl Pts',(-2.64716822300006,15.2,-10.648615642));
#293833=CARTESIAN_POINT('Ctrl Pts',(-2.64716822300006,11.6,-10.648615642));
#293834=CARTESIAN_POINT('Ctrl Pts',(-2.64687028500005,15.2,-10.651617586));
#293835=CARTESIAN_POINT('Ctrl Pts',(-2.64687028500005,11.6,-10.651617586));
#293836=CARTESIAN_POINT('Ctrl Pts',(-2.64656935600006,15.2,-10.654624629));
#293837=CARTESIAN_POINT('Ctrl Pts',(-2.64656935600006,11.6,-10.654624629));
#293838=CARTESIAN_POINT('Ctrl Pts',(-2.64626543000006,15.2,-10.657636763));
#293839=CARTESIAN_POINT('Ctrl Pts',(-2.64626543000006,11.6,-10.657636763));
#293840=CARTESIAN_POINT('Ctrl Pts',(-2.64595849900005,15.2,-10.660653975));
#293841=CARTESIAN_POINT('Ctrl Pts',(-2.64595849900005,11.6,-10.660653975));
#293842=CARTESIAN_POINT('Ctrl Pts',(-2.64564855800006,15.2,-10.663676257));
#293843=CARTESIAN_POINT('Ctrl Pts',(-2.64564855800006,11.6,-10.663676257));
#293844=CARTESIAN_POINT('Ctrl Pts',(-2.64533560000006,15.2,-10.666703598));
#293845=CARTESIAN_POINT('Ctrl Pts',(-2.64533560000006,11.6,-10.666703598));
#293846=CARTESIAN_POINT('Ctrl Pts',(-2.64501961800006,15.2,-10.669735989));
#293847=CARTESIAN_POINT('Ctrl Pts',(-2.64501961800006,11.6,-10.669735989));
#293848=CARTESIAN_POINT('Ctrl Pts',(-2.64470060600006,15.2,-10.672773418));
#293849=CARTESIAN_POINT('Ctrl Pts',(-2.64470060600006,11.6,-10.672773418));
#293850=CARTESIAN_POINT('Ctrl Pts',(-2.64437855800006,15.2,-10.675815877));
#293851=CARTESIAN_POINT('Ctrl Pts',(-2.64437855800006,11.6,-10.675815877));
#293852=CARTESIAN_POINT('Ctrl Pts',(-2.64405346800006,15.2,-10.678863354));
#293853=CARTESIAN_POINT('Ctrl Pts',(-2.64405346800006,11.6,-10.678863354));
#293854=CARTESIAN_POINT('Ctrl Pts',(-2.64372532800006,15.2,-10.681915841));
#293855=CARTESIAN_POINT('Ctrl Pts',(-2.64372532800006,11.6,-10.681915841));
#293856=CARTESIAN_POINT('Ctrl Pts',(-2.64339413300006,15.2,-10.684973325));
#293857=CARTESIAN_POINT('Ctrl Pts',(-2.64339413300006,11.6,-10.684973325));
#293858=CARTESIAN_POINT('Ctrl Pts',(-2.64305987700005,15.2,-10.688035798));
#293859=CARTESIAN_POINT('Ctrl Pts',(-2.64305987700005,11.6,-10.688035798));
#293860=CARTESIAN_POINT('Ctrl Pts',(-2.64272255200006,15.2,-10.691103251));
#293861=CARTESIAN_POINT('Ctrl Pts',(-2.64272255200006,11.6,-10.691103251));
#293862=CARTESIAN_POINT('Ctrl Pts',(-2.64238215300006,15.2,-10.694175673));
#293863=CARTESIAN_POINT('Ctrl Pts',(-2.64238215300006,11.6,-10.694175673));
#293864=CARTESIAN_POINT('Ctrl Pts',(-2.64203867400005,15.2,-10.697253053));
#293865=CARTESIAN_POINT('Ctrl Pts',(-2.64203867400005,11.6,-10.697253053));
#293866=CARTESIAN_POINT('Ctrl Pts',(-2.64169210800006,15.2,-10.700335382));
#293867=CARTESIAN_POINT('Ctrl Pts',(-2.64169210800006,11.6,-10.700335382));
#293868=CARTESIAN_POINT('Ctrl Pts',(-2.64134244900006,15.2,-10.703422651));
#293869=CARTESIAN_POINT('Ctrl Pts',(-2.64134244900006,11.6,-10.703422651));
#293870=CARTESIAN_POINT('Ctrl Pts',(-2.64098969100006,15.2,-10.706514848));
#293871=CARTESIAN_POINT('Ctrl Pts',(-2.64098969100006,11.6,-10.706514848));
#293872=CARTESIAN_POINT('Ctrl Pts',(-2.64063382800006,15.2,-10.709611965));
#293873=CARTESIAN_POINT('Ctrl Pts',(-2.64063382800006,11.6,-10.709611965));
#293874=CARTESIAN_POINT('Ctrl Pts',(-2.64027485200006,15.2,-10.712713991));
#293875=CARTESIAN_POINT('Ctrl Pts',(-2.64027485200006,11.6,-10.712713991));
#293876=CARTESIAN_POINT('Ctrl Pts',(-2.63991276100006,15.2,-10.715820916));
#293877=CARTESIAN_POINT('Ctrl Pts',(-2.63991276100006,11.6,-10.715820916));
#293878=CARTESIAN_POINT('Ctrl Pts',(-2.63954754500006,15.2,-10.718932731));
#293879=CARTESIAN_POINT('Ctrl Pts',(-2.63954754500006,11.6,-10.718932731));
#293880=CARTESIAN_POINT('Ctrl Pts',(-2.63917919900006,15.2,-10.722049426));
#293881=CARTESIAN_POINT('Ctrl Pts',(-2.63917919900006,11.6,-10.722049426));
#293882=CARTESIAN_POINT('Ctrl Pts',(-2.63880771700005,15.2,-10.725170991));
#293883=CARTESIAN_POINT('Ctrl Pts',(-2.63880771700005,11.6,-10.725170991));
#293884=CARTESIAN_POINT('Ctrl Pts',(-2.63843309400006,15.2,-10.728297416));
#293885=CARTESIAN_POINT('Ctrl Pts',(-2.63843309400006,11.6,-10.728297416));
#293886=CARTESIAN_POINT('Ctrl Pts',(-2.63805532400006,15.2,-10.731428692));
#293887=CARTESIAN_POINT('Ctrl Pts',(-2.63805532400006,11.6,-10.731428692));
#293888=CARTESIAN_POINT('Ctrl Pts',(-2.63767439800006,15.2,-10.734564808));
#293889=CARTESIAN_POINT('Ctrl Pts',(-2.63767439800006,11.6,-10.734564808));
#293890=CARTESIAN_POINT('Ctrl Pts',(-2.63729031400006,15.2,-10.737705755));
#293891=CARTESIAN_POINT('Ctrl Pts',(-2.63729031400006,11.6,-10.737705755));
#293892=CARTESIAN_POINT('Ctrl Pts',(-2.63690306200006,15.2,-10.740851524));
#293893=CARTESIAN_POINT('Ctrl Pts',(-2.63690306200006,11.6,-10.740851524));
#293894=CARTESIAN_POINT('Ctrl Pts',(-2.63651264000006,15.2,-10.744002104));
#293895=CARTESIAN_POINT('Ctrl Pts',(-2.63651264000006,11.6,-10.744002104));
#293896=CARTESIAN_POINT('Ctrl Pts',(-2.63611904100005,15.2,-10.747157485));
#293897=CARTESIAN_POINT('Ctrl Pts',(-2.63611904100005,11.6,-10.747157485));
#293898=CARTESIAN_POINT('Ctrl Pts',(-2.63572225700006,15.2,-10.750317658));
#293899=CARTESIAN_POINT('Ctrl Pts',(-2.63572225700006,11.6,-10.750317658));
#293900=CARTESIAN_POINT('Ctrl Pts',(-2.63532228500006,15.2,-10.753482615));
#293901=CARTESIAN_POINT('Ctrl Pts',(-2.63532228500006,11.6,-10.753482615));
#293902=CARTESIAN_POINT('Ctrl Pts',(-2.63491911700005,15.2,-10.756652345));
#293903=CARTESIAN_POINT('Ctrl Pts',(-2.63491911700005,11.6,-10.756652345));
#293904=CARTESIAN_POINT('Ctrl Pts',(-2.63451274800006,15.2,-10.759826836));
#293905=CARTESIAN_POINT('Ctrl Pts',(-2.63451274800006,11.6,-10.759826836));
#293906=CARTESIAN_POINT('Ctrl Pts',(-2.63410317200006,15.2,-10.763006082));
#293907=CARTESIAN_POINT('Ctrl Pts',(-2.63410317200006,11.6,-10.763006082));
#293908=CARTESIAN_POINT('Ctrl Pts',(-2.63369038300006,15.2,-10.766190071));
#293909=CARTESIAN_POINT('Ctrl Pts',(-2.63369038300006,11.6,-10.766190071));
#293910=CARTESIAN_POINT('Ctrl Pts',(-2.63327437600006,15.2,-10.769378796));
#293911=CARTESIAN_POINT('Ctrl Pts',(-2.63327437600006,11.6,-10.769378796));
#293912=CARTESIAN_POINT('Ctrl Pts',(-2.63285514500006,15.2,-10.772572244));
#293913=CARTESIAN_POINT('Ctrl Pts',(-2.63285514500006,11.6,-10.772572244));
#293914=CARTESIAN_POINT('Ctrl Pts',(-2.63243268300006,15.2,-10.775770408));
#293915=CARTESIAN_POINT('Ctrl Pts',(-2.63243268300006,11.6,-10.775770408));
#293916=CARTESIAN_POINT('Ctrl Pts',(-2.63200698600006,15.2,-10.778973278));
#293917=CARTESIAN_POINT('Ctrl Pts',(-2.63200698600006,11.6,-10.778973278));
#293918=CARTESIAN_POINT('Ctrl Pts',(-2.63157804800006,15.2,-10.782180844));
#293919=CARTESIAN_POINT('Ctrl Pts',(-2.63157804800006,11.6,-10.782180844));
#293920=CARTESIAN_POINT('Ctrl Pts',(-2.63114586200006,15.2,-10.785393096));
#293921=CARTESIAN_POINT('Ctrl Pts',(-2.63114586200006,11.6,-10.785393096));
#293922=CARTESIAN_POINT('Ctrl Pts',(-2.63071042300006,15.2,-10.788610025));
#293923=CARTESIAN_POINT('Ctrl Pts',(-2.63071042300006,11.6,-10.788610025));
#293924=CARTESIAN_POINT('Ctrl Pts',(-2.63027172600005,15.2,-10.791831622));
#293925=CARTESIAN_POINT('Ctrl Pts',(-2.63027172600005,11.6,-10.791831622));
#293926=CARTESIAN_POINT('Ctrl Pts',(-2.62982976500005,15.2,-10.795057878));
#293927=CARTESIAN_POINT('Ctrl Pts',(-2.62982976500005,11.6,-10.795057878));
#293928=CARTESIAN_POINT('Ctrl Pts',(-2.62938453600006,15.2,-10.798288782));
#293929=CARTESIAN_POINT('Ctrl Pts',(-2.62938453600006,11.6,-10.798288782));
#293930=CARTESIAN_POINT('Ctrl Pts',(-2.62893603000005,15.2,-10.801524326));
#293931=CARTESIAN_POINT('Ctrl Pts',(-2.62893603000005,11.6,-10.801524326));
#293932=CARTESIAN_POINT('Ctrl Pts',(-2.62848424300006,15.2,-10.804764499));
#293933=CARTESIAN_POINT('Ctrl Pts',(-2.62848424300006,11.6,-10.804764499));
#293934=CARTESIAN_POINT('Ctrl Pts',(-2.62802917100006,15.2,-10.808009292));
#293935=CARTESIAN_POINT('Ctrl Pts',(-2.62802917100006,11.6,-10.808009292));
#293936=CARTESIAN_POINT('Ctrl Pts',(-2.62757080600006,15.2,-10.811258697));
#293937=CARTESIAN_POINT('Ctrl Pts',(-2.62757080600006,11.6,-10.811258697));
#293938=CARTESIAN_POINT('Ctrl Pts',(-2.62710914400006,15.2,-10.814512704));
#293939=CARTESIAN_POINT('Ctrl Pts',(-2.62710914400006,11.6,-10.814512704));
#293940=CARTESIAN_POINT('Ctrl Pts',(-2.62664417900006,15.2,-10.817771302));
#293941=CARTESIAN_POINT('Ctrl Pts',(-2.62664417900006,11.6,-10.817771302));
#293942=CARTESIAN_POINT('Ctrl Pts',(-2.62617590600006,15.2,-10.821034484));
#293943=CARTESIAN_POINT('Ctrl Pts',(-2.62617590600006,11.6,-10.821034484));
#293944=CARTESIAN_POINT('Ctrl Pts',(-2.62570431900006,15.2,-10.82430224));
#293945=CARTESIAN_POINT('Ctrl Pts',(-2.62570431900006,11.6,-10.82430224));
#293946=CARTESIAN_POINT('Ctrl Pts',(-2.62522941300006,15.2,-10.82757456));
#293947=CARTESIAN_POINT('Ctrl Pts',(-2.62522941300006,11.6,-10.82757456));
#293948=CARTESIAN_POINT('Ctrl Pts',(-2.62475118200005,15.2,-10.830851435));
#293949=CARTESIAN_POINT('Ctrl Pts',(-2.62475118200005,11.6,-10.830851435));
#293950=CARTESIAN_POINT('Ctrl Pts',(-2.62426962100006,15.2,-10.834132855));
#293951=CARTESIAN_POINT('Ctrl Pts',(-2.62426962100006,11.6,-10.834132855));
#293952=CARTESIAN_POINT('Ctrl Pts',(-2.62378472400006,15.2,-10.837418812));
#293953=CARTESIAN_POINT('Ctrl Pts',(-2.62378472400006,11.6,-10.837418812));
#293954=CARTESIAN_POINT('Ctrl Pts',(-2.62329648700006,15.2,-10.840709295));
#293955=CARTESIAN_POINT('Ctrl Pts',(-2.62329648700006,11.6,-10.840709295));
#293956=CARTESIAN_POINT('Ctrl Pts',(-2.62280490400005,15.2,-10.844004298));
#293957=CARTESIAN_POINT('Ctrl Pts',(-2.62280490400005,11.6,-10.844004298));
#293958=CARTESIAN_POINT('Ctrl Pts',(-2.62230997000006,15.2,-10.847303808));
#293959=CARTESIAN_POINT('Ctrl Pts',(-2.62230997000006,11.6,-10.847303808));
#293960=CARTESIAN_POINT('Ctrl Pts',(-2.62181167800006,15.2,-10.850607819));
#293961=CARTESIAN_POINT('Ctrl Pts',(-2.62181167800006,11.6,-10.850607819));
#293962=CARTESIAN_POINT('Ctrl Pts',(-2.62131002400006,15.2,-10.853916319));
#293963=CARTESIAN_POINT('Ctrl Pts',(-2.62131002400006,11.6,-10.853916319));
#293964=CARTESIAN_POINT('Ctrl Pts',(-2.62080500300006,15.2,-10.857229301));
#293965=CARTESIAN_POINT('Ctrl Pts',(-2.62080500300006,11.6,-10.857229301));
#293966=CARTESIAN_POINT('Ctrl Pts',(-2.62029660900006,15.2,-10.860546754));
#293967=CARTESIAN_POINT('Ctrl Pts',(-2.62029660900006,11.6,-10.860546754));
#293968=CARTESIAN_POINT('Ctrl Pts',(-2.61978483700006,15.2,-10.863868671));
#293969=CARTESIAN_POINT('Ctrl Pts',(-2.61978483700006,11.6,-10.863868671));
#293970=CARTESIAN_POINT('Ctrl Pts',(-2.61926968300005,15.2,-10.86719504));
#293971=CARTESIAN_POINT('Ctrl Pts',(-2.61926968300005,11.6,-10.86719504));
#293972=CARTESIAN_POINT('Ctrl Pts',(-2.61875114000006,15.2,-10.870525854));
#293973=CARTESIAN_POINT('Ctrl Pts',(-2.61875114000006,11.6,-10.870525854));
#293974=CARTESIAN_POINT('Ctrl Pts',(-2.61822920300005,15.2,-10.873861104));
#293975=CARTESIAN_POINT('Ctrl Pts',(-2.61822920300005,11.6,-10.873861104));
#293976=CARTESIAN_POINT('Ctrl Pts',(-2.61770386800006,15.2,-10.877200779));
#293977=CARTESIAN_POINT('Ctrl Pts',(-2.61770386800006,11.6,-10.877200779));
#293978=CARTESIAN_POINT('Ctrl Pts',(-2.61717512900006,15.2,-10.880544872));
#293979=CARTESIAN_POINT('Ctrl Pts',(-2.61717512900006,11.6,-10.880544872));
#293980=CARTESIAN_POINT('Ctrl Pts',(-2.61664298100006,15.2,-10.883893373));
#293981=CARTESIAN_POINT('Ctrl Pts',(-2.61664298100006,11.6,-10.883893373));
#293982=CARTESIAN_POINT('Ctrl Pts',(-2.61610741900005,15.2,-10.887246272));
#293983=CARTESIAN_POINT('Ctrl Pts',(-2.61610741900005,11.6,-10.887246272));
#293984=CARTESIAN_POINT('Ctrl Pts',(-2.61556843800005,15.2,-10.890603561));
#293985=CARTESIAN_POINT('Ctrl Pts',(-2.61556843800005,11.6,-10.890603561));
#293986=CARTESIAN_POINT('Ctrl Pts',(-2.61502603200006,15.2,-10.893965232));
#293987=CARTESIAN_POINT('Ctrl Pts',(-2.61502603200006,11.6,-10.893965232));
#293988=CARTESIAN_POINT('Ctrl Pts',(-2.61448019800006,15.2,-10.897331274));
#293989=CARTESIAN_POINT('Ctrl Pts',(-2.61448019800006,11.6,-10.897331274));
#293990=CARTESIAN_POINT('Ctrl Pts',(-2.61393092800006,15.2,-10.900701679));
#293991=CARTESIAN_POINT('Ctrl Pts',(-2.61393092800006,11.6,-10.900701679));
#293992=CARTESIAN_POINT('Ctrl Pts',(-2.61337822000006,15.2,-10.904076438));
#293993=CARTESIAN_POINT('Ctrl Pts',(-2.61337822000006,11.6,-10.904076438));
#293994=CARTESIAN_POINT('Ctrl Pts',(-2.61282206700006,15.2,-10.907455541));
#293995=CARTESIAN_POINT('Ctrl Pts',(-2.61282206700006,11.6,-10.907455541));
#293996=CARTESIAN_POINT('Ctrl Pts',(-2.61226246400006,15.2,-10.91083898));
#293997=CARTESIAN_POINT('Ctrl Pts',(-2.61226246400006,11.6,-10.91083898));
#293998=CARTESIAN_POINT('Ctrl Pts',(-2.61169940800006,15.2,-10.914226746));
#293999=CARTESIAN_POINT('Ctrl Pts',(-2.61169940800006,11.6,-10.914226746));
#294000=CARTESIAN_POINT('Ctrl Pts',(-2.61113289100006,15.2,-10.91761883));
#294001=CARTESIAN_POINT('Ctrl Pts',(-2.61113289100006,11.6,-10.91761883));
#294002=CARTESIAN_POINT('Ctrl Pts',(-2.61056291100005,15.2,-10.921015223));
#294003=CARTESIAN_POINT('Ctrl Pts',(-2.61056291100005,11.6,-10.921015223));
#294004=CARTESIAN_POINT('Ctrl Pts',(-2.60998946100006,15.2,-10.924415916));
#294005=CARTESIAN_POINT('Ctrl Pts',(-2.60998946100006,11.6,-10.924415916));
#294006=CARTESIAN_POINT('Ctrl Pts',(-2.60941253700006,15.2,-10.9278209));
#294007=CARTESIAN_POINT('Ctrl Pts',(-2.60941253700006,11.6,-10.9278209));
#294008=CARTESIAN_POINT('Ctrl Pts',(-2.60883213400006,15.2,-10.931230167));
#294009=CARTESIAN_POINT('Ctrl Pts',(-2.60883213400006,11.6,-10.931230167));
#294010=CARTESIAN_POINT('Ctrl Pts',(-2.60824824700005,15.2,-10.934643706));
#294011=CARTESIAN_POINT('Ctrl Pts',(-2.60824824700005,11.6,-10.934643706));
#294012=CARTESIAN_POINT('Ctrl Pts',(-2.60766087100006,15.2,-10.93806151));
#294013=CARTESIAN_POINT('Ctrl Pts',(-2.60766087100006,11.6,-10.93806151));
#294014=CARTESIAN_POINT('Ctrl Pts',(-2.60707000100005,15.2,-10.94148357));
#294015=CARTESIAN_POINT('Ctrl Pts',(-2.60707000100005,11.6,-10.94148357));
#294016=CARTESIAN_POINT('Ctrl Pts',(-2.60647563300005,15.2,-10.944909876));
#294017=CARTESIAN_POINT('Ctrl Pts',(-2.60647563300005,11.6,-10.944909876));
#294018=CARTESIAN_POINT('Ctrl Pts',(-2.60587776200006,15.2,-10.948340421));
#294019=CARTESIAN_POINT('Ctrl Pts',(-2.60587776200006,11.6,-10.948340421));
#294020=CARTESIAN_POINT('Ctrl Pts',(-2.60527638100006,15.2,-10.951775194));
#294021=CARTESIAN_POINT('Ctrl Pts',(-2.60527638100006,11.6,-10.951775194));
#294022=CARTESIAN_POINT('Ctrl Pts',(-2.60467148900006,15.2,-10.955214187));
#294023=CARTESIAN_POINT('Ctrl Pts',(-2.60467148900006,11.6,-10.955214187));
#294024=CARTESIAN_POINT('Ctrl Pts',(-2.60406307900006,15.2,-10.958657392));
#294025=CARTESIAN_POINT('Ctrl Pts',(-2.60406307900006,11.6,-10.958657392));
#294026=CARTESIAN_POINT('Ctrl Pts',(-2.60345114600006,15.2,-10.9621048));
#294027=CARTESIAN_POINT('Ctrl Pts',(-2.60345114600006,11.6,-10.9621048));
#294028=CARTESIAN_POINT('Ctrl Pts',(-2.60283568600005,15.2,-10.965556401));
#294029=CARTESIAN_POINT('Ctrl Pts',(-2.60283568600005,11.6,-10.965556401));
#294030=CARTESIAN_POINT('Ctrl Pts',(-2.60221669300006,15.2,-10.969012188));
#294031=CARTESIAN_POINT('Ctrl Pts',(-2.60221669300006,11.6,-10.969012188));
#294032=CARTESIAN_POINT('Ctrl Pts',(-2.60159416500006,15.2,-10.972472151));
#294033=CARTESIAN_POINT('Ctrl Pts',(-2.60159416500006,11.6,-10.972472151));
#294034=CARTESIAN_POINT('Ctrl Pts',(-2.60096809500005,15.2,-10.975936281));
#294035=CARTESIAN_POINT('Ctrl Pts',(-2.60096809500005,11.6,-10.975936281));
#294036=CARTESIAN_POINT('Ctrl Pts',(-2.60033847900006,15.2,-10.979404571));
#294037=CARTESIAN_POINT('Ctrl Pts',(-2.60033847900006,11.6,-10.979404571));
#294038=CARTESIAN_POINT('Ctrl Pts',(-2.59970531300006,15.2,-10.98287701));
#294039=CARTESIAN_POINT('Ctrl Pts',(-2.59970531300006,11.6,-10.98287701));
#294040=CARTESIAN_POINT('Ctrl Pts',(-2.59906859000006,15.2,-10.986353591));
#294041=CARTESIAN_POINT('Ctrl Pts',(-2.59906859000006,11.6,-10.986353591));
#294042=CARTESIAN_POINT('Ctrl Pts',(-2.59842830800005,15.2,-10.989834305));
#294043=CARTESIAN_POINT('Ctrl Pts',(-2.59842830800005,11.6,-10.989834305));
#294044=CARTESIAN_POINT('Ctrl Pts',(-2.59778446200006,15.2,-10.993319143));
#294045=CARTESIAN_POINT('Ctrl Pts',(-2.59778446200006,11.6,-10.993319143));
#294046=CARTESIAN_POINT('Ctrl Pts',(-2.59713704700005,15.2,-10.996808096));
#294047=CARTESIAN_POINT('Ctrl Pts',(-2.59713704700005,11.6,-10.996808096));
#294048=CARTESIAN_POINT('Ctrl Pts',(-2.59648605700006,15.2,-11.000301157));
#294049=CARTESIAN_POINT('Ctrl Pts',(-2.59648605700006,11.6,-11.000301157));
#294050=CARTESIAN_POINT('Ctrl Pts',(-2.59583148900006,15.2,-11.003798315));
#294051=CARTESIAN_POINT('Ctrl Pts',(-2.59583148900006,11.6,-11.003798315));
#294052=CARTESIAN_POINT('Ctrl Pts',(-2.59517333800006,15.2,-11.007299564));
#294053=CARTESIAN_POINT('Ctrl Pts',(-2.59517333800006,11.6,-11.007299564));
#294054=CARTESIAN_POINT('Ctrl Pts',(-2.59451160000005,15.2,-11.010804893));
#294055=CARTESIAN_POINT('Ctrl Pts',(-2.59451160000005,11.6,-11.010804893));
#294056=CARTESIAN_POINT('Ctrl Pts',(-2.59384627000005,15.2,-11.014314294));
#294057=CARTESIAN_POINT('Ctrl Pts',(-2.59384627000005,11.6,-11.014314294));
#294058=CARTESIAN_POINT('Ctrl Pts',(-2.59317734300006,15.2,-11.017827759));
#294059=CARTESIAN_POINT('Ctrl Pts',(-2.59317734300006,11.6,-11.017827759));
#294060=CARTESIAN_POINT('Ctrl Pts',(-2.59250481600006,15.2,-11.021345279));
#294061=CARTESIAN_POINT('Ctrl Pts',(-2.59250481600006,11.6,-11.021345279));
#294062=CARTESIAN_POINT('Ctrl Pts',(-2.59182868400006,15.2,-11.024866846));
#294063=CARTESIAN_POINT('Ctrl Pts',(-2.59182868400006,11.6,-11.024866846));
#294064=CARTESIAN_POINT('Ctrl Pts',(-2.59114894000006,15.2,-11.02839245));
#294065=CARTESIAN_POINT('Ctrl Pts',(-2.59114894000006,11.6,-11.02839245));
#294066=CARTESIAN_POINT('Ctrl Pts',(-2.59046558300006,15.2,-11.031922084));
#294067=CARTESIAN_POINT('Ctrl Pts',(-2.59046558300006,11.6,-11.031922084));
#294068=CARTESIAN_POINT('Ctrl Pts',(-2.58977860700006,15.2,-11.035455739));
#294069=CARTESIAN_POINT('Ctrl Pts',(-2.58977860700006,11.6,-11.035455739));
#294070=CARTESIAN_POINT('Ctrl Pts',(-2.58908800800006,15.2,-11.038993407));
#294071=CARTESIAN_POINT('Ctrl Pts',(-2.58908800800006,11.6,-11.038993407));
#294072=CARTESIAN_POINT('Ctrl Pts',(-2.58839378100005,15.2,-11.042535078));
#294073=CARTESIAN_POINT('Ctrl Pts',(-2.58839378100005,11.6,-11.042535078));
#294074=CARTESIAN_POINT('Ctrl Pts',(-2.58769592300006,15.2,-11.046080744));
#294075=CARTESIAN_POINT('Ctrl Pts',(-2.58769592300006,11.6,-11.046080744));
#294076=CARTESIAN_POINT('Ctrl Pts',(-2.58699442800005,15.2,-11.049630398));
#294077=CARTESIAN_POINT('Ctrl Pts',(-2.58699442800005,11.6,-11.049630398));
#294078=CARTESIAN_POINT('Ctrl Pts',(-2.58628929200006,15.2,-11.05318403));
#294079=CARTESIAN_POINT('Ctrl Pts',(-2.58628929200006,11.6,-11.05318403));
#294080=CARTESIAN_POINT('Ctrl Pts',(-2.58558051100006,15.2,-11.056741631));
#294081=CARTESIAN_POINT('Ctrl Pts',(-2.58558051100006,11.6,-11.056741631));
#294082=CARTESIAN_POINT('Ctrl Pts',(-2.58486808100006,15.2,-11.060303195));
#294083=CARTESIAN_POINT('Ctrl Pts',(-2.58486808100006,11.6,-11.060303195));
#294084=CARTESIAN_POINT('Ctrl Pts',(-2.58415199700006,15.2,-11.063868711));
#294085=CARTESIAN_POINT('Ctrl Pts',(-2.58415199700006,11.6,-11.063868711));
#294086=CARTESIAN_POINT('Ctrl Pts',(-2.58343225500006,15.2,-11.067438171));
#294087=CARTESIAN_POINT('Ctrl Pts',(-2.58343225500006,11.6,-11.067438171));
#294088=CARTESIAN_POINT('Ctrl Pts',(-2.58270885100006,15.2,-11.071011569));
#294089=CARTESIAN_POINT('Ctrl Pts',(-2.58270885100006,11.6,-11.071011569));
#294090=CARTESIAN_POINT('Ctrl Pts',(-2.58198178000006,15.2,-11.074588893));
#294091=CARTESIAN_POINT('Ctrl Pts',(-2.58198178000006,11.6,-11.074588893));
#294092=CARTESIAN_POINT('Ctrl Pts',(-2.58125103800006,15.2,-11.078170137));
#294093=CARTESIAN_POINT('Ctrl Pts',(-2.58125103800006,11.6,-11.078170137));
#294094=CARTESIAN_POINT('Ctrl Pts',(-2.58051662100006,15.2,-11.081755292));
#294095=CARTESIAN_POINT('Ctrl Pts',(-2.58051662100006,11.6,-11.081755292));
#294096=CARTESIAN_POINT('Ctrl Pts',(-2.57977852500006,15.2,-11.08534435));
#294097=CARTESIAN_POINT('Ctrl Pts',(-2.57977852500006,11.6,-11.08534435));
#294098=CARTESIAN_POINT('Ctrl Pts',(-2.57903674600006,15.2,-11.088937302));
#294099=CARTESIAN_POINT('Ctrl Pts',(-2.57903674600006,11.6,-11.088937302));
#294100=CARTESIAN_POINT('Ctrl Pts',(-2.57829127900005,15.2,-11.09253414));
#294101=CARTESIAN_POINT('Ctrl Pts',(-2.57829127900005,11.6,-11.09253414));
#294102=CARTESIAN_POINT('Ctrl Pts',(-2.57754212000005,15.2,-11.096134855));
#294103=CARTESIAN_POINT('Ctrl Pts',(-2.57754212000005,11.6,-11.096134855));
#294104=CARTESIAN_POINT('Ctrl Pts',(-2.57678926400006,15.2,-11.099739441));
#294105=CARTESIAN_POINT('Ctrl Pts',(-2.57678926400006,11.6,-11.099739441));
#294106=CARTESIAN_POINT('Ctrl Pts',(-2.57603270800006,15.2,-11.103347885));
#294107=CARTESIAN_POINT('Ctrl Pts',(-2.57603270800006,11.6,-11.103347885));
#294108=CARTESIAN_POINT('Ctrl Pts',(-2.57527244700006,15.2,-11.106960183));
#294109=CARTESIAN_POINT('Ctrl Pts',(-2.57527244700006,11.6,-11.106960183));
#294110=CARTESIAN_POINT('Ctrl Pts',(-2.57450847900006,15.2,-11.110576324));
#294111=CARTESIAN_POINT('Ctrl Pts',(-2.57450847900006,11.6,-11.110576324));
#294112=CARTESIAN_POINT('Ctrl Pts',(-2.57374079800006,15.2,-11.114196302));
#294113=CARTESIAN_POINT('Ctrl Pts',(-2.57374079800006,11.6,-11.114196302));
#294114=CARTESIAN_POINT('Ctrl Pts',(-2.57296940000006,15.2,-11.117820108));
#294115=CARTESIAN_POINT('Ctrl Pts',(-2.57296940000006,11.6,-11.117820108));
#294116=CARTESIAN_POINT('Ctrl Pts',(-2.57219428000006,15.2,-11.121447733));
#294117=CARTESIAN_POINT('Ctrl Pts',(-2.57219428000006,11.6,-11.121447733));
#294118=CARTESIAN_POINT('Ctrl Pts',(-2.57141543700006,15.2,-11.125079169));
#294119=CARTESIAN_POINT('Ctrl Pts',(-2.57141543700006,11.6,-11.125079169));
#294120=CARTESIAN_POINT('Ctrl Pts',(-2.57063286500005,15.2,-11.128714409));
#294121=CARTESIAN_POINT('Ctrl Pts',(-2.57063286500005,11.6,-11.128714409));
#294122=CARTESIAN_POINT('Ctrl Pts',(-2.56984656000005,15.2,-11.132353444));
#294123=CARTESIAN_POINT('Ctrl Pts',(-2.56984656000005,11.6,-11.132353444));
#294124=CARTESIAN_POINT('Ctrl Pts',(-2.56905651800006,15.2,-11.135996266));
#294125=CARTESIAN_POINT('Ctrl Pts',(-2.56905651800006,11.6,-11.135996266));
#294126=CARTESIAN_POINT('Ctrl Pts',(-2.56826273400006,15.2,-11.139642864));
#294127=CARTESIAN_POINT('Ctrl Pts',(-2.56826273400006,11.6,-11.139642864));
#294128=CARTESIAN_POINT('Ctrl Pts',(-2.56746520400006,15.2,-11.143293232));
#294129=CARTESIAN_POINT('Ctrl Pts',(-2.56746520400006,11.6,-11.143293232));
#294130=CARTESIAN_POINT('Ctrl Pts',(-2.56666392600006,15.2,-11.146947361));
#294131=CARTESIAN_POINT('Ctrl Pts',(-2.56666392600006,11.6,-11.146947361));
#294132=CARTESIAN_POINT('Ctrl Pts',(-2.56585889400006,15.2,-11.150605243));
#294133=CARTESIAN_POINT('Ctrl Pts',(-2.56585889400006,11.6,-11.150605243));
#294134=CARTESIAN_POINT('Ctrl Pts',(-2.56505010400006,15.2,-11.15426687));
#294135=CARTESIAN_POINT('Ctrl Pts',(-2.56505010400006,11.6,-11.15426687));
#294136=CARTESIAN_POINT('Ctrl Pts',(-2.56423755400006,15.2,-11.157932234));
#294137=CARTESIAN_POINT('Ctrl Pts',(-2.56423755400006,11.6,-11.157932234));
#294138=CARTESIAN_POINT('Ctrl Pts',(-2.56342123900006,15.2,-11.161601329));
#294139=CARTESIAN_POINT('Ctrl Pts',(-2.56342123900006,11.6,-11.161601329));
#294140=CARTESIAN_POINT('Ctrl Pts',(-2.56260115700006,15.2,-11.165274147));
#294141=CARTESIAN_POINT('Ctrl Pts',(-2.56260115700006,11.6,-11.165274147));
#294142=CARTESIAN_POINT('Ctrl Pts',(-2.56177730200006,15.2,-11.16895068));
#294143=CARTESIAN_POINT('Ctrl Pts',(-2.56177730200006,11.6,-11.16895068));
#294144=CARTESIAN_POINT('Ctrl Pts',(-2.56094967200006,15.2,-11.172630919));
#294145=CARTESIAN_POINT('Ctrl Pts',(-2.56094967200006,11.6,-11.172630919));
#294146=CARTESIAN_POINT('Ctrl Pts',(-2.56011826200006,15.2,-11.176314856));
#294147=CARTESIAN_POINT('Ctrl Pts',(-2.56011826200006,11.6,-11.176314856));
#294148=CARTESIAN_POINT('Ctrl Pts',(-2.55928306700006,15.2,-11.18000248));
#294149=CARTESIAN_POINT('Ctrl Pts',(-2.55928306700006,11.6,-11.18000248));
#294150=CARTESIAN_POINT('Ctrl Pts',(-2.55844408200006,15.2,-11.183693781));
#294151=CARTESIAN_POINT('Ctrl Pts',(-2.55844408200006,11.6,-11.183693781));
#294152=CARTESIAN_POINT('Ctrl Pts',(-2.55760130200006,15.2,-11.18738875));
#294153=CARTESIAN_POINT('Ctrl Pts',(-2.55760130200006,11.6,-11.18738875));
#294154=CARTESIAN_POINT('Ctrl Pts',(-2.55675472300006,15.2,-11.191087378));
#294155=CARTESIAN_POINT('Ctrl Pts',(-2.55675472300006,11.6,-11.191087378));
#294156=CARTESIAN_POINT('Ctrl Pts',(-2.55590434200006,15.2,-11.194789656));
#294157=CARTESIAN_POINT('Ctrl Pts',(-2.55590434200006,11.6,-11.194789656));
#294158=CARTESIAN_POINT('Ctrl Pts',(-2.55505015600006,15.2,-11.198495579));
#294159=CARTESIAN_POINT('Ctrl Pts',(-2.55505015600006,11.6,-11.198495579));
#294160=CARTESIAN_POINT('Ctrl Pts',(-2.55419216400006,15.2,-11.202205146));
#294161=CARTESIAN_POINT('Ctrl Pts',(-2.55419216400006,11.6,-11.202205146));
#294162=CARTESIAN_POINT('Ctrl Pts',(-2.55333036400006,15.2,-11.205918353));
#294163=CARTESIAN_POINT('Ctrl Pts',(-2.55333036400006,11.6,-11.205918353));
#294164=CARTESIAN_POINT('Ctrl Pts',(-2.55263787800006,15.2,-11.20889183));
#294165=CARTESIAN_POINT('Ctrl Pts',(-2.55263787800006,11.6,-11.20889183));
#294166=CARTESIAN_POINT('Ctrl Pts',(-2.55211680100006,15.2,-11.211123574));
#294167=CARTESIAN_POINT('Ctrl Pts',(-2.55211680100006,11.6,-11.211123574));
#294168=CARTESIAN_POINT('Ctrl Pts',(-2.55176865500006,15.2,-11.212612131));
#294169=CARTESIAN_POINT('Ctrl Pts',(-2.55176865500006,11.6,-11.212612131));
#294170=CARTESIAN_POINT('Ctrl Pts',(-2.55159439100006,15.2,-11.213356592));
#294171=CARTESIAN_POINT('Ctrl Pts',(-2.55159439100006,11.6,-11.213356592));
#294172=CARTESIAN_POINT('Ctrl Pts',(-2.64164356400005,15.2,-10.033062558));
#294173=CARTESIAN_POINT('Ctrl Pts',(-2.64194832280646,15.2,-10.0348230291495));
#294174=CARTESIAN_POINT('Ctrl Pts',(-2.64225752123829,15.2,-10.0366407490542));
#294175=CARTESIAN_POINT('Ctrl Pts',(-2.64257038372412,15.2,-10.0385148613197));
#294176=CARTESIAN_POINT('Ctrl Pts',(-2.642884754991,15.2,-10.0403980115018));
#294177=CARTESIAN_POINT('Ctrl Pts',(-2.64320281628075,15.2,-10.0423381055564));
#294178=CARTESIAN_POINT('Ctrl Pts',(-2.64352378181444,15.2,-10.0443343061848));
#294179=CARTESIAN_POINT('Ctrl Pts',(-2.64384474731898,15.2,-10.046330506632));
#294180=CARTESIAN_POINT('Ctrl Pts',(-2.64416861707023,15.2,-10.0483828179432));
#294181=CARTESIAN_POINT('Ctrl Pts',(-2.64449462947505,15.2,-10.0504904280332));
#294182=CARTESIAN_POINT('Ctrl Pts',(-2.64482064187987,15.2,-10.0525980381233));
#294183=CARTESIAN_POINT('Ctrl Pts',(-2.64514879650543,15.1999999999999,
-10.0547609446918));
#294184=CARTESIAN_POINT('Ctrl Pts',(-2.64547835425984,15.2,-10.0569783620522));
#294185=CARTESIAN_POINT('Ctrl Pts',(-2.64580791204419,15.2,-10.059195779614));
#294186=CARTESIAN_POINT('Ctrl Pts',(-2.64613887655142,15.2,-10.061467706473));
#294187=CARTESIAN_POINT('Ctrl Pts',(-2.64647052756954,15.2,-10.0637933712701));
#294188=CARTESIAN_POINT('Ctrl Pts',(-2.64680217855753,15.2,-10.0661190358559));
#294189=CARTESIAN_POINT('Ctrl Pts',(-2.64713452030244,15.2,-10.0684984401782));
#294190=CARTESIAN_POINT('Ctrl Pts',(-2.64746685620854,15.2,-10.0709308317677));
#294191=CARTESIAN_POINT('Ctrl Pts',(-2.64779919211464,15.2,-10.0733632233572));
#294192=CARTESIAN_POINT('Ctrl Pts',(-2.64813152490233,15.2,-10.0758486046313));
#294193=CARTESIAN_POINT('Ctrl Pts',(-2.64846317797365,15.2,-10.0783862401202));
#294194=CARTESIAN_POINT('Ctrl Pts',(-2.64879483107508,15.2,-10.0809238758395));
#294195=CARTESIAN_POINT('Ctrl Pts',(-2.64912580739311,15.2,-10.0835137670404));
#294196=CARTESIAN_POINT('Ctrl Pts',(-2.64945545332766,15.2,-10.0861551970212));
#294197=CARTESIAN_POINT('Ctrl Pts',(-2.64978509923225,15.2,-10.088796626762));
#294198=CARTESIAN_POINT('Ctrl Pts',(-2.65011341197145,15.2,-10.0914895979888));
#294199=CARTESIAN_POINT('Ctrl Pts',(-2.65043976104284,15.2,-10.0942334086413));
#294200=CARTESIAN_POINT('Ctrl Pts',(-2.65076611011422,15.2,-10.0969772192938));
#294201=CARTESIAN_POINT('Ctrl Pts',(-2.65109049354409,15.2,-10.099771869884));
#294202=CARTESIAN_POINT('Ctrl Pts',(-2.65141229569918,15.2,-10.1026166776118));
#294203=CARTESIAN_POINT('Ctrl Pts',(-2.65173409785426,15.2,-10.1054614853395));
#294204=CARTESIAN_POINT('Ctrl Pts',(-2.65205331640188,15.2,-10.108356448881));
#294205=CARTESIAN_POINT('Ctrl Pts',(-2.65236935747395,15.2,-10.1113009016873));
#294206=CARTESIAN_POINT('Ctrl Pts',(-2.65268539857472,15.2,-10.1142453547611));
#294207=CARTESIAN_POINT('Ctrl Pts',(-2.65299825684187,15.2,-10.117239296673));
#294208=CARTESIAN_POINT('Ctrl Pts',(-2.65330735327523,15.2,-10.1202820709243));
#294209=CARTESIAN_POINT('Ctrl Pts',(-2.6536164496805,15.2,-10.1233248448992));
#294210=CARTESIAN_POINT('Ctrl Pts',(-2.65392178424282,15.2,-10.1264164543317));
#294211=CARTESIAN_POINT('Ctrl Pts',(-2.65422278873326,15.2,-10.1295562562318));
#294212=CARTESIAN_POINT('Ctrl Pts',(-2.6545237932237,15.2,-10.1326960581319));
#294213=CARTESIAN_POINT('Ctrl Pts',(-2.6548204693202,15.2,-10.1358840535347));
#294214=CARTESIAN_POINT('Ctrl Pts',(-2.65511226572659,15.2,-10.1391196154139));
#294215=CARTESIAN_POINT('Ctrl Pts',(-2.65540406215949,15.2,-10.142355177587));
#294216=CARTESIAN_POINT('Ctrl Pts',(-2.65569097776695,15.2,-10.1456383044564));
#294217=CARTESIAN_POINT('Ctrl Pts',(-2.65597247828205,15.2,-10.1489683828899));
#294218=CARTESIAN_POINT('Ctrl Pts',(-2.65625397877158,15.2,-10.152298461021));
#294219=CARTESIAN_POINT('Ctrl Pts',(-2.65653006180852,15.2,-10.1556754927156));
#294220=CARTESIAN_POINT('Ctrl Pts',(-2.65680020829994,15.2,-10.1590988700234));
#294221=CARTESIAN_POINT('Ctrl Pts',(-2.65707035479137,15.2,-10.1625222473311));
#294222=CARTESIAN_POINT('Ctrl Pts',(-2.65733456181423,15.2,-10.1659919742893));
#294223=CARTESIAN_POINT('Ctrl Pts',(-2.65759232347197,15.2,-10.1695074575751));
#294224=CARTESIAN_POINT('Ctrl Pts',(-2.65785008515312,15.2,-10.1730229411802));
#294225=CARTESIAN_POINT('Ctrl Pts',(-2.65810140084023,15.2,-10.1765841834696));
#294226=CARTESIAN_POINT('Ctrl Pts',(-2.65834577378202,15.2,-10.1801906021823));
#294227=CARTESIAN_POINT('Ctrl Pts',(-2.65859014670161,15.2,-10.1837970205673));
#294228=CARTESIAN_POINT('Ctrl Pts',(-2.65882758030843,15.2,-10.1874486162425));
#294229=CARTESIAN_POINT('Ctrl Pts',(-2.65905758730007,15.2,-10.1911448195249));
#294230=CARTESIAN_POINT('Ctrl Pts',(-2.65928759429171,15.2,-10.1948410228073));
#294231=CARTESIAN_POINT('Ctrl Pts',(-2.65951017928423,15.2,-10.1985818334432));
#294232=CARTESIAN_POINT('Ctrl Pts',(-2.65972486820428,15.2,-10.2023666939089));
#294233=CARTESIAN_POINT('Ctrl Pts',(-2.65993955714384,15.2,-10.2061515547184));
#294234=CARTESIAN_POINT('Ctrl Pts',(-2.66014635065311,15.2,-10.2099804649914));
#294235=CARTESIAN_POINT('Ctrl Pts',(-2.66034479258003,15.2,-10.2138528737054));
#294236=CARTESIAN_POINT('Ctrl Pts',(-2.66054323448892,15.2,-10.2177252820677));
#294237=CARTESIAN_POINT('Ctrl Pts',(-2.66073332248927,15.2,-10.2216411908608));
#294238=CARTESIAN_POINT('Ctrl Pts',(-2.66091461048349,15.2,-10.2256000592351));
#294239=CARTESIAN_POINT('Ctrl Pts',(-2.66109589847771,15.2,-10.2295589276093));
#294240=CARTESIAN_POINT('Ctrl Pts',(-2.661268386155,15.2,-10.2335607571951));
#294241=CARTESIAN_POINT('Ctrl Pts',(-2.6614316372328,15.2,-10.2376050155464));
#294242=CARTESIAN_POINT('Ctrl Pts',(-2.66156767980258,15.2,-10.2409752309615));
#294243=CARTESIAN_POINT('Ctrl Pts',(-2.66169730820831,15.2,-10.2443749107774));
#294244=CARTESIAN_POINT('Ctrl Pts',(-2.66182027570866,15.2,-10.2478037545259));
#294245=CARTESIAN_POINT('Ctrl Pts',(-2.661943243209,15.2,-10.2512325982743));
#294246=CARTESIAN_POINT('Ctrl Pts',(-2.6620595504495,15.2,-10.2546906051323));
#294247=CARTESIAN_POINT('Ctrl Pts',(-2.66216895399168,15.2,-10.258177475773));
#294248=CARTESIAN_POINT('Ctrl Pts',(-2.66227835753386,15.2,-10.2616643464138));
#294249=CARTESIAN_POINT('Ctrl Pts',(-2.66238085976118,15.2,-10.2651800830166));
#294250=CARTESIAN_POINT('Ctrl Pts',(-2.66247622073341,15.2,-10.2687243894749));
#294251=CARTESIAN_POINT('Ctrl Pts',(-2.66257158170563,15.2,-10.2722686959333));
#294252=CARTESIAN_POINT('Ctrl Pts',(-2.66265980250532,15.2,-10.2758415734521));
#294253=CARTESIAN_POINT('Ctrl Pts',(-2.66274065174178,15.2,-10.2794427307602));
#294254=CARTESIAN_POINT('Ctrl Pts',(-2.66282150097824,15.2,-10.2830438880684));
#294255=CARTESIAN_POINT('Ctrl Pts',(-2.66289497861584,15.2,-10.2866733273045));
#294256=CARTESIAN_POINT('Ctrl Pts',(-2.662960854796,15.2,-10.2903307587643));
#294257=CARTESIAN_POINT('Ctrl Pts',(-2.66302673097616,15.2,-10.2939881902241));
#294258=CARTESIAN_POINT('Ctrl Pts',(-2.6630850084204,15.2,-10.2976736171804));
#294259=CARTESIAN_POINT('Ctrl Pts',(-2.66313546196166,15.2,-10.301386754543));
#294260=CARTESIAN_POINT('Ctrl Pts',(-2.66318591550292,15.2,-10.3050998919055));
#294261=CARTESIAN_POINT('Ctrl Pts',(-2.66322854556956,15.2,-10.3088407394751));
#294262=CARTESIAN_POINT('Ctrl Pts',(-2.66326313327906,15.2,-10.3126090202208));
#294263=CARTESIAN_POINT('Ctrl Pts',(-2.66329772098856,15.2,-10.3163773009665));
#294264=CARTESIAN_POINT('Ctrl Pts',(-2.66332426743092,15.2,-10.3201730127978));
#294265=CARTESIAN_POINT('Ctrl Pts',(-2.66334255527747,15.2,-10.3239958817583));
#294266=CARTESIAN_POINT('Ctrl Pts',(-2.66336084312401,15.2,-10.3278187507189));
#294267=CARTESIAN_POINT('Ctrl Pts',(-2.66337087492875,15.2,-10.3316687747715));
#294268=CARTESIAN_POINT('Ctrl Pts',(-2.66337243777528,15.2,-10.3355456837321));
#294269=CARTESIAN_POINT('Ctrl Pts',(-2.66337400062164,15.2,-10.33942259227));
#294270=CARTESIAN_POINT('Ctrl Pts',(-2.66336709709971,15.2,-10.3433263838442));
#294271=CARTESIAN_POINT('Ctrl Pts',(-2.66335151751878,15.2,-10.3472567914692));
#294272=CARTESIAN_POINT('Ctrl Pts',(-2.66333282201861,15.2,-10.3519732813903));
#294273=CARTESIAN_POINT('Ctrl Pts',(-2.66330163719225,15.2,-10.3567280939318));
#294274=CARTESIAN_POINT('Ctrl Pts',(-2.66325760877262,15.2,-10.361520775028));
#294275=CARTESIAN_POINT('Ctrl Pts',(-2.66322091842494,15.2,-10.3655146757238));
#294276=CARTESIAN_POINT('Ctrl Pts',(-2.66317531145247,15.2,-10.3695348726356));
#294277=CARTESIAN_POINT('Ctrl Pts',(-2.66312058922978,15.2,-10.3735811027064));
#294278=CARTESIAN_POINT('Ctrl Pts',(-2.66306586700708,15.2,-10.3776273327772));
#294279=CARTESIAN_POINT('Ctrl Pts',(-2.66300202853475,15.2,-10.381699597897));
#294280=CARTESIAN_POINT('Ctrl Pts',(-2.66292888047489,15.2,-10.3857976372008));
#294281=CARTESIAN_POINT('Ctrl Pts',(-2.66285573241503,15.2,-10.3898956765045));
#294282=CARTESIAN_POINT('Ctrl Pts',(-2.66277327411105,15.2,-10.3940194903017));
#294283=CARTESIAN_POINT('Ctrl Pts',(-2.66268131376305,15.2,-10.3981688235677));
#294284=CARTESIAN_POINT('Ctrl Pts',(-2.66260774549067,15.2,-10.4014882899091));
#294285=CARTESIAN_POINT('Ctrl Pts',(-2.66252809754961,15.2,-10.404824088165));
#294286=CARTESIAN_POINT('Ctrl Pts',(-2.66244227255704,15.2,-10.4081760885011));
#294287=CARTESIAN_POINT('Ctrl Pts',(-2.66235644755276,15.2,-10.4115280892938));
#294288=CARTESIAN_POINT('Ctrl Pts',(-2.6622644454466,15.2,-10.4148962919556));
#294289=CARTESIAN_POINT('Ctrl Pts',(-2.66216617176912,15.2,-10.4182805676994));
#294290=CARTESIAN_POINT('Ctrl Pts',(-2.66206789810503,15.2,-10.4216648429821));
#294291=CARTESIAN_POINT('Ctrl Pts',(-2.66196335286905,15.2,-10.4250651920484));
#294292=CARTESIAN_POINT('Ctrl Pts',(-2.66185244326742,15.2,-10.4284814877125));
#294293=CARTESIAN_POINT('Ctrl Pts',(-2.66174153365068,15.2,-10.4318977838421));
#294294=CARTESIAN_POINT('Ctrl Pts',(-2.66162425824429,15.2,-10.4353300249986));
#294295=CARTESIAN_POINT('Ctrl Pts',(-2.66150052718157,15.2,-10.4387780852986));
#294296=CARTESIAN_POINT('Ctrl Pts',(-2.6613458633616,15.2,-10.4430881604388));
#294297=CARTESIAN_POINT('Ctrl Pts',(-2.66118111038363,15.2,-10.4474229541032));
#294298=CARTESIAN_POINT('Ctrl Pts',(-2.66100609176306,15.2,-10.4517822209894));
#294299=CARTESIAN_POINT('Ctrl Pts',(-2.66086607687805,15.2,-10.4552696342132));
#294300=CARTESIAN_POINT('Ctrl Pts',(-2.66071949119958,15.2,-10.4587727095928));
#294301=CARTESIAN_POINT('Ctrl Pts',(-2.66056624754588,15.2,-10.4622913234708));
#294302=CARTESIAN_POINT('Ctrl Pts',(-2.66041300387129,15.2,-10.4658099378282));
#294303=CARTESIAN_POINT('Ctrl Pts',(-2.6602531008348,15.2,-10.4693440916791));
#294304=CARTESIAN_POINT('Ctrl Pts',(-2.66008645126973,15.2,-10.4728936605403));
#294305=CARTESIAN_POINT('Ctrl Pts',(-2.65991980172736,15.2,-10.4764432289178));
#294306=CARTESIAN_POINT('Ctrl Pts',(-2.65974640600598,15.2,-10.4800082136206));
#294307=CARTESIAN_POINT('Ctrl Pts',(-2.65956617706786,15.2,-10.4835884910055));
#294308=CARTESIAN_POINT('Ctrl Pts',(-2.65938594810519,15.2,-10.4871687688782));
#294309=CARTESIAN_POINT('Ctrl Pts',(-2.65919888488685,15.2,-10.4907643412586));
#294310=CARTESIAN_POINT('Ctrl Pts',(-2.65900490404249,15.2,-10.4943750850119));
#294311=CARTESIAN_POINT('Ctrl Pts',(-2.65881092322457,15.2,-10.4979858282733));
#294312=CARTESIAN_POINT('Ctrl Pts',(-2.65861002469136,15.2,-10.5016117448372));
#294313=CARTESIAN_POINT('Ctrl Pts',(-2.6584021225424,15.2,-10.5052527138713));
#294314=CARTESIAN_POINT('Ctrl Pts',(-2.65819422036513,15.2,-10.5088936834015));
#294315=CARTESIAN_POINT('Ctrl Pts',(-2.65797931725473,15.2,-10.5125497050079));
#294316=CARTESIAN_POINT('Ctrl Pts',(-2.6577573277416,15.2,-10.5162206600025));
#294317=CARTESIAN_POINT('Ctrl Pts',(-2.65753533825871,15.2,-10.5198916144969));
#294318=CARTESIAN_POINT('Ctrl Pts',(-2.65730626374366,15.2,-10.5235775024712));
#294319=CARTESIAN_POINT('Ctrl Pts',(-2.65707002226371,15.2,-10.5272782056116));
#294320=CARTESIAN_POINT('Ctrl Pts',(-2.65683378075156,15.2,-10.5309789092562));
#294321=CARTESIAN_POINT('Ctrl Pts',(-2.65659037236097,15.2,-10.5346944278967));
#294322=CARTESIAN_POINT('Ctrl Pts',(-2.65633971629175,15.2,-10.5384246447666));
#294323=CARTESIAN_POINT('Ctrl Pts',(-2.65608906022254,15.2,-10.5421548616366));
#294324=CARTESIAN_POINT('Ctrl Pts',(-2.65583115793581,15.2,-10.5458997760694));
#294325=CARTESIAN_POINT('Ctrl Pts',(-2.65556592719838,15.2,-10.5496592718313));
#294326=CARTESIAN_POINT('Ctrl Pts',(-2.65530069649709,15.2,-10.553418767081));
#294327=CARTESIAN_POINT('Ctrl Pts',(-2.65502813934808,15.2,-10.5571928445983));
#294328=CARTESIAN_POINT('Ctrl Pts',(-2.65474817775861,15.2,-10.5609813878057));
#294329=CARTESIAN_POINT('Ctrl Pts',(-2.65446821613099,15.2,-10.5647699315293));
#294330=CARTESIAN_POINT('Ctrl Pts',(-2.65418084869649,15.2,-10.5685729405813));
#294331=CARTESIAN_POINT('Ctrl Pts',(-2.65388599923521,15.2,-10.5723903021241));
#294332=CARTESIAN_POINT('Ctrl Pts',(-2.6535911498141,15.2,-10.5762076631468));
#294333=CARTESIAN_POINT('Ctrl Pts',(-2.65328881799674,15.2,-10.5800393753649));
#294334=CARTESIAN_POINT('Ctrl Pts',(-2.65297892730035,15.2,-10.5838853246607));
#294335=CARTESIAN_POINT('Ctrl Pts',(-2.65266903656173,15.2,-10.5877312744805));
#294336=CARTESIAN_POINT('Ctrl Pts',(-2.65235158764583,15.2,-10.5915914635646));
#294337=CARTESIAN_POINT('Ctrl Pts',(-2.65202650544454,15.2,-10.5954657768039));
#294338=CARTESIAN_POINT('Ctrl Pts',(-2.65170142328754,15.2,-10.5993400895153));
#294339=CARTESIAN_POINT('Ctrl Pts',(-2.65136870715507,15.2,-10.6032285265288));
#294340=CARTESIAN_POINT('Ctrl Pts',(-2.65102828429451,15.2,-10.6071309764311));
#294341=CARTESIAN_POINT('Ctrl Pts',(-2.6505176499341,15.2,-10.612984652082));
#294342=CARTESIAN_POINT('Ctrl Pts',(-2.64998967146322,15.2,-10.6188698572203));
#294343=CARTESIAN_POINT('Ctrl Pts',(-2.64944410718228,15.2,-10.6247862148782));
#294344=CARTESIAN_POINT('Ctrl Pts',(-2.64908039771122,15.2,-10.6287304527794));
#294345=CARTESIAN_POINT('Ctrl Pts',(-2.64870887096825,15.2,-10.6326885385512));
#294346=CARTESIAN_POINT('Ctrl Pts',(-2.64832945627534,15.2,-10.6366603585223));
#294347=CARTESIAN_POINT('Ctrl Pts',(-2.64795004153075,15.2,-10.6406321790345));
#294348=CARTESIAN_POINT('Ctrl Pts',(-2.64756273816892,15.2,-10.6446177358234));
#294349=CARTESIAN_POINT('Ctrl Pts',(-2.64716747670212,15.2,-10.6486169201538));
#294350=CARTESIAN_POINT('Ctrl Pts',(-2.64677221528918,15.2,-10.6526161039394));
#294351=CARTESIAN_POINT('Ctrl Pts',(-2.64636899514949,15.2,-10.6566289141982));
#294352=CARTESIAN_POINT('Ctrl Pts',(-2.64595774651696,15.2,-10.6606552421459));
#294353=CARTESIAN_POINT('Ctrl Pts',(-2.64534087348413,15.2,-10.6666947348904));
#294354=CARTESIAN_POINT('Ctrl Pts',(-2.64470593657406,15.2,-10.6727646445387));
#294355=CARTESIAN_POINT('Ctrl Pts',(-2.64405270545388,15.2,-10.6788646071232));
#294356=CARTESIAN_POINT('Ctrl Pts',(-2.64361721809977,15.2,-10.6829312482921));
#294357=CARTESIAN_POINT('Ctrl Pts',(-2.64317360006826,15.2,-10.6870112447855));
#294358=CARTESIAN_POINT('Ctrl Pts',(-2.64272178349206,15.2,-10.6911044932472));
#294359=CARTESIAN_POINT('Ctrl Pts',(-2.6422699668543,15.2,-10.6951977422666));
#294360=CARTESIAN_POINT('Ctrl Pts',(-2.64180995286655,15.2,-10.6993042405921));
#294361=CARTESIAN_POINT('Ctrl Pts',(-2.64134167417352,15.2,-10.7034238837069));
#294362=CARTESIAN_POINT('Ctrl Pts',(-2.64087339554429,15.2,-10.7075435262603));
#294363=CARTESIAN_POINT('Ctrl Pts',(-2.6403968519578,15.2,-10.7116763128815));
#294364=CARTESIAN_POINT('Ctrl Pts',(-2.63991197983132,15.2,-10.7158221381528));
#294365=CARTESIAN_POINT('Ctrl Pts',(-2.63942710763877,15.2,-10.719967963989));
#294366=CARTESIAN_POINT('Ctrl Pts',(-2.63893390337205,15.2,-10.7241268293463));
#294367=CARTESIAN_POINT('Ctrl Pts',(-2.63843230715226,15.2,-10.7282986293387));
#294368=CARTESIAN_POINT('Ctrl Pts',(-2.63780531191169,15.2,-10.7335133790451));
#294369=CARTESIAN_POINT('Ctrl Pts',(-2.63716519753237,15.2,-10.7387483387635));
#294370=CARTESIAN_POINT('Ctrl Pts',(-2.63651184565629,15.2,-10.7440033049456));
#294371=CARTESIAN_POINT('Ctrl Pts',(-2.63598916419815,15.2,-10.7482072775477));
#294372=CARTESIAN_POINT('Ctrl Pts',(-2.63545800868556,15.2,-10.7524240556342));
#294373=CARTESIAN_POINT('Ctrl Pts',(-2.63491831678579,15.2,-10.7566535349543));
#294374=CARTESIAN_POINT('Ctrl Pts',(-2.63437862481249,15.2,-10.7608830148507));
#294375=CARTESIAN_POINT('Ctrl Pts',(-2.63383039602538,15.2,-10.765125196083));
#294376=CARTESIAN_POINT('Ctrl Pts',(-2.63327356991091,15.2,-10.7693799774174));
#294377=CARTESIAN_POINT('Ctrl Pts',(-2.63271674387231,15.2,-10.7736347581721));
#294378=CARTESIAN_POINT('Ctrl Pts',(-2.63215131934944,15.2,-10.7779021378981));
#294379=CARTESIAN_POINT('Ctrl Pts',(-2.63157723606361,15.2,-10.7821820151585));
#294380=CARTESIAN_POINT('Ctrl Pts',(-2.63100315269955,15.2,-10.7864618930021));
#294381=CARTESIAN_POINT('Ctrl Pts',(-2.63042040866501,15.2,-10.7907542678638));
#294382=CARTESIAN_POINT('Ctrl Pts',(-2.62982894790999,15.2,-10.795059040377));
#294383=CARTESIAN_POINT('Ctrl Pts',(-2.6290896220065,15.2,-10.8004400057252));
#294384=CARTESIAN_POINT('Ctrl Pts',(-2.62833667154474,15.2,-10.8058403393071));
#294385=CARTESIAN_POINT('Ctrl Pts',(-2.62756998164437,15.2,-10.8112598481208));
#294386=CARTESIAN_POINT('Ctrl Pts',(-2.62695662977422,15.2,-10.8155954548174));
#294387=CARTESIAN_POINT('Ctrl Pts',(-2.62633448518554,15.2,-10.8199433313981));
#294388=CARTESIAN_POINT('Ctrl Pts',(-2.62570348929326,15.2,-10.824303380652));
#294389=CARTESIAN_POINT('Ctrl Pts',(-2.625072493315,15.2,-10.8286634305));
#294390=CARTESIAN_POINT('Ctrl Pts',(-2.6244326455218,15.2,-10.8330356512715));
#294391=CARTESIAN_POINT('Ctrl Pts',(-2.6237838889303,15.2,-10.8374199439002));
#294392=CARTESIAN_POINT('Ctrl Pts',(-2.62297294323513,15.2,-10.8429003093873));
#294393=CARTESIAN_POINT('Ctrl Pts',(-2.62214807878443,15.2,-10.8483995394136));
#294394=CARTESIAN_POINT('Ctrl Pts',(-2.62130918214433,15.2,-10.8539174401072));
#294395=CARTESIAN_POINT('Ctrl Pts',(-2.62080584417855,15.2,-10.8572281804031));
#294396=CARTESIAN_POINT('Ctrl Pts',(-2.62029745485916,15.2,-10.8605456423159));
#294397=CARTESIAN_POINT('Ctrl Pts',(-2.61978399141904,15.2,-10.8638697844041));
#294398=CARTESIAN_POINT('Ctrl Pts',(-2.61927052797892,15.2,-10.8671939264922));
#294399=CARTESIAN_POINT('Ctrl Pts',(-2.61875198988107,15.2,-10.8705247486546));
#294400=CARTESIAN_POINT('Ctrl Pts',(-2.61822835348343,15.2,-10.8738622102833));
#294401=CARTESIAN_POINT('Ctrl Pts',(-2.61753017155649,15.2,-10.8783121595258));
#294402=CARTESIAN_POINT('Ctrl Pts',(-2.61682292677571,15.2,-10.8827739122086));
#294403=CARTESIAN_POINT('Ctrl Pts',(-2.61610656412463,15.2,-10.8872473702314));
#294404=CARTESIAN_POINT('Ctrl Pts',(-2.61556929218512,15.2,-10.8906024634437));
#294405=CARTESIAN_POINT('Ctrl Pts',(-2.61502689136883,15.2,-10.893964142555));
#294406=CARTESIAN_POINT('Ctrl Pts',(-2.6144793389441,15.2,-10.8973323653934));
#294407=CARTESIAN_POINT('Ctrl Pts',(-2.61393178651938,15.2,-10.9007005882317));
#294408=CARTESIAN_POINT('Ctrl Pts',(-2.61337908276938,15.2,-10.9040753551909));
#294409=CARTESIAN_POINT('Ctrl Pts',(-2.61282120445586,15.2,-10.9074566253603));
#294410=CARTESIAN_POINT('Ctrl Pts',(-2.61226332614235,15.2,-10.9108378955297));
#294411=CARTESIAN_POINT('Ctrl Pts',(-2.61170027406278,15.2,-10.9142256696233));
#294412=CARTESIAN_POINT('Ctrl Pts',(-2.61113202520843,15.2,-10.91761990725));
#294413=CARTESIAN_POINT('Ctrl Pts',(-2.61037436000046,15.2,-10.92214555783));
#294414=CARTESIAN_POINT('Ctrl Pts',(-2.60960745680532,15.2,-10.9266826991946));
#294415=CARTESIAN_POINT('Ctrl Pts',(-2.60883126287318,15.2,-10.931231235777));
#294416=CARTESIAN_POINT('Ctrl Pts',(-2.60824911747695,15.2,-10.9346426379039));
#294417=CARTESIAN_POINT('Ctrl Pts',(-2.60766174576073,15.2,-10.9380604498485));
#294418=CARTESIAN_POINT('Ctrl Pts',(-2.60706912637705,15.2,-10.9414846321875));
#294419=CARTESIAN_POINT('Ctrl Pts',(-2.60647650699337,15.2,-10.9449088145266));
#294420=CARTESIAN_POINT('Ctrl Pts',(-2.60587863994614,15.2,-10.9483393671657));
#294421=CARTESIAN_POINT('Ctrl Pts',(-2.60527550313426,15.2,-10.9517762493747));
#294422=CARTESIAN_POINT('Ctrl Pts',(-2.60467236632238,15.2,-10.9552131315837));
#294423=CARTESIAN_POINT('Ctrl Pts',(-2.6040639611278,15.2,-10.9586563446086));
#294424=CARTESIAN_POINT('Ctrl Pts',(-2.60345026423343,15.2,-10.962105848275));
#294425=CARTESIAN_POINT('Ctrl Pts',(-2.60283656733906,15.2,-10.9655553519413));
#294426=CARTESIAN_POINT('Ctrl Pts',(-2.60221757902824,15.2,-10.9690111466824));
#294427=CARTESIAN_POINT('Ctrl Pts',(-2.60159327959305,15.2,-10.9724731923894));
#294428=CARTESIAN_POINT('Ctrl Pts',(-2.60096898015786,15.2,-10.9759352380964));
#294429=CARTESIAN_POINT('Ctrl Pts',(-2.60033936879759,15.2,-10.9794035354312));
#294430=CARTESIAN_POINT('Ctrl Pts',(-2.59970442391455,15.2,-10.9828780448111));
#294431=CARTESIAN_POINT('Ctrl Pts',(-2.59906947903152,15.2,-10.9863525541911));
#294432=CARTESIAN_POINT('Ctrl Pts',(-2.59842920081665,15.2,-10.9898332763007));
#294433=CARTESIAN_POINT('Ctrl Pts',(-2.5977835698825,15.2,-10.9933201710065));
#294434=CARTESIAN_POINT('Ctrl Pts',(-2.59713793883107,15.2,-10.9968070663458));
#294435=CARTESIAN_POINT('Ctrl Pts',(-2.59648695308646,15.2,-11.0003001351701));
#294436=CARTESIAN_POINT('Ctrl Pts',(-2.59583059311534,15.2,-11.0037993384711));
#294437=CARTESIAN_POINT('Ctrl Pts',(-2.5947366599891,15.2,-11.0096313431253));
#294438=CARTESIAN_POINT('Ctrl Pts',(-2.59362779792098,15.2,-11.0154803869159));
#294439=CARTESIAN_POINT('Ctrl Pts',(-2.59250391458642,15.2,-11.0213462915006));
#294440=CARTESIAN_POINT('Ctrl Pts',(-2.59182958461018,15.2,-11.0248658341235));
#294441=CARTESIAN_POINT('Ctrl Pts',(-2.59114984508423,15.2,-11.0283914459795));
#294442=CARTESIAN_POINT('Ctrl Pts',(-2.59046467819199,15.2,-11.0319230896434));
#294443=CARTESIAN_POINT('Ctrl Pts',(-2.58977951129974,15.2,-11.0354547333072));
#294444=CARTESIAN_POINT('Ctrl Pts',(-2.58908891607736,15.2,-11.0389924089991));
#294445=CARTESIAN_POINT('Ctrl Pts',(-2.58839287322446,15.2,-11.0425360767615));
#294446=CARTESIAN_POINT('Ctrl Pts',(-2.58769683037156,15.2,-11.0460797445239));
#294447=CARTESIAN_POINT('Ctrl Pts',(-2.58699533956157,15.2,-11.0496294065098));
#294448=CARTESIAN_POINT('Ctrl Pts',(-2.58628838075073,15.2,-11.0531850222717));
#294449=CARTESIAN_POINT('Ctrl Pts',(-2.5851101160232,15.2,-11.059111048757));
#294450=CARTESIAN_POINT('Ctrl Pts',(-2.58391666405009,15.2,-11.0650536168));
#294451=CARTESIAN_POINT('Ctrl Pts',(-2.58270793425843,15.2,-11.07101255055));
#294452=CARTESIAN_POINT('Ctrl Pts',(-2.5817409503724,15.2,-11.0757796978098));
#294453=CARTESIAN_POINT('Ctrl Pts',(-2.58076418796855,15.2,-11.0805573183069));
#294454=CARTESIAN_POINT('Ctrl Pts',(-2.57977760408045,15.2,-11.0853453242911));
#294455=CARTESIAN_POINT('Ctrl Pts',(-2.57903766623159,15.2,-11.0889363284531));
#294456=CARTESIAN_POINT('Ctrl Pts',(-2.57829220346561,15.2,-11.0925331736306));
#294457=CARTESIAN_POINT('Ctrl Pts',(-2.5775411956214,15.2,-11.0961358233887));
#294458=CARTESIAN_POINT('Ctrl Pts',(-2.5767901877772,15.2,-11.0997384731468));
#294459=CARTESIAN_POINT('Ctrl Pts',(-2.57603363493972,15.2,-11.1033469255248));
#294460=CARTESIAN_POINT('Ctrl Pts',(-2.5752715201336,15.2,-11.1069611441857));
#294461=CARTESIAN_POINT('Ctrl Pts',(-2.57450940532747,15.2,-11.1105753628465));
#294462=CARTESIAN_POINT('Ctrl Pts',(-2.57374172875534,15.2,-11.1141953480984));
#294463=CARTESIAN_POINT('Ctrl Pts',(-2.57296846953343,15.2,-11.1178210627583));
#294464=CARTESIAN_POINT('Ctrl Pts',(-2.57219521031153,15.2,-11.1214467774182));
#294465=CARTESIAN_POINT('Ctrl Pts',(-2.57141637063985,15.2,-11.1250782207029));
#294466=CARTESIAN_POINT('Ctrl Pts',(-2.5706319318355,15.2,-11.128715357362));
#294467=CARTESIAN_POINT('Ctrl Pts',(-2.56984749303116,15.2,-11.132352494021));
#294468=CARTESIAN_POINT('Ctrl Pts',(-2.56905745493083,15.2,-11.1359953233451));
#294469=CARTESIAN_POINT('Ctrl Pts',(-2.56826179767065,15.2,-11.1396438057691));
#294470=CARTESIAN_POINT('Ctrl Pts',(-2.56720092122736,15.2,-11.1445084494431));
#294471=CARTESIAN_POINT('Ctrl Pts',(-2.56613005766842,15.2,-11.1493831445103));
#294472=CARTESIAN_POINT('Ctrl Pts',(-2.56504916388664,15.2,-11.1542678046661));
#294473=CARTESIAN_POINT('Ctrl Pts',(-2.56423849362394,15.2,-11.1579312994501));
#294474=CARTESIAN_POINT('Ctrl Pts',(-2.5634221825869,15.2,-11.1616004010835));
#294475=CARTESIAN_POINT('Ctrl Pts',(-2.56260021378343,15.2,-11.1652750757416));
#294476=CARTESIAN_POINT('Ctrl Pts',(-2.56177824497996,15.2,-11.1689497503998));
#294477=CARTESIAN_POINT('Ctrl Pts',(-2.56095061872672,15.2,-11.172629997866));
#294478=CARTESIAN_POINT('Ctrl Pts',(-2.56011731584083,15.2,-11.1763157773567));
#294479=CARTESIAN_POINT('Ctrl Pts',(-2.55928401295493,15.2,-11.1800015568473));
#294480=CARTESIAN_POINT('Ctrl Pts',(-2.55844503222431,15.2,-11.183692866235));
#294481=CARTESIAN_POINT('Ctrl Pts',(-2.5576003524218,15.2,-11.1873896640348));
#294482=CARTESIAN_POINT('Ctrl Pts',(-2.55675567261928,15.2,-11.1910864618345));
#294483=CARTESIAN_POINT('Ctrl Pts',(-2.5559052937715,15.2,-11.1947887445105));
#294484=CARTESIAN_POINT('Ctrl Pts',(-2.55504920467839,15.2,-11.1984964891667));
#294485=CARTESIAN_POINT('Ctrl Pts',(-2.55390775245054,15.2,-11.2034401491574));
#294486=CARTESIAN_POINT('Ctrl Pts',(-2.55275615131663,15.2,-11.2083935173142));
#294487=CARTESIAN_POINT('Ctrl Pts',(-2.55159439100006,15.2,-11.213356592));
#294488=CARTESIAN_POINT('Ctrl Pts',(-2.64164356400005,12.2,-10.033062558));
#294489=CARTESIAN_POINT('Ctrl Pts',(-2.64194832280646,12.2,-10.0348230291495));
#294490=CARTESIAN_POINT('Ctrl Pts',(-2.64225752123829,12.2,-10.0366407490542));
#294491=CARTESIAN_POINT('Ctrl Pts',(-2.64257038372412,12.2,-10.0385148613197));
#294492=CARTESIAN_POINT('Ctrl Pts',(-2.642884754991,12.2,-10.0403980115018));
#294493=CARTESIAN_POINT('Ctrl Pts',(-2.64320281628075,12.2,-10.0423381055564));
#294494=CARTESIAN_POINT('Ctrl Pts',(-2.64352378181444,12.2,-10.0443343061848));
#294495=CARTESIAN_POINT('Ctrl Pts',(-2.64384474731898,12.2,-10.046330506632));
#294496=CARTESIAN_POINT('Ctrl Pts',(-2.64416861707023,12.2,-10.0483828179432));
#294497=CARTESIAN_POINT('Ctrl Pts',(-2.64449462947505,12.2,-10.0504904280332));
#294498=CARTESIAN_POINT('Ctrl Pts',(-2.64482064187987,12.2,-10.0525980381233));
#294499=CARTESIAN_POINT('Ctrl Pts',(-2.64514879650543,12.2,-10.0547609446918));
#294500=CARTESIAN_POINT('Ctrl Pts',(-2.64547835425984,12.2,-10.0569783620522));
#294501=CARTESIAN_POINT('Ctrl Pts',(-2.64580791204419,12.2,-10.059195779614));
#294502=CARTESIAN_POINT('Ctrl Pts',(-2.64613887655142,12.2,-10.061467706473));
#294503=CARTESIAN_POINT('Ctrl Pts',(-2.64647052756954,12.2,-10.0637933712701));
#294504=CARTESIAN_POINT('Ctrl Pts',(-2.64680217855753,12.2,-10.0661190358559));
#294505=CARTESIAN_POINT('Ctrl Pts',(-2.64713452030244,12.2,-10.0684984401782));
#294506=CARTESIAN_POINT('Ctrl Pts',(-2.64746685620854,12.2,-10.0709308317677));
#294507=CARTESIAN_POINT('Ctrl Pts',(-2.64779919211464,12.2,-10.0733632233572));
#294508=CARTESIAN_POINT('Ctrl Pts',(-2.64813152490233,12.2,-10.0758486046313));
#294509=CARTESIAN_POINT('Ctrl Pts',(-2.64846317797365,12.2,-10.0783862401202));
#294510=CARTESIAN_POINT('Ctrl Pts',(-2.64879483107508,12.2,-10.0809238758395));
#294511=CARTESIAN_POINT('Ctrl Pts',(-2.64912580739311,12.2,-10.0835137670404));
#294512=CARTESIAN_POINT('Ctrl Pts',(-2.64945545332766,12.2,-10.0861551970212));
#294513=CARTESIAN_POINT('Ctrl Pts',(-2.64978509923225,12.2,-10.088796626762));
#294514=CARTESIAN_POINT('Ctrl Pts',(-2.65011341197145,12.2,-10.0914895979888));
#294515=CARTESIAN_POINT('Ctrl Pts',(-2.65043976104284,12.2,-10.0942334086413));
#294516=CARTESIAN_POINT('Ctrl Pts',(-2.65076611011422,12.2,-10.0969772192938));
#294517=CARTESIAN_POINT('Ctrl Pts',(-2.65109049354409,12.2,-10.099771869884));
#294518=CARTESIAN_POINT('Ctrl Pts',(-2.65141229569918,12.2,-10.1026166776118));
#294519=CARTESIAN_POINT('Ctrl Pts',(-2.65173409785426,12.2,-10.1054614853395));
#294520=CARTESIAN_POINT('Ctrl Pts',(-2.65205331640188,12.2,-10.108356448881));
#294521=CARTESIAN_POINT('Ctrl Pts',(-2.65236935747395,12.2,-10.1113009016873));
#294522=CARTESIAN_POINT('Ctrl Pts',(-2.65268539857472,12.2,-10.1142453547611));
#294523=CARTESIAN_POINT('Ctrl Pts',(-2.65299825684187,12.2,-10.117239296673));
#294524=CARTESIAN_POINT('Ctrl Pts',(-2.65330735327523,12.2,-10.1202820709243));
#294525=CARTESIAN_POINT('Ctrl Pts',(-2.6536164496805,12.2,-10.1233248448992));
#294526=CARTESIAN_POINT('Ctrl Pts',(-2.65392178424282,12.2,-10.1264164543318));
#294527=CARTESIAN_POINT('Ctrl Pts',(-2.65422278873326,12.2,-10.1295562562319));
#294528=CARTESIAN_POINT('Ctrl Pts',(-2.6545237932237,12.2,-10.1326960581319));
#294529=CARTESIAN_POINT('Ctrl Pts',(-2.6548204693202,12.2,-10.1358840535347));
#294530=CARTESIAN_POINT('Ctrl Pts',(-2.65511226572659,12.2,-10.1391196154139));
#294531=CARTESIAN_POINT('Ctrl Pts',(-2.65540406215949,12.2,-10.142355177587));
#294532=CARTESIAN_POINT('Ctrl Pts',(-2.65569097776695,12.2,-10.1456383044564));
#294533=CARTESIAN_POINT('Ctrl Pts',(-2.65597247828205,12.2,-10.14896838289));
#294534=CARTESIAN_POINT('Ctrl Pts',(-2.65625397877158,12.2,-10.152298461021));
#294535=CARTESIAN_POINT('Ctrl Pts',(-2.65653006180852,12.2,-10.1556754927156));
#294536=CARTESIAN_POINT('Ctrl Pts',(-2.65680020829994,12.2,-10.1590988700234));
#294537=CARTESIAN_POINT('Ctrl Pts',(-2.65707035479137,12.2,-10.1625222473311));
#294538=CARTESIAN_POINT('Ctrl Pts',(-2.65733456181423,12.2,-10.1659919742893));
#294539=CARTESIAN_POINT('Ctrl Pts',(-2.65759232347197,12.2,-10.1695074575751));
#294540=CARTESIAN_POINT('Ctrl Pts',(-2.65785008515312,12.2,-10.1730229411802));
#294541=CARTESIAN_POINT('Ctrl Pts',(-2.65810140084023,12.2,-10.1765841834696));
#294542=CARTESIAN_POINT('Ctrl Pts',(-2.65834577378202,12.2,-10.1801906021823));
#294543=CARTESIAN_POINT('Ctrl Pts',(-2.65859014670162,12.2,-10.1837970205673));
#294544=CARTESIAN_POINT('Ctrl Pts',(-2.65882758030843,12.2,-10.1874486162425));
#294545=CARTESIAN_POINT('Ctrl Pts',(-2.65905758730007,12.2,-10.1911448195249));
#294546=CARTESIAN_POINT('Ctrl Pts',(-2.65928759429171,12.2,-10.1948410228073));
#294547=CARTESIAN_POINT('Ctrl Pts',(-2.65951017928423,12.2,-10.1985818334432));
#294548=CARTESIAN_POINT('Ctrl Pts',(-2.65972486820428,12.2,-10.2023666939089));
#294549=CARTESIAN_POINT('Ctrl Pts',(-2.65993955714384,12.2,-10.2061515547184));
#294550=CARTESIAN_POINT('Ctrl Pts',(-2.66014635065312,12.2,-10.2099804649914));
#294551=CARTESIAN_POINT('Ctrl Pts',(-2.66034479258003,12.2,-10.2138528737054));
#294552=CARTESIAN_POINT('Ctrl Pts',(-2.66054323448892,12.2,-10.2177252820677));
#294553=CARTESIAN_POINT('Ctrl Pts',(-2.66073332248927,12.2,-10.2216411908608));
#294554=CARTESIAN_POINT('Ctrl Pts',(-2.66091461048349,12.2,-10.2256000592351));
#294555=CARTESIAN_POINT('Ctrl Pts',(-2.66109589847771,12.2,-10.2295589276093));
#294556=CARTESIAN_POINT('Ctrl Pts',(-2.661268386155,12.2,-10.2335607571951));
#294557=CARTESIAN_POINT('Ctrl Pts',(-2.6614316372328,12.2,-10.2376050155464));
#294558=CARTESIAN_POINT('Ctrl Pts',(-2.66156767980258,12.2,-10.2409752309615));
#294559=CARTESIAN_POINT('Ctrl Pts',(-2.66169730820831,12.2,-10.2443749107774));
#294560=CARTESIAN_POINT('Ctrl Pts',(-2.66182027570866,12.2,-10.2478037545259));
#294561=CARTESIAN_POINT('Ctrl Pts',(-2.661943243209,12.2,-10.2512325982743));
#294562=CARTESIAN_POINT('Ctrl Pts',(-2.6620595504495,12.2,-10.2546906051323));
#294563=CARTESIAN_POINT('Ctrl Pts',(-2.66216895399168,12.2,-10.258177475773));
#294564=CARTESIAN_POINT('Ctrl Pts',(-2.66227835753386,12.2,-10.2616643464138));
#294565=CARTESIAN_POINT('Ctrl Pts',(-2.66238085976118,12.2,-10.2651800830166));
#294566=CARTESIAN_POINT('Ctrl Pts',(-2.66247622073341,12.2,-10.2687243894749));
#294567=CARTESIAN_POINT('Ctrl Pts',(-2.66257158170563,12.2,-10.2722686959333));
#294568=CARTESIAN_POINT('Ctrl Pts',(-2.66265980250532,12.2,-10.2758415734521));
#294569=CARTESIAN_POINT('Ctrl Pts',(-2.66274065174178,12.2,-10.2794427307602));
#294570=CARTESIAN_POINT('Ctrl Pts',(-2.66282150097824,12.2,-10.2830438880684));
#294571=CARTESIAN_POINT('Ctrl Pts',(-2.66289497861584,12.2,-10.2866733273045));
#294572=CARTESIAN_POINT('Ctrl Pts',(-2.662960854796,12.2,-10.2903307587643));
#294573=CARTESIAN_POINT('Ctrl Pts',(-2.66302673097616,12.2,-10.2939881902241));
#294574=CARTESIAN_POINT('Ctrl Pts',(-2.6630850084204,12.2,-10.2976736171804));
#294575=CARTESIAN_POINT('Ctrl Pts',(-2.66313546196166,12.2,-10.301386754543));
#294576=CARTESIAN_POINT('Ctrl Pts',(-2.66318591550292,12.2,-10.3050998919055));
#294577=CARTESIAN_POINT('Ctrl Pts',(-2.66322854556956,12.2,-10.3088407394751));
#294578=CARTESIAN_POINT('Ctrl Pts',(-2.66326313327906,12.2,-10.3126090202208));
#294579=CARTESIAN_POINT('Ctrl Pts',(-2.66329772098856,12.2,-10.3163773009665));
#294580=CARTESIAN_POINT('Ctrl Pts',(-2.66332426743092,12.2,-10.3201730127977));
#294581=CARTESIAN_POINT('Ctrl Pts',(-2.66334255527747,12.2,-10.3239958817583));
#294582=CARTESIAN_POINT('Ctrl Pts',(-2.66336084312401,12.2,-10.3278187507189));
#294583=CARTESIAN_POINT('Ctrl Pts',(-2.66337087492875,12.2,-10.3316687747715));
#294584=CARTESIAN_POINT('Ctrl Pts',(-2.66337243777528,12.2,-10.3355456837321));
#294585=CARTESIAN_POINT('Ctrl Pts',(-2.66337400062164,12.2,-10.33942259227));
#294586=CARTESIAN_POINT('Ctrl Pts',(-2.66336709709971,12.2,-10.3433263838442));
#294587=CARTESIAN_POINT('Ctrl Pts',(-2.66335151751878,12.2,-10.3472567914692));
#294588=CARTESIAN_POINT('Ctrl Pts',(-2.66333282201861,12.2,-10.3519732813903));
#294589=CARTESIAN_POINT('Ctrl Pts',(-2.66330163719225,12.2,-10.3567280939318));
#294590=CARTESIAN_POINT('Ctrl Pts',(-2.66325760877262,12.2,-10.361520775028));
#294591=CARTESIAN_POINT('Ctrl Pts',(-2.66322091842494,12.2,-10.3655146757238));
#294592=CARTESIAN_POINT('Ctrl Pts',(-2.66317531145247,12.2,-10.3695348726356));
#294593=CARTESIAN_POINT('Ctrl Pts',(-2.66312058922978,12.2,-10.3735811027064));
#294594=CARTESIAN_POINT('Ctrl Pts',(-2.66306586700708,12.2,-10.3776273327772));
#294595=CARTESIAN_POINT('Ctrl Pts',(-2.66300202853475,12.2,-10.381699597897));
#294596=CARTESIAN_POINT('Ctrl Pts',(-2.66292888047489,12.2,-10.3857976372008));
#294597=CARTESIAN_POINT('Ctrl Pts',(-2.66285573241503,12.2,-10.3898956765045));
#294598=CARTESIAN_POINT('Ctrl Pts',(-2.66277327411105,12.2,-10.3940194903017));
#294599=CARTESIAN_POINT('Ctrl Pts',(-2.66268131376305,12.2,-10.3981688235677));
#294600=CARTESIAN_POINT('Ctrl Pts',(-2.66260774549067,12.2,-10.4014882899091));
#294601=CARTESIAN_POINT('Ctrl Pts',(-2.66252809754961,12.2,-10.404824088165));
#294602=CARTESIAN_POINT('Ctrl Pts',(-2.66244227255704,12.2,-10.4081760885011));
#294603=CARTESIAN_POINT('Ctrl Pts',(-2.66233499130754,12.2,-10.4123660892637));
#294604=CARTESIAN_POINT('Ctrl Pts',(-2.66221805842847,12.2,-10.4165814049896));
#294605=CARTESIAN_POINT('Ctrl Pts',(-2.66209128898348,12.2,-10.4208217857726));
#294606=CARTESIAN_POINT('Ctrl Pts',(-2.66198987342196,12.2,-10.424214090584));
#294607=CARTESIAN_POINT('Ctrl Pts',(-2.66188216388829,12.2,-10.4276224374716));
#294608=CARTESIAN_POINT('Ctrl Pts',(-2.66176806621476,12.2,-10.4310466983265));
#294609=CARTESIAN_POINT('Ctrl Pts',(-2.6616254441306,12.2,-10.4353270241618));
#294610=CARTESIAN_POINT('Ctrl Pts',(-2.66147284076851,12.2,-10.439632214531));
#294611=CARTESIAN_POINT('Ctrl Pts',(-2.66131007646212,12.2,-10.4439620253663));
#294612=CARTESIAN_POINT('Ctrl Pts',(-2.66117986502765,12.2,-10.4474258737514));
#294613=CARTESIAN_POINT('Ctrl Pts',(-2.66104315280853,12.2,-10.4509054788203));
#294614=CARTESIAN_POINT('Ctrl Pts',(-2.66089984720851,12.2,-10.4544007152726));
#294615=CARTESIAN_POINT('Ctrl Pts',(-2.66075654158896,12.2,-10.4578959522011));
#294616=CARTESIAN_POINT('Ctrl Pts',(-2.66060664360592,12.2,-10.46140681998));
#294617=CARTESIAN_POINT('Ctrl Pts',(-2.66045006470781,12.2,-10.4649331967849));
#294618=CARTESIAN_POINT('Ctrl Pts',(-2.66029348583104,12.2,-10.4684595731093));
#294619=CARTESIAN_POINT('Ctrl Pts',(-2.66013022593846,12.2,-10.47200145649));
#294620=CARTESIAN_POINT('Ctrl Pts',(-2.65996019773058,12.2,-10.475558724976));
#294621=CARTESIAN_POINT('Ctrl Pts',(-2.65979016949954,12.2,-10.4791159939466));
#294622=CARTESIAN_POINT('Ctrl Pts',(-2.65961337396817,12.2,-10.4826886485362));
#294623=CARTESIAN_POINT('Ctrl Pts',(-2.6594297224484,12.2,-10.4862765657457));
#294624=CARTESIAN_POINT('Ctrl Pts',(-2.65924607095364,12.2,-10.4898644824663));
#294625=CARTESIAN_POINT('Ctrl Pts',(-2.65905556482179,12.2,-10.493467662465));
#294626=CARTESIAN_POINT('Ctrl Pts',(-2.65885811994949,12.2,-10.497085985446));
#294627=CARTESIAN_POINT('Ctrl Pts',(-2.6586606750503,12.2,-10.5007043089199));
#294628=CARTESIAN_POINT('Ctrl Pts',(-2.65845628990305,12.2,-10.5043377740846));
#294629=CARTESIAN_POINT('Ctrl Pts',(-2.6582448817244,12.2,-10.50798626234));
#294630=CARTESIAN_POINT('Ctrl Pts',(-2.6579806215155,12.2,-10.5125468724107));
#294631=CARTESIAN_POINT('Ctrl Pts',(-2.65770538780966,12.2,-10.517130954392));
#294632=CARTESIAN_POINT('Ctrl Pts',(-2.65741901918347,12.2,-10.5217382780265));
#294633=CARTESIAN_POINT('Ctrl Pts',(-2.65718992430124,12.2,-10.5254241366329));
#294634=CARTESIAN_POINT('Ctrl Pts',(-2.65695370326065,12.2,-10.5291248693788));
#294635=CARTESIAN_POINT('Ctrl Pts',(-2.65671027450325,12.2,-10.532840357963));
#294636=CARTESIAN_POINT('Ctrl Pts',(-2.65646684571267,12.2,-10.5365558470534));
#294637=CARTESIAN_POINT('Ctrl Pts',(-2.65621620986013,12.2,-10.540286092654));
#294638=CARTESIAN_POINT('Ctrl Pts',(-2.65595828751226,12.2,-10.5440309782479));
#294639=CARTESIAN_POINT('Ctrl Pts',(-2.65570036519954,12.2,-10.5477758633316));
#294640=CARTESIAN_POINT('Ctrl Pts',(-2.65543515385807,12.2,-10.5515353878681));
#294641=CARTESIAN_POINT('Ctrl Pts',(-2.6551625770896,12.2,-10.5553094359691));
#294642=CARTESIAN_POINT('Ctrl Pts',(-2.65489000028398,12.2,-10.5590834845843));
#294643=CARTESIAN_POINT('Ctrl Pts',(-2.65461005795656,12.2,-10.5628720576417));
#294644=CARTESIAN_POINT('Ctrl Pts',(-2.65432267121819,12.2,-10.5666750386277));
#294645=CARTESIAN_POINT('Ctrl Pts',(-2.65403528451897,12.2,-10.5704780190955));
#294646=CARTESIAN_POINT('Ctrl Pts',(-2.65374045463237,12.2,-10.5742954080271));
#294647=CARTESIAN_POINT('Ctrl Pts',(-2.65343810382452,12.2,-10.5781270918235));
#294648=CARTESIAN_POINT('Ctrl Pts',(-2.65313575297547,12.2,-10.581958776142));
#294649=CARTESIAN_POINT('Ctrl Pts',(-2.65282588106031,12.2,-10.5858047541635));
#294650=CARTESIAN_POINT('Ctrl Pts',(-2.65250841354154,12.2,-10.5896649145026));
#294651=CARTESIAN_POINT('Ctrl Pts',(-2.65219094606602,12.2,-10.5935250743157));
#294652=CARTESIAN_POINT('Ctrl Pts',(-2.65186588245983,12.2,-10.5973994151752));
#294653=CARTESIAN_POINT('Ctrl Pts',(-2.65153314782115,12.2,-10.6012878243559));
#294654=CARTESIAN_POINT('Ctrl Pts',(-2.6511172294888,12.2,-10.6061483362291));
#294655=CARTESIAN_POINT('Ctrl Pts',(-2.65068932673998,12.2,-10.6110308312825));
#294656=CARTESIAN_POINT('Ctrl Pts',(-2.65024929486597,12.2,-10.6159350898918));
#294657=CARTESIAN_POINT('Ctrl Pts',(-2.64989726934758,12.2,-10.6198584969931));
#294658=CARTESIAN_POINT('Ctrl Pts',(-2.64953748101879,12.2,-10.6237958324443));
#294659=CARTESIAN_POINT('Ctrl Pts',(-2.64916985827483,12.2,-10.627746987511));
#294660=CARTESIAN_POINT('Ctrl Pts',(-2.64880223558097,12.2,-10.6316981420393));
#294661=CARTESIAN_POINT('Ctrl Pts',(-2.64842677839451,12.2,-10.6356631155872));
#294662=CARTESIAN_POINT('Ctrl Pts',(-2.64804341503776,12.2,-10.6396417968161));
#294663=CARTESIAN_POINT('Ctrl Pts',(-2.64766005162879,12.2,-10.6436204785871));
#294664=CARTESIAN_POINT('Ctrl Pts',(-2.64726878260518,12.2,-10.6476128702788));
#294665=CARTESIAN_POINT('Ctrl Pts',(-2.64686953725009,12.2,-10.6516188607749));
#294666=CARTESIAN_POINT('Ctrl Pts',(-2.646470291895,12.2,-10.6556248512711));
#294667=CARTESIAN_POINT('Ctrl Pts',(-2.64606307048342,12.2,-10.659644441316));
#294668=CARTESIAN_POINT('Ctrl Pts',(-2.64564780368219,12.2,-10.663677522426));
#294669=CARTESIAN_POINT('Ctrl Pts',(-2.64523253693753,12.2,-10.6677106029866));
#294670=CARTESIAN_POINT('Ctrl Pts',(-2.64480922359393,12.2,-10.6717571753121));
#294671=CARTESIAN_POINT('Ctrl Pts',(-2.64437779751861,12.2,-10.6758171312015));
#294672=CARTESIAN_POINT('Ctrl Pts',(-2.64394637138452,12.2,-10.6798770876441));
#294673=CARTESIAN_POINT('Ctrl Pts',(-2.64350683114644,12.2,-10.6839504269261));
#294674=CARTESIAN_POINT('Ctrl Pts',(-2.64305910971007,12.2,-10.6880370435764));
#294675=CARTESIAN_POINT('Ctrl Pts',(-2.64261138833471,12.2,-10.6921236596698));
#294676=CARTESIAN_POINT('Ctrl Pts',(-2.64215548541614,12.2,-10.6962235528093));
#294677=CARTESIAN_POINT('Ctrl Pts',(-2.64169133478795,12.2,-10.7003366166388));
#294678=CARTESIAN_POINT('Ctrl Pts',(-2.64111114645529,12.2,-10.7054779468461));
#294679=CARTESIAN_POINT('Ctrl Pts',(-2.64051807003897,12.2,-10.71063985614));
#294680=CARTESIAN_POINT('Ctrl Pts',(-2.63991197983132,12.2,-10.7158221381528));
#294681=CARTESIAN_POINT('Ctrl Pts',(-2.63942710763877,12.2,-10.719967963989));
#294682=CARTESIAN_POINT('Ctrl Pts',(-2.63893390337205,12.2,-10.7241268293463));
#294683=CARTESIAN_POINT('Ctrl Pts',(-2.63843230715226,12.2,-10.7282986293387));
#294684=CARTESIAN_POINT('Ctrl Pts',(-2.63793071100081,12.2,-10.7324704287628));
#294685=CARTESIAN_POINT('Ctrl Pts',(-2.63742071929113,12.2,-10.7366551619259));
#294686=CARTESIAN_POINT('Ctrl Pts',(-2.63690226950073,12.2,-10.7408527264153));
#294687=CARTESIAN_POINT('Ctrl Pts',(-2.63638381963969,12.2,-10.7450502914765));
#294688=CARTESIAN_POINT('Ctrl Pts',(-2.63585691339987,12.2,-10.7492606849671));
#294689=CARTESIAN_POINT('Ctrl Pts',(-2.63532148598124,12.2,-10.753483808587));
#294690=CARTESIAN_POINT('Ctrl Pts',(-2.63478605863556,12.2,-10.7577069316315));
#294691=CARTESIAN_POINT('Ctrl Pts',(-2.63424210983135,12.2,-10.7619427795808));
#294692=CARTESIAN_POINT('Ctrl Pts',(-2.63368957857189,12.2,-10.7661912543336));
#294693=CARTESIAN_POINT('Ctrl Pts',(-2.63299891444108,12.2,-10.7715018482086));
#294694=CARTESIAN_POINT('Ctrl Pts',(-2.63229484022956,12.2,-10.7768321681457));
#294695=CARTESIAN_POINT('Ctrl Pts',(-2.63157723606361,12.2,-10.7821820151585));
#294696=CARTESIAN_POINT('Ctrl Pts',(-2.63085963189765,12.2,-10.7875318621714));
#294697=CARTESIAN_POINT('Ctrl Pts',(-2.63012849690911,12.2,-10.7929012362764));
#294698=CARTESIAN_POINT('Ctrl Pts',(-2.62938371684038,12.2,-10.7982899416227));
#294699=CARTESIAN_POINT('Ctrl Pts',(-2.62878789275292,12.2,-10.8026009061346));
#294700=CARTESIAN_POINT('Ctrl Pts',(-2.62818333359809,12.2,-10.8069242408335));
#294701=CARTESIAN_POINT('Ctrl Pts',(-2.62756998164437,12.2,-10.8112598481208));
#294702=CARTESIAN_POINT('Ctrl Pts',(-2.62695662977422,12.2,-10.8155954548174));
#294703=CARTESIAN_POINT('Ctrl Pts',(-2.62633448518554,12.2,-10.8199433313981));
#294704=CARTESIAN_POINT('Ctrl Pts',(-2.62570348929326,12.2,-10.824303380652));
#294705=CARTESIAN_POINT('Ctrl Pts',(-2.62491474436342,12.2,-10.8297534426649));
#294706=CARTESIAN_POINT('Ctrl Pts',(-2.62411216799157,12.2,-10.8352225209033));
#294707=CARTESIAN_POINT('Ctrl Pts',(-2.62329565056174,12.2,-10.8407104245828));
#294708=CARTESIAN_POINT('Ctrl Pts',(-2.62280574012164,12.2,-10.8440031666709));
#294709=CARTESIAN_POINT('Ctrl Pts',(-2.62231081096967,12.2,-10.8473026858994));
#294710=CARTESIAN_POINT('Ctrl Pts',(-2.62181083758844,12.2,-10.850608940652));
#294711=CARTESIAN_POINT('Ctrl Pts',(-2.62131086420721,12.2,-10.8539151954046));
#294712=CARTESIAN_POINT('Ctrl Pts',(-2.6208058479754,12.2,-10.8572281851478));
#294713=CARTESIAN_POINT('Ctrl Pts',(-2.62029576461962,12.2,-10.8605478692346));
#294714=CARTESIAN_POINT('Ctrl Pts',(-2.61978568117117,12.2,-10.8638675539245));
#294715=CARTESIAN_POINT('Ctrl Pts',(-2.61927053184631,12.2,-10.867193932058));
#294716=CARTESIAN_POINT('Ctrl Pts',(-2.61875029139501,12.2,-10.8705269637099));
#294717=CARTESIAN_POINT('Ctrl Pts',(-2.61823005103822,12.2,-10.8738599947564));
#294718=CARTESIAN_POINT('Ctrl Pts',(-2.61770472059003,12.2,-10.8771996783192));
#294719=CARTESIAN_POINT('Ctrl Pts',(-2.61717427669219,12.2,-10.8805459743648));
#294720=CARTESIAN_POINT('Ctrl Pts',(-2.61664383279435,12.2,-10.8838922704105));
#294721=CARTESIAN_POINT('Ctrl Pts',(-2.61610827563243,12.2,-10.8872451773764));
#294722=CARTESIAN_POINT('Ctrl Pts',(-2.6155675817746,12.2,-10.890604656478));
#294723=CARTESIAN_POINT('Ctrl Pts',(-2.61502688791676,12.2,-10.8939641355796));
#294724=CARTESIAN_POINT('Ctrl Pts',(-2.61448105781638,12.2,-10.8973301863875));
#294725=CARTESIAN_POINT('Ctrl Pts',(-2.61393006845892,12.2,-10.9007027674886));
#294726=CARTESIAN_POINT('Ctrl Pts',(-2.61337907910146,12.2,-10.9040753485896));
#294727=CARTESIAN_POINT('Ctrl Pts',(-2.61282293070701,12.2,-10.9074544597546));
#294728=CARTESIAN_POINT('Ctrl Pts',(-2.61226160076952,12.2,-10.910840061381));
#294729=CARTESIAN_POINT('Ctrl Pts',(-2.61170027083203,12.2,-10.9142256630075));
#294730=CARTESIAN_POINT('Ctrl Pts',(-2.61113375908657,12.2,-10.9176177551335));
#294731=CARTESIAN_POINT('Ctrl Pts',(-2.61056204364972,12.2,-10.9210162972591));
#294732=CARTESIAN_POINT('Ctrl Pts',(-2.609990328109,12.2,-10.9244148400021));
#294733=CARTESIAN_POINT('Ctrl Pts',(-2.60941340837517,12.2,-10.9278198330303));
#294734=CARTESIAN_POINT('Ctrl Pts',(-2.60883126287318,12.2,-10.931231235777));
#294735=CARTESIAN_POINT('Ctrl Pts',(-2.60824911747695,12.2,-10.9346426379039));
#294736=CARTESIAN_POINT('Ctrl Pts',(-2.60766174576073,12.2,-10.9380604498485));
#294737=CARTESIAN_POINT('Ctrl Pts',(-2.60706912637705,12.2,-10.9414846321875));
#294738=CARTESIAN_POINT('Ctrl Pts',(-2.60647650699336,12.2,-10.9449088145266));
#294739=CARTESIAN_POINT('Ctrl Pts',(-2.60587863994614,12.2,-10.9483393671657));
#294740=CARTESIAN_POINT('Ctrl Pts',(-2.60527550313426,12.2,-10.9517762493747));
#294741=CARTESIAN_POINT('Ctrl Pts',(-2.60467236632238,12.2,-10.9552131315837));
#294742=CARTESIAN_POINT('Ctrl Pts',(-2.6040639611278,12.2,-10.9586563446086));
#294743=CARTESIAN_POINT('Ctrl Pts',(-2.60345026423343,12.2,-10.962105848275));
#294744=CARTESIAN_POINT('Ctrl Pts',(-2.60283656733906,12.2,-10.9655553519413));
#294745=CARTESIAN_POINT('Ctrl Pts',(-2.60221757902824,12.2,-10.9690111466824));
#294746=CARTESIAN_POINT('Ctrl Pts',(-2.60159327959305,12.2,-10.9724731923894));
#294747=CARTESIAN_POINT('Ctrl Pts',(-2.60096898015786,12.2,-10.9759352380964));
#294748=CARTESIAN_POINT('Ctrl Pts',(-2.60033936879759,12.2,-10.9794035354312));
#294749=CARTESIAN_POINT('Ctrl Pts',(-2.59970442391456,12.2,-10.9828780448111));
#294750=CARTESIAN_POINT('Ctrl Pts',(-2.59906947903152,12.2,-10.9863525541911));
#294751=CARTESIAN_POINT('Ctrl Pts',(-2.59842920081665,12.2,-10.9898332763007));
#294752=CARTESIAN_POINT('Ctrl Pts',(-2.5977835698825,12.2,-10.9933201710065));
#294753=CARTESIAN_POINT('Ctrl Pts',(-2.59713793883106,12.2,-10.9968070663458));
#294754=CARTESIAN_POINT('Ctrl Pts',(-2.59648695308646,12.2,-11.0003001351701));
#294755=CARTESIAN_POINT('Ctrl Pts',(-2.59583059311534,12.2,-11.0037993384711));
#294756=CARTESIAN_POINT('Ctrl Pts',(-2.59495544668589,12.2,-11.0084649418131));
#294757=CARTESIAN_POINT('Ctrl Pts',(-2.59407074609382,12.2,-11.0131414503702));
#294758=CARTESIAN_POINT('Ctrl Pts',(-2.59317644305645,12.2,-11.0178287723752));
#294759=CARTESIAN_POINT('Ctrl Pts',(-2.59250571574795,12.2,-11.0213442640386));
#294760=CARTESIAN_POINT('Ctrl Pts',(-2.59182958762317,12.2,-11.0248658385099));
#294761=CARTESIAN_POINT('Ctrl Pts',(-2.591148036857,12.2,-11.0283934567143));
#294762=CARTESIAN_POINT('Ctrl Pts',(-2.59046648596702,12.2,-11.0319210755595));
#294763=CARTESIAN_POINT('Ctrl Pts',(-2.58977951430051,12.2,-11.0354547392731));
#294764=CARTESIAN_POINT('Ctrl Pts',(-2.58908710086581,12.2,-11.0389944085383));
#294765=CARTESIAN_POINT('Ctrl Pts',(-2.58793307876814,12.2,-11.0448938558133));
#294766=CARTESIAN_POINT('Ctrl Pts',(-2.58676394189133,12.2,-11.0508099852608));
#294767=CARTESIAN_POINT('Ctrl Pts',(-2.58557959889667,12.2,-11.0567426209323));
#294768=CARTESIAN_POINT('Ctrl Pts',(-2.58439525577291,12.2,-11.0626752572504));
#294769=CARTESIAN_POINT('Ctrl Pts',(-2.58319570712997,12.2,-11.0686243999043));
#294770=CARTESIAN_POINT('Ctrl Pts',(-2.58198086240899,12.2,-11.0745898721947));
#294771=CARTESIAN_POINT('Ctrl Pts',(-2.58125195547047,12.2,-11.0781691560891));
#294772=CARTESIAN_POINT('Ctrl Pts',(-2.58051754206374,12.2,-11.0817543194768));
#294773=CARTESIAN_POINT('Ctrl Pts',(-2.57977760408045,12.2,-11.0853453242911));
#294774=CARTESIAN_POINT('Ctrl Pts',(-2.57903766623159,12.2,-11.0889363284531));
#294775=CARTESIAN_POINT('Ctrl Pts',(-2.57829220346561,12.2,-11.0925331736306));
#294776=CARTESIAN_POINT('Ctrl Pts',(-2.5775411956214,12.2,-11.0961358233887));
#294777=CARTESIAN_POINT('Ctrl Pts',(-2.5767901877772,12.2,-11.0997384731468));
#294778=CARTESIAN_POINT('Ctrl Pts',(-2.57603363493972,12.2,-11.1033469255248));
#294779=CARTESIAN_POINT('Ctrl Pts',(-2.5752715201336,12.2,-11.1069611441857));
#294780=CARTESIAN_POINT('Ctrl Pts',(-2.57450940532747,12.2,-11.1105753628466));
#294781=CARTESIAN_POINT('Ctrl Pts',(-2.57374172875534,12.2,-11.1141953480984));
#294782=CARTESIAN_POINT('Ctrl Pts',(-2.57296846953343,12.2,-11.1178210627583));
#294783=CARTESIAN_POINT('Ctrl Pts',(-2.57219521031153,12.2,-11.1214467774182));
#294784=CARTESIAN_POINT('Ctrl Pts',(-2.57141637063985,12.2,-11.1250782207029));
#294785=CARTESIAN_POINT('Ctrl Pts',(-2.5706319318355,12.2,-11.128715357362));
#294786=CARTESIAN_POINT('Ctrl Pts',(-2.56984749303116,12.2,-11.132352494021));
#294787=CARTESIAN_POINT('Ctrl Pts',(-2.56905745493083,12.2,-11.1359953233451));
#294788=CARTESIAN_POINT('Ctrl Pts',(-2.56826179767065,12.2,-11.1396438057691));
#294789=CARTESIAN_POINT('Ctrl Pts',(-2.56746614041046,12.2,-11.1432922881932));
#294790=CARTESIAN_POINT('Ctrl Pts',(-2.56666486591258,12.2,-11.1469464247525));
#294791=CARTESIAN_POINT('Ctrl Pts',(-2.56585795469266,12.2,-11.1506061784522));
#294792=CARTESIAN_POINT('Ctrl Pts',(-2.56478207296838,12.2,-11.1554858504949));
#294793=CARTESIAN_POINT('Ctrl Pts',(-2.56369617228761,12.2,-11.1603755090857));
#294794=CARTESIAN_POINT('Ctrl Pts',(-2.56260021378343,12.2,-11.1652750757416));
#294795=CARTESIAN_POINT('Ctrl Pts',(-2.56177824497996,12.2,-11.1689497503998));
#294796=CARTESIAN_POINT('Ctrl Pts',(-2.56095061872672,12.2,-11.172629997866));
#294797=CARTESIAN_POINT('Ctrl Pts',(-2.56011731584083,12.2,-11.1763157773567));
#294798=CARTESIAN_POINT('Ctrl Pts',(-2.55928401295493,12.2,-11.1800015568472));
#294799=CARTESIAN_POINT('Ctrl Pts',(-2.55844503222431,12.2,-11.183692866235));
#294800=CARTESIAN_POINT('Ctrl Pts',(-2.5576003524218,12.2,-11.1873896640348));
#294801=CARTESIAN_POINT('Ctrl Pts',(-2.5564741125828,12.2,-11.1923187282155));
#294802=CARTESIAN_POINT('Ctrl Pts',(-2.55533774007136,12.2,-11.1972575404348));
#294803=CARTESIAN_POINT('Ctrl Pts',(-2.5541912119275,12.2,-11.20220605643));
#294804=CARTESIAN_POINT('Ctrl Pts',(-2.55333131589771,12.2,-11.2059174430893));
#294805=CARTESIAN_POINT('Ctrl Pts',(-2.55246571115834,12.2,-11.2096342863238));
#294806=CARTESIAN_POINT('Ctrl Pts',(-2.55159439100006,12.2,-11.213356592));
#294807=CARTESIAN_POINT('Ctrl Pts',(-2.17615954800006,15.2,-11.292224299));
#294808=CARTESIAN_POINT('Ctrl Pts',(-2.17615954800006,11.6,-11.292224299));
#294809=CARTESIAN_POINT('Ctrl Pts',(-2.17570045500006,15.2,-11.291612887));
#294810=CARTESIAN_POINT('Ctrl Pts',(-2.17570045500006,11.6,-11.291612887));
#294811=CARTESIAN_POINT('Ctrl Pts',(-2.17478276600006,15.2,-11.290390245));
#294812=CARTESIAN_POINT('Ctrl Pts',(-2.17478276600006,11.6,-11.290390245));
#294813=CARTESIAN_POINT('Ctrl Pts',(-2.17340771700006,15.2,-11.28855682));
#294814=CARTESIAN_POINT('Ctrl Pts',(-2.17340771700006,11.6,-11.28855682));
#294815=CARTESIAN_POINT('Ctrl Pts',(-2.17157728800006,15.2,-11.286113334));
#294816=CARTESIAN_POINT('Ctrl Pts',(-2.17157728800006,11.6,-11.286113334));
#294817=CARTESIAN_POINT('Ctrl Pts',(-2.16929420200006,15.2,-11.283060773));
#294818=CARTESIAN_POINT('Ctrl Pts',(-2.16929420200006,11.6,-11.283060773));
#294819=CARTESIAN_POINT('Ctrl Pts',(-2.16701606700005,15.2,-11.280010015));
#294820=CARTESIAN_POINT('Ctrl Pts',(-2.16701606700005,11.6,-11.280010015));
#294821=CARTESIAN_POINT('Ctrl Pts',(-2.16474288100006,15.2,-11.276961058));
#294822=CARTESIAN_POINT('Ctrl Pts',(-2.16474288100006,11.6,-11.276961058));
#294823=CARTESIAN_POINT('Ctrl Pts',(-2.16247464600006,15.2,-11.273913908));
#294824=CARTESIAN_POINT('Ctrl Pts',(-2.16247464600006,11.6,-11.273913908));
#294825=CARTESIAN_POINT('Ctrl Pts',(-2.16021136000006,15.2,-11.27086857));
#294826=CARTESIAN_POINT('Ctrl Pts',(-2.16021136000006,11.6,-11.27086857));
#294827=CARTESIAN_POINT('Ctrl Pts',(-2.15795302500006,15.2,-11.267825054));
#294828=CARTESIAN_POINT('Ctrl Pts',(-2.15795302500006,11.6,-11.267825054));
#294829=CARTESIAN_POINT('Ctrl Pts',(-2.15569963800006,15.2,-11.264783368));
#294830=CARTESIAN_POINT('Ctrl Pts',(-2.15569963800006,11.6,-11.264783368));
#294831=CARTESIAN_POINT('Ctrl Pts',(-2.15345120200006,15.2,-11.261743524));
#294832=CARTESIAN_POINT('Ctrl Pts',(-2.15345120200006,11.6,-11.261743524));
#294833=CARTESIAN_POINT('Ctrl Pts',(-2.15120771500006,15.2,-11.258705531));
#294834=CARTESIAN_POINT('Ctrl Pts',(-2.15120771500006,11.6,-11.258705531));
#294835=CARTESIAN_POINT('Ctrl Pts',(-2.14896917600006,15.2,-11.255669403));
#294836=CARTESIAN_POINT('Ctrl Pts',(-2.14896917600006,11.6,-11.255669403));
#294837=CARTESIAN_POINT('Ctrl Pts',(-2.14673558400006,15.2,-11.252635149));
#294838=CARTESIAN_POINT('Ctrl Pts',(-2.14673558400006,11.6,-11.252635149));
#294839=CARTESIAN_POINT('Ctrl Pts',(-2.14450694000006,15.2,-11.249602777));
#294840=CARTESIAN_POINT('Ctrl Pts',(-2.14450694000006,11.6,-11.249602777));
#294841=CARTESIAN_POINT('Ctrl Pts',(-2.14228324400006,15.2,-11.246572299));
#294842=CARTESIAN_POINT('Ctrl Pts',(-2.14228324400006,11.6,-11.246572299));
#294843=CARTESIAN_POINT('Ctrl Pts',(-2.14006449500005,15.2,-11.243543721));
#294844=CARTESIAN_POINT('Ctrl Pts',(-2.14006449500005,11.6,-11.243543721));
#294845=CARTESIAN_POINT('Ctrl Pts',(-2.13785069300005,15.2,-11.24051705));
#294846=CARTESIAN_POINT('Ctrl Pts',(-2.13785069300005,11.6,-11.24051705));
#294847=CARTESIAN_POINT('Ctrl Pts',(-2.13564183800006,15.2,-11.237492297));
#294848=CARTESIAN_POINT('Ctrl Pts',(-2.13564183800006,11.6,-11.237492297));
#294849=CARTESIAN_POINT('Ctrl Pts',(-2.13343792800006,15.2,-11.234469469));
#294850=CARTESIAN_POINT('Ctrl Pts',(-2.13343792800006,11.6,-11.234469469));
#294851=CARTESIAN_POINT('Ctrl Pts',(-2.13123896500006,15.2,-11.231448574));
#294852=CARTESIAN_POINT('Ctrl Pts',(-2.13123896500006,11.6,-11.231448574));
#294853=CARTESIAN_POINT('Ctrl Pts',(-2.12904494800005,15.2,-11.228429624));
#294854=CARTESIAN_POINT('Ctrl Pts',(-2.12904494800005,11.6,-11.228429624));
#294855=CARTESIAN_POINT('Ctrl Pts',(-2.12685587600005,15.2,-11.225412626));
#294856=CARTESIAN_POINT('Ctrl Pts',(-2.12685587600005,11.6,-11.225412626));
#294857=CARTESIAN_POINT('Ctrl Pts',(-2.12467174800006,15.2,-11.222397592));
#294858=CARTESIAN_POINT('Ctrl Pts',(-2.12467174800006,11.6,-11.222397592));
#294859=CARTESIAN_POINT('Ctrl Pts',(-2.12249256500006,15.2,-11.219384528));
#294860=CARTESIAN_POINT('Ctrl Pts',(-2.12249256500006,11.6,-11.219384528));
#294861=CARTESIAN_POINT('Ctrl Pts',(-2.12031832600006,15.2,-11.216373446));
#294862=CARTESIAN_POINT('Ctrl Pts',(-2.12031832600006,11.6,-11.216373446));
#294863=CARTESIAN_POINT('Ctrl Pts',(-2.11814903000006,15.2,-11.213364356));
#294864=CARTESIAN_POINT('Ctrl Pts',(-2.11814903000006,11.6,-11.213364356));
#294865=CARTESIAN_POINT('Ctrl Pts',(-2.11598467700005,15.2,-11.210357264));
#294866=CARTESIAN_POINT('Ctrl Pts',(-2.11598467700005,11.6,-11.210357264));
#294867=CARTESIAN_POINT('Ctrl Pts',(-2.11382526700006,15.2,-11.207352181));
#294868=CARTESIAN_POINT('Ctrl Pts',(-2.11382526700006,11.6,-11.207352181));
#294869=CARTESIAN_POINT('Ctrl Pts',(-2.11167080000005,15.2,-11.204349116));
#294870=CARTESIAN_POINT('Ctrl Pts',(-2.11167080000005,11.6,-11.204349116));
#294871=CARTESIAN_POINT('Ctrl Pts',(-2.10952127400006,15.2,-11.201348078));
#294872=CARTESIAN_POINT('Ctrl Pts',(-2.10952127400006,11.6,-11.201348078));
#294873=CARTESIAN_POINT('Ctrl Pts',(-2.10737669000005,15.2,-11.198349076));
#294874=CARTESIAN_POINT('Ctrl Pts',(-2.10737669000005,11.6,-11.198349076));
#294875=CARTESIAN_POINT('Ctrl Pts',(-2.10523704700006,15.2,-11.19535212));
#294876=CARTESIAN_POINT('Ctrl Pts',(-2.10523704700006,11.6,-11.19535212));
#294877=CARTESIAN_POINT('Ctrl Pts',(-2.10310234500006,15.2,-11.192357218));
#294878=CARTESIAN_POINT('Ctrl Pts',(-2.10310234500006,11.6,-11.192357218));
#294879=CARTESIAN_POINT('Ctrl Pts',(-2.10097258200005,15.2,-11.18936438));
#294880=CARTESIAN_POINT('Ctrl Pts',(-2.10097258200005,11.6,-11.18936438));
#294881=CARTESIAN_POINT('Ctrl Pts',(-2.09884776000006,15.2,-11.186373616));
#294882=CARTESIAN_POINT('Ctrl Pts',(-2.09884776000006,11.6,-11.186373616));
#294883=CARTESIAN_POINT('Ctrl Pts',(-2.09672787600006,15.2,-11.183384935));
#294884=CARTESIAN_POINT('Ctrl Pts',(-2.09672787600006,11.6,-11.183384935));
#294885=CARTESIAN_POINT('Ctrl Pts',(-2.09461293200006,15.2,-11.180398346));
#294886=CARTESIAN_POINT('Ctrl Pts',(-2.09461293200006,11.6,-11.180398346));
#294887=CARTESIAN_POINT('Ctrl Pts',(-2.09250292400006,15.2,-11.177413859));
#294888=CARTESIAN_POINT('Ctrl Pts',(-2.09250292400006,11.6,-11.177413859));
#294889=CARTESIAN_POINT('Ctrl Pts',(-2.09039785500006,15.2,-11.174431482));
#294890=CARTESIAN_POINT('Ctrl Pts',(-2.09039785500006,11.6,-11.174431482));
#294891=CARTESIAN_POINT('Ctrl Pts',(-2.08829772300006,15.2,-11.171451227));
#294892=CARTESIAN_POINT('Ctrl Pts',(-2.08829772300006,11.6,-11.171451227));
#294893=CARTESIAN_POINT('Ctrl Pts',(-2.08620252700006,15.2,-11.1684731));
#294894=CARTESIAN_POINT('Ctrl Pts',(-2.08620252700006,11.6,-11.1684731));
#294895=CARTESIAN_POINT('Ctrl Pts',(-2.08411226900005,15.2,-11.165497114));
#294896=CARTESIAN_POINT('Ctrl Pts',(-2.08411226900005,11.6,-11.165497114));
#294897=CARTESIAN_POINT('Ctrl Pts',(-2.08202694500006,15.2,-11.162523276));
#294898=CARTESIAN_POINT('Ctrl Pts',(-2.08202694500006,11.6,-11.162523276));
#294899=CARTESIAN_POINT('Ctrl Pts',(-2.07994655600006,15.2,-11.159551596));
#294900=CARTESIAN_POINT('Ctrl Pts',(-2.07994655600006,11.6,-11.159551596));
#294901=CARTESIAN_POINT('Ctrl Pts',(-2.07787110100006,15.2,-11.156582084));
#294902=CARTESIAN_POINT('Ctrl Pts',(-2.07787110100006,11.6,-11.156582084));
#294903=CARTESIAN_POINT('Ctrl Pts',(-2.07580058000006,15.2,-11.153614748));
#294904=CARTESIAN_POINT('Ctrl Pts',(-2.07580058000006,11.6,-11.153614748));
#294905=CARTESIAN_POINT('Ctrl Pts',(-2.07373499200005,15.2,-11.1506496));
#294906=CARTESIAN_POINT('Ctrl Pts',(-2.07373499200005,11.6,-11.1506496));
#294907=CARTESIAN_POINT('Ctrl Pts',(-2.07167433800006,15.2,-11.147686647));
#294908=CARTESIAN_POINT('Ctrl Pts',(-2.07167433800006,11.6,-11.147686647));
#294909=CARTESIAN_POINT('Ctrl Pts',(-2.06961861500006,15.2,-11.1447259));
#294910=CARTESIAN_POINT('Ctrl Pts',(-2.06961861500006,11.6,-11.1447259));
#294911=CARTESIAN_POINT('Ctrl Pts',(-2.06756782400006,15.2,-11.141767369));
#294912=CARTESIAN_POINT('Ctrl Pts',(-2.06756782400006,11.6,-11.141767369));
#294913=CARTESIAN_POINT('Ctrl Pts',(-2.06552196300006,15.2,-11.138811062));
#294914=CARTESIAN_POINT('Ctrl Pts',(-2.06552196300006,11.6,-11.138811062));
#294915=CARTESIAN_POINT('Ctrl Pts',(-2.06348103200006,15.2,-11.13585699));
#294916=CARTESIAN_POINT('Ctrl Pts',(-2.06348103200006,11.6,-11.13585699));
#294917=CARTESIAN_POINT('Ctrl Pts',(-2.06144503200006,15.2,-11.132905162));
#294918=CARTESIAN_POINT('Ctrl Pts',(-2.06144503200006,11.6,-11.132905162));
#294919=CARTESIAN_POINT('Ctrl Pts',(-2.05941396000005,15.2,-11.129955589));
#294920=CARTESIAN_POINT('Ctrl Pts',(-2.05941396000005,11.6,-11.129955589));
#294921=CARTESIAN_POINT('Ctrl Pts',(-2.05738781600005,15.2,-11.127008278));
#294922=CARTESIAN_POINT('Ctrl Pts',(-2.05738781600005,11.6,-11.127008278));
#294923=CARTESIAN_POINT('Ctrl Pts',(-2.05536660000006,15.2,-11.12406324));
#294924=CARTESIAN_POINT('Ctrl Pts',(-2.05536660000006,11.6,-11.12406324));
#294925=CARTESIAN_POINT('Ctrl Pts',(-2.05335031200006,15.2,-11.121120485));
#294926=CARTESIAN_POINT('Ctrl Pts',(-2.05335031200006,11.6,-11.121120485));
#294927=CARTESIAN_POINT('Ctrl Pts',(-2.05133894900006,15.2,-11.118180023));
#294928=CARTESIAN_POINT('Ctrl Pts',(-2.05133894900006,11.6,-11.118180023));
#294929=CARTESIAN_POINT('Ctrl Pts',(-2.04933251100006,15.2,-11.115241862));
#294930=CARTESIAN_POINT('Ctrl Pts',(-2.04933251100006,11.6,-11.115241862));
#294931=CARTESIAN_POINT('Ctrl Pts',(-2.04733100000006,15.2,-11.112306013));
#294932=CARTESIAN_POINT('Ctrl Pts',(-2.04733100000006,11.6,-11.112306013));
#294933=CARTESIAN_POINT('Ctrl Pts',(-2.04533441100006,15.2,-11.109372486));
#294934=CARTESIAN_POINT('Ctrl Pts',(-2.04533441100006,11.6,-11.109372486));
#294935=CARTESIAN_POINT('Ctrl Pts',(-2.04334274700006,15.2,-11.106441291));
#294936=CARTESIAN_POINT('Ctrl Pts',(-2.04334274700006,11.6,-11.106441291));
#294937=CARTESIAN_POINT('Ctrl Pts',(-2.04135600500006,15.2,-11.103512437));
#294938=CARTESIAN_POINT('Ctrl Pts',(-2.04135600500006,11.6,-11.103512437));
#294939=CARTESIAN_POINT('Ctrl Pts',(-2.03937418400006,15.2,-11.100585934));
#294940=CARTESIAN_POINT('Ctrl Pts',(-2.03937418400006,11.6,-11.100585934));
#294941=CARTESIAN_POINT('Ctrl Pts',(-2.03739728600006,15.2,-11.097661791));
#294942=CARTESIAN_POINT('Ctrl Pts',(-2.03739728600006,11.6,-11.097661791));
#294943=CARTESIAN_POINT('Ctrl Pts',(-2.03542530900005,15.2,-11.094740019));
#294944=CARTESIAN_POINT('Ctrl Pts',(-2.03542530900005,11.6,-11.094740019));
#294945=CARTESIAN_POINT('Ctrl Pts',(-2.03345825000006,15.2,-11.091820627));
#294946=CARTESIAN_POINT('Ctrl Pts',(-2.03345825000006,11.6,-11.091820627));
#294947=CARTESIAN_POINT('Ctrl Pts',(-2.03149611100006,15.2,-11.088903627));
#294948=CARTESIAN_POINT('Ctrl Pts',(-2.03149611100006,11.6,-11.088903627));
#294949=CARTESIAN_POINT('Ctrl Pts',(-2.02953889000006,15.2,-11.085989026));
#294950=CARTESIAN_POINT('Ctrl Pts',(-2.02953889000006,11.6,-11.085989026));
#294951=CARTESIAN_POINT('Ctrl Pts',(-2.02758658500006,15.2,-11.083076836));
#294952=CARTESIAN_POINT('Ctrl Pts',(-2.02758658500006,11.6,-11.083076836));
#294953=CARTESIAN_POINT('Ctrl Pts',(-2.02563919900005,15.2,-11.080167065));
#294954=CARTESIAN_POINT('Ctrl Pts',(-2.02563919900005,11.6,-11.080167065));
#294955=CARTESIAN_POINT('Ctrl Pts',(-2.02369672800006,15.2,-11.077259724));
#294956=CARTESIAN_POINT('Ctrl Pts',(-2.02369672800006,11.6,-11.077259724));
#294957=CARTESIAN_POINT('Ctrl Pts',(-2.02175917100006,15.2,-11.074354824));
#294958=CARTESIAN_POINT('Ctrl Pts',(-2.02175917100006,11.6,-11.074354824));
#294959=CARTESIAN_POINT('Ctrl Pts',(-2.01982652900006,15.2,-11.071452373));
#294960=CARTESIAN_POINT('Ctrl Pts',(-2.01982652900006,11.6,-11.071452373));
#294961=CARTESIAN_POINT('Ctrl Pts',(-2.01789880000006,15.2,-11.068552382));
#294962=CARTESIAN_POINT('Ctrl Pts',(-2.01789880000006,11.6,-11.068552382));
#294963=CARTESIAN_POINT('Ctrl Pts',(-2.01597598400005,15.2,-11.065654863));
#294964=CARTESIAN_POINT('Ctrl Pts',(-2.01597598400005,11.6,-11.065654863));
#294965=CARTESIAN_POINT('Ctrl Pts',(-2.01405807900006,15.2,-11.062759821));
#294966=CARTESIAN_POINT('Ctrl Pts',(-2.01405807900006,11.6,-11.062759821));
#294967=CARTESIAN_POINT('Ctrl Pts',(-2.01214508600006,15.2,-11.059867271));
#294968=CARTESIAN_POINT('Ctrl Pts',(-2.01214508600006,11.6,-11.059867271));
#294969=CARTESIAN_POINT('Ctrl Pts',(-2.01023700100006,15.2,-11.056977221));
#294970=CARTESIAN_POINT('Ctrl Pts',(-2.01023700100006,11.6,-11.056977221));
#294971=CARTESIAN_POINT('Ctrl Pts',(-2.00833382600006,15.2,-11.054089681));
#294972=CARTESIAN_POINT('Ctrl Pts',(-2.00833382600006,11.6,-11.054089681));
#294973=CARTESIAN_POINT('Ctrl Pts',(-2.00643555900006,15.2,-11.05120466));
#294974=CARTESIAN_POINT('Ctrl Pts',(-2.00643555900006,11.6,-11.05120466));
#294975=CARTESIAN_POINT('Ctrl Pts',(-2.00454219900006,15.2,-11.048322171));
#294976=CARTESIAN_POINT('Ctrl Pts',(-2.00454219900006,11.6,-11.048322171));
#294977=CARTESIAN_POINT('Ctrl Pts',(-2.00265374600006,15.2,-11.045442222));
#294978=CARTESIAN_POINT('Ctrl Pts',(-2.00265374600006,11.6,-11.045442222));
#294979=CARTESIAN_POINT('Ctrl Pts',(-2.00077019700006,15.2,-11.042564824));
#294980=CARTESIAN_POINT('Ctrl Pts',(-2.00077019700006,11.6,-11.042564824));
#294981=CARTESIAN_POINT('Ctrl Pts',(-1.99889155400006,15.2,-11.039689987));
#294982=CARTESIAN_POINT('Ctrl Pts',(-1.99889155400006,11.6,-11.039689987));
#294983=CARTESIAN_POINT('Ctrl Pts',(-1.99701781300006,15.2,-11.03681772));
#294984=CARTESIAN_POINT('Ctrl Pts',(-1.99701781300006,11.6,-11.03681772));
#294985=CARTESIAN_POINT('Ctrl Pts',(-1.99514897500006,15.2,-11.033948035));
#294986=CARTESIAN_POINT('Ctrl Pts',(-1.99514897500006,11.6,-11.033948035));
#294987=CARTESIAN_POINT('Ctrl Pts',(-1.99328503900006,15.2,-11.031080942));
#294988=CARTESIAN_POINT('Ctrl Pts',(-1.99328503900006,11.6,-11.031080942));
#294989=CARTESIAN_POINT('Ctrl Pts',(-1.99142600300006,15.2,-11.02821645));
#294990=CARTESIAN_POINT('Ctrl Pts',(-1.99142600300006,11.6,-11.02821645));
#294991=CARTESIAN_POINT('Ctrl Pts',(-1.98957186800006,15.2,-11.025354571));
#294992=CARTESIAN_POINT('Ctrl Pts',(-1.98957186800006,11.6,-11.025354571));
#294993=CARTESIAN_POINT('Ctrl Pts',(-1.98772263100006,15.2,-11.022495313));
#294994=CARTESIAN_POINT('Ctrl Pts',(-1.98772263100006,11.6,-11.022495313));
#294995=CARTESIAN_POINT('Ctrl Pts',(-1.98587829000005,15.2,-11.019638689));
#294996=CARTESIAN_POINT('Ctrl Pts',(-1.98587829000005,11.6,-11.019638689));
#294997=CARTESIAN_POINT('Ctrl Pts',(-1.98403884700005,15.2,-11.016784707));
#294998=CARTESIAN_POINT('Ctrl Pts',(-1.98403884700005,11.6,-11.016784707));
#294999=CARTESIAN_POINT('Ctrl Pts',(-1.98220430000006,15.2,-11.013933379));
#295000=CARTESIAN_POINT('Ctrl Pts',(-1.98220430000006,11.6,-11.013933379));
#295001=CARTESIAN_POINT('Ctrl Pts',(-1.98037464600006,15.2,-11.011084714));
#295002=CARTESIAN_POINT('Ctrl Pts',(-1.98037464600006,11.6,-11.011084714));
#295003=CARTESIAN_POINT('Ctrl Pts',(-1.97854988600006,15.2,-11.008238724));
#295004=CARTESIAN_POINT('Ctrl Pts',(-1.97854988600006,11.6,-11.008238724));
#295005=CARTESIAN_POINT('Ctrl Pts',(-1.97673001900006,15.2,-11.005395418));
#295006=CARTESIAN_POINT('Ctrl Pts',(-1.97673001900006,11.6,-11.005395418));
#295007=CARTESIAN_POINT('Ctrl Pts',(-1.97491504200005,15.2,-11.002554807));
#295008=CARTESIAN_POINT('Ctrl Pts',(-1.97491504200005,11.6,-11.002554807));
#295009=CARTESIAN_POINT('Ctrl Pts',(-1.97310495700005,15.2,-10.999716901));
#295010=CARTESIAN_POINT('Ctrl Pts',(-1.97310495700005,11.6,-10.999716901));
#295011=CARTESIAN_POINT('Ctrl Pts',(-1.97129976000005,15.2,-10.996881712));
#295012=CARTESIAN_POINT('Ctrl Pts',(-1.97129976000005,11.6,-10.996881712));
#295013=CARTESIAN_POINT('Ctrl Pts',(-1.96949945100006,15.2,-10.994049247));
#295014=CARTESIAN_POINT('Ctrl Pts',(-1.96949945100006,11.6,-10.994049247));
#295015=CARTESIAN_POINT('Ctrl Pts',(-1.96770402900006,15.2,-10.99121952));
#295016=CARTESIAN_POINT('Ctrl Pts',(-1.96770402900006,11.6,-10.99121952));
#295017=CARTESIAN_POINT('Ctrl Pts',(-1.96591349400005,15.2,-10.988392541));
#295018=CARTESIAN_POINT('Ctrl Pts',(-1.96591349400005,11.6,-10.988392541));
#295019=CARTESIAN_POINT('Ctrl Pts',(-1.96412784300006,15.2,-10.985568319));
#295020=CARTESIAN_POINT('Ctrl Pts',(-1.96412784300006,11.6,-10.985568319));
#295021=CARTESIAN_POINT('Ctrl Pts',(-1.96234707500006,15.2,-10.982746866));
#295022=CARTESIAN_POINT('Ctrl Pts',(-1.96234707500006,11.6,-10.982746866));
#295023=CARTESIAN_POINT('Ctrl Pts',(-1.96057119000006,15.2,-10.979928192));
#295024=CARTESIAN_POINT('Ctrl Pts',(-1.96057119000006,11.6,-10.979928192));
#295025=CARTESIAN_POINT('Ctrl Pts',(-1.95880018600006,15.2,-10.977112307));
#295026=CARTESIAN_POINT('Ctrl Pts',(-1.95880018600006,11.6,-10.977112307));
#295027=CARTESIAN_POINT('Ctrl Pts',(-1.95703406200006,15.2,-10.974299223));
#295028=CARTESIAN_POINT('Ctrl Pts',(-1.95703406200006,11.6,-10.974299223));
#295029=CARTESIAN_POINT('Ctrl Pts',(-1.95527281700006,15.2,-10.971488949));
#295030=CARTESIAN_POINT('Ctrl Pts',(-1.95527281700006,11.6,-10.971488949));
#295031=CARTESIAN_POINT('Ctrl Pts',(-1.95351645100006,15.2,-10.968681498));
#295032=CARTESIAN_POINT('Ctrl Pts',(-1.95351645100006,11.6,-10.968681498));
#295033=CARTESIAN_POINT('Ctrl Pts',(-1.95176495900005,15.2,-10.965876877));
#295034=CARTESIAN_POINT('Ctrl Pts',(-1.95176495900005,11.6,-10.965876877));
#295035=CARTESIAN_POINT('Ctrl Pts',(-1.95001834500005,15.2,-10.963075101));
#295036=CARTESIAN_POINT('Ctrl Pts',(-1.95001834500005,11.6,-10.963075101));
#295037=CARTESIAN_POINT('Ctrl Pts',(-1.94827660300006,15.2,-10.960276177));
#295038=CARTESIAN_POINT('Ctrl Pts',(-1.94827660300006,11.6,-10.960276177));
#295039=CARTESIAN_POINT('Ctrl Pts',(-1.94653973400006,15.2,-10.957480118));
#295040=CARTESIAN_POINT('Ctrl Pts',(-1.94653973400006,11.6,-10.957480118));
#295041=CARTESIAN_POINT('Ctrl Pts',(-1.94480773800006,15.2,-10.954686934));
#295042=CARTESIAN_POINT('Ctrl Pts',(-1.94480773800006,11.6,-10.954686934));
#295043=CARTESIAN_POINT('Ctrl Pts',(-1.94308061000006,15.2,-10.951896636));
#295044=CARTESIAN_POINT('Ctrl Pts',(-1.94308061000006,11.6,-10.951896636));
#295045=CARTESIAN_POINT('Ctrl Pts',(-1.94135835200006,15.2,-10.949109235));
#295046=CARTESIAN_POINT('Ctrl Pts',(-1.94135835200006,11.6,-10.949109235));
#295047=CARTESIAN_POINT('Ctrl Pts',(-1.93964096300005,15.2,-10.946324741));
#295048=CARTESIAN_POINT('Ctrl Pts',(-1.93964096300005,11.6,-10.946324741));
#295049=CARTESIAN_POINT('Ctrl Pts',(-1.93792843900006,15.2,-10.943543166));
#295050=CARTESIAN_POINT('Ctrl Pts',(-1.93792843900006,11.6,-10.943543166));
#295051=CARTESIAN_POINT('Ctrl Pts',(-1.93622078100006,15.2,-10.940764519));
#295052=CARTESIAN_POINT('Ctrl Pts',(-1.93622078100006,11.6,-10.940764519));
#295053=CARTESIAN_POINT('Ctrl Pts',(-1.93451798600006,15.2,-10.937988814));
#295054=CARTESIAN_POINT('Ctrl Pts',(-1.93451798600006,11.6,-10.937988814));
#295055=CARTESIAN_POINT('Ctrl Pts',(-1.93282005500006,15.2,-10.935216058));
#295056=CARTESIAN_POINT('Ctrl Pts',(-1.93282005500006,11.6,-10.935216058));
#295057=CARTESIAN_POINT('Ctrl Pts',(-1.93112698400005,15.2,-10.932446266));
#295058=CARTESIAN_POINT('Ctrl Pts',(-1.93112698400005,11.6,-10.932446266));
#295059=CARTESIAN_POINT('Ctrl Pts',(-1.92943877200005,15.2,-10.929679446));
#295060=CARTESIAN_POINT('Ctrl Pts',(-1.92943877200005,11.6,-10.929679446));
#295061=CARTESIAN_POINT('Ctrl Pts',(-1.92775541900006,15.2,-10.92691561));
#295062=CARTESIAN_POINT('Ctrl Pts',(-1.92775541900006,11.6,-10.92691561));
#295063=CARTESIAN_POINT('Ctrl Pts',(-1.92607692400005,15.2,-10.924154768));
#295064=CARTESIAN_POINT('Ctrl Pts',(-1.92607692400005,11.6,-10.924154768));
#295065=CARTESIAN_POINT('Ctrl Pts',(-1.92440328400005,15.2,-10.921396933));
#295066=CARTESIAN_POINT('Ctrl Pts',(-1.92440328400005,11.6,-10.921396933));
#295067=CARTESIAN_POINT('Ctrl Pts',(-1.92273449900005,15.2,-10.918642115));
#295068=CARTESIAN_POINT('Ctrl Pts',(-1.92273449900005,11.6,-10.918642115));
#295069=CARTESIAN_POINT('Ctrl Pts',(-1.92107056600005,15.2,-10.915890324));
#295070=CARTESIAN_POINT('Ctrl Pts',(-1.92107056600005,11.6,-10.915890324));
#295071=CARTESIAN_POINT('Ctrl Pts',(-1.91941148400006,15.2,-10.913141573));
#295072=CARTESIAN_POINT('Ctrl Pts',(-1.91941148400006,11.6,-10.913141573));
#295073=CARTESIAN_POINT('Ctrl Pts',(-1.91775725300006,15.2,-10.910395872));
#295074=CARTESIAN_POINT('Ctrl Pts',(-1.91775725300006,11.6,-10.910395872));
#295075=CARTESIAN_POINT('Ctrl Pts',(-1.91610787000006,15.2,-10.907653232));
#295076=CARTESIAN_POINT('Ctrl Pts',(-1.91610787000006,11.6,-10.907653232));
#295077=CARTESIAN_POINT('Ctrl Pts',(-1.91446333500006,15.2,-10.904913664));
#295078=CARTESIAN_POINT('Ctrl Pts',(-1.91446333500006,11.6,-10.904913664));
#295079=CARTESIAN_POINT('Ctrl Pts',(-1.91282364500006,15.2,-10.902177181));
#295080=CARTESIAN_POINT('Ctrl Pts',(-1.91282364500006,11.6,-10.902177181));
#295081=CARTESIAN_POINT('Ctrl Pts',(-1.91118879900006,15.2,-10.899443792));
#295082=CARTESIAN_POINT('Ctrl Pts',(-1.91118879900006,11.6,-10.899443792));
#295083=CARTESIAN_POINT('Ctrl Pts',(-1.90955879600006,15.2,-10.89671351));
#295084=CARTESIAN_POINT('Ctrl Pts',(-1.90955879600006,11.6,-10.89671351));
#295085=CARTESIAN_POINT('Ctrl Pts',(-1.90793363400006,15.2,-10.893986344));
#295086=CARTESIAN_POINT('Ctrl Pts',(-1.90793363400006,11.6,-10.893986344));
#295087=CARTESIAN_POINT('Ctrl Pts',(-1.90631331200006,15.2,-10.891262307));
#295088=CARTESIAN_POINT('Ctrl Pts',(-1.90631331200006,11.6,-10.891262307));
#295089=CARTESIAN_POINT('Ctrl Pts',(-1.90469782800006,15.2,-10.888541409));
#295090=CARTESIAN_POINT('Ctrl Pts',(-1.90469782800006,11.6,-10.888541409));
#295091=CARTESIAN_POINT('Ctrl Pts',(-1.90308718100006,15.2,-10.885823664));
#295092=CARTESIAN_POINT('Ctrl Pts',(-1.90308718100006,11.6,-10.885823664));
#295093=CARTESIAN_POINT('Ctrl Pts',(-1.90148136800006,15.2,-10.88310908));
#295094=CARTESIAN_POINT('Ctrl Pts',(-1.90148136800006,11.6,-10.88310908));
#295095=CARTESIAN_POINT('Ctrl Pts',(-1.89988038900006,15.2,-10.880397671));
#295096=CARTESIAN_POINT('Ctrl Pts',(-1.89988038900006,11.6,-10.880397671));
#295097=CARTESIAN_POINT('Ctrl Pts',(-1.89828424200006,15.2,-10.877689446));
#295098=CARTESIAN_POINT('Ctrl Pts',(-1.89828424200006,11.6,-10.877689446));
#295099=CARTESIAN_POINT('Ctrl Pts',(-1.89669292500006,15.2,-10.874984418));
#295100=CARTESIAN_POINT('Ctrl Pts',(-1.89669292500006,11.6,-10.874984418));
#295101=CARTESIAN_POINT('Ctrl Pts',(-1.89510643700005,15.2,-10.872282597));
#295102=CARTESIAN_POINT('Ctrl Pts',(-1.89510643700005,11.6,-10.872282597));
#295103=CARTESIAN_POINT('Ctrl Pts',(-1.89352477600006,15.2,-10.869583997));
#295104=CARTESIAN_POINT('Ctrl Pts',(-1.89352477600006,11.6,-10.869583997));
#295105=CARTESIAN_POINT('Ctrl Pts',(-1.89194794100006,15.2,-10.866888627));
#295106=CARTESIAN_POINT('Ctrl Pts',(-1.89194794100006,11.6,-10.866888627));
#295107=CARTESIAN_POINT('Ctrl Pts',(-1.89037592900006,15.2,-10.8641965));
#295108=CARTESIAN_POINT('Ctrl Pts',(-1.89037592900006,11.6,-10.8641965));
#295109=CARTESIAN_POINT('Ctrl Pts',(-1.88880874000006,15.2,-10.861507626));
#295110=CARTESIAN_POINT('Ctrl Pts',(-1.88880874000006,11.6,-10.861507626));
#295111=CARTESIAN_POINT('Ctrl Pts',(-1.88724637200006,15.2,-10.858822018));
#295112=CARTESIAN_POINT('Ctrl Pts',(-1.88724637200006,11.6,-10.858822018));
#295113=CARTESIAN_POINT('Ctrl Pts',(-1.88568882100005,15.2,-10.856139687));
#295114=CARTESIAN_POINT('Ctrl Pts',(-1.88568882100005,11.6,-10.856139687));
#295115=CARTESIAN_POINT('Ctrl Pts',(-1.88413608800006,15.2,-10.853460644));
#295116=CARTESIAN_POINT('Ctrl Pts',(-1.88413608800006,11.6,-10.853460644));
#295117=CARTESIAN_POINT('Ctrl Pts',(-1.88258817100006,15.2,-10.850784903));
#295118=CARTESIAN_POINT('Ctrl Pts',(-1.88258817100006,11.6,-10.850784903));
#295119=CARTESIAN_POINT('Ctrl Pts',(-1.88104506800005,15.2,-10.848112472));
#295120=CARTESIAN_POINT('Ctrl Pts',(-1.88104506800005,11.6,-10.848112472));
#295121=CARTESIAN_POINT('Ctrl Pts',(-1.87950677700006,15.2,-10.845443365));
#295122=CARTESIAN_POINT('Ctrl Pts',(-1.87950677700006,11.6,-10.845443365));
#295123=CARTESIAN_POINT('Ctrl Pts',(-1.87797329500006,15.2,-10.842777593));
#295124=CARTESIAN_POINT('Ctrl Pts',(-1.87797329500006,11.6,-10.842777593));
#295125=CARTESIAN_POINT('Ctrl Pts',(-1.87644462200006,15.2,-10.840115167));
#295126=CARTESIAN_POINT('Ctrl Pts',(-1.87644462200006,11.6,-10.840115167));
#295127=CARTESIAN_POINT('Ctrl Pts',(-1.87492075700006,15.2,-10.837456101));
#295128=CARTESIAN_POINT('Ctrl Pts',(-1.87492075700006,11.6,-10.837456101));
#295129=CARTESIAN_POINT('Ctrl Pts',(-1.87340169600006,15.2,-10.834800405));
#295130=CARTESIAN_POINT('Ctrl Pts',(-1.87340169600006,11.6,-10.834800405));
#295131=CARTESIAN_POINT('Ctrl Pts',(-1.87188743800006,15.2,-10.832148091));
#295132=CARTESIAN_POINT('Ctrl Pts',(-1.87188743800006,11.6,-10.832148091));
#295133=CARTESIAN_POINT('Ctrl Pts',(-1.87037798200006,15.2,-10.829499171));
#295134=CARTESIAN_POINT('Ctrl Pts',(-1.87037798200006,11.6,-10.829499171));
#295135=CARTESIAN_POINT('Ctrl Pts',(-1.86887332500006,15.2,-10.826853656));
#295136=CARTESIAN_POINT('Ctrl Pts',(-1.86887332500006,11.6,-10.826853656));
#295137=CARTESIAN_POINT('Ctrl Pts',(-1.86737346700005,15.2,-10.82421156));
#295138=CARTESIAN_POINT('Ctrl Pts',(-1.86737346700005,11.6,-10.82421156));
#295139=CARTESIAN_POINT('Ctrl Pts',(-1.86587840400006,15.2,-10.821572893));
#295140=CARTESIAN_POINT('Ctrl Pts',(-1.86587840400006,11.6,-10.821572893));
#295141=CARTESIAN_POINT('Ctrl Pts',(-1.86438813500006,15.2,-10.818937666));
#295142=CARTESIAN_POINT('Ctrl Pts',(-1.86438813500006,11.6,-10.818937666));
#295143=CARTESIAN_POINT('Ctrl Pts',(-1.86290265800006,15.2,-10.816305894));
#295144=CARTESIAN_POINT('Ctrl Pts',(-1.86290265800006,11.6,-10.816305894));
#295145=CARTESIAN_POINT('Ctrl Pts',(-1.86142197200006,15.2,-10.813677586));
#295146=CARTESIAN_POINT('Ctrl Pts',(-1.86142197200006,11.6,-10.813677586));
#295147=CARTESIAN_POINT('Ctrl Pts',(-1.85994607300006,15.2,-10.811052755));
#295148=CARTESIAN_POINT('Ctrl Pts',(-1.85994607300006,11.6,-10.811052755));
#295149=CARTESIAN_POINT('Ctrl Pts',(-1.85847496200006,15.2,-10.808431414));
#295150=CARTESIAN_POINT('Ctrl Pts',(-1.85847496200006,11.6,-10.808431414));
#295151=CARTESIAN_POINT('Ctrl Pts',(-1.85700863500006,15.2,-10.805813575));
#295152=CARTESIAN_POINT('Ctrl Pts',(-1.85700863500006,11.6,-10.805813575));
#295153=CARTESIAN_POINT('Ctrl Pts',(-1.85554709100006,15.2,-10.803199248));
#295154=CARTESIAN_POINT('Ctrl Pts',(-1.85554709100006,11.6,-10.803199248));
#295155=CARTESIAN_POINT('Ctrl Pts',(-1.85409032800006,15.2,-10.800588447));
#295156=CARTESIAN_POINT('Ctrl Pts',(-1.85409032800006,11.6,-10.800588447));
#295157=CARTESIAN_POINT('Ctrl Pts',(-1.85263834300006,15.2,-10.797981184));
#295158=CARTESIAN_POINT('Ctrl Pts',(-1.85263834300006,11.6,-10.797981184));
#295159=CARTESIAN_POINT('Ctrl Pts',(-1.85119113400006,15.2,-10.795377469));
#295160=CARTESIAN_POINT('Ctrl Pts',(-1.85119113400006,11.6,-10.795377469));
#295161=CARTESIAN_POINT('Ctrl Pts',(-1.84974870200006,15.2,-10.792777317));
#295162=CARTESIAN_POINT('Ctrl Pts',(-1.84974870200006,11.6,-10.792777317));
#295163=CARTESIAN_POINT('Ctrl Pts',(-1.84831104100006,15.2,-10.790180739));
#295164=CARTESIAN_POINT('Ctrl Pts',(-1.84831104100006,11.6,-10.790180739));
#295165=CARTESIAN_POINT('Ctrl Pts',(-1.84687815100005,15.2,-10.787587746));
#295166=CARTESIAN_POINT('Ctrl Pts',(-1.84687815100005,11.6,-10.787587746));
#295167=CARTESIAN_POINT('Ctrl Pts',(-1.84545003000005,15.2,-10.784998353));
#295168=CARTESIAN_POINT('Ctrl Pts',(-1.84545003000005,11.6,-10.784998353));
#295169=CARTESIAN_POINT('Ctrl Pts',(-1.84402667500006,15.2,-10.78241257));
#295170=CARTESIAN_POINT('Ctrl Pts',(-1.84402667500006,11.6,-10.78241257));
#295171=CARTESIAN_POINT('Ctrl Pts',(-1.84260808600006,15.2,-10.77983041));
#295172=CARTESIAN_POINT('Ctrl Pts',(-1.84260808600006,11.6,-10.77983041));
#295173=CARTESIAN_POINT('Ctrl Pts',(-1.84119425800006,15.2,-10.777251885));
#295174=CARTESIAN_POINT('Ctrl Pts',(-1.84119425800006,11.6,-10.777251885));
#295175=CARTESIAN_POINT('Ctrl Pts',(-1.83978519200006,15.2,-10.774677008));
#295176=CARTESIAN_POINT('Ctrl Pts',(-1.83978519200006,11.6,-10.774677008));
#295177=CARTESIAN_POINT('Ctrl Pts',(-1.83838088300006,15.2,-10.77210579));
#295178=CARTESIAN_POINT('Ctrl Pts',(-1.83838088300006,11.6,-10.77210579));
#295179=CARTESIAN_POINT('Ctrl Pts',(-1.83698133100005,15.2,-10.769538245));
#295180=CARTESIAN_POINT('Ctrl Pts',(-1.83698133100005,11.6,-10.769538245));
#295181=CARTESIAN_POINT('Ctrl Pts',(-1.83558653300006,15.2,-10.766974386));
#295182=CARTESIAN_POINT('Ctrl Pts',(-1.83558653300006,11.6,-10.766974386));
#295183=CARTESIAN_POINT('Ctrl Pts',(-1.83419648600006,15.2,-10.764414223));
#295184=CARTESIAN_POINT('Ctrl Pts',(-1.83419648600006,11.6,-10.764414223));
#295185=CARTESIAN_POINT('Ctrl Pts',(-1.83281119000006,15.2,-10.76185777));
#295186=CARTESIAN_POINT('Ctrl Pts',(-1.83281119000006,11.6,-10.76185777));
#295187=CARTESIAN_POINT('Ctrl Pts',(-1.83143064100005,15.2,-10.759305039));
#295188=CARTESIAN_POINT('Ctrl Pts',(-1.83143064100005,11.6,-10.759305039));
#295189=CARTESIAN_POINT('Ctrl Pts',(-1.83005483700006,15.2,-10.756756043));
#295190=CARTESIAN_POINT('Ctrl Pts',(-1.83005483700006,11.6,-10.756756043));
#295191=CARTESIAN_POINT('Ctrl Pts',(-1.82868377600006,15.2,-10.754210794));
#295192=CARTESIAN_POINT('Ctrl Pts',(-1.82868377600006,11.6,-10.754210794));
#295193=CARTESIAN_POINT('Ctrl Pts',(-1.82731745700006,15.2,-10.751669306));
#295194=CARTESIAN_POINT('Ctrl Pts',(-1.82731745700006,11.6,-10.751669306));
#295195=CARTESIAN_POINT('Ctrl Pts',(-1.82595587600006,15.2,-10.749131589));
#295196=CARTESIAN_POINT('Ctrl Pts',(-1.82595587600006,11.6,-10.749131589));
#295197=CARTESIAN_POINT('Ctrl Pts',(-1.82459903200006,15.2,-10.746597658));
#295198=CARTESIAN_POINT('Ctrl Pts',(-1.82459903200006,11.6,-10.746597658));
#295199=CARTESIAN_POINT('Ctrl Pts',(-1.82324692200006,15.2,-10.744067526));
#295200=CARTESIAN_POINT('Ctrl Pts',(-1.82324692200006,11.6,-10.744067526));
#295201=CARTESIAN_POINT('Ctrl Pts',(-1.82189954400006,15.2,-10.741541203));
#295202=CARTESIAN_POINT('Ctrl Pts',(-1.82189954400006,11.6,-10.741541203));
#295203=CARTESIAN_POINT('Ctrl Pts',(-1.82055689600006,15.2,-10.739018703));
#295204=CARTESIAN_POINT('Ctrl Pts',(-1.82055689600006,11.6,-10.739018703));
#295205=CARTESIAN_POINT('Ctrl Pts',(-1.81921897500006,15.2,-10.73650004));
#295206=CARTESIAN_POINT('Ctrl Pts',(-1.81921897500006,11.6,-10.73650004));
#295207=CARTESIAN_POINT('Ctrl Pts',(-1.81788577800006,15.2,-10.733985227));
#295208=CARTESIAN_POINT('Ctrl Pts',(-1.81788577800006,11.6,-10.733985227));
#295209=CARTESIAN_POINT('Ctrl Pts',(-1.81655730500006,15.2,-10.731474274));
#295210=CARTESIAN_POINT('Ctrl Pts',(-1.81655730500006,11.6,-10.731474274));
#295211=CARTESIAN_POINT('Ctrl Pts',(-1.81523355200006,15.2,-10.728967196));
#295212=CARTESIAN_POINT('Ctrl Pts',(-1.81523355200006,11.6,-10.728967196));
#295213=CARTESIAN_POINT('Ctrl Pts',(-1.81391451700006,15.2,-10.726464005));
#295214=CARTESIAN_POINT('Ctrl Pts',(-1.81391451700006,11.6,-10.726464005));
#295215=CARTESIAN_POINT('Ctrl Pts',(-1.81260019800006,15.2,-10.723964715));
#295216=CARTESIAN_POINT('Ctrl Pts',(-1.81260019800006,11.6,-10.723964715));
#295217=CARTESIAN_POINT('Ctrl Pts',(-1.81129059100006,15.2,-10.721469338));
#295218=CARTESIAN_POINT('Ctrl Pts',(-1.81129059100006,11.6,-10.721469338));
#295219=CARTESIAN_POINT('Ctrl Pts',(-1.80998569500006,15.2,-10.718977888));
#295220=CARTESIAN_POINT('Ctrl Pts',(-1.80998569500006,11.6,-10.718977888));
#295221=CARTESIAN_POINT('Ctrl Pts',(-1.80868550800006,15.2,-10.716490376));
#295222=CARTESIAN_POINT('Ctrl Pts',(-1.80868550800006,11.6,-10.716490376));
#295223=CARTESIAN_POINT('Ctrl Pts',(-1.80739002700005,15.2,-10.714006817));
#295224=CARTESIAN_POINT('Ctrl Pts',(-1.80739002700005,11.6,-10.714006817));
#295225=CARTESIAN_POINT('Ctrl Pts',(-1.80609924900006,15.2,-10.711527223));
#295226=CARTESIAN_POINT('Ctrl Pts',(-1.80609924900006,11.6,-10.711527223));
#295227=CARTESIAN_POINT('Ctrl Pts',(-1.80481317200006,15.2,-10.709051608));
#295228=CARTESIAN_POINT('Ctrl Pts',(-1.80481317200006,11.6,-10.709051608));
#295229=CARTESIAN_POINT('Ctrl Pts',(-1.80353179300006,15.2,-10.706579983));
#295230=CARTESIAN_POINT('Ctrl Pts',(-1.80353179300006,11.6,-10.706579983));
#295231=CARTESIAN_POINT('Ctrl Pts',(-1.80225511100006,15.2,-10.704112363));
#295232=CARTESIAN_POINT('Ctrl Pts',(-1.80225511100006,11.6,-10.704112363));
#295233=CARTESIAN_POINT('Ctrl Pts',(-1.80098312100006,15.2,-10.701648762));
#295234=CARTESIAN_POINT('Ctrl Pts',(-1.80098312100006,11.6,-10.701648762));
#295235=CARTESIAN_POINT('Ctrl Pts',(-1.79971582300006,15.2,-10.699189192));
#295236=CARTESIAN_POINT('Ctrl Pts',(-1.79971582300006,11.6,-10.699189192));
#295237=CARTESIAN_POINT('Ctrl Pts',(-1.79845321300005,15.2,-10.696733666));
#295238=CARTESIAN_POINT('Ctrl Pts',(-1.79845321300005,11.6,-10.696733666));
#295239=CARTESIAN_POINT('Ctrl Pts',(-1.79719528800006,15.2,-10.694282196));
#295240=CARTESIAN_POINT('Ctrl Pts',(-1.79719528800006,11.6,-10.694282196));
#295241=CARTESIAN_POINT('Ctrl Pts',(-1.79594204700006,15.2,-10.691834799));
#295242=CARTESIAN_POINT('Ctrl Pts',(-1.79594204700006,11.6,-10.691834799));
#295243=CARTESIAN_POINT('Ctrl Pts',(-1.79469348600006,15.2,-10.689391486));
#295244=CARTESIAN_POINT('Ctrl Pts',(-1.79469348600006,11.6,-10.689391486));
#295245=CARTESIAN_POINT('Ctrl Pts',(-1.79344960300006,15.2,-10.686952269));
#295246=CARTESIAN_POINT('Ctrl Pts',(-1.79344960300006,11.6,-10.686952269));
#295247=CARTESIAN_POINT('Ctrl Pts',(-1.79221039500006,15.2,-10.684517164));
#295248=CARTESIAN_POINT('Ctrl Pts',(-1.79221039500006,11.6,-10.684517164));
#295249=CARTESIAN_POINT('Ctrl Pts',(-1.79097586000006,15.2,-10.682086183));
#295250=CARTESIAN_POINT('Ctrl Pts',(-1.79097586000006,11.6,-10.682086183));
#295251=CARTESIAN_POINT('Ctrl Pts',(-1.78974599400005,15.2,-10.67965934));
#295252=CARTESIAN_POINT('Ctrl Pts',(-1.78974599400005,11.6,-10.67965934));
#295253=CARTESIAN_POINT('Ctrl Pts',(-1.78852079600006,15.2,-10.677236648));
#295254=CARTESIAN_POINT('Ctrl Pts',(-1.78852079600006,11.6,-10.677236648));
#295255=CARTESIAN_POINT('Ctrl Pts',(-1.78730026300005,15.2,-10.674818122));
#295256=CARTESIAN_POINT('Ctrl Pts',(-1.78730026300005,11.6,-10.674818122));
#295257=CARTESIAN_POINT('Ctrl Pts',(-1.78608439100006,15.2,-10.672403774));
#295258=CARTESIAN_POINT('Ctrl Pts',(-1.78608439100006,11.6,-10.672403774));
#295259=CARTESIAN_POINT('Ctrl Pts',(-1.78487317800006,15.2,-10.669993617));
#295260=CARTESIAN_POINT('Ctrl Pts',(-1.78487317800006,11.6,-10.669993617));
#295261=CARTESIAN_POINT('Ctrl Pts',(-1.78366662300005,15.2,-10.667587667));
#295262=CARTESIAN_POINT('Ctrl Pts',(-1.78366662300005,11.6,-10.667587667));
#295263=CARTESIAN_POINT('Ctrl Pts',(-1.78246472000006,15.2,-10.665185935));
#295264=CARTESIAN_POINT('Ctrl Pts',(-1.78246472000006,11.6,-10.665185935));
#295265=CARTESIAN_POINT('Ctrl Pts',(-1.78126746700006,15.2,-10.662788437));
#295266=CARTESIAN_POINT('Ctrl Pts',(-1.78126746700006,11.6,-10.662788437));
#295267=CARTESIAN_POINT('Ctrl Pts',(-1.78007486300006,15.2,-10.660395184));
#295268=CARTESIAN_POINT('Ctrl Pts',(-1.78007486300006,11.6,-10.660395184));
#295269=CARTESIAN_POINT('Ctrl Pts',(-1.77888690400006,15.2,-10.658006194));
#295270=CARTESIAN_POINT('Ctrl Pts',(-1.77888690400006,11.6,-10.658006194));
#295271=CARTESIAN_POINT('Ctrl Pts',(-1.77770358700006,15.2,-10.655621476));
#295272=CARTESIAN_POINT('Ctrl Pts',(-1.77770358700006,11.6,-10.655621476));
#295273=CARTESIAN_POINT('Ctrl Pts',(-1.77652491000006,15.2,-10.653241047));
#295274=CARTESIAN_POINT('Ctrl Pts',(-1.77652491000006,11.6,-10.653241047));
#295275=CARTESIAN_POINT('Ctrl Pts',(-1.77535086900006,15.2,-10.65086492));
#295276=CARTESIAN_POINT('Ctrl Pts',(-1.77535086900006,11.6,-10.65086492));
#295277=CARTESIAN_POINT('Ctrl Pts',(-1.77418146100006,15.2,-10.648493108));
#295278=CARTESIAN_POINT('Ctrl Pts',(-1.77418146100006,11.6,-10.648493108));
#295279=CARTESIAN_POINT('Ctrl Pts',(-1.77301668500006,15.2,-10.646125627));
#295280=CARTESIAN_POINT('Ctrl Pts',(-1.77301668500006,11.6,-10.646125627));
#295281=CARTESIAN_POINT('Ctrl Pts',(-1.77185653500006,15.2,-10.643762488));
#295282=CARTESIAN_POINT('Ctrl Pts',(-1.77185653500006,11.6,-10.643762488));
#295283=CARTESIAN_POINT('Ctrl Pts',(-1.77070101200006,15.2,-10.641403708));
#295284=CARTESIAN_POINT('Ctrl Pts',(-1.77070101200006,11.6,-10.641403708));
#295285=CARTESIAN_POINT('Ctrl Pts',(-1.76955010900006,15.2,-10.639049299));
#295286=CARTESIAN_POINT('Ctrl Pts',(-1.76955010900006,11.6,-10.639049299));
#295287=CARTESIAN_POINT('Ctrl Pts',(-1.76840382600005,15.2,-10.636699276));
#295288=CARTESIAN_POINT('Ctrl Pts',(-1.76840382600005,11.6,-10.636699276));
#295289=CARTESIAN_POINT('Ctrl Pts',(-1.76726215900006,15.2,-10.634353653));
#295290=CARTESIAN_POINT('Ctrl Pts',(-1.76726215900006,11.6,-10.634353653));
#295291=CARTESIAN_POINT('Ctrl Pts',(-1.76612510400005,15.2,-10.632012444));
#295292=CARTESIAN_POINT('Ctrl Pts',(-1.76612510400005,11.6,-10.632012444));
#295293=CARTESIAN_POINT('Ctrl Pts',(-1.76499265900006,15.2,-10.629675663));
#295294=CARTESIAN_POINT('Ctrl Pts',(-1.76499265900006,11.6,-10.629675663));
#295295=CARTESIAN_POINT('Ctrl Pts',(-1.76386482100006,15.2,-10.627343324));
#295296=CARTESIAN_POINT('Ctrl Pts',(-1.76386482100006,11.6,-10.627343324));
#295297=CARTESIAN_POINT('Ctrl Pts',(-1.76274158600006,15.2,-10.625015442));
#295298=CARTESIAN_POINT('Ctrl Pts',(-1.76274158600006,11.6,-10.625015442));
#295299=CARTESIAN_POINT('Ctrl Pts',(-1.76162295200006,15.2,-10.622692031));
#295300=CARTESIAN_POINT('Ctrl Pts',(-1.76162295200006,11.6,-10.622692031));
#295301=CARTESIAN_POINT('Ctrl Pts',(-1.76050891600006,15.2,-10.620373104));
#295302=CARTESIAN_POINT('Ctrl Pts',(-1.76050891600006,11.6,-10.620373104));
#295303=CARTESIAN_POINT('Ctrl Pts',(-1.75939947300006,15.2,-10.618058678));
#295304=CARTESIAN_POINT('Ctrl Pts',(-1.75939947300006,11.6,-10.618058678));
#295305=CARTESIAN_POINT('Ctrl Pts',(-1.75829462200006,15.2,-10.615748764));
#295306=CARTESIAN_POINT('Ctrl Pts',(-1.75829462200006,11.6,-10.615748764));
#295307=CARTESIAN_POINT('Ctrl Pts',(-1.75719435900006,15.2,-10.61344338));
#295308=CARTESIAN_POINT('Ctrl Pts',(-1.75719435900006,11.6,-10.61344338));
#295309=CARTESIAN_POINT('Ctrl Pts',(-1.75609868000006,15.2,-10.611142538));
#295310=CARTESIAN_POINT('Ctrl Pts',(-1.75609868000006,11.6,-10.611142538));
#295311=CARTESIAN_POINT('Ctrl Pts',(-1.75500758400006,15.2,-10.608846253));
#295312=CARTESIAN_POINT('Ctrl Pts',(-1.75500758400006,11.6,-10.608846253));
#295313=CARTESIAN_POINT('Ctrl Pts',(-1.75392106600006,15.2,-10.60655454));
#295314=CARTESIAN_POINT('Ctrl Pts',(-1.75392106600006,11.6,-10.60655454));
#295315=CARTESIAN_POINT('Ctrl Pts',(-1.75283912300006,15.2,-10.604267414));
#295316=CARTESIAN_POINT('Ctrl Pts',(-1.75283912300006,11.6,-10.604267414));
#295317=CARTESIAN_POINT('Ctrl Pts',(-1.75176175100006,15.2,-10.601984888));
#295318=CARTESIAN_POINT('Ctrl Pts',(-1.75176175100006,11.6,-10.601984888));
#295319=CARTESIAN_POINT('Ctrl Pts',(-1.75068894900006,15.2,-10.599706978));
#295320=CARTESIAN_POINT('Ctrl Pts',(-1.75068894900006,11.6,-10.599706978));
#295321=CARTESIAN_POINT('Ctrl Pts',(-1.74962071200006,15.2,-10.597433698));
#295322=CARTESIAN_POINT('Ctrl Pts',(-1.74962071200006,11.6,-10.597433698));
#295323=CARTESIAN_POINT('Ctrl Pts',(-1.74855703600006,15.2,-10.595165063));
#295324=CARTESIAN_POINT('Ctrl Pts',(-1.74855703600006,11.6,-10.595165063));
#295325=CARTESIAN_POINT('Ctrl Pts',(-1.74749792000006,15.2,-10.592901087));
#295326=CARTESIAN_POINT('Ctrl Pts',(-1.74749792000006,11.6,-10.592901087));
#295327=CARTESIAN_POINT('Ctrl Pts',(-1.74644335700005,15.2,-10.590641786));
#295328=CARTESIAN_POINT('Ctrl Pts',(-1.74644335700005,11.6,-10.590641786));
#295329=CARTESIAN_POINT('Ctrl Pts',(-1.74539334800006,15.2,-10.588387175));
#295330=CARTESIAN_POINT('Ctrl Pts',(-1.74539334800006,11.6,-10.588387175));
#295331=CARTESIAN_POINT('Ctrl Pts',(-1.74434788700006,15.2,-10.586137267));
#295332=CARTESIAN_POINT('Ctrl Pts',(-1.74434788700006,11.6,-10.586137267));
#295333=CARTESIAN_POINT('Ctrl Pts',(-1.74330697100005,15.2,-10.58389208));
#295334=CARTESIAN_POINT('Ctrl Pts',(-1.74330697100005,11.6,-10.58389208));
#295335=CARTESIAN_POINT('Ctrl Pts',(-1.74227059600006,15.2,-10.581651626));
#295336=CARTESIAN_POINT('Ctrl Pts',(-1.74227059600006,11.6,-10.581651626));
#295337=CARTESIAN_POINT('Ctrl Pts',(-1.74123875900006,15.2,-10.57941592));
#295338=CARTESIAN_POINT('Ctrl Pts',(-1.74123875900006,11.6,-10.57941592));
#295339=CARTESIAN_POINT('Ctrl Pts',(-1.74021145800005,15.2,-10.577184979));
#295340=CARTESIAN_POINT('Ctrl Pts',(-1.74021145800005,11.6,-10.577184979));
#295341=CARTESIAN_POINT('Ctrl Pts',(-1.73918868600006,15.2,-10.574958817));
#295342=CARTESIAN_POINT('Ctrl Pts',(-1.73918868600006,11.6,-10.574958817));
#295343=CARTESIAN_POINT('Ctrl Pts',(-1.73817044300006,15.2,-10.572737449));
#295344=CARTESIAN_POINT('Ctrl Pts',(-1.73817044300006,11.6,-10.572737449));
#295345=CARTESIAN_POINT('Ctrl Pts',(-1.73715672500005,15.2,-10.570520891));
#295346=CARTESIAN_POINT('Ctrl Pts',(-1.73715672500005,11.6,-10.570520891));
#295347=CARTESIAN_POINT('Ctrl Pts',(-1.73614752700006,15.2,-10.568309157));
#295348=CARTESIAN_POINT('Ctrl Pts',(-1.73614752700006,11.6,-10.568309157));
#295349=CARTESIAN_POINT('Ctrl Pts',(-1.73514284500006,15.2,-10.566102263));
#295350=CARTESIAN_POINT('Ctrl Pts',(-1.73514284500006,11.6,-10.566102263));
#295351=CARTESIAN_POINT('Ctrl Pts',(-1.73414267600006,15.2,-10.563900224));
#295352=CARTESIAN_POINT('Ctrl Pts',(-1.73414267600006,11.6,-10.563900224));
#295353=CARTESIAN_POINT('Ctrl Pts',(-1.73314701900006,15.2,-10.561703056));
#295354=CARTESIAN_POINT('Ctrl Pts',(-1.73314701900006,11.6,-10.561703056));
#295355=CARTESIAN_POINT('Ctrl Pts',(-1.73215586600006,15.2,-10.559510773));
#295356=CARTESIAN_POINT('Ctrl Pts',(-1.73215586600006,11.6,-10.559510773));
#295357=CARTESIAN_POINT('Ctrl Pts',(-1.73116921600006,15.2,-10.55732339));
#295358=CARTESIAN_POINT('Ctrl Pts',(-1.73116921600006,11.6,-10.55732339));
#295359=CARTESIAN_POINT('Ctrl Pts',(-1.73018706500006,15.2,-10.555140925));
#295360=CARTESIAN_POINT('Ctrl Pts',(-1.73018706500006,11.6,-10.555140925));
#295361=CARTESIAN_POINT('Ctrl Pts',(-1.72920940800006,15.2,-10.552963391));
#295362=CARTESIAN_POINT('Ctrl Pts',(-1.72920940800006,11.6,-10.552963391));
#295363=CARTESIAN_POINT('Ctrl Pts',(-1.72823624300006,15.2,-10.550790805));
#295364=CARTESIAN_POINT('Ctrl Pts',(-1.72823624300006,11.6,-10.550790805));
#295365=CARTESIAN_POINT('Ctrl Pts',(-1.72726756600006,15.2,-10.548623183));
#295366=CARTESIAN_POINT('Ctrl Pts',(-1.72726756600006,11.6,-10.548623183));
#295367=CARTESIAN_POINT('Ctrl Pts',(-1.72630337200005,15.2,-10.546460538));
#295368=CARTESIAN_POINT('Ctrl Pts',(-1.72630337200005,11.6,-10.546460538));
#295369=CARTESIAN_POINT('Ctrl Pts',(-1.72534365800006,15.2,-10.544302889));
#295370=CARTESIAN_POINT('Ctrl Pts',(-1.72534365800006,11.6,-10.544302889));
#295371=CARTESIAN_POINT('Ctrl Pts',(-1.72438842000005,15.2,-10.542150249));
#295372=CARTESIAN_POINT('Ctrl Pts',(-1.72438842000005,11.6,-10.542150249));
#295373=CARTESIAN_POINT('Ctrl Pts',(-1.72343765400006,15.2,-10.540002635));
#295374=CARTESIAN_POINT('Ctrl Pts',(-1.72343765400006,11.6,-10.540002635));
#295375=CARTESIAN_POINT('Ctrl Pts',(-1.72249135800006,15.2,-10.537860062));
#295376=CARTESIAN_POINT('Ctrl Pts',(-1.72249135800006,11.6,-10.537860062));
#295377=CARTESIAN_POINT('Ctrl Pts',(-1.72154952600006,15.2,-10.535722547));
#295378=CARTESIAN_POINT('Ctrl Pts',(-1.72154952600006,11.6,-10.535722547));
#295379=CARTESIAN_POINT('Ctrl Pts',(-1.72061215300006,15.2,-10.533590105));
#295380=CARTESIAN_POINT('Ctrl Pts',(-1.72061215300006,11.6,-10.533590105));
#295381=CARTESIAN_POINT('Ctrl Pts',(-1.71967923800006,15.2,-10.531462752));
#295382=CARTESIAN_POINT('Ctrl Pts',(-1.71967923800006,11.6,-10.531462752));
#295383=CARTESIAN_POINT('Ctrl Pts',(-1.71875077600005,15.2,-10.529340504));
#295384=CARTESIAN_POINT('Ctrl Pts',(-1.71875077600005,11.6,-10.529340504));
#295385=CARTESIAN_POINT('Ctrl Pts',(-1.71782676200006,15.2,-10.527223376));
#295386=CARTESIAN_POINT('Ctrl Pts',(-1.71782676200006,11.6,-10.527223376));
#295387=CARTESIAN_POINT('Ctrl Pts',(-1.71690719200006,15.2,-10.525111386));
#295388=CARTESIAN_POINT('Ctrl Pts',(-1.71690719200006,11.6,-10.525111386));
#295389=CARTESIAN_POINT('Ctrl Pts',(-1.71599206400006,15.2,-10.523004549));
#295390=CARTESIAN_POINT('Ctrl Pts',(-1.71599206400006,11.6,-10.523004549));
#295391=CARTESIAN_POINT('Ctrl Pts',(-1.71508137200005,15.2,-10.520902882));
#295392=CARTESIAN_POINT('Ctrl Pts',(-1.71508137200005,11.6,-10.520902882));
#295393=CARTESIAN_POINT('Ctrl Pts',(-1.71417511300006,15.2,-10.5188064));
#295394=CARTESIAN_POINT('Ctrl Pts',(-1.71417511300006,11.6,-10.5188064));
#295395=CARTESIAN_POINT('Ctrl Pts',(-1.71327328300006,15.2,-10.516715119));
#295396=CARTESIAN_POINT('Ctrl Pts',(-1.71327328300006,11.6,-10.516715119));
#295397=CARTESIAN_POINT('Ctrl Pts',(-1.71237587800006,15.2,-10.514629056));
#295398=CARTESIAN_POINT('Ctrl Pts',(-1.71237587800006,11.6,-10.514629056));
#295399=CARTESIAN_POINT('Ctrl Pts',(-1.71148289100006,15.2,-10.512548228));
#295400=CARTESIAN_POINT('Ctrl Pts',(-1.71148289100006,11.6,-10.512548228));
#295401=CARTESIAN_POINT('Ctrl Pts',(-1.71059432200006,15.2,-10.510472651));
#295402=CARTESIAN_POINT('Ctrl Pts',(-1.71059432200006,11.6,-10.510472651));
#295403=CARTESIAN_POINT('Ctrl Pts',(-1.70971016400005,15.2,-10.50840234));
#295404=CARTESIAN_POINT('Ctrl Pts',(-1.70971016400005,11.6,-10.50840234));
#295405=CARTESIAN_POINT('Ctrl Pts',(-1.70883041500006,15.2,-10.506337312));
#295406=CARTESIAN_POINT('Ctrl Pts',(-1.70883041500006,11.6,-10.506337312));
#295407=CARTESIAN_POINT('Ctrl Pts',(-1.70795506800005,15.2,-10.504277584));
#295408=CARTESIAN_POINT('Ctrl Pts',(-1.70795506800005,11.6,-10.504277584));
#295409=CARTESIAN_POINT('Ctrl Pts',(-1.70708412100006,15.2,-10.502223174));
#295410=CARTESIAN_POINT('Ctrl Pts',(-1.70708412100006,11.6,-10.502223174));
#295411=CARTESIAN_POINT('Ctrl Pts',(-1.70621756900006,15.2,-10.500174096));
#295412=CARTESIAN_POINT('Ctrl Pts',(-1.70621756900006,11.6,-10.500174096));
#295413=CARTESIAN_POINT('Ctrl Pts',(-1.70535540700006,15.2,-10.498130368));
#295414=CARTESIAN_POINT('Ctrl Pts',(-1.70535540700006,11.6,-10.498130368));
#295415=CARTESIAN_POINT('Ctrl Pts',(-1.70449763200006,15.2,-10.496092006));
#295416=CARTESIAN_POINT('Ctrl Pts',(-1.70449763200006,11.6,-10.496092006));
#295417=CARTESIAN_POINT('Ctrl Pts',(-1.70364423900006,15.2,-10.494059027));
#295418=CARTESIAN_POINT('Ctrl Pts',(-1.70364423900006,11.6,-10.494059027));
#295419=CARTESIAN_POINT('Ctrl Pts',(-1.70279522300006,15.2,-10.492031449));
#295420=CARTESIAN_POINT('Ctrl Pts',(-1.70279522300006,11.6,-10.492031449));
#295421=CARTESIAN_POINT('Ctrl Pts',(-1.70195058100005,15.2,-10.490009287));
#295422=CARTESIAN_POINT('Ctrl Pts',(-1.70195058100005,11.6,-10.490009287));
#295423=CARTESIAN_POINT('Ctrl Pts',(-1.70111030700005,15.2,-10.487992559));
#295424=CARTESIAN_POINT('Ctrl Pts',(-1.70111030700005,11.6,-10.487992559));
#295425=CARTESIAN_POINT('Ctrl Pts',(-1.70027439800006,15.2,-10.485981281));
#295426=CARTESIAN_POINT('Ctrl Pts',(-1.70027439800006,11.6,-10.485981281));
#295427=CARTESIAN_POINT('Ctrl Pts',(-1.69944284900006,15.2,-10.483975472));
#295428=CARTESIAN_POINT('Ctrl Pts',(-1.69944284900006,11.6,-10.483975472));
#295429=CARTESIAN_POINT('Ctrl Pts',(-1.69861565500006,15.2,-10.481975146));
#295430=CARTESIAN_POINT('Ctrl Pts',(-1.69861565500006,11.6,-10.481975146));
#295431=CARTESIAN_POINT('Ctrl Pts',(-1.69779281100006,15.2,-10.479980323));
#295432=CARTESIAN_POINT('Ctrl Pts',(-1.69779281100006,11.6,-10.479980323));
#295433=CARTESIAN_POINT('Ctrl Pts',(-1.69697431500006,15.2,-10.477991019));
#295434=CARTESIAN_POINT('Ctrl Pts',(-1.69697431500006,11.6,-10.477991019));
#295435=CARTESIAN_POINT('Ctrl Pts',(-1.69616015900006,15.2,-10.476007249));
#295436=CARTESIAN_POINT('Ctrl Pts',(-1.69616015900006,11.6,-10.476007249));
#295437=CARTESIAN_POINT('Ctrl Pts',(-1.69535034100006,15.2,-10.474029034));
#295438=CARTESIAN_POINT('Ctrl Pts',(-1.69535034100006,11.6,-10.474029034));
#295439=CARTESIAN_POINT('Ctrl Pts',(-1.69454485500005,15.2,-10.47205639));
#295440=CARTESIAN_POINT('Ctrl Pts',(-1.69454485500005,11.6,-10.47205639));
#295441=CARTESIAN_POINT('Ctrl Pts',(-1.69374369700006,15.2,-10.470089332));
#295442=CARTESIAN_POINT('Ctrl Pts',(-1.69374369700006,11.6,-10.470089332));
#295443=CARTESIAN_POINT('Ctrl Pts',(-1.69294686200006,15.2,-10.468127881));
#295444=CARTESIAN_POINT('Ctrl Pts',(-1.69294686200006,11.6,-10.468127881));
#295445=CARTESIAN_POINT('Ctrl Pts',(-1.69215434600006,15.2,-10.466172052));
#295446=CARTESIAN_POINT('Ctrl Pts',(-1.69215434600006,11.6,-10.466172052));
#295447=CARTESIAN_POINT('Ctrl Pts',(-1.69136614300006,15.2,-10.464221864));
#295448=CARTESIAN_POINT('Ctrl Pts',(-1.69136614300006,11.6,-10.464221864));
#295449=CARTESIAN_POINT('Ctrl Pts',(-1.69058224900006,15.2,-10.462277333));
#295450=CARTESIAN_POINT('Ctrl Pts',(-1.69058224900006,11.6,-10.462277333));
#295451=CARTESIAN_POINT('Ctrl Pts',(-1.68980265900006,15.2,-10.460338479));
#295452=CARTESIAN_POINT('Ctrl Pts',(-1.68980265900006,11.6,-10.460338479));
#295453=CARTESIAN_POINT('Ctrl Pts',(-1.68902736900006,15.2,-10.458405316));
#295454=CARTESIAN_POINT('Ctrl Pts',(-1.68902736900006,11.6,-10.458405316));
#295455=CARTESIAN_POINT('Ctrl Pts',(-1.68825637300006,15.2,-10.456477865));
#295456=CARTESIAN_POINT('Ctrl Pts',(-1.68825637300006,11.6,-10.456477865));
#295457=CARTESIAN_POINT('Ctrl Pts',(-1.68748966700006,15.2,-10.454556142));
#295458=CARTESIAN_POINT('Ctrl Pts',(-1.68748966700006,11.6,-10.454556142));
#295459=CARTESIAN_POINT('Ctrl Pts',(-1.68672724500006,15.2,-10.452640166));
#295460=CARTESIAN_POINT('Ctrl Pts',(-1.68672724500006,11.6,-10.452640166));
#295461=CARTESIAN_POINT('Ctrl Pts',(-1.68596910300006,15.2,-10.450729954));
#295462=CARTESIAN_POINT('Ctrl Pts',(-1.68596910300006,11.6,-10.450729954));
#295463=CARTESIAN_POINT('Ctrl Pts',(-1.68521523600006,15.2,-10.448825525));
#295464=CARTESIAN_POINT('Ctrl Pts',(-1.68521523600006,11.6,-10.448825525));
#295465=CARTESIAN_POINT('Ctrl Pts',(-1.68446563900006,15.2,-10.446926896));
#295466=CARTESIAN_POINT('Ctrl Pts',(-1.68446563900006,11.6,-10.446926896));
#295467=CARTESIAN_POINT('Ctrl Pts',(-1.68372030600006,15.2,-10.445034085));
#295468=CARTESIAN_POINT('Ctrl Pts',(-1.68372030600006,11.6,-10.445034085));
#295469=CARTESIAN_POINT('Ctrl Pts',(-1.68297923400006,15.2,-10.44314711));
#295470=CARTESIAN_POINT('Ctrl Pts',(-1.68297923400006,11.6,-10.44314711));
#295471=CARTESIAN_POINT('Ctrl Pts',(-1.68224241500006,15.2,-10.44126599));
#295472=CARTESIAN_POINT('Ctrl Pts',(-1.68224241500006,11.6,-10.44126599));
#295473=CARTESIAN_POINT('Ctrl Pts',(-1.68150984700006,15.2,-10.439390743));
#295474=CARTESIAN_POINT('Ctrl Pts',(-1.68150984700006,11.6,-10.439390743));
#295475=CARTESIAN_POINT('Ctrl Pts',(-1.68078152300006,15.2,-10.437521386));
#295476=CARTESIAN_POINT('Ctrl Pts',(-1.68078152300006,11.6,-10.437521386));
#295477=CARTESIAN_POINT('Ctrl Pts',(-1.68005743900005,15.2,-10.435657939));
#295478=CARTESIAN_POINT('Ctrl Pts',(-1.68005743900005,11.6,-10.435657939));
#295479=CARTESIAN_POINT('Ctrl Pts',(-1.67933758800005,15.2,-10.433800421));
#295480=CARTESIAN_POINT('Ctrl Pts',(-1.67933758800005,11.6,-10.433800421));
#295481=CARTESIAN_POINT('Ctrl Pts',(-1.67862196700006,15.2,-10.431948849));
#295482=CARTESIAN_POINT('Ctrl Pts',(-1.67862196700006,11.6,-10.431948849));
#295483=CARTESIAN_POINT('Ctrl Pts',(-1.67791057000006,15.2,-10.430103241));
#295484=CARTESIAN_POINT('Ctrl Pts',(-1.67791057000006,11.6,-10.430103241));
#295485=CARTESIAN_POINT('Ctrl Pts',(-1.67720339000006,15.2,-10.428263616));
#295486=CARTESIAN_POINT('Ctrl Pts',(-1.67720339000006,11.6,-10.428263616));
#295487=CARTESIAN_POINT('Ctrl Pts',(-1.67650042400005,15.2,-10.426429993));
#295488=CARTESIAN_POINT('Ctrl Pts',(-1.67650042400005,11.6,-10.426429993));
#295489=CARTESIAN_POINT('Ctrl Pts',(-1.67580166700006,15.2,-10.424602391));
#295490=CARTESIAN_POINT('Ctrl Pts',(-1.67580166700006,11.6,-10.424602391));
#295491=CARTESIAN_POINT('Ctrl Pts',(-1.67510711100005,15.2,-10.422780829));
#295492=CARTESIAN_POINT('Ctrl Pts',(-1.67510711100005,11.6,-10.422780829));
#295493=CARTESIAN_POINT('Ctrl Pts',(-1.67441675200006,15.2,-10.420965325));
#295494=CARTESIAN_POINT('Ctrl Pts',(-1.67441675200006,11.6,-10.420965325));
#295495=CARTESIAN_POINT('Ctrl Pts',(-1.67373058500006,15.2,-10.419155897));
#295496=CARTESIAN_POINT('Ctrl Pts',(-1.67373058500006,11.6,-10.419155897));
#295497=CARTESIAN_POINT('Ctrl Pts',(-1.67304860500006,15.2,-10.417352566));
#295498=CARTESIAN_POINT('Ctrl Pts',(-1.67304860500006,11.6,-10.417352566));
#295499=CARTESIAN_POINT('Ctrl Pts',(-1.67237080500006,15.2,-10.41555535));
#295500=CARTESIAN_POINT('Ctrl Pts',(-1.67237080500006,11.6,-10.41555535));
#295501=CARTESIAN_POINT('Ctrl Pts',(-1.67169718000005,15.2,-10.413764268));
#295502=CARTESIAN_POINT('Ctrl Pts',(-1.67169718000005,11.6,-10.413764268));
#295503=CARTESIAN_POINT('Ctrl Pts',(-1.67102772500006,15.2,-10.411979339));
#295504=CARTESIAN_POINT('Ctrl Pts',(-1.67102772500006,11.6,-10.411979339));
#295505=CARTESIAN_POINT('Ctrl Pts',(-1.67036243400006,15.2,-10.410200583));
#295506=CARTESIAN_POINT('Ctrl Pts',(-1.67036243400006,11.6,-10.410200583));
#295507=CARTESIAN_POINT('Ctrl Pts',(-1.66970130200006,15.2,-10.408428019));
#295508=CARTESIAN_POINT('Ctrl Pts',(-1.66970130200006,11.6,-10.408428019));
#295509=CARTESIAN_POINT('Ctrl Pts',(-1.66904432300006,15.2,-10.406661664));
#295510=CARTESIAN_POINT('Ctrl Pts',(-1.66904432300006,11.6,-10.406661664));
#295511=CARTESIAN_POINT('Ctrl Pts',(-1.66839149100006,15.2,-10.404901541));
#295512=CARTESIAN_POINT('Ctrl Pts',(-1.66839149100006,11.6,-10.404901541));
#295513=CARTESIAN_POINT('Ctrl Pts',(-1.66774280000005,15.2,-10.403147668));
#295514=CARTESIAN_POINT('Ctrl Pts',(-1.66774280000005,11.6,-10.403147668));
#295515=CARTESIAN_POINT('Ctrl Pts',(-1.66709824500006,15.2,-10.401400063));
#295516=CARTESIAN_POINT('Ctrl Pts',(-1.66709824500006,11.6,-10.401400063));
#295517=CARTESIAN_POINT('Ctrl Pts',(-1.66645782000006,15.2,-10.399658748));
#295518=CARTESIAN_POINT('Ctrl Pts',(-1.66645782000006,11.6,-10.399658748));
#295519=CARTESIAN_POINT('Ctrl Pts',(-1.66582152000006,15.2,-10.397923741));
#295520=CARTESIAN_POINT('Ctrl Pts',(-1.66582152000006,11.6,-10.397923741));
#295521=CARTESIAN_POINT('Ctrl Pts',(-1.66518933800006,15.2,-10.396195062));
#295522=CARTESIAN_POINT('Ctrl Pts',(-1.66518933800006,11.6,-10.396195062));
#295523=CARTESIAN_POINT('Ctrl Pts',(-1.66456126800006,15.2,-10.394472732));
#295524=CARTESIAN_POINT('Ctrl Pts',(-1.66456126800006,11.6,-10.394472732));
#295525=CARTESIAN_POINT('Ctrl Pts',(-1.66393730600006,15.2,-10.392756769));
#295526=CARTESIAN_POINT('Ctrl Pts',(-1.66393730600006,11.6,-10.392756769));
#295527=CARTESIAN_POINT('Ctrl Pts',(-1.66331744300006,15.2,-10.391047193));
#295528=CARTESIAN_POINT('Ctrl Pts',(-1.66331744300006,11.6,-10.391047193));
#295529=CARTESIAN_POINT('Ctrl Pts',(-1.66270167700006,15.2,-10.389344026));
#295530=CARTESIAN_POINT('Ctrl Pts',(-1.66270167700006,11.6,-10.389344026));
#295531=CARTESIAN_POINT('Ctrl Pts',(-1.66208999800005,15.2,-10.387647286));
#295532=CARTESIAN_POINT('Ctrl Pts',(-1.66208999800005,11.6,-10.387647286));
#295533=CARTESIAN_POINT('Ctrl Pts',(-1.66148240300006,15.2,-10.385956994));
#295534=CARTESIAN_POINT('Ctrl Pts',(-1.66148240300006,11.6,-10.385956994));
#295535=CARTESIAN_POINT('Ctrl Pts',(-1.66087888400006,15.2,-10.38427317));
#295536=CARTESIAN_POINT('Ctrl Pts',(-1.66087888400006,11.6,-10.38427317));
#295537=CARTESIAN_POINT('Ctrl Pts',(-1.66027943500006,15.2,-10.382595835));
#295538=CARTESIAN_POINT('Ctrl Pts',(-1.66027943500006,11.6,-10.382595835));
#295539=CARTESIAN_POINT('Ctrl Pts',(-1.65968405200006,15.2,-10.380925008));
#295540=CARTESIAN_POINT('Ctrl Pts',(-1.65968405200006,11.6,-10.380925008));
#295541=CARTESIAN_POINT('Ctrl Pts',(-1.65909272600006,15.2,-10.37926071));
#295542=CARTESIAN_POINT('Ctrl Pts',(-1.65909272600006,11.6,-10.37926071));
#295543=CARTESIAN_POINT('Ctrl Pts',(-1.65850545200006,15.2,-10.377602961));
#295544=CARTESIAN_POINT('Ctrl Pts',(-1.65850545200006,11.6,-10.377602961));
#295545=CARTESIAN_POINT('Ctrl Pts',(-1.65792222600006,15.2,-10.375951783));
#295546=CARTESIAN_POINT('Ctrl Pts',(-1.65792222600006,11.6,-10.375951783));
#295547=CARTESIAN_POINT('Ctrl Pts',(-1.65734303700006,15.2,-10.374307195));
#295548=CARTESIAN_POINT('Ctrl Pts',(-1.65734303700006,11.6,-10.374307195));
#295549=CARTESIAN_POINT('Ctrl Pts',(-1.65676788300006,15.2,-10.372669218));
#295550=CARTESIAN_POINT('Ctrl Pts',(-1.65676788300006,11.6,-10.372669218));
#295551=CARTESIAN_POINT('Ctrl Pts',(-1.65619675600006,15.2,-10.371037873));
#295552=CARTESIAN_POINT('Ctrl Pts',(-1.65619675600006,11.6,-10.371037873));
#295553=CARTESIAN_POINT('Ctrl Pts',(-1.65562964900006,15.2,-10.369413181));
#295554=CARTESIAN_POINT('Ctrl Pts',(-1.65562964900006,11.6,-10.369413181));
#295555=CARTESIAN_POINT('Ctrl Pts',(-1.65506655700006,15.2,-10.367795164));
#295556=CARTESIAN_POINT('Ctrl Pts',(-1.65506655700006,11.6,-10.367795164));
#295557=CARTESIAN_POINT('Ctrl Pts',(-1.65450747200006,15.2,-10.36618384));
#295558=CARTESIAN_POINT('Ctrl Pts',(-1.65450747200006,11.6,-10.36618384));
#295559=CARTESIAN_POINT('Ctrl Pts',(-1.65395238800006,15.2,-10.364579233));
#295560=CARTESIAN_POINT('Ctrl Pts',(-1.65395238800006,11.6,-10.364579233));
#295561=CARTESIAN_POINT('Ctrl Pts',(-1.65340130000006,15.2,-10.362981362));
#295562=CARTESIAN_POINT('Ctrl Pts',(-1.65340130000006,11.6,-10.362981362));
#295563=CARTESIAN_POINT('Ctrl Pts',(-1.65285419900006,15.2,-10.361390249));
#295564=CARTESIAN_POINT('Ctrl Pts',(-1.65285419900006,11.6,-10.361390249));
#295565=CARTESIAN_POINT('Ctrl Pts',(-1.65231108000006,15.2,-10.359805917));
#295566=CARTESIAN_POINT('Ctrl Pts',(-1.65231108000006,11.6,-10.359805917));
#295567=CARTESIAN_POINT('Ctrl Pts',(-1.65177193600006,15.2,-10.358228384));
#295568=CARTESIAN_POINT('Ctrl Pts',(-1.65177193600006,11.6,-10.358228384));
#295569=CARTESIAN_POINT('Ctrl Pts',(-1.65123676100006,15.2,-10.356657674));
#295570=CARTESIAN_POINT('Ctrl Pts',(-1.65123676100006,11.6,-10.356657674));
#295571=CARTESIAN_POINT('Ctrl Pts',(-1.65070554700006,15.2,-10.355093807));
#295572=CARTESIAN_POINT('Ctrl Pts',(-1.65070554700006,11.6,-10.355093807));
#295573=CARTESIAN_POINT('Ctrl Pts',(-1.65017828800006,15.2,-10.353536807));
#295574=CARTESIAN_POINT('Ctrl Pts',(-1.65017828800006,11.6,-10.353536807));
#295575=CARTESIAN_POINT('Ctrl Pts',(-1.64965497700006,15.2,-10.351986691));
#295576=CARTESIAN_POINT('Ctrl Pts',(-1.64965497700006,11.6,-10.351986691));
#295577=CARTESIAN_POINT('Ctrl Pts',(-1.64913560800006,15.2,-10.350443486));
#295578=CARTESIAN_POINT('Ctrl Pts',(-1.64913560800006,11.6,-10.350443486));
#295579=CARTESIAN_POINT('Ctrl Pts',(-1.64862017200006,15.2,-10.348907211));
#295580=CARTESIAN_POINT('Ctrl Pts',(-1.64862017200006,11.6,-10.348907211));
#295581=CARTESIAN_POINT('Ctrl Pts',(-1.64810866500006,15.2,-10.347377888));
#295582=CARTESIAN_POINT('Ctrl Pts',(-1.64810866500006,11.6,-10.347377888));
#295583=CARTESIAN_POINT('Ctrl Pts',(-1.64760107800005,15.2,-10.34585554));
#295584=CARTESIAN_POINT('Ctrl Pts',(-1.64760107800005,11.6,-10.34585554));
#295585=CARTESIAN_POINT('Ctrl Pts',(-1.64709740400005,15.2,-10.344340188));
#295586=CARTESIAN_POINT('Ctrl Pts',(-1.64709740400005,11.6,-10.344340188));
#295587=CARTESIAN_POINT('Ctrl Pts',(-1.64659763700006,15.2,-10.342831854));
#295588=CARTESIAN_POINT('Ctrl Pts',(-1.64659763700006,11.6,-10.342831854));
#295589=CARTESIAN_POINT('Ctrl Pts',(-1.64610177000006,15.2,-10.341330563));
#295590=CARTESIAN_POINT('Ctrl Pts',(-1.64610177000006,11.6,-10.341330563));
#295591=CARTESIAN_POINT('Ctrl Pts',(-1.64560979500005,15.2,-10.339836333));
#295592=CARTESIAN_POINT('Ctrl Pts',(-1.64560979500005,11.6,-10.339836333));
#295593=CARTESIAN_POINT('Ctrl Pts',(-1.64512170500006,15.2,-10.33834919));
#295594=CARTESIAN_POINT('Ctrl Pts',(-1.64512170500006,11.6,-10.33834919));
#295595=CARTESIAN_POINT('Ctrl Pts',(-1.64463749400006,15.2,-10.336869154));
#295596=CARTESIAN_POINT('Ctrl Pts',(-1.64463749400006,11.6,-10.336869154));
#295597=CARTESIAN_POINT('Ctrl Pts',(-1.64415715300006,15.2,-10.33539625));
#295598=CARTESIAN_POINT('Ctrl Pts',(-1.64415715300006,11.6,-10.33539625));
#295599=CARTESIAN_POINT('Ctrl Pts',(-1.64368067600006,15.2,-10.333930498));
#295600=CARTESIAN_POINT('Ctrl Pts',(-1.64368067600006,11.6,-10.333930498));
#295601=CARTESIAN_POINT('Ctrl Pts',(-1.64320805500005,15.2,-10.332471923));
#295602=CARTESIAN_POINT('Ctrl Pts',(-1.64320805500005,11.6,-10.332471923));
#295603=CARTESIAN_POINT('Ctrl Pts',(-1.64273928400006,15.2,-10.331020547));
#295604=CARTESIAN_POINT('Ctrl Pts',(-1.64273928400006,11.6,-10.331020547));
#295605=CARTESIAN_POINT('Ctrl Pts',(-1.64227435300006,15.2,-10.329576392));
#295606=CARTESIAN_POINT('Ctrl Pts',(-1.64227435300006,11.6,-10.329576392));
#295607=CARTESIAN_POINT('Ctrl Pts',(-1.64181325800006,15.2,-10.328139482));
#295608=CARTESIAN_POINT('Ctrl Pts',(-1.64181325800006,11.6,-10.328139482));
#295609=CARTESIAN_POINT('Ctrl Pts',(-1.64135598800006,15.2,-10.32670984));
#295610=CARTESIAN_POINT('Ctrl Pts',(-1.64135598800006,11.6,-10.32670984));
#295611=CARTESIAN_POINT('Ctrl Pts',(-1.64090253900006,15.2,-10.325287489));
#295612=CARTESIAN_POINT('Ctrl Pts',(-1.64090253900006,11.6,-10.325287489));
#295613=CARTESIAN_POINT('Ctrl Pts',(-1.64045290000006,15.2,-10.323872454));
#295614=CARTESIAN_POINT('Ctrl Pts',(-1.64045290000006,11.6,-10.323872454));
#295615=CARTESIAN_POINT('Ctrl Pts',(-1.64000706600006,15.2,-10.322464755));
#295616=CARTESIAN_POINT('Ctrl Pts',(-1.64000706600006,11.6,-10.322464755));
#295617=CARTESIAN_POINT('Ctrl Pts',(-1.63956502700006,15.2,-10.321064418));
#295618=CARTESIAN_POINT('Ctrl Pts',(-1.63956502700006,11.6,-10.321064418));
#295619=CARTESIAN_POINT('Ctrl Pts',(-1.63912677800006,15.2,-10.319671466));
#295620=CARTESIAN_POINT('Ctrl Pts',(-1.63912677800006,11.6,-10.319671466));
#295621=CARTESIAN_POINT('Ctrl Pts',(-1.63869231000006,15.2,-10.318285921));
#295622=CARTESIAN_POINT('Ctrl Pts',(-1.63869231000006,11.6,-10.318285921));
#295623=CARTESIAN_POINT('Ctrl Pts',(-1.63826161500006,15.2,-10.316907809));
#295624=CARTESIAN_POINT('Ctrl Pts',(-1.63826161500006,11.6,-10.316907809));
#295625=CARTESIAN_POINT('Ctrl Pts',(-1.63783468500006,15.2,-10.315537154));
#295626=CARTESIAN_POINT('Ctrl Pts',(-1.63783468500006,11.6,-10.315537154));
#295627=CARTESIAN_POINT('Ctrl Pts',(-1.63741151300006,15.2,-10.314173978));
#295628=CARTESIAN_POINT('Ctrl Pts',(-1.63741151300006,11.6,-10.314173978));
#295629=CARTESIAN_POINT('Ctrl Pts',(-1.63699208900006,15.2,-10.312818307));
#295630=CARTESIAN_POINT('Ctrl Pts',(-1.63699208900006,11.6,-10.312818307));
#295631=CARTESIAN_POINT('Ctrl Pts',(-1.63657640900006,15.2,-10.311470164));
#295632=CARTESIAN_POINT('Ctrl Pts',(-1.63657640900006,11.6,-10.311470164));
#295633=CARTESIAN_POINT('Ctrl Pts',(-1.63616446000006,15.2,-10.310129573));
#295634=CARTESIAN_POINT('Ctrl Pts',(-1.63616446000006,11.6,-10.310129573));
#295635=CARTESIAN_POINT('Ctrl Pts',(-1.63575623900006,15.2,-10.308796558));
#295636=CARTESIAN_POINT('Ctrl Pts',(-1.63575623900006,11.6,-10.308796558));
#295637=CARTESIAN_POINT('Ctrl Pts',(-1.63535173400006,15.2,-10.307471145));
#295638=CARTESIAN_POINT('Ctrl Pts',(-1.63535173400006,11.6,-10.307471145));
#295639=CARTESIAN_POINT('Ctrl Pts',(-1.63495093900006,15.2,-10.306153358));
#295640=CARTESIAN_POINT('Ctrl Pts',(-1.63495093900006,11.6,-10.306153358));
#295641=CARTESIAN_POINT('Ctrl Pts',(-1.63455384500006,15.2,-10.30484322));
#295642=CARTESIAN_POINT('Ctrl Pts',(-1.63455384500006,11.6,-10.30484322));
#295643=CARTESIAN_POINT('Ctrl Pts',(-1.63416044300006,15.2,-10.303540757));
#295644=CARTESIAN_POINT('Ctrl Pts',(-1.63416044300006,11.6,-10.303540757));
#295645=CARTESIAN_POINT('Ctrl Pts',(-1.63377072600006,15.2,-10.302245994));
#295646=CARTESIAN_POINT('Ctrl Pts',(-1.63377072600006,11.6,-10.302245994));
#295647=CARTESIAN_POINT('Ctrl Pts',(-1.63338468600006,15.2,-10.300958957));
#295648=CARTESIAN_POINT('Ctrl Pts',(-1.63338468600006,11.6,-10.300958957));
#295649=CARTESIAN_POINT('Ctrl Pts',(-1.63300231200005,15.2,-10.299679669));
#295650=CARTESIAN_POINT('Ctrl Pts',(-1.63300231200005,11.6,-10.299679669));
#295651=CARTESIAN_POINT('Ctrl Pts',(-1.63262359900005,15.2,-10.298408156));
#295652=CARTESIAN_POINT('Ctrl Pts',(-1.63262359900005,11.6,-10.298408156));
#295653=CARTESIAN_POINT('Ctrl Pts',(-1.63224853600005,15.2,-10.297144443));
#295654=CARTESIAN_POINT('Ctrl Pts',(-1.63224853600005,11.6,-10.297144443));
#295655=CARTESIAN_POINT('Ctrl Pts',(-1.63187711600006,15.2,-10.295888554));
#295656=CARTESIAN_POINT('Ctrl Pts',(-1.63187711600006,11.6,-10.295888554));
#295657=CARTESIAN_POINT('Ctrl Pts',(-1.63150933000006,15.2,-10.294640518));
#295658=CARTESIAN_POINT('Ctrl Pts',(-1.63150933000006,11.6,-10.294640518));
#295659=CARTESIAN_POINT('Ctrl Pts',(-1.63114516900006,15.2,-10.293400358));
#295660=CARTESIAN_POINT('Ctrl Pts',(-1.63114516900006,11.6,-10.293400358));
#295661=CARTESIAN_POINT('Ctrl Pts',(-1.63078462400006,15.2,-10.292168099));
#295662=CARTESIAN_POINT('Ctrl Pts',(-1.63078462400006,11.6,-10.292168099));
#295663=CARTESIAN_POINT('Ctrl Pts',(-1.63042768700006,15.2,-10.290943769));
#295664=CARTESIAN_POINT('Ctrl Pts',(-1.63042768700006,11.6,-10.290943769));
#295665=CARTESIAN_POINT('Ctrl Pts',(-1.63007434900006,15.2,-10.289727392));
#295666=CARTESIAN_POINT('Ctrl Pts',(-1.63007434900006,11.6,-10.289727392));
#295667=CARTESIAN_POINT('Ctrl Pts',(-1.62972460000006,15.2,-10.288518995));
#295668=CARTESIAN_POINT('Ctrl Pts',(-1.62972460000006,11.6,-10.288518995));
#295669=CARTESIAN_POINT('Ctrl Pts',(-1.62937843400006,15.2,-10.287318604));
#295670=CARTESIAN_POINT('Ctrl Pts',(-1.62937843400006,11.6,-10.287318604));
#295671=CARTESIAN_POINT('Ctrl Pts',(-1.62903583800006,15.2,-10.286126246));
#295672=CARTESIAN_POINT('Ctrl Pts',(-1.62903583800006,11.6,-10.286126246));
#295673=CARTESIAN_POINT('Ctrl Pts',(-1.62869680700006,15.2,-10.284941945));
#295674=CARTESIAN_POINT('Ctrl Pts',(-1.62869680700006,11.6,-10.284941945));
#295675=CARTESIAN_POINT('Ctrl Pts',(-1.62836133000006,15.2,-10.283765729));
#295676=CARTESIAN_POINT('Ctrl Pts',(-1.62836133000006,11.6,-10.283765729));
#295677=CARTESIAN_POINT('Ctrl Pts',(-1.62802939800006,15.2,-10.282597626));
#295678=CARTESIAN_POINT('Ctrl Pts',(-1.62802939800006,11.6,-10.282597626));
#295679=CARTESIAN_POINT('Ctrl Pts',(-1.62770100100006,15.2,-10.281437659));
#295680=CARTESIAN_POINT('Ctrl Pts',(-1.62770100100006,11.6,-10.281437659));
#295681=CARTESIAN_POINT('Ctrl Pts',(-1.62737613100005,15.2,-10.280285858));
#295682=CARTESIAN_POINT('Ctrl Pts',(-1.62737613100005,11.6,-10.280285858));
#295683=CARTESIAN_POINT('Ctrl Pts',(-1.62705477800006,15.2,-10.279142249));
#295684=CARTESIAN_POINT('Ctrl Pts',(-1.62705477800006,11.6,-10.279142249));
#295685=CARTESIAN_POINT('Ctrl Pts',(-1.62673693500006,15.2,-10.278006858));
#295686=CARTESIAN_POINT('Ctrl Pts',(-1.62673693500006,11.6,-10.278006858));
#295687=CARTESIAN_POINT('Ctrl Pts',(-1.62642258900005,15.2,-10.276879714));
#295688=CARTESIAN_POINT('Ctrl Pts',(-1.62642258900005,11.6,-10.276879714));
#295689=CARTESIAN_POINT('Ctrl Pts',(-1.62611173300005,15.2,-10.275760843));
#295690=CARTESIAN_POINT('Ctrl Pts',(-1.62611173300005,11.6,-10.275760843));
#295691=CARTESIAN_POINT('Ctrl Pts',(-1.62580435500006,15.2,-10.274650272));
#295692=CARTESIAN_POINT('Ctrl Pts',(-1.62580435500006,11.6,-10.274650272));
#295693=CARTESIAN_POINT('Ctrl Pts',(-1.62550044800006,15.2,-10.27354803));
#295694=CARTESIAN_POINT('Ctrl Pts',(-1.62550044800006,11.6,-10.27354803));
#295695=CARTESIAN_POINT('Ctrl Pts',(-1.62520000300006,15.2,-10.272454143));
#295696=CARTESIAN_POINT('Ctrl Pts',(-1.62520000300006,11.6,-10.272454143));
#295697=CARTESIAN_POINT('Ctrl Pts',(-1.62490300800005,15.2,-10.27136864));
#295698=CARTESIAN_POINT('Ctrl Pts',(-1.62490300800005,11.6,-10.27136864));
#295699=CARTESIAN_POINT('Ctrl Pts',(-1.62460945300006,15.2,-10.270291548));
#295700=CARTESIAN_POINT('Ctrl Pts',(-1.62460945300006,11.6,-10.270291548));
#295701=CARTESIAN_POINT('Ctrl Pts',(-1.62431933100006,15.2,-10.269222895));
#295702=CARTESIAN_POINT('Ctrl Pts',(-1.62431933100006,11.6,-10.269222895));
#295703=CARTESIAN_POINT('Ctrl Pts',(-1.62403263000006,15.2,-10.268162711));
#295704=CARTESIAN_POINT('Ctrl Pts',(-1.62403263000006,11.6,-10.268162711));
#295705=CARTESIAN_POINT('Ctrl Pts',(-1.62374934000006,15.2,-10.267111021));
#295706=CARTESIAN_POINT('Ctrl Pts',(-1.62374934000006,11.6,-10.267111021));
#295707=CARTESIAN_POINT('Ctrl Pts',(-1.62346945200006,15.2,-10.266067857));
#295708=CARTESIAN_POINT('Ctrl Pts',(-1.62346945200006,11.6,-10.266067857));
#295709=CARTESIAN_POINT('Ctrl Pts',(-1.62319295600006,15.2,-10.265033246));
#295710=CARTESIAN_POINT('Ctrl Pts',(-1.62319295600006,11.6,-10.265033246));
#295711=CARTESIAN_POINT('Ctrl Pts',(-1.62291984100006,15.2,-10.264007214));
#295712=CARTESIAN_POINT('Ctrl Pts',(-1.62291984100006,11.6,-10.264007214));
#295713=CARTESIAN_POINT('Ctrl Pts',(-1.62265009700006,15.2,-10.262989795));
#295714=CARTESIAN_POINT('Ctrl Pts',(-1.62265009700006,11.6,-10.262989795));
#295715=CARTESIAN_POINT('Ctrl Pts',(-1.62238371500006,15.2,-10.261981014));
#295716=CARTESIAN_POINT('Ctrl Pts',(-1.62238371500006,11.6,-10.261981014));
#295717=CARTESIAN_POINT('Ctrl Pts',(-1.62212068400006,15.2,-10.260980901));
#295718=CARTESIAN_POINT('Ctrl Pts',(-1.62212068400006,11.6,-10.260980901));
#295719=CARTESIAN_POINT('Ctrl Pts',(-1.62186099300006,15.2,-10.259989485));
#295720=CARTESIAN_POINT('Ctrl Pts',(-1.62186099300006,11.6,-10.259989485));
#295721=CARTESIAN_POINT('Ctrl Pts',(-1.62160463200005,15.2,-10.259006796));
#295722=CARTESIAN_POINT('Ctrl Pts',(-1.62160463200005,11.6,-10.259006796));
#295723=CARTESIAN_POINT('Ctrl Pts',(-1.62135159100006,15.2,-10.258032864));
#295724=CARTESIAN_POINT('Ctrl Pts',(-1.62135159100006,11.6,-10.258032864));
#295725=CARTESIAN_POINT('Ctrl Pts',(-1.62110185800006,15.2,-10.257067717));
#295726=CARTESIAN_POINT('Ctrl Pts',(-1.62110185800006,11.6,-10.257067717));
#295727=CARTESIAN_POINT('Ctrl Pts',(-1.62085542500006,15.2,-10.256111386));
#295728=CARTESIAN_POINT('Ctrl Pts',(-1.62085542500006,11.6,-10.256111386));
#295729=CARTESIAN_POINT('Ctrl Pts',(-1.62061227900006,15.2,-10.255163901));
#295730=CARTESIAN_POINT('Ctrl Pts',(-1.62061227900006,11.6,-10.255163901));
#295731=CARTESIAN_POINT('Ctrl Pts',(-1.62037241000006,15.2,-10.254225291));
#295732=CARTESIAN_POINT('Ctrl Pts',(-1.62037241000006,11.6,-10.254225291));
#295733=CARTESIAN_POINT('Ctrl Pts',(-1.62013580800005,15.2,-10.253295586));
#295734=CARTESIAN_POINT('Ctrl Pts',(-1.62013580800005,11.6,-10.253295586));
#295735=CARTESIAN_POINT('Ctrl Pts',(-1.61990246100005,15.2,-10.252374817));
#295736=CARTESIAN_POINT('Ctrl Pts',(-1.61990246100005,11.6,-10.252374817));
#295737=CARTESIAN_POINT('Ctrl Pts',(-1.61967235800006,15.2,-10.251463016));
#295738=CARTESIAN_POINT('Ctrl Pts',(-1.61967235800006,11.6,-10.251463016));
#295739=CARTESIAN_POINT('Ctrl Pts',(-1.61944548900005,15.2,-10.250560211));
#295740=CARTESIAN_POINT('Ctrl Pts',(-1.61944548900005,11.6,-10.250560211));
#295741=CARTESIAN_POINT('Ctrl Pts',(-1.61922313100006,15.2,-10.249671582));
#295742=CARTESIAN_POINT('Ctrl Pts',(-1.61922313100006,11.6,-10.249671582));
#295743=CARTESIAN_POINT('Ctrl Pts',(-1.61904803300006,15.2,-10.248968851));
#295744=CARTESIAN_POINT('Ctrl Pts',(-1.61904803300006,11.6,-10.248968851));
#295745=CARTESIAN_POINT('Ctrl Pts',(-1.61891844100006,15.2,-10.24844709));
#295746=CARTESIAN_POINT('Ctrl Pts',(-1.61891844100006,11.6,-10.24844709));
#295747=CARTESIAN_POINT('Ctrl Pts',(-1.61883308400005,15.2,-10.248102703));
#295748=CARTESIAN_POINT('Ctrl Pts',(-1.61883308400005,11.6,-10.248102703));
#295749=CARTESIAN_POINT('Ctrl Pts',(-1.61879118000006,15.2,-10.247933456));
#295750=CARTESIAN_POINT('Ctrl Pts',(-1.61879118000006,11.6,-10.247933456));
#295751=CARTESIAN_POINT('',(-1.61879117999241,12.2,-10.2479334556183));
#295752=CARTESIAN_POINT('',(-1.61879117999241,15.2,-10.2479334556183));
#295753=CARTESIAN_POINT('',(-1.61879118000006,12.2,-10.247933455));
#295754=CARTESIAN_POINT('Ctrl Pts',(-2.17615954800006,12.2,-11.292224299));
#295755=CARTESIAN_POINT('Ctrl Pts',(-2.17570045500006,12.2,-11.291612887));
#295756=CARTESIAN_POINT('Ctrl Pts',(-2.17478276600006,12.2,-11.290390245));
#295757=CARTESIAN_POINT('Ctrl Pts',(-2.17340771700006,12.2,-11.28855682));
#295758=CARTESIAN_POINT('Ctrl Pts',(-2.17157728800006,12.2,-11.286113334));
#295759=CARTESIAN_POINT('Ctrl Pts',(-2.16929420200006,12.2,-11.283060773));
#295760=CARTESIAN_POINT('Ctrl Pts',(-2.16701606700005,12.2,-11.280010015));
#295761=CARTESIAN_POINT('Ctrl Pts',(-2.16474288100006,12.2,-11.276961058));
#295762=CARTESIAN_POINT('Ctrl Pts',(-2.16247464600006,12.2,-11.273913908));
#295763=CARTESIAN_POINT('Ctrl Pts',(-2.16021136000006,12.2,-11.27086857));
#295764=CARTESIAN_POINT('Ctrl Pts',(-2.15795302500006,12.2,-11.267825054));
#295765=CARTESIAN_POINT('Ctrl Pts',(-2.15569963800006,12.2,-11.264783368));
#295766=CARTESIAN_POINT('Ctrl Pts',(-2.15345120200006,12.2,-11.261743524));
#295767=CARTESIAN_POINT('Ctrl Pts',(-2.15120771500006,12.2,-11.258705531));
#295768=CARTESIAN_POINT('Ctrl Pts',(-2.14896917600006,12.2,-11.255669403));
#295769=CARTESIAN_POINT('Ctrl Pts',(-2.14673558400006,12.2,-11.252635149));
#295770=CARTESIAN_POINT('Ctrl Pts',(-2.14450694000006,12.2,-11.249602777));
#295771=CARTESIAN_POINT('Ctrl Pts',(-2.14228324400006,12.2,-11.246572299));
#295772=CARTESIAN_POINT('Ctrl Pts',(-2.14006449500005,12.2,-11.243543721));
#295773=CARTESIAN_POINT('Ctrl Pts',(-2.13785069300005,12.2,-11.24051705));
#295774=CARTESIAN_POINT('Ctrl Pts',(-2.13564183800006,12.2,-11.237492297));
#295775=CARTESIAN_POINT('Ctrl Pts',(-2.13343792800006,12.2,-11.234469469));
#295776=CARTESIAN_POINT('Ctrl Pts',(-2.13123896500006,12.2,-11.231448574));
#295777=CARTESIAN_POINT('Ctrl Pts',(-2.12904494800005,12.2,-11.228429624));
#295778=CARTESIAN_POINT('Ctrl Pts',(-2.12685587600005,12.2,-11.225412626));
#295779=CARTESIAN_POINT('Ctrl Pts',(-2.12467174800006,12.2,-11.222397592));
#295780=CARTESIAN_POINT('Ctrl Pts',(-2.12249256500006,12.2,-11.219384528));
#295781=CARTESIAN_POINT('Ctrl Pts',(-2.12031832600006,12.2,-11.216373446));
#295782=CARTESIAN_POINT('Ctrl Pts',(-2.11814903000006,12.2,-11.213364356));
#295783=CARTESIAN_POINT('Ctrl Pts',(-2.11598467700005,12.2,-11.210357264));
#295784=CARTESIAN_POINT('Ctrl Pts',(-2.11382526700006,12.2,-11.207352181));
#295785=CARTESIAN_POINT('Ctrl Pts',(-2.11167080000005,12.2,-11.204349116));
#295786=CARTESIAN_POINT('Ctrl Pts',(-2.10952127400006,12.2,-11.201348078));
#295787=CARTESIAN_POINT('Ctrl Pts',(-2.10737669000005,12.2,-11.198349076));
#295788=CARTESIAN_POINT('Ctrl Pts',(-2.10523704700006,12.2,-11.19535212));
#295789=CARTESIAN_POINT('Ctrl Pts',(-2.10310234500006,12.2,-11.192357218));
#295790=CARTESIAN_POINT('Ctrl Pts',(-2.10097258200005,12.2,-11.18936438));
#295791=CARTESIAN_POINT('Ctrl Pts',(-2.09884776000006,12.2,-11.186373616));
#295792=CARTESIAN_POINT('Ctrl Pts',(-2.09672787600006,12.2,-11.183384935));
#295793=CARTESIAN_POINT('Ctrl Pts',(-2.09461293200006,12.2,-11.180398346));
#295794=CARTESIAN_POINT('Ctrl Pts',(-2.09250292400006,12.2,-11.177413859));
#295795=CARTESIAN_POINT('Ctrl Pts',(-2.09039785500006,12.2,-11.174431482));
#295796=CARTESIAN_POINT('Ctrl Pts',(-2.08829772300006,12.2,-11.171451227));
#295797=CARTESIAN_POINT('Ctrl Pts',(-2.08620252700006,12.2,-11.1684731));
#295798=CARTESIAN_POINT('Ctrl Pts',(-2.08411226900005,12.2,-11.165497114));
#295799=CARTESIAN_POINT('Ctrl Pts',(-2.08202694500006,12.2,-11.162523276));
#295800=CARTESIAN_POINT('Ctrl Pts',(-2.07994655600006,12.2,-11.159551596));
#295801=CARTESIAN_POINT('Ctrl Pts',(-2.07787110100006,12.2,-11.156582084));
#295802=CARTESIAN_POINT('Ctrl Pts',(-2.07580058000006,12.2,-11.153614748));
#295803=CARTESIAN_POINT('Ctrl Pts',(-2.07373499200005,12.2,-11.1506496));
#295804=CARTESIAN_POINT('Ctrl Pts',(-2.07167433800006,12.2,-11.147686647));
#295805=CARTESIAN_POINT('Ctrl Pts',(-2.06961861500006,12.2,-11.1447259));
#295806=CARTESIAN_POINT('Ctrl Pts',(-2.06756782400006,12.2,-11.141767369));
#295807=CARTESIAN_POINT('Ctrl Pts',(-2.06552196300006,12.2,-11.138811062));
#295808=CARTESIAN_POINT('Ctrl Pts',(-2.06348103200006,12.2,-11.13585699));
#295809=CARTESIAN_POINT('Ctrl Pts',(-2.06144503200006,12.2,-11.132905162));
#295810=CARTESIAN_POINT('Ctrl Pts',(-2.05941396000005,12.2,-11.129955589));
#295811=CARTESIAN_POINT('Ctrl Pts',(-2.05738781600005,12.2,-11.127008278));
#295812=CARTESIAN_POINT('Ctrl Pts',(-2.05536660000006,12.2,-11.12406324));
#295813=CARTESIAN_POINT('Ctrl Pts',(-2.05335031200006,12.2,-11.121120485));
#295814=CARTESIAN_POINT('Ctrl Pts',(-2.05133894900006,12.2,-11.118180023));
#295815=CARTESIAN_POINT('Ctrl Pts',(-2.04933251100006,12.2,-11.115241862));
#295816=CARTESIAN_POINT('Ctrl Pts',(-2.04733100000006,12.2,-11.112306013));
#295817=CARTESIAN_POINT('Ctrl Pts',(-2.04533441100006,12.2,-11.109372486));
#295818=CARTESIAN_POINT('Ctrl Pts',(-2.04334274700006,12.2,-11.106441291));
#295819=CARTESIAN_POINT('Ctrl Pts',(-2.04135600500006,12.2,-11.103512437));
#295820=CARTESIAN_POINT('Ctrl Pts',(-2.03937418400006,12.2,-11.100585934));
#295821=CARTESIAN_POINT('Ctrl Pts',(-2.03739728600006,12.2,-11.097661791));
#295822=CARTESIAN_POINT('Ctrl Pts',(-2.03542530900005,12.2,-11.094740019));
#295823=CARTESIAN_POINT('Ctrl Pts',(-2.03345825000006,12.2,-11.091820627));
#295824=CARTESIAN_POINT('Ctrl Pts',(-2.03149611100006,12.2,-11.088903627));
#295825=CARTESIAN_POINT('Ctrl Pts',(-2.02953889000006,12.2,-11.085989026));
#295826=CARTESIAN_POINT('Ctrl Pts',(-2.02758658500006,12.2,-11.083076836));
#295827=CARTESIAN_POINT('Ctrl Pts',(-2.02563919900005,12.2,-11.080167065));
#295828=CARTESIAN_POINT('Ctrl Pts',(-2.02369672800006,12.2,-11.077259724));
#295829=CARTESIAN_POINT('Ctrl Pts',(-2.02175917100006,12.2,-11.074354824));
#295830=CARTESIAN_POINT('Ctrl Pts',(-2.01982652900006,12.2,-11.071452373));
#295831=CARTESIAN_POINT('Ctrl Pts',(-2.01789880000006,12.2,-11.068552382));
#295832=CARTESIAN_POINT('Ctrl Pts',(-2.01597598400005,12.2,-11.065654863));
#295833=CARTESIAN_POINT('Ctrl Pts',(-2.01405807900006,12.2,-11.062759821));
#295834=CARTESIAN_POINT('Ctrl Pts',(-2.01214508600006,12.2,-11.059867271));
#295835=CARTESIAN_POINT('Ctrl Pts',(-2.01023700100006,12.2,-11.056977221));
#295836=CARTESIAN_POINT('Ctrl Pts',(-2.00833382600006,12.2,-11.054089681));
#295837=CARTESIAN_POINT('Ctrl Pts',(-2.00643555900006,12.2,-11.05120466));
#295838=CARTESIAN_POINT('Ctrl Pts',(-2.00454219900006,12.2,-11.048322171));
#295839=CARTESIAN_POINT('Ctrl Pts',(-2.00265374600006,12.2,-11.045442222));
#295840=CARTESIAN_POINT('Ctrl Pts',(-2.00077019700006,12.2,-11.042564824));
#295841=CARTESIAN_POINT('Ctrl Pts',(-1.99889155400006,12.2,-11.039689987));
#295842=CARTESIAN_POINT('Ctrl Pts',(-1.99701781300006,12.2,-11.03681772));
#295843=CARTESIAN_POINT('Ctrl Pts',(-1.99514897500006,12.2,-11.033948035));
#295844=CARTESIAN_POINT('Ctrl Pts',(-1.99328503900006,12.2,-11.031080942));
#295845=CARTESIAN_POINT('Ctrl Pts',(-1.99142600300006,12.2,-11.02821645));
#295846=CARTESIAN_POINT('Ctrl Pts',(-1.98957186800006,12.2,-11.025354571));
#295847=CARTESIAN_POINT('Ctrl Pts',(-1.98772263100006,12.2,-11.022495313));
#295848=CARTESIAN_POINT('Ctrl Pts',(-1.98587829000005,12.2,-11.019638689));
#295849=CARTESIAN_POINT('Ctrl Pts',(-1.98403884700005,12.2,-11.016784707));
#295850=CARTESIAN_POINT('Ctrl Pts',(-1.98220430000006,12.2,-11.013933379));
#295851=CARTESIAN_POINT('Ctrl Pts',(-1.98037464600006,12.2,-11.011084714));
#295852=CARTESIAN_POINT('Ctrl Pts',(-1.97854988600006,12.2,-11.008238724));
#295853=CARTESIAN_POINT('Ctrl Pts',(-1.97673001900006,12.2,-11.005395418));
#295854=CARTESIAN_POINT('Ctrl Pts',(-1.97491504200005,12.2,-11.002554807));
#295855=CARTESIAN_POINT('Ctrl Pts',(-1.97310495700005,12.2,-10.999716901));
#295856=CARTESIAN_POINT('Ctrl Pts',(-1.97129976000005,12.2,-10.996881712));
#295857=CARTESIAN_POINT('Ctrl Pts',(-1.96949945100006,12.2,-10.994049247));
#295858=CARTESIAN_POINT('Ctrl Pts',(-1.96770402900006,12.2,-10.99121952));
#295859=CARTESIAN_POINT('Ctrl Pts',(-1.96591349400005,12.2,-10.988392541));
#295860=CARTESIAN_POINT('Ctrl Pts',(-1.96412784300006,12.2,-10.985568319));
#295861=CARTESIAN_POINT('Ctrl Pts',(-1.96234707500006,12.2,-10.982746866));
#295862=CARTESIAN_POINT('Ctrl Pts',(-1.96057119000006,12.2,-10.979928192));
#295863=CARTESIAN_POINT('Ctrl Pts',(-1.95880018600006,12.2,-10.977112307));
#295864=CARTESIAN_POINT('Ctrl Pts',(-1.95703406200006,12.2,-10.974299223));
#295865=CARTESIAN_POINT('Ctrl Pts',(-1.95527281700006,12.2,-10.971488949));
#295866=CARTESIAN_POINT('Ctrl Pts',(-1.95351645100006,12.2,-10.968681498));
#295867=CARTESIAN_POINT('Ctrl Pts',(-1.95176495900005,12.2,-10.965876877));
#295868=CARTESIAN_POINT('Ctrl Pts',(-1.95001834500005,12.2,-10.963075101));
#295869=CARTESIAN_POINT('Ctrl Pts',(-1.94827660300006,12.2,-10.960276177));
#295870=CARTESIAN_POINT('Ctrl Pts',(-1.94653973400006,12.2,-10.957480118));
#295871=CARTESIAN_POINT('Ctrl Pts',(-1.94480773800006,12.2,-10.954686934));
#295872=CARTESIAN_POINT('Ctrl Pts',(-1.94308061000006,12.2,-10.951896636));
#295873=CARTESIAN_POINT('Ctrl Pts',(-1.94135835200006,12.2,-10.949109235));
#295874=CARTESIAN_POINT('Ctrl Pts',(-1.93964096300005,12.2,-10.946324741));
#295875=CARTESIAN_POINT('Ctrl Pts',(-1.93792843900006,12.2,-10.943543166));
#295876=CARTESIAN_POINT('Ctrl Pts',(-1.93622078100006,12.2,-10.940764519));
#295877=CARTESIAN_POINT('Ctrl Pts',(-1.93451798600006,12.2,-10.937988814));
#295878=CARTESIAN_POINT('Ctrl Pts',(-1.93282005500006,12.2,-10.935216058));
#295879=CARTESIAN_POINT('Ctrl Pts',(-1.93112698400005,12.2,-10.932446266));
#295880=CARTESIAN_POINT('Ctrl Pts',(-1.92943877200005,12.2,-10.929679446));
#295881=CARTESIAN_POINT('Ctrl Pts',(-1.92775541900006,12.2,-10.92691561));
#295882=CARTESIAN_POINT('Ctrl Pts',(-1.92607692400005,12.2,-10.924154768));
#295883=CARTESIAN_POINT('Ctrl Pts',(-1.92440328400005,12.2,-10.921396933));
#295884=CARTESIAN_POINT('Ctrl Pts',(-1.92273449900005,12.2,-10.918642115));
#295885=CARTESIAN_POINT('Ctrl Pts',(-1.92107056600005,12.2,-10.915890324));
#295886=CARTESIAN_POINT('Ctrl Pts',(-1.91941148400006,12.2,-10.913141573));
#295887=CARTESIAN_POINT('Ctrl Pts',(-1.91775725300006,12.2,-10.910395872));
#295888=CARTESIAN_POINT('Ctrl Pts',(-1.91610787000006,12.2,-10.907653232));
#295889=CARTESIAN_POINT('Ctrl Pts',(-1.91446333500006,12.2,-10.904913664));
#295890=CARTESIAN_POINT('Ctrl Pts',(-1.91282364500006,12.2,-10.902177181));
#295891=CARTESIAN_POINT('Ctrl Pts',(-1.91118879900006,12.2,-10.899443792));
#295892=CARTESIAN_POINT('Ctrl Pts',(-1.90955879600006,12.2,-10.89671351));
#295893=CARTESIAN_POINT('Ctrl Pts',(-1.90793363400006,12.2,-10.893986344));
#295894=CARTESIAN_POINT('Ctrl Pts',(-1.90631331200006,12.2,-10.891262307));
#295895=CARTESIAN_POINT('Ctrl Pts',(-1.90469782800006,12.2,-10.888541409));
#295896=CARTESIAN_POINT('Ctrl Pts',(-1.90308718100006,12.2,-10.885823664));
#295897=CARTESIAN_POINT('Ctrl Pts',(-1.90148136800006,12.2,-10.88310908));
#295898=CARTESIAN_POINT('Ctrl Pts',(-1.89988038900006,12.2,-10.880397671));
#295899=CARTESIAN_POINT('Ctrl Pts',(-1.89828424200006,12.2,-10.877689446));
#295900=CARTESIAN_POINT('Ctrl Pts',(-1.89669292500006,12.2,-10.874984418));
#295901=CARTESIAN_POINT('Ctrl Pts',(-1.89510643700005,12.2,-10.872282597));
#295902=CARTESIAN_POINT('Ctrl Pts',(-1.89352477600006,12.2,-10.869583997));
#295903=CARTESIAN_POINT('Ctrl Pts',(-1.89194794100006,12.2,-10.866888627));
#295904=CARTESIAN_POINT('Ctrl Pts',(-1.89037592900006,12.2,-10.8641965));
#295905=CARTESIAN_POINT('Ctrl Pts',(-1.88880874000006,12.2,-10.861507626));
#295906=CARTESIAN_POINT('Ctrl Pts',(-1.88724637200006,12.2,-10.858822018));
#295907=CARTESIAN_POINT('Ctrl Pts',(-1.88568882100005,12.2,-10.856139687));
#295908=CARTESIAN_POINT('Ctrl Pts',(-1.88413608800006,12.2,-10.853460644));
#295909=CARTESIAN_POINT('Ctrl Pts',(-1.88258817100006,12.2,-10.850784903));
#295910=CARTESIAN_POINT('Ctrl Pts',(-1.88104506800005,12.2,-10.848112472));
#295911=CARTESIAN_POINT('Ctrl Pts',(-1.87950677700006,12.2,-10.845443365));
#295912=CARTESIAN_POINT('Ctrl Pts',(-1.87797329500006,12.2,-10.842777593));
#295913=CARTESIAN_POINT('Ctrl Pts',(-1.87644462200006,12.2,-10.840115167));
#295914=CARTESIAN_POINT('Ctrl Pts',(-1.87492075700006,12.2,-10.837456101));
#295915=CARTESIAN_POINT('Ctrl Pts',(-1.87340169600006,12.2,-10.834800405));
#295916=CARTESIAN_POINT('Ctrl Pts',(-1.87188743800006,12.2,-10.832148091));
#295917=CARTESIAN_POINT('Ctrl Pts',(-1.87037798200006,12.2,-10.829499171));
#295918=CARTESIAN_POINT('Ctrl Pts',(-1.86887332500006,12.2,-10.826853656));
#295919=CARTESIAN_POINT('Ctrl Pts',(-1.86737346700005,12.2,-10.82421156));
#295920=CARTESIAN_POINT('Ctrl Pts',(-1.86587840400006,12.2,-10.821572893));
#295921=CARTESIAN_POINT('Ctrl Pts',(-1.86438813500006,12.2,-10.818937666));
#295922=CARTESIAN_POINT('Ctrl Pts',(-1.86290265800006,12.2,-10.816305894));
#295923=CARTESIAN_POINT('Ctrl Pts',(-1.86142197200006,12.2,-10.813677586));
#295924=CARTESIAN_POINT('Ctrl Pts',(-1.85994607300006,12.2,-10.811052755));
#295925=CARTESIAN_POINT('Ctrl Pts',(-1.85847496200006,12.2,-10.808431414));
#295926=CARTESIAN_POINT('Ctrl Pts',(-1.85700863500006,12.2,-10.805813575));
#295927=CARTESIAN_POINT('Ctrl Pts',(-1.85554709100006,12.2,-10.803199248));
#295928=CARTESIAN_POINT('Ctrl Pts',(-1.85409032800006,12.2,-10.800588447));
#295929=CARTESIAN_POINT('Ctrl Pts',(-1.85263834300006,12.2,-10.797981184));
#295930=CARTESIAN_POINT('Ctrl Pts',(-1.85119113400006,12.2,-10.795377469));
#295931=CARTESIAN_POINT('Ctrl Pts',(-1.84974870200006,12.2,-10.792777317));
#295932=CARTESIAN_POINT('Ctrl Pts',(-1.84831104100006,12.2,-10.790180739));
#295933=CARTESIAN_POINT('Ctrl Pts',(-1.84687815100005,12.2,-10.787587746));
#295934=CARTESIAN_POINT('Ctrl Pts',(-1.84545003000005,12.2,-10.784998353));
#295935=CARTESIAN_POINT('Ctrl Pts',(-1.84402667500006,12.2,-10.78241257));
#295936=CARTESIAN_POINT('Ctrl Pts',(-1.84260808600006,12.2,-10.77983041));
#295937=CARTESIAN_POINT('Ctrl Pts',(-1.84119425800006,12.2,-10.777251885));
#295938=CARTESIAN_POINT('Ctrl Pts',(-1.83978519200006,12.2,-10.774677008));
#295939=CARTESIAN_POINT('Ctrl Pts',(-1.83838088300006,12.2,-10.77210579));
#295940=CARTESIAN_POINT('Ctrl Pts',(-1.83698133100005,12.2,-10.769538245));
#295941=CARTESIAN_POINT('Ctrl Pts',(-1.83558653300006,12.2,-10.766974386));
#295942=CARTESIAN_POINT('Ctrl Pts',(-1.83419648600006,12.2,-10.764414223));
#295943=CARTESIAN_POINT('Ctrl Pts',(-1.83281119000006,12.2,-10.76185777));
#295944=CARTESIAN_POINT('Ctrl Pts',(-1.83143064100005,12.2,-10.759305039));
#295945=CARTESIAN_POINT('Ctrl Pts',(-1.83005483700006,12.2,-10.756756043));
#295946=CARTESIAN_POINT('Ctrl Pts',(-1.82868377600006,12.2,-10.754210794));
#295947=CARTESIAN_POINT('Ctrl Pts',(-1.82731745700006,12.2,-10.751669306));
#295948=CARTESIAN_POINT('Ctrl Pts',(-1.82595587600006,12.2,-10.749131589));
#295949=CARTESIAN_POINT('Ctrl Pts',(-1.82459903200006,12.2,-10.746597658));
#295950=CARTESIAN_POINT('Ctrl Pts',(-1.82324692200006,12.2,-10.744067526));
#295951=CARTESIAN_POINT('Ctrl Pts',(-1.82189954400006,12.2,-10.741541203));
#295952=CARTESIAN_POINT('Ctrl Pts',(-1.82055689600006,12.2,-10.739018703));
#295953=CARTESIAN_POINT('Ctrl Pts',(-1.81921897500006,12.2,-10.73650004));
#295954=CARTESIAN_POINT('Ctrl Pts',(-1.81788577800006,12.2,-10.733985227));
#295955=CARTESIAN_POINT('Ctrl Pts',(-1.81655730500006,12.2,-10.731474274));
#295956=CARTESIAN_POINT('Ctrl Pts',(-1.81523355200006,12.2,-10.728967196));
#295957=CARTESIAN_POINT('Ctrl Pts',(-1.81391451700006,12.2,-10.726464005));
#295958=CARTESIAN_POINT('Ctrl Pts',(-1.81260019800006,12.2,-10.723964715));
#295959=CARTESIAN_POINT('Ctrl Pts',(-1.81129059100006,12.2,-10.721469338));
#295960=CARTESIAN_POINT('Ctrl Pts',(-1.80998569500006,12.2,-10.718977888));
#295961=CARTESIAN_POINT('Ctrl Pts',(-1.80868550800006,12.2,-10.716490376));
#295962=CARTESIAN_POINT('Ctrl Pts',(-1.80739002700005,12.2,-10.714006817));
#295963=CARTESIAN_POINT('Ctrl Pts',(-1.80609924900006,12.2,-10.711527223));
#295964=CARTESIAN_POINT('Ctrl Pts',(-1.80481317200006,12.2,-10.709051608));
#295965=CARTESIAN_POINT('Ctrl Pts',(-1.80353179300006,12.2,-10.706579983));
#295966=CARTESIAN_POINT('Ctrl Pts',(-1.80225511100006,12.2,-10.704112363));
#295967=CARTESIAN_POINT('Ctrl Pts',(-1.80098312100006,12.2,-10.701648762));
#295968=CARTESIAN_POINT('Ctrl Pts',(-1.79971582300006,12.2,-10.699189192));
#295969=CARTESIAN_POINT('Ctrl Pts',(-1.79845321300005,12.2,-10.696733666));
#295970=CARTESIAN_POINT('Ctrl Pts',(-1.79719528800006,12.2,-10.694282196));
#295971=CARTESIAN_POINT('Ctrl Pts',(-1.79594204700006,12.2,-10.691834799));
#295972=CARTESIAN_POINT('Ctrl Pts',(-1.79469348600006,12.2,-10.689391486));
#295973=CARTESIAN_POINT('Ctrl Pts',(-1.79344960300006,12.2,-10.686952269));
#295974=CARTESIAN_POINT('Ctrl Pts',(-1.79221039500006,12.2,-10.684517164));
#295975=CARTESIAN_POINT('Ctrl Pts',(-1.79097586000006,12.2,-10.682086183));
#295976=CARTESIAN_POINT('Ctrl Pts',(-1.78974599400005,12.2,-10.67965934));
#295977=CARTESIAN_POINT('Ctrl Pts',(-1.78852079600006,12.2,-10.677236648));
#295978=CARTESIAN_POINT('Ctrl Pts',(-1.78730026300005,12.2,-10.674818122));
#295979=CARTESIAN_POINT('Ctrl Pts',(-1.78608439100006,12.2,-10.672403774));
#295980=CARTESIAN_POINT('Ctrl Pts',(-1.78487317800006,12.2,-10.669993617));
#295981=CARTESIAN_POINT('Ctrl Pts',(-1.78366662300005,12.2,-10.667587667));
#295982=CARTESIAN_POINT('Ctrl Pts',(-1.78246472000006,12.2,-10.665185935));
#295983=CARTESIAN_POINT('Ctrl Pts',(-1.78126746700006,12.2,-10.662788437));
#295984=CARTESIAN_POINT('Ctrl Pts',(-1.78007486300006,12.2,-10.660395184));
#295985=CARTESIAN_POINT('Ctrl Pts',(-1.77888690400006,12.2,-10.658006194));
#295986=CARTESIAN_POINT('Ctrl Pts',(-1.77770358700006,12.2,-10.655621476));
#295987=CARTESIAN_POINT('Ctrl Pts',(-1.77652491000006,12.2,-10.653241047));
#295988=CARTESIAN_POINT('Ctrl Pts',(-1.77535086900006,12.2,-10.65086492));
#295989=CARTESIAN_POINT('Ctrl Pts',(-1.77418146100006,12.2,-10.648493108));
#295990=CARTESIAN_POINT('Ctrl Pts',(-1.77301668500006,12.2,-10.646125627));
#295991=CARTESIAN_POINT('Ctrl Pts',(-1.77185653500006,12.2,-10.643762488));
#295992=CARTESIAN_POINT('Ctrl Pts',(-1.77070101200006,12.2,-10.641403708));
#295993=CARTESIAN_POINT('Ctrl Pts',(-1.76955010900006,12.2,-10.639049299));
#295994=CARTESIAN_POINT('Ctrl Pts',(-1.76840382600005,12.2,-10.636699276));
#295995=CARTESIAN_POINT('Ctrl Pts',(-1.76726215900006,12.2,-10.634353653));
#295996=CARTESIAN_POINT('Ctrl Pts',(-1.76612510400005,12.2,-10.632012444));
#295997=CARTESIAN_POINT('Ctrl Pts',(-1.76499265900006,12.2,-10.629675663));
#295998=CARTESIAN_POINT('Ctrl Pts',(-1.76386482100006,12.2,-10.627343324));
#295999=CARTESIAN_POINT('Ctrl Pts',(-1.76274158600006,12.2,-10.625015442));
#296000=CARTESIAN_POINT('Ctrl Pts',(-1.76162295200006,12.2,-10.622692031));
#296001=CARTESIAN_POINT('Ctrl Pts',(-1.76050891600006,12.2,-10.620373104));
#296002=CARTESIAN_POINT('Ctrl Pts',(-1.75939947300006,12.2,-10.618058678));
#296003=CARTESIAN_POINT('Ctrl Pts',(-1.75829462200006,12.2,-10.615748764));
#296004=CARTESIAN_POINT('Ctrl Pts',(-1.75719435900006,12.2,-10.61344338));
#296005=CARTESIAN_POINT('Ctrl Pts',(-1.75609868000006,12.2,-10.611142538));
#296006=CARTESIAN_POINT('Ctrl Pts',(-1.75500758400006,12.2,-10.608846253));
#296007=CARTESIAN_POINT('Ctrl Pts',(-1.75392106600006,12.2,-10.60655454));
#296008=CARTESIAN_POINT('Ctrl Pts',(-1.75283912300006,12.2,-10.604267414));
#296009=CARTESIAN_POINT('Ctrl Pts',(-1.75176175100006,12.2,-10.601984888));
#296010=CARTESIAN_POINT('Ctrl Pts',(-1.75068894900006,12.2,-10.599706978));
#296011=CARTESIAN_POINT('Ctrl Pts',(-1.74962071200006,12.2,-10.597433698));
#296012=CARTESIAN_POINT('Ctrl Pts',(-1.74855703600006,12.2,-10.595165063));
#296013=CARTESIAN_POINT('Ctrl Pts',(-1.74749792000006,12.2,-10.592901087));
#296014=CARTESIAN_POINT('Ctrl Pts',(-1.74644335700005,12.2,-10.590641786));
#296015=CARTESIAN_POINT('Ctrl Pts',(-1.74539334800006,12.2,-10.588387175));
#296016=CARTESIAN_POINT('Ctrl Pts',(-1.74434788700006,12.2,-10.586137267));
#296017=CARTESIAN_POINT('Ctrl Pts',(-1.74330697100005,12.2,-10.58389208));
#296018=CARTESIAN_POINT('Ctrl Pts',(-1.74227059600006,12.2,-10.581651626));
#296019=CARTESIAN_POINT('Ctrl Pts',(-1.74123875900006,12.2,-10.57941592));
#296020=CARTESIAN_POINT('Ctrl Pts',(-1.74021145800005,12.2,-10.577184979));
#296021=CARTESIAN_POINT('Ctrl Pts',(-1.73918868600006,12.2,-10.574958817));
#296022=CARTESIAN_POINT('Ctrl Pts',(-1.73817044300006,12.2,-10.572737449));
#296023=CARTESIAN_POINT('Ctrl Pts',(-1.73715672500005,12.2,-10.570520891));
#296024=CARTESIAN_POINT('Ctrl Pts',(-1.73614752700006,12.2,-10.568309157));
#296025=CARTESIAN_POINT('Ctrl Pts',(-1.73514284500006,12.2,-10.566102263));
#296026=CARTESIAN_POINT('Ctrl Pts',(-1.73414267600006,12.2,-10.563900224));
#296027=CARTESIAN_POINT('Ctrl Pts',(-1.73314701900006,12.2,-10.561703056));
#296028=CARTESIAN_POINT('Ctrl Pts',(-1.73215586600006,12.2,-10.559510773));
#296029=CARTESIAN_POINT('Ctrl Pts',(-1.73116921600006,12.2,-10.55732339));
#296030=CARTESIAN_POINT('Ctrl Pts',(-1.73018706500006,12.2,-10.555140925));
#296031=CARTESIAN_POINT('Ctrl Pts',(-1.72920940800006,12.2,-10.552963391));
#296032=CARTESIAN_POINT('Ctrl Pts',(-1.72823624300006,12.2,-10.550790805));
#296033=CARTESIAN_POINT('Ctrl Pts',(-1.72726756600006,12.2,-10.548623183));
#296034=CARTESIAN_POINT('Ctrl Pts',(-1.72630337200005,12.2,-10.546460538));
#296035=CARTESIAN_POINT('Ctrl Pts',(-1.72534365800006,12.2,-10.544302889));
#296036=CARTESIAN_POINT('Ctrl Pts',(-1.72438842000005,12.2,-10.542150249));
#296037=CARTESIAN_POINT('Ctrl Pts',(-1.72343765400006,12.2,-10.540002635));
#296038=CARTESIAN_POINT('Ctrl Pts',(-1.72249135800006,12.2,-10.537860062));
#296039=CARTESIAN_POINT('Ctrl Pts',(-1.72154952600006,12.2,-10.535722547));
#296040=CARTESIAN_POINT('Ctrl Pts',(-1.72061215300006,12.2,-10.533590105));
#296041=CARTESIAN_POINT('Ctrl Pts',(-1.71967923800006,12.2,-10.531462752));
#296042=CARTESIAN_POINT('Ctrl Pts',(-1.71875077600005,12.2,-10.529340504));
#296043=CARTESIAN_POINT('Ctrl Pts',(-1.71782676200006,12.2,-10.527223376));
#296044=CARTESIAN_POINT('Ctrl Pts',(-1.71690719200006,12.2,-10.525111386));
#296045=CARTESIAN_POINT('Ctrl Pts',(-1.71599206400006,12.2,-10.523004549));
#296046=CARTESIAN_POINT('Ctrl Pts',(-1.71508137200005,12.2,-10.520902882));
#296047=CARTESIAN_POINT('Ctrl Pts',(-1.71417511300006,12.2,-10.5188064));
#296048=CARTESIAN_POINT('Ctrl Pts',(-1.71327328300006,12.2,-10.516715119));
#296049=CARTESIAN_POINT('Ctrl Pts',(-1.71237587800006,12.2,-10.514629056));
#296050=CARTESIAN_POINT('Ctrl Pts',(-1.71148289100006,12.2,-10.512548228));
#296051=CARTESIAN_POINT('Ctrl Pts',(-1.71059432200006,12.2,-10.510472651));
#296052=CARTESIAN_POINT('Ctrl Pts',(-1.70971016400005,12.2,-10.50840234));
#296053=CARTESIAN_POINT('Ctrl Pts',(-1.70883041500006,12.2,-10.506337312));
#296054=CARTESIAN_POINT('Ctrl Pts',(-1.70795506800005,12.2,-10.504277584));
#296055=CARTESIAN_POINT('Ctrl Pts',(-1.70708412100006,12.2,-10.502223174));
#296056=CARTESIAN_POINT('Ctrl Pts',(-1.70621756900006,12.2,-10.500174096));
#296057=CARTESIAN_POINT('Ctrl Pts',(-1.70535540700006,12.2,-10.498130368));
#296058=CARTESIAN_POINT('Ctrl Pts',(-1.70449763200006,12.2,-10.496092006));
#296059=CARTESIAN_POINT('Ctrl Pts',(-1.70364423900006,12.2,-10.494059027));
#296060=CARTESIAN_POINT('Ctrl Pts',(-1.70279522300006,12.2,-10.492031449));
#296061=CARTESIAN_POINT('Ctrl Pts',(-1.70195058100005,12.2,-10.490009287));
#296062=CARTESIAN_POINT('Ctrl Pts',(-1.70111030700005,12.2,-10.487992559));
#296063=CARTESIAN_POINT('Ctrl Pts',(-1.70027439800006,12.2,-10.485981281));
#296064=CARTESIAN_POINT('Ctrl Pts',(-1.69944284900006,12.2,-10.483975472));
#296065=CARTESIAN_POINT('Ctrl Pts',(-1.69861565500006,12.2,-10.481975146));
#296066=CARTESIAN_POINT('Ctrl Pts',(-1.69779281100006,12.2,-10.479980323));
#296067=CARTESIAN_POINT('Ctrl Pts',(-1.69697431500006,12.2,-10.477991019));
#296068=CARTESIAN_POINT('Ctrl Pts',(-1.69616015900006,12.2,-10.476007249));
#296069=CARTESIAN_POINT('Ctrl Pts',(-1.69535034100006,12.2,-10.474029034));
#296070=CARTESIAN_POINT('Ctrl Pts',(-1.69454485500005,12.2,-10.47205639));
#296071=CARTESIAN_POINT('Ctrl Pts',(-1.69374369700006,12.2,-10.470089332));
#296072=CARTESIAN_POINT('Ctrl Pts',(-1.69294686200006,12.2,-10.468127881));
#296073=CARTESIAN_POINT('Ctrl Pts',(-1.69215434600006,12.2,-10.466172052));
#296074=CARTESIAN_POINT('Ctrl Pts',(-1.69136614300006,12.2,-10.464221864));
#296075=CARTESIAN_POINT('Ctrl Pts',(-1.69058224900006,12.2,-10.462277333));
#296076=CARTESIAN_POINT('Ctrl Pts',(-1.68980265900006,12.2,-10.460338479));
#296077=CARTESIAN_POINT('Ctrl Pts',(-1.68902736900006,12.2,-10.458405316));
#296078=CARTESIAN_POINT('Ctrl Pts',(-1.68825637300006,12.2,-10.456477865));
#296079=CARTESIAN_POINT('Ctrl Pts',(-1.68748966700006,12.2,-10.454556142));
#296080=CARTESIAN_POINT('Ctrl Pts',(-1.68672724500006,12.2,-10.452640166));
#296081=CARTESIAN_POINT('Ctrl Pts',(-1.68596910300006,12.2,-10.450729954));
#296082=CARTESIAN_POINT('Ctrl Pts',(-1.68521523600006,12.2,-10.448825525));
#296083=CARTESIAN_POINT('Ctrl Pts',(-1.68446563900006,12.2,-10.446926896));
#296084=CARTESIAN_POINT('Ctrl Pts',(-1.68372030600006,12.2,-10.445034085));
#296085=CARTESIAN_POINT('Ctrl Pts',(-1.68297923400006,12.2,-10.44314711));
#296086=CARTESIAN_POINT('Ctrl Pts',(-1.68224241500006,12.2,-10.44126599));
#296087=CARTESIAN_POINT('Ctrl Pts',(-1.68150984700006,12.2,-10.439390743));
#296088=CARTESIAN_POINT('Ctrl Pts',(-1.68078152300006,12.2,-10.437521386));
#296089=CARTESIAN_POINT('Ctrl Pts',(-1.68005743900005,12.2,-10.435657939));
#296090=CARTESIAN_POINT('Ctrl Pts',(-1.67933758800005,12.2,-10.433800421));
#296091=CARTESIAN_POINT('Ctrl Pts',(-1.67862196700006,12.2,-10.431948849));
#296092=CARTESIAN_POINT('Ctrl Pts',(-1.67791057000006,12.2,-10.430103241));
#296093=CARTESIAN_POINT('Ctrl Pts',(-1.67720339000006,12.2,-10.428263616));
#296094=CARTESIAN_POINT('Ctrl Pts',(-1.67650042400005,12.2,-10.426429993));
#296095=CARTESIAN_POINT('Ctrl Pts',(-1.67580166700006,12.2,-10.424602391));
#296096=CARTESIAN_POINT('Ctrl Pts',(-1.67510711100005,12.2,-10.422780829));
#296097=CARTESIAN_POINT('Ctrl Pts',(-1.67441675200006,12.2,-10.420965325));
#296098=CARTESIAN_POINT('Ctrl Pts',(-1.67373058500006,12.2,-10.419155897));
#296099=CARTESIAN_POINT('Ctrl Pts',(-1.67304860500006,12.2,-10.417352566));
#296100=CARTESIAN_POINT('Ctrl Pts',(-1.67237080500006,12.2,-10.41555535));
#296101=CARTESIAN_POINT('Ctrl Pts',(-1.67169718000005,12.2,-10.413764268));
#296102=CARTESIAN_POINT('Ctrl Pts',(-1.67102772500006,12.2,-10.411979339));
#296103=CARTESIAN_POINT('Ctrl Pts',(-1.67036243400006,12.2,-10.410200583));
#296104=CARTESIAN_POINT('Ctrl Pts',(-1.66970130200006,12.2,-10.408428019));
#296105=CARTESIAN_POINT('Ctrl Pts',(-1.66904432300006,12.2,-10.406661664));
#296106=CARTESIAN_POINT('Ctrl Pts',(-1.66839149100006,12.2,-10.404901541));
#296107=CARTESIAN_POINT('Ctrl Pts',(-1.66774280000005,12.2,-10.403147668));
#296108=CARTESIAN_POINT('Ctrl Pts',(-1.66709824500006,12.2,-10.401400063));
#296109=CARTESIAN_POINT('Ctrl Pts',(-1.66645782000006,12.2,-10.399658748));
#296110=CARTESIAN_POINT('Ctrl Pts',(-1.66582152000006,12.2,-10.397923741));
#296111=CARTESIAN_POINT('Ctrl Pts',(-1.66518933800006,12.2,-10.396195062));
#296112=CARTESIAN_POINT('Ctrl Pts',(-1.66456126800006,12.2,-10.394472732));
#296113=CARTESIAN_POINT('Ctrl Pts',(-1.66393730600006,12.2,-10.392756769));
#296114=CARTESIAN_POINT('Ctrl Pts',(-1.66331744300006,12.2,-10.391047193));
#296115=CARTESIAN_POINT('Ctrl Pts',(-1.66270167700006,12.2,-10.389344026));
#296116=CARTESIAN_POINT('Ctrl Pts',(-1.66208999800005,12.2,-10.387647286));
#296117=CARTESIAN_POINT('Ctrl Pts',(-1.66148240300006,12.2,-10.385956994));
#296118=CARTESIAN_POINT('Ctrl Pts',(-1.66087888400006,12.2,-10.38427317));
#296119=CARTESIAN_POINT('Ctrl Pts',(-1.66027943500006,12.2,-10.382595835));
#296120=CARTESIAN_POINT('Ctrl Pts',(-1.65968405200006,12.2,-10.380925008));
#296121=CARTESIAN_POINT('Ctrl Pts',(-1.65909272600006,12.2,-10.37926071));
#296122=CARTESIAN_POINT('Ctrl Pts',(-1.65850545200006,12.2,-10.377602961));
#296123=CARTESIAN_POINT('Ctrl Pts',(-1.65792222600006,12.2,-10.375951783));
#296124=CARTESIAN_POINT('Ctrl Pts',(-1.65734303700006,12.2,-10.374307195));
#296125=CARTESIAN_POINT('Ctrl Pts',(-1.65676788300006,12.2,-10.372669218));
#296126=CARTESIAN_POINT('Ctrl Pts',(-1.65619675600006,12.2,-10.371037873));
#296127=CARTESIAN_POINT('Ctrl Pts',(-1.65562964900006,12.2,-10.369413181));
#296128=CARTESIAN_POINT('Ctrl Pts',(-1.65506655700006,12.2,-10.367795164));
#296129=CARTESIAN_POINT('Ctrl Pts',(-1.65450747200006,12.2,-10.36618384));
#296130=CARTESIAN_POINT('Ctrl Pts',(-1.65395238800006,12.2,-10.364579233));
#296131=CARTESIAN_POINT('Ctrl Pts',(-1.65340130000006,12.2,-10.362981362));
#296132=CARTESIAN_POINT('Ctrl Pts',(-1.65285419900006,12.2,-10.361390249));
#296133=CARTESIAN_POINT('Ctrl Pts',(-1.65231108000006,12.2,-10.359805917));
#296134=CARTESIAN_POINT('Ctrl Pts',(-1.65177193600006,12.2,-10.358228384));
#296135=CARTESIAN_POINT('Ctrl Pts',(-1.65123676100006,12.2,-10.356657674));
#296136=CARTESIAN_POINT('Ctrl Pts',(-1.65070554700006,12.2,-10.355093807));
#296137=CARTESIAN_POINT('Ctrl Pts',(-1.65017828800006,12.2,-10.353536807));
#296138=CARTESIAN_POINT('Ctrl Pts',(-1.64965497700006,12.2,-10.351986691));
#296139=CARTESIAN_POINT('Ctrl Pts',(-1.64913560800006,12.2,-10.350443486));
#296140=CARTESIAN_POINT('Ctrl Pts',(-1.64862017200006,12.2,-10.348907211));
#296141=CARTESIAN_POINT('Ctrl Pts',(-1.64810866500006,12.2,-10.347377888));
#296142=CARTESIAN_POINT('Ctrl Pts',(-1.64760107800005,12.2,-10.34585554));
#296143=CARTESIAN_POINT('Ctrl Pts',(-1.64709740400005,12.2,-10.344340188));
#296144=CARTESIAN_POINT('Ctrl Pts',(-1.64659763700006,12.2,-10.342831854));
#296145=CARTESIAN_POINT('Ctrl Pts',(-1.64610177000006,12.2,-10.341330563));
#296146=CARTESIAN_POINT('Ctrl Pts',(-1.64560979500005,12.2,-10.339836333));
#296147=CARTESIAN_POINT('Ctrl Pts',(-1.64512170500006,12.2,-10.33834919));
#296148=CARTESIAN_POINT('Ctrl Pts',(-1.64463749400006,12.2,-10.336869154));
#296149=CARTESIAN_POINT('Ctrl Pts',(-1.64415715300006,12.2,-10.33539625));
#296150=CARTESIAN_POINT('Ctrl Pts',(-1.64368067600006,12.2,-10.333930498));
#296151=CARTESIAN_POINT('Ctrl Pts',(-1.64320805500005,12.2,-10.332471923));
#296152=CARTESIAN_POINT('Ctrl Pts',(-1.64273928400006,12.2,-10.331020547));
#296153=CARTESIAN_POINT('Ctrl Pts',(-1.64227435300006,12.2,-10.329576392));
#296154=CARTESIAN_POINT('Ctrl Pts',(-1.64181325800006,12.2,-10.328139482));
#296155=CARTESIAN_POINT('Ctrl Pts',(-1.64135598800006,12.2,-10.32670984));
#296156=CARTESIAN_POINT('Ctrl Pts',(-1.64090253900006,12.2,-10.325287489));
#296157=CARTESIAN_POINT('Ctrl Pts',(-1.64045290000006,12.2,-10.323872454));
#296158=CARTESIAN_POINT('Ctrl Pts',(-1.64000706600006,12.2,-10.322464755));
#296159=CARTESIAN_POINT('Ctrl Pts',(-1.63956502700006,12.2,-10.321064418));
#296160=CARTESIAN_POINT('Ctrl Pts',(-1.63912677800006,12.2,-10.319671466));
#296161=CARTESIAN_POINT('Ctrl Pts',(-1.63869231000006,12.2,-10.318285921));
#296162=CARTESIAN_POINT('Ctrl Pts',(-1.63826161500006,12.2,-10.316907809));
#296163=CARTESIAN_POINT('Ctrl Pts',(-1.63783468500006,12.2,-10.315537154));
#296164=CARTESIAN_POINT('Ctrl Pts',(-1.63741151300006,12.2,-10.314173978));
#296165=CARTESIAN_POINT('Ctrl Pts',(-1.63699208900006,12.2,-10.312818307));
#296166=CARTESIAN_POINT('Ctrl Pts',(-1.63657640900006,12.2,-10.311470164));
#296167=CARTESIAN_POINT('Ctrl Pts',(-1.63616446000006,12.2,-10.310129573));
#296168=CARTESIAN_POINT('Ctrl Pts',(-1.63575623900006,12.2,-10.308796558));
#296169=CARTESIAN_POINT('Ctrl Pts',(-1.63535173400006,12.2,-10.307471145));
#296170=CARTESIAN_POINT('Ctrl Pts',(-1.63495093900006,12.2,-10.306153358));
#296171=CARTESIAN_POINT('Ctrl Pts',(-1.63455384500006,12.2,-10.30484322));
#296172=CARTESIAN_POINT('Ctrl Pts',(-1.63416044300006,12.2,-10.303540757));
#296173=CARTESIAN_POINT('Ctrl Pts',(-1.63377072600006,12.2,-10.302245994));
#296174=CARTESIAN_POINT('Ctrl Pts',(-1.63338468600006,12.2,-10.300958957));
#296175=CARTESIAN_POINT('Ctrl Pts',(-1.63300231200005,12.2,-10.299679669));
#296176=CARTESIAN_POINT('Ctrl Pts',(-1.63262359900005,12.2,-10.298408156));
#296177=CARTESIAN_POINT('Ctrl Pts',(-1.63224853600005,12.2,-10.297144443));
#296178=CARTESIAN_POINT('Ctrl Pts',(-1.63187711600006,12.2,-10.295888554));
#296179=CARTESIAN_POINT('Ctrl Pts',(-1.63150933000006,12.2,-10.294640518));
#296180=CARTESIAN_POINT('Ctrl Pts',(-1.63114516900006,12.2,-10.293400358));
#296181=CARTESIAN_POINT('Ctrl Pts',(-1.63078462400006,12.2,-10.292168099));
#296182=CARTESIAN_POINT('Ctrl Pts',(-1.63042768700006,12.2,-10.290943769));
#296183=CARTESIAN_POINT('Ctrl Pts',(-1.63007434900006,12.2,-10.289727392));
#296184=CARTESIAN_POINT('Ctrl Pts',(-1.62972460000006,12.2,-10.288518995));
#296185=CARTESIAN_POINT('Ctrl Pts',(-1.62937843400006,12.2,-10.287318604));
#296186=CARTESIAN_POINT('Ctrl Pts',(-1.62903583800006,12.2,-10.286126246));
#296187=CARTESIAN_POINT('Ctrl Pts',(-1.62869680700006,12.2,-10.284941945));
#296188=CARTESIAN_POINT('Ctrl Pts',(-1.62836133000006,12.2,-10.283765729));
#296189=CARTESIAN_POINT('Ctrl Pts',(-1.62802939800006,12.2,-10.282597626));
#296190=CARTESIAN_POINT('Ctrl Pts',(-1.62770100100006,12.2,-10.281437659));
#296191=CARTESIAN_POINT('Ctrl Pts',(-1.62737613100005,12.2,-10.280285858));
#296192=CARTESIAN_POINT('Ctrl Pts',(-1.62705477800006,12.2,-10.279142249));
#296193=CARTESIAN_POINT('Ctrl Pts',(-1.62673693500006,12.2,-10.278006858));
#296194=CARTESIAN_POINT('Ctrl Pts',(-1.62642258900005,12.2,-10.276879714));
#296195=CARTESIAN_POINT('Ctrl Pts',(-1.62611173300005,12.2,-10.275760843));
#296196=CARTESIAN_POINT('Ctrl Pts',(-1.62580435500006,12.2,-10.274650272));
#296197=CARTESIAN_POINT('Ctrl Pts',(-1.62550044800006,12.2,-10.27354803));
#296198=CARTESIAN_POINT('Ctrl Pts',(-1.62520000300006,12.2,-10.272454143));
#296199=CARTESIAN_POINT('Ctrl Pts',(-1.62490300800005,12.2,-10.27136864));
#296200=CARTESIAN_POINT('Ctrl Pts',(-1.62460945300006,12.2,-10.270291548));
#296201=CARTESIAN_POINT('Ctrl Pts',(-1.62431933100006,12.2,-10.269222895));
#296202=CARTESIAN_POINT('Ctrl Pts',(-1.62403263000006,12.2,-10.268162711));
#296203=CARTESIAN_POINT('Ctrl Pts',(-1.62374934000006,12.2,-10.267111021));
#296204=CARTESIAN_POINT('Ctrl Pts',(-1.62346945200006,12.2,-10.266067857));
#296205=CARTESIAN_POINT('Ctrl Pts',(-1.62319295600006,12.2,-10.265033246));
#296206=CARTESIAN_POINT('Ctrl Pts',(-1.62291984100006,12.2,-10.264007214));
#296207=CARTESIAN_POINT('Ctrl Pts',(-1.62265009700006,12.2,-10.262989795));
#296208=CARTESIAN_POINT('Ctrl Pts',(-1.62238371500006,12.2,-10.261981014));
#296209=CARTESIAN_POINT('Ctrl Pts',(-1.62212068400006,12.2,-10.260980901));
#296210=CARTESIAN_POINT('Ctrl Pts',(-1.62186099300006,12.2,-10.259989485));
#296211=CARTESIAN_POINT('Ctrl Pts',(-1.62160463200005,12.2,-10.259006796));
#296212=CARTESIAN_POINT('Ctrl Pts',(-1.62135159100006,12.2,-10.258032864));
#296213=CARTESIAN_POINT('Ctrl Pts',(-1.62110185800006,12.2,-10.257067717));
#296214=CARTESIAN_POINT('Ctrl Pts',(-1.62085542500006,12.2,-10.256111386));
#296215=CARTESIAN_POINT('Ctrl Pts',(-1.62061227900006,12.2,-10.255163901));
#296216=CARTESIAN_POINT('Ctrl Pts',(-1.62037241000006,12.2,-10.254225291));
#296217=CARTESIAN_POINT('Ctrl Pts',(-1.62013580800005,12.2,-10.253295586));
#296218=CARTESIAN_POINT('Ctrl Pts',(-1.61990246100005,12.2,-10.252374817));
#296219=CARTESIAN_POINT('Ctrl Pts',(-1.61967235800006,12.2,-10.251463016));
#296220=CARTESIAN_POINT('Ctrl Pts',(-1.61944548900005,12.2,-10.250560211));
#296221=CARTESIAN_POINT('Ctrl Pts',(-1.61922313100006,12.2,-10.249671582));
#296222=CARTESIAN_POINT('Ctrl Pts',(-1.61904803300006,12.2,-10.248968851));
#296223=CARTESIAN_POINT('Ctrl Pts',(-1.61891844100006,12.2,-10.248447089));
#296224=CARTESIAN_POINT('Ctrl Pts',(-1.61883308400005,12.2,-10.248102703));
#296225=CARTESIAN_POINT('Ctrl Pts',(-1.61879118000006,12.2,-10.247933456));
#296226=CARTESIAN_POINT('Ctrl Pts',(-1.61879118000006,15.2,-10.247933456));
#296227=CARTESIAN_POINT('Ctrl Pts',(-1.61883308400005,15.2,-10.248102703));
#296228=CARTESIAN_POINT('Ctrl Pts',(-1.61891844100006,15.2,-10.248447089));
#296229=CARTESIAN_POINT('Ctrl Pts',(-1.61904803300006,15.2,-10.248968851));
#296230=CARTESIAN_POINT('Ctrl Pts',(-1.61922313100006,15.2,-10.249671582));
#296231=CARTESIAN_POINT('Ctrl Pts',(-1.61944548900005,15.2,-10.250560211));
#296232=CARTESIAN_POINT('Ctrl Pts',(-1.61967235800006,15.2,-10.251463016));
#296233=CARTESIAN_POINT('Ctrl Pts',(-1.61990246100005,15.2,-10.252374817));
#296234=CARTESIAN_POINT('Ctrl Pts',(-1.62013580800005,15.2,-10.253295586));
#296235=CARTESIAN_POINT('Ctrl Pts',(-1.62037241000006,15.2,-10.254225291));
#296236=CARTESIAN_POINT('Ctrl Pts',(-1.62061227900006,15.2,-10.255163901));
#296237=CARTESIAN_POINT('Ctrl Pts',(-1.62085542500006,15.2,-10.256111386));
#296238=CARTESIAN_POINT('Ctrl Pts',(-1.62110185800006,15.2,-10.257067717));
#296239=CARTESIAN_POINT('Ctrl Pts',(-1.62135159100006,15.2,-10.258032864));
#296240=CARTESIAN_POINT('Ctrl Pts',(-1.62160463200005,15.2,-10.259006796));
#296241=CARTESIAN_POINT('Ctrl Pts',(-1.62186099300006,15.2,-10.259989485));
#296242=CARTESIAN_POINT('Ctrl Pts',(-1.62212068400006,15.2,-10.260980901));
#296243=CARTESIAN_POINT('Ctrl Pts',(-1.62238371500006,15.2,-10.261981014));
#296244=CARTESIAN_POINT('Ctrl Pts',(-1.62265009700006,15.2,-10.262989795));
#296245=CARTESIAN_POINT('Ctrl Pts',(-1.62291984100006,15.2,-10.264007214));
#296246=CARTESIAN_POINT('Ctrl Pts',(-1.62319295600006,15.2,-10.265033246));
#296247=CARTESIAN_POINT('Ctrl Pts',(-1.62346945200006,15.2,-10.266067857));
#296248=CARTESIAN_POINT('Ctrl Pts',(-1.62374934000006,15.2,-10.267111021));
#296249=CARTESIAN_POINT('Ctrl Pts',(-1.62403263000006,15.2,-10.268162711));
#296250=CARTESIAN_POINT('Ctrl Pts',(-1.62431933100006,15.2,-10.269222895));
#296251=CARTESIAN_POINT('Ctrl Pts',(-1.62460945300006,15.2,-10.270291548));
#296252=CARTESIAN_POINT('Ctrl Pts',(-1.62490300800005,15.2,-10.27136864));
#296253=CARTESIAN_POINT('Ctrl Pts',(-1.62520000300006,15.2,-10.272454143));
#296254=CARTESIAN_POINT('Ctrl Pts',(-1.62550044800006,15.2,-10.27354803));
#296255=CARTESIAN_POINT('Ctrl Pts',(-1.62580435500006,15.2,-10.274650272));
#296256=CARTESIAN_POINT('Ctrl Pts',(-1.62611173300005,15.2,-10.275760843));
#296257=CARTESIAN_POINT('Ctrl Pts',(-1.62642258900005,15.2,-10.276879714));
#296258=CARTESIAN_POINT('Ctrl Pts',(-1.62673693500006,15.2,-10.278006858));
#296259=CARTESIAN_POINT('Ctrl Pts',(-1.62705477800006,15.2,-10.279142249));
#296260=CARTESIAN_POINT('Ctrl Pts',(-1.62737613100005,15.2,-10.280285858));
#296261=CARTESIAN_POINT('Ctrl Pts',(-1.62770100100006,15.2,-10.281437659));
#296262=CARTESIAN_POINT('Ctrl Pts',(-1.62802939800006,15.2,-10.282597626));
#296263=CARTESIAN_POINT('Ctrl Pts',(-1.62836133000006,15.2,-10.283765729));
#296264=CARTESIAN_POINT('Ctrl Pts',(-1.62869680700006,15.2,-10.284941945));
#296265=CARTESIAN_POINT('Ctrl Pts',(-1.62903583800006,15.2,-10.286126246));
#296266=CARTESIAN_POINT('Ctrl Pts',(-1.62937843400006,15.2,-10.287318604));
#296267=CARTESIAN_POINT('Ctrl Pts',(-1.62972460000006,15.2,-10.288518995));
#296268=CARTESIAN_POINT('Ctrl Pts',(-1.63007434900006,15.2,-10.289727392));
#296269=CARTESIAN_POINT('Ctrl Pts',(-1.63042768700006,15.2,-10.290943769));
#296270=CARTESIAN_POINT('Ctrl Pts',(-1.63078462400006,15.2,-10.292168099));
#296271=CARTESIAN_POINT('Ctrl Pts',(-1.63114516900006,15.2,-10.293400358));
#296272=CARTESIAN_POINT('Ctrl Pts',(-1.63150933000006,15.2,-10.294640518));
#296273=CARTESIAN_POINT('Ctrl Pts',(-1.63187711600006,15.2,-10.295888554));
#296274=CARTESIAN_POINT('Ctrl Pts',(-1.63224853600005,15.2,-10.297144443));
#296275=CARTESIAN_POINT('Ctrl Pts',(-1.63262359900005,15.2,-10.298408156));
#296276=CARTESIAN_POINT('Ctrl Pts',(-1.63300231200005,15.2,-10.299679669));
#296277=CARTESIAN_POINT('Ctrl Pts',(-1.63338468600006,15.2,-10.300958957));
#296278=CARTESIAN_POINT('Ctrl Pts',(-1.63377072600006,15.2,-10.302245994));
#296279=CARTESIAN_POINT('Ctrl Pts',(-1.63416044300006,15.2,-10.303540757));
#296280=CARTESIAN_POINT('Ctrl Pts',(-1.63455384500006,15.2,-10.30484322));
#296281=CARTESIAN_POINT('Ctrl Pts',(-1.63495093900006,15.2,-10.306153358));
#296282=CARTESIAN_POINT('Ctrl Pts',(-1.63535173400006,15.2,-10.307471145));
#296283=CARTESIAN_POINT('Ctrl Pts',(-1.63575623900006,15.2,-10.308796558));
#296284=CARTESIAN_POINT('Ctrl Pts',(-1.63616446000006,15.2,-10.310129573));
#296285=CARTESIAN_POINT('Ctrl Pts',(-1.63657640900006,15.2,-10.311470164));
#296286=CARTESIAN_POINT('Ctrl Pts',(-1.63699208900006,15.2,-10.312818307));
#296287=CARTESIAN_POINT('Ctrl Pts',(-1.63741151300006,15.2,-10.314173978));
#296288=CARTESIAN_POINT('Ctrl Pts',(-1.63783468500006,15.2,-10.315537154));
#296289=CARTESIAN_POINT('Ctrl Pts',(-1.63826161500006,15.2,-10.316907809));
#296290=CARTESIAN_POINT('Ctrl Pts',(-1.63869231000006,15.2,-10.318285921));
#296291=CARTESIAN_POINT('Ctrl Pts',(-1.63912677800006,15.2,-10.319671466));
#296292=CARTESIAN_POINT('Ctrl Pts',(-1.63956502700006,15.2,-10.321064418));
#296293=CARTESIAN_POINT('Ctrl Pts',(-1.64000706600006,15.2,-10.322464755));
#296294=CARTESIAN_POINT('Ctrl Pts',(-1.64045290000006,15.2,-10.323872454));
#296295=CARTESIAN_POINT('Ctrl Pts',(-1.64090253900006,15.2,-10.325287489));
#296296=CARTESIAN_POINT('Ctrl Pts',(-1.64135598800006,15.2,-10.32670984));
#296297=CARTESIAN_POINT('Ctrl Pts',(-1.64181325800006,15.2,-10.328139482));
#296298=CARTESIAN_POINT('Ctrl Pts',(-1.64227435300006,15.2,-10.329576392));
#296299=CARTESIAN_POINT('Ctrl Pts',(-1.64273928400006,15.2,-10.331020547));
#296300=CARTESIAN_POINT('Ctrl Pts',(-1.64320805500005,15.2,-10.332471923));
#296301=CARTESIAN_POINT('Ctrl Pts',(-1.64368067600006,15.2,-10.333930498));
#296302=CARTESIAN_POINT('Ctrl Pts',(-1.64415715300006,15.2,-10.33539625));
#296303=CARTESIAN_POINT('Ctrl Pts',(-1.64463749400006,15.2,-10.336869154));
#296304=CARTESIAN_POINT('Ctrl Pts',(-1.64512170500006,15.2,-10.33834919));
#296305=CARTESIAN_POINT('Ctrl Pts',(-1.64560979500005,15.2,-10.339836333));
#296306=CARTESIAN_POINT('Ctrl Pts',(-1.64610177000006,15.2,-10.341330563));
#296307=CARTESIAN_POINT('Ctrl Pts',(-1.64659763700006,15.2,-10.342831854));
#296308=CARTESIAN_POINT('Ctrl Pts',(-1.64709740400005,15.2,-10.344340188));
#296309=CARTESIAN_POINT('Ctrl Pts',(-1.64760107800005,15.2,-10.34585554));
#296310=CARTESIAN_POINT('Ctrl Pts',(-1.64810866500006,15.2,-10.347377888));
#296311=CARTESIAN_POINT('Ctrl Pts',(-1.64862017200006,15.2,-10.348907211));
#296312=CARTESIAN_POINT('Ctrl Pts',(-1.64913560800006,15.2,-10.350443486));
#296313=CARTESIAN_POINT('Ctrl Pts',(-1.64965497700006,15.2,-10.351986691));
#296314=CARTESIAN_POINT('Ctrl Pts',(-1.65017828800006,15.2,-10.353536807));
#296315=CARTESIAN_POINT('Ctrl Pts',(-1.65070554700006,15.2,-10.355093807));
#296316=CARTESIAN_POINT('Ctrl Pts',(-1.65123676100006,15.2,-10.356657674));
#296317=CARTESIAN_POINT('Ctrl Pts',(-1.65177193600006,15.2,-10.358228384));
#296318=CARTESIAN_POINT('Ctrl Pts',(-1.65231108000006,15.2,-10.359805917));
#296319=CARTESIAN_POINT('Ctrl Pts',(-1.65285419900006,15.2,-10.361390249));
#296320=CARTESIAN_POINT('Ctrl Pts',(-1.65340130000006,15.2,-10.362981362));
#296321=CARTESIAN_POINT('Ctrl Pts',(-1.65395238800006,15.2,-10.364579233));
#296322=CARTESIAN_POINT('Ctrl Pts',(-1.65450747200006,15.2,-10.36618384));
#296323=CARTESIAN_POINT('Ctrl Pts',(-1.65506655700006,15.2,-10.367795164));
#296324=CARTESIAN_POINT('Ctrl Pts',(-1.65562964900006,15.2,-10.369413181));
#296325=CARTESIAN_POINT('Ctrl Pts',(-1.65619675600006,15.2,-10.371037873));
#296326=CARTESIAN_POINT('Ctrl Pts',(-1.65676788300006,15.2,-10.372669218));
#296327=CARTESIAN_POINT('Ctrl Pts',(-1.65734303700006,15.2,-10.374307195));
#296328=CARTESIAN_POINT('Ctrl Pts',(-1.65792222600006,15.2,-10.375951783));
#296329=CARTESIAN_POINT('Ctrl Pts',(-1.65850545200006,15.2,-10.377602961));
#296330=CARTESIAN_POINT('Ctrl Pts',(-1.65909272600006,15.2,-10.37926071));
#296331=CARTESIAN_POINT('Ctrl Pts',(-1.65968405200006,15.2,-10.380925008));
#296332=CARTESIAN_POINT('Ctrl Pts',(-1.66027943500006,15.2,-10.382595835));
#296333=CARTESIAN_POINT('Ctrl Pts',(-1.66087888400006,15.2,-10.38427317));
#296334=CARTESIAN_POINT('Ctrl Pts',(-1.66148240300006,15.2,-10.385956994));
#296335=CARTESIAN_POINT('Ctrl Pts',(-1.66208999800005,15.2,-10.387647286));
#296336=CARTESIAN_POINT('Ctrl Pts',(-1.66270167700006,15.2,-10.389344026));
#296337=CARTESIAN_POINT('Ctrl Pts',(-1.66331744300006,15.2,-10.391047193));
#296338=CARTESIAN_POINT('Ctrl Pts',(-1.66393730600006,15.2,-10.392756769));
#296339=CARTESIAN_POINT('Ctrl Pts',(-1.66456126800006,15.2,-10.394472732));
#296340=CARTESIAN_POINT('Ctrl Pts',(-1.66518933800006,15.2,-10.396195062));
#296341=CARTESIAN_POINT('Ctrl Pts',(-1.66582152000006,15.2,-10.397923741));
#296342=CARTESIAN_POINT('Ctrl Pts',(-1.66645782000006,15.2,-10.399658748));
#296343=CARTESIAN_POINT('Ctrl Pts',(-1.66709824500006,15.2,-10.401400063));
#296344=CARTESIAN_POINT('Ctrl Pts',(-1.66774280000005,15.2,-10.403147668));
#296345=CARTESIAN_POINT('Ctrl Pts',(-1.66839149100006,15.2,-10.404901541));
#296346=CARTESIAN_POINT('Ctrl Pts',(-1.66904432300006,15.2,-10.406661664));
#296347=CARTESIAN_POINT('Ctrl Pts',(-1.66970130200006,15.2,-10.408428019));
#296348=CARTESIAN_POINT('Ctrl Pts',(-1.67036243400006,15.2,-10.410200583));
#296349=CARTESIAN_POINT('Ctrl Pts',(-1.67102772500006,15.2,-10.411979339));
#296350=CARTESIAN_POINT('Ctrl Pts',(-1.67169718000005,15.2,-10.413764268));
#296351=CARTESIAN_POINT('Ctrl Pts',(-1.67237080500006,15.2,-10.41555535));
#296352=CARTESIAN_POINT('Ctrl Pts',(-1.67304860500006,15.2,-10.417352566));
#296353=CARTESIAN_POINT('Ctrl Pts',(-1.67373058500006,15.2,-10.419155897));
#296354=CARTESIAN_POINT('Ctrl Pts',(-1.67441675200006,15.2,-10.420965325));
#296355=CARTESIAN_POINT('Ctrl Pts',(-1.67510711100005,15.2,-10.422780829));
#296356=CARTESIAN_POINT('Ctrl Pts',(-1.67580166700006,15.2,-10.424602391));
#296357=CARTESIAN_POINT('Ctrl Pts',(-1.67650042400005,15.2,-10.426429993));
#296358=CARTESIAN_POINT('Ctrl Pts',(-1.67720339000006,15.2,-10.428263616));
#296359=CARTESIAN_POINT('Ctrl Pts',(-1.67791057000006,15.2,-10.430103241));
#296360=CARTESIAN_POINT('Ctrl Pts',(-1.67862196700006,15.2,-10.431948849));
#296361=CARTESIAN_POINT('Ctrl Pts',(-1.67933758800005,15.2,-10.433800421));
#296362=CARTESIAN_POINT('Ctrl Pts',(-1.68005743900005,15.2,-10.435657939));
#296363=CARTESIAN_POINT('Ctrl Pts',(-1.68078152300006,15.2,-10.437521386));
#296364=CARTESIAN_POINT('Ctrl Pts',(-1.68150984700006,15.2,-10.439390743));
#296365=CARTESIAN_POINT('Ctrl Pts',(-1.68224241500006,15.2,-10.44126599));
#296366=CARTESIAN_POINT('Ctrl Pts',(-1.68297923400006,15.2,-10.44314711));
#296367=CARTESIAN_POINT('Ctrl Pts',(-1.68372030600006,15.2,-10.445034085));
#296368=CARTESIAN_POINT('Ctrl Pts',(-1.68446563900006,15.2,-10.446926896));
#296369=CARTESIAN_POINT('Ctrl Pts',(-1.68521523600006,15.2,-10.448825525));
#296370=CARTESIAN_POINT('Ctrl Pts',(-1.68596910300006,15.2,-10.450729954));
#296371=CARTESIAN_POINT('Ctrl Pts',(-1.68672724500006,15.2,-10.452640166));
#296372=CARTESIAN_POINT('Ctrl Pts',(-1.68748966700006,15.2,-10.454556142));
#296373=CARTESIAN_POINT('Ctrl Pts',(-1.68825637300006,15.2,-10.456477865));
#296374=CARTESIAN_POINT('Ctrl Pts',(-1.68902736900006,15.2,-10.458405316));
#296375=CARTESIAN_POINT('Ctrl Pts',(-1.68980265900006,15.2,-10.460338479));
#296376=CARTESIAN_POINT('Ctrl Pts',(-1.69058224900006,15.2,-10.462277333));
#296377=CARTESIAN_POINT('Ctrl Pts',(-1.69136614300006,15.2,-10.464221864));
#296378=CARTESIAN_POINT('Ctrl Pts',(-1.69215434600006,15.2,-10.466172052));
#296379=CARTESIAN_POINT('Ctrl Pts',(-1.69294686200006,15.2,-10.468127881));
#296380=CARTESIAN_POINT('Ctrl Pts',(-1.69374369700006,15.2,-10.470089332));
#296381=CARTESIAN_POINT('Ctrl Pts',(-1.69454485500005,15.2,-10.47205639));
#296382=CARTESIAN_POINT('Ctrl Pts',(-1.69535034100006,15.2,-10.474029034));
#296383=CARTESIAN_POINT('Ctrl Pts',(-1.69616015900006,15.2,-10.476007249));
#296384=CARTESIAN_POINT('Ctrl Pts',(-1.69697431500006,15.2,-10.477991019));
#296385=CARTESIAN_POINT('Ctrl Pts',(-1.69779281100006,15.2,-10.479980323));
#296386=CARTESIAN_POINT('Ctrl Pts',(-1.69861565500006,15.2,-10.481975146));
#296387=CARTESIAN_POINT('Ctrl Pts',(-1.69944284900006,15.2,-10.483975472));
#296388=CARTESIAN_POINT('Ctrl Pts',(-1.70027439800006,15.2,-10.485981281));
#296389=CARTESIAN_POINT('Ctrl Pts',(-1.70111030700005,15.2,-10.487992559));
#296390=CARTESIAN_POINT('Ctrl Pts',(-1.70195058100005,15.2,-10.490009287));
#296391=CARTESIAN_POINT('Ctrl Pts',(-1.70279522300006,15.2,-10.492031449));
#296392=CARTESIAN_POINT('Ctrl Pts',(-1.70364423900006,15.2,-10.494059027));
#296393=CARTESIAN_POINT('Ctrl Pts',(-1.70449763200006,15.2,-10.496092006));
#296394=CARTESIAN_POINT('Ctrl Pts',(-1.70535540700006,15.2,-10.498130368));
#296395=CARTESIAN_POINT('Ctrl Pts',(-1.70621756900006,15.2,-10.500174096));
#296396=CARTESIAN_POINT('Ctrl Pts',(-1.70708412100006,15.2,-10.502223174));
#296397=CARTESIAN_POINT('Ctrl Pts',(-1.70795506800005,15.2,-10.504277584));
#296398=CARTESIAN_POINT('Ctrl Pts',(-1.70883041500006,15.2,-10.506337312));
#296399=CARTESIAN_POINT('Ctrl Pts',(-1.70971016400005,15.2,-10.50840234));
#296400=CARTESIAN_POINT('Ctrl Pts',(-1.71059432200006,15.2,-10.510472651));
#296401=CARTESIAN_POINT('Ctrl Pts',(-1.71148289100006,15.2,-10.512548228));
#296402=CARTESIAN_POINT('Ctrl Pts',(-1.71237587800006,15.2,-10.514629056));
#296403=CARTESIAN_POINT('Ctrl Pts',(-1.71327328300006,15.2,-10.516715119));
#296404=CARTESIAN_POINT('Ctrl Pts',(-1.71417511300006,15.2,-10.5188064));
#296405=CARTESIAN_POINT('Ctrl Pts',(-1.71508137200005,15.2,-10.520902882));
#296406=CARTESIAN_POINT('Ctrl Pts',(-1.71599206400006,15.2,-10.523004549));
#296407=CARTESIAN_POINT('Ctrl Pts',(-1.71690719200006,15.2,-10.525111386));
#296408=CARTESIAN_POINT('Ctrl Pts',(-1.71782676200006,15.2,-10.527223376));
#296409=CARTESIAN_POINT('Ctrl Pts',(-1.71875077600005,15.2,-10.529340504));
#296410=CARTESIAN_POINT('Ctrl Pts',(-1.71967923800006,15.2,-10.531462752));
#296411=CARTESIAN_POINT('Ctrl Pts',(-1.72061215300006,15.2,-10.533590105));
#296412=CARTESIAN_POINT('Ctrl Pts',(-1.72154952600006,15.2,-10.535722547));
#296413=CARTESIAN_POINT('Ctrl Pts',(-1.72249135800006,15.2,-10.537860062));
#296414=CARTESIAN_POINT('Ctrl Pts',(-1.72343765400006,15.2,-10.540002635));
#296415=CARTESIAN_POINT('Ctrl Pts',(-1.72438842000005,15.2,-10.542150249));
#296416=CARTESIAN_POINT('Ctrl Pts',(-1.72534365800006,15.2,-10.544302889));
#296417=CARTESIAN_POINT('Ctrl Pts',(-1.72630337200005,15.2,-10.546460538));
#296418=CARTESIAN_POINT('Ctrl Pts',(-1.72726756600006,15.2,-10.548623183));
#296419=CARTESIAN_POINT('Ctrl Pts',(-1.72823624300006,15.2,-10.550790805));
#296420=CARTESIAN_POINT('Ctrl Pts',(-1.72920940800006,15.2,-10.552963391));
#296421=CARTESIAN_POINT('Ctrl Pts',(-1.73018706500006,15.2,-10.555140925));
#296422=CARTESIAN_POINT('Ctrl Pts',(-1.73116921600006,15.2,-10.55732339));
#296423=CARTESIAN_POINT('Ctrl Pts',(-1.73215586600006,15.2,-10.559510773));
#296424=CARTESIAN_POINT('Ctrl Pts',(-1.73314701900006,15.2,-10.561703056));
#296425=CARTESIAN_POINT('Ctrl Pts',(-1.73414267600006,15.2,-10.563900224));
#296426=CARTESIAN_POINT('Ctrl Pts',(-1.73514284500006,15.2,-10.566102263));
#296427=CARTESIAN_POINT('Ctrl Pts',(-1.73614752700006,15.2,-10.568309157));
#296428=CARTESIAN_POINT('Ctrl Pts',(-1.73715672500005,15.2,-10.570520891));
#296429=CARTESIAN_POINT('Ctrl Pts',(-1.73817044300006,15.2,-10.572737449));
#296430=CARTESIAN_POINT('Ctrl Pts',(-1.73918868600006,15.2,-10.574958817));
#296431=CARTESIAN_POINT('Ctrl Pts',(-1.74021145800005,15.2,-10.577184979));
#296432=CARTESIAN_POINT('Ctrl Pts',(-1.74123875900006,15.2,-10.57941592));
#296433=CARTESIAN_POINT('Ctrl Pts',(-1.74227059600006,15.2,-10.581651626));
#296434=CARTESIAN_POINT('Ctrl Pts',(-1.74330697100005,15.2,-10.58389208));
#296435=CARTESIAN_POINT('Ctrl Pts',(-1.74434788700006,15.2,-10.586137267));
#296436=CARTESIAN_POINT('Ctrl Pts',(-1.74539334800006,15.2,-10.588387175));
#296437=CARTESIAN_POINT('Ctrl Pts',(-1.74644335700005,15.2,-10.590641786));
#296438=CARTESIAN_POINT('Ctrl Pts',(-1.74749792000006,15.2,-10.592901087));
#296439=CARTESIAN_POINT('Ctrl Pts',(-1.74855703600006,15.2,-10.595165063));
#296440=CARTESIAN_POINT('Ctrl Pts',(-1.74962071200006,15.2,-10.597433698));
#296441=CARTESIAN_POINT('Ctrl Pts',(-1.75068894900006,15.2,-10.599706978));
#296442=CARTESIAN_POINT('Ctrl Pts',(-1.75176175100006,15.2,-10.601984888));
#296443=CARTESIAN_POINT('Ctrl Pts',(-1.75283912300006,15.2,-10.604267414));
#296444=CARTESIAN_POINT('Ctrl Pts',(-1.75392106600006,15.2,-10.60655454));
#296445=CARTESIAN_POINT('Ctrl Pts',(-1.75500758400006,15.2,-10.608846253));
#296446=CARTESIAN_POINT('Ctrl Pts',(-1.75609868000006,15.2,-10.611142538));
#296447=CARTESIAN_POINT('Ctrl Pts',(-1.75719435900006,15.2,-10.61344338));
#296448=CARTESIAN_POINT('Ctrl Pts',(-1.75829462200006,15.2,-10.615748764));
#296449=CARTESIAN_POINT('Ctrl Pts',(-1.75939947300006,15.2,-10.618058678));
#296450=CARTESIAN_POINT('Ctrl Pts',(-1.76050891600006,15.2,-10.620373104));
#296451=CARTESIAN_POINT('Ctrl Pts',(-1.76162295200006,15.2,-10.622692031));
#296452=CARTESIAN_POINT('Ctrl Pts',(-1.76274158600006,15.2,-10.625015442));
#296453=CARTESIAN_POINT('Ctrl Pts',(-1.76386482100006,15.2,-10.627343324));
#296454=CARTESIAN_POINT('Ctrl Pts',(-1.76499265900006,15.2,-10.629675663));
#296455=CARTESIAN_POINT('Ctrl Pts',(-1.76612510400005,15.2,-10.632012444));
#296456=CARTESIAN_POINT('Ctrl Pts',(-1.76726215900006,15.2,-10.634353653));
#296457=CARTESIAN_POINT('Ctrl Pts',(-1.76840382600005,15.2,-10.636699276));
#296458=CARTESIAN_POINT('Ctrl Pts',(-1.76955010900006,15.2,-10.639049299));
#296459=CARTESIAN_POINT('Ctrl Pts',(-1.77070101200006,15.2,-10.641403708));
#296460=CARTESIAN_POINT('Ctrl Pts',(-1.77185653500006,15.2,-10.643762488));
#296461=CARTESIAN_POINT('Ctrl Pts',(-1.77301668500006,15.2,-10.646125627));
#296462=CARTESIAN_POINT('Ctrl Pts',(-1.77418146100006,15.2,-10.648493108));
#296463=CARTESIAN_POINT('Ctrl Pts',(-1.77535086900006,15.2,-10.65086492));
#296464=CARTESIAN_POINT('Ctrl Pts',(-1.77652491000006,15.2,-10.653241047));
#296465=CARTESIAN_POINT('Ctrl Pts',(-1.77770358700006,15.2,-10.655621476));
#296466=CARTESIAN_POINT('Ctrl Pts',(-1.77888690400006,15.2,-10.658006194));
#296467=CARTESIAN_POINT('Ctrl Pts',(-1.78007486300006,15.2,-10.660395184));
#296468=CARTESIAN_POINT('Ctrl Pts',(-1.78126746700006,15.2,-10.662788437));
#296469=CARTESIAN_POINT('Ctrl Pts',(-1.78246472000006,15.2,-10.665185935));
#296470=CARTESIAN_POINT('Ctrl Pts',(-1.78366662300005,15.2,-10.667587667));
#296471=CARTESIAN_POINT('Ctrl Pts',(-1.78487317800006,15.2,-10.669993617));
#296472=CARTESIAN_POINT('Ctrl Pts',(-1.78608439100006,15.2,-10.672403774));
#296473=CARTESIAN_POINT('Ctrl Pts',(-1.78730026300005,15.2,-10.674818122));
#296474=CARTESIAN_POINT('Ctrl Pts',(-1.78852079600006,15.2,-10.677236648));
#296475=CARTESIAN_POINT('Ctrl Pts',(-1.78974599400005,15.2,-10.67965934));
#296476=CARTESIAN_POINT('Ctrl Pts',(-1.79097586000006,15.2,-10.682086183));
#296477=CARTESIAN_POINT('Ctrl Pts',(-1.79221039500006,15.2,-10.684517164));
#296478=CARTESIAN_POINT('Ctrl Pts',(-1.79344960300006,15.2,-10.686952269));
#296479=CARTESIAN_POINT('Ctrl Pts',(-1.79469348600006,15.2,-10.689391486));
#296480=CARTESIAN_POINT('Ctrl Pts',(-1.79594204700006,15.2,-10.691834799));
#296481=CARTESIAN_POINT('Ctrl Pts',(-1.79719528800006,15.2,-10.694282196));
#296482=CARTESIAN_POINT('Ctrl Pts',(-1.79845321300005,15.2,-10.696733666));
#296483=CARTESIAN_POINT('Ctrl Pts',(-1.79971582300006,15.2,-10.699189192));
#296484=CARTESIAN_POINT('Ctrl Pts',(-1.80098312100006,15.2,-10.701648762));
#296485=CARTESIAN_POINT('Ctrl Pts',(-1.80225511100006,15.2,-10.704112363));
#296486=CARTESIAN_POINT('Ctrl Pts',(-1.80353179300006,15.2,-10.706579983));
#296487=CARTESIAN_POINT('Ctrl Pts',(-1.80481317200006,15.2,-10.709051608));
#296488=CARTESIAN_POINT('Ctrl Pts',(-1.80609924900006,15.2,-10.711527223));
#296489=CARTESIAN_POINT('Ctrl Pts',(-1.80739002700005,15.2,-10.714006817));
#296490=CARTESIAN_POINT('Ctrl Pts',(-1.80868550800006,15.2,-10.716490376));
#296491=CARTESIAN_POINT('Ctrl Pts',(-1.80998569500006,15.2,-10.718977888));
#296492=CARTESIAN_POINT('Ctrl Pts',(-1.81129059100006,15.2,-10.721469338));
#296493=CARTESIAN_POINT('Ctrl Pts',(-1.81260019800006,15.2,-10.723964715));
#296494=CARTESIAN_POINT('Ctrl Pts',(-1.81391451700006,15.2,-10.726464005));
#296495=CARTESIAN_POINT('Ctrl Pts',(-1.81523355200006,15.2,-10.728967196));
#296496=CARTESIAN_POINT('Ctrl Pts',(-1.81655730500006,15.2,-10.731474274));
#296497=CARTESIAN_POINT('Ctrl Pts',(-1.81788577800006,15.2,-10.733985227));
#296498=CARTESIAN_POINT('Ctrl Pts',(-1.81921897500006,15.2,-10.73650004));
#296499=CARTESIAN_POINT('Ctrl Pts',(-1.82055689600006,15.2,-10.739018703));
#296500=CARTESIAN_POINT('Ctrl Pts',(-1.82189954400006,15.2,-10.741541203));
#296501=CARTESIAN_POINT('Ctrl Pts',(-1.82324692200006,15.2,-10.744067526));
#296502=CARTESIAN_POINT('Ctrl Pts',(-1.82459903200006,15.2,-10.746597658));
#296503=CARTESIAN_POINT('Ctrl Pts',(-1.82595587600006,15.2,-10.749131589));
#296504=CARTESIAN_POINT('Ctrl Pts',(-1.82731745700006,15.2,-10.751669306));
#296505=CARTESIAN_POINT('Ctrl Pts',(-1.82868377600006,15.2,-10.754210794));
#296506=CARTESIAN_POINT('Ctrl Pts',(-1.83005483700006,15.2,-10.756756043));
#296507=CARTESIAN_POINT('Ctrl Pts',(-1.83143064100005,15.2,-10.759305039));
#296508=CARTESIAN_POINT('Ctrl Pts',(-1.83281119000006,15.2,-10.76185777));
#296509=CARTESIAN_POINT('Ctrl Pts',(-1.83419648600006,15.2,-10.764414223));
#296510=CARTESIAN_POINT('Ctrl Pts',(-1.83558653300006,15.2,-10.766974386));
#296511=CARTESIAN_POINT('Ctrl Pts',(-1.83698133100005,15.2,-10.769538245));
#296512=CARTESIAN_POINT('Ctrl Pts',(-1.83838088300006,15.2,-10.77210579));
#296513=CARTESIAN_POINT('Ctrl Pts',(-1.83978519200006,15.2,-10.774677008));
#296514=CARTESIAN_POINT('Ctrl Pts',(-1.84119425800006,15.2,-10.777251885));
#296515=CARTESIAN_POINT('Ctrl Pts',(-1.84260808600006,15.2,-10.77983041));
#296516=CARTESIAN_POINT('Ctrl Pts',(-1.84402667500006,15.2,-10.78241257));
#296517=CARTESIAN_POINT('Ctrl Pts',(-1.84545003000005,15.2,-10.784998353));
#296518=CARTESIAN_POINT('Ctrl Pts',(-1.84687815100005,15.2,-10.787587746));
#296519=CARTESIAN_POINT('Ctrl Pts',(-1.84831104100006,15.2,-10.790180739));
#296520=CARTESIAN_POINT('Ctrl Pts',(-1.84974870200006,15.2,-10.792777317));
#296521=CARTESIAN_POINT('Ctrl Pts',(-1.85119113400006,15.2,-10.795377469));
#296522=CARTESIAN_POINT('Ctrl Pts',(-1.85263834300006,15.2,-10.797981184));
#296523=CARTESIAN_POINT('Ctrl Pts',(-1.85409032800006,15.2,-10.800588447));
#296524=CARTESIAN_POINT('Ctrl Pts',(-1.85554709100006,15.2,-10.803199248));
#296525=CARTESIAN_POINT('Ctrl Pts',(-1.85700863500006,15.2,-10.805813575));
#296526=CARTESIAN_POINT('Ctrl Pts',(-1.85847496200006,15.2,-10.808431414));
#296527=CARTESIAN_POINT('Ctrl Pts',(-1.85994607300006,15.2,-10.811052755));
#296528=CARTESIAN_POINT('Ctrl Pts',(-1.86142197200006,15.2,-10.813677586));
#296529=CARTESIAN_POINT('Ctrl Pts',(-1.86290265800006,15.2,-10.816305894));
#296530=CARTESIAN_POINT('Ctrl Pts',(-1.86438813500006,15.2,-10.818937666));
#296531=CARTESIAN_POINT('Ctrl Pts',(-1.86587840400006,15.2,-10.821572893));
#296532=CARTESIAN_POINT('Ctrl Pts',(-1.86737346700005,15.2,-10.82421156));
#296533=CARTESIAN_POINT('Ctrl Pts',(-1.86887332500006,15.2,-10.826853656));
#296534=CARTESIAN_POINT('Ctrl Pts',(-1.87037798200006,15.2,-10.829499171));
#296535=CARTESIAN_POINT('Ctrl Pts',(-1.87188743800006,15.2,-10.832148091));
#296536=CARTESIAN_POINT('Ctrl Pts',(-1.87340169600006,15.2,-10.834800405));
#296537=CARTESIAN_POINT('Ctrl Pts',(-1.87492075700006,15.2,-10.837456101));
#296538=CARTESIAN_POINT('Ctrl Pts',(-1.87644462200006,15.2,-10.840115167));
#296539=CARTESIAN_POINT('Ctrl Pts',(-1.87797329500006,15.2,-10.842777593));
#296540=CARTESIAN_POINT('Ctrl Pts',(-1.87950677700006,15.2,-10.845443365));
#296541=CARTESIAN_POINT('Ctrl Pts',(-1.88104506800005,15.2,-10.848112472));
#296542=CARTESIAN_POINT('Ctrl Pts',(-1.88258817100006,15.2,-10.850784903));
#296543=CARTESIAN_POINT('Ctrl Pts',(-1.88413608800006,15.2,-10.853460644));
#296544=CARTESIAN_POINT('Ctrl Pts',(-1.88568882100005,15.2,-10.856139687));
#296545=CARTESIAN_POINT('Ctrl Pts',(-1.88724637200006,15.2,-10.858822018));
#296546=CARTESIAN_POINT('Ctrl Pts',(-1.88880874000006,15.2,-10.861507626));
#296547=CARTESIAN_POINT('Ctrl Pts',(-1.89037592900006,15.2,-10.8641965));
#296548=CARTESIAN_POINT('Ctrl Pts',(-1.89194794100006,15.2,-10.866888627));
#296549=CARTESIAN_POINT('Ctrl Pts',(-1.89352477600006,15.2,-10.869583997));
#296550=CARTESIAN_POINT('Ctrl Pts',(-1.89510643700005,15.2,-10.872282597));
#296551=CARTESIAN_POINT('Ctrl Pts',(-1.89669292500006,15.2,-10.874984418));
#296552=CARTESIAN_POINT('Ctrl Pts',(-1.89828424200006,15.2,-10.877689446));
#296553=CARTESIAN_POINT('Ctrl Pts',(-1.89988038900006,15.2,-10.880397671));
#296554=CARTESIAN_POINT('Ctrl Pts',(-1.90148136800006,15.2,-10.88310908));
#296555=CARTESIAN_POINT('Ctrl Pts',(-1.90308718100006,15.2,-10.885823664));
#296556=CARTESIAN_POINT('Ctrl Pts',(-1.90469782800006,15.2,-10.888541409));
#296557=CARTESIAN_POINT('Ctrl Pts',(-1.90631331200006,15.2,-10.891262307));
#296558=CARTESIAN_POINT('Ctrl Pts',(-1.90793363400006,15.2,-10.893986344));
#296559=CARTESIAN_POINT('Ctrl Pts',(-1.90955879600006,15.2,-10.89671351));
#296560=CARTESIAN_POINT('Ctrl Pts',(-1.91118879900006,15.2,-10.899443792));
#296561=CARTESIAN_POINT('Ctrl Pts',(-1.91282364500006,15.2,-10.902177181));
#296562=CARTESIAN_POINT('Ctrl Pts',(-1.91446333500006,15.2,-10.904913664));
#296563=CARTESIAN_POINT('Ctrl Pts',(-1.91610787000006,15.2,-10.907653232));
#296564=CARTESIAN_POINT('Ctrl Pts',(-1.91775725300006,15.2,-10.910395872));
#296565=CARTESIAN_POINT('Ctrl Pts',(-1.91941148400006,15.2,-10.913141573));
#296566=CARTESIAN_POINT('Ctrl Pts',(-1.92107056600005,15.2,-10.915890324));
#296567=CARTESIAN_POINT('Ctrl Pts',(-1.92273449900005,15.2,-10.918642115));
#296568=CARTESIAN_POINT('Ctrl Pts',(-1.92440328400005,15.2,-10.921396933));
#296569=CARTESIAN_POINT('Ctrl Pts',(-1.92607692400005,15.2,-10.924154768));
#296570=CARTESIAN_POINT('Ctrl Pts',(-1.92775541900006,15.2,-10.92691561));
#296571=CARTESIAN_POINT('Ctrl Pts',(-1.92943877200005,15.2,-10.929679446));
#296572=CARTESIAN_POINT('Ctrl Pts',(-1.93112698400005,15.2,-10.932446266));
#296573=CARTESIAN_POINT('Ctrl Pts',(-1.93282005500006,15.2,-10.935216058));
#296574=CARTESIAN_POINT('Ctrl Pts',(-1.93451798600006,15.2,-10.937988814));
#296575=CARTESIAN_POINT('Ctrl Pts',(-1.93622078100006,15.2,-10.940764519));
#296576=CARTESIAN_POINT('Ctrl Pts',(-1.93792843900006,15.2,-10.943543166));
#296577=CARTESIAN_POINT('Ctrl Pts',(-1.93964096300005,15.2,-10.946324741));
#296578=CARTESIAN_POINT('Ctrl Pts',(-1.94135835200006,15.2,-10.949109235));
#296579=CARTESIAN_POINT('Ctrl Pts',(-1.94308061000006,15.2,-10.951896636));
#296580=CARTESIAN_POINT('Ctrl Pts',(-1.94480773800006,15.2,-10.954686934));
#296581=CARTESIAN_POINT('Ctrl Pts',(-1.94653973400006,15.2,-10.957480118));
#296582=CARTESIAN_POINT('Ctrl Pts',(-1.94827660300006,15.2,-10.960276177));
#296583=CARTESIAN_POINT('Ctrl Pts',(-1.95001834500005,15.2,-10.963075101));
#296584=CARTESIAN_POINT('Ctrl Pts',(-1.95176495900005,15.2,-10.965876877));
#296585=CARTESIAN_POINT('Ctrl Pts',(-1.95351645100006,15.2,-10.968681498));
#296586=CARTESIAN_POINT('Ctrl Pts',(-1.95527281700006,15.2,-10.971488949));
#296587=CARTESIAN_POINT('Ctrl Pts',(-1.95703406200006,15.2,-10.974299223));
#296588=CARTESIAN_POINT('Ctrl Pts',(-1.95880018600006,15.2,-10.977112307));
#296589=CARTESIAN_POINT('Ctrl Pts',(-1.96057119000006,15.2,-10.979928192));
#296590=CARTESIAN_POINT('Ctrl Pts',(-1.96234707500006,15.2,-10.982746866));
#296591=CARTESIAN_POINT('Ctrl Pts',(-1.96412784300006,15.2,-10.985568319));
#296592=CARTESIAN_POINT('Ctrl Pts',(-1.96591349400005,15.2,-10.988392541));
#296593=CARTESIAN_POINT('Ctrl Pts',(-1.96770402900006,15.2,-10.99121952));
#296594=CARTESIAN_POINT('Ctrl Pts',(-1.96949945100006,15.2,-10.994049247));
#296595=CARTESIAN_POINT('Ctrl Pts',(-1.97129976000005,15.2,-10.996881712));
#296596=CARTESIAN_POINT('Ctrl Pts',(-1.97310495700005,15.2,-10.999716901));
#296597=CARTESIAN_POINT('Ctrl Pts',(-1.97491504200005,15.2,-11.002554807));
#296598=CARTESIAN_POINT('Ctrl Pts',(-1.97673001900006,15.2,-11.005395418));
#296599=CARTESIAN_POINT('Ctrl Pts',(-1.97854988600006,15.2,-11.008238724));
#296600=CARTESIAN_POINT('Ctrl Pts',(-1.98037464600006,15.2,-11.011084714));
#296601=CARTESIAN_POINT('Ctrl Pts',(-1.98220430000006,15.2,-11.013933379));
#296602=CARTESIAN_POINT('Ctrl Pts',(-1.98403884700005,15.2,-11.016784707));
#296603=CARTESIAN_POINT('Ctrl Pts',(-1.98587829000005,15.2,-11.019638689));
#296604=CARTESIAN_POINT('Ctrl Pts',(-1.98772263100006,15.2,-11.022495313));
#296605=CARTESIAN_POINT('Ctrl Pts',(-1.98957186800006,15.2,-11.025354571));
#296606=CARTESIAN_POINT('Ctrl Pts',(-1.99142600300006,15.2,-11.02821645));
#296607=CARTESIAN_POINT('Ctrl Pts',(-1.99328503900006,15.2,-11.031080942));
#296608=CARTESIAN_POINT('Ctrl Pts',(-1.99514897500006,15.2,-11.033948035));
#296609=CARTESIAN_POINT('Ctrl Pts',(-1.99701781300006,15.2,-11.03681772));
#296610=CARTESIAN_POINT('Ctrl Pts',(-1.99889155400006,15.2,-11.039689987));
#296611=CARTESIAN_POINT('Ctrl Pts',(-2.00077019700006,15.2,-11.042564824));
#296612=CARTESIAN_POINT('Ctrl Pts',(-2.00265374600006,15.2,-11.045442222));
#296613=CARTESIAN_POINT('Ctrl Pts',(-2.00454219900006,15.2,-11.048322171));
#296614=CARTESIAN_POINT('Ctrl Pts',(-2.00643555900006,15.2,-11.05120466));
#296615=CARTESIAN_POINT('Ctrl Pts',(-2.00833382600006,15.2,-11.054089681));
#296616=CARTESIAN_POINT('Ctrl Pts',(-2.01023700100006,15.2,-11.056977221));
#296617=CARTESIAN_POINT('Ctrl Pts',(-2.01214508600006,15.2,-11.059867271));
#296618=CARTESIAN_POINT('Ctrl Pts',(-2.01405807900006,15.2,-11.062759821));
#296619=CARTESIAN_POINT('Ctrl Pts',(-2.01597598400005,15.2,-11.065654863));
#296620=CARTESIAN_POINT('Ctrl Pts',(-2.01789880000006,15.2,-11.068552382));
#296621=CARTESIAN_POINT('Ctrl Pts',(-2.01982652900006,15.2,-11.071452373));
#296622=CARTESIAN_POINT('Ctrl Pts',(-2.02175917100006,15.2,-11.074354824));
#296623=CARTESIAN_POINT('Ctrl Pts',(-2.02369672800006,15.2,-11.077259724));
#296624=CARTESIAN_POINT('Ctrl Pts',(-2.02563919900005,15.2,-11.080167065));
#296625=CARTESIAN_POINT('Ctrl Pts',(-2.02758658500006,15.2,-11.083076836));
#296626=CARTESIAN_POINT('Ctrl Pts',(-2.02953889000006,15.2,-11.085989026));
#296627=CARTESIAN_POINT('Ctrl Pts',(-2.03149611100006,15.2,-11.088903627));
#296628=CARTESIAN_POINT('Ctrl Pts',(-2.03345825000006,15.2,-11.091820627));
#296629=CARTESIAN_POINT('Ctrl Pts',(-2.03542530900005,15.2,-11.094740019));
#296630=CARTESIAN_POINT('Ctrl Pts',(-2.03739728600006,15.2,-11.097661791));
#296631=CARTESIAN_POINT('Ctrl Pts',(-2.03937418400006,15.2,-11.100585934));
#296632=CARTESIAN_POINT('Ctrl Pts',(-2.04135600500006,15.2,-11.103512437));
#296633=CARTESIAN_POINT('Ctrl Pts',(-2.04334274700006,15.2,-11.106441291));
#296634=CARTESIAN_POINT('Ctrl Pts',(-2.04533441100006,15.2,-11.109372486));
#296635=CARTESIAN_POINT('Ctrl Pts',(-2.04733100000006,15.2,-11.112306013));
#296636=CARTESIAN_POINT('Ctrl Pts',(-2.04933251100006,15.2,-11.115241862));
#296637=CARTESIAN_POINT('Ctrl Pts',(-2.05133894900006,15.2,-11.118180023));
#296638=CARTESIAN_POINT('Ctrl Pts',(-2.05335031200006,15.2,-11.121120485));
#296639=CARTESIAN_POINT('Ctrl Pts',(-2.05536660000006,15.2,-11.12406324));
#296640=CARTESIAN_POINT('Ctrl Pts',(-2.05738781600005,15.2,-11.127008278));
#296641=CARTESIAN_POINT('Ctrl Pts',(-2.05941396000005,15.2,-11.129955589));
#296642=CARTESIAN_POINT('Ctrl Pts',(-2.06144503200006,15.2,-11.132905162));
#296643=CARTESIAN_POINT('Ctrl Pts',(-2.06348103200006,15.2,-11.13585699));
#296644=CARTESIAN_POINT('Ctrl Pts',(-2.06552196300006,15.2,-11.138811062));
#296645=CARTESIAN_POINT('Ctrl Pts',(-2.06756782400006,15.2,-11.141767369));
#296646=CARTESIAN_POINT('Ctrl Pts',(-2.06961861500006,15.2,-11.1447259));
#296647=CARTESIAN_POINT('Ctrl Pts',(-2.07167433800006,15.2,-11.147686647));
#296648=CARTESIAN_POINT('Ctrl Pts',(-2.07373499200005,15.2,-11.1506496));
#296649=CARTESIAN_POINT('Ctrl Pts',(-2.07580058000006,15.2,-11.153614748));
#296650=CARTESIAN_POINT('Ctrl Pts',(-2.07787110100006,15.2,-11.156582084));
#296651=CARTESIAN_POINT('Ctrl Pts',(-2.07994655600006,15.2,-11.159551596));
#296652=CARTESIAN_POINT('Ctrl Pts',(-2.08202694500006,15.2,-11.162523276));
#296653=CARTESIAN_POINT('Ctrl Pts',(-2.08411226900005,15.2,-11.165497114));
#296654=CARTESIAN_POINT('Ctrl Pts',(-2.08620252700006,15.2,-11.1684731));
#296655=CARTESIAN_POINT('Ctrl Pts',(-2.08829772300006,15.2,-11.171451227));
#296656=CARTESIAN_POINT('Ctrl Pts',(-2.09039785500006,15.2,-11.174431482));
#296657=CARTESIAN_POINT('Ctrl Pts',(-2.09250292400006,15.2,-11.177413859));
#296658=CARTESIAN_POINT('Ctrl Pts',(-2.09461293200006,15.2,-11.180398346));
#296659=CARTESIAN_POINT('Ctrl Pts',(-2.09672787600006,15.2,-11.183384935));
#296660=CARTESIAN_POINT('Ctrl Pts',(-2.09884776000006,15.2,-11.186373616));
#296661=CARTESIAN_POINT('Ctrl Pts',(-2.10097258200005,15.2,-11.18936438));
#296662=CARTESIAN_POINT('Ctrl Pts',(-2.10310234500006,15.2,-11.192357218));
#296663=CARTESIAN_POINT('Ctrl Pts',(-2.10523704700006,15.2,-11.19535212));
#296664=CARTESIAN_POINT('Ctrl Pts',(-2.10737669000005,15.2,-11.198349076));
#296665=CARTESIAN_POINT('Ctrl Pts',(-2.10952127400006,15.2,-11.201348078));
#296666=CARTESIAN_POINT('Ctrl Pts',(-2.11167080000005,15.2,-11.204349116));
#296667=CARTESIAN_POINT('Ctrl Pts',(-2.11382526700006,15.2,-11.207352181));
#296668=CARTESIAN_POINT('Ctrl Pts',(-2.11598467700005,15.2,-11.210357264));
#296669=CARTESIAN_POINT('Ctrl Pts',(-2.11814903000006,15.2,-11.213364356));
#296670=CARTESIAN_POINT('Ctrl Pts',(-2.12031832600006,15.2,-11.216373446));
#296671=CARTESIAN_POINT('Ctrl Pts',(-2.12249256500006,15.2,-11.219384528));
#296672=CARTESIAN_POINT('Ctrl Pts',(-2.12467174800006,15.2,-11.222397592));
#296673=CARTESIAN_POINT('Ctrl Pts',(-2.12685587600005,15.2,-11.225412626));
#296674=CARTESIAN_POINT('Ctrl Pts',(-2.12904494800005,15.2,-11.228429624));
#296675=CARTESIAN_POINT('Ctrl Pts',(-2.13123896500006,15.2,-11.231448574));
#296676=CARTESIAN_POINT('Ctrl Pts',(-2.13343792800006,15.2,-11.234469469));
#296677=CARTESIAN_POINT('Ctrl Pts',(-2.13564183800006,15.2,-11.237492297));
#296678=CARTESIAN_POINT('Ctrl Pts',(-2.13785069300005,15.2,-11.24051705));
#296679=CARTESIAN_POINT('Ctrl Pts',(-2.14006449500005,15.2,-11.243543721));
#296680=CARTESIAN_POINT('Ctrl Pts',(-2.14228324400006,15.2,-11.246572299));
#296681=CARTESIAN_POINT('Ctrl Pts',(-2.14450694000006,15.2,-11.249602777));
#296682=CARTESIAN_POINT('Ctrl Pts',(-2.14673558400006,15.2,-11.252635149));
#296683=CARTESIAN_POINT('Ctrl Pts',(-2.14896917600006,15.2,-11.255669403));
#296684=CARTESIAN_POINT('Ctrl Pts',(-2.15120771500006,15.2,-11.258705531));
#296685=CARTESIAN_POINT('Ctrl Pts',(-2.15345120200006,15.2,-11.261743524));
#296686=CARTESIAN_POINT('Ctrl Pts',(-2.15569963800006,15.2,-11.264783368));
#296687=CARTESIAN_POINT('Ctrl Pts',(-2.15795302500006,15.2,-11.267825054));
#296688=CARTESIAN_POINT('Ctrl Pts',(-2.16021136000006,15.2,-11.27086857));
#296689=CARTESIAN_POINT('Ctrl Pts',(-2.16247464600006,15.2,-11.273913908));
#296690=CARTESIAN_POINT('Ctrl Pts',(-2.16474288100006,15.2,-11.276961058));
#296691=CARTESIAN_POINT('Ctrl Pts',(-2.16701606700005,15.2,-11.280010015));
#296692=CARTESIAN_POINT('Ctrl Pts',(-2.16929420200006,15.2,-11.283060773));
#296693=CARTESIAN_POINT('Ctrl Pts',(-2.17157728800006,15.2,-11.286113334));
#296694=CARTESIAN_POINT('Ctrl Pts',(-2.17340771700006,15.2,-11.28855682));
#296695=CARTESIAN_POINT('Ctrl Pts',(-2.17478276600006,15.2,-11.290390245));
#296696=CARTESIAN_POINT('Ctrl Pts',(-2.17570045500006,15.2,-11.291612887));
#296697=CARTESIAN_POINT('Ctrl Pts',(-2.17615954800006,15.2,-11.292224299));
#296698=CARTESIAN_POINT('Origin',(-5.66257110645729E-14,15.2,-1.77635683940025E-14));
#296699=CARTESIAN_POINT('',(-1.18690176602512,15.2,-10.306885523551));
#296700=CARTESIAN_POINT('Origin',(-5.66257110645729E-14,15.2,-1.77635683940025E-14));
#296701=CARTESIAN_POINT('',(-0.143881228002569,15.2,-10.3740022745144));
#296702=CARTESIAN_POINT('Origin',(-5.66257110645729E-14,15.2,-1.77635683940025E-14));
#296703=CARTESIAN_POINT('',(-0.546958306000055,15.2,-11.486985532));
#296704=CARTESIAN_POINT('Ctrl Pts',(-0.143881228000057,15.2,-10.374002275));
#296705=CARTESIAN_POINT('Ctrl Pts',(-0.143898619000057,15.2,-10.374175763));
#296706=CARTESIAN_POINT('Ctrl Pts',(-0.143934095000056,15.2,-10.37452879));
#296707=CARTESIAN_POINT('Ctrl Pts',(-0.143988114000055,15.2,-10.375063685));
#296708=CARTESIAN_POINT('Ctrl Pts',(-0.144061421000057,15.2,-10.375784183));
#296709=CARTESIAN_POINT('Ctrl Pts',(-0.144155050000055,15.2,-10.376695412));
#296710=CARTESIAN_POINT('Ctrl Pts',(-0.144251127000056,15.2,-10.377621314));
#296711=CARTESIAN_POINT('Ctrl Pts',(-0.144349125000056,15.2,-10.378556581));
#296712=CARTESIAN_POINT('Ctrl Pts',(-0.144449058000056,15.2,-10.379501186));
#296713=CARTESIAN_POINT('Ctrl Pts',(-0.144550942000056,15.2,-10.380455099));
#296714=CARTESIAN_POINT('Ctrl Pts',(-0.144654791000055,15.2,-10.381418293));
#296715=CARTESIAN_POINT('Ctrl Pts',(-0.144760620000056,15.2,-10.382390738));
#296716=CARTESIAN_POINT('Ctrl Pts',(-0.144868446000055,15.2,-10.383372406));
#296717=CARTESIAN_POINT('Ctrl Pts',(-0.144978281000055,15.2,-10.38436327));
#296718=CARTESIAN_POINT('Ctrl Pts',(-0.145090142000056,15.2,-10.3853633));
#296719=CARTESIAN_POINT('Ctrl Pts',(-0.145204042000057,15.2,-10.38637247));
#296720=CARTESIAN_POINT('Ctrl Pts',(-0.145319997000056,15.2,-10.387390753));
#296721=CARTESIAN_POINT('Ctrl Pts',(-0.145438020000055,15.2,-10.388418119));
#296722=CARTESIAN_POINT('Ctrl Pts',(-0.145558126000056,15.2,-10.389454543));
#296723=CARTESIAN_POINT('Ctrl Pts',(-0.145680330000056,15.2,-10.390499995));
#296724=CARTESIAN_POINT('Ctrl Pts',(-0.145804646000055,15.2,-10.39155445));
#296725=CARTESIAN_POINT('Ctrl Pts',(-0.145931087000056,15.2,-10.392617881));
#296726=CARTESIAN_POINT('Ctrl Pts',(-0.146059668000056,15.2,-10.39369026));
#296727=CARTESIAN_POINT('Ctrl Pts',(-0.146190404000055,15.2,-10.394771561));
#296728=CARTESIAN_POINT('Ctrl Pts',(-0.146323306000056,15.2,-10.395861756));
#296729=CARTESIAN_POINT('Ctrl Pts',(-0.146458391000056,15.2,-10.39696082));
#296730=CARTESIAN_POINT('Ctrl Pts',(-0.146595671000057,15.2,-10.398068726));
#296731=CARTESIAN_POINT('Ctrl Pts',(-0.146735160000055,15.2,-10.399185446));
#296732=CARTESIAN_POINT('Ctrl Pts',(-0.146876872000057,15.2,-10.400310957));
#296733=CARTESIAN_POINT('Ctrl Pts',(-0.147020820000057,15.2,-10.401445231));
#296734=CARTESIAN_POINT('Ctrl Pts',(-0.147167017000056,15.2,-10.402588242));
#296735=CARTESIAN_POINT('Ctrl Pts',(-0.147315478000056,15.2,-10.403739965));
#296736=CARTESIAN_POINT('Ctrl Pts',(-0.147466215000056,15.2,-10.404900372));
#296737=CARTESIAN_POINT('Ctrl Pts',(-0.147619240000055,15.2,-10.40606944));
#296738=CARTESIAN_POINT('Ctrl Pts',(-0.147774569000055,15.2,-10.407247142));
#296739=CARTESIAN_POINT('Ctrl Pts',(-0.147932214000056,15.2,-10.408433454));
#296740=CARTESIAN_POINT('Ctrl Pts',(-0.148092187000056,15.2,-10.409628348));
#296741=CARTESIAN_POINT('Ctrl Pts',(-0.148254502000055,15.2,-10.410831802));
#296742=CARTESIAN_POINT('Ctrl Pts',(-0.148419173000055,15.2,-10.412043788));
#296743=CARTESIAN_POINT('Ctrl Pts',(-0.148586210000056,15.2,-10.413264283));
#296744=CARTESIAN_POINT('Ctrl Pts',(-0.148755627000057,15.2,-10.414493262));
#296745=CARTESIAN_POINT('Ctrl Pts',(-0.148927437000056,15.2,-10.4157307));
#296746=CARTESIAN_POINT('Ctrl Pts',(-0.149101652000055,15.2,-10.416976571));
#296747=CARTESIAN_POINT('Ctrl Pts',(-0.149278286000056,15.2,-10.418230852));
#296748=CARTESIAN_POINT('Ctrl Pts',(-0.149457350000055,15.2,-10.419493518));
#296749=CARTESIAN_POINT('Ctrl Pts',(-0.149638856000056,15.2,-10.420764545));
#296750=CARTESIAN_POINT('Ctrl Pts',(-0.149822818000055,15.2,-10.422043907));
#296751=CARTESIAN_POINT('Ctrl Pts',(-0.150009246000057,15.2,-10.423331583));
#296752=CARTESIAN_POINT('Ctrl Pts',(-0.150198154000056,15.2,-10.424627545));
#296753=CARTESIAN_POINT('Ctrl Pts',(-0.150389553000055,15.2,-10.425931773));
#296754=CARTESIAN_POINT('Ctrl Pts',(-0.150583457000056,15.2,-10.427244241));
#296755=CARTESIAN_POINT('Ctrl Pts',(-0.150779876000057,15.2,-10.428564925));
#296756=CARTESIAN_POINT('Ctrl Pts',(-0.150978823000055,15.2,-10.429893802));
#296757=CARTESIAN_POINT('Ctrl Pts',(-0.151180310000055,15.2,-10.431230848));
#296758=CARTESIAN_POINT('Ctrl Pts',(-0.151384347000055,15.2,-10.43257604));
#296759=CARTESIAN_POINT('Ctrl Pts',(-0.151590948000055,15.2,-10.433929354));
#296760=CARTESIAN_POINT('Ctrl Pts',(-0.151800122000055,15.2,-10.435290769));
#296761=CARTESIAN_POINT('Ctrl Pts',(-0.152011884000055,15.2,-10.436660258));
#296762=CARTESIAN_POINT('Ctrl Pts',(-0.152226243000056,15.2,-10.4380378));
#296763=CARTESIAN_POINT('Ctrl Pts',(-0.152443212000056,15.2,-10.439423372));
#296764=CARTESIAN_POINT('Ctrl Pts',(-0.152662802000056,15.2,-10.440816951));
#296765=CARTESIAN_POINT('Ctrl Pts',(-0.152885022000057,15.2,-10.442218514));
#296766=CARTESIAN_POINT('Ctrl Pts',(-0.153109888000056,15.2,-10.443628038));
#296767=CARTESIAN_POINT('Ctrl Pts',(-0.153337407000055,15.2,-10.4450455));
#296768=CARTESIAN_POINT('Ctrl Pts',(-0.153567593000057,15.2,-10.446470879));
#296769=CARTESIAN_POINT('Ctrl Pts',(-0.153800456000056,15.2,-10.447904152));
#296770=CARTESIAN_POINT('Ctrl Pts',(-0.154036006000055,15.2,-10.449345296));
#296771=CARTESIAN_POINT('Ctrl Pts',(-0.154274256000055,15.2,-10.450794288));
#296772=CARTESIAN_POINT('Ctrl Pts',(-0.154515216000056,15.2,-10.452251106));
#296773=CARTESIAN_POINT('Ctrl Pts',(-0.154758897000056,15.2,-10.45371573));
#296774=CARTESIAN_POINT('Ctrl Pts',(-0.155005310000057,15.2,-10.455188136));
#296775=CARTESIAN_POINT('Ctrl Pts',(-0.155254466000055,15.2,-10.456668302));
#296776=CARTESIAN_POINT('Ctrl Pts',(-0.155506375000056,15.2,-10.458156207));
#296777=CARTESIAN_POINT('Ctrl Pts',(-0.155761048000055,15.2,-10.459651829));
#296778=CARTESIAN_POINT('Ctrl Pts',(-0.156018496000057,15.2,-10.461155145));
#296779=CARTESIAN_POINT('Ctrl Pts',(-0.156278730000056,15.2,-10.462666135));
#296780=CARTESIAN_POINT('Ctrl Pts',(-0.156541758000056,15.2,-10.464184778));
#296781=CARTESIAN_POINT('Ctrl Pts',(-0.156807594000057,15.2,-10.46571105));
#296782=CARTESIAN_POINT('Ctrl Pts',(-0.157076245000055,15.2,-10.467244931));
#296783=CARTESIAN_POINT('Ctrl Pts',(-0.157347725000055,15.2,-10.4687864));
#296784=CARTESIAN_POINT('Ctrl Pts',(-0.157622041000056,15.2,-10.470335435));
#296785=CARTESIAN_POINT('Ctrl Pts',(-0.157899205000056,15.2,-10.471892016));
#296786=CARTESIAN_POINT('Ctrl Pts',(-0.158179227000056,15.2,-10.473456121));
#296787=CARTESIAN_POINT('Ctrl Pts',(-0.158462117000056,15.2,-10.475027729));
#296788=CARTESIAN_POINT('Ctrl Pts',(-0.158747884000056,15.2,-10.476606819));
#296789=CARTESIAN_POINT('Ctrl Pts',(-0.159036540000056,15.2,-10.478193371));
#296790=CARTESIAN_POINT('Ctrl Pts',(-0.159328094000056,15.2,-10.479787363));
#296791=CARTESIAN_POINT('Ctrl Pts',(-0.159622556000055,15.2,-10.481388775));
#296792=CARTESIAN_POINT('Ctrl Pts',(-0.159919937000056,15.2,-10.482997586));
#296793=CARTESIAN_POINT('Ctrl Pts',(-0.160220245000057,15.2,-10.484613776));
#296794=CARTESIAN_POINT('Ctrl Pts',(-0.160523489000056,15.2,-10.486237324));
#296795=CARTESIAN_POINT('Ctrl Pts',(-0.160829682000055,15.2,-10.487868211));
#296796=CARTESIAN_POINT('Ctrl Pts',(-0.161138833000055,15.2,-10.489506414));
#296797=CARTESIAN_POINT('Ctrl Pts',(-0.161450949000056,15.2,-10.491151915));
#296798=CARTESIAN_POINT('Ctrl Pts',(-0.161766042000057,15.2,-10.492804693));
#296799=CARTESIAN_POINT('Ctrl Pts',(-0.162084120000056,15.2,-10.494464728));
#296800=CARTESIAN_POINT('Ctrl Pts',(-0.162405194000056,15.2,-10.496131999));
#296801=CARTESIAN_POINT('Ctrl Pts',(-0.162729274000055,15.2,-10.497806488));
#296802=CARTESIAN_POINT('Ctrl Pts',(-0.163056366000056,15.2,-10.499488173));
#296803=CARTESIAN_POINT('Ctrl Pts',(-0.163386483000056,15.2,-10.501177036));
#296804=CARTESIAN_POINT('Ctrl Pts',(-0.163719632000056,15.2,-10.502873055));
#296805=CARTESIAN_POINT('Ctrl Pts',(-0.164055824000057,15.2,-10.504576212));
#296806=CARTESIAN_POINT('Ctrl Pts',(-0.164395067000056,15.2,-10.506286487));
#296807=CARTESIAN_POINT('Ctrl Pts',(-0.164737371000055,15.2,-10.508003862));
#296808=CARTESIAN_POINT('Ctrl Pts',(-0.165082744000056,15.2,-10.509728314));
#296809=CARTESIAN_POINT('Ctrl Pts',(-0.165431198000056,15.2,-10.511459826));
#296810=CARTESIAN_POINT('Ctrl Pts',(-0.165782737000055,15.2,-10.513198378));
#296811=CARTESIAN_POINT('Ctrl Pts',(-0.166137374000056,15.2,-10.514943952));
#296812=CARTESIAN_POINT('Ctrl Pts',(-0.166495117000055,15.2,-10.516696527));
#296813=CARTESIAN_POINT('Ctrl Pts',(-0.166855974000055,15.2,-10.518456084));
#296814=CARTESIAN_POINT('Ctrl Pts',(-0.167219956000055,15.2,-10.520222604));
#296815=CARTESIAN_POINT('Ctrl Pts',(-0.167587069000056,15.2,-10.521996069));
#296816=CARTESIAN_POINT('Ctrl Pts',(-0.167957324000056,15.2,-10.523776458));
#296817=CARTESIAN_POINT('Ctrl Pts',(-0.168330729000056,15.2,-10.525563754));
#296818=CARTESIAN_POINT('Ctrl Pts',(-0.168707293000055,15.2,-10.527357938));
#296819=CARTESIAN_POINT('Ctrl Pts',(-0.169087023000056,15.2,-10.529158991));
#296820=CARTESIAN_POINT('Ctrl Pts',(-0.169469930000057,15.2,-10.530966892));
#296821=CARTESIAN_POINT('Ctrl Pts',(-0.169856021000055,15.2,-10.532781626));
#296822=CARTESIAN_POINT('Ctrl Pts',(-0.170245305000056,15.2,-10.534603171));
#296823=CARTESIAN_POINT('Ctrl Pts',(-0.170637791000056,15.2,-10.536431511));
#296824=CARTESIAN_POINT('Ctrl Pts',(-0.171033486000055,15.2,-10.538266627));
#296825=CARTESIAN_POINT('Ctrl Pts',(-0.171432400000056,15.2,-10.5401085));
#296826=CARTESIAN_POINT('Ctrl Pts',(-0.171834541000055,15.2,-10.541957111));
#296827=CARTESIAN_POINT('Ctrl Pts',(-0.172239916000055,15.2,-10.543812443));
#296828=CARTESIAN_POINT('Ctrl Pts',(-0.172648536000055,15.2,-10.545674477));
#296829=CARTESIAN_POINT('Ctrl Pts',(-0.173060406000056,15.2,-10.547543195));
#296830=CARTESIAN_POINT('Ctrl Pts',(-0.173475537000056,15.2,-10.549418579));
#296831=CARTESIAN_POINT('Ctrl Pts',(-0.173893934000056,15.2,-10.551300611));
#296832=CARTESIAN_POINT('Ctrl Pts',(-0.174315609000055,15.2,-10.553189273));
#296833=CARTESIAN_POINT('Ctrl Pts',(-0.174740568000056,15.2,-10.555084546));
#296834=CARTESIAN_POINT('Ctrl Pts',(-0.175168818000057,15.2,-10.556986413));
#296835=CARTESIAN_POINT('Ctrl Pts',(-0.175600369000056,15.2,-10.558894856));
#296836=CARTESIAN_POINT('Ctrl Pts',(-0.176035228000057,15.2,-10.560809857));
#296837=CARTESIAN_POINT('Ctrl Pts',(-0.176473403000056,15.2,-10.562731399));
#296838=CARTESIAN_POINT('Ctrl Pts',(-0.176914903000055,15.2,-10.564659465));
#296839=CARTESIAN_POINT('Ctrl Pts',(-0.177359734000057,15.2,-10.566594035));
#296840=CARTESIAN_POINT('Ctrl Pts',(-0.177807905000057,15.2,-10.568535092));
#296841=CARTESIAN_POINT('Ctrl Pts',(-0.178259423000057,15.2,-10.570482619));
#296842=CARTESIAN_POINT('Ctrl Pts',(-0.178714296000055,15.2,-10.572436599));
#296843=CARTESIAN_POINT('Ctrl Pts',(-0.179172532000056,15.2,-10.574397014));
#296844=CARTESIAN_POINT('Ctrl Pts',(-0.179634139000056,15.2,-10.576363848));
#296845=CARTESIAN_POINT('Ctrl Pts',(-0.180099125000056,15.2,-10.578337081));
#296846=CARTESIAN_POINT('Ctrl Pts',(-0.180567496000055,15.2,-10.580316698));
#296847=CARTESIAN_POINT('Ctrl Pts',(-0.181039260000055,15.2,-10.582302681));
#296848=CARTESIAN_POINT('Ctrl Pts',(-0.181514425000057,15.2,-10.584295012));
#296849=CARTESIAN_POINT('Ctrl Pts',(-0.181992998000055,15.2,-10.586293676));
#296850=CARTESIAN_POINT('Ctrl Pts',(-0.182474988000055,15.2,-10.588298654));
#296851=CARTESIAN_POINT('Ctrl Pts',(-0.182960401000055,15.2,-10.59030993));
#296852=CARTESIAN_POINT('Ctrl Pts',(-0.183449244000055,15.2,-10.592327487));
#296853=CARTESIAN_POINT('Ctrl Pts',(-0.183941526000057,15.2,-10.594351307));
#296854=CARTESIAN_POINT('Ctrl Pts',(-0.184437253000055,15.2,-10.596381375));
#296855=CARTESIAN_POINT('Ctrl Pts',(-0.184936432000056,15.2,-10.598417672));
#296856=CARTESIAN_POINT('Ctrl Pts',(-0.185439071000056,15.2,-10.600460183));
#296857=CARTESIAN_POINT('Ctrl Pts',(-0.185945177000055,15.2,-10.602508892));
#296858=CARTESIAN_POINT('Ctrl Pts',(-0.186454758000056,15.2,-10.60456378));
#296859=CARTESIAN_POINT('Ctrl Pts',(-0.186967820000056,15.2,-10.606624832));
#296860=CARTESIAN_POINT('Ctrl Pts',(-0.187484370000056,15.2,-10.60869203));
#296861=CARTESIAN_POINT('Ctrl Pts',(-0.188004417000055,15.2,-10.610765359));
#296862=CARTESIAN_POINT('Ctrl Pts',(-0.188527965000055,15.2,-10.612844802));
#296863=CARTESIAN_POINT('Ctrl Pts',(-0.189055024000057,15.2,-10.614930343));
#296864=CARTESIAN_POINT('Ctrl Pts',(-0.189585599000056,15.2,-10.617021965));
#296865=CARTESIAN_POINT('Ctrl Pts',(-0.190119697000056,15.2,-10.619119652));
#296866=CARTESIAN_POINT('Ctrl Pts',(-0.190657326000055,15.2,-10.621223388));
#296867=CARTESIAN_POINT('Ctrl Pts',(-0.191198493000057,15.2,-10.623333156));
#296868=CARTESIAN_POINT('Ctrl Pts',(-0.191743203000057,15.2,-10.62544894));
#296869=CARTESIAN_POINT('Ctrl Pts',(-0.192291464000055,15.2,-10.627570723));
#296870=CARTESIAN_POINT('Ctrl Pts',(-0.192843283000055,15.2,-10.629698492));
#296871=CARTESIAN_POINT('Ctrl Pts',(-0.193398667000055,15.2,-10.631832228));
#296872=CARTESIAN_POINT('Ctrl Pts',(-0.193957623000056,15.2,-10.633971916));
#296873=CARTESIAN_POINT('Ctrl Pts',(-0.194520156000056,15.2,-10.636117541));
#296874=CARTESIAN_POINT('Ctrl Pts',(-0.195086274000056,15.2,-10.638269086));
#296875=CARTESIAN_POINT('Ctrl Pts',(-0.195655982000057,15.2,-10.640426534));
#296876=CARTESIAN_POINT('Ctrl Pts',(-0.196229289000056,15.2,-10.642589871));
#296877=CARTESIAN_POINT('Ctrl Pts',(-0.196806201000056,15.2,-10.644759081));
#296878=CARTESIAN_POINT('Ctrl Pts',(-0.197386723000056,15.2,-10.646934148));
#296879=CARTESIAN_POINT('Ctrl Pts',(-0.197970862000056,15.2,-10.649115056));
#296880=CARTESIAN_POINT('Ctrl Pts',(-0.198558626000055,15.2,-10.651301789));
#296881=CARTESIAN_POINT('Ctrl Pts',(-0.199150020000056,15.2,-10.653494333));
#296882=CARTESIAN_POINT('Ctrl Pts',(-0.199745051000055,15.2,-10.655692671));
#296883=CARTESIAN_POINT('Ctrl Pts',(-0.200343725000056,15.2,-10.657896788));
#296884=CARTESIAN_POINT('Ctrl Pts',(-0.200946049000056,15.2,-10.660106669));
#296885=CARTESIAN_POINT('Ctrl Pts',(-0.201552028000057,15.2,-10.662322297));
#296886=CARTESIAN_POINT('Ctrl Pts',(-0.202161670000055,15.2,-10.664543659));
#296887=CARTESIAN_POINT('Ctrl Pts',(-0.202774980000056,15.2,-10.666770738));
#296888=CARTESIAN_POINT('Ctrl Pts',(-0.203391965000056,15.2,-10.669003519));
#296889=CARTESIAN_POINT('Ctrl Pts',(-0.204012631000056,15.2,-10.671241986));
#296890=CARTESIAN_POINT('Ctrl Pts',(-0.204636983000055,15.2,-10.673486125));
#296891=CARTESIAN_POINT('Ctrl Pts',(-0.205265029000056,15.2,-10.67573592));
#296892=CARTESIAN_POINT('Ctrl Pts',(-0.205896774000056,15.2,-10.677991357));
#296893=CARTESIAN_POINT('Ctrl Pts',(-0.206532225000055,15.2,-10.68025242));
#296894=CARTESIAN_POINT('Ctrl Pts',(-0.207171387000056,15.2,-10.682519093));
#296895=CARTESIAN_POINT('Ctrl Pts',(-0.207814267000056,15.2,-10.684791362));
#296896=CARTESIAN_POINT('Ctrl Pts',(-0.208460870000057,15.2,-10.687069213));
#296897=CARTESIAN_POINT('Ctrl Pts',(-0.209111203000055,15.2,-10.68935263));
#296898=CARTESIAN_POINT('Ctrl Pts',(-0.209765271000055,15.2,-10.691641597));
#296899=CARTESIAN_POINT('Ctrl Pts',(-0.210423081000056,15.2,-10.693936102));
#296900=CARTESIAN_POINT('Ctrl Pts',(-0.211084639000055,15.2,-10.696236127));
#296901=CARTESIAN_POINT('Ctrl Pts',(-0.211749948000056,15.2,-10.69854166));
#296902=CARTESIAN_POINT('Ctrl Pts',(-0.212419019000055,15.2,-10.700852684));
#296903=CARTESIAN_POINT('Ctrl Pts',(-0.213091853000057,15.2,-10.703169187));
#296904=CARTESIAN_POINT('Ctrl Pts',(-0.213903779044305,15.2,-10.7059555439519));
#296905=CARTESIAN_POINT('Ctrl Pts',(-0.214721369015063,15.2,-10.708750071151));
#296906=CARTESIAN_POINT('Ctrl Pts',(-0.21554463698505,15.2,-10.711552744849));
#296907=CARTESIAN_POINT('Ctrl Pts',(-0.21637359103007,15.2,-10.714363529302));
#296908=CARTESIAN_POINT('Ctrl Pts',(-0.217208245000055,15.2,-10.7171824));
#296909=CARTESIAN_POINT('Ctrl Pts',(-0.217907594000056,15.2,-10.719536833));
#296910=CARTESIAN_POINT('Ctrl Pts',(-0.218610753000055,15.2,-10.721896628));
#296911=CARTESIAN_POINT('Ctrl Pts',(-0.219317730000055,15.2,-10.724261768));
#296912=CARTESIAN_POINT('Ctrl Pts',(-0.220028527000055,15.2,-10.726632241));
#296913=CARTESIAN_POINT('Ctrl Pts',(-0.220743152000056,15.2,-10.729008033));
#296914=CARTESIAN_POINT('Ctrl Pts',(-0.221461609000055,15.2,-10.731389127));
#296915=CARTESIAN_POINT('Ctrl Pts',(-0.222183905000056,15.2,-10.733775512));
#296916=CARTESIAN_POINT('Ctrl Pts',(-0.222910044000055,15.2,-10.736167171));
#296917=CARTESIAN_POINT('Ctrl Pts',(-0.223640033000055,15.2,-10.738564091));
#296918=CARTESIAN_POINT('Ctrl Pts',(-0.224373875000056,15.2,-10.740966259));
#296919=CARTESIAN_POINT('Ctrl Pts',(-0.225111578000057,15.2,-10.743373659));
#296920=CARTESIAN_POINT('Ctrl Pts',(-0.225853145000056,15.2,-10.745786278));
#296921=CARTESIAN_POINT('Ctrl Pts',(-0.226598585000056,15.2,-10.748204102));
#296922=CARTESIAN_POINT('Ctrl Pts',(-0.227347899000057,15.2,-10.750627116));
#296923=CARTESIAN_POINT('Ctrl Pts',(-0.228101094000056,15.2,-10.753055307));
#296924=CARTESIAN_POINT('Ctrl Pts',(-0.228858176000056,15.2,-10.75548866));
#296925=CARTESIAN_POINT('Ctrl Pts',(-0.229619150000057,15.2,-10.757927163));
#296926=CARTESIAN_POINT('Ctrl Pts',(-0.230384020000055,15.2,-10.760370801));
#296927=CARTESIAN_POINT('Ctrl Pts',(-0.231152793000057,15.2,-10.76281956));
#296928=CARTESIAN_POINT('Ctrl Pts',(-0.231925472000055,15.2,-10.765273428));
#296929=CARTESIAN_POINT('Ctrl Pts',(-0.232702064000057,15.2,-10.767732388));
#296930=CARTESIAN_POINT('Ctrl Pts',(-0.233482574000057,15.2,-10.770196429));
#296931=CARTESIAN_POINT('Ctrl Pts',(-0.234267006000056,15.2,-10.772665536));
#296932=CARTESIAN_POINT('Ctrl Pts',(-0.235055365000055,15.2,-10.775139696));
#296933=CARTESIAN_POINT('Ctrl Pts',(-0.235847657000056,15.2,-10.777618895));
#296934=CARTESIAN_POINT('Ctrl Pts',(-0.236643888000057,15.2,-10.780103119));
#296935=CARTESIAN_POINT('Ctrl Pts',(-0.237444060000056,15.2,-10.782592355));
#296936=CARTESIAN_POINT('Ctrl Pts',(-0.238248181000056,15.2,-10.78508659));
#296937=CARTESIAN_POINT('Ctrl Pts',(-0.239056253000056,15.2,-10.78758581));
#296938=CARTESIAN_POINT('Ctrl Pts',(-0.239868284000057,15.2,-10.790090001));
#296939=CARTESIAN_POINT('Ctrl Pts',(-0.240684278000056,15.2,-10.79259915));
#296940=CARTESIAN_POINT('Ctrl Pts',(-0.241504238000055,15.2,-10.795113244));
#296941=CARTESIAN_POINT('Ctrl Pts',(-0.242328171000056,15.2,-10.797632269));
#296942=CARTESIAN_POINT('Ctrl Pts',(-0.243156080000055,15.2,-10.800156212));
#296943=CARTESIAN_POINT('Ctrl Pts',(-0.243987973000056,15.2,-10.80268506));
#296944=CARTESIAN_POINT('Ctrl Pts',(-0.244823851000057,15.2,-10.805218799));
#296945=CARTESIAN_POINT('Ctrl Pts',(-0.245663721000057,15.2,-10.807757416));
#296946=CARTESIAN_POINT('Ctrl Pts',(-0.246507587000057,15.2,-10.810300898));
#296947=CARTESIAN_POINT('Ctrl Pts',(-0.247355454000056,15.2,-10.812849232));
#296948=CARTESIAN_POINT('Ctrl Pts',(-0.248207327000056,15.2,-10.815402404));
#296949=CARTESIAN_POINT('Ctrl Pts',(-0.249063210000056,15.2,-10.817960403));
#296950=CARTESIAN_POINT('Ctrl Pts',(-0.249923109000055,15.2,-10.820523213));
#296951=CARTESIAN_POINT('Ctrl Pts',(-0.250787027000056,15.2,-10.823090823));
#296952=CARTESIAN_POINT('Ctrl Pts',(-0.251654969000056,15.2,-10.825663219));
#296953=CARTESIAN_POINT('Ctrl Pts',(-0.252526940000056,15.2,-10.828240388));
#296954=CARTESIAN_POINT('Ctrl Pts',(-0.253402945000056,15.2,-10.830822318));
#296955=CARTESIAN_POINT('Ctrl Pts',(-0.254282988000056,15.2,-10.833408995));
#296956=CARTESIAN_POINT('Ctrl Pts',(-0.255167073000055,15.2,-10.836000406));
#296957=CARTESIAN_POINT('Ctrl Pts',(-0.256055206000055,15.2,-10.838596538));
#296958=CARTESIAN_POINT('Ctrl Pts',(-0.256947390000055,15.2,-10.84119738));
#296959=CARTESIAN_POINT('Ctrl Pts',(-0.257843631000056,15.2,-10.843802918));
#296960=CARTESIAN_POINT('Ctrl Pts',(-0.258743931000056,15.2,-10.846413139));
#296961=CARTESIAN_POINT('Ctrl Pts',(-0.259648297000057,15.2,-10.84902803));
#296962=CARTESIAN_POINT('Ctrl Pts',(-0.260556733000056,15.2,-10.851647578));
#296963=CARTESIAN_POINT('Ctrl Pts',(-0.261469242000055,15.2,-10.854271772));
#296964=CARTESIAN_POINT('Ctrl Pts',(-0.262385828000056,15.2,-10.856900598));
#296965=CARTESIAN_POINT('Ctrl Pts',(-0.263306498000055,15.2,-10.859534042));
#296966=CARTESIAN_POINT('Ctrl Pts',(-0.264231255000055,15.2,-10.862172095));
#296967=CARTESIAN_POINT('Ctrl Pts',(-0.265160103000056,15.2,-10.864814742));
#296968=CARTESIAN_POINT('Ctrl Pts',(-0.266093047000057,15.2,-10.86746197));
#296969=CARTESIAN_POINT('Ctrl Pts',(-0.267030089000055,15.2,-10.870113767));
#296970=CARTESIAN_POINT('Ctrl Pts',(-0.267971237000056,15.2,-10.872770121));
#296971=CARTESIAN_POINT('Ctrl Pts',(-0.268916493000055,15.2,-10.87543102));
#296972=CARTESIAN_POINT('Ctrl Pts',(-0.269865860000056,15.2,-10.878096449));
#296973=CARTESIAN_POINT('Ctrl Pts',(-0.270819345000056,15.2,-10.880766398));
#296974=CARTESIAN_POINT('Ctrl Pts',(-0.271776951000057,15.2,-10.883440854));
#296975=CARTESIAN_POINT('Ctrl Pts',(-0.272738681000056,15.2,-10.886119805));
#296976=CARTESIAN_POINT('Ctrl Pts',(-0.273704541000056,15.2,-10.888803238));
#296977=CARTESIAN_POINT('Ctrl Pts',(-0.274674534000056,15.2,-10.891491141));
#296978=CARTESIAN_POINT('Ctrl Pts',(-0.275648666000056,15.2,-10.8941835));
#296979=CARTESIAN_POINT('Ctrl Pts',(-0.276626937000056,15.2,-10.896880306));
#296980=CARTESIAN_POINT('Ctrl Pts',(-0.277609355000056,15.2,-10.899581544));
#296981=CARTESIAN_POINT('Ctrl Pts',(-0.278595921000055,15.2,-10.902287203));
#296982=CARTESIAN_POINT('Ctrl Pts',(-0.279586642000057,15.2,-10.904997271));
#296983=CARTESIAN_POINT('Ctrl Pts',(-0.280581520000055,15.2,-10.907711734));
#296984=CARTESIAN_POINT('Ctrl Pts',(-0.281580560000056,15.2,-10.910430583));
#296985=CARTESIAN_POINT('Ctrl Pts',(-0.282583766000055,15.2,-10.913153802));
#296986=CARTESIAN_POINT('Ctrl Pts',(-0.283591141000056,15.2,-10.915881383));
#296987=CARTESIAN_POINT('Ctrl Pts',(-0.284602690000056,15.2,-10.918613312));
#296988=CARTESIAN_POINT('Ctrl Pts',(-0.285618416000055,15.2,-10.921349576));
#296989=CARTESIAN_POINT('Ctrl Pts',(-0.286638323000057,15.2,-10.924090164));
#296990=CARTESIAN_POINT('Ctrl Pts',(-0.287662415000056,15.2,-10.926835064));
#296991=CARTESIAN_POINT('Ctrl Pts',(-0.288690696000057,15.2,-10.929584264));
#296992=CARTESIAN_POINT('Ctrl Pts',(-0.289723171000055,15.2,-10.932337751));
#296993=CARTESIAN_POINT('Ctrl Pts',(-0.290759842000057,15.2,-10.935095515));
#296994=CARTESIAN_POINT('Ctrl Pts',(-0.291800713000056,15.2,-10.937857543));
#296995=CARTESIAN_POINT('Ctrl Pts',(-0.292845789000056,15.2,-10.940623823));
#296996=CARTESIAN_POINT('Ctrl Pts',(-0.293895073000057,15.2,-10.943394344));
#296997=CARTESIAN_POINT('Ctrl Pts',(-0.294948568000055,15.2,-10.946169093));
#296998=CARTESIAN_POINT('Ctrl Pts',(-0.296006280000055,15.2,-10.948948059));
#296999=CARTESIAN_POINT('Ctrl Pts',(-0.297068210000055,15.2,-10.951731231));
#297000=CARTESIAN_POINT('Ctrl Pts',(-0.298134363000055,15.2,-10.954518595));
#297001=CARTESIAN_POINT('Ctrl Pts',(-0.299204743000056,15.2,-10.957310141));
#297002=CARTESIAN_POINT('Ctrl Pts',(-0.300279354000056,15.2,-10.960105857));
#297003=CARTESIAN_POINT('Ctrl Pts',(-0.301358198000056,15.2,-10.962905731));
#297004=CARTESIAN_POINT('Ctrl Pts',(-0.302441280000056,15.2,-10.965709752));
#297005=CARTESIAN_POINT('Ctrl Pts',(-0.303528603000055,15.2,-10.968517907));
#297006=CARTESIAN_POINT('Ctrl Pts',(-0.304620171000056,15.2,-10.971330186));
#297007=CARTESIAN_POINT('Ctrl Pts',(-0.305715987000056,15.2,-10.974146576));
#297008=CARTESIAN_POINT('Ctrl Pts',(-0.306816056000055,15.2,-10.976967067));
#297009=CARTESIAN_POINT('Ctrl Pts',(-0.307920380000055,15.2,-10.979791646));
#297010=CARTESIAN_POINT('Ctrl Pts',(-0.309028962000056,15.2,-10.982620303));
#297011=CARTESIAN_POINT('Ctrl Pts',(-0.310141808000056,15.2,-10.985453024));
#297012=CARTESIAN_POINT('Ctrl Pts',(-0.311258919000055,15.2,-10.988289801));
#297013=CARTESIAN_POINT('Ctrl Pts',(-0.312380301000056,15.2,-10.991130619));
#297014=CARTESIAN_POINT('Ctrl Pts',(-0.313505954000056,15.2,-10.993975469));
#297015=CARTESIAN_POINT('Ctrl Pts',(-0.314635885000056,15.2,-10.996824339));
#297016=CARTESIAN_POINT('Ctrl Pts',(-0.315770096000056,15.2,-10.999677217));
#297017=CARTESIAN_POINT('Ctrl Pts',(-0.316908589000056,15.2,-11.002534092));
#297018=CARTESIAN_POINT('Ctrl Pts',(-0.318051369000055,15.2,-11.005394953));
#297019=CARTESIAN_POINT('Ctrl Pts',(-0.319198440000056,15.2,-11.008259788));
#297020=CARTESIAN_POINT('Ctrl Pts',(-0.320349803000056,15.2,-11.011128588));
#297021=CARTESIAN_POINT('Ctrl Pts',(-0.321505465000056,15.2,-11.014001338));
#297022=CARTESIAN_POINT('Ctrl Pts',(-0.322665426000055,15.2,-11.01687803));
#297023=CARTESIAN_POINT('Ctrl Pts',(-0.323829689000057,15.2,-11.01975865));
#297024=CARTESIAN_POINT('Ctrl Pts',(-0.324998260000056,15.2,-11.022643189));
#297025=CARTESIAN_POINT('Ctrl Pts',(-0.326171142000057,15.2,-11.025531635));
#297026=CARTESIAN_POINT('Ctrl Pts',(-0.327348336000056,15.2,-11.028423977));
#297027=CARTESIAN_POINT('Ctrl Pts',(-0.328529847000055,15.2,-11.031320204));
#297028=CARTESIAN_POINT('Ctrl Pts',(-0.329715678000057,15.2,-11.034220304));
#297029=CARTESIAN_POINT('Ctrl Pts',(-0.330905831000056,15.2,-11.037124266));
#297030=CARTESIAN_POINT('Ctrl Pts',(-0.332100311000056,15.2,-11.040032081));
#297031=CARTESIAN_POINT('Ctrl Pts',(-0.333299121000056,15.2,-11.042943735));
#297032=CARTESIAN_POINT('Ctrl Pts',(-0.334502263000056,15.2,-11.045859219));
#297033=CARTESIAN_POINT('Ctrl Pts',(-0.335709740000055,15.2,-11.048778521));
#297034=CARTESIAN_POINT('Ctrl Pts',(-0.336921557000055,15.2,-11.051701631));
#297035=CARTESIAN_POINT('Ctrl Pts',(-0.338137716000055,15.2,-11.054628537));
#297036=CARTESIAN_POINT('Ctrl Pts',(-0.339358220000056,15.2,-11.057559229));
#297037=CARTESIAN_POINT('Ctrl Pts',(-0.340583073000056,15.2,-11.060493695));
#297038=CARTESIAN_POINT('Ctrl Pts',(-0.341812276000055,15.2,-11.063431925));
#297039=CARTESIAN_POINT('Ctrl Pts',(-0.343045833000056,15.2,-11.066373907));
#297040=CARTESIAN_POINT('Ctrl Pts',(-0.344283750000055,15.2,-11.069319632));
#297041=CARTESIAN_POINT('Ctrl Pts',(-0.345526025000057,15.2,-11.072269087));
#297042=CARTESIAN_POINT('Ctrl Pts',(-0.346772665000056,15.2,-11.075222262));
#297043=CARTESIAN_POINT('Ctrl Pts',(-0.348023671000056,15.2,-11.078179147));
#297044=CARTESIAN_POINT('Ctrl Pts',(-0.349279047000056,15.2,-11.08113973));
#297045=CARTESIAN_POINT('Ctrl Pts',(-0.350538795000055,15.2,-11.084104002));
#297046=CARTESIAN_POINT('Ctrl Pts',(-0.351802919000056,15.2,-11.08707195));
#297047=CARTESIAN_POINT('Ctrl Pts',(-0.353071422000056,15.2,-11.090043565));
#297048=CARTESIAN_POINT('Ctrl Pts',(-0.354344305000056,15.2,-11.093018835));
#297049=CARTESIAN_POINT('Ctrl Pts',(-0.355621573000056,15.2,-11.09599775));
#297050=CARTESIAN_POINT('Ctrl Pts',(-0.356903229000055,15.2,-11.0989803));
#297051=CARTESIAN_POINT('Ctrl Pts',(-0.358189274000056,15.2,-11.101966474));
#297052=CARTESIAN_POINT('Ctrl Pts',(-0.359479712000056,15.2,-11.104956259));
#297053=CARTESIAN_POINT('Ctrl Pts',(-0.360774547000055,15.2,-11.107949648));
#297054=CARTESIAN_POINT('Ctrl Pts',(-0.362073780000056,15.2,-11.110946628));
#297055=CARTESIAN_POINT('Ctrl Pts',(-0.363377414000056,15.2,-11.11394719));
#297056=CARTESIAN_POINT('Ctrl Pts',(-0.364685453000057,15.2,-11.116951323));
#297057=CARTESIAN_POINT('Ctrl Pts',(-0.365997899000057,15.2,-11.119959015));
#297058=CARTESIAN_POINT('Ctrl Pts',(-0.367314756000056,15.2,-11.122970257));
#297059=CARTESIAN_POINT('Ctrl Pts',(-0.368636025000055,15.2,-11.125985039));
#297060=CARTESIAN_POINT('Ctrl Pts',(-0.369961710000055,15.2,-11.129003349));
#297061=CARTESIAN_POINT('Ctrl Pts',(-0.371291813000055,15.2,-11.132025177));
#297062=CARTESIAN_POINT('Ctrl Pts',(-0.372626336000056,15.2,-11.135050513));
#297063=CARTESIAN_POINT('Ctrl Pts',(-0.373965284000055,15.2,-11.138079346));
#297064=CARTESIAN_POINT('Ctrl Pts',(-0.375308659000056,15.2,-11.141111667));
#297065=CARTESIAN_POINT('Ctrl Pts',(-0.376656462000057,15.2,-11.144147464));
#297066=CARTESIAN_POINT('Ctrl Pts',(-0.378008697000055,15.2,-11.147186726));
#297067=CARTESIAN_POINT('Ctrl Pts',(-0.379365367000055,15.2,-11.150229445));
#297068=CARTESIAN_POINT('Ctrl Pts',(-0.380726475000056,15.2,-11.153275611));
#297069=CARTESIAN_POINT('Ctrl Pts',(-0.382092022000055,15.2,-11.156325211));
#297070=CARTESIAN_POINT('Ctrl Pts',(-0.383462012000055,15.2,-11.159378235));
#297071=CARTESIAN_POINT('Ctrl Pts',(-0.384836446000056,15.2,-11.162434675));
#297072=CARTESIAN_POINT('Ctrl Pts',(-0.386215329000056,15.2,-11.165494519));
#297073=CARTESIAN_POINT('Ctrl Pts',(-0.387598661000055,15.2,-11.168557756));
#297074=CARTESIAN_POINT('Ctrl Pts',(-0.388986447000056,15.2,-11.171624379));
#297075=CARTESIAN_POINT('Ctrl Pts',(-0.390378688000055,15.2,-11.174694374));
#297076=CARTESIAN_POINT('Ctrl Pts',(-0.391775388000056,15.2,-11.177767733));
#297077=CARTESIAN_POINT('Ctrl Pts',(-0.393176547000056,15.2,-11.180844447));
#297078=CARTESIAN_POINT('Ctrl Pts',(-0.394582170000056,15.2,-11.183924502));
#297079=CARTESIAN_POINT('Ctrl Pts',(-0.395992258000056,15.2,-11.187007892));
#297080=CARTESIAN_POINT('Ctrl Pts',(-0.397406814000056,15.2,-11.190094604));
#297081=CARTESIAN_POINT('Ctrl Pts',(-0.398825842000056,15.2,-11.193184629));
#297082=CARTESIAN_POINT('Ctrl Pts',(-0.400249343000055,15.2,-11.196277957));
#297083=CARTESIAN_POINT('Ctrl Pts',(-0.401677318000055,15.2,-11.199374578));
#297084=CARTESIAN_POINT('Ctrl Pts',(-0.403109771000055,15.2,-11.202474481));
#297085=CARTESIAN_POINT('Ctrl Pts',(-0.404546705000056,15.2,-11.205577658));
#297086=CARTESIAN_POINT('Ctrl Pts',(-0.405988122000055,15.2,-11.208684097));
#297087=CARTESIAN_POINT('Ctrl Pts',(-0.407434025000055,15.2,-11.211793789));
#297088=CARTESIAN_POINT('Ctrl Pts',(-0.408884415000056,15.2,-11.214906723));
#297089=CARTESIAN_POINT('Ctrl Pts',(-0.410339295000056,15.2,-11.21802289));
#297090=CARTESIAN_POINT('Ctrl Pts',(-0.411798667000056,15.2,-11.221142281));
#297091=CARTESIAN_POINT('Ctrl Pts',(-0.413262534000056,15.2,-11.224264883));
#297092=CARTESIAN_POINT('Ctrl Pts',(-0.414730899000055,15.2,-11.22739069));
#297093=CARTESIAN_POINT('Ctrl Pts',(-0.416203762000055,15.2,-11.230519688));
#297094=CARTESIAN_POINT('Ctrl Pts',(-0.417681127000057,15.2,-11.233651872));
#297095=CARTESIAN_POINT('Ctrl Pts',(-0.419162997000055,15.2,-11.236787227));
#297096=CARTESIAN_POINT('Ctrl Pts',(-0.420649373000056,15.2,-11.239925747));
#297097=CARTESIAN_POINT('Ctrl Pts',(-0.422140258000056,15.2,-11.243067421));
#297098=CARTESIAN_POINT('Ctrl Pts',(-0.423635654000056,15.2,-11.246212238));
#297099=CARTESIAN_POINT('Ctrl Pts',(-0.425135562000056,15.2,-11.249360189));
#297100=CARTESIAN_POINT('Ctrl Pts',(-0.426639987000056,15.2,-11.252511265));
#297101=CARTESIAN_POINT('Ctrl Pts',(-0.428148929000055,15.2,-11.255665455));
#297102=CARTESIAN_POINT('Ctrl Pts',(-0.429662391000055,15.2,-11.258822751));
#297103=CARTESIAN_POINT('Ctrl Pts',(-0.431180374000055,15.2,-11.261983141));
#297104=CARTESIAN_POINT('Ctrl Pts',(-0.432702884000056,15.2,-11.265146617));
#297105=CARTESIAN_POINT('Ctrl Pts',(-0.434229918000056,15.2,-11.268313169));
#297106=CARTESIAN_POINT('Ctrl Pts',(-0.435761482000055,15.2,-11.271482787));
#297107=CARTESIAN_POINT('Ctrl Pts',(-0.437297576000055,15.2,-11.274655461));
#297108=CARTESIAN_POINT('Ctrl Pts',(-0.438838204000056,15.2,-11.277831182));
#297109=CARTESIAN_POINT('Ctrl Pts',(-0.440383367000056,15.2,-11.281009939));
#297110=CARTESIAN_POINT('Ctrl Pts',(-0.441933068000055,15.2,-11.284191725));
#297111=CARTESIAN_POINT('Ctrl Pts',(-0.443487307000057,15.2,-11.287376529));
#297112=CARTESIAN_POINT('Ctrl Pts',(-0.445046088000056,15.2,-11.290564341));
#297113=CARTESIAN_POINT('Ctrl Pts',(-0.446609414000055,15.2,-11.293755152));
#297114=CARTESIAN_POINT('Ctrl Pts',(-0.448177284000056,15.2,-11.296948952));
#297115=CARTESIAN_POINT('Ctrl Pts',(-0.449749702000056,15.2,-11.300145731));
#297116=CARTESIAN_POINT('Ctrl Pts',(-0.451326671000055,15.2,-11.303345481));
#297117=CARTESIAN_POINT('Ctrl Pts',(-0.452908191000055,15.2,-11.306548191));
#297118=CARTESIAN_POINT('Ctrl Pts',(-0.454494265000056,15.2,-11.309753853));
#297119=CARTESIAN_POINT('Ctrl Pts',(-0.456084896000055,15.2,-11.312962457));
#297120=CARTESIAN_POINT('Ctrl Pts',(-0.457680085000056,15.2,-11.316173992));
#297121=CARTESIAN_POINT('Ctrl Pts',(-0.459279833000057,15.2,-11.319388451));
#297122=CARTESIAN_POINT('Ctrl Pts',(-0.460884143000057,15.2,-11.322605822));
#297123=CARTESIAN_POINT('Ctrl Pts',(-0.462493018000056,15.2,-11.325826098));
#297124=CARTESIAN_POINT('Ctrl Pts',(-0.464106457000056,15.2,-11.329049269));
#297125=CARTESIAN_POINT('Ctrl Pts',(-0.465724466000056,15.2,-11.332275325));
#297126=CARTESIAN_POINT('Ctrl Pts',(-0.467347044000055,15.2,-11.335504256));
#297127=CARTESIAN_POINT('Ctrl Pts',(-0.468974194000056,15.2,-11.338736054));
#297128=CARTESIAN_POINT('Ctrl Pts',(-0.470605918000055,15.2,-11.341970709));
#297129=CARTESIAN_POINT('Ctrl Pts',(-0.472242218000056,15.2,-11.345208212));
#297130=CARTESIAN_POINT('Ctrl Pts',(-0.473883095000056,15.2,-11.348448553));
#297131=CARTESIAN_POINT('Ctrl Pts',(-0.475528552000055,15.2,-11.351691723));
#297132=CARTESIAN_POINT('Ctrl Pts',(-0.477178589000056,15.2,-11.354937714));
#297133=CARTESIAN_POINT('Ctrl Pts',(-0.478833210000056,15.2,-11.358186515));
#297134=CARTESIAN_POINT('Ctrl Pts',(-0.480492416000056,15.2,-11.361438118));
#297135=CARTESIAN_POINT('Ctrl Pts',(-0.482156209000056,15.2,-11.364692512));
#297136=CARTESIAN_POINT('Ctrl Pts',(-0.483824592000056,15.2,-11.367949691));
#297137=CARTESIAN_POINT('Ctrl Pts',(-0.485497564000056,15.2,-11.371209642));
#297138=CARTESIAN_POINT('Ctrl Pts',(-0.487175129000056,15.2,-11.374472358));
#297139=CARTESIAN_POINT('Ctrl Pts',(-0.488857288000055,15.2,-11.377737829));
#297140=CARTESIAN_POINT('Ctrl Pts',(-0.490544043000056,15.2,-11.381006047));
#297141=CARTESIAN_POINT('Ctrl Pts',(-0.492235397000057,15.2,-11.384277003));
#297142=CARTESIAN_POINT('Ctrl Pts',(-0.493931349000055,15.2,-11.387550685));
#297143=CARTESIAN_POINT('Ctrl Pts',(-0.495631904000057,15.2,-11.390827086));
#297144=CARTESIAN_POINT('Ctrl Pts',(-0.497337060000056,15.2,-11.394106196));
#297145=CARTESIAN_POINT('Ctrl Pts',(-0.499046823000056,15.2,-11.397388008));
#297146=CARTESIAN_POINT('Ctrl Pts',(-0.500761192000055,15.2,-11.400672511));
#297147=CARTESIAN_POINT('Ctrl Pts',(-0.502480169000057,15.2,-11.403959697));
#297148=CARTESIAN_POINT('Ctrl Pts',(-0.504203756000056,15.2,-11.407249556));
#297149=CARTESIAN_POINT('Ctrl Pts',(-0.505931954000056,15.2,-11.410542081));
#297150=CARTESIAN_POINT('Ctrl Pts',(-0.507664766000057,15.2,-11.413837262));
#297151=CARTESIAN_POINT('Ctrl Pts',(-0.509402194000056,15.2,-11.417135088));
#297152=CARTESIAN_POINT('Ctrl Pts',(-0.511144239000056,15.2,-11.420435551));
#297153=CARTESIAN_POINT('Ctrl Pts',(-0.512890901000055,15.2,-11.423738642));
#297154=CARTESIAN_POINT('Ctrl Pts',(-0.514642185000056,15.2,-11.427044351));
#297155=CARTESIAN_POINT('Ctrl Pts',(-0.516398090000055,15.2,-11.43035267));
#297156=CARTESIAN_POINT('Ctrl Pts',(-0.518158619000056,15.2,-11.433663589));
#297157=CARTESIAN_POINT('Ctrl Pts',(-0.519923771000055,15.2,-11.436977103));
#297158=CARTESIAN_POINT('Ctrl Pts',(-0.521693552000055,15.2,-11.4402932));
#297159=CARTESIAN_POINT('Ctrl Pts',(-0.523467959000056,15.2,-11.443611875));
#297160=CARTESIAN_POINT('Ctrl Pts',(-0.525246997000056,15.2,-11.446933118));
#297161=CARTESIAN_POINT('Ctrl Pts',(-0.527030665000057,15.2,-11.450256921));
#297162=CARTESIAN_POINT('Ctrl Pts',(-0.528818965000056,15.2,-11.453583273));
#297163=CARTESIAN_POINT('Ctrl Pts',(-0.530611902000055,15.2,-11.456912162));
#297164=CARTESIAN_POINT('Ctrl Pts',(-0.532409474000056,15.2,-11.460243578));
#297165=CARTESIAN_POINT('Ctrl Pts',(-0.534211686000056,15.2,-11.46357751));
#297166=CARTESIAN_POINT('Ctrl Pts',(-0.536018537000055,15.2,-11.466913949));
#297167=CARTESIAN_POINT('Ctrl Pts',(-0.537830030000055,15.2,-11.470252887));
#297168=CARTESIAN_POINT('Ctrl Pts',(-0.539646167000055,15.2,-11.473594318));
#297169=CARTESIAN_POINT('Ctrl Pts',(-0.541466946000057,15.2,-11.476938237));
#297170=CARTESIAN_POINT('Ctrl Pts',(-0.543292369000056,15.2,-11.480284643));
#297171=CARTESIAN_POINT('Ctrl Pts',(-0.544756421000056,15.2,-11.482963757));
#297172=CARTESIAN_POINT('Ctrl Pts',(-0.545856551000057,15.2,-11.484974209));
#297173=CARTESIAN_POINT('Ctrl Pts',(-0.546590899000057,15.2,-11.486315008));
#297174=CARTESIAN_POINT('Ctrl Pts',(-0.546958306000055,15.2,-11.486985532));
#297175=CARTESIAN_POINT('',(-0.929795809014353,15.2,-11.4623505335096));
#297176=CARTESIAN_POINT('Origin',(-5.66257110645729E-14,15.2,-1.77635683940025E-14));
#297177=CARTESIAN_POINT('Ctrl Pts',(-1.18690176600006,15.2,-10.306885524));
#297178=CARTESIAN_POINT('Ctrl Pts',(-1.18695287825247,15.2,-10.3086714504511));
#297179=CARTESIAN_POINT('Ctrl Pts',(-1.18700024431844,15.2,-10.3105146700777));
#297180=CARTESIAN_POINT('Ctrl Pts',(-1.18704320796202,15.2,-10.3124142312835));
#297181=CARTESIAN_POINT('Ctrl Pts',(-1.18708637879801,15.2,-10.3143229531337));
#297182=CARTESIAN_POINT('Ctrl Pts',(-1.18712509994175,15.2,-10.3162885639395));
#297183=CARTESIAN_POINT('Ctrl Pts',(-1.1871587090283,15.2,-10.3183101249039));
#297184=CARTESIAN_POINT('Ctrl Pts',(-1.1871923181118,15.2,-10.3203316856847));
#297185=CARTESIAN_POINT('Ctrl Pts',(-1.18722081733423,15.2,-10.322409198819));
#297186=CARTESIAN_POINT('Ctrl Pts',(-1.18724356650007,15.2,-10.3245417524916));
#297187=CARTESIAN_POINT('Ctrl Pts',(-1.18726631566591,15.2,-10.3266743061641));
#297188=CARTESIAN_POINT('Ctrl Pts',(-1.18728331741518,15.1999999999999,
-10.3288618993474));
#297189=CARTESIAN_POINT('Ctrl Pts',(-1.18729394974902,15.2,-10.3311036472915));
#297190=CARTESIAN_POINT('Ctrl Pts',(-1.18730458208384,15.2,-10.3333453954392));
#297191=CARTESIAN_POINT('Ctrl Pts',(-1.18730884758373,15.2,-10.335641298191));
#297192=CARTESIAN_POINT('Ctrl Pts',(-1.18730614774977,15.2,-10.3379904903227));
#297193=CARTESIAN_POINT('Ctrl Pts',(-1.18730344791606,15.2,-10.3403396822409));
#297194=CARTESIAN_POINT('Ctrl Pts',(-1.18729378039953,15.2,-10.3427421643207));
#297195=CARTESIAN_POINT('Ctrl Pts',(-1.18727656873339,15.2,-10.3451970944927));
#297196=CARTESIAN_POINT('Ctrl Pts',(-1.18725935706726,15.2,-10.3476520246647));
#297197=CARTESIAN_POINT('Ctrl Pts',(-1.18723459815028,15.2,-10.3501594023475));
#297198=CARTESIAN_POINT('Ctrl Pts',(-1.18720173348516,15.2,-10.3527184083357));
#297199=CARTESIAN_POINT('Ctrl Pts',(-1.18716886881705,15.2,-10.3552774145562));
#297200=CARTESIAN_POINT('Ctrl Pts',(-1.18712789608962,15.2,-10.3578880464332));
#297201=CARTESIAN_POINT('Ctrl Pts',(-1.18707827150299,15.2,-10.3605495048317));
#297202=CARTESIAN_POINT('Ctrl Pts',(-1.18702864692087,15.2,-10.3632109629885));
#297203=CARTESIAN_POINT('Ctrl Pts',(-1.18697036877764,15.2,-10.3659232462155));
#297204=CARTESIAN_POINT('Ctrl Pts',(-1.18690291127969,15.2,-10.3686855726173));
#297205=CARTESIAN_POINT('Ctrl Pts',(-1.18683545378174,15.2,-10.3714478990192));
#297206=CARTESIAN_POINT('Ctrl Pts',(-1.18675881418451,15.2,-10.3742602688836));
#297207=CARTESIAN_POINT('Ctrl Pts',(-1.18667248268807,15.2,-10.3771219181108));
#297208=CARTESIAN_POINT('Ctrl Pts',(-1.18658615119163,15.2,-10.379983567338));
#297209=CARTESIAN_POINT('Ctrl Pts',(-1.18649012644043,15.2,-10.3828944944465));
#297210=CARTESIAN_POINT('Ctrl Pts',(-1.18638390927832,15.2,-10.385853953919));
#297211=CARTESIAN_POINT('Ctrl Pts',(-1.18627769210655,15.2,-10.3888134136604));
#297212=CARTESIAN_POINT('Ctrl Pts',(-1.18616128558383,15.2,-10.3918214053147));
#297213=CARTESIAN_POINT('Ctrl Pts',(-1.1860342042431,15.2,-10.39487719815));
#297214=CARTESIAN_POINT('Ctrl Pts',(-1.18590712291392,15.2,-10.3979329907077));
#297215=CARTESIAN_POINT('Ctrl Pts',(-1.18576936691205,15.2,-10.4010365852655));
#297216=CARTESIAN_POINT('Ctrl Pts',(-1.18562046775014,15.2,-10.4041872659985));
#297217=CARTESIAN_POINT('Ctrl Pts',(-1.18547156858824,15.2,-10.4073379467315));
#297218=CARTESIAN_POINT('Ctrl Pts',(-1.18531152576172,15.2,-10.410535714918));
#297219=CARTESIAN_POINT('Ctrl Pts',(-1.18513988276875,15.2,-10.4137798696303));
#297220=CARTESIAN_POINT('Ctrl Pts',(-1.18496823976018,15.2,-10.4170240246374));
#297221=CARTESIAN_POINT('Ctrl Pts',(-1.18478499820055,15.2,-10.4203145675565));
#297222=CARTESIAN_POINT('Ctrl Pts',(-1.18458971402272,15.2,-10.423650812657));
#297223=CARTESIAN_POINT('Ctrl Pts',(-1.18439442986262,15.2,-10.4269870574544));
#297224=CARTESIAN_POINT('Ctrl Pts',(-1.18418710221816,15.2,-10.4303690046824));
#297225=CARTESIAN_POINT('Ctrl Pts',(-1.18396730047518,15.2,-10.43379598349));
#297226=CARTESIAN_POINT('Ctrl Pts',(-1.18374749873219,15.2,-10.4372229622977));
#297227=CARTESIAN_POINT('Ctrl Pts',(-1.18351522376701,15.2,-10.4406949718391));
#297228=CARTESIAN_POINT('Ctrl Pts',(-1.1832700567768,15.2,-10.444211356625));
#297229=CARTESIAN_POINT('Ctrl Pts',(-1.18302488976432,15.2,-10.4477277417303));
#297230=CARTESIAN_POINT('Ctrl Pts',(-1.18276682798624,15.2,-10.4512885011113));
#297231=CARTESIAN_POINT('Ctrl Pts',(-1.18249546795713,15.2,-10.4548929895737));
#297232=CARTESIAN_POINT('Ctrl Pts',(-1.18222410795266,15.2,-10.4584974777087));
#297233=CARTESIAN_POINT('Ctrl Pts',(-1.18193944638091,15.2,-10.4621456945924));
#297234=CARTESIAN_POINT('Ctrl Pts',(-1.18164108847508,15.2,-10.4658370095416));
#297235=CARTESIAN_POINT('Ctrl Pts',(-1.18124327792495,15.2,-10.4707587629189));
#297236=CARTESIAN_POINT('Ctrl Pts',(-1.1808211147739,15.2,-10.4757571319861));
#297237=CARTESIAN_POINT('Ctrl Pts',(-1.18037369100023,15.2,-10.4808306522732));
#297238=CARTESIAN_POINT('Ctrl Pts',(-1.1800381231776,15.2,-10.4846357924021));
#297239=CARTESIAN_POINT('Ctrl Pts',(-1.17968834555056,15.2,-10.4884832053535));
#297240=CARTESIAN_POINT('Ctrl Pts',(-1.17932398598146,15.2,-10.492372285376));
#297241=CARTESIAN_POINT('Ctrl Pts',(-1.17895962637926,15.2,-10.4962613657518));
#297242=CARTESIAN_POINT('Ctrl Pts',(-1.17858068606229,15.2,-10.5001921147587));
#297243=CARTESIAN_POINT('Ctrl Pts',(-1.17818680043694,15.2,-10.5041639364259));
#297244=CARTESIAN_POINT('Ctrl Pts',(-1.17785856243371,15.2,-10.5074737876349));
#297245=CARTESIAN_POINT('Ctrl Pts',(-1.1775199460886,15.2,-10.5108121629491));
#297246=CARTESIAN_POINT('Ctrl Pts',(-1.17717074796274,15.2,-10.5141787224653));
#297247=CARTESIAN_POINT('Ctrl Pts',(-1.17682154983687,15.2,-10.5175452819815));
#297248=CARTESIAN_POINT('Ctrl Pts',(-1.17646176907471,15.2,-10.520940028212));
#297249=CARTESIAN_POINT('Ctrl Pts',(-1.17609120372661,15.2,-10.5243626244643));
#297250=CARTESIAN_POINT('Ctrl Pts',(-1.1757206384189,15.2,-10.5277852203435));
#297251=CARTESIAN_POINT('Ctrl Pts',(-1.17533929147996,15.2,-10.5312356701097));
#297252=CARTESIAN_POINT('Ctrl Pts',(-1.1749469643014,15.2,-10.5347136418117));
#297253=CARTESIAN_POINT('Ctrl Pts',(-1.17455463708007,15.2,-10.5381916138928));
#297254=CARTESIAN_POINT('Ctrl Pts',(-1.1741513308756,15.2,-10.541697109029));
#297255=CARTESIAN_POINT('Ctrl Pts',(-1.17373685302929,15.2,-10.5452298043045));
#297256=CARTESIAN_POINT('Ctrl Pts',(-1.17332237518299,15.2,-10.5487624995801));
#297257=CARTESIAN_POINT('Ctrl Pts',(-1.17289672702737,15.2,-10.5523223925563));
#297258=CARTESIAN_POINT('Ctrl Pts',(-1.17245971832577,15.2,-10.5559091671087));
#297259=CARTESIAN_POINT('Ctrl Pts',(-1.17202270962417,15.2,-10.559495941661));
#297260=CARTESIAN_POINT('Ctrl Pts',(-1.17157434308505,15.2,-10.563109595319));
#297261=CARTESIAN_POINT('Ctrl Pts',(-1.17111443273843,15.2,-10.5667498133037));
#297262=CARTESIAN_POINT('Ctrl Pts',(-1.17056254029241,15.2,-10.5711180751234));
#297263=CARTESIAN_POINT('Ctrl Pts',(-1.16999402641933,15.2,-10.5755245905979));
#297264=CARTESIAN_POINT('Ctrl Pts',(-1.1694085782196,15.2,-10.579968822426));
#297265=CARTESIAN_POINT('Ctrl Pts',(-1.16892070479959,15.2,-10.583672348344));
#297266=CARTESIAN_POINT('Ctrl Pts',(-1.16842107412137,15.2,-10.5874020667535));
#297267=CARTESIAN_POINT('Ctrl Pts',(-1.167909508067,15.2,-10.5911576717587));
#297268=CARTESIAN_POINT('Ctrl Pts',(-1.16739794195686,15.2,-10.5949132771732));
#297269=CARTESIAN_POINT('Ctrl Pts',(-1.16687444269685,15.2,-10.5986947696602));
#297270=CARTESIAN_POINT('Ctrl Pts',(-1.16633883658673,15.2,-10.6025018445192));
#297271=CARTESIAN_POINT('Ctrl Pts',(-1.16569610921955,15.2,-10.6070703345991));
#297272=CARTESIAN_POINT('Ctrl Pts',(-1.16503595023964,15.2,-10.6116756682454));
#297273=CARTESIAN_POINT('Ctrl Pts',(-1.16435806500113,15.2,-10.6163173283991));
#297274=CARTESIAN_POINT('Ctrl Pts',(-1.1637931606665,15.2,-10.6201853783163));
#297275=CARTESIAN_POINT('Ctrl Pts',(-1.16321594966842,15.2,-10.6240786547382));
#297276=CARTESIAN_POINT('Ctrl Pts',(-1.16262626688962,15.2,-10.6279968652958));
#297277=CARTESIAN_POINT('Ctrl Pts',(-1.16203658411082,15.2,-10.6319150758534));
#297278=CARTESIAN_POINT('Ctrl Pts',(-1.16143442917626,15.2,-10.6358582204114));
#297279=CARTESIAN_POINT('Ctrl Pts',(-1.160819640703,15.2,-10.6398260084689));
#297280=CARTESIAN_POINT('Ctrl Pts',(-1.16020485222975,15.2,-10.6437937965265));
#297281=CARTESIAN_POINT('Ctrl Pts',(-1.15957743160628,15.2,-10.6477862292234));
#297282=CARTESIAN_POINT('Ctrl Pts',(-1.15893722042468,15.2,-10.651803019017));
#297283=CARTESIAN_POINT('Ctrl Pts',(-1.15816896703467,15.2,-10.6566231665943));
#297284=CARTESIAN_POINT('Ctrl Pts',(-1.15738229466934,15.2,-10.6614783887011));
#297285=CARTESIAN_POINT('Ctrl Pts',(-1.15657693744778,15.2,-10.6663681982749));
#297286=CARTESIAN_POINT('Ctrl Pts',(-1.15590580640544,15.2,-10.6704430397345));
#297287=CARTESIAN_POINT('Ctrl Pts',(-1.15522170016621,15.2,-10.6745418988963));
#297288=CARTESIAN_POINT('Ctrl Pts',(-1.15452446822108,15.2,-10.6786644979947));
#297289=CARTESIAN_POINT('Ctrl Pts',(-1.15396668271057,15.2,-10.6819625770039));
#297290=CARTESIAN_POINT('Ctrl Pts',(-1.15340049515609,15.2,-10.6852758510325));
#297291=CARTESIAN_POINT('Ctrl Pts',(-1.15282583234176,15.2,-10.6886041767588));
#297292=CARTESIAN_POINT('Ctrl Pts',(-1.15225116944913,15.2,-10.6919325029384));
#297293=CARTESIAN_POINT('Ctrl Pts',(-1.15166802957889,15.2,-10.6952758802129));
#297294=CARTESIAN_POINT('Ctrl Pts',(-1.15107633943497,15.2,-10.698634171508));
#297295=CARTESIAN_POINT('Ctrl Pts',(-1.15033672679538,15.2,-10.7028320353981));
#297296=CARTESIAN_POINT('Ctrl Pts',(-1.1495837529728,15.2,-10.7070531990154));
#297297=CARTESIAN_POINT('Ctrl Pts',(-1.14881727470821,15.2,-10.7112973930443));
#297298=CARTESIAN_POINT('Ctrl Pts',(-1.14805079644363,15.2,-10.7155415870733));
#297299=CARTESIAN_POINT('Ctrl Pts',(-1.14727081541518,15.2,-10.7198088116099));
#297300=CARTESIAN_POINT('Ctrl Pts',(-1.14647719016625,15.2,-10.7240987992564));
#297301=CARTESIAN_POINT('Ctrl Pts',(-1.14584229001901,15.2,-10.7275307890929));
#297302=CARTESIAN_POINT('Ctrl Pts',(-1.1451986568661,15.2,-10.7309773469649));
#297303=CARTESIAN_POINT('Ctrl Pts',(-1.14454622158668,15.2,-10.7344383379588));
#297304=CARTESIAN_POINT('Ctrl Pts',(-1.14389378621836,15.2,-10.7378993294243));
#297305=CARTESIAN_POINT('Ctrl Pts',(-1.14323254940177,15.2,-10.7413747540387));
#297306=CARTESIAN_POINT('Ctrl Pts',(-1.14256243942023,15.2,-10.7448644767854));
#297307=CARTESIAN_POINT('Ctrl Pts',(-1.14189232952998,15.2,-10.7483541990566));
#297308=CARTESIAN_POINT('Ctrl Pts',(-1.14121334901333,15.2,-10.7518582199831));
#297309=CARTESIAN_POINT('Ctrl Pts',(-1.14052542709153,15.2,-10.7553764064812));
#297310=CARTESIAN_POINT('Ctrl Pts',(-1.139837505076,15.2,-10.7588945934586));
#297311=CARTESIAN_POINT('Ctrl Pts',(-1.13914064425914,15.2,-10.7624269452319));
#297312=CARTESIAN_POINT('Ctrl Pts',(-1.1384347754423,15.2,-10.765973330815));
#297313=CARTESIAN_POINT('Ctrl Pts',(-1.13772890672164,15.2,-10.7695197159149));
#297314=CARTESIAN_POINT('Ctrl Pts',(-1.13701403064168,15.2,-10.773080135087));
#297315=CARTESIAN_POINT('Ctrl Pts',(-1.13629008136845,15.2,-10.7766544566822));
#297316=CARTESIAN_POINT('Ctrl Pts',(-1.13538514470294,15.2,-10.7811223590416));
#297317=CARTESIAN_POINT('Ctrl Pts',(-1.13446602963737,15.2,-10.7856119837191));
#297318=CARTESIAN_POINT('Ctrl Pts',(-1.13353261209173,15.2,-10.790123078943));
#297319=CARTESIAN_POINT('Ctrl Pts',(-1.13278587801452,15.2,-10.7937319553188));
#297320=CARTESIAN_POINT('Ctrl Pts',(-1.13202998984642,15.2,-10.7973545722789));
#297321=CARTESIAN_POINT('Ctrl Pts',(-1.13126488247079,15.2,-10.8009908017557));
#297322=CARTESIAN_POINT('Ctrl Pts',(-1.1304997751994,15.2,-10.8046270307371));
#297323=CARTESIAN_POINT('Ctrl Pts',(-1.12972545059653,15.2,-10.8082768706824));
#297324=CARTESIAN_POINT('Ctrl Pts',(-1.12894184466154,15.2,-10.8119401976594));
#297325=CARTESIAN_POINT('Ctrl Pts',(-1.12815823861978,15.2,-10.8156035251354));
#297326=CARTESIAN_POINT('Ctrl Pts',(-1.12736534972472,15.2,-10.819280336279));
#297327=CARTESIAN_POINT('Ctrl Pts',(-1.12656312023288,15.2,-10.8229705077191));
#297328=CARTESIAN_POINT('Ctrl Pts',(-1.12576089085034,15.2,-10.8266606786565));
#297329=CARTESIAN_POINT('Ctrl Pts',(-1.1249493176718,15.2,-10.8303642080502));
#297330=CARTESIAN_POINT('Ctrl Pts',(-1.12412834118432,15.2,-10.8340809711339));
#297331=CARTESIAN_POINT('Ctrl Pts',(-1.12330736458498,15.2,-10.8377977347241));
#297332=CARTESIAN_POINT('Ctrl Pts',(-1.12247698474864,15.2,-10.8415277334043));
#297333=CARTESIAN_POINT('Ctrl Pts',(-1.12163714075843,15.2,-10.845270839775));
#297334=CARTESIAN_POINT('Ctrl Pts',(-1.12079729676822,15.2,-10.8490139461456));
#297335=CARTESIAN_POINT('Ctrl Pts',(-1.11994799076579,15.2,-10.8527701631317));
#297336=CARTESIAN_POINT('Ctrl Pts',(-1.11908916088467,15.2,-10.8565393661162));
#297337=CARTESIAN_POINT('Ctrl Pts',(-1.11823033112057,15.2,-10.8603085685872));
#297338=CARTESIAN_POINT('Ctrl Pts',(-1.1173619804551,15.2,-10.8640907580737));
#297339=CARTESIAN_POINT('Ctrl Pts',(-1.11648404796736,15.2,-10.8678858117807));
#297340=CARTESIAN_POINT('Ctrl Pts',(-1.11560611536,15.2,-10.8716808660047));
#297341=CARTESIAN_POINT('Ctrl Pts',(-1.1147186030644,15.2,-10.8754887839373));
#297342=CARTESIAN_POINT('Ctrl Pts',(-1.11382145257007,15.2,-10.8793094449246));
#297343=CARTESIAN_POINT('Ctrl Pts',(-1.11292430219798,15.2,-10.8831301053914));
#297344=CARTESIAN_POINT('Ctrl Pts',(-1.11201751551881,15.2,-10.8869635091092));
#297345=CARTESIAN_POINT('Ctrl Pts',(-1.11110103431659,15.2,-10.8908095349607));
#297346=CARTESIAN_POINT('Ctrl Pts',(-1.1101845529895,15.2,-10.8946555613361));
#297347=CARTESIAN_POINT('Ctrl Pts',(-1.10925837840729,15.2,-10.8985142115119));
#297348=CARTESIAN_POINT('Ctrl Pts',(-1.10832245386423,15.2,-10.9023853640284));
#297349=CARTESIAN_POINT('Ctrl Pts',(-1.1073865294487,15.2,-10.9062565160176));
#297350=CARTESIAN_POINT('Ctrl Pts',(-1.10644085710492,15.2,-10.9101401728953));
#297351=CARTESIAN_POINT('Ctrl Pts',(-1.10548538062811,15.2,-10.9140362134649));
#297352=CARTESIAN_POINT('Ctrl Pts',(-1.10452990402112,15.2,-10.9179322545654));
#297353=CARTESIAN_POINT('Ctrl Pts',(-1.10356462468796,15.2,-10.9218406810645));
#297354=CARTESIAN_POINT('Ctrl Pts',(-1.10258948691195,15.2,-10.9257613741123));
#297355=CARTESIAN_POINT('Ctrl Pts',(-1.10161434926881,15.2,-10.9296820666259));
#297356=CARTESIAN_POINT('Ctrl Pts',(-1.10062935524985,15.2,-10.9336150266954));
#297357=CARTESIAN_POINT('Ctrl Pts',(-1.09963445138776,15.2,-10.9375601383716));
#297358=CARTESIAN_POINT('Ctrl Pts',(-1.0986395473901,15.2,-10.9415052505854));
#297359=CARTESIAN_POINT('Ctrl Pts',(-1.09763473318157,15.2,-10.9454625118544));
#297360=CARTESIAN_POINT('Ctrl Pts',(-1.09661995723274,15.2,-10.9494318094777));
#297361=CARTESIAN_POINT('Ctrl Pts',(-1.09560518142216,15.2,-10.9534011065601));
#297362=CARTESIAN_POINT('Ctrl Pts',(-1.0945804442281,15.2,-10.9573824381109));
#297363=CARTESIAN_POINT('Ctrl Pts',(-1.09354569320261,15.2,-10.9613756898387));
#297364=CARTESIAN_POINT('Ctrl Pts',(-1.09251094203613,15.2,-10.9653689421107));
#297365=CARTESIAN_POINT('Ctrl Pts',(-1.09146617741037,15.2,-10.9693741141449));
#297366=CARTESIAN_POINT('Ctrl Pts',(-1.09041135074177,15.2,-10.973391091975));
#297367=CARTESIAN_POINT('Ctrl Pts',(-1.08935652407317,15.2,-10.977408069805));
#297368=CARTESIAN_POINT('Ctrl Pts',(-1.08829163310617,15.2,-10.9814368537948));
#297369=CARTESIAN_POINT('Ctrl Pts',(-1.08721662982433,15.2,-10.9854773301273));
#297370=CARTESIAN_POINT('Ctrl Pts',(-1.08614162668895,15.2,-10.9895178059093));
#297371=CARTESIAN_POINT('Ctrl Pts',(-1.08505651033569,15.2,-10.9935699738332));
#297372=CARTESIAN_POINT('Ctrl Pts',(-1.08396123247584,15.2,-10.9976337229639));
#297373=CARTESIAN_POINT('Ctrl Pts',(-1.08286595446676,15.2,-11.0016974726482));
#297374=CARTESIAN_POINT('Ctrl Pts',(-1.08176051414342,15.2,-11.0057728019692));
#297375=CARTESIAN_POINT('Ctrl Pts',(-1.08064486435935,15.2,-11.0098595996932));
#297376=CARTESIAN_POINT('Ctrl Pts',(-1.07952921472728,15.2,-11.0139463968603));
#297377=CARTESIAN_POINT('Ctrl Pts',(-1.07840335555766,15.2,-11.0180446622591));
#297378=CARTESIAN_POINT('Ctrl Pts',(-1.07726723915121,15.2,-11.0221542854225));
#297379=CARTESIAN_POINT('Ctrl Pts',(-1.07613112258996,15.2,-11.0262639091457));
#297380=CARTESIAN_POINT('Ctrl Pts',(-1.07498474934558,15.2,-11.0303848909948));
#297381=CARTESIAN_POINT('Ctrl Pts',(-1.0738280720572,15.2,-11.0345171196496));
#297382=CARTESIAN_POINT('Ctrl Pts',(-1.07238222552552,15.2,-11.0396824051867));
#297383=CARTESIAN_POINT('Ctrl Pts',(-1.07092027880252,15.2,-11.0448652644399));
#297384=CARTESIAN_POINT('Ctrl Pts',(-1.06944214477342,15.2,-11.0500654854135));
#297385=CARTESIAN_POINT('Ctrl Pts',(-1.06796401074431,15.2,-11.0552657063871));
#297386=CARTESIAN_POINT('Ctrl Pts',(-1.06646968679268,15.2,-11.0604832869279));
#297387=CARTESIAN_POINT('Ctrl Pts',(-1.06495908706919,15.2,-11.0657180179013));
#297388=CARTESIAN_POINT('Ctrl Pts',(-1.06375060738919,15.2,-11.0699058023376));
#297389=CARTESIAN_POINT('Ctrl Pts',(-1.06253171105598,15.2,-11.0741045619194));
#297390=CARTESIAN_POINT('Ctrl Pts',(-1.06130235348427,15.2,-11.0783141892054));
#297391=CARTESIAN_POINT('Ctrl Pts',(-1.06007299574505,15.2,-11.0825238170651));
#297392=CARTESIAN_POINT('Ctrl Pts',(-1.05883317762321,15.2,-11.0867443131629));
#297393=CARTESIAN_POINT('Ctrl Pts',(-1.057582855054,15.2,-11.0909755714501));
#297394=CARTESIAN_POINT('Ctrl Pts',(-1.05633253265514,15.2,-11.0952068291609));
#297395=CARTESIAN_POINT('Ctrl Pts',(-1.05507170624375,15.2,-11.0994488459952));
#297396=CARTESIAN_POINT('Ctrl Pts',(-1.0538003325706,15.2,-11.1037015198691));
#297397=CARTESIAN_POINT('Ctrl Pts',(-1.05252895872422,15.2,-11.1079541943224));
#297398=CARTESIAN_POINT('Ctrl Pts',(-1.05124703809842,15.2,-11.1122175233006));
#297399=CARTESIAN_POINT('Ctrl Pts',(-1.04995452829582,15.2,-11.1164914026369));
#297400=CARTESIAN_POINT('Ctrl Pts',(-1.04898514603192,15.2,-11.1196968118479));
#297401=CARTESIAN_POINT('Ctrl Pts',(-1.04800980859123,15.2,-11.1229081555005));
#297402=CARTESIAN_POINT('Ctrl Pts',(-1.04702849637637,15.2,-11.1261253890924));
#297403=CARTESIAN_POINT('Ctrl Pts',(-1.0460471841615,15.2,-11.1293426226844));
#297404=CARTESIAN_POINT('Ctrl Pts',(-1.04505989848068,15.2,-11.1325657464673));
#297405=CARTESIAN_POINT('Ctrl Pts',(-1.0440666217251,15.2,-11.135794716475));
#297406=CARTESIAN_POINT('Ctrl Pts',(-1.04307334496953,15.2,-11.1390236864826));
#297407=CARTESIAN_POINT('Ctrl Pts',(-1.04207407795586,15.2,-11.1422585019317));
#297408=CARTESIAN_POINT('Ctrl Pts',(-1.0410688026179,15.2,-11.1454991204385));
#297409=CARTESIAN_POINT('Ctrl Pts',(-1.04006352727995,15.2,-11.1487397389453));
#297410=CARTESIAN_POINT('Ctrl Pts',(-1.03905224281003,15.2,-11.1519861597272));
#297411=CARTESIAN_POINT('Ctrl Pts',(-1.03803493396353,15.2,-11.1552383398958));
#297412=CARTESIAN_POINT('Ctrl Pts',(-1.03701762511703,15.2,-11.1584905200645));
#297413=CARTESIAN_POINT('Ctrl Pts',(-1.03599429145294,15.2,-11.1617484580745));
#297414=CARTESIAN_POINT('Ctrl Pts',(-1.03496491624116,15.2,-11.1650121125802));
#297415=CARTESIAN_POINT('Ctrl Pts',(-1.03393554084238,15.2,-11.1682757676787));
#297416=CARTESIAN_POINT('Ctrl Pts',(-1.03290012460857,15.2,-11.1715451375205));
#297417=CARTESIAN_POINT('Ctrl Pts',(-1.03185864924805,15.2,-11.1748201802056));
#297418=CARTESIAN_POINT('Ctrl Pts',(-1.03081717407673,15.2,-11.1780952222957));
#297419=CARTESIAN_POINT('Ctrl Pts',(-1.02976964141406,15.2,-11.1813759363939));
#297420=CARTESIAN_POINT('Ctrl Pts',(-1.02871603461848,15.2,-11.1846622800666));
#297421=CARTESIAN_POINT('Ctrl Pts',(-1.0276624278229,15.2,-11.1879486237394));
#297422=CARTESIAN_POINT('Ctrl Pts',(-1.02660274653194,15.2,-11.1912405979911));
#297423=CARTESIAN_POINT('Ctrl Pts',(-1.02553697477413,15.2,-11.194538157678));
#297424=CARTESIAN_POINT('Ctrl Pts',(-1.02447120301632,15.2,-11.1978357173648));
#297425=CARTESIAN_POINT('Ctrl Pts',(-1.02339934128344,15.2,-11.2011388652189));
#297426=CARTESIAN_POINT('Ctrl Pts',(-1.02232137302608,15.2,-11.2044475567803));
#297427=CARTESIAN_POINT('Ctrl Pts',(-1.02124340476871,15.2,-11.2077562483417));
#297428=CARTESIAN_POINT('Ctrl Pts',(-1.02015932972868,15.2,-11.2110704833093));
#297429=CARTESIAN_POINT('Ctrl Pts',(-1.01906913385216,15.2,-11.2143902208549));
#297430=CARTESIAN_POINT('Ctrl Pts',(-1.01797893797563,15.2,-11.2177099584005));
#297431=CARTESIAN_POINT('Ctrl Pts',(-1.01688261859954,15.2,-11.2210351971956));
#297432=CARTESIAN_POINT('Ctrl Pts',(-1.01578016326543,15.2,-11.2243658962822));
#297433=CARTESIAN_POINT('Ctrl Pts',(-1.01467770773104,15.2,-11.2276965959739));
#297434=CARTESIAN_POINT('Ctrl Pts',(-1.01356911463659,15.2,-11.2310327557087));
#297435=CARTESIAN_POINT('Ctrl Pts',(-1.01245436826541,15.2,-11.2343743329451));
#297436=CARTESIAN_POINT('Ctrl Pts',(-1.01133962209675,15.2,-11.2377159095744));
#297437=CARTESIAN_POINT('Ctrl Pts',(-1.01021872428139,15.2,-11.2410629044357));
#297438=CARTESIAN_POINT('Ctrl Pts',(-1.00909165755698,15.2,-11.2444152756486));
#297439=CARTESIAN_POINT('Ctrl Pts',(-1.00796459083257,15.2,-11.2477676468616));
#297440=CARTESIAN_POINT('Ctrl Pts',(-1.00683135638494,15.2,-11.251125393055));
#297441=CARTESIAN_POINT('Ctrl Pts',(-1.00569193959246,15.2,-11.2544884746));
#297442=CARTESIAN_POINT('Ctrl Pts',(-1.00455252279999,15.2,-11.2578515561449));
#297443=CARTESIAN_POINT('Ctrl Pts',(-1.00340692262492,15.2,-11.2612199716726));
#297444=CARTESIAN_POINT('Ctrl Pts',(-1.00225512579177,15.2,-11.2645936812583));
#297445=CARTESIAN_POINT('Ctrl Pts',(-1.0007193965414,15.2,-11.2690919611146));
#297446=CARTESIAN_POINT('Ctrl Pts',(-0.9991726478092,15.2,-11.2735996508886));
#297447=CARTESIAN_POINT('Ctrl Pts',(-0.997614847945394,15.2,-11.2781166527468));
#297448=CARTESIAN_POINT('Ctrl Pts',(-0.996446498153664,15.2,-11.2815044038328));
#297449=CARTESIAN_POINT('Ctrl Pts',(-0.995271930628931,15.2,-11.2848973936268));
#297450=CARTESIAN_POINT('Ctrl Pts',(-0.994091132379621,15.2,-11.2882955811705));
#297451=CARTESIAN_POINT('Ctrl Pts',(-0.992910334130311,15.2,-11.2916937687141));
#297452=CARTESIAN_POINT('Ctrl Pts',(-0.991723304977775,15.2,-11.2950971526781));
#297453=CARTESIAN_POINT('Ctrl Pts',(-0.990530030224015,15.2,-11.2985056942781));
#297454=CARTESIAN_POINT('Ctrl Pts',(-0.989336755470255,15.2,-11.3019142358781));
#297455=CARTESIAN_POINT('Ctrl Pts',(-0.988137235029497,15.2,-11.3053279337889));
#297456=CARTESIAN_POINT('Ctrl Pts',(-0.986931455317859,15.2,-11.3087467479719));
#297457=CARTESIAN_POINT('Ctrl Pts',(-0.984921822392114,15.2,-11.3144447718172));
#297458=CARTESIAN_POINT('Ctrl Pts',(-0.982894802494541,15.2,-11.3201570080722));
#297459=CARTESIAN_POINT('Ctrl Pts',(-0.980850330550103,15.2,-11.325883267725));
#297460=CARTESIAN_POINT('Ctrl Pts',(-0.979623647428009,15.2,-11.3293190233918));
#297461=CARTESIAN_POINT('Ctrl Pts',(-0.97839068277283,15.2,-11.3327598287168));
#297462=CARTESIAN_POINT('Ctrl Pts',(-0.97715142165174,15.2,-11.3362056423828));
#297463=CARTESIAN_POINT('Ctrl Pts',(-0.97591216053065,15.2,-11.3396514560488));
#297464=CARTESIAN_POINT('Ctrl Pts',(-0.974666603441903,15.2,-11.3431022787682));
#297465=CARTESIAN_POINT('Ctrl Pts',(-0.973414737175575,15.2,-11.3465580705648));
#297466=CARTESIAN_POINT('Ctrl Pts',(-0.972162870909247,15.2,-11.3500138623613));
#297467=CARTESIAN_POINT('Ctrl Pts',(-0.970904695512286,15.2,-11.3534746229377));
#297468=CARTESIAN_POINT('Ctrl Pts',(-0.969640197309088,15.2,-11.3569403125195));
#297469=CARTESIAN_POINT('Ctrl Pts',(-0.968375698876172,15.2,-11.3604060027308));
#297470=CARTESIAN_POINT('Ctrl Pts',(-0.967104878474818,15.2,-11.3638766210019));
#297471=CARTESIAN_POINT('Ctrl Pts',(-0.965827722496673,15.2,-11.3673521297576));
#297472=CARTESIAN_POINT('Ctrl Pts',(-0.964550566750545,15.2,-11.370827637882));
#297473=CARTESIAN_POINT('Ctrl Pts',(-0.963267074113089,15.2,-11.3743080363062));
#297474=CARTESIAN_POINT('Ctrl Pts',(-0.961977234867734,15.2,-11.37779328543));
#297475=CARTESIAN_POINT('Ctrl Pts',(-0.96068739562238,15.2,-11.3812785345537));
#297476=CARTESIAN_POINT('Ctrl Pts',(-0.959391207590864,15.2,-11.3847686341476));
#297477=CARTESIAN_POINT('Ctrl Pts',(-0.958088658423916,15.2,-11.3882635447448));
#297478=CARTESIAN_POINT('Ctrl Pts',(-0.956786109256967,15.2,-11.3917584553421));
#297479=CARTESIAN_POINT('Ctrl Pts',(-0.955477199409448,15.2,-11.3952581757582));
#297480=CARTESIAN_POINT('Ctrl Pts',(-0.95416191474296,15.2,-11.3987626660218));
#297481=CARTESIAN_POINT('Ctrl Pts',(-0.952846630076473,15.2,-11.4022671562854));
#297482=CARTESIAN_POINT('Ctrl Pts',(-0.951524971795942,15.2,-11.4057764180618));
#297483=CARTESIAN_POINT('Ctrl Pts',(-0.950196927678083,15.2,-11.4092904138504));
#297484=CARTESIAN_POINT('Ctrl Pts',(-0.948868883560225,15.2,-11.4128044096389));
#297485=CARTESIAN_POINT('Ctrl Pts',(-0.947534454142807,15.2,-11.4163231416439));
#297486=CARTESIAN_POINT('Ctrl Pts',(-0.946193627484058,15.2,-11.4198465707652));
#297487=CARTESIAN_POINT('Ctrl Pts',(-0.944852800581726,15.2,-11.4233700005267));
#297488=CARTESIAN_POINT('Ctrl Pts',(-0.943505576719271,15.2,-11.4268981283394));
#297489=CARTESIAN_POINT('Ctrl Pts',(-0.942151941188334,15.2,-11.4304309065618));
#297490=CARTESIAN_POINT('Ctrl Pts',(-0.940798305903308,15.2,-11.4339636841424));
#297491=CARTESIAN_POINT('Ctrl Pts',(-0.939438257755021,15.2,-11.4375011121365));
#297492=CARTESIAN_POINT('Ctrl Pts',(-0.93807178498566,15.2,-11.441043147727));
#297493=CARTESIAN_POINT('Ctrl Pts',(-0.936705312216299,15.2,-11.4445851833174));
#297494=CARTESIAN_POINT('Ctrl Pts',(-0.935332413680909,15.2,-11.4481318270889));
#297495=CARTESIAN_POINT('Ctrl Pts',(-0.933953085108609,15.2,-11.4516830608689));
#297496=CARTESIAN_POINT('Ctrl Pts',(-0.932573756536309,15.2,-11.4552342946488));
#297497=CARTESIAN_POINT('Ctrl Pts',(-0.931187997895759,15.2,-11.4587901218222));
#297498=CARTESIAN_POINT('Ctrl Pts',(-0.929795809339219,15.2,-11.4623505331326));
#297499=CARTESIAN_POINT('',(-3.28892417320473,15.2,-1.19707050039253));
#297500=CARTESIAN_POINT('Origin',(-5.66257110645729E-14,15.2,-1.77635683940025E-14));
#297501=CARTESIAN_POINT('Origin',(-5.66257110645729E-14,15.2,-1.77635683940025E-14));
#297502=CARTESIAN_POINT('',(-0.143881228002569,12.2,-10.3740022745144));
#297503=CARTESIAN_POINT('',(-0.143881228000057,12.2,-10.374002274));
#297504=CARTESIAN_POINT('Origin',(-5.66257110645729E-14,12.2,-1.77635683940025E-14));
#297505=CARTESIAN_POINT('Origin',(-5.66257110645729E-14,15.2,-1.77635683940025E-14));
#297506=CARTESIAN_POINT('',(-1.18690176602512,12.2,-10.306885523551));
#297507=CARTESIAN_POINT('',(-1.18690176600006,15.2,-10.306885523));
#297508=CARTESIAN_POINT('Origin',(-5.66257110645729E-14,12.2,-1.77635683940025E-14));
#297509=CARTESIAN_POINT('Origin',(-5.66257110645729E-14,15.2,-1.77635683940025E-14));
#297510=CARTESIAN_POINT('',(-0.546958306000055,12.2,-11.486985532));
#297511=CARTESIAN_POINT('',(-0.546958306000055,15.2,-11.486985532));
#297512=CARTESIAN_POINT('',(-0.929795809000057,12.2,-11.462350533));
#297513=CARTESIAN_POINT('Origin',(-5.66257110645729E-14,12.2,-1.77635683940025E-14));
#297514=CARTESIAN_POINT('',(-0.929795809000057,15.2,-11.462350533));
#297515=CARTESIAN_POINT('Ctrl Pts',(-0.546958306000055,15.2,-11.486985532));
#297516=CARTESIAN_POINT('Ctrl Pts',(-0.546958306000055,11.6,-11.486985532));
#297517=CARTESIAN_POINT('Ctrl Pts',(-0.546590899000057,15.2,-11.486315008));
#297518=CARTESIAN_POINT('Ctrl Pts',(-0.546590899000057,11.6,-11.486315008));
#297519=CARTESIAN_POINT('Ctrl Pts',(-0.545856551000057,15.2,-11.484974209));
#297520=CARTESIAN_POINT('Ctrl Pts',(-0.545856551000057,11.6,-11.484974209));
#297521=CARTESIAN_POINT('Ctrl Pts',(-0.544756421000056,15.2,-11.482963757));
#297522=CARTESIAN_POINT('Ctrl Pts',(-0.544756421000056,11.6,-11.482963757));
#297523=CARTESIAN_POINT('Ctrl Pts',(-0.543292369000056,15.2,-11.480284643));
#297524=CARTESIAN_POINT('Ctrl Pts',(-0.543292369000056,11.6,-11.480284643));
#297525=CARTESIAN_POINT('Ctrl Pts',(-0.541466946000057,15.2,-11.476938237));
#297526=CARTESIAN_POINT('Ctrl Pts',(-0.541466946000057,11.6,-11.476938237));
#297527=CARTESIAN_POINT('Ctrl Pts',(-0.539646167000055,15.2,-11.473594318));
#297528=CARTESIAN_POINT('Ctrl Pts',(-0.539646167000055,11.6,-11.473594318));
#297529=CARTESIAN_POINT('Ctrl Pts',(-0.537830030000055,15.2,-11.470252887));
#297530=CARTESIAN_POINT('Ctrl Pts',(-0.537830030000055,11.6,-11.470252887));
#297531=CARTESIAN_POINT('Ctrl Pts',(-0.536018537000055,15.2,-11.466913949));
#297532=CARTESIAN_POINT('Ctrl Pts',(-0.536018537000055,11.6,-11.466913949));
#297533=CARTESIAN_POINT('Ctrl Pts',(-0.534211686000056,15.2,-11.46357751));
#297534=CARTESIAN_POINT('Ctrl Pts',(-0.534211686000056,11.6,-11.46357751));
#297535=CARTESIAN_POINT('Ctrl Pts',(-0.532409474000056,15.2,-11.460243578));
#297536=CARTESIAN_POINT('Ctrl Pts',(-0.532409474000056,11.6,-11.460243578));
#297537=CARTESIAN_POINT('Ctrl Pts',(-0.530611902000055,15.2,-11.456912162));
#297538=CARTESIAN_POINT('Ctrl Pts',(-0.530611902000055,11.6,-11.456912162));
#297539=CARTESIAN_POINT('Ctrl Pts',(-0.528818965000056,15.2,-11.453583273));
#297540=CARTESIAN_POINT('Ctrl Pts',(-0.528818965000056,11.6,-11.453583273));
#297541=CARTESIAN_POINT('Ctrl Pts',(-0.527030665000057,15.2,-11.450256921));
#297542=CARTESIAN_POINT('Ctrl Pts',(-0.527030665000057,11.6,-11.450256921));
#297543=CARTESIAN_POINT('Ctrl Pts',(-0.525246997000056,15.2,-11.446933118));
#297544=CARTESIAN_POINT('Ctrl Pts',(-0.525246997000056,11.6,-11.446933118));
#297545=CARTESIAN_POINT('Ctrl Pts',(-0.523467959000056,15.2,-11.443611875));
#297546=CARTESIAN_POINT('Ctrl Pts',(-0.523467959000056,11.6,-11.443611875));
#297547=CARTESIAN_POINT('Ctrl Pts',(-0.521693552000055,15.2,-11.4402932));
#297548=CARTESIAN_POINT('Ctrl Pts',(-0.521693552000055,11.6,-11.4402932));
#297549=CARTESIAN_POINT('Ctrl Pts',(-0.519923771000055,15.2,-11.436977103));
#297550=CARTESIAN_POINT('Ctrl Pts',(-0.519923771000055,11.6,-11.436977103));
#297551=CARTESIAN_POINT('Ctrl Pts',(-0.518158619000056,15.2,-11.433663589));
#297552=CARTESIAN_POINT('Ctrl Pts',(-0.518158619000056,11.6,-11.433663589));
#297553=CARTESIAN_POINT('Ctrl Pts',(-0.516398090000055,15.2,-11.43035267));
#297554=CARTESIAN_POINT('Ctrl Pts',(-0.516398090000055,11.6,-11.43035267));
#297555=CARTESIAN_POINT('Ctrl Pts',(-0.514642185000056,15.2,-11.427044351));
#297556=CARTESIAN_POINT('Ctrl Pts',(-0.514642185000056,11.6,-11.427044351));
#297557=CARTESIAN_POINT('Ctrl Pts',(-0.512890901000055,15.2,-11.423738642));
#297558=CARTESIAN_POINT('Ctrl Pts',(-0.512890901000055,11.6,-11.423738642));
#297559=CARTESIAN_POINT('Ctrl Pts',(-0.511144239000056,15.2,-11.420435551));
#297560=CARTESIAN_POINT('Ctrl Pts',(-0.511144239000056,11.6,-11.420435551));
#297561=CARTESIAN_POINT('Ctrl Pts',(-0.509402194000056,15.2,-11.417135088));
#297562=CARTESIAN_POINT('Ctrl Pts',(-0.509402194000056,11.6,-11.417135088));
#297563=CARTESIAN_POINT('Ctrl Pts',(-0.507664766000057,15.2,-11.413837262));
#297564=CARTESIAN_POINT('Ctrl Pts',(-0.507664766000057,11.6,-11.413837262));
#297565=CARTESIAN_POINT('Ctrl Pts',(-0.505931954000056,15.2,-11.410542081));
#297566=CARTESIAN_POINT('Ctrl Pts',(-0.505931954000056,11.6,-11.410542081));
#297567=CARTESIAN_POINT('Ctrl Pts',(-0.504203756000056,15.2,-11.407249556));
#297568=CARTESIAN_POINT('Ctrl Pts',(-0.504203756000056,11.6,-11.407249556));
#297569=CARTESIAN_POINT('Ctrl Pts',(-0.502480169000057,15.2,-11.403959697));
#297570=CARTESIAN_POINT('Ctrl Pts',(-0.502480169000057,11.6,-11.403959697));
#297571=CARTESIAN_POINT('Ctrl Pts',(-0.500761192000055,15.2,-11.400672511));
#297572=CARTESIAN_POINT('Ctrl Pts',(-0.500761192000055,11.6,-11.400672511));
#297573=CARTESIAN_POINT('Ctrl Pts',(-0.499046823000056,15.2,-11.397388008));
#297574=CARTESIAN_POINT('Ctrl Pts',(-0.499046823000056,11.6,-11.397388008));
#297575=CARTESIAN_POINT('Ctrl Pts',(-0.497337060000056,15.2,-11.394106196));
#297576=CARTESIAN_POINT('Ctrl Pts',(-0.497337060000056,11.6,-11.394106196));
#297577=CARTESIAN_POINT('Ctrl Pts',(-0.495631904000057,15.2,-11.390827086));
#297578=CARTESIAN_POINT('Ctrl Pts',(-0.495631904000057,11.6,-11.390827086));
#297579=CARTESIAN_POINT('Ctrl Pts',(-0.493931349000055,15.2,-11.387550685));
#297580=CARTESIAN_POINT('Ctrl Pts',(-0.493931349000055,11.6,-11.387550685));
#297581=CARTESIAN_POINT('Ctrl Pts',(-0.492235397000057,15.2,-11.384277003));
#297582=CARTESIAN_POINT('Ctrl Pts',(-0.492235397000057,11.6,-11.384277003));
#297583=CARTESIAN_POINT('Ctrl Pts',(-0.490544043000056,15.2,-11.381006047));
#297584=CARTESIAN_POINT('Ctrl Pts',(-0.490544043000056,11.6,-11.381006047));
#297585=CARTESIAN_POINT('Ctrl Pts',(-0.488857288000055,15.2,-11.377737829));
#297586=CARTESIAN_POINT('Ctrl Pts',(-0.488857288000055,11.6,-11.377737829));
#297587=CARTESIAN_POINT('Ctrl Pts',(-0.487175129000056,15.2,-11.374472358));
#297588=CARTESIAN_POINT('Ctrl Pts',(-0.487175129000056,11.6,-11.374472358));
#297589=CARTESIAN_POINT('Ctrl Pts',(-0.485497564000056,15.2,-11.371209642));
#297590=CARTESIAN_POINT('Ctrl Pts',(-0.485497564000056,11.6,-11.371209642));
#297591=CARTESIAN_POINT('Ctrl Pts',(-0.483824592000056,15.2,-11.367949691));
#297592=CARTESIAN_POINT('Ctrl Pts',(-0.483824592000056,11.6,-11.367949691));
#297593=CARTESIAN_POINT('Ctrl Pts',(-0.482156209000056,15.2,-11.364692512));
#297594=CARTESIAN_POINT('Ctrl Pts',(-0.482156209000056,11.6,-11.364692512));
#297595=CARTESIAN_POINT('Ctrl Pts',(-0.480492416000056,15.2,-11.361438118));
#297596=CARTESIAN_POINT('Ctrl Pts',(-0.480492416000056,11.6,-11.361438118));
#297597=CARTESIAN_POINT('Ctrl Pts',(-0.478833210000056,15.2,-11.358186515));
#297598=CARTESIAN_POINT('Ctrl Pts',(-0.478833210000056,11.6,-11.358186515));
#297599=CARTESIAN_POINT('Ctrl Pts',(-0.477178589000056,15.2,-11.354937714));
#297600=CARTESIAN_POINT('Ctrl Pts',(-0.477178589000056,11.6,-11.354937714));
#297601=CARTESIAN_POINT('Ctrl Pts',(-0.475528552000055,15.2,-11.351691723));
#297602=CARTESIAN_POINT('Ctrl Pts',(-0.475528552000055,11.6,-11.351691723));
#297603=CARTESIAN_POINT('Ctrl Pts',(-0.473883095000056,15.2,-11.348448553));
#297604=CARTESIAN_POINT('Ctrl Pts',(-0.473883095000056,11.6,-11.348448553));
#297605=CARTESIAN_POINT('Ctrl Pts',(-0.472242218000056,15.2,-11.345208212));
#297606=CARTESIAN_POINT('Ctrl Pts',(-0.472242218000056,11.6,-11.345208212));
#297607=CARTESIAN_POINT('Ctrl Pts',(-0.470605918000055,15.2,-11.341970709));
#297608=CARTESIAN_POINT('Ctrl Pts',(-0.470605918000055,11.6,-11.341970709));
#297609=CARTESIAN_POINT('Ctrl Pts',(-0.468974194000056,15.2,-11.338736054));
#297610=CARTESIAN_POINT('Ctrl Pts',(-0.468974194000056,11.6,-11.338736054));
#297611=CARTESIAN_POINT('Ctrl Pts',(-0.467347044000055,15.2,-11.335504256));
#297612=CARTESIAN_POINT('Ctrl Pts',(-0.467347044000055,11.6,-11.335504256));
#297613=CARTESIAN_POINT('Ctrl Pts',(-0.465724466000056,15.2,-11.332275325));
#297614=CARTESIAN_POINT('Ctrl Pts',(-0.465724466000056,11.6,-11.332275325));
#297615=CARTESIAN_POINT('Ctrl Pts',(-0.464106457000056,15.2,-11.329049269));
#297616=CARTESIAN_POINT('Ctrl Pts',(-0.464106457000056,11.6,-11.329049269));
#297617=CARTESIAN_POINT('Ctrl Pts',(-0.462493018000056,15.2,-11.325826098));
#297618=CARTESIAN_POINT('Ctrl Pts',(-0.462493018000056,11.6,-11.325826098));
#297619=CARTESIAN_POINT('Ctrl Pts',(-0.460884143000057,15.2,-11.322605822));
#297620=CARTESIAN_POINT('Ctrl Pts',(-0.460884143000057,11.6,-11.322605822));
#297621=CARTESIAN_POINT('Ctrl Pts',(-0.459279833000057,15.2,-11.319388451));
#297622=CARTESIAN_POINT('Ctrl Pts',(-0.459279833000057,11.6,-11.319388451));
#297623=CARTESIAN_POINT('Ctrl Pts',(-0.457680085000056,15.2,-11.316173992));
#297624=CARTESIAN_POINT('Ctrl Pts',(-0.457680085000056,11.6,-11.316173992));
#297625=CARTESIAN_POINT('Ctrl Pts',(-0.456084896000055,15.2,-11.312962457));
#297626=CARTESIAN_POINT('Ctrl Pts',(-0.456084896000055,11.6,-11.312962457));
#297627=CARTESIAN_POINT('Ctrl Pts',(-0.454494265000056,15.2,-11.309753853));
#297628=CARTESIAN_POINT('Ctrl Pts',(-0.454494265000056,11.6,-11.309753853));
#297629=CARTESIAN_POINT('Ctrl Pts',(-0.452908191000055,15.2,-11.306548191));
#297630=CARTESIAN_POINT('Ctrl Pts',(-0.452908191000055,11.6,-11.306548191));
#297631=CARTESIAN_POINT('Ctrl Pts',(-0.451326671000055,15.2,-11.303345481));
#297632=CARTESIAN_POINT('Ctrl Pts',(-0.451326671000055,11.6,-11.303345481));
#297633=CARTESIAN_POINT('Ctrl Pts',(-0.449749702000056,15.2,-11.300145731));
#297634=CARTESIAN_POINT('Ctrl Pts',(-0.449749702000056,11.6,-11.300145731));
#297635=CARTESIAN_POINT('Ctrl Pts',(-0.448177284000056,15.2,-11.296948952));
#297636=CARTESIAN_POINT('Ctrl Pts',(-0.448177284000056,11.6,-11.296948952));
#297637=CARTESIAN_POINT('Ctrl Pts',(-0.446609414000055,15.2,-11.293755152));
#297638=CARTESIAN_POINT('Ctrl Pts',(-0.446609414000055,11.6,-11.293755152));
#297639=CARTESIAN_POINT('Ctrl Pts',(-0.445046088000056,15.2,-11.290564341));
#297640=CARTESIAN_POINT('Ctrl Pts',(-0.445046088000056,11.6,-11.290564341));
#297641=CARTESIAN_POINT('Ctrl Pts',(-0.443487307000057,15.2,-11.287376529));
#297642=CARTESIAN_POINT('Ctrl Pts',(-0.443487307000057,11.6,-11.287376529));
#297643=CARTESIAN_POINT('Ctrl Pts',(-0.441933068000055,15.2,-11.284191725));
#297644=CARTESIAN_POINT('Ctrl Pts',(-0.441933068000055,11.6,-11.284191725));
#297645=CARTESIAN_POINT('Ctrl Pts',(-0.440383367000056,15.2,-11.281009939));
#297646=CARTESIAN_POINT('Ctrl Pts',(-0.440383367000056,11.6,-11.281009939));
#297647=CARTESIAN_POINT('Ctrl Pts',(-0.438838204000056,15.2,-11.277831182));
#297648=CARTESIAN_POINT('Ctrl Pts',(-0.438838204000056,11.6,-11.277831182));
#297649=CARTESIAN_POINT('Ctrl Pts',(-0.437297576000055,15.2,-11.274655461));
#297650=CARTESIAN_POINT('Ctrl Pts',(-0.437297576000055,11.6,-11.274655461));
#297651=CARTESIAN_POINT('Ctrl Pts',(-0.435761482000055,15.2,-11.271482787));
#297652=CARTESIAN_POINT('Ctrl Pts',(-0.435761482000055,11.6,-11.271482787));
#297653=CARTESIAN_POINT('Ctrl Pts',(-0.434229918000056,15.2,-11.268313169));
#297654=CARTESIAN_POINT('Ctrl Pts',(-0.434229918000056,11.6,-11.268313169));
#297655=CARTESIAN_POINT('Ctrl Pts',(-0.432702884000056,15.2,-11.265146617));
#297656=CARTESIAN_POINT('Ctrl Pts',(-0.432702884000056,11.6,-11.265146617));
#297657=CARTESIAN_POINT('Ctrl Pts',(-0.431180374000055,15.2,-11.261983141));
#297658=CARTESIAN_POINT('Ctrl Pts',(-0.431180374000055,11.6,-11.261983141));
#297659=CARTESIAN_POINT('Ctrl Pts',(-0.429662391000055,15.2,-11.258822751));
#297660=CARTESIAN_POINT('Ctrl Pts',(-0.429662391000055,11.6,-11.258822751));
#297661=CARTESIAN_POINT('Ctrl Pts',(-0.428148929000055,15.2,-11.255665455));
#297662=CARTESIAN_POINT('Ctrl Pts',(-0.428148929000055,11.6,-11.255665455));
#297663=CARTESIAN_POINT('Ctrl Pts',(-0.426639987000056,15.2,-11.252511265));
#297664=CARTESIAN_POINT('Ctrl Pts',(-0.426639987000056,11.6,-11.252511265));
#297665=CARTESIAN_POINT('Ctrl Pts',(-0.425135562000056,15.2,-11.249360189));
#297666=CARTESIAN_POINT('Ctrl Pts',(-0.425135562000056,11.6,-11.249360189));
#297667=CARTESIAN_POINT('Ctrl Pts',(-0.423635654000056,15.2,-11.246212238));
#297668=CARTESIAN_POINT('Ctrl Pts',(-0.423635654000056,11.6,-11.246212238));
#297669=CARTESIAN_POINT('Ctrl Pts',(-0.422140258000056,15.2,-11.243067421));
#297670=CARTESIAN_POINT('Ctrl Pts',(-0.422140258000056,11.6,-11.243067421));
#297671=CARTESIAN_POINT('Ctrl Pts',(-0.420649373000056,15.2,-11.239925747));
#297672=CARTESIAN_POINT('Ctrl Pts',(-0.420649373000056,11.6,-11.239925747));
#297673=CARTESIAN_POINT('Ctrl Pts',(-0.419162997000055,15.2,-11.236787227));
#297674=CARTESIAN_POINT('Ctrl Pts',(-0.419162997000055,11.6,-11.236787227));
#297675=CARTESIAN_POINT('Ctrl Pts',(-0.417681127000057,15.2,-11.233651872));
#297676=CARTESIAN_POINT('Ctrl Pts',(-0.417681127000057,11.6,-11.233651872));
#297677=CARTESIAN_POINT('Ctrl Pts',(-0.416203762000055,15.2,-11.230519688));
#297678=CARTESIAN_POINT('Ctrl Pts',(-0.416203762000055,11.6,-11.230519688));
#297679=CARTESIAN_POINT('Ctrl Pts',(-0.414730899000055,15.2,-11.22739069));
#297680=CARTESIAN_POINT('Ctrl Pts',(-0.414730899000055,11.6,-11.22739069));
#297681=CARTESIAN_POINT('Ctrl Pts',(-0.413262534000056,15.2,-11.224264883));
#297682=CARTESIAN_POINT('Ctrl Pts',(-0.413262534000056,11.6,-11.224264883));
#297683=CARTESIAN_POINT('Ctrl Pts',(-0.411798667000056,15.2,-11.221142281));
#297684=CARTESIAN_POINT('Ctrl Pts',(-0.411798667000056,11.6,-11.221142281));
#297685=CARTESIAN_POINT('Ctrl Pts',(-0.410339295000056,15.2,-11.21802289));
#297686=CARTESIAN_POINT('Ctrl Pts',(-0.410339295000056,11.6,-11.21802289));
#297687=CARTESIAN_POINT('Ctrl Pts',(-0.408884415000056,15.2,-11.214906723));
#297688=CARTESIAN_POINT('Ctrl Pts',(-0.408884415000056,11.6,-11.214906723));
#297689=CARTESIAN_POINT('Ctrl Pts',(-0.407434025000055,15.2,-11.211793789));
#297690=CARTESIAN_POINT('Ctrl Pts',(-0.407434025000055,11.6,-11.211793789));
#297691=CARTESIAN_POINT('Ctrl Pts',(-0.405988122000055,15.2,-11.208684097));
#297692=CARTESIAN_POINT('Ctrl Pts',(-0.405988122000055,11.6,-11.208684097));
#297693=CARTESIAN_POINT('Ctrl Pts',(-0.404546705000056,15.2,-11.205577658));
#297694=CARTESIAN_POINT('Ctrl Pts',(-0.404546705000056,11.6,-11.205577658));
#297695=CARTESIAN_POINT('Ctrl Pts',(-0.403109771000055,15.2,-11.202474481));
#297696=CARTESIAN_POINT('Ctrl Pts',(-0.403109771000055,11.6,-11.202474481));
#297697=CARTESIAN_POINT('Ctrl Pts',(-0.401677318000055,15.2,-11.199374578));
#297698=CARTESIAN_POINT('Ctrl Pts',(-0.401677318000055,11.6,-11.199374578));
#297699=CARTESIAN_POINT('Ctrl Pts',(-0.400249343000055,15.2,-11.196277957));
#297700=CARTESIAN_POINT('Ctrl Pts',(-0.400249343000055,11.6,-11.196277957));
#297701=CARTESIAN_POINT('Ctrl Pts',(-0.398825842000056,15.2,-11.193184629));
#297702=CARTESIAN_POINT('Ctrl Pts',(-0.398825842000056,11.6,-11.193184629));
#297703=CARTESIAN_POINT('Ctrl Pts',(-0.397406814000056,15.2,-11.190094604));
#297704=CARTESIAN_POINT('Ctrl Pts',(-0.397406814000056,11.6,-11.190094604));
#297705=CARTESIAN_POINT('Ctrl Pts',(-0.395992258000056,15.2,-11.187007892));
#297706=CARTESIAN_POINT('Ctrl Pts',(-0.395992258000056,11.6,-11.187007892));
#297707=CARTESIAN_POINT('Ctrl Pts',(-0.394582170000056,15.2,-11.183924502));
#297708=CARTESIAN_POINT('Ctrl Pts',(-0.394582170000056,11.6,-11.183924502));
#297709=CARTESIAN_POINT('Ctrl Pts',(-0.393176547000056,15.2,-11.180844447));
#297710=CARTESIAN_POINT('Ctrl Pts',(-0.393176547000056,11.6,-11.180844447));
#297711=CARTESIAN_POINT('Ctrl Pts',(-0.391775388000056,15.2,-11.177767733));
#297712=CARTESIAN_POINT('Ctrl Pts',(-0.391775388000056,11.6,-11.177767733));
#297713=CARTESIAN_POINT('Ctrl Pts',(-0.390378688000055,15.2,-11.174694374));
#297714=CARTESIAN_POINT('Ctrl Pts',(-0.390378688000055,11.6,-11.174694374));
#297715=CARTESIAN_POINT('Ctrl Pts',(-0.388986447000056,15.2,-11.171624379));
#297716=CARTESIAN_POINT('Ctrl Pts',(-0.388986447000056,11.6,-11.171624379));
#297717=CARTESIAN_POINT('Ctrl Pts',(-0.387598661000055,15.2,-11.168557756));
#297718=CARTESIAN_POINT('Ctrl Pts',(-0.387598661000055,11.6,-11.168557756));
#297719=CARTESIAN_POINT('Ctrl Pts',(-0.386215329000056,15.2,-11.165494519));
#297720=CARTESIAN_POINT('Ctrl Pts',(-0.386215329000056,11.6,-11.165494519));
#297721=CARTESIAN_POINT('Ctrl Pts',(-0.384836446000056,15.2,-11.162434675));
#297722=CARTESIAN_POINT('Ctrl Pts',(-0.384836446000056,11.6,-11.162434675));
#297723=CARTESIAN_POINT('Ctrl Pts',(-0.383462012000055,15.2,-11.159378235));
#297724=CARTESIAN_POINT('Ctrl Pts',(-0.383462012000055,11.6,-11.159378235));
#297725=CARTESIAN_POINT('Ctrl Pts',(-0.382092022000055,15.2,-11.156325211));
#297726=CARTESIAN_POINT('Ctrl Pts',(-0.382092022000055,11.6,-11.156325211));
#297727=CARTESIAN_POINT('Ctrl Pts',(-0.380726475000056,15.2,-11.153275611));
#297728=CARTESIAN_POINT('Ctrl Pts',(-0.380726475000056,11.6,-11.153275611));
#297729=CARTESIAN_POINT('Ctrl Pts',(-0.379365367000055,15.2,-11.150229445));
#297730=CARTESIAN_POINT('Ctrl Pts',(-0.379365367000055,11.6,-11.150229445));
#297731=CARTESIAN_POINT('Ctrl Pts',(-0.378008697000055,15.2,-11.147186726));
#297732=CARTESIAN_POINT('Ctrl Pts',(-0.378008697000055,11.6,-11.147186726));
#297733=CARTESIAN_POINT('Ctrl Pts',(-0.376656462000057,15.2,-11.144147464));
#297734=CARTESIAN_POINT('Ctrl Pts',(-0.376656462000057,11.6,-11.144147464));
#297735=CARTESIAN_POINT('Ctrl Pts',(-0.375308659000056,15.2,-11.141111667));
#297736=CARTESIAN_POINT('Ctrl Pts',(-0.375308659000056,11.6,-11.141111667));
#297737=CARTESIAN_POINT('Ctrl Pts',(-0.373965284000055,15.2,-11.138079346));
#297738=CARTESIAN_POINT('Ctrl Pts',(-0.373965284000055,11.6,-11.138079346));
#297739=CARTESIAN_POINT('Ctrl Pts',(-0.372626336000056,15.2,-11.135050513));
#297740=CARTESIAN_POINT('Ctrl Pts',(-0.372626336000056,11.6,-11.135050513));
#297741=CARTESIAN_POINT('Ctrl Pts',(-0.371291813000055,15.2,-11.132025177));
#297742=CARTESIAN_POINT('Ctrl Pts',(-0.371291813000055,11.6,-11.132025177));
#297743=CARTESIAN_POINT('Ctrl Pts',(-0.369961710000055,15.2,-11.129003349));
#297744=CARTESIAN_POINT('Ctrl Pts',(-0.369961710000055,11.6,-11.129003349));
#297745=CARTESIAN_POINT('Ctrl Pts',(-0.368636025000055,15.2,-11.125985039));
#297746=CARTESIAN_POINT('Ctrl Pts',(-0.368636025000055,11.6,-11.125985039));
#297747=CARTESIAN_POINT('Ctrl Pts',(-0.367314756000056,15.2,-11.122970257));
#297748=CARTESIAN_POINT('Ctrl Pts',(-0.367314756000056,11.6,-11.122970257));
#297749=CARTESIAN_POINT('Ctrl Pts',(-0.365997899000057,15.2,-11.119959015));
#297750=CARTESIAN_POINT('Ctrl Pts',(-0.365997899000057,11.6,-11.119959015));
#297751=CARTESIAN_POINT('Ctrl Pts',(-0.364685453000057,15.2,-11.116951323));
#297752=CARTESIAN_POINT('Ctrl Pts',(-0.364685453000057,11.6,-11.116951323));
#297753=CARTESIAN_POINT('Ctrl Pts',(-0.363377414000056,15.2,-11.11394719));
#297754=CARTESIAN_POINT('Ctrl Pts',(-0.363377414000056,11.6,-11.11394719));
#297755=CARTESIAN_POINT('Ctrl Pts',(-0.362073780000056,15.2,-11.110946628));
#297756=CARTESIAN_POINT('Ctrl Pts',(-0.362073780000056,11.6,-11.110946628));
#297757=CARTESIAN_POINT('Ctrl Pts',(-0.360774547000055,15.2,-11.107949648));
#297758=CARTESIAN_POINT('Ctrl Pts',(-0.360774547000055,11.6,-11.107949648));
#297759=CARTESIAN_POINT('Ctrl Pts',(-0.359479712000056,15.2,-11.104956259));
#297760=CARTESIAN_POINT('Ctrl Pts',(-0.359479712000056,11.6,-11.104956259));
#297761=CARTESIAN_POINT('Ctrl Pts',(-0.358189274000056,15.2,-11.101966474));
#297762=CARTESIAN_POINT('Ctrl Pts',(-0.358189274000056,11.6,-11.101966474));
#297763=CARTESIAN_POINT('Ctrl Pts',(-0.356903229000055,15.2,-11.0989803));
#297764=CARTESIAN_POINT('Ctrl Pts',(-0.356903229000055,11.6,-11.0989803));
#297765=CARTESIAN_POINT('Ctrl Pts',(-0.355621573000056,15.2,-11.09599775));
#297766=CARTESIAN_POINT('Ctrl Pts',(-0.355621573000056,11.6,-11.09599775));
#297767=CARTESIAN_POINT('Ctrl Pts',(-0.354344305000056,15.2,-11.093018835));
#297768=CARTESIAN_POINT('Ctrl Pts',(-0.354344305000056,11.6,-11.093018835));
#297769=CARTESIAN_POINT('Ctrl Pts',(-0.353071422000056,15.2,-11.090043565));
#297770=CARTESIAN_POINT('Ctrl Pts',(-0.353071422000056,11.6,-11.090043565));
#297771=CARTESIAN_POINT('Ctrl Pts',(-0.351802919000056,15.2,-11.08707195));
#297772=CARTESIAN_POINT('Ctrl Pts',(-0.351802919000056,11.6,-11.08707195));
#297773=CARTESIAN_POINT('Ctrl Pts',(-0.350538795000055,15.2,-11.084104002));
#297774=CARTESIAN_POINT('Ctrl Pts',(-0.350538795000055,11.6,-11.084104002));
#297775=CARTESIAN_POINT('Ctrl Pts',(-0.349279047000056,15.2,-11.08113973));
#297776=CARTESIAN_POINT('Ctrl Pts',(-0.349279047000056,11.6,-11.08113973));
#297777=CARTESIAN_POINT('Ctrl Pts',(-0.348023671000056,15.2,-11.078179147));
#297778=CARTESIAN_POINT('Ctrl Pts',(-0.348023671000056,11.6,-11.078179147));
#297779=CARTESIAN_POINT('Ctrl Pts',(-0.346772665000056,15.2,-11.075222262));
#297780=CARTESIAN_POINT('Ctrl Pts',(-0.346772665000056,11.6,-11.075222262));
#297781=CARTESIAN_POINT('Ctrl Pts',(-0.345526025000057,15.2,-11.072269087));
#297782=CARTESIAN_POINT('Ctrl Pts',(-0.345526025000057,11.6,-11.072269087));
#297783=CARTESIAN_POINT('Ctrl Pts',(-0.344283750000055,15.2,-11.069319632));
#297784=CARTESIAN_POINT('Ctrl Pts',(-0.344283750000055,11.6,-11.069319632));
#297785=CARTESIAN_POINT('Ctrl Pts',(-0.343045833000056,15.2,-11.066373907));
#297786=CARTESIAN_POINT('Ctrl Pts',(-0.343045833000056,11.6,-11.066373907));
#297787=CARTESIAN_POINT('Ctrl Pts',(-0.341812276000055,15.2,-11.063431925));
#297788=CARTESIAN_POINT('Ctrl Pts',(-0.341812276000055,11.6,-11.063431925));
#297789=CARTESIAN_POINT('Ctrl Pts',(-0.340583073000056,15.2,-11.060493695));
#297790=CARTESIAN_POINT('Ctrl Pts',(-0.340583073000056,11.6,-11.060493695));
#297791=CARTESIAN_POINT('Ctrl Pts',(-0.339358220000056,15.2,-11.057559229));
#297792=CARTESIAN_POINT('Ctrl Pts',(-0.339358220000056,11.6,-11.057559229));
#297793=CARTESIAN_POINT('Ctrl Pts',(-0.338137716000055,15.2,-11.054628537));
#297794=CARTESIAN_POINT('Ctrl Pts',(-0.338137716000055,11.6,-11.054628537));
#297795=CARTESIAN_POINT('Ctrl Pts',(-0.336921557000055,15.2,-11.051701631));
#297796=CARTESIAN_POINT('Ctrl Pts',(-0.336921557000055,11.6,-11.051701631));
#297797=CARTESIAN_POINT('Ctrl Pts',(-0.335709740000055,15.2,-11.048778521));
#297798=CARTESIAN_POINT('Ctrl Pts',(-0.335709740000055,11.6,-11.048778521));
#297799=CARTESIAN_POINT('Ctrl Pts',(-0.334502263000056,15.2,-11.045859219));
#297800=CARTESIAN_POINT('Ctrl Pts',(-0.334502263000056,11.6,-11.045859219));
#297801=CARTESIAN_POINT('Ctrl Pts',(-0.333299121000056,15.2,-11.042943735));
#297802=CARTESIAN_POINT('Ctrl Pts',(-0.333299121000056,11.6,-11.042943735));
#297803=CARTESIAN_POINT('Ctrl Pts',(-0.332100311000056,15.2,-11.040032081));
#297804=CARTESIAN_POINT('Ctrl Pts',(-0.332100311000056,11.6,-11.040032081));
#297805=CARTESIAN_POINT('Ctrl Pts',(-0.330905831000056,15.2,-11.037124266));
#297806=CARTESIAN_POINT('Ctrl Pts',(-0.330905831000056,11.6,-11.037124266));
#297807=CARTESIAN_POINT('Ctrl Pts',(-0.329715678000057,15.2,-11.034220304));
#297808=CARTESIAN_POINT('Ctrl Pts',(-0.329715678000057,11.6,-11.034220304));
#297809=CARTESIAN_POINT('Ctrl Pts',(-0.328529847000055,15.2,-11.031320204));
#297810=CARTESIAN_POINT('Ctrl Pts',(-0.328529847000055,11.6,-11.031320204));
#297811=CARTESIAN_POINT('Ctrl Pts',(-0.327348336000056,15.2,-11.028423977));
#297812=CARTESIAN_POINT('Ctrl Pts',(-0.327348336000056,11.6,-11.028423977));
#297813=CARTESIAN_POINT('Ctrl Pts',(-0.326171142000057,15.2,-11.025531635));
#297814=CARTESIAN_POINT('Ctrl Pts',(-0.326171142000057,11.6,-11.025531635));
#297815=CARTESIAN_POINT('Ctrl Pts',(-0.324998260000056,15.2,-11.022643189));
#297816=CARTESIAN_POINT('Ctrl Pts',(-0.324998260000056,11.6,-11.022643189));
#297817=CARTESIAN_POINT('Ctrl Pts',(-0.323829689000057,15.2,-11.01975865));
#297818=CARTESIAN_POINT('Ctrl Pts',(-0.323829689000057,11.6,-11.01975865));
#297819=CARTESIAN_POINT('Ctrl Pts',(-0.322665426000055,15.2,-11.01687803));
#297820=CARTESIAN_POINT('Ctrl Pts',(-0.322665426000055,11.6,-11.01687803));
#297821=CARTESIAN_POINT('Ctrl Pts',(-0.321505465000056,15.2,-11.014001338));
#297822=CARTESIAN_POINT('Ctrl Pts',(-0.321505465000056,11.6,-11.014001338));
#297823=CARTESIAN_POINT('Ctrl Pts',(-0.320349803000056,15.2,-11.011128588));
#297824=CARTESIAN_POINT('Ctrl Pts',(-0.320349803000056,11.6,-11.011128588));
#297825=CARTESIAN_POINT('Ctrl Pts',(-0.319198440000056,15.2,-11.008259788));
#297826=CARTESIAN_POINT('Ctrl Pts',(-0.319198440000056,11.6,-11.008259788));
#297827=CARTESIAN_POINT('Ctrl Pts',(-0.318051369000055,15.2,-11.005394953));
#297828=CARTESIAN_POINT('Ctrl Pts',(-0.318051369000055,11.6,-11.005394953));
#297829=CARTESIAN_POINT('Ctrl Pts',(-0.316908589000056,15.2,-11.002534092));
#297830=CARTESIAN_POINT('Ctrl Pts',(-0.316908589000056,11.6,-11.002534092));
#297831=CARTESIAN_POINT('Ctrl Pts',(-0.315770096000056,15.2,-10.999677217));
#297832=CARTESIAN_POINT('Ctrl Pts',(-0.315770096000056,11.6,-10.999677217));
#297833=CARTESIAN_POINT('Ctrl Pts',(-0.314635885000056,15.2,-10.996824339));
#297834=CARTESIAN_POINT('Ctrl Pts',(-0.314635885000056,11.6,-10.996824339));
#297835=CARTESIAN_POINT('Ctrl Pts',(-0.313505954000056,15.2,-10.993975469));
#297836=CARTESIAN_POINT('Ctrl Pts',(-0.313505954000056,11.6,-10.993975469));
#297837=CARTESIAN_POINT('Ctrl Pts',(-0.312380301000056,15.2,-10.991130619));
#297838=CARTESIAN_POINT('Ctrl Pts',(-0.312380301000056,11.6,-10.991130619));
#297839=CARTESIAN_POINT('Ctrl Pts',(-0.311258919000055,15.2,-10.988289801));
#297840=CARTESIAN_POINT('Ctrl Pts',(-0.311258919000055,11.6,-10.988289801));
#297841=CARTESIAN_POINT('Ctrl Pts',(-0.310141808000056,15.2,-10.985453024));
#297842=CARTESIAN_POINT('Ctrl Pts',(-0.310141808000056,11.6,-10.985453024));
#297843=CARTESIAN_POINT('Ctrl Pts',(-0.309028962000056,15.2,-10.982620303));
#297844=CARTESIAN_POINT('Ctrl Pts',(-0.309028962000056,11.6,-10.982620303));
#297845=CARTESIAN_POINT('Ctrl Pts',(-0.307920380000055,15.2,-10.979791646));
#297846=CARTESIAN_POINT('Ctrl Pts',(-0.307920380000055,11.6,-10.979791646));
#297847=CARTESIAN_POINT('Ctrl Pts',(-0.306816056000055,15.2,-10.976967067));
#297848=CARTESIAN_POINT('Ctrl Pts',(-0.306816056000055,11.6,-10.976967067));
#297849=CARTESIAN_POINT('Ctrl Pts',(-0.305715987000056,15.2,-10.974146576));
#297850=CARTESIAN_POINT('Ctrl Pts',(-0.305715987000056,11.6,-10.974146576));
#297851=CARTESIAN_POINT('Ctrl Pts',(-0.304620171000056,15.2,-10.971330186));
#297852=CARTESIAN_POINT('Ctrl Pts',(-0.304620171000056,11.6,-10.971330186));
#297853=CARTESIAN_POINT('Ctrl Pts',(-0.303528603000055,15.2,-10.968517907));
#297854=CARTESIAN_POINT('Ctrl Pts',(-0.303528603000055,11.6,-10.968517907));
#297855=CARTESIAN_POINT('Ctrl Pts',(-0.302441280000056,15.2,-10.965709752));
#297856=CARTESIAN_POINT('Ctrl Pts',(-0.302441280000056,11.6,-10.965709752));
#297857=CARTESIAN_POINT('Ctrl Pts',(-0.301358198000056,15.2,-10.962905731));
#297858=CARTESIAN_POINT('Ctrl Pts',(-0.301358198000056,11.6,-10.962905731));
#297859=CARTESIAN_POINT('Ctrl Pts',(-0.300279354000056,15.2,-10.960105857));
#297860=CARTESIAN_POINT('Ctrl Pts',(-0.300279354000056,11.6,-10.960105857));
#297861=CARTESIAN_POINT('Ctrl Pts',(-0.299204743000056,15.2,-10.957310141));
#297862=CARTESIAN_POINT('Ctrl Pts',(-0.299204743000056,11.6,-10.957310141));
#297863=CARTESIAN_POINT('Ctrl Pts',(-0.298134363000055,15.2,-10.954518595));
#297864=CARTESIAN_POINT('Ctrl Pts',(-0.298134363000055,11.6,-10.954518595));
#297865=CARTESIAN_POINT('Ctrl Pts',(-0.297068210000055,15.2,-10.951731231));
#297866=CARTESIAN_POINT('Ctrl Pts',(-0.297068210000055,11.6,-10.951731231));
#297867=CARTESIAN_POINT('Ctrl Pts',(-0.296006280000055,15.2,-10.948948059));
#297868=CARTESIAN_POINT('Ctrl Pts',(-0.296006280000055,11.6,-10.948948059));
#297869=CARTESIAN_POINT('Ctrl Pts',(-0.294948568000055,15.2,-10.946169093));
#297870=CARTESIAN_POINT('Ctrl Pts',(-0.294948568000055,11.6,-10.946169093));
#297871=CARTESIAN_POINT('Ctrl Pts',(-0.293895073000057,15.2,-10.943394344));
#297872=CARTESIAN_POINT('Ctrl Pts',(-0.293895073000057,11.6,-10.943394344));
#297873=CARTESIAN_POINT('Ctrl Pts',(-0.292845789000056,15.2,-10.940623823));
#297874=CARTESIAN_POINT('Ctrl Pts',(-0.292845789000056,11.6,-10.940623823));
#297875=CARTESIAN_POINT('Ctrl Pts',(-0.291800713000056,15.2,-10.937857543));
#297876=CARTESIAN_POINT('Ctrl Pts',(-0.291800713000056,11.6,-10.937857543));
#297877=CARTESIAN_POINT('Ctrl Pts',(-0.290759842000057,15.2,-10.935095515));
#297878=CARTESIAN_POINT('Ctrl Pts',(-0.290759842000057,11.6,-10.935095515));
#297879=CARTESIAN_POINT('Ctrl Pts',(-0.289723171000055,15.2,-10.932337751));
#297880=CARTESIAN_POINT('Ctrl Pts',(-0.289723171000055,11.6,-10.932337751));
#297881=CARTESIAN_POINT('Ctrl Pts',(-0.288690696000057,15.2,-10.929584264));
#297882=CARTESIAN_POINT('Ctrl Pts',(-0.288690696000057,11.6,-10.929584264));
#297883=CARTESIAN_POINT('Ctrl Pts',(-0.287662415000056,15.2,-10.926835064));
#297884=CARTESIAN_POINT('Ctrl Pts',(-0.287662415000056,11.6,-10.926835064));
#297885=CARTESIAN_POINT('Ctrl Pts',(-0.286638323000057,15.2,-10.924090164));
#297886=CARTESIAN_POINT('Ctrl Pts',(-0.286638323000057,11.6,-10.924090164));
#297887=CARTESIAN_POINT('Ctrl Pts',(-0.285618416000055,15.2,-10.921349576));
#297888=CARTESIAN_POINT('Ctrl Pts',(-0.285618416000055,11.6,-10.921349576));
#297889=CARTESIAN_POINT('Ctrl Pts',(-0.284602690000056,15.2,-10.918613312));
#297890=CARTESIAN_POINT('Ctrl Pts',(-0.284602690000056,11.6,-10.918613312));
#297891=CARTESIAN_POINT('Ctrl Pts',(-0.283591141000056,15.2,-10.915881383));
#297892=CARTESIAN_POINT('Ctrl Pts',(-0.283591141000056,11.6,-10.915881383));
#297893=CARTESIAN_POINT('Ctrl Pts',(-0.282583766000055,15.2,-10.913153802));
#297894=CARTESIAN_POINT('Ctrl Pts',(-0.282583766000055,11.6,-10.913153802));
#297895=CARTESIAN_POINT('Ctrl Pts',(-0.281580560000056,15.2,-10.910430583));
#297896=CARTESIAN_POINT('Ctrl Pts',(-0.281580560000056,11.6,-10.910430583));
#297897=CARTESIAN_POINT('Ctrl Pts',(-0.280581520000055,15.2,-10.907711734));
#297898=CARTESIAN_POINT('Ctrl Pts',(-0.280581520000055,11.6,-10.907711734));
#297899=CARTESIAN_POINT('Ctrl Pts',(-0.279586642000057,15.2,-10.904997271));
#297900=CARTESIAN_POINT('Ctrl Pts',(-0.279586642000057,11.6,-10.904997271));
#297901=CARTESIAN_POINT('Ctrl Pts',(-0.278595921000055,15.2,-10.902287203));
#297902=CARTESIAN_POINT('Ctrl Pts',(-0.278595921000055,11.6,-10.902287203));
#297903=CARTESIAN_POINT('Ctrl Pts',(-0.277609355000056,15.2,-10.899581544));
#297904=CARTESIAN_POINT('Ctrl Pts',(-0.277609355000056,11.6,-10.899581544));
#297905=CARTESIAN_POINT('Ctrl Pts',(-0.276626937000056,15.2,-10.896880306));
#297906=CARTESIAN_POINT('Ctrl Pts',(-0.276626937000056,11.6,-10.896880306));
#297907=CARTESIAN_POINT('Ctrl Pts',(-0.275648666000056,15.2,-10.8941835));
#297908=CARTESIAN_POINT('Ctrl Pts',(-0.275648666000056,11.6,-10.8941835));
#297909=CARTESIAN_POINT('Ctrl Pts',(-0.274674534000056,15.2,-10.891491141));
#297910=CARTESIAN_POINT('Ctrl Pts',(-0.274674534000056,11.6,-10.891491141));
#297911=CARTESIAN_POINT('Ctrl Pts',(-0.273704541000056,15.2,-10.888803238));
#297912=CARTESIAN_POINT('Ctrl Pts',(-0.273704541000056,11.6,-10.888803238));
#297913=CARTESIAN_POINT('Ctrl Pts',(-0.272738681000056,15.2,-10.886119805));
#297914=CARTESIAN_POINT('Ctrl Pts',(-0.272738681000056,11.6,-10.886119805));
#297915=CARTESIAN_POINT('Ctrl Pts',(-0.271776951000057,15.2,-10.883440854));
#297916=CARTESIAN_POINT('Ctrl Pts',(-0.271776951000057,11.6,-10.883440854));
#297917=CARTESIAN_POINT('Ctrl Pts',(-0.270819345000056,15.2,-10.880766398));
#297918=CARTESIAN_POINT('Ctrl Pts',(-0.270819345000056,11.6,-10.880766398));
#297919=CARTESIAN_POINT('Ctrl Pts',(-0.269865860000056,15.2,-10.878096449));
#297920=CARTESIAN_POINT('Ctrl Pts',(-0.269865860000056,11.6,-10.878096449));
#297921=CARTESIAN_POINT('Ctrl Pts',(-0.268916493000055,15.2,-10.87543102));
#297922=CARTESIAN_POINT('Ctrl Pts',(-0.268916493000055,11.6,-10.87543102));
#297923=CARTESIAN_POINT('Ctrl Pts',(-0.267971237000056,15.2,-10.872770121));
#297924=CARTESIAN_POINT('Ctrl Pts',(-0.267971237000056,11.6,-10.872770121));
#297925=CARTESIAN_POINT('Ctrl Pts',(-0.267030089000055,15.2,-10.870113767));
#297926=CARTESIAN_POINT('Ctrl Pts',(-0.267030089000055,11.6,-10.870113767));
#297927=CARTESIAN_POINT('Ctrl Pts',(-0.266093047000057,15.2,-10.86746197));
#297928=CARTESIAN_POINT('Ctrl Pts',(-0.266093047000057,11.6,-10.86746197));
#297929=CARTESIAN_POINT('Ctrl Pts',(-0.265160103000056,15.2,-10.864814742));
#297930=CARTESIAN_POINT('Ctrl Pts',(-0.265160103000056,11.6,-10.864814742));
#297931=CARTESIAN_POINT('Ctrl Pts',(-0.264231255000055,15.2,-10.862172095));
#297932=CARTESIAN_POINT('Ctrl Pts',(-0.264231255000055,11.6,-10.862172095));
#297933=CARTESIAN_POINT('Ctrl Pts',(-0.263306498000055,15.2,-10.859534042));
#297934=CARTESIAN_POINT('Ctrl Pts',(-0.263306498000055,11.6,-10.859534042));
#297935=CARTESIAN_POINT('Ctrl Pts',(-0.262385828000056,15.2,-10.856900598));
#297936=CARTESIAN_POINT('Ctrl Pts',(-0.262385828000056,11.6,-10.856900598));
#297937=CARTESIAN_POINT('Ctrl Pts',(-0.261469242000055,15.2,-10.854271772));
#297938=CARTESIAN_POINT('Ctrl Pts',(-0.261469242000055,11.6,-10.854271772));
#297939=CARTESIAN_POINT('Ctrl Pts',(-0.260556733000056,15.2,-10.851647578));
#297940=CARTESIAN_POINT('Ctrl Pts',(-0.260556733000056,11.6,-10.851647578));
#297941=CARTESIAN_POINT('Ctrl Pts',(-0.259648297000057,15.2,-10.84902803));
#297942=CARTESIAN_POINT('Ctrl Pts',(-0.259648297000057,11.6,-10.84902803));
#297943=CARTESIAN_POINT('Ctrl Pts',(-0.258743931000056,15.2,-10.846413139));
#297944=CARTESIAN_POINT('Ctrl Pts',(-0.258743931000056,11.6,-10.846413139));
#297945=CARTESIAN_POINT('Ctrl Pts',(-0.257843631000056,15.2,-10.843802918));
#297946=CARTESIAN_POINT('Ctrl Pts',(-0.257843631000056,11.6,-10.843802918));
#297947=CARTESIAN_POINT('Ctrl Pts',(-0.256947390000055,15.2,-10.84119738));
#297948=CARTESIAN_POINT('Ctrl Pts',(-0.256947390000055,11.6,-10.84119738));
#297949=CARTESIAN_POINT('Ctrl Pts',(-0.256055206000055,15.2,-10.838596538));
#297950=CARTESIAN_POINT('Ctrl Pts',(-0.256055206000055,11.6,-10.838596538));
#297951=CARTESIAN_POINT('Ctrl Pts',(-0.255167073000055,15.2,-10.836000406));
#297952=CARTESIAN_POINT('Ctrl Pts',(-0.255167073000055,11.6,-10.836000406));
#297953=CARTESIAN_POINT('Ctrl Pts',(-0.254282988000056,15.2,-10.833408995));
#297954=CARTESIAN_POINT('Ctrl Pts',(-0.254282988000056,11.6,-10.833408995));
#297955=CARTESIAN_POINT('Ctrl Pts',(-0.253402945000056,15.2,-10.830822318));
#297956=CARTESIAN_POINT('Ctrl Pts',(-0.253402945000056,11.6,-10.830822318));
#297957=CARTESIAN_POINT('Ctrl Pts',(-0.252526940000056,15.2,-10.828240388));
#297958=CARTESIAN_POINT('Ctrl Pts',(-0.252526940000056,11.6,-10.828240388));
#297959=CARTESIAN_POINT('Ctrl Pts',(-0.251654969000056,15.2,-10.825663219));
#297960=CARTESIAN_POINT('Ctrl Pts',(-0.251654969000056,11.6,-10.825663219));
#297961=CARTESIAN_POINT('Ctrl Pts',(-0.250787027000056,15.2,-10.823090823));
#297962=CARTESIAN_POINT('Ctrl Pts',(-0.250787027000056,11.6,-10.823090823));
#297963=CARTESIAN_POINT('Ctrl Pts',(-0.249923109000055,15.2,-10.820523213));
#297964=CARTESIAN_POINT('Ctrl Pts',(-0.249923109000055,11.6,-10.820523213));
#297965=CARTESIAN_POINT('Ctrl Pts',(-0.249063210000056,15.2,-10.817960403));
#297966=CARTESIAN_POINT('Ctrl Pts',(-0.249063210000056,11.6,-10.817960403));
#297967=CARTESIAN_POINT('Ctrl Pts',(-0.248207327000056,15.2,-10.815402404));
#297968=CARTESIAN_POINT('Ctrl Pts',(-0.248207327000056,11.6,-10.815402404));
#297969=CARTESIAN_POINT('Ctrl Pts',(-0.247355454000056,15.2,-10.812849232));
#297970=CARTESIAN_POINT('Ctrl Pts',(-0.247355454000056,11.6,-10.812849232));
#297971=CARTESIAN_POINT('Ctrl Pts',(-0.246507587000057,15.2,-10.810300898));
#297972=CARTESIAN_POINT('Ctrl Pts',(-0.246507587000057,11.6,-10.810300898));
#297973=CARTESIAN_POINT('Ctrl Pts',(-0.245663721000057,15.2,-10.807757416));
#297974=CARTESIAN_POINT('Ctrl Pts',(-0.245663721000057,11.6,-10.807757416));
#297975=CARTESIAN_POINT('Ctrl Pts',(-0.244823851000057,15.2,-10.805218799));
#297976=CARTESIAN_POINT('Ctrl Pts',(-0.244823851000057,11.6,-10.805218799));
#297977=CARTESIAN_POINT('Ctrl Pts',(-0.243987973000056,15.2,-10.80268506));
#297978=CARTESIAN_POINT('Ctrl Pts',(-0.243987973000056,11.6,-10.80268506));
#297979=CARTESIAN_POINT('Ctrl Pts',(-0.243156080000055,15.2,-10.800156212));
#297980=CARTESIAN_POINT('Ctrl Pts',(-0.243156080000055,11.6,-10.800156212));
#297981=CARTESIAN_POINT('Ctrl Pts',(-0.242328171000056,15.2,-10.797632269));
#297982=CARTESIAN_POINT('Ctrl Pts',(-0.242328171000056,11.6,-10.797632269));
#297983=CARTESIAN_POINT('Ctrl Pts',(-0.241504238000055,15.2,-10.795113244));
#297984=CARTESIAN_POINT('Ctrl Pts',(-0.241504238000055,11.6,-10.795113244));
#297985=CARTESIAN_POINT('Ctrl Pts',(-0.240684278000056,15.2,-10.79259915));
#297986=CARTESIAN_POINT('Ctrl Pts',(-0.240684278000056,11.6,-10.79259915));
#297987=CARTESIAN_POINT('Ctrl Pts',(-0.239868284000057,15.2,-10.790090001));
#297988=CARTESIAN_POINT('Ctrl Pts',(-0.239868284000057,11.6,-10.790090001));
#297989=CARTESIAN_POINT('Ctrl Pts',(-0.239056253000056,15.2,-10.78758581));
#297990=CARTESIAN_POINT('Ctrl Pts',(-0.239056253000056,11.6,-10.78758581));
#297991=CARTESIAN_POINT('Ctrl Pts',(-0.238248181000056,15.2,-10.78508659));
#297992=CARTESIAN_POINT('Ctrl Pts',(-0.238248181000056,11.6,-10.78508659));
#297993=CARTESIAN_POINT('Ctrl Pts',(-0.237444060000056,15.2,-10.782592355));
#297994=CARTESIAN_POINT('Ctrl Pts',(-0.237444060000056,11.6,-10.782592355));
#297995=CARTESIAN_POINT('Ctrl Pts',(-0.236643888000057,15.2,-10.780103119));
#297996=CARTESIAN_POINT('Ctrl Pts',(-0.236643888000057,11.6,-10.780103119));
#297997=CARTESIAN_POINT('Ctrl Pts',(-0.235847657000056,15.2,-10.777618895));
#297998=CARTESIAN_POINT('Ctrl Pts',(-0.235847657000056,11.6,-10.777618895));
#297999=CARTESIAN_POINT('Ctrl Pts',(-0.235055365000055,15.2,-10.775139696));
#298000=CARTESIAN_POINT('Ctrl Pts',(-0.235055365000055,11.6,-10.775139696));
#298001=CARTESIAN_POINT('Ctrl Pts',(-0.234267006000056,15.2,-10.772665536));
#298002=CARTESIAN_POINT('Ctrl Pts',(-0.234267006000056,11.6,-10.772665536));
#298003=CARTESIAN_POINT('Ctrl Pts',(-0.233482574000057,15.2,-10.770196429));
#298004=CARTESIAN_POINT('Ctrl Pts',(-0.233482574000057,11.6,-10.770196429));
#298005=CARTESIAN_POINT('Ctrl Pts',(-0.232702064000057,15.2,-10.767732388));
#298006=CARTESIAN_POINT('Ctrl Pts',(-0.232702064000057,11.6,-10.767732388));
#298007=CARTESIAN_POINT('Ctrl Pts',(-0.231925472000055,15.2,-10.765273428));
#298008=CARTESIAN_POINT('Ctrl Pts',(-0.231925472000055,11.6,-10.765273428));
#298009=CARTESIAN_POINT('Ctrl Pts',(-0.231152793000057,15.2,-10.76281956));
#298010=CARTESIAN_POINT('Ctrl Pts',(-0.231152793000057,11.6,-10.76281956));
#298011=CARTESIAN_POINT('Ctrl Pts',(-0.230384020000055,15.2,-10.760370801));
#298012=CARTESIAN_POINT('Ctrl Pts',(-0.230384020000055,11.6,-10.760370801));
#298013=CARTESIAN_POINT('Ctrl Pts',(-0.229619150000057,15.2,-10.757927163));
#298014=CARTESIAN_POINT('Ctrl Pts',(-0.229619150000057,11.6,-10.757927163));
#298015=CARTESIAN_POINT('Ctrl Pts',(-0.228858176000056,15.2,-10.75548866));
#298016=CARTESIAN_POINT('Ctrl Pts',(-0.228858176000056,11.6,-10.75548866));
#298017=CARTESIAN_POINT('Ctrl Pts',(-0.228101094000056,15.2,-10.753055307));
#298018=CARTESIAN_POINT('Ctrl Pts',(-0.228101094000056,11.6,-10.753055307));
#298019=CARTESIAN_POINT('Ctrl Pts',(-0.227347899000057,15.2,-10.750627116));
#298020=CARTESIAN_POINT('Ctrl Pts',(-0.227347899000057,11.6,-10.750627116));
#298021=CARTESIAN_POINT('Ctrl Pts',(-0.226598585000056,15.2,-10.748204102));
#298022=CARTESIAN_POINT('Ctrl Pts',(-0.226598585000056,11.6,-10.748204102));
#298023=CARTESIAN_POINT('Ctrl Pts',(-0.225853145000056,15.2,-10.745786278));
#298024=CARTESIAN_POINT('Ctrl Pts',(-0.225853145000056,11.6,-10.745786278));
#298025=CARTESIAN_POINT('Ctrl Pts',(-0.225111578000057,15.2,-10.743373659));
#298026=CARTESIAN_POINT('Ctrl Pts',(-0.225111578000057,11.6,-10.743373659));
#298027=CARTESIAN_POINT('Ctrl Pts',(-0.224373875000056,15.2,-10.740966259));
#298028=CARTESIAN_POINT('Ctrl Pts',(-0.224373875000056,11.6,-10.740966259));
#298029=CARTESIAN_POINT('Ctrl Pts',(-0.223640033000055,15.2,-10.738564091));
#298030=CARTESIAN_POINT('Ctrl Pts',(-0.223640033000055,11.6,-10.738564091));
#298031=CARTESIAN_POINT('Ctrl Pts',(-0.222910044000055,15.2,-10.736167171));
#298032=CARTESIAN_POINT('Ctrl Pts',(-0.222910044000055,11.6,-10.736167171));
#298033=CARTESIAN_POINT('Ctrl Pts',(-0.222183905000056,15.2,-10.733775512));
#298034=CARTESIAN_POINT('Ctrl Pts',(-0.222183905000056,11.6,-10.733775512));
#298035=CARTESIAN_POINT('Ctrl Pts',(-0.221461609000055,15.2,-10.731389127));
#298036=CARTESIAN_POINT('Ctrl Pts',(-0.221461609000055,11.6,-10.731389127));
#298037=CARTESIAN_POINT('Ctrl Pts',(-0.220743152000056,15.2,-10.729008033));
#298038=CARTESIAN_POINT('Ctrl Pts',(-0.220743152000056,11.6,-10.729008033));
#298039=CARTESIAN_POINT('Ctrl Pts',(-0.220028527000055,15.2,-10.726632241));
#298040=CARTESIAN_POINT('Ctrl Pts',(-0.220028527000055,11.6,-10.726632241));
#298041=CARTESIAN_POINT('Ctrl Pts',(-0.219317730000055,15.2,-10.724261768));
#298042=CARTESIAN_POINT('Ctrl Pts',(-0.219317730000055,11.6,-10.724261768));
#298043=CARTESIAN_POINT('Ctrl Pts',(-0.218610753000055,15.2,-10.721896628));
#298044=CARTESIAN_POINT('Ctrl Pts',(-0.218610753000055,11.6,-10.721896628));
#298045=CARTESIAN_POINT('Ctrl Pts',(-0.217907594000056,15.2,-10.719536833));
#298046=CARTESIAN_POINT('Ctrl Pts',(-0.217907594000056,11.6,-10.719536833));
#298047=CARTESIAN_POINT('Ctrl Pts',(-0.217208245000055,15.2,-10.7171824));
#298048=CARTESIAN_POINT('Ctrl Pts',(-0.217208245000055,11.6,-10.7171824));
#298049=CARTESIAN_POINT('Ctrl Pts',(-0.216512700000056,15.2,-10.714833341));
#298050=CARTESIAN_POINT('Ctrl Pts',(-0.216512700000056,11.6,-10.714833341));
#298051=CARTESIAN_POINT('Ctrl Pts',(-0.215820955000057,15.2,-10.712489673));
#298052=CARTESIAN_POINT('Ctrl Pts',(-0.215820955000057,11.6,-10.712489673));
#298053=CARTESIAN_POINT('Ctrl Pts',(-0.215133003000056,15.2,-10.710151408));
#298054=CARTESIAN_POINT('Ctrl Pts',(-0.215133003000056,11.6,-10.710151408));
#298055=CARTESIAN_POINT('Ctrl Pts',(-0.214448839000055,15.2,-10.707818562));
#298056=CARTESIAN_POINT('Ctrl Pts',(-0.214448839000055,11.6,-10.707818562));
#298057=CARTESIAN_POINT('Ctrl Pts',(-0.213768458000055,15.2,-10.705491151));
#298058=CARTESIAN_POINT('Ctrl Pts',(-0.213768458000055,11.6,-10.705491151));
#298059=CARTESIAN_POINT('Ctrl Pts',(-0.213091853000057,15.2,-10.703169187));
#298060=CARTESIAN_POINT('Ctrl Pts',(-0.213091853000057,11.6,-10.703169187));
#298061=CARTESIAN_POINT('Ctrl Pts',(-0.212419019000055,15.2,-10.700852684));
#298062=CARTESIAN_POINT('Ctrl Pts',(-0.212419019000055,11.6,-10.700852684));
#298063=CARTESIAN_POINT('Ctrl Pts',(-0.211749948000056,15.2,-10.69854166));
#298064=CARTESIAN_POINT('Ctrl Pts',(-0.211749948000056,11.6,-10.69854166));
#298065=CARTESIAN_POINT('Ctrl Pts',(-0.211084639000055,15.2,-10.696236127));
#298066=CARTESIAN_POINT('Ctrl Pts',(-0.211084639000055,11.6,-10.696236127));
#298067=CARTESIAN_POINT('Ctrl Pts',(-0.210423081000056,15.2,-10.693936102));
#298068=CARTESIAN_POINT('Ctrl Pts',(-0.210423081000056,11.6,-10.693936102));
#298069=CARTESIAN_POINT('Ctrl Pts',(-0.209765271000055,15.2,-10.691641597));
#298070=CARTESIAN_POINT('Ctrl Pts',(-0.209765271000055,11.6,-10.691641597));
#298071=CARTESIAN_POINT('Ctrl Pts',(-0.209111203000055,15.2,-10.68935263));
#298072=CARTESIAN_POINT('Ctrl Pts',(-0.209111203000055,11.6,-10.68935263));
#298073=CARTESIAN_POINT('Ctrl Pts',(-0.208460870000057,15.2,-10.687069213));
#298074=CARTESIAN_POINT('Ctrl Pts',(-0.208460870000057,11.6,-10.687069213));
#298075=CARTESIAN_POINT('Ctrl Pts',(-0.207814267000056,15.2,-10.684791362));
#298076=CARTESIAN_POINT('Ctrl Pts',(-0.207814267000056,11.6,-10.684791362));
#298077=CARTESIAN_POINT('Ctrl Pts',(-0.207171387000056,15.2,-10.682519093));
#298078=CARTESIAN_POINT('Ctrl Pts',(-0.207171387000056,11.6,-10.682519093));
#298079=CARTESIAN_POINT('Ctrl Pts',(-0.206532225000055,15.2,-10.68025242));
#298080=CARTESIAN_POINT('Ctrl Pts',(-0.206532225000055,11.6,-10.68025242));
#298081=CARTESIAN_POINT('Ctrl Pts',(-0.205896774000056,15.2,-10.677991357));
#298082=CARTESIAN_POINT('Ctrl Pts',(-0.205896774000056,11.6,-10.677991357));
#298083=CARTESIAN_POINT('Ctrl Pts',(-0.205265029000056,15.2,-10.67573592));
#298084=CARTESIAN_POINT('Ctrl Pts',(-0.205265029000056,11.6,-10.67573592));
#298085=CARTESIAN_POINT('Ctrl Pts',(-0.204636983000055,15.2,-10.673486125));
#298086=CARTESIAN_POINT('Ctrl Pts',(-0.204636983000055,11.6,-10.673486125));
#298087=CARTESIAN_POINT('Ctrl Pts',(-0.204012631000056,15.2,-10.671241986));
#298088=CARTESIAN_POINT('Ctrl Pts',(-0.204012631000056,11.6,-10.671241986));
#298089=CARTESIAN_POINT('Ctrl Pts',(-0.203391965000056,15.2,-10.669003519));
#298090=CARTESIAN_POINT('Ctrl Pts',(-0.203391965000056,11.6,-10.669003519));
#298091=CARTESIAN_POINT('Ctrl Pts',(-0.202774980000056,15.2,-10.666770738));
#298092=CARTESIAN_POINT('Ctrl Pts',(-0.202774980000056,11.6,-10.666770738));
#298093=CARTESIAN_POINT('Ctrl Pts',(-0.202161670000055,15.2,-10.664543659));
#298094=CARTESIAN_POINT('Ctrl Pts',(-0.202161670000055,11.6,-10.664543659));
#298095=CARTESIAN_POINT('Ctrl Pts',(-0.201552028000057,15.2,-10.662322297));
#298096=CARTESIAN_POINT('Ctrl Pts',(-0.201552028000057,11.6,-10.662322297));
#298097=CARTESIAN_POINT('Ctrl Pts',(-0.200946049000056,15.2,-10.660106669));
#298098=CARTESIAN_POINT('Ctrl Pts',(-0.200946049000056,11.6,-10.660106669));
#298099=CARTESIAN_POINT('Ctrl Pts',(-0.200343725000056,15.2,-10.657896788));
#298100=CARTESIAN_POINT('Ctrl Pts',(-0.200343725000056,11.6,-10.657896788));
#298101=CARTESIAN_POINT('Ctrl Pts',(-0.199745051000055,15.2,-10.655692671));
#298102=CARTESIAN_POINT('Ctrl Pts',(-0.199745051000055,11.6,-10.655692671));
#298103=CARTESIAN_POINT('Ctrl Pts',(-0.199150020000056,15.2,-10.653494333));
#298104=CARTESIAN_POINT('Ctrl Pts',(-0.199150020000056,11.6,-10.653494333));
#298105=CARTESIAN_POINT('Ctrl Pts',(-0.198558626000055,15.2,-10.651301789));
#298106=CARTESIAN_POINT('Ctrl Pts',(-0.198558626000055,11.6,-10.651301789));
#298107=CARTESIAN_POINT('Ctrl Pts',(-0.197970862000056,15.2,-10.649115056));
#298108=CARTESIAN_POINT('Ctrl Pts',(-0.197970862000056,11.6,-10.649115056));
#298109=CARTESIAN_POINT('Ctrl Pts',(-0.197386723000056,15.2,-10.646934148));
#298110=CARTESIAN_POINT('Ctrl Pts',(-0.197386723000056,11.6,-10.646934148));
#298111=CARTESIAN_POINT('Ctrl Pts',(-0.196806201000056,15.2,-10.644759081));
#298112=CARTESIAN_POINT('Ctrl Pts',(-0.196806201000056,11.6,-10.644759081));
#298113=CARTESIAN_POINT('Ctrl Pts',(-0.196229289000056,15.2,-10.642589871));
#298114=CARTESIAN_POINT('Ctrl Pts',(-0.196229289000056,11.6,-10.642589871));
#298115=CARTESIAN_POINT('Ctrl Pts',(-0.195655982000057,15.2,-10.640426534));
#298116=CARTESIAN_POINT('Ctrl Pts',(-0.195655982000057,11.6,-10.640426534));
#298117=CARTESIAN_POINT('Ctrl Pts',(-0.195086274000056,15.2,-10.638269086));
#298118=CARTESIAN_POINT('Ctrl Pts',(-0.195086274000056,11.6,-10.638269086));
#298119=CARTESIAN_POINT('Ctrl Pts',(-0.194520156000056,15.2,-10.636117541));
#298120=CARTESIAN_POINT('Ctrl Pts',(-0.194520156000056,11.6,-10.636117541));
#298121=CARTESIAN_POINT('Ctrl Pts',(-0.193957623000056,15.2,-10.633971916));
#298122=CARTESIAN_POINT('Ctrl Pts',(-0.193957623000056,11.6,-10.633971916));
#298123=CARTESIAN_POINT('Ctrl Pts',(-0.193398667000055,15.2,-10.631832228));
#298124=CARTESIAN_POINT('Ctrl Pts',(-0.193398667000055,11.6,-10.631832228));
#298125=CARTESIAN_POINT('Ctrl Pts',(-0.192843283000055,15.2,-10.629698492));
#298126=CARTESIAN_POINT('Ctrl Pts',(-0.192843283000055,11.6,-10.629698492));
#298127=CARTESIAN_POINT('Ctrl Pts',(-0.192291464000055,15.2,-10.627570723));
#298128=CARTESIAN_POINT('Ctrl Pts',(-0.192291464000055,11.6,-10.627570723));
#298129=CARTESIAN_POINT('Ctrl Pts',(-0.191743203000057,15.2,-10.62544894));
#298130=CARTESIAN_POINT('Ctrl Pts',(-0.191743203000057,11.6,-10.62544894));
#298131=CARTESIAN_POINT('Ctrl Pts',(-0.191198493000057,15.2,-10.623333156));
#298132=CARTESIAN_POINT('Ctrl Pts',(-0.191198493000057,11.6,-10.623333156));
#298133=CARTESIAN_POINT('Ctrl Pts',(-0.190657326000055,15.2,-10.621223388));
#298134=CARTESIAN_POINT('Ctrl Pts',(-0.190657326000055,11.6,-10.621223388));
#298135=CARTESIAN_POINT('Ctrl Pts',(-0.190119697000056,15.2,-10.619119652));
#298136=CARTESIAN_POINT('Ctrl Pts',(-0.190119697000056,11.6,-10.619119652));
#298137=CARTESIAN_POINT('Ctrl Pts',(-0.189585599000056,15.2,-10.617021965));
#298138=CARTESIAN_POINT('Ctrl Pts',(-0.189585599000056,11.6,-10.617021965));
#298139=CARTESIAN_POINT('Ctrl Pts',(-0.189055024000057,15.2,-10.614930343));
#298140=CARTESIAN_POINT('Ctrl Pts',(-0.189055024000057,11.6,-10.614930343));
#298141=CARTESIAN_POINT('Ctrl Pts',(-0.188527965000055,15.2,-10.612844802));
#298142=CARTESIAN_POINT('Ctrl Pts',(-0.188527965000055,11.6,-10.612844802));
#298143=CARTESIAN_POINT('Ctrl Pts',(-0.188004417000055,15.2,-10.610765359));
#298144=CARTESIAN_POINT('Ctrl Pts',(-0.188004417000055,11.6,-10.610765359));
#298145=CARTESIAN_POINT('Ctrl Pts',(-0.187484370000056,15.2,-10.60869203));
#298146=CARTESIAN_POINT('Ctrl Pts',(-0.187484370000056,11.6,-10.60869203));
#298147=CARTESIAN_POINT('Ctrl Pts',(-0.186967820000056,15.2,-10.606624832));
#298148=CARTESIAN_POINT('Ctrl Pts',(-0.186967820000056,11.6,-10.606624832));
#298149=CARTESIAN_POINT('Ctrl Pts',(-0.186454758000056,15.2,-10.60456378));
#298150=CARTESIAN_POINT('Ctrl Pts',(-0.186454758000056,11.6,-10.60456378));
#298151=CARTESIAN_POINT('Ctrl Pts',(-0.185945177000055,15.2,-10.602508892));
#298152=CARTESIAN_POINT('Ctrl Pts',(-0.185945177000055,11.6,-10.602508892));
#298153=CARTESIAN_POINT('Ctrl Pts',(-0.185439071000056,15.2,-10.600460183));
#298154=CARTESIAN_POINT('Ctrl Pts',(-0.185439071000056,11.6,-10.600460183));
#298155=CARTESIAN_POINT('Ctrl Pts',(-0.184936432000056,15.2,-10.598417672));
#298156=CARTESIAN_POINT('Ctrl Pts',(-0.184936432000056,11.6,-10.598417672));
#298157=CARTESIAN_POINT('Ctrl Pts',(-0.184437253000055,15.2,-10.596381375));
#298158=CARTESIAN_POINT('Ctrl Pts',(-0.184437253000055,11.6,-10.596381375));
#298159=CARTESIAN_POINT('Ctrl Pts',(-0.183941526000057,15.2,-10.594351307));
#298160=CARTESIAN_POINT('Ctrl Pts',(-0.183941526000057,11.6,-10.594351307));
#298161=CARTESIAN_POINT('Ctrl Pts',(-0.183449244000055,15.2,-10.592327487));
#298162=CARTESIAN_POINT('Ctrl Pts',(-0.183449244000055,11.6,-10.592327487));
#298163=CARTESIAN_POINT('Ctrl Pts',(-0.182960401000055,15.2,-10.59030993));
#298164=CARTESIAN_POINT('Ctrl Pts',(-0.182960401000055,11.6,-10.59030993));
#298165=CARTESIAN_POINT('Ctrl Pts',(-0.182474988000055,15.2,-10.588298654));
#298166=CARTESIAN_POINT('Ctrl Pts',(-0.182474988000055,11.6,-10.588298654));
#298167=CARTESIAN_POINT('Ctrl Pts',(-0.181992998000055,15.2,-10.586293676));
#298168=CARTESIAN_POINT('Ctrl Pts',(-0.181992998000055,11.6,-10.586293676));
#298169=CARTESIAN_POINT('Ctrl Pts',(-0.181514425000057,15.2,-10.584295012));
#298170=CARTESIAN_POINT('Ctrl Pts',(-0.181514425000057,11.6,-10.584295012));
#298171=CARTESIAN_POINT('Ctrl Pts',(-0.181039260000055,15.2,-10.582302681));
#298172=CARTESIAN_POINT('Ctrl Pts',(-0.181039260000055,11.6,-10.582302681));
#298173=CARTESIAN_POINT('Ctrl Pts',(-0.180567496000055,15.2,-10.580316698));
#298174=CARTESIAN_POINT('Ctrl Pts',(-0.180567496000055,11.6,-10.580316698));
#298175=CARTESIAN_POINT('Ctrl Pts',(-0.180099125000056,15.2,-10.578337081));
#298176=CARTESIAN_POINT('Ctrl Pts',(-0.180099125000056,11.6,-10.578337081));
#298177=CARTESIAN_POINT('Ctrl Pts',(-0.179634139000056,15.2,-10.576363848));
#298178=CARTESIAN_POINT('Ctrl Pts',(-0.179634139000056,11.6,-10.576363848));
#298179=CARTESIAN_POINT('Ctrl Pts',(-0.179172532000056,15.2,-10.574397014));
#298180=CARTESIAN_POINT('Ctrl Pts',(-0.179172532000056,11.6,-10.574397014));
#298181=CARTESIAN_POINT('Ctrl Pts',(-0.178714296000055,15.2,-10.572436599));
#298182=CARTESIAN_POINT('Ctrl Pts',(-0.178714296000055,11.6,-10.572436599));
#298183=CARTESIAN_POINT('Ctrl Pts',(-0.178259423000057,15.2,-10.570482619));
#298184=CARTESIAN_POINT('Ctrl Pts',(-0.178259423000057,11.6,-10.570482619));
#298185=CARTESIAN_POINT('Ctrl Pts',(-0.177807905000057,15.2,-10.568535092));
#298186=CARTESIAN_POINT('Ctrl Pts',(-0.177807905000057,11.6,-10.568535092));
#298187=CARTESIAN_POINT('Ctrl Pts',(-0.177359734000057,15.2,-10.566594035));
#298188=CARTESIAN_POINT('Ctrl Pts',(-0.177359734000057,11.6,-10.566594035));
#298189=CARTESIAN_POINT('Ctrl Pts',(-0.176914903000055,15.2,-10.564659465));
#298190=CARTESIAN_POINT('Ctrl Pts',(-0.176914903000055,11.6,-10.564659465));
#298191=CARTESIAN_POINT('Ctrl Pts',(-0.176473403000056,15.2,-10.562731399));
#298192=CARTESIAN_POINT('Ctrl Pts',(-0.176473403000056,11.6,-10.562731399));
#298193=CARTESIAN_POINT('Ctrl Pts',(-0.176035228000057,15.2,-10.560809857));
#298194=CARTESIAN_POINT('Ctrl Pts',(-0.176035228000057,11.6,-10.560809857));
#298195=CARTESIAN_POINT('Ctrl Pts',(-0.175600369000056,15.2,-10.558894856));
#298196=CARTESIAN_POINT('Ctrl Pts',(-0.175600369000056,11.6,-10.558894856));
#298197=CARTESIAN_POINT('Ctrl Pts',(-0.175168818000057,15.2,-10.556986413));
#298198=CARTESIAN_POINT('Ctrl Pts',(-0.175168818000057,11.6,-10.556986413));
#298199=CARTESIAN_POINT('Ctrl Pts',(-0.174740568000056,15.2,-10.555084546));
#298200=CARTESIAN_POINT('Ctrl Pts',(-0.174740568000056,11.6,-10.555084546));
#298201=CARTESIAN_POINT('Ctrl Pts',(-0.174315609000055,15.2,-10.553189273));
#298202=CARTESIAN_POINT('Ctrl Pts',(-0.174315609000055,11.6,-10.553189273));
#298203=CARTESIAN_POINT('Ctrl Pts',(-0.173893934000056,15.2,-10.551300611));
#298204=CARTESIAN_POINT('Ctrl Pts',(-0.173893934000056,11.6,-10.551300611));
#298205=CARTESIAN_POINT('Ctrl Pts',(-0.173475537000056,15.2,-10.549418579));
#298206=CARTESIAN_POINT('Ctrl Pts',(-0.173475537000056,11.6,-10.549418579));
#298207=CARTESIAN_POINT('Ctrl Pts',(-0.173060406000056,15.2,-10.547543195));
#298208=CARTESIAN_POINT('Ctrl Pts',(-0.173060406000056,11.6,-10.547543195));
#298209=CARTESIAN_POINT('Ctrl Pts',(-0.172648536000055,15.2,-10.545674477));
#298210=CARTESIAN_POINT('Ctrl Pts',(-0.172648536000055,11.6,-10.545674477));
#298211=CARTESIAN_POINT('Ctrl Pts',(-0.172239916000055,15.2,-10.543812443));
#298212=CARTESIAN_POINT('Ctrl Pts',(-0.172239916000055,11.6,-10.543812443));
#298213=CARTESIAN_POINT('Ctrl Pts',(-0.171834541000055,15.2,-10.541957111));
#298214=CARTESIAN_POINT('Ctrl Pts',(-0.171834541000055,11.6,-10.541957111));
#298215=CARTESIAN_POINT('Ctrl Pts',(-0.171432400000056,15.2,-10.5401085));
#298216=CARTESIAN_POINT('Ctrl Pts',(-0.171432400000056,11.6,-10.5401085));
#298217=CARTESIAN_POINT('Ctrl Pts',(-0.171033486000055,15.2,-10.538266627));
#298218=CARTESIAN_POINT('Ctrl Pts',(-0.171033486000055,11.6,-10.538266627));
#298219=CARTESIAN_POINT('Ctrl Pts',(-0.170637791000056,15.2,-10.536431511));
#298220=CARTESIAN_POINT('Ctrl Pts',(-0.170637791000056,11.6,-10.536431511));
#298221=CARTESIAN_POINT('Ctrl Pts',(-0.170245305000056,15.2,-10.534603171));
#298222=CARTESIAN_POINT('Ctrl Pts',(-0.170245305000056,11.6,-10.534603171));
#298223=CARTESIAN_POINT('Ctrl Pts',(-0.169856021000055,15.2,-10.532781626));
#298224=CARTESIAN_POINT('Ctrl Pts',(-0.169856021000055,11.6,-10.532781626));
#298225=CARTESIAN_POINT('Ctrl Pts',(-0.169469930000057,15.2,-10.530966892));
#298226=CARTESIAN_POINT('Ctrl Pts',(-0.169469930000057,11.6,-10.530966892));
#298227=CARTESIAN_POINT('Ctrl Pts',(-0.169087023000056,15.2,-10.529158991));
#298228=CARTESIAN_POINT('Ctrl Pts',(-0.169087023000056,11.6,-10.529158991));
#298229=CARTESIAN_POINT('Ctrl Pts',(-0.168707293000055,15.2,-10.527357938));
#298230=CARTESIAN_POINT('Ctrl Pts',(-0.168707293000055,11.6,-10.527357938));
#298231=CARTESIAN_POINT('Ctrl Pts',(-0.168330729000056,15.2,-10.525563754));
#298232=CARTESIAN_POINT('Ctrl Pts',(-0.168330729000056,11.6,-10.525563754));
#298233=CARTESIAN_POINT('Ctrl Pts',(-0.167957324000056,15.2,-10.523776458));
#298234=CARTESIAN_POINT('Ctrl Pts',(-0.167957324000056,11.6,-10.523776458));
#298235=CARTESIAN_POINT('Ctrl Pts',(-0.167587069000056,15.2,-10.521996069));
#298236=CARTESIAN_POINT('Ctrl Pts',(-0.167587069000056,11.6,-10.521996069));
#298237=CARTESIAN_POINT('Ctrl Pts',(-0.167219956000055,15.2,-10.520222604));
#298238=CARTESIAN_POINT('Ctrl Pts',(-0.167219956000055,11.6,-10.520222604));
#298239=CARTESIAN_POINT('Ctrl Pts',(-0.166855974000055,15.2,-10.518456084));
#298240=CARTESIAN_POINT('Ctrl Pts',(-0.166855974000055,11.6,-10.518456084));
#298241=CARTESIAN_POINT('Ctrl Pts',(-0.166495117000055,15.2,-10.516696527));
#298242=CARTESIAN_POINT('Ctrl Pts',(-0.166495117000055,11.6,-10.516696527));
#298243=CARTESIAN_POINT('Ctrl Pts',(-0.166137374000056,15.2,-10.514943952));
#298244=CARTESIAN_POINT('Ctrl Pts',(-0.166137374000056,11.6,-10.514943952));
#298245=CARTESIAN_POINT('Ctrl Pts',(-0.165782737000055,15.2,-10.513198378));
#298246=CARTESIAN_POINT('Ctrl Pts',(-0.165782737000055,11.6,-10.513198378));
#298247=CARTESIAN_POINT('Ctrl Pts',(-0.165431198000056,15.2,-10.511459826));
#298248=CARTESIAN_POINT('Ctrl Pts',(-0.165431198000056,11.6,-10.511459826));
#298249=CARTESIAN_POINT('Ctrl Pts',(-0.165082744000056,15.2,-10.509728314));
#298250=CARTESIAN_POINT('Ctrl Pts',(-0.165082744000056,11.6,-10.509728314));
#298251=CARTESIAN_POINT('Ctrl Pts',(-0.164737371000055,15.2,-10.508003862));
#298252=CARTESIAN_POINT('Ctrl Pts',(-0.164737371000055,11.6,-10.508003862));
#298253=CARTESIAN_POINT('Ctrl Pts',(-0.164395067000056,15.2,-10.506286487));
#298254=CARTESIAN_POINT('Ctrl Pts',(-0.164395067000056,11.6,-10.506286487));
#298255=CARTESIAN_POINT('Ctrl Pts',(-0.164055824000057,15.2,-10.504576212));
#298256=CARTESIAN_POINT('Ctrl Pts',(-0.164055824000057,11.6,-10.504576212));
#298257=CARTESIAN_POINT('Ctrl Pts',(-0.163719632000056,15.2,-10.502873055));
#298258=CARTESIAN_POINT('Ctrl Pts',(-0.163719632000056,11.6,-10.502873055));
#298259=CARTESIAN_POINT('Ctrl Pts',(-0.163386483000056,15.2,-10.501177036));
#298260=CARTESIAN_POINT('Ctrl Pts',(-0.163386483000056,11.6,-10.501177036));
#298261=CARTESIAN_POINT('Ctrl Pts',(-0.163056366000056,15.2,-10.499488173));
#298262=CARTESIAN_POINT('Ctrl Pts',(-0.163056366000056,11.6,-10.499488173));
#298263=CARTESIAN_POINT('Ctrl Pts',(-0.162729274000055,15.2,-10.497806488));
#298264=CARTESIAN_POINT('Ctrl Pts',(-0.162729274000055,11.6,-10.497806488));
#298265=CARTESIAN_POINT('Ctrl Pts',(-0.162405194000056,15.2,-10.496131999));
#298266=CARTESIAN_POINT('Ctrl Pts',(-0.162405194000056,11.6,-10.496131999));
#298267=CARTESIAN_POINT('Ctrl Pts',(-0.162084120000056,15.2,-10.494464728));
#298268=CARTESIAN_POINT('Ctrl Pts',(-0.162084120000056,11.6,-10.494464728));
#298269=CARTESIAN_POINT('Ctrl Pts',(-0.161766042000057,15.2,-10.492804693));
#298270=CARTESIAN_POINT('Ctrl Pts',(-0.161766042000057,11.6,-10.492804693));
#298271=CARTESIAN_POINT('Ctrl Pts',(-0.161450949000056,15.2,-10.491151915));
#298272=CARTESIAN_POINT('Ctrl Pts',(-0.161450949000056,11.6,-10.491151915));
#298273=CARTESIAN_POINT('Ctrl Pts',(-0.161138833000055,15.2,-10.489506414));
#298274=CARTESIAN_POINT('Ctrl Pts',(-0.161138833000055,11.6,-10.489506414));
#298275=CARTESIAN_POINT('Ctrl Pts',(-0.160829682000055,15.2,-10.487868211));
#298276=CARTESIAN_POINT('Ctrl Pts',(-0.160829682000055,11.6,-10.487868211));
#298277=CARTESIAN_POINT('Ctrl Pts',(-0.160523489000056,15.2,-10.486237324));
#298278=CARTESIAN_POINT('Ctrl Pts',(-0.160523489000056,11.6,-10.486237324));
#298279=CARTESIAN_POINT('Ctrl Pts',(-0.160220245000057,15.2,-10.484613776));
#298280=CARTESIAN_POINT('Ctrl Pts',(-0.160220245000057,11.6,-10.484613776));
#298281=CARTESIAN_POINT('Ctrl Pts',(-0.159919937000056,15.2,-10.482997586));
#298282=CARTESIAN_POINT('Ctrl Pts',(-0.159919937000056,11.6,-10.482997586));
#298283=CARTESIAN_POINT('Ctrl Pts',(-0.159622556000055,15.2,-10.481388775));
#298284=CARTESIAN_POINT('Ctrl Pts',(-0.159622556000055,11.6,-10.481388775));
#298285=CARTESIAN_POINT('Ctrl Pts',(-0.159328094000056,15.2,-10.479787363));
#298286=CARTESIAN_POINT('Ctrl Pts',(-0.159328094000056,11.6,-10.479787363));
#298287=CARTESIAN_POINT('Ctrl Pts',(-0.159036540000056,15.2,-10.478193371));
#298288=CARTESIAN_POINT('Ctrl Pts',(-0.159036540000056,11.6,-10.478193371));
#298289=CARTESIAN_POINT('Ctrl Pts',(-0.158747884000056,15.2,-10.476606819));
#298290=CARTESIAN_POINT('Ctrl Pts',(-0.158747884000056,11.6,-10.476606819));
#298291=CARTESIAN_POINT('Ctrl Pts',(-0.158462117000056,15.2,-10.475027729));
#298292=CARTESIAN_POINT('Ctrl Pts',(-0.158462117000056,11.6,-10.475027729));
#298293=CARTESIAN_POINT('Ctrl Pts',(-0.158179227000056,15.2,-10.473456121));
#298294=CARTESIAN_POINT('Ctrl Pts',(-0.158179227000056,11.6,-10.473456121));
#298295=CARTESIAN_POINT('Ctrl Pts',(-0.157899205000056,15.2,-10.471892016));
#298296=CARTESIAN_POINT('Ctrl Pts',(-0.157899205000056,11.6,-10.471892016));
#298297=CARTESIAN_POINT('Ctrl Pts',(-0.157622041000056,15.2,-10.470335435));
#298298=CARTESIAN_POINT('Ctrl Pts',(-0.157622041000056,11.6,-10.470335435));
#298299=CARTESIAN_POINT('Ctrl Pts',(-0.157347725000055,15.2,-10.4687864));
#298300=CARTESIAN_POINT('Ctrl Pts',(-0.157347725000055,11.6,-10.4687864));
#298301=CARTESIAN_POINT('Ctrl Pts',(-0.157076245000055,15.2,-10.467244931));
#298302=CARTESIAN_POINT('Ctrl Pts',(-0.157076245000055,11.6,-10.467244931));
#298303=CARTESIAN_POINT('Ctrl Pts',(-0.156807594000057,15.2,-10.46571105));
#298304=CARTESIAN_POINT('Ctrl Pts',(-0.156807594000057,11.6,-10.46571105));
#298305=CARTESIAN_POINT('Ctrl Pts',(-0.156541758000056,15.2,-10.464184778));
#298306=CARTESIAN_POINT('Ctrl Pts',(-0.156541758000056,11.6,-10.464184778));
#298307=CARTESIAN_POINT('Ctrl Pts',(-0.156278730000056,15.2,-10.462666135));
#298308=CARTESIAN_POINT('Ctrl Pts',(-0.156278730000056,11.6,-10.462666135));
#298309=CARTESIAN_POINT('Ctrl Pts',(-0.156018496000057,15.2,-10.461155145));
#298310=CARTESIAN_POINT('Ctrl Pts',(-0.156018496000057,11.6,-10.461155145));
#298311=CARTESIAN_POINT('Ctrl Pts',(-0.155761048000055,15.2,-10.459651829));
#298312=CARTESIAN_POINT('Ctrl Pts',(-0.155761048000055,11.6,-10.459651829));
#298313=CARTESIAN_POINT('Ctrl Pts',(-0.155506375000056,15.2,-10.458156207));
#298314=CARTESIAN_POINT('Ctrl Pts',(-0.155506375000056,11.6,-10.458156207));
#298315=CARTESIAN_POINT('Ctrl Pts',(-0.155254466000055,15.2,-10.456668302));
#298316=CARTESIAN_POINT('Ctrl Pts',(-0.155254466000055,11.6,-10.456668302));
#298317=CARTESIAN_POINT('Ctrl Pts',(-0.155005310000057,15.2,-10.455188136));
#298318=CARTESIAN_POINT('Ctrl Pts',(-0.155005310000057,11.6,-10.455188136));
#298319=CARTESIAN_POINT('Ctrl Pts',(-0.154758897000056,15.2,-10.45371573));
#298320=CARTESIAN_POINT('Ctrl Pts',(-0.154758897000056,11.6,-10.45371573));
#298321=CARTESIAN_POINT('Ctrl Pts',(-0.154515216000056,15.2,-10.452251106));
#298322=CARTESIAN_POINT('Ctrl Pts',(-0.154515216000056,11.6,-10.452251106));
#298323=CARTESIAN_POINT('Ctrl Pts',(-0.154274256000055,15.2,-10.450794288));
#298324=CARTESIAN_POINT('Ctrl Pts',(-0.154274256000055,11.6,-10.450794288));
#298325=CARTESIAN_POINT('Ctrl Pts',(-0.154036006000055,15.2,-10.449345296));
#298326=CARTESIAN_POINT('Ctrl Pts',(-0.154036006000055,11.6,-10.449345296));
#298327=CARTESIAN_POINT('Ctrl Pts',(-0.153800456000056,15.2,-10.447904152));
#298328=CARTESIAN_POINT('Ctrl Pts',(-0.153800456000056,11.6,-10.447904152));
#298329=CARTESIAN_POINT('Ctrl Pts',(-0.153567593000057,15.2,-10.446470879));
#298330=CARTESIAN_POINT('Ctrl Pts',(-0.153567593000057,11.6,-10.446470879));
#298331=CARTESIAN_POINT('Ctrl Pts',(-0.153337407000055,15.2,-10.4450455));
#298332=CARTESIAN_POINT('Ctrl Pts',(-0.153337407000055,11.6,-10.4450455));
#298333=CARTESIAN_POINT('Ctrl Pts',(-0.153109888000056,15.2,-10.443628038));
#298334=CARTESIAN_POINT('Ctrl Pts',(-0.153109888000056,11.6,-10.443628038));
#298335=CARTESIAN_POINT('Ctrl Pts',(-0.152885022000057,15.2,-10.442218514));
#298336=CARTESIAN_POINT('Ctrl Pts',(-0.152885022000057,11.6,-10.442218514));
#298337=CARTESIAN_POINT('Ctrl Pts',(-0.152662802000056,15.2,-10.440816951));
#298338=CARTESIAN_POINT('Ctrl Pts',(-0.152662802000056,11.6,-10.440816951));
#298339=CARTESIAN_POINT('Ctrl Pts',(-0.152443212000056,15.2,-10.439423372));
#298340=CARTESIAN_POINT('Ctrl Pts',(-0.152443212000056,11.6,-10.439423372));
#298341=CARTESIAN_POINT('Ctrl Pts',(-0.152226243000056,15.2,-10.4380378));
#298342=CARTESIAN_POINT('Ctrl Pts',(-0.152226243000056,11.6,-10.4380378));
#298343=CARTESIAN_POINT('Ctrl Pts',(-0.152011884000055,15.2,-10.436660258));
#298344=CARTESIAN_POINT('Ctrl Pts',(-0.152011884000055,11.6,-10.436660258));
#298345=CARTESIAN_POINT('Ctrl Pts',(-0.151800122000055,15.2,-10.435290769));
#298346=CARTESIAN_POINT('Ctrl Pts',(-0.151800122000055,11.6,-10.435290769));
#298347=CARTESIAN_POINT('Ctrl Pts',(-0.151590948000055,15.2,-10.433929354));
#298348=CARTESIAN_POINT('Ctrl Pts',(-0.151590948000055,11.6,-10.433929354));
#298349=CARTESIAN_POINT('Ctrl Pts',(-0.151384347000055,15.2,-10.43257604));
#298350=CARTESIAN_POINT('Ctrl Pts',(-0.151384347000055,11.6,-10.43257604));
#298351=CARTESIAN_POINT('Ctrl Pts',(-0.151180310000055,15.2,-10.431230848));
#298352=CARTESIAN_POINT('Ctrl Pts',(-0.151180310000055,11.6,-10.431230848));
#298353=CARTESIAN_POINT('Ctrl Pts',(-0.150978823000055,15.2,-10.429893802));
#298354=CARTESIAN_POINT('Ctrl Pts',(-0.150978823000055,11.6,-10.429893802));
#298355=CARTESIAN_POINT('Ctrl Pts',(-0.150779876000057,15.2,-10.428564925));
#298356=CARTESIAN_POINT('Ctrl Pts',(-0.150779876000057,11.6,-10.428564925));
#298357=CARTESIAN_POINT('Ctrl Pts',(-0.150583457000056,15.2,-10.427244241));
#298358=CARTESIAN_POINT('Ctrl Pts',(-0.150583457000056,11.6,-10.427244241));
#298359=CARTESIAN_POINT('Ctrl Pts',(-0.150389553000055,15.2,-10.425931773));
#298360=CARTESIAN_POINT('Ctrl Pts',(-0.150389553000055,11.6,-10.425931773));
#298361=CARTESIAN_POINT('Ctrl Pts',(-0.150198154000056,15.2,-10.424627545));
#298362=CARTESIAN_POINT('Ctrl Pts',(-0.150198154000056,11.6,-10.424627545));
#298363=CARTESIAN_POINT('Ctrl Pts',(-0.150009246000057,15.2,-10.423331583));
#298364=CARTESIAN_POINT('Ctrl Pts',(-0.150009246000057,11.6,-10.423331583));
#298365=CARTESIAN_POINT('Ctrl Pts',(-0.149822818000055,15.2,-10.422043907));
#298366=CARTESIAN_POINT('Ctrl Pts',(-0.149822818000055,11.6,-10.422043907));
#298367=CARTESIAN_POINT('Ctrl Pts',(-0.149638856000056,15.2,-10.420764545));
#298368=CARTESIAN_POINT('Ctrl Pts',(-0.149638856000056,11.6,-10.420764545));
#298369=CARTESIAN_POINT('Ctrl Pts',(-0.149457350000055,15.2,-10.419493518));
#298370=CARTESIAN_POINT('Ctrl Pts',(-0.149457350000055,11.6,-10.419493518));
#298371=CARTESIAN_POINT('Ctrl Pts',(-0.149278286000056,15.2,-10.418230852));
#298372=CARTESIAN_POINT('Ctrl Pts',(-0.149278286000056,11.6,-10.418230852));
#298373=CARTESIAN_POINT('Ctrl Pts',(-0.149101652000055,15.2,-10.416976571));
#298374=CARTESIAN_POINT('Ctrl Pts',(-0.149101652000055,11.6,-10.416976571));
#298375=CARTESIAN_POINT('Ctrl Pts',(-0.148927437000056,15.2,-10.4157307));
#298376=CARTESIAN_POINT('Ctrl Pts',(-0.148927437000056,11.6,-10.4157307));
#298377=CARTESIAN_POINT('Ctrl Pts',(-0.148755627000057,15.2,-10.414493262));
#298378=CARTESIAN_POINT('Ctrl Pts',(-0.148755627000057,11.6,-10.414493262));
#298379=CARTESIAN_POINT('Ctrl Pts',(-0.148586210000056,15.2,-10.413264283));
#298380=CARTESIAN_POINT('Ctrl Pts',(-0.148586210000056,11.6,-10.413264283));
#298381=CARTESIAN_POINT('Ctrl Pts',(-0.148419173000055,15.2,-10.412043788));
#298382=CARTESIAN_POINT('Ctrl Pts',(-0.148419173000055,11.6,-10.412043788));
#298383=CARTESIAN_POINT('Ctrl Pts',(-0.148254502000055,15.2,-10.410831802));
#298384=CARTESIAN_POINT('Ctrl Pts',(-0.148254502000055,11.6,-10.410831802));
#298385=CARTESIAN_POINT('Ctrl Pts',(-0.148092187000056,15.2,-10.409628348));
#298386=CARTESIAN_POINT('Ctrl Pts',(-0.148092187000056,11.6,-10.409628348));
#298387=CARTESIAN_POINT('Ctrl Pts',(-0.147932214000056,15.2,-10.408433454));
#298388=CARTESIAN_POINT('Ctrl Pts',(-0.147932214000056,11.6,-10.408433454));
#298389=CARTESIAN_POINT('Ctrl Pts',(-0.147774569000055,15.2,-10.407247142));
#298390=CARTESIAN_POINT('Ctrl Pts',(-0.147774569000055,11.6,-10.407247142));
#298391=CARTESIAN_POINT('Ctrl Pts',(-0.147619240000055,15.2,-10.40606944));
#298392=CARTESIAN_POINT('Ctrl Pts',(-0.147619240000055,11.6,-10.40606944));
#298393=CARTESIAN_POINT('Ctrl Pts',(-0.147466215000056,15.2,-10.404900372));
#298394=CARTESIAN_POINT('Ctrl Pts',(-0.147466215000056,11.6,-10.404900372));
#298395=CARTESIAN_POINT('Ctrl Pts',(-0.147315478000056,15.2,-10.403739965));
#298396=CARTESIAN_POINT('Ctrl Pts',(-0.147315478000056,11.6,-10.403739965));
#298397=CARTESIAN_POINT('Ctrl Pts',(-0.147167017000056,15.2,-10.402588242));
#298398=CARTESIAN_POINT('Ctrl Pts',(-0.147167017000056,11.6,-10.402588242));
#298399=CARTESIAN_POINT('Ctrl Pts',(-0.147020820000057,15.2,-10.401445231));
#298400=CARTESIAN_POINT('Ctrl Pts',(-0.147020820000057,11.6,-10.401445231));
#298401=CARTESIAN_POINT('Ctrl Pts',(-0.146876872000057,15.2,-10.400310957));
#298402=CARTESIAN_POINT('Ctrl Pts',(-0.146876872000057,11.6,-10.400310957));
#298403=CARTESIAN_POINT('Ctrl Pts',(-0.146735160000055,15.2,-10.399185446));
#298404=CARTESIAN_POINT('Ctrl Pts',(-0.146735160000055,11.6,-10.399185446));
#298405=CARTESIAN_POINT('Ctrl Pts',(-0.146595671000057,15.2,-10.398068726));
#298406=CARTESIAN_POINT('Ctrl Pts',(-0.146595671000057,11.6,-10.398068726));
#298407=CARTESIAN_POINT('Ctrl Pts',(-0.146458391000056,15.2,-10.39696082));
#298408=CARTESIAN_POINT('Ctrl Pts',(-0.146458391000056,11.6,-10.39696082));
#298409=CARTESIAN_POINT('Ctrl Pts',(-0.146323306000056,15.2,-10.395861756));
#298410=CARTESIAN_POINT('Ctrl Pts',(-0.146323306000056,11.6,-10.395861756));
#298411=CARTESIAN_POINT('Ctrl Pts',(-0.146190404000055,15.2,-10.394771561));
#298412=CARTESIAN_POINT('Ctrl Pts',(-0.146190404000055,11.6,-10.394771561));
#298413=CARTESIAN_POINT('Ctrl Pts',(-0.146059668000056,15.2,-10.39369026));
#298414=CARTESIAN_POINT('Ctrl Pts',(-0.146059668000056,11.6,-10.39369026));
#298415=CARTESIAN_POINT('Ctrl Pts',(-0.145931087000056,15.2,-10.392617881));
#298416=CARTESIAN_POINT('Ctrl Pts',(-0.145931087000056,11.6,-10.392617881));
#298417=CARTESIAN_POINT('Ctrl Pts',(-0.145804646000055,15.2,-10.39155445));
#298418=CARTESIAN_POINT('Ctrl Pts',(-0.145804646000055,11.6,-10.39155445));
#298419=CARTESIAN_POINT('Ctrl Pts',(-0.145680330000056,15.2,-10.390499995));
#298420=CARTESIAN_POINT('Ctrl Pts',(-0.145680330000056,11.6,-10.390499995));
#298421=CARTESIAN_POINT('Ctrl Pts',(-0.145558126000056,15.2,-10.389454543));
#298422=CARTESIAN_POINT('Ctrl Pts',(-0.145558126000056,11.6,-10.389454543));
#298423=CARTESIAN_POINT('Ctrl Pts',(-0.145438020000055,15.2,-10.388418119));
#298424=CARTESIAN_POINT('Ctrl Pts',(-0.145438020000055,11.6,-10.388418119));
#298425=CARTESIAN_POINT('Ctrl Pts',(-0.145319997000056,15.2,-10.387390753));
#298426=CARTESIAN_POINT('Ctrl Pts',(-0.145319997000056,11.6,-10.387390753));
#298427=CARTESIAN_POINT('Ctrl Pts',(-0.145204042000057,15.2,-10.38637247));
#298428=CARTESIAN_POINT('Ctrl Pts',(-0.145204042000057,11.6,-10.38637247));
#298429=CARTESIAN_POINT('Ctrl Pts',(-0.145090142000056,15.2,-10.3853633));
#298430=CARTESIAN_POINT('Ctrl Pts',(-0.145090142000056,11.6,-10.3853633));
#298431=CARTESIAN_POINT('Ctrl Pts',(-0.144978281000055,15.2,-10.38436327));
#298432=CARTESIAN_POINT('Ctrl Pts',(-0.144978281000055,11.6,-10.38436327));
#298433=CARTESIAN_POINT('Ctrl Pts',(-0.144868446000055,15.2,-10.383372406));
#298434=CARTESIAN_POINT('Ctrl Pts',(-0.144868446000055,11.6,-10.383372406));
#298435=CARTESIAN_POINT('Ctrl Pts',(-0.144760620000056,15.2,-10.382390738));
#298436=CARTESIAN_POINT('Ctrl Pts',(-0.144760620000056,11.6,-10.382390738));
#298437=CARTESIAN_POINT('Ctrl Pts',(-0.144654791000055,15.2,-10.381418293));
#298438=CARTESIAN_POINT('Ctrl Pts',(-0.144654791000055,11.6,-10.381418293));
#298439=CARTESIAN_POINT('Ctrl Pts',(-0.144550942000056,15.2,-10.380455099));
#298440=CARTESIAN_POINT('Ctrl Pts',(-0.144550942000056,11.6,-10.380455099));
#298441=CARTESIAN_POINT('Ctrl Pts',(-0.144449058000056,15.2,-10.379501186));
#298442=CARTESIAN_POINT('Ctrl Pts',(-0.144449058000056,11.6,-10.379501186));
#298443=CARTESIAN_POINT('Ctrl Pts',(-0.144349125000056,15.2,-10.378556581));
#298444=CARTESIAN_POINT('Ctrl Pts',(-0.144349125000056,11.6,-10.378556581));
#298445=CARTESIAN_POINT('Ctrl Pts',(-0.144251127000056,15.2,-10.377621314));
#298446=CARTESIAN_POINT('Ctrl Pts',(-0.144251127000056,11.6,-10.377621314));
#298447=CARTESIAN_POINT('Ctrl Pts',(-0.144155050000055,15.2,-10.376695412));
#298448=CARTESIAN_POINT('Ctrl Pts',(-0.144155050000055,11.6,-10.376695412));
#298449=CARTESIAN_POINT('Ctrl Pts',(-0.144061421000057,15.2,-10.375784183));
#298450=CARTESIAN_POINT('Ctrl Pts',(-0.144061421000057,11.6,-10.375784183));
#298451=CARTESIAN_POINT('Ctrl Pts',(-0.143988114000055,15.2,-10.375063685));
#298452=CARTESIAN_POINT('Ctrl Pts',(-0.143988114000055,11.6,-10.375063685));
#298453=CARTESIAN_POINT('Ctrl Pts',(-0.143934095000056,15.2,-10.374528791));
#298454=CARTESIAN_POINT('Ctrl Pts',(-0.143934095000056,11.6,-10.374528791));
#298455=CARTESIAN_POINT('Ctrl Pts',(-0.143898619000057,15.2,-10.374175764));
#298456=CARTESIAN_POINT('Ctrl Pts',(-0.143898619000057,11.6,-10.374175764));
#298457=CARTESIAN_POINT('Ctrl Pts',(-0.143881228000057,15.2,-10.374002275));
#298458=CARTESIAN_POINT('Ctrl Pts',(-0.143881228000057,11.6,-10.374002275));
#298459=CARTESIAN_POINT('Ctrl Pts',(-0.546958306000055,12.2,-11.486985532));
#298460=CARTESIAN_POINT('Ctrl Pts',(-0.546590899000057,12.2,-11.486315008));
#298461=CARTESIAN_POINT('Ctrl Pts',(-0.545856551000057,12.2,-11.484974209));
#298462=CARTESIAN_POINT('Ctrl Pts',(-0.544756421000056,12.2,-11.482963757));
#298463=CARTESIAN_POINT('Ctrl Pts',(-0.543292369000056,12.2,-11.480284643));
#298464=CARTESIAN_POINT('Ctrl Pts',(-0.541466946000057,12.2,-11.476938237));
#298465=CARTESIAN_POINT('Ctrl Pts',(-0.539646167000055,12.2,-11.473594318));
#298466=CARTESIAN_POINT('Ctrl Pts',(-0.537830030000055,12.2,-11.470252887));
#298467=CARTESIAN_POINT('Ctrl Pts',(-0.536018537000055,12.2,-11.466913949));
#298468=CARTESIAN_POINT('Ctrl Pts',(-0.534211686000056,12.2,-11.46357751));
#298469=CARTESIAN_POINT('Ctrl Pts',(-0.532409474000056,12.2,-11.460243578));
#298470=CARTESIAN_POINT('Ctrl Pts',(-0.530611902000055,12.2,-11.456912162));
#298471=CARTESIAN_POINT('Ctrl Pts',(-0.528818965000056,12.2,-11.453583273));
#298472=CARTESIAN_POINT('Ctrl Pts',(-0.527030665000057,12.2,-11.450256921));
#298473=CARTESIAN_POINT('Ctrl Pts',(-0.525246997000056,12.2,-11.446933118));
#298474=CARTESIAN_POINT('Ctrl Pts',(-0.523467959000056,12.2,-11.443611875));
#298475=CARTESIAN_POINT('Ctrl Pts',(-0.521693552000055,12.2,-11.4402932));
#298476=CARTESIAN_POINT('Ctrl Pts',(-0.519923771000055,12.2,-11.436977103));
#298477=CARTESIAN_POINT('Ctrl Pts',(-0.518158619000056,12.2,-11.433663589));
#298478=CARTESIAN_POINT('Ctrl Pts',(-0.516398090000055,12.2,-11.43035267));
#298479=CARTESIAN_POINT('Ctrl Pts',(-0.514642185000056,12.2,-11.427044351));
#298480=CARTESIAN_POINT('Ctrl Pts',(-0.512890901000055,12.2,-11.423738642));
#298481=CARTESIAN_POINT('Ctrl Pts',(-0.511144239000056,12.2,-11.420435551));
#298482=CARTESIAN_POINT('Ctrl Pts',(-0.509402194000056,12.2,-11.417135088));
#298483=CARTESIAN_POINT('Ctrl Pts',(-0.507664766000057,12.2,-11.413837262));
#298484=CARTESIAN_POINT('Ctrl Pts',(-0.505931954000056,12.2,-11.410542081));
#298485=CARTESIAN_POINT('Ctrl Pts',(-0.504203756000056,12.2,-11.407249556));
#298486=CARTESIAN_POINT('Ctrl Pts',(-0.502480169000057,12.2,-11.403959697));
#298487=CARTESIAN_POINT('Ctrl Pts',(-0.500761192000055,12.2,-11.400672511));
#298488=CARTESIAN_POINT('Ctrl Pts',(-0.499046823000056,12.2,-11.397388008));
#298489=CARTESIAN_POINT('Ctrl Pts',(-0.497337060000056,12.2,-11.394106196));
#298490=CARTESIAN_POINT('Ctrl Pts',(-0.495631904000057,12.2,-11.390827086));
#298491=CARTESIAN_POINT('Ctrl Pts',(-0.493931349000055,12.2,-11.387550685));
#298492=CARTESIAN_POINT('Ctrl Pts',(-0.492235397000057,12.2,-11.384277003));
#298493=CARTESIAN_POINT('Ctrl Pts',(-0.490544043000056,12.2,-11.381006047));
#298494=CARTESIAN_POINT('Ctrl Pts',(-0.488857288000055,12.2,-11.377737829));
#298495=CARTESIAN_POINT('Ctrl Pts',(-0.487175129000056,12.2,-11.374472358));
#298496=CARTESIAN_POINT('Ctrl Pts',(-0.485497564000056,12.2,-11.371209642));
#298497=CARTESIAN_POINT('Ctrl Pts',(-0.483824592000056,12.2,-11.367949691));
#298498=CARTESIAN_POINT('Ctrl Pts',(-0.482156209000056,12.2,-11.364692512));
#298499=CARTESIAN_POINT('Ctrl Pts',(-0.480492416000056,12.2,-11.361438118));
#298500=CARTESIAN_POINT('Ctrl Pts',(-0.478833210000056,12.2,-11.358186515));
#298501=CARTESIAN_POINT('Ctrl Pts',(-0.477178589000056,12.2,-11.354937714));
#298502=CARTESIAN_POINT('Ctrl Pts',(-0.475528552000055,12.2,-11.351691723));
#298503=CARTESIAN_POINT('Ctrl Pts',(-0.473883095000056,12.2,-11.348448553));
#298504=CARTESIAN_POINT('Ctrl Pts',(-0.472242218000056,12.2,-11.345208212));
#298505=CARTESIAN_POINT('Ctrl Pts',(-0.470605918000055,12.2,-11.341970709));
#298506=CARTESIAN_POINT('Ctrl Pts',(-0.468974194000056,12.2,-11.338736054));
#298507=CARTESIAN_POINT('Ctrl Pts',(-0.467347044000055,12.2,-11.335504256));
#298508=CARTESIAN_POINT('Ctrl Pts',(-0.465724466000056,12.2,-11.332275325));
#298509=CARTESIAN_POINT('Ctrl Pts',(-0.464106457000056,12.2,-11.329049269));
#298510=CARTESIAN_POINT('Ctrl Pts',(-0.462493018000056,12.2,-11.325826098));
#298511=CARTESIAN_POINT('Ctrl Pts',(-0.460884143000057,12.2,-11.322605822));
#298512=CARTESIAN_POINT('Ctrl Pts',(-0.459279833000057,12.2,-11.319388451));
#298513=CARTESIAN_POINT('Ctrl Pts',(-0.457680085000056,12.2,-11.316173992));
#298514=CARTESIAN_POINT('Ctrl Pts',(-0.456084896000055,12.2,-11.312962457));
#298515=CARTESIAN_POINT('Ctrl Pts',(-0.454494265000056,12.2,-11.309753853));
#298516=CARTESIAN_POINT('Ctrl Pts',(-0.452908191000055,12.2,-11.306548191));
#298517=CARTESIAN_POINT('Ctrl Pts',(-0.451326671000055,12.2,-11.303345481));
#298518=CARTESIAN_POINT('Ctrl Pts',(-0.449749702000056,12.2,-11.300145731));
#298519=CARTESIAN_POINT('Ctrl Pts',(-0.448177284000056,12.2,-11.296948952));
#298520=CARTESIAN_POINT('Ctrl Pts',(-0.446609414000055,12.2,-11.293755152));
#298521=CARTESIAN_POINT('Ctrl Pts',(-0.445046088000056,12.2,-11.290564341));
#298522=CARTESIAN_POINT('Ctrl Pts',(-0.443487307000057,12.2,-11.287376529));
#298523=CARTESIAN_POINT('Ctrl Pts',(-0.441933068000055,12.2,-11.284191725));
#298524=CARTESIAN_POINT('Ctrl Pts',(-0.440383367000056,12.2,-11.281009939));
#298525=CARTESIAN_POINT('Ctrl Pts',(-0.438838204000056,12.2,-11.277831182));
#298526=CARTESIAN_POINT('Ctrl Pts',(-0.437297576000055,12.2,-11.274655461));
#298527=CARTESIAN_POINT('Ctrl Pts',(-0.435761482000055,12.2,-11.271482787));
#298528=CARTESIAN_POINT('Ctrl Pts',(-0.434229918000056,12.2,-11.268313169));
#298529=CARTESIAN_POINT('Ctrl Pts',(-0.432702884000056,12.2,-11.265146617));
#298530=CARTESIAN_POINT('Ctrl Pts',(-0.431180374000055,12.2,-11.261983141));
#298531=CARTESIAN_POINT('Ctrl Pts',(-0.429662391000055,12.2,-11.258822751));
#298532=CARTESIAN_POINT('Ctrl Pts',(-0.428148929000055,12.2,-11.255665455));
#298533=CARTESIAN_POINT('Ctrl Pts',(-0.426639987000056,12.2,-11.252511265));
#298534=CARTESIAN_POINT('Ctrl Pts',(-0.425135562000056,12.2,-11.249360189));
#298535=CARTESIAN_POINT('Ctrl Pts',(-0.423635654000056,12.2,-11.246212238));
#298536=CARTESIAN_POINT('Ctrl Pts',(-0.422140258000056,12.2,-11.243067421));
#298537=CARTESIAN_POINT('Ctrl Pts',(-0.420649373000056,12.2,-11.239925747));
#298538=CARTESIAN_POINT('Ctrl Pts',(-0.419162997000055,12.2,-11.236787227));
#298539=CARTESIAN_POINT('Ctrl Pts',(-0.417681127000057,12.2,-11.233651872));
#298540=CARTESIAN_POINT('Ctrl Pts',(-0.416203762000055,12.2,-11.230519688));
#298541=CARTESIAN_POINT('Ctrl Pts',(-0.414730899000055,12.2,-11.22739069));
#298542=CARTESIAN_POINT('Ctrl Pts',(-0.413262534000056,12.2,-11.224264883));
#298543=CARTESIAN_POINT('Ctrl Pts',(-0.411798667000056,12.2,-11.221142281));
#298544=CARTESIAN_POINT('Ctrl Pts',(-0.410339295000056,12.2,-11.21802289));
#298545=CARTESIAN_POINT('Ctrl Pts',(-0.408884415000056,12.2,-11.214906723));
#298546=CARTESIAN_POINT('Ctrl Pts',(-0.407434025000055,12.2,-11.211793789));
#298547=CARTESIAN_POINT('Ctrl Pts',(-0.405988122000055,12.2,-11.208684097));
#298548=CARTESIAN_POINT('Ctrl Pts',(-0.404546705000056,12.2,-11.205577658));
#298549=CARTESIAN_POINT('Ctrl Pts',(-0.403109771000055,12.2,-11.202474481));
#298550=CARTESIAN_POINT('Ctrl Pts',(-0.401677318000055,12.2,-11.199374578));
#298551=CARTESIAN_POINT('Ctrl Pts',(-0.400249343000055,12.2,-11.196277957));
#298552=CARTESIAN_POINT('Ctrl Pts',(-0.398825842000056,12.2,-11.193184629));
#298553=CARTESIAN_POINT('Ctrl Pts',(-0.397406814000056,12.2,-11.190094604));
#298554=CARTESIAN_POINT('Ctrl Pts',(-0.395992258000056,12.2,-11.187007892));
#298555=CARTESIAN_POINT('Ctrl Pts',(-0.394582170000056,12.2,-11.183924502));
#298556=CARTESIAN_POINT('Ctrl Pts',(-0.393176547000056,12.2,-11.180844447));
#298557=CARTESIAN_POINT('Ctrl Pts',(-0.391775388000056,12.2,-11.177767733));
#298558=CARTESIAN_POINT('Ctrl Pts',(-0.390378688000055,12.2,-11.174694374));
#298559=CARTESIAN_POINT('Ctrl Pts',(-0.388986447000056,12.2,-11.171624379));
#298560=CARTESIAN_POINT('Ctrl Pts',(-0.387598661000055,12.2,-11.168557756));
#298561=CARTESIAN_POINT('Ctrl Pts',(-0.386215329000056,12.2,-11.165494519));
#298562=CARTESIAN_POINT('Ctrl Pts',(-0.384836446000056,12.2,-11.162434675));
#298563=CARTESIAN_POINT('Ctrl Pts',(-0.383462012000055,12.2,-11.159378235));
#298564=CARTESIAN_POINT('Ctrl Pts',(-0.382092022000055,12.2,-11.156325211));
#298565=CARTESIAN_POINT('Ctrl Pts',(-0.380726475000056,12.2,-11.153275611));
#298566=CARTESIAN_POINT('Ctrl Pts',(-0.379365367000055,12.2,-11.150229445));
#298567=CARTESIAN_POINT('Ctrl Pts',(-0.378008697000055,12.2,-11.147186726));
#298568=CARTESIAN_POINT('Ctrl Pts',(-0.376656462000057,12.2,-11.144147464));
#298569=CARTESIAN_POINT('Ctrl Pts',(-0.375308659000056,12.2,-11.141111667));
#298570=CARTESIAN_POINT('Ctrl Pts',(-0.373965284000055,12.2,-11.138079346));
#298571=CARTESIAN_POINT('Ctrl Pts',(-0.372626336000056,12.2,-11.135050513));
#298572=CARTESIAN_POINT('Ctrl Pts',(-0.371291813000055,12.2,-11.132025177));
#298573=CARTESIAN_POINT('Ctrl Pts',(-0.369961710000055,12.2,-11.129003349));
#298574=CARTESIAN_POINT('Ctrl Pts',(-0.368636025000055,12.2,-11.125985039));
#298575=CARTESIAN_POINT('Ctrl Pts',(-0.367314756000056,12.2,-11.122970257));
#298576=CARTESIAN_POINT('Ctrl Pts',(-0.365997899000057,12.2,-11.119959015));
#298577=CARTESIAN_POINT('Ctrl Pts',(-0.364685453000057,12.2,-11.116951323));
#298578=CARTESIAN_POINT('Ctrl Pts',(-0.363377414000056,12.2,-11.11394719));
#298579=CARTESIAN_POINT('Ctrl Pts',(-0.362073780000056,12.2,-11.110946628));
#298580=CARTESIAN_POINT('Ctrl Pts',(-0.360774547000055,12.2,-11.107949648));
#298581=CARTESIAN_POINT('Ctrl Pts',(-0.359479712000056,12.2,-11.104956259));
#298582=CARTESIAN_POINT('Ctrl Pts',(-0.358189274000056,12.2,-11.101966474));
#298583=CARTESIAN_POINT('Ctrl Pts',(-0.356903229000055,12.2,-11.0989803));
#298584=CARTESIAN_POINT('Ctrl Pts',(-0.355621573000056,12.2,-11.09599775));
#298585=CARTESIAN_POINT('Ctrl Pts',(-0.354344305000056,12.2,-11.093018835));
#298586=CARTESIAN_POINT('Ctrl Pts',(-0.353071422000056,12.2,-11.090043565));
#298587=CARTESIAN_POINT('Ctrl Pts',(-0.351802919000056,12.2,-11.08707195));
#298588=CARTESIAN_POINT('Ctrl Pts',(-0.350538795000055,12.2,-11.084104002));
#298589=CARTESIAN_POINT('Ctrl Pts',(-0.349279047000056,12.2,-11.08113973));
#298590=CARTESIAN_POINT('Ctrl Pts',(-0.348023671000056,12.2,-11.078179147));
#298591=CARTESIAN_POINT('Ctrl Pts',(-0.346772665000056,12.2,-11.075222262));
#298592=CARTESIAN_POINT('Ctrl Pts',(-0.345526025000057,12.2,-11.072269087));
#298593=CARTESIAN_POINT('Ctrl Pts',(-0.344283750000055,12.2,-11.069319632));
#298594=CARTESIAN_POINT('Ctrl Pts',(-0.343045833000056,12.2,-11.066373907));
#298595=CARTESIAN_POINT('Ctrl Pts',(-0.341812276000055,12.2,-11.063431925));
#298596=CARTESIAN_POINT('Ctrl Pts',(-0.340583073000056,12.2,-11.060493695));
#298597=CARTESIAN_POINT('Ctrl Pts',(-0.339358220000056,12.2,-11.057559229));
#298598=CARTESIAN_POINT('Ctrl Pts',(-0.338137716000055,12.2,-11.054628537));
#298599=CARTESIAN_POINT('Ctrl Pts',(-0.336921557000055,12.2,-11.051701631));
#298600=CARTESIAN_POINT('Ctrl Pts',(-0.335709740000055,12.2,-11.048778521));
#298601=CARTESIAN_POINT('Ctrl Pts',(-0.334502263000056,12.2,-11.045859219));
#298602=CARTESIAN_POINT('Ctrl Pts',(-0.333299121000056,12.2,-11.042943735));
#298603=CARTESIAN_POINT('Ctrl Pts',(-0.332100311000056,12.2,-11.040032081));
#298604=CARTESIAN_POINT('Ctrl Pts',(-0.330905831000056,12.2,-11.037124266));
#298605=CARTESIAN_POINT('Ctrl Pts',(-0.329715678000057,12.2,-11.034220304));
#298606=CARTESIAN_POINT('Ctrl Pts',(-0.328529847000055,12.2,-11.031320204));
#298607=CARTESIAN_POINT('Ctrl Pts',(-0.327348336000056,12.2,-11.028423977));
#298608=CARTESIAN_POINT('Ctrl Pts',(-0.326171142000057,12.2,-11.025531635));
#298609=CARTESIAN_POINT('Ctrl Pts',(-0.324998260000056,12.2,-11.022643189));
#298610=CARTESIAN_POINT('Ctrl Pts',(-0.323829689000057,12.2,-11.01975865));
#298611=CARTESIAN_POINT('Ctrl Pts',(-0.322665426000055,12.2,-11.01687803));
#298612=CARTESIAN_POINT('Ctrl Pts',(-0.321505465000056,12.2,-11.014001338));
#298613=CARTESIAN_POINT('Ctrl Pts',(-0.320349803000056,12.2,-11.011128588));
#298614=CARTESIAN_POINT('Ctrl Pts',(-0.319198440000056,12.2,-11.008259788));
#298615=CARTESIAN_POINT('Ctrl Pts',(-0.318051369000055,12.2,-11.005394953));
#298616=CARTESIAN_POINT('Ctrl Pts',(-0.316908589000056,12.2,-11.002534092));
#298617=CARTESIAN_POINT('Ctrl Pts',(-0.315770096000056,12.2,-10.999677217));
#298618=CARTESIAN_POINT('Ctrl Pts',(-0.314635885000056,12.2,-10.996824339));
#298619=CARTESIAN_POINT('Ctrl Pts',(-0.313505954000056,12.2,-10.993975469));
#298620=CARTESIAN_POINT('Ctrl Pts',(-0.312380301000056,12.2,-10.991130619));
#298621=CARTESIAN_POINT('Ctrl Pts',(-0.311258919000055,12.2,-10.988289801));
#298622=CARTESIAN_POINT('Ctrl Pts',(-0.310141808000056,12.2,-10.985453024));
#298623=CARTESIAN_POINT('Ctrl Pts',(-0.309028962000056,12.2,-10.982620303));
#298624=CARTESIAN_POINT('Ctrl Pts',(-0.307920380000055,12.2,-10.979791646));
#298625=CARTESIAN_POINT('Ctrl Pts',(-0.306816056000055,12.2,-10.976967067));
#298626=CARTESIAN_POINT('Ctrl Pts',(-0.305715987000056,12.2,-10.974146576));
#298627=CARTESIAN_POINT('Ctrl Pts',(-0.304620171000056,12.2,-10.971330186));
#298628=CARTESIAN_POINT('Ctrl Pts',(-0.303528603000055,12.2,-10.968517907));
#298629=CARTESIAN_POINT('Ctrl Pts',(-0.302441280000056,12.2,-10.965709752));
#298630=CARTESIAN_POINT('Ctrl Pts',(-0.301358198000056,12.2,-10.962905731));
#298631=CARTESIAN_POINT('Ctrl Pts',(-0.300279354000056,12.2,-10.960105857));
#298632=CARTESIAN_POINT('Ctrl Pts',(-0.299204743000056,12.2,-10.957310141));
#298633=CARTESIAN_POINT('Ctrl Pts',(-0.298134363000055,12.2,-10.954518595));
#298634=CARTESIAN_POINT('Ctrl Pts',(-0.297068210000055,12.2,-10.951731231));
#298635=CARTESIAN_POINT('Ctrl Pts',(-0.296006280000055,12.2,-10.948948059));
#298636=CARTESIAN_POINT('Ctrl Pts',(-0.294948568000055,12.2,-10.946169093));
#298637=CARTESIAN_POINT('Ctrl Pts',(-0.293895073000057,12.2,-10.943394344));
#298638=CARTESIAN_POINT('Ctrl Pts',(-0.292845789000056,12.2,-10.940623823));
#298639=CARTESIAN_POINT('Ctrl Pts',(-0.291800713000056,12.2,-10.937857543));
#298640=CARTESIAN_POINT('Ctrl Pts',(-0.290759842000057,12.2,-10.935095515));
#298641=CARTESIAN_POINT('Ctrl Pts',(-0.289723171000055,12.2,-10.932337751));
#298642=CARTESIAN_POINT('Ctrl Pts',(-0.288690696000057,12.2,-10.929584264));
#298643=CARTESIAN_POINT('Ctrl Pts',(-0.287662415000056,12.2,-10.926835064));
#298644=CARTESIAN_POINT('Ctrl Pts',(-0.286638323000057,12.2,-10.924090164));
#298645=CARTESIAN_POINT('Ctrl Pts',(-0.285618416000055,12.2,-10.921349576));
#298646=CARTESIAN_POINT('Ctrl Pts',(-0.284602690000056,12.2,-10.918613312));
#298647=CARTESIAN_POINT('Ctrl Pts',(-0.283591141000056,12.2,-10.915881383));
#298648=CARTESIAN_POINT('Ctrl Pts',(-0.282583766000055,12.2,-10.913153802));
#298649=CARTESIAN_POINT('Ctrl Pts',(-0.281580560000056,12.2,-10.910430583));
#298650=CARTESIAN_POINT('Ctrl Pts',(-0.280581520000055,12.2,-10.907711734));
#298651=CARTESIAN_POINT('Ctrl Pts',(-0.279586642000057,12.2,-10.904997271));
#298652=CARTESIAN_POINT('Ctrl Pts',(-0.278595921000055,12.2,-10.902287203));
#298653=CARTESIAN_POINT('Ctrl Pts',(-0.277609355000056,12.2,-10.899581544));
#298654=CARTESIAN_POINT('Ctrl Pts',(-0.276626937000056,12.2,-10.896880306));
#298655=CARTESIAN_POINT('Ctrl Pts',(-0.275648666000056,12.2,-10.8941835));
#298656=CARTESIAN_POINT('Ctrl Pts',(-0.274674534000056,12.2,-10.891491141));
#298657=CARTESIAN_POINT('Ctrl Pts',(-0.273704541000056,12.2,-10.888803238));
#298658=CARTESIAN_POINT('Ctrl Pts',(-0.272738681000056,12.2,-10.886119805));
#298659=CARTESIAN_POINT('Ctrl Pts',(-0.271776951000057,12.2,-10.883440854));
#298660=CARTESIAN_POINT('Ctrl Pts',(-0.270819345000056,12.2,-10.880766398));
#298661=CARTESIAN_POINT('Ctrl Pts',(-0.269865860000056,12.2,-10.878096449));
#298662=CARTESIAN_POINT('Ctrl Pts',(-0.268916493000055,12.2,-10.87543102));
#298663=CARTESIAN_POINT('Ctrl Pts',(-0.267971237000056,12.2,-10.872770121));
#298664=CARTESIAN_POINT('Ctrl Pts',(-0.267030089000055,12.2,-10.870113767));
#298665=CARTESIAN_POINT('Ctrl Pts',(-0.266093047000057,12.2,-10.86746197));
#298666=CARTESIAN_POINT('Ctrl Pts',(-0.265160103000056,12.2,-10.864814742));
#298667=CARTESIAN_POINT('Ctrl Pts',(-0.264231255000055,12.2,-10.862172095));
#298668=CARTESIAN_POINT('Ctrl Pts',(-0.263306498000055,12.2,-10.859534042));
#298669=CARTESIAN_POINT('Ctrl Pts',(-0.262385828000056,12.2,-10.856900598));
#298670=CARTESIAN_POINT('Ctrl Pts',(-0.261469242000055,12.2,-10.854271772));
#298671=CARTESIAN_POINT('Ctrl Pts',(-0.260556733000056,12.2,-10.851647578));
#298672=CARTESIAN_POINT('Ctrl Pts',(-0.259648297000057,12.2,-10.84902803));
#298673=CARTESIAN_POINT('Ctrl Pts',(-0.258743931000056,12.2,-10.846413139));
#298674=CARTESIAN_POINT('Ctrl Pts',(-0.257843631000056,12.2,-10.843802918));
#298675=CARTESIAN_POINT('Ctrl Pts',(-0.256947390000055,12.2,-10.84119738));
#298676=CARTESIAN_POINT('Ctrl Pts',(-0.256055206000055,12.2,-10.838596538));
#298677=CARTESIAN_POINT('Ctrl Pts',(-0.255167073000055,12.2,-10.836000406));
#298678=CARTESIAN_POINT('Ctrl Pts',(-0.254282988000056,12.2,-10.833408995));
#298679=CARTESIAN_POINT('Ctrl Pts',(-0.253402945000056,12.2,-10.830822318));
#298680=CARTESIAN_POINT('Ctrl Pts',(-0.252526940000056,12.2,-10.828240388));
#298681=CARTESIAN_POINT('Ctrl Pts',(-0.251654969000056,12.2,-10.825663219));
#298682=CARTESIAN_POINT('Ctrl Pts',(-0.250787027000056,12.2,-10.823090823));
#298683=CARTESIAN_POINT('Ctrl Pts',(-0.249923109000055,12.2,-10.820523213));
#298684=CARTESIAN_POINT('Ctrl Pts',(-0.249063210000056,12.2,-10.817960403));
#298685=CARTESIAN_POINT('Ctrl Pts',(-0.248207327000056,12.2,-10.815402404));
#298686=CARTESIAN_POINT('Ctrl Pts',(-0.247355454000056,12.2,-10.812849232));
#298687=CARTESIAN_POINT('Ctrl Pts',(-0.246507587000057,12.2,-10.810300898));
#298688=CARTESIAN_POINT('Ctrl Pts',(-0.245663721000057,12.2,-10.807757416));
#298689=CARTESIAN_POINT('Ctrl Pts',(-0.244823851000057,12.2,-10.805218799));
#298690=CARTESIAN_POINT('Ctrl Pts',(-0.243987973000056,12.2,-10.80268506));
#298691=CARTESIAN_POINT('Ctrl Pts',(-0.243156080000055,12.2,-10.800156212));
#298692=CARTESIAN_POINT('Ctrl Pts',(-0.242328171000056,12.2,-10.797632269));
#298693=CARTESIAN_POINT('Ctrl Pts',(-0.241504238000055,12.2,-10.795113244));
#298694=CARTESIAN_POINT('Ctrl Pts',(-0.240684278000056,12.2,-10.79259915));
#298695=CARTESIAN_POINT('Ctrl Pts',(-0.239868284000057,12.2,-10.790090001));
#298696=CARTESIAN_POINT('Ctrl Pts',(-0.239056253000056,12.2,-10.78758581));
#298697=CARTESIAN_POINT('Ctrl Pts',(-0.238248181000056,12.2,-10.78508659));
#298698=CARTESIAN_POINT('Ctrl Pts',(-0.237444060000056,12.2,-10.782592355));
#298699=CARTESIAN_POINT('Ctrl Pts',(-0.236643888000057,12.2,-10.780103119));
#298700=CARTESIAN_POINT('Ctrl Pts',(-0.235847657000056,12.2,-10.777618895));
#298701=CARTESIAN_POINT('Ctrl Pts',(-0.235055365000055,12.2,-10.775139696));
#298702=CARTESIAN_POINT('Ctrl Pts',(-0.234267006000056,12.2,-10.772665536));
#298703=CARTESIAN_POINT('Ctrl Pts',(-0.233482574000057,12.2,-10.770196429));
#298704=CARTESIAN_POINT('Ctrl Pts',(-0.232702064000057,12.2,-10.767732388));
#298705=CARTESIAN_POINT('Ctrl Pts',(-0.231925472000055,12.2,-10.765273428));
#298706=CARTESIAN_POINT('Ctrl Pts',(-0.231152793000057,12.2,-10.76281956));
#298707=CARTESIAN_POINT('Ctrl Pts',(-0.230384020000055,12.2,-10.760370801));
#298708=CARTESIAN_POINT('Ctrl Pts',(-0.229619150000057,12.2,-10.757927163));
#298709=CARTESIAN_POINT('Ctrl Pts',(-0.228858176000056,12.2,-10.75548866));
#298710=CARTESIAN_POINT('Ctrl Pts',(-0.228101094000056,12.2,-10.753055307));
#298711=CARTESIAN_POINT('Ctrl Pts',(-0.227347899000057,12.2,-10.750627116));
#298712=CARTESIAN_POINT('Ctrl Pts',(-0.226598585000056,12.2,-10.748204102));
#298713=CARTESIAN_POINT('Ctrl Pts',(-0.225853145000056,12.2,-10.745786278));
#298714=CARTESIAN_POINT('Ctrl Pts',(-0.225111578000057,12.2,-10.743373659));
#298715=CARTESIAN_POINT('Ctrl Pts',(-0.224373875000056,12.2,-10.740966259));
#298716=CARTESIAN_POINT('Ctrl Pts',(-0.223640033000055,12.2,-10.738564091));
#298717=CARTESIAN_POINT('Ctrl Pts',(-0.222910044000055,12.2,-10.736167171));
#298718=CARTESIAN_POINT('Ctrl Pts',(-0.222183905000056,12.2,-10.733775512));
#298719=CARTESIAN_POINT('Ctrl Pts',(-0.221461609000055,12.2,-10.731389127));
#298720=CARTESIAN_POINT('Ctrl Pts',(-0.220743152000056,12.2,-10.729008033));
#298721=CARTESIAN_POINT('Ctrl Pts',(-0.220028527000055,12.2,-10.726632241));
#298722=CARTESIAN_POINT('Ctrl Pts',(-0.219317730000055,12.2,-10.724261768));
#298723=CARTESIAN_POINT('Ctrl Pts',(-0.218610753000055,12.2,-10.721896628));
#298724=CARTESIAN_POINT('Ctrl Pts',(-0.217907594000056,12.2,-10.719536833));
#298725=CARTESIAN_POINT('Ctrl Pts',(-0.217208245000055,12.2,-10.7171824));
#298726=CARTESIAN_POINT('Ctrl Pts',(-0.216373591030381,12.2,-10.7143635293024));
#298727=CARTESIAN_POINT('Ctrl Pts',(-0.215544636984895,12.2,-10.7115527448488));
#298728=CARTESIAN_POINT('Ctrl Pts',(-0.214721369015218,12.2,-10.7087500711512));
#298729=CARTESIAN_POINT('Ctrl Pts',(-0.213903779043993,12.2,-10.7059555439514));
#298730=CARTESIAN_POINT('Ctrl Pts',(-0.213091853000057,12.2,-10.703169187));
#298731=CARTESIAN_POINT('Ctrl Pts',(-0.212419019000055,12.2,-10.700852684));
#298732=CARTESIAN_POINT('Ctrl Pts',(-0.211749948000056,12.2,-10.69854166));
#298733=CARTESIAN_POINT('Ctrl Pts',(-0.211084639000055,12.2,-10.696236127));
#298734=CARTESIAN_POINT('Ctrl Pts',(-0.210423081000056,12.2,-10.693936102));
#298735=CARTESIAN_POINT('Ctrl Pts',(-0.209765271000055,12.2,-10.691641597));
#298736=CARTESIAN_POINT('Ctrl Pts',(-0.209111203000055,12.2,-10.68935263));
#298737=CARTESIAN_POINT('Ctrl Pts',(-0.208460870000057,12.2,-10.687069213));
#298738=CARTESIAN_POINT('Ctrl Pts',(-0.207814267000056,12.2,-10.684791362));
#298739=CARTESIAN_POINT('Ctrl Pts',(-0.207171387000056,12.2,-10.682519093));
#298740=CARTESIAN_POINT('Ctrl Pts',(-0.206532225000055,12.2,-10.68025242));
#298741=CARTESIAN_POINT('Ctrl Pts',(-0.205896774000056,12.2,-10.677991357));
#298742=CARTESIAN_POINT('Ctrl Pts',(-0.205265029000056,12.2,-10.67573592));
#298743=CARTESIAN_POINT('Ctrl Pts',(-0.204636983000055,12.2,-10.673486125));
#298744=CARTESIAN_POINT('Ctrl Pts',(-0.204012631000056,12.2,-10.671241986));
#298745=CARTESIAN_POINT('Ctrl Pts',(-0.203391965000056,12.2,-10.669003519));
#298746=CARTESIAN_POINT('Ctrl Pts',(-0.202774980000056,12.2,-10.666770738));
#298747=CARTESIAN_POINT('Ctrl Pts',(-0.202161670000055,12.2,-10.664543659));
#298748=CARTESIAN_POINT('Ctrl Pts',(-0.201552028000057,12.2,-10.662322297));
#298749=CARTESIAN_POINT('Ctrl Pts',(-0.200946049000056,12.2,-10.660106669));
#298750=CARTESIAN_POINT('Ctrl Pts',(-0.200343725000056,12.2,-10.657896788));
#298751=CARTESIAN_POINT('Ctrl Pts',(-0.199745051000055,12.2,-10.655692671));
#298752=CARTESIAN_POINT('Ctrl Pts',(-0.199150020000056,12.2,-10.653494333));
#298753=CARTESIAN_POINT('Ctrl Pts',(-0.198558626000055,12.2,-10.651301789));
#298754=CARTESIAN_POINT('Ctrl Pts',(-0.197970862000056,12.2,-10.649115056));
#298755=CARTESIAN_POINT('Ctrl Pts',(-0.197386723000056,12.2,-10.646934148));
#298756=CARTESIAN_POINT('Ctrl Pts',(-0.196806201000056,12.2,-10.644759081));
#298757=CARTESIAN_POINT('Ctrl Pts',(-0.196229289000056,12.2,-10.642589871));
#298758=CARTESIAN_POINT('Ctrl Pts',(-0.195655982000057,12.2,-10.640426534));
#298759=CARTESIAN_POINT('Ctrl Pts',(-0.195086274000056,12.2,-10.638269086));
#298760=CARTESIAN_POINT('Ctrl Pts',(-0.194520156000056,12.2,-10.636117541));
#298761=CARTESIAN_POINT('Ctrl Pts',(-0.193957623000056,12.2,-10.633971916));
#298762=CARTESIAN_POINT('Ctrl Pts',(-0.193398667000055,12.2,-10.631832228));
#298763=CARTESIAN_POINT('Ctrl Pts',(-0.192843283000055,12.2,-10.629698492));
#298764=CARTESIAN_POINT('Ctrl Pts',(-0.192291464000055,12.2,-10.627570723));
#298765=CARTESIAN_POINT('Ctrl Pts',(-0.191743203000057,12.2,-10.62544894));
#298766=CARTESIAN_POINT('Ctrl Pts',(-0.191198493000057,12.2,-10.623333156));
#298767=CARTESIAN_POINT('Ctrl Pts',(-0.190657326000055,12.2,-10.621223388));
#298768=CARTESIAN_POINT('Ctrl Pts',(-0.190119697000056,12.2,-10.619119652));
#298769=CARTESIAN_POINT('Ctrl Pts',(-0.189585599000056,12.2,-10.617021965));
#298770=CARTESIAN_POINT('Ctrl Pts',(-0.189055024000057,12.2,-10.614930343));
#298771=CARTESIAN_POINT('Ctrl Pts',(-0.188527965000055,12.2,-10.612844802));
#298772=CARTESIAN_POINT('Ctrl Pts',(-0.188004417000055,12.2,-10.610765359));
#298773=CARTESIAN_POINT('Ctrl Pts',(-0.187484370000056,12.2,-10.60869203));
#298774=CARTESIAN_POINT('Ctrl Pts',(-0.186967820000056,12.2,-10.606624832));
#298775=CARTESIAN_POINT('Ctrl Pts',(-0.186454758000056,12.2,-10.60456378));
#298776=CARTESIAN_POINT('Ctrl Pts',(-0.185945177000055,12.2,-10.602508892));
#298777=CARTESIAN_POINT('Ctrl Pts',(-0.185439071000056,12.2,-10.600460183));
#298778=CARTESIAN_POINT('Ctrl Pts',(-0.184936432000056,12.2,-10.598417672));
#298779=CARTESIAN_POINT('Ctrl Pts',(-0.184437253000055,12.2,-10.596381375));
#298780=CARTESIAN_POINT('Ctrl Pts',(-0.183941526000057,12.2,-10.594351307));
#298781=CARTESIAN_POINT('Ctrl Pts',(-0.183449244000055,12.2,-10.592327487));
#298782=CARTESIAN_POINT('Ctrl Pts',(-0.182960401000055,12.2,-10.59030993));
#298783=CARTESIAN_POINT('Ctrl Pts',(-0.182474988000055,12.2,-10.588298654));
#298784=CARTESIAN_POINT('Ctrl Pts',(-0.181992998000055,12.2,-10.586293676));
#298785=CARTESIAN_POINT('Ctrl Pts',(-0.181514425000057,12.2,-10.584295012));
#298786=CARTESIAN_POINT('Ctrl Pts',(-0.181039260000055,12.2,-10.582302681));
#298787=CARTESIAN_POINT('Ctrl Pts',(-0.180567496000055,12.2,-10.580316698));
#298788=CARTESIAN_POINT('Ctrl Pts',(-0.180099125000056,12.2,-10.578337081));
#298789=CARTESIAN_POINT('Ctrl Pts',(-0.179634139000056,12.2,-10.576363848));
#298790=CARTESIAN_POINT('Ctrl Pts',(-0.179172532000056,12.2,-10.574397014));
#298791=CARTESIAN_POINT('Ctrl Pts',(-0.178714296000055,12.2,-10.572436599));
#298792=CARTESIAN_POINT('Ctrl Pts',(-0.178259423000057,12.2,-10.570482619));
#298793=CARTESIAN_POINT('Ctrl Pts',(-0.177807905000057,12.2,-10.568535092));
#298794=CARTESIAN_POINT('Ctrl Pts',(-0.177359734000057,12.2,-10.566594035));
#298795=CARTESIAN_POINT('Ctrl Pts',(-0.176914903000055,12.2,-10.564659465));
#298796=CARTESIAN_POINT('Ctrl Pts',(-0.176473403000056,12.2,-10.562731399));
#298797=CARTESIAN_POINT('Ctrl Pts',(-0.176035228000057,12.2,-10.560809857));
#298798=CARTESIAN_POINT('Ctrl Pts',(-0.175600369000056,12.2,-10.558894856));
#298799=CARTESIAN_POINT('Ctrl Pts',(-0.175168818000057,12.2,-10.556986413));
#298800=CARTESIAN_POINT('Ctrl Pts',(-0.174740568000056,12.2,-10.555084546));
#298801=CARTESIAN_POINT('Ctrl Pts',(-0.174315609000055,12.2,-10.553189273));
#298802=CARTESIAN_POINT('Ctrl Pts',(-0.173893934000056,12.2,-10.551300611));
#298803=CARTESIAN_POINT('Ctrl Pts',(-0.173475537000056,12.2,-10.549418579));
#298804=CARTESIAN_POINT('Ctrl Pts',(-0.173060406000056,12.2,-10.547543195));
#298805=CARTESIAN_POINT('Ctrl Pts',(-0.172648536000055,12.2,-10.545674477));
#298806=CARTESIAN_POINT('Ctrl Pts',(-0.172239916000055,12.2,-10.543812443));
#298807=CARTESIAN_POINT('Ctrl Pts',(-0.171834541000055,12.2,-10.541957111));
#298808=CARTESIAN_POINT('Ctrl Pts',(-0.171432400000056,12.2,-10.5401085));
#298809=CARTESIAN_POINT('Ctrl Pts',(-0.171033486000055,12.2,-10.538266627));
#298810=CARTESIAN_POINT('Ctrl Pts',(-0.170637791000056,12.2,-10.536431511));
#298811=CARTESIAN_POINT('Ctrl Pts',(-0.170245305000056,12.2,-10.534603171));
#298812=CARTESIAN_POINT('Ctrl Pts',(-0.169856021000055,12.2,-10.532781626));
#298813=CARTESIAN_POINT('Ctrl Pts',(-0.169469930000057,12.2,-10.530966892));
#298814=CARTESIAN_POINT('Ctrl Pts',(-0.169087023000056,12.2,-10.529158991));
#298815=CARTESIAN_POINT('Ctrl Pts',(-0.168707293000055,12.2,-10.527357938));
#298816=CARTESIAN_POINT('Ctrl Pts',(-0.168330729000056,12.2,-10.525563754));
#298817=CARTESIAN_POINT('Ctrl Pts',(-0.167957324000056,12.2,-10.523776458));
#298818=CARTESIAN_POINT('Ctrl Pts',(-0.167587069000056,12.2,-10.521996069));
#298819=CARTESIAN_POINT('Ctrl Pts',(-0.167219956000055,12.2,-10.520222604));
#298820=CARTESIAN_POINT('Ctrl Pts',(-0.166855974000055,12.2,-10.518456084));
#298821=CARTESIAN_POINT('Ctrl Pts',(-0.166495117000055,12.2,-10.516696527));
#298822=CARTESIAN_POINT('Ctrl Pts',(-0.166137374000056,12.2,-10.514943952));
#298823=CARTESIAN_POINT('Ctrl Pts',(-0.165782737000055,12.2,-10.513198378));
#298824=CARTESIAN_POINT('Ctrl Pts',(-0.165431198000056,12.2,-10.511459826));
#298825=CARTESIAN_POINT('Ctrl Pts',(-0.165082744000056,12.2,-10.509728314));
#298826=CARTESIAN_POINT('Ctrl Pts',(-0.164737371000055,12.2,-10.508003862));
#298827=CARTESIAN_POINT('Ctrl Pts',(-0.164395067000056,12.2,-10.506286487));
#298828=CARTESIAN_POINT('Ctrl Pts',(-0.164055824000057,12.2,-10.504576212));
#298829=CARTESIAN_POINT('Ctrl Pts',(-0.163719632000056,12.2,-10.502873055));
#298830=CARTESIAN_POINT('Ctrl Pts',(-0.163386483000056,12.2,-10.501177036));
#298831=CARTESIAN_POINT('Ctrl Pts',(-0.163056366000056,12.2,-10.499488173));
#298832=CARTESIAN_POINT('Ctrl Pts',(-0.162729274000055,12.2,-10.497806488));
#298833=CARTESIAN_POINT('Ctrl Pts',(-0.162405194000056,12.2,-10.496131999));
#298834=CARTESIAN_POINT('Ctrl Pts',(-0.162084120000056,12.2,-10.494464728));
#298835=CARTESIAN_POINT('Ctrl Pts',(-0.161766042000057,12.2,-10.492804693));
#298836=CARTESIAN_POINT('Ctrl Pts',(-0.161450949000056,12.2,-10.491151915));
#298837=CARTESIAN_POINT('Ctrl Pts',(-0.161138833000055,12.2,-10.489506414));
#298838=CARTESIAN_POINT('Ctrl Pts',(-0.160829682000055,12.2,-10.487868211));
#298839=CARTESIAN_POINT('Ctrl Pts',(-0.160523489000056,12.2,-10.486237324));
#298840=CARTESIAN_POINT('Ctrl Pts',(-0.160220245000057,12.2,-10.484613776));
#298841=CARTESIAN_POINT('Ctrl Pts',(-0.159919937000056,12.2,-10.482997586));
#298842=CARTESIAN_POINT('Ctrl Pts',(-0.159622556000055,12.2,-10.481388775));
#298843=CARTESIAN_POINT('Ctrl Pts',(-0.159328094000056,12.2,-10.479787363));
#298844=CARTESIAN_POINT('Ctrl Pts',(-0.159036540000056,12.2,-10.478193371));
#298845=CARTESIAN_POINT('Ctrl Pts',(-0.158747884000056,12.2,-10.476606819));
#298846=CARTESIAN_POINT('Ctrl Pts',(-0.158462117000056,12.2,-10.475027729));
#298847=CARTESIAN_POINT('Ctrl Pts',(-0.158179227000056,12.2,-10.473456121));
#298848=CARTESIAN_POINT('Ctrl Pts',(-0.157899205000056,12.2,-10.471892016));
#298849=CARTESIAN_POINT('Ctrl Pts',(-0.157622041000056,12.2,-10.470335435));
#298850=CARTESIAN_POINT('Ctrl Pts',(-0.157347725000055,12.2,-10.4687864));
#298851=CARTESIAN_POINT('Ctrl Pts',(-0.157076245000055,12.2,-10.467244931));
#298852=CARTESIAN_POINT('Ctrl Pts',(-0.156807594000057,12.2,-10.46571105));
#298853=CARTESIAN_POINT('Ctrl Pts',(-0.156541758000056,12.2,-10.464184778));
#298854=CARTESIAN_POINT('Ctrl Pts',(-0.156278730000056,12.2,-10.462666135));
#298855=CARTESIAN_POINT('Ctrl Pts',(-0.156018496000057,12.2,-10.461155145));
#298856=CARTESIAN_POINT('Ctrl Pts',(-0.155761048000055,12.2,-10.459651829));
#298857=CARTESIAN_POINT('Ctrl Pts',(-0.155506375000056,12.2,-10.458156207));
#298858=CARTESIAN_POINT('Ctrl Pts',(-0.155254466000055,12.2,-10.456668302));
#298859=CARTESIAN_POINT('Ctrl Pts',(-0.155005310000057,12.2,-10.455188136));
#298860=CARTESIAN_POINT('Ctrl Pts',(-0.154758897000056,12.2,-10.45371573));
#298861=CARTESIAN_POINT('Ctrl Pts',(-0.154515216000056,12.2,-10.452251106));
#298862=CARTESIAN_POINT('Ctrl Pts',(-0.154274256000055,12.2,-10.450794288));
#298863=CARTESIAN_POINT('Ctrl Pts',(-0.154036006000055,12.2,-10.449345296));
#298864=CARTESIAN_POINT('Ctrl Pts',(-0.153800456000056,12.2,-10.447904152));
#298865=CARTESIAN_POINT('Ctrl Pts',(-0.153567593000057,12.2,-10.446470879));
#298866=CARTESIAN_POINT('Ctrl Pts',(-0.153337407000055,12.2,-10.4450455));
#298867=CARTESIAN_POINT('Ctrl Pts',(-0.153109888000056,12.2,-10.443628038));
#298868=CARTESIAN_POINT('Ctrl Pts',(-0.152885022000057,12.2,-10.442218514));
#298869=CARTESIAN_POINT('Ctrl Pts',(-0.152662802000056,12.2,-10.440816951));
#298870=CARTESIAN_POINT('Ctrl Pts',(-0.152443212000056,12.2,-10.439423372));
#298871=CARTESIAN_POINT('Ctrl Pts',(-0.152226243000056,12.2,-10.4380378));
#298872=CARTESIAN_POINT('Ctrl Pts',(-0.152011884000055,12.2,-10.436660258));
#298873=CARTESIAN_POINT('Ctrl Pts',(-0.151800122000055,12.2,-10.435290769));
#298874=CARTESIAN_POINT('Ctrl Pts',(-0.151590948000055,12.2,-10.433929354));
#298875=CARTESIAN_POINT('Ctrl Pts',(-0.151384347000055,12.2,-10.43257604));
#298876=CARTESIAN_POINT('Ctrl Pts',(-0.151180310000055,12.2,-10.431230848));
#298877=CARTESIAN_POINT('Ctrl Pts',(-0.150978823000055,12.2,-10.429893802));
#298878=CARTESIAN_POINT('Ctrl Pts',(-0.150779876000057,12.2,-10.428564925));
#298879=CARTESIAN_POINT('Ctrl Pts',(-0.150583457000056,12.2,-10.427244241));
#298880=CARTESIAN_POINT('Ctrl Pts',(-0.150389553000055,12.2,-10.425931773));
#298881=CARTESIAN_POINT('Ctrl Pts',(-0.150198154000056,12.2,-10.424627545));
#298882=CARTESIAN_POINT('Ctrl Pts',(-0.150009246000057,12.2,-10.423331583));
#298883=CARTESIAN_POINT('Ctrl Pts',(-0.149822818000055,12.2,-10.422043907));
#298884=CARTESIAN_POINT('Ctrl Pts',(-0.149638856000056,12.2,-10.420764545));
#298885=CARTESIAN_POINT('Ctrl Pts',(-0.149457350000055,12.2,-10.419493518));
#298886=CARTESIAN_POINT('Ctrl Pts',(-0.149278286000056,12.2,-10.418230852));
#298887=CARTESIAN_POINT('Ctrl Pts',(-0.149101652000055,12.2,-10.416976571));
#298888=CARTESIAN_POINT('Ctrl Pts',(-0.148927437000056,12.2,-10.4157307));
#298889=CARTESIAN_POINT('Ctrl Pts',(-0.148755627000057,12.2,-10.414493262));
#298890=CARTESIAN_POINT('Ctrl Pts',(-0.148586210000056,12.2,-10.413264283));
#298891=CARTESIAN_POINT('Ctrl Pts',(-0.148419173000055,12.2,-10.412043788));
#298892=CARTESIAN_POINT('Ctrl Pts',(-0.148254502000055,12.2,-10.410831802));
#298893=CARTESIAN_POINT('Ctrl Pts',(-0.148092187000056,12.2,-10.409628348));
#298894=CARTESIAN_POINT('Ctrl Pts',(-0.147932214000056,12.2,-10.408433454));
#298895=CARTESIAN_POINT('Ctrl Pts',(-0.147774569000055,12.2,-10.407247142));
#298896=CARTESIAN_POINT('Ctrl Pts',(-0.147619240000055,12.2,-10.40606944));
#298897=CARTESIAN_POINT('Ctrl Pts',(-0.147466215000056,12.2,-10.404900372));
#298898=CARTESIAN_POINT('Ctrl Pts',(-0.147315478000056,12.2,-10.403739965));
#298899=CARTESIAN_POINT('Ctrl Pts',(-0.147167017000056,12.2,-10.402588242));
#298900=CARTESIAN_POINT('Ctrl Pts',(-0.147020820000057,12.2,-10.401445231));
#298901=CARTESIAN_POINT('Ctrl Pts',(-0.146876872000057,12.2,-10.400310957));
#298902=CARTESIAN_POINT('Ctrl Pts',(-0.146735160000055,12.2,-10.399185446));
#298903=CARTESIAN_POINT('Ctrl Pts',(-0.146595671000057,12.2,-10.398068726));
#298904=CARTESIAN_POINT('Ctrl Pts',(-0.146458391000056,12.2,-10.39696082));
#298905=CARTESIAN_POINT('Ctrl Pts',(-0.146323306000056,12.2,-10.395861756));
#298906=CARTESIAN_POINT('Ctrl Pts',(-0.146190404000055,12.2,-10.394771561));
#298907=CARTESIAN_POINT('Ctrl Pts',(-0.146059668000056,12.2,-10.39369026));
#298908=CARTESIAN_POINT('Ctrl Pts',(-0.145931087000056,12.2,-10.392617881));
#298909=CARTESIAN_POINT('Ctrl Pts',(-0.145804646000055,12.2,-10.39155445));
#298910=CARTESIAN_POINT('Ctrl Pts',(-0.145680330000056,12.2,-10.390499995));
#298911=CARTESIAN_POINT('Ctrl Pts',(-0.145558126000056,12.2,-10.389454543));
#298912=CARTESIAN_POINT('Ctrl Pts',(-0.145438020000055,12.2,-10.388418119));
#298913=CARTESIAN_POINT('Ctrl Pts',(-0.145319997000056,12.2,-10.387390753));
#298914=CARTESIAN_POINT('Ctrl Pts',(-0.145204042000057,12.2,-10.38637247));
#298915=CARTESIAN_POINT('Ctrl Pts',(-0.145090142000056,12.2,-10.3853633));
#298916=CARTESIAN_POINT('Ctrl Pts',(-0.144978281000055,12.2,-10.38436327));
#298917=CARTESIAN_POINT('Ctrl Pts',(-0.144868446000055,12.2,-10.383372406));
#298918=CARTESIAN_POINT('Ctrl Pts',(-0.144760620000056,12.2,-10.382390738));
#298919=CARTESIAN_POINT('Ctrl Pts',(-0.144654791000055,12.2,-10.381418293));
#298920=CARTESIAN_POINT('Ctrl Pts',(-0.144550942000056,12.2,-10.380455099));
#298921=CARTESIAN_POINT('Ctrl Pts',(-0.144449058000056,12.2,-10.379501186));
#298922=CARTESIAN_POINT('Ctrl Pts',(-0.144349125000056,12.2,-10.378556581));
#298923=CARTESIAN_POINT('Ctrl Pts',(-0.144251127000056,12.2,-10.377621314));
#298924=CARTESIAN_POINT('Ctrl Pts',(-0.144155050000055,12.2,-10.376695412));
#298925=CARTESIAN_POINT('Ctrl Pts',(-0.144061421000057,12.2,-10.375784183));
#298926=CARTESIAN_POINT('Ctrl Pts',(-0.143988114000055,12.2,-10.375063685));
#298927=CARTESIAN_POINT('Ctrl Pts',(-0.143934095000056,12.2,-10.37452879));
#298928=CARTESIAN_POINT('Ctrl Pts',(-0.143898619000057,12.2,-10.374175763));
#298929=CARTESIAN_POINT('Ctrl Pts',(-0.143881228000057,12.2,-10.374002275));
#298930=CARTESIAN_POINT('Ctrl Pts',(-1.18690176600006,15.2,-10.306885524));
#298931=CARTESIAN_POINT('Ctrl Pts',(-1.18690176600006,11.6,-10.306885524));
#298932=CARTESIAN_POINT('Ctrl Pts',(-1.18690675400006,15.2,-10.307059811));
#298933=CARTESIAN_POINT('Ctrl Pts',(-1.18690675400006,11.6,-10.307059811));
#298934=CARTESIAN_POINT('Ctrl Pts',(-1.18691681600006,15.2,-10.307414474));
#298935=CARTESIAN_POINT('Ctrl Pts',(-1.18691681600006,11.6,-10.307414474));
#298936=CARTESIAN_POINT('Ctrl Pts',(-1.18693179800006,15.2,-10.30795188));
#298937=CARTESIAN_POINT('Ctrl Pts',(-1.18693179800006,11.6,-10.30795188));
#298938=CARTESIAN_POINT('Ctrl Pts',(-1.18695144000006,15.2,-10.30867583));
#298939=CARTESIAN_POINT('Ctrl Pts',(-1.18695144000006,11.6,-10.30867583));
#298940=CARTESIAN_POINT('Ctrl Pts',(-1.18697537100006,15.2,-10.309591544));
#298941=CARTESIAN_POINT('Ctrl Pts',(-1.18697537100006,11.6,-10.309591544));
#298942=CARTESIAN_POINT('Ctrl Pts',(-1.18699875600006,15.2,-10.310522124));
#298943=CARTESIAN_POINT('Ctrl Pts',(-1.18699875600006,11.6,-10.310522124));
#298944=CARTESIAN_POINT('Ctrl Pts',(-1.18702143600006,15.2,-10.311462239));
#298945=CARTESIAN_POINT('Ctrl Pts',(-1.18702143600006,11.6,-10.311462239));
#298946=CARTESIAN_POINT('Ctrl Pts',(-1.18704339300006,15.2,-10.312411861));
#298947=CARTESIAN_POINT('Ctrl Pts',(-1.18704339300006,11.6,-10.312411861));
#298948=CARTESIAN_POINT('Ctrl Pts',(-1.18706461000005,15.2,-10.313370965));
#298949=CARTESIAN_POINT('Ctrl Pts',(-1.18706461000005,11.6,-10.313370965));
#298950=CARTESIAN_POINT('Ctrl Pts',(-1.18708506600006,15.2,-10.314339525));
#298951=CARTESIAN_POINT('Ctrl Pts',(-1.18708506600006,11.6,-10.314339525));
#298952=CARTESIAN_POINT('Ctrl Pts',(-1.18710474400006,15.2,-10.315317513));
#298953=CARTESIAN_POINT('Ctrl Pts',(-1.18710474400006,11.6,-10.315317513));
#298954=CARTESIAN_POINT('Ctrl Pts',(-1.18712362500006,15.2,-10.316304905));
#298955=CARTESIAN_POINT('Ctrl Pts',(-1.18712362500006,11.6,-10.316304905));
#298956=CARTESIAN_POINT('Ctrl Pts',(-1.18714169000006,15.2,-10.317301674));
#298957=CARTESIAN_POINT('Ctrl Pts',(-1.18714169000006,11.6,-10.317301674));
#298958=CARTESIAN_POINT('Ctrl Pts',(-1.18715892200006,15.2,-10.318307793));
#298959=CARTESIAN_POINT('Ctrl Pts',(-1.18715892200006,11.6,-10.318307793));
#298960=CARTESIAN_POINT('Ctrl Pts',(-1.18717530200006,15.2,-10.319323239));
#298961=CARTESIAN_POINT('Ctrl Pts',(-1.18717530200006,11.6,-10.319323239));
#298962=CARTESIAN_POINT('Ctrl Pts',(-1.18719081400006,15.2,-10.320347984));
#298963=CARTESIAN_POINT('Ctrl Pts',(-1.18719081400006,11.6,-10.320347984));
#298964=CARTESIAN_POINT('Ctrl Pts',(-1.18720543700006,15.2,-10.321382005));
#298965=CARTESIAN_POINT('Ctrl Pts',(-1.18720543700006,11.6,-10.321382005));
#298966=CARTESIAN_POINT('Ctrl Pts',(-1.18721915500006,15.2,-10.322425274));
#298967=CARTESIAN_POINT('Ctrl Pts',(-1.18721915500006,11.6,-10.322425274));
#298968=CARTESIAN_POINT('Ctrl Pts',(-1.18723195100006,15.2,-10.323477767));
#298969=CARTESIAN_POINT('Ctrl Pts',(-1.18723195100006,11.6,-10.323477767));
#298970=CARTESIAN_POINT('Ctrl Pts',(-1.18724380600006,15.2,-10.324539459));
#298971=CARTESIAN_POINT('Ctrl Pts',(-1.18724380600006,11.6,-10.324539459));
#298972=CARTESIAN_POINT('Ctrl Pts',(-1.18725470300006,15.2,-10.325610325));
#298973=CARTESIAN_POINT('Ctrl Pts',(-1.18725470300006,11.6,-10.325610325));
#298974=CARTESIAN_POINT('Ctrl Pts',(-1.18726462500006,15.2,-10.326690339));
#298975=CARTESIAN_POINT('Ctrl Pts',(-1.18726462500006,11.6,-10.326690339));
#298976=CARTESIAN_POINT('Ctrl Pts',(-1.18727355500006,15.2,-10.327779477));
#298977=CARTESIAN_POINT('Ctrl Pts',(-1.18727355500006,11.6,-10.327779477));
#298978=CARTESIAN_POINT('Ctrl Pts',(-1.18728147400006,15.2,-10.328877716));
#298979=CARTESIAN_POINT('Ctrl Pts',(-1.18728147400006,11.6,-10.328877716));
#298980=CARTESIAN_POINT('Ctrl Pts',(-1.18728836700006,15.2,-10.329985028));
#298981=CARTESIAN_POINT('Ctrl Pts',(-1.18728836700006,11.6,-10.329985028));
#298982=CARTESIAN_POINT('Ctrl Pts',(-1.18729421500006,15.2,-10.331101391));
#298983=CARTESIAN_POINT('Ctrl Pts',(-1.18729421500006,11.6,-10.331101391));
#298984=CARTESIAN_POINT('Ctrl Pts',(-1.18729900200006,15.2,-10.33222678));
#298985=CARTESIAN_POINT('Ctrl Pts',(-1.18729900200006,11.6,-10.33222678));
#298986=CARTESIAN_POINT('Ctrl Pts',(-1.18730271200006,15.2,-10.333361171));
#298987=CARTESIAN_POINT('Ctrl Pts',(-1.18730271200006,11.6,-10.333361171));
#298988=CARTESIAN_POINT('Ctrl Pts',(-1.18730532700006,15.2,-10.33450454));
#298989=CARTESIAN_POINT('Ctrl Pts',(-1.18730532700006,11.6,-10.33450454));
#298990=CARTESIAN_POINT('Ctrl Pts',(-1.18730683000006,15.2,-10.335656862));
#298991=CARTESIAN_POINT('Ctrl Pts',(-1.18730683000006,11.6,-10.335656862));
#298992=CARTESIAN_POINT('Ctrl Pts',(-1.18730720600006,15.2,-10.336818112));
#298993=CARTESIAN_POINT('Ctrl Pts',(-1.18730720600006,11.6,-10.336818112));
#298994=CARTESIAN_POINT('Ctrl Pts',(-1.18730643800006,15.2,-10.33798827));
#298995=CARTESIAN_POINT('Ctrl Pts',(-1.18730643800006,11.6,-10.33798827));
#298996=CARTESIAN_POINT('Ctrl Pts',(-1.18730450900006,15.2,-10.339167308));
#298997=CARTESIAN_POINT('Ctrl Pts',(-1.18730450900006,11.6,-10.339167308));
#298998=CARTESIAN_POINT('Ctrl Pts',(-1.18730140200006,15.2,-10.340355206));
#298999=CARTESIAN_POINT('Ctrl Pts',(-1.18730140200006,11.6,-10.340355206));
#299000=CARTESIAN_POINT('Ctrl Pts',(-1.18729710300006,15.2,-10.341551938));
#299001=CARTESIAN_POINT('Ctrl Pts',(-1.18729710300006,11.6,-10.341551938));
#299002=CARTESIAN_POINT('Ctrl Pts',(-1.18729159300006,15.2,-10.342757481));
#299003=CARTESIAN_POINT('Ctrl Pts',(-1.18729159300006,11.6,-10.342757481));
#299004=CARTESIAN_POINT('Ctrl Pts',(-1.18728485900006,15.2,-10.343971813));
#299005=CARTESIAN_POINT('Ctrl Pts',(-1.18728485900006,11.6,-10.343971813));
#299006=CARTESIAN_POINT('Ctrl Pts',(-1.18727688300006,15.2,-10.345194909));
#299007=CARTESIAN_POINT('Ctrl Pts',(-1.18727688300006,11.6,-10.345194909));
#299008=CARTESIAN_POINT('Ctrl Pts',(-1.18726765000006,15.2,-10.346426747));
#299009=CARTESIAN_POINT('Ctrl Pts',(-1.18726765000006,11.6,-10.346426747));
#299010=CARTESIAN_POINT('Ctrl Pts',(-1.18725714300006,15.2,-10.347667304));
#299011=CARTESIAN_POINT('Ctrl Pts',(-1.18725714300006,11.6,-10.347667304));
#299012=CARTESIAN_POINT('Ctrl Pts',(-1.18724534800006,15.2,-10.348916556));
#299013=CARTESIAN_POINT('Ctrl Pts',(-1.18724534800006,11.6,-10.348916556));
#299014=CARTESIAN_POINT('Ctrl Pts',(-1.18723224800006,15.2,-10.350174481));
#299015=CARTESIAN_POINT('Ctrl Pts',(-1.18723224800006,11.6,-10.350174481));
#299016=CARTESIAN_POINT('Ctrl Pts',(-1.18721782700006,15.2,-10.351441055));
#299017=CARTESIAN_POINT('Ctrl Pts',(-1.18721782700006,11.6,-10.351441055));
#299018=CARTESIAN_POINT('Ctrl Pts',(-1.18720207100006,15.2,-10.352716257));
#299019=CARTESIAN_POINT('Ctrl Pts',(-1.18720207100006,11.6,-10.352716257));
#299020=CARTESIAN_POINT('Ctrl Pts',(-1.18718496500006,15.2,-10.354000065));
#299021=CARTESIAN_POINT('Ctrl Pts',(-1.18718496500006,11.6,-10.354000065));
#299022=CARTESIAN_POINT('Ctrl Pts',(-1.18716649200006,15.2,-10.355292454));
#299023=CARTESIAN_POINT('Ctrl Pts',(-1.18716649200006,11.6,-10.355292454));
#299024=CARTESIAN_POINT('Ctrl Pts',(-1.18714663700006,15.2,-10.356593403));
#299025=CARTESIAN_POINT('Ctrl Pts',(-1.18714663700006,11.6,-10.356593403));
#299026=CARTESIAN_POINT('Ctrl Pts',(-1.18712538600006,15.2,-10.35790289));
#299027=CARTESIAN_POINT('Ctrl Pts',(-1.18712538600006,11.6,-10.35790289));
#299028=CARTESIAN_POINT('Ctrl Pts',(-1.18710272200006,15.2,-10.359220891));
#299029=CARTESIAN_POINT('Ctrl Pts',(-1.18710272200006,11.6,-10.359220891));
#299030=CARTESIAN_POINT('Ctrl Pts',(-1.18707863200005,15.2,-10.360547387));
#299031=CARTESIAN_POINT('Ctrl Pts',(-1.18707863200005,11.6,-10.360547387));
#299032=CARTESIAN_POINT('Ctrl Pts',(-1.18705310000006,15.2,-10.361882353));
#299033=CARTESIAN_POINT('Ctrl Pts',(-1.18705310000006,11.6,-10.361882353));
#299034=CARTESIAN_POINT('Ctrl Pts',(-1.18702611100006,15.2,-10.363225769));
#299035=CARTESIAN_POINT('Ctrl Pts',(-1.18702611100006,11.6,-10.363225769));
#299036=CARTESIAN_POINT('Ctrl Pts',(-1.18699765000006,15.2,-10.364577611));
#299037=CARTESIAN_POINT('Ctrl Pts',(-1.18699765000006,11.6,-10.364577611));
#299038=CARTESIAN_POINT('Ctrl Pts',(-1.18696770400006,15.2,-10.36593786));
#299039=CARTESIAN_POINT('Ctrl Pts',(-1.18696770400006,11.6,-10.36593786));
#299040=CARTESIAN_POINT('Ctrl Pts',(-1.18693625600006,15.2,-10.367306493));
#299041=CARTESIAN_POINT('Ctrl Pts',(-1.18693625600006,11.6,-10.367306493));
#299042=CARTESIAN_POINT('Ctrl Pts',(-1.18690329400006,15.2,-10.368683487));
#299043=CARTESIAN_POINT('Ctrl Pts',(-1.18690329400006,11.6,-10.368683487));
#299044=CARTESIAN_POINT('Ctrl Pts',(-1.18686880100006,15.2,-10.370068823));
#299045=CARTESIAN_POINT('Ctrl Pts',(-1.18686880100006,11.6,-10.370068823));
#299046=CARTESIAN_POINT('Ctrl Pts',(-1.18683276400006,15.2,-10.371462478));
#299047=CARTESIAN_POINT('Ctrl Pts',(-1.18683276400006,11.6,-10.371462478));
#299048=CARTESIAN_POINT('Ctrl Pts',(-1.18679516800006,15.2,-10.372864431));
#299049=CARTESIAN_POINT('Ctrl Pts',(-1.18679516800006,11.6,-10.372864431));
#299050=CARTESIAN_POINT('Ctrl Pts',(-1.18675600000006,15.2,-10.374274661));
#299051=CARTESIAN_POINT('Ctrl Pts',(-1.18675600000006,11.6,-10.374274661));
#299052=CARTESIAN_POINT('Ctrl Pts',(-1.18671524400006,15.2,-10.375693145));
#299053=CARTESIAN_POINT('Ctrl Pts',(-1.18671524400006,11.6,-10.375693145));
#299054=CARTESIAN_POINT('Ctrl Pts',(-1.18667288600006,15.2,-10.377119865));
#299055=CARTESIAN_POINT('Ctrl Pts',(-1.18667288600006,11.6,-10.377119865));
#299056=CARTESIAN_POINT('Ctrl Pts',(-1.18662891500006,15.2,-10.378554798));
#299057=CARTESIAN_POINT('Ctrl Pts',(-1.18662891500006,11.6,-10.378554798));
#299058=CARTESIAN_POINT('Ctrl Pts',(-1.18658331200006,15.2,-10.379997923));
#299059=CARTESIAN_POINT('Ctrl Pts',(-1.18658331200006,11.6,-10.379997923));
#299060=CARTESIAN_POINT('Ctrl Pts',(-1.18653606700006,15.2,-10.38144922));
#299061=CARTESIAN_POINT('Ctrl Pts',(-1.18653606700006,11.6,-10.38144922));
#299062=CARTESIAN_POINT('Ctrl Pts',(-1.18648716500006,15.2,-10.382908667));
#299063=CARTESIAN_POINT('Ctrl Pts',(-1.18648716500006,11.6,-10.382908667));
#299064=CARTESIAN_POINT('Ctrl Pts',(-1.18643659200006,15.2,-10.384376245));
#299065=CARTESIAN_POINT('Ctrl Pts',(-1.18643659200006,11.6,-10.384376245));
#299066=CARTESIAN_POINT('Ctrl Pts',(-1.18638433400006,15.2,-10.385851932));
#299067=CARTESIAN_POINT('Ctrl Pts',(-1.18638433400006,11.6,-10.385851932));
#299068=CARTESIAN_POINT('Ctrl Pts',(-1.18633037700006,15.2,-10.387335708));
#299069=CARTESIAN_POINT('Ctrl Pts',(-1.18633037700006,11.6,-10.387335708));
#299070=CARTESIAN_POINT('Ctrl Pts',(-1.18627470900006,15.2,-10.388827552));
#299071=CARTESIAN_POINT('Ctrl Pts',(-1.18627470900006,11.6,-10.388827552));
#299072=CARTESIAN_POINT('Ctrl Pts',(-1.18621731600006,15.2,-10.390327444));
#299073=CARTESIAN_POINT('Ctrl Pts',(-1.18621731600006,11.6,-10.390327444));
#299074=CARTESIAN_POINT('Ctrl Pts',(-1.18615818400006,15.2,-10.391835365));
#299075=CARTESIAN_POINT('Ctrl Pts',(-1.18615818400006,11.6,-10.391835365));
#299076=CARTESIAN_POINT('Ctrl Pts',(-1.18609729900006,15.2,-10.393351292));
#299077=CARTESIAN_POINT('Ctrl Pts',(-1.18609729900006,11.6,-10.393351292));
#299078=CARTESIAN_POINT('Ctrl Pts',(-1.18603464900006,15.2,-10.394875206));
#299079=CARTESIAN_POINT('Ctrl Pts',(-1.18603464900006,11.6,-10.394875206));
#299080=CARTESIAN_POINT('Ctrl Pts',(-1.18597022000006,15.2,-10.396407088));
#299081=CARTESIAN_POINT('Ctrl Pts',(-1.18597022000006,11.6,-10.396407088));
#299082=CARTESIAN_POINT('Ctrl Pts',(-1.18590399800006,15.2,-10.397946917));
#299083=CARTESIAN_POINT('Ctrl Pts',(-1.18590399800006,11.6,-10.397946917));
#299084=CARTESIAN_POINT('Ctrl Pts',(-1.18583597200006,15.2,-10.399494673));
#299085=CARTESIAN_POINT('Ctrl Pts',(-1.18583597200006,11.6,-10.399494673));
#299086=CARTESIAN_POINT('Ctrl Pts',(-1.18576612800006,15.2,-10.401050335));
#299087=CARTESIAN_POINT('Ctrl Pts',(-1.18576612800006,11.6,-10.401050335));
#299088=CARTESIAN_POINT('Ctrl Pts',(-1.18569445200006,15.2,-10.402613886));
#299089=CARTESIAN_POINT('Ctrl Pts',(-1.18569445200006,11.6,-10.402613886));
#299090=CARTESIAN_POINT('Ctrl Pts',(-1.18562093200006,15.2,-10.404185304));
#299091=CARTESIAN_POINT('Ctrl Pts',(-1.18562093200006,11.6,-10.404185304));
#299092=CARTESIAN_POINT('Ctrl Pts',(-1.18554555500006,15.2,-10.40576457));
#299093=CARTESIAN_POINT('Ctrl Pts',(-1.18554555500006,11.6,-10.40576457));
#299094=CARTESIAN_POINT('Ctrl Pts',(-1.18546830800006,15.2,-10.407351665));
#299095=CARTESIAN_POINT('Ctrl Pts',(-1.18546830800006,11.6,-10.407351665));
#299096=CARTESIAN_POINT('Ctrl Pts',(-1.18538917800006,15.2,-10.408946568));
#299097=CARTESIAN_POINT('Ctrl Pts',(-1.18538917800006,11.6,-10.408946568));
#299098=CARTESIAN_POINT('Ctrl Pts',(-1.18530815300006,15.2,-10.410549261));
#299099=CARTESIAN_POINT('Ctrl Pts',(-1.18530815300006,11.6,-10.410549261));
#299100=CARTESIAN_POINT('Ctrl Pts',(-1.18522522000006,15.2,-10.412159724));
#299101=CARTESIAN_POINT('Ctrl Pts',(-1.18522522000006,11.6,-10.412159724));
#299102=CARTESIAN_POINT('Ctrl Pts',(-1.18514036600006,15.2,-10.413777937));
#299103=CARTESIAN_POINT('Ctrl Pts',(-1.18514036600006,11.6,-10.413777937));
#299104=CARTESIAN_POINT('Ctrl Pts',(-1.18505357900006,15.2,-10.415403882));
#299105=CARTESIAN_POINT('Ctrl Pts',(-1.18505357900006,11.6,-10.415403882));
#299106=CARTESIAN_POINT('Ctrl Pts',(-1.18496484700006,15.2,-10.417037539));
#299107=CARTESIAN_POINT('Ctrl Pts',(-1.18496484700006,11.6,-10.417037539));
#299108=CARTESIAN_POINT('Ctrl Pts',(-1.18487415700006,15.2,-10.418678889));
#299109=CARTESIAN_POINT('Ctrl Pts',(-1.18487415700006,11.6,-10.418678889));
#299110=CARTESIAN_POINT('Ctrl Pts',(-1.18478149700006,15.2,-10.420327913));
#299111=CARTESIAN_POINT('Ctrl Pts',(-1.18478149700006,11.6,-10.420327913));
#299112=CARTESIAN_POINT('Ctrl Pts',(-1.18468685300006,15.2,-10.421984593));
#299113=CARTESIAN_POINT('Ctrl Pts',(-1.18468685300006,11.6,-10.421984593));
#299114=CARTESIAN_POINT('Ctrl Pts',(-1.18459021600006,15.2,-10.423648908));
#299115=CARTESIAN_POINT('Ctrl Pts',(-1.18459021600006,11.6,-10.423648908));
#299116=CARTESIAN_POINT('Ctrl Pts',(-1.18449157100006,15.2,-10.425320841));
#299117=CARTESIAN_POINT('Ctrl Pts',(-1.18449157100006,11.6,-10.425320841));
#299118=CARTESIAN_POINT('Ctrl Pts',(-1.18439090700006,15.2,-10.427000372));
#299119=CARTESIAN_POINT('Ctrl Pts',(-1.18439090700006,11.6,-10.427000372));
#299120=CARTESIAN_POINT('Ctrl Pts',(-1.18428821200006,15.2,-10.428687482));
#299121=CARTESIAN_POINT('Ctrl Pts',(-1.18428821200006,11.6,-10.428687482));
#299122=CARTESIAN_POINT('Ctrl Pts',(-1.18418347300006,15.2,-10.430382155));
#299123=CARTESIAN_POINT('Ctrl Pts',(-1.18418347300006,11.6,-10.430382155));
#299124=CARTESIAN_POINT('Ctrl Pts',(-1.18407668100006,15.2,-10.432084369));
#299125=CARTESIAN_POINT('Ctrl Pts',(-1.18407668100006,11.6,-10.432084369));
#299126=CARTESIAN_POINT('Ctrl Pts',(-1.18396782000006,15.2,-10.433794107));
#299127=CARTESIAN_POINT('Ctrl Pts',(-1.18396782000006,11.6,-10.433794107));
#299128=CARTESIAN_POINT('Ctrl Pts',(-1.18385688100005,15.2,-10.435511351));
#299129=CARTESIAN_POINT('Ctrl Pts',(-1.18385688100005,11.6,-10.435511351));
#299130=CARTESIAN_POINT('Ctrl Pts',(-1.18374385200006,15.2,-10.437236082));
#299131=CARTESIAN_POINT('Ctrl Pts',(-1.18374385200006,11.6,-10.437236082));
#299132=CARTESIAN_POINT('Ctrl Pts',(-1.18362872000006,15.2,-10.438968281));
#299133=CARTESIAN_POINT('Ctrl Pts',(-1.18362872000006,11.6,-10.438968281));
#299134=CARTESIAN_POINT('Ctrl Pts',(-1.18351147300006,15.2,-10.440707931));
#299135=CARTESIAN_POINT('Ctrl Pts',(-1.18351147300006,11.6,-10.440707931));
#299136=CARTESIAN_POINT('Ctrl Pts',(-1.18339210200006,15.2,-10.442455012));
#299137=CARTESIAN_POINT('Ctrl Pts',(-1.18339210200006,11.6,-10.442455012));
#299138=CARTESIAN_POINT('Ctrl Pts',(-1.18327059400006,15.2,-10.444209508));
#299139=CARTESIAN_POINT('Ctrl Pts',(-1.18327059400006,11.6,-10.444209508));
#299140=CARTESIAN_POINT('Ctrl Pts',(-1.18314693700006,15.2,-10.4459714));
#299141=CARTESIAN_POINT('Ctrl Pts',(-1.18314693700006,11.6,-10.4459714));
#299142=CARTESIAN_POINT('Ctrl Pts',(-1.18302111900006,15.2,-10.44774067));
#299143=CARTESIAN_POINT('Ctrl Pts',(-1.18302111900006,11.6,-10.44774067));
#299144=CARTESIAN_POINT('Ctrl Pts',(-1.18289313000006,15.2,-10.449517299));
#299145=CARTESIAN_POINT('Ctrl Pts',(-1.18289313000006,11.6,-10.449517299));
#299146=CARTESIAN_POINT('Ctrl Pts',(-1.18276295900006,15.2,-10.45130127));
#299147=CARTESIAN_POINT('Ctrl Pts',(-1.18276295900006,11.6,-10.45130127));
#299148=CARTESIAN_POINT('Ctrl Pts',(-1.18263059300006,15.2,-10.453092566));
#299149=CARTESIAN_POINT('Ctrl Pts',(-1.18263059300006,11.6,-10.453092566));
#299150=CARTESIAN_POINT('Ctrl Pts',(-1.18249602200006,15.2,-10.454891167));
#299151=CARTESIAN_POINT('Ctrl Pts',(-1.18249602200006,11.6,-10.454891167));
#299152=CARTESIAN_POINT('Ctrl Pts',(-1.18235923500006,15.2,-10.456697057));
#299153=CARTESIAN_POINT('Ctrl Pts',(-1.18235923500006,11.6,-10.456697057));
#299154=CARTESIAN_POINT('Ctrl Pts',(-1.18222021900006,15.2,-10.458510217));
#299155=CARTESIAN_POINT('Ctrl Pts',(-1.18222021900006,11.6,-10.458510217));
#299156=CARTESIAN_POINT('Ctrl Pts',(-1.18207896500006,15.2,-10.460330631));
#299157=CARTESIAN_POINT('Ctrl Pts',(-1.18207896500006,11.6,-10.460330631));
#299158=CARTESIAN_POINT('Ctrl Pts',(-1.18193546100006,15.2,-10.46215828));
#299159=CARTESIAN_POINT('Ctrl Pts',(-1.18193546100006,11.6,-10.46215828));
#299160=CARTESIAN_POINT('Ctrl Pts',(-1.18178969600006,15.2,-10.463993146));
#299161=CARTESIAN_POINT('Ctrl Pts',(-1.18178969600006,11.6,-10.463993146));
#299162=CARTESIAN_POINT('Ctrl Pts',(-1.18164165900006,15.2,-10.465835214));
#299163=CARTESIAN_POINT('Ctrl Pts',(-1.18164165900006,11.6,-10.465835214));
#299164=CARTESIAN_POINT('Ctrl Pts',(-1.18149134000006,15.2,-10.467684464));
#299165=CARTESIAN_POINT('Ctrl Pts',(-1.18149134000006,11.6,-10.467684464));
#299166=CARTESIAN_POINT('Ctrl Pts',(-1.18133872600006,15.2,-10.469540881));
#299167=CARTESIAN_POINT('Ctrl Pts',(-1.18133872600006,11.6,-10.469540881));
#299168=CARTESIAN_POINT('Ctrl Pts',(-1.18118380900005,15.2,-10.471404445));
#299169=CARTESIAN_POINT('Ctrl Pts',(-1.18118380900005,11.6,-10.471404445));
#299170=CARTESIAN_POINT('Ctrl Pts',(-1.18102657700006,15.2,-10.473275141));
#299171=CARTESIAN_POINT('Ctrl Pts',(-1.18102657700006,11.6,-10.473275141));
#299172=CARTESIAN_POINT('Ctrl Pts',(-1.18086701900006,15.2,-10.475152951));
#299173=CARTESIAN_POINT('Ctrl Pts',(-1.18086701900006,11.6,-10.475152951));
#299174=CARTESIAN_POINT('Ctrl Pts',(-1.18070512400006,15.2,-10.477037856));
#299175=CARTESIAN_POINT('Ctrl Pts',(-1.18070512400006,11.6,-10.477037856));
#299176=CARTESIAN_POINT('Ctrl Pts',(-1.18054088200006,15.2,-10.478929842));
#299177=CARTESIAN_POINT('Ctrl Pts',(-1.18054088200006,11.6,-10.478929842));
#299178=CARTESIAN_POINT('Ctrl Pts',(-1.18037428300006,15.2,-10.480828891));
#299179=CARTESIAN_POINT('Ctrl Pts',(-1.18037428300006,11.6,-10.480828891));
#299180=CARTESIAN_POINT('Ctrl Pts',(-1.18020531600005,15.2,-10.482734985));
#299181=CARTESIAN_POINT('Ctrl Pts',(-1.18020531600005,11.6,-10.482734985));
#299182=CARTESIAN_POINT('Ctrl Pts',(-1.18003397000006,15.2,-10.484648109));
#299183=CARTESIAN_POINT('Ctrl Pts',(-1.18003397000006,11.6,-10.484648109));
#299184=CARTESIAN_POINT('Ctrl Pts',(-1.17986023500006,15.2,-10.486568243));
#299185=CARTESIAN_POINT('Ctrl Pts',(-1.17986023500006,11.6,-10.486568243));
#299186=CARTESIAN_POINT('Ctrl Pts',(-1.17968410100006,15.2,-10.488495373));
#299187=CARTESIAN_POINT('Ctrl Pts',(-1.17968410100006,11.6,-10.488495373));
#299188=CARTESIAN_POINT('Ctrl Pts',(-1.17950555800006,15.2,-10.49042948));
#299189=CARTESIAN_POINT('Ctrl Pts',(-1.17950555800006,11.6,-10.49042948));
#299190=CARTESIAN_POINT('Ctrl Pts',(-1.17932459300006,15.2,-10.49237055));
#299191=CARTESIAN_POINT('Ctrl Pts',(-1.17932459300006,11.6,-10.49237055));
#299192=CARTESIAN_POINT('Ctrl Pts',(-1.17914120000005,15.2,-10.494318563));
#299193=CARTESIAN_POINT('Ctrl Pts',(-1.17914120000005,11.6,-10.494318563));
#299194=CARTESIAN_POINT('Ctrl Pts',(-1.17895536600006,15.2,-10.496273505));
#299195=CARTESIAN_POINT('Ctrl Pts',(-1.17895536600006,11.6,-10.496273505));
#299196=CARTESIAN_POINT('Ctrl Pts',(-1.17876708000006,15.2,-10.498235359));
#299197=CARTESIAN_POINT('Ctrl Pts',(-1.17876708000006,11.6,-10.498235359));
#299198=CARTESIAN_POINT('Ctrl Pts',(-1.17857633500006,15.2,-10.500204108));
#299199=CARTESIAN_POINT('Ctrl Pts',(-1.17857633500006,11.6,-10.500204108));
#299200=CARTESIAN_POINT('Ctrl Pts',(-1.17838312000006,15.2,-10.502179735));
#299201=CARTESIAN_POINT('Ctrl Pts',(-1.17838312000006,11.6,-10.502179735));
#299202=CARTESIAN_POINT('Ctrl Pts',(-1.17818742300006,15.2,-10.504162225));
#299203=CARTESIAN_POINT('Ctrl Pts',(-1.17818742300006,11.6,-10.504162225));
#299204=CARTESIAN_POINT('Ctrl Pts',(-1.17798923600006,15.2,-10.506151559));
#299205=CARTESIAN_POINT('Ctrl Pts',(-1.17798923600006,11.6,-10.506151559));
#299206=CARTESIAN_POINT('Ctrl Pts',(-1.17778854800005,15.2,-10.508147723));
#299207=CARTESIAN_POINT('Ctrl Pts',(-1.17778854800005,11.6,-10.508147723));
#299208=CARTESIAN_POINT('Ctrl Pts',(-1.17758535000006,15.2,-10.510150702));
#299209=CARTESIAN_POINT('Ctrl Pts',(-1.17758535000006,11.6,-10.510150702));
#299210=CARTESIAN_POINT('Ctrl Pts',(-1.17737963100006,15.2,-10.512160476));
#299211=CARTESIAN_POINT('Ctrl Pts',(-1.17737963100006,11.6,-10.512160476));
#299212=CARTESIAN_POINT('Ctrl Pts',(-1.17717138300006,15.2,-10.514177031));
#299213=CARTESIAN_POINT('Ctrl Pts',(-1.17717138300006,11.6,-10.514177031));
#299214=CARTESIAN_POINT('Ctrl Pts',(-1.17696059500006,15.2,-10.51620035));
#299215=CARTESIAN_POINT('Ctrl Pts',(-1.17696059500006,11.6,-10.51620035));
#299216=CARTESIAN_POINT('Ctrl Pts',(-1.17674725700006,15.2,-10.518230419));
#299217=CARTESIAN_POINT('Ctrl Pts',(-1.17674725700006,11.6,-10.518230419));
#299218=CARTESIAN_POINT('Ctrl Pts',(-1.17653136000005,15.2,-10.520267219));
#299219=CARTESIAN_POINT('Ctrl Pts',(-1.17653136000005,11.6,-10.520267219));
#299220=CARTESIAN_POINT('Ctrl Pts',(-1.17631289500006,15.2,-10.522310736));
#299221=CARTESIAN_POINT('Ctrl Pts',(-1.17631289500006,11.6,-10.522310736));
#299222=CARTESIAN_POINT('Ctrl Pts',(-1.17609185100006,15.2,-10.524360953));
#299223=CARTESIAN_POINT('Ctrl Pts',(-1.17609185100006,11.6,-10.524360953));
#299224=CARTESIAN_POINT('Ctrl Pts',(-1.17586821800006,15.2,-10.526417854));
#299225=CARTESIAN_POINT('Ctrl Pts',(-1.17586821800006,11.6,-10.526417854));
#299226=CARTESIAN_POINT('Ctrl Pts',(-1.17564198900006,15.2,-10.528481425));
#299227=CARTESIAN_POINT('Ctrl Pts',(-1.17564198900006,11.6,-10.528481425));
#299228=CARTESIAN_POINT('Ctrl Pts',(-1.17541315400006,15.2,-10.530551648));
#299229=CARTESIAN_POINT('Ctrl Pts',(-1.17541315400006,11.6,-10.530551648));
#299230=CARTESIAN_POINT('Ctrl Pts',(-1.17518170100006,15.2,-10.532628509));
#299231=CARTESIAN_POINT('Ctrl Pts',(-1.17518170100006,11.6,-10.532628509));
#299232=CARTESIAN_POINT('Ctrl Pts',(-1.17494762300006,15.2,-10.534711991));
#299233=CARTESIAN_POINT('Ctrl Pts',(-1.17494762300006,11.6,-10.534711991));
#299234=CARTESIAN_POINT('Ctrl Pts',(-1.17471091000006,15.2,-10.536802078));
#299235=CARTESIAN_POINT('Ctrl Pts',(-1.17471091000006,11.6,-10.536802078));
#299236=CARTESIAN_POINT('Ctrl Pts',(-1.17447155200006,15.2,-10.538898756));
#299237=CARTESIAN_POINT('Ctrl Pts',(-1.17447155200006,11.6,-10.538898756));
#299238=CARTESIAN_POINT('Ctrl Pts',(-1.17422954200006,15.2,-10.541002007));
#299239=CARTESIAN_POINT('Ctrl Pts',(-1.17422954200006,11.6,-10.541002007));
#299240=CARTESIAN_POINT('Ctrl Pts',(-1.17398486900006,15.2,-10.543111818));
#299241=CARTESIAN_POINT('Ctrl Pts',(-1.17398486900006,11.6,-10.543111818));
#299242=CARTESIAN_POINT('Ctrl Pts',(-1.17373752300006,15.2,-10.545228173));
#299243=CARTESIAN_POINT('Ctrl Pts',(-1.17373752300006,11.6,-10.545228173));
#299244=CARTESIAN_POINT('Ctrl Pts',(-1.17348749700006,15.2,-10.547351055));
#299245=CARTESIAN_POINT('Ctrl Pts',(-1.17348749700006,11.6,-10.547351055));
#299246=CARTESIAN_POINT('Ctrl Pts',(-1.17323478100006,15.2,-10.549480449));
#299247=CARTESIAN_POINT('Ctrl Pts',(-1.17323478100006,11.6,-10.549480449));
#299248=CARTESIAN_POINT('Ctrl Pts',(-1.17297936500006,15.2,-10.551616341));
#299249=CARTESIAN_POINT('Ctrl Pts',(-1.17297936500006,11.6,-10.551616341));
#299250=CARTESIAN_POINT('Ctrl Pts',(-1.17272124100006,15.2,-10.553758714));
#299251=CARTESIAN_POINT('Ctrl Pts',(-1.17272124100006,11.6,-10.553758714));
#299252=CARTESIAN_POINT('Ctrl Pts',(-1.17246040000005,15.2,-10.555907555));
#299253=CARTESIAN_POINT('Ctrl Pts',(-1.17246040000005,11.6,-10.555907555));
#299254=CARTESIAN_POINT('Ctrl Pts',(-1.17219683200006,15.2,-10.558062846));
#299255=CARTESIAN_POINT('Ctrl Pts',(-1.17219683200006,11.6,-10.558062846));
#299256=CARTESIAN_POINT('Ctrl Pts',(-1.17193053000006,15.2,-10.560224572));
#299257=CARTESIAN_POINT('Ctrl Pts',(-1.17193053000006,11.6,-10.560224572));
#299258=CARTESIAN_POINT('Ctrl Pts',(-1.17166148400006,15.2,-10.562392721));
#299259=CARTESIAN_POINT('Ctrl Pts',(-1.17166148400006,11.6,-10.562392721));
#299260=CARTESIAN_POINT('Ctrl Pts',(-1.17138968600006,15.2,-10.564567275));
#299261=CARTESIAN_POINT('Ctrl Pts',(-1.17138968600006,11.6,-10.564567275));
#299262=CARTESIAN_POINT('Ctrl Pts',(-1.17111512500006,15.2,-10.56674822));
#299263=CARTESIAN_POINT('Ctrl Pts',(-1.17111512500006,11.6,-10.56674822));
#299264=CARTESIAN_POINT('Ctrl Pts',(-1.17083779500006,15.2,-10.568935539));
#299265=CARTESIAN_POINT('Ctrl Pts',(-1.17083779500006,11.6,-10.568935539));
#299266=CARTESIAN_POINT('Ctrl Pts',(-1.17055768500006,15.2,-10.57112922));
#299267=CARTESIAN_POINT('Ctrl Pts',(-1.17055768500006,11.6,-10.57112922));
#299268=CARTESIAN_POINT('Ctrl Pts',(-1.17027478800006,15.2,-10.573329247));
#299269=CARTESIAN_POINT('Ctrl Pts',(-1.17027478800006,11.6,-10.573329247));
#299270=CARTESIAN_POINT('Ctrl Pts',(-1.16998909400006,15.2,-10.575535603));
#299271=CARTESIAN_POINT('Ctrl Pts',(-1.16998909400006,11.6,-10.575535603));
#299272=CARTESIAN_POINT('Ctrl Pts',(-1.16970059600006,15.2,-10.577748277));
#299273=CARTESIAN_POINT('Ctrl Pts',(-1.16970059600006,11.6,-10.577748277));
#299274=CARTESIAN_POINT('Ctrl Pts',(-1.16940928400005,15.2,-10.57996725));
#299275=CARTESIAN_POINT('Ctrl Pts',(-1.16940928400005,11.6,-10.57996725));
#299276=CARTESIAN_POINT('Ctrl Pts',(-1.16911514900006,15.2,-10.582192511));
#299277=CARTESIAN_POINT('Ctrl Pts',(-1.16911514900006,11.6,-10.582192511));
#299278=CARTESIAN_POINT('Ctrl Pts',(-1.16881818600006,15.2,-10.584424042));
#299279=CARTESIAN_POINT('Ctrl Pts',(-1.16881818600006,11.6,-10.584424042));
#299280=CARTESIAN_POINT('Ctrl Pts',(-1.16851838200006,15.2,-10.586661831));
#299281=CARTESIAN_POINT('Ctrl Pts',(-1.16851838200006,11.6,-10.586661831));
#299282=CARTESIAN_POINT('Ctrl Pts',(-1.16821573100006,15.2,-10.588905861));
#299283=CARTESIAN_POINT('Ctrl Pts',(-1.16821573100006,11.6,-10.588905861));
#299284=CARTESIAN_POINT('Ctrl Pts',(-1.16791022400006,15.2,-10.591156119));
#299285=CARTESIAN_POINT('Ctrl Pts',(-1.16791022400006,11.6,-10.591156119));
#299286=CARTESIAN_POINT('Ctrl Pts',(-1.16760185300006,15.2,-10.59341259));
#299287=CARTESIAN_POINT('Ctrl Pts',(-1.16760185300006,11.6,-10.59341259));
#299288=CARTESIAN_POINT('Ctrl Pts',(-1.16729061000005,15.2,-10.595675259));
#299289=CARTESIAN_POINT('Ctrl Pts',(-1.16729061000005,11.6,-10.595675259));
#299290=CARTESIAN_POINT('Ctrl Pts',(-1.16697648600006,15.2,-10.597944112));
#299291=CARTESIAN_POINT('Ctrl Pts',(-1.16697648600006,11.6,-10.597944112));
#299292=CARTESIAN_POINT('Ctrl Pts',(-1.16665947300006,15.2,-10.600219134));
#299293=CARTESIAN_POINT('Ctrl Pts',(-1.16665947300006,11.6,-10.600219134));
#299294=CARTESIAN_POINT('Ctrl Pts',(-1.16633956300006,15.2,-10.60250031));
#299295=CARTESIAN_POINT('Ctrl Pts',(-1.16633956300006,11.6,-10.60250031));
#299296=CARTESIAN_POINT('Ctrl Pts',(-1.16601674700005,15.2,-10.604787626));
#299297=CARTESIAN_POINT('Ctrl Pts',(-1.16601674700005,11.6,-10.604787626));
#299298=CARTESIAN_POINT('Ctrl Pts',(-1.16569101800006,15.2,-10.60708107));
#299299=CARTESIAN_POINT('Ctrl Pts',(-1.16569101800006,11.6,-10.60708107));
#299300=CARTESIAN_POINT('Ctrl Pts',(-1.16536236700005,15.2,-10.609380624));
#299301=CARTESIAN_POINT('Ctrl Pts',(-1.16536236700005,11.6,-10.609380624));
#299302=CARTESIAN_POINT('Ctrl Pts',(-1.16503078700006,15.2,-10.611686275));
#299303=CARTESIAN_POINT('Ctrl Pts',(-1.16503078700006,11.6,-10.611686275));
#299304=CARTESIAN_POINT('Ctrl Pts',(-1.16469626800005,15.2,-10.613998011));
#299305=CARTESIAN_POINT('Ctrl Pts',(-1.16469626800005,11.6,-10.613998011));
#299306=CARTESIAN_POINT('Ctrl Pts',(-1.16435880400006,15.2,-10.616315814));
#299307=CARTESIAN_POINT('Ctrl Pts',(-1.16435880400006,11.6,-10.616315814));
#299308=CARTESIAN_POINT('Ctrl Pts',(-1.16401838400006,15.2,-10.618639673));
#299309=CARTESIAN_POINT('Ctrl Pts',(-1.16401838400006,11.6,-10.618639673));
#299310=CARTESIAN_POINT('Ctrl Pts',(-1.16367500500006,15.2,-10.620969571));
#299311=CARTESIAN_POINT('Ctrl Pts',(-1.16367500500006,11.6,-10.620969571));
#299312=CARTESIAN_POINT('Ctrl Pts',(-1.16332865500006,15.2,-10.623305496));
#299313=CARTESIAN_POINT('Ctrl Pts',(-1.16332865500006,11.6,-10.623305496));
#299314=CARTESIAN_POINT('Ctrl Pts',(-1.16297932800006,15.2,-10.625647433));
#299315=CARTESIAN_POINT('Ctrl Pts',(-1.16297932800006,11.6,-10.625647433));
#299316=CARTESIAN_POINT('Ctrl Pts',(-1.16262701500006,15.2,-10.627995369));
#299317=CARTESIAN_POINT('Ctrl Pts',(-1.16262701500006,11.6,-10.627995369));
#299318=CARTESIAN_POINT('Ctrl Pts',(-1.16227171000006,15.2,-10.630349288));
#299319=CARTESIAN_POINT('Ctrl Pts',(-1.16227171000006,11.6,-10.630349288));
#299320=CARTESIAN_POINT('Ctrl Pts',(-1.16191340300006,15.2,-10.632709178));
#299321=CARTESIAN_POINT('Ctrl Pts',(-1.16191340300006,11.6,-10.632709178));
#299322=CARTESIAN_POINT('Ctrl Pts',(-1.16155208700006,15.2,-10.635075024));
#299323=CARTESIAN_POINT('Ctrl Pts',(-1.16155208700006,11.6,-10.635075024));
#299324=CARTESIAN_POINT('Ctrl Pts',(-1.16118775500005,15.2,-10.637446813));
#299325=CARTESIAN_POINT('Ctrl Pts',(-1.16118775500005,11.6,-10.637446813));
#299326=CARTESIAN_POINT('Ctrl Pts',(-1.16082039900006,15.2,-10.639824529));
#299327=CARTESIAN_POINT('Ctrl Pts',(-1.16082039900006,11.6,-10.639824529));
#299328=CARTESIAN_POINT('Ctrl Pts',(-1.16045001000006,15.2,-10.642208161));
#299329=CARTESIAN_POINT('Ctrl Pts',(-1.16045001000006,11.6,-10.642208161));
#299330=CARTESIAN_POINT('Ctrl Pts',(-1.16007658300005,15.2,-10.644597692));
#299331=CARTESIAN_POINT('Ctrl Pts',(-1.16007658300005,11.6,-10.644597692));
#299332=CARTESIAN_POINT('Ctrl Pts',(-1.15970010900006,15.2,-10.646993112));
#299333=CARTESIAN_POINT('Ctrl Pts',(-1.15970010900006,11.6,-10.646993112));
#299334=CARTESIAN_POINT('Ctrl Pts',(-1.15932057900006,15.2,-10.649394405));
#299335=CARTESIAN_POINT('Ctrl Pts',(-1.15932057900006,11.6,-10.649394405));
#299336=CARTESIAN_POINT('Ctrl Pts',(-1.15893798800006,15.2,-10.651801557));
#299337=CARTESIAN_POINT('Ctrl Pts',(-1.15893798800006,11.6,-10.651801557));
#299338=CARTESIAN_POINT('Ctrl Pts',(-1.15855232700006,15.2,-10.654214555));
#299339=CARTESIAN_POINT('Ctrl Pts',(-1.15855232700006,11.6,-10.654214555));
#299340=CARTESIAN_POINT('Ctrl Pts',(-1.15816358800006,15.2,-10.656633385));
#299341=CARTESIAN_POINT('Ctrl Pts',(-1.15816358800006,11.6,-10.656633385));
#299342=CARTESIAN_POINT('Ctrl Pts',(-1.15777176600006,15.2,-10.659058034));
#299343=CARTESIAN_POINT('Ctrl Pts',(-1.15777176600006,11.6,-10.659058034));
#299344=CARTESIAN_POINT('Ctrl Pts',(-1.15737685100005,15.2,-10.661488487));
#299345=CARTESIAN_POINT('Ctrl Pts',(-1.15737685100005,11.6,-10.661488487));
#299346=CARTESIAN_POINT('Ctrl Pts',(-1.15697883700006,15.2,-10.663924733));
#299347=CARTESIAN_POINT('Ctrl Pts',(-1.15697883700006,11.6,-10.663924733));
#299348=CARTESIAN_POINT('Ctrl Pts',(-1.15657771600006,15.2,-10.666366757));
#299349=CARTESIAN_POINT('Ctrl Pts',(-1.15657771600006,11.6,-10.666366757));
#299350=CARTESIAN_POINT('Ctrl Pts',(-1.15617348100006,15.2,-10.668814545));
#299351=CARTESIAN_POINT('Ctrl Pts',(-1.15617348100006,11.6,-10.668814545));
#299352=CARTESIAN_POINT('Ctrl Pts',(-1.15576612400006,15.2,-10.671268084));
#299353=CARTESIAN_POINT('Ctrl Pts',(-1.15576612400006,11.6,-10.671268084));
#299354=CARTESIAN_POINT('Ctrl Pts',(-1.15535564000006,15.2,-10.673727361));
#299355=CARTESIAN_POINT('Ctrl Pts',(-1.15535564000006,11.6,-10.673727361));
#299356=CARTESIAN_POINT('Ctrl Pts',(-1.15494201900006,15.2,-10.676192362));
#299357=CARTESIAN_POINT('Ctrl Pts',(-1.15494201900006,11.6,-10.676192362));
#299358=CARTESIAN_POINT('Ctrl Pts',(-1.15452525600006,15.2,-10.678663073));
#299359=CARTESIAN_POINT('Ctrl Pts',(-1.15452525600006,11.6,-10.678663073));
#299360=CARTESIAN_POINT('Ctrl Pts',(-1.15410534200006,15.2,-10.681139483));
#299361=CARTESIAN_POINT('Ctrl Pts',(-1.15410534200006,11.6,-10.681139483));
#299362=CARTESIAN_POINT('Ctrl Pts',(-1.15368227000006,15.2,-10.683621578));
#299363=CARTESIAN_POINT('Ctrl Pts',(-1.15368227000006,11.6,-10.683621578));
#299364=CARTESIAN_POINT('Ctrl Pts',(-1.15325603400006,15.2,-10.686109343));
#299365=CARTESIAN_POINT('Ctrl Pts',(-1.15325603400006,11.6,-10.686109343));
#299366=CARTESIAN_POINT('Ctrl Pts',(-1.15282662700006,15.2,-10.688602766));
#299367=CARTESIAN_POINT('Ctrl Pts',(-1.15282662700006,11.6,-10.688602766));
#299368=CARTESIAN_POINT('Ctrl Pts',(-1.15239404100006,15.2,-10.691101834));
#299369=CARTESIAN_POINT('Ctrl Pts',(-1.15239404100006,11.6,-10.691101834));
#299370=CARTESIAN_POINT('Ctrl Pts',(-1.15195826900006,15.2,-10.693606533));
#299371=CARTESIAN_POINT('Ctrl Pts',(-1.15195826900006,11.6,-10.693606533));
#299372=CARTESIAN_POINT('Ctrl Pts',(-1.15151930500006,15.2,-10.69611685));
#299373=CARTESIAN_POINT('Ctrl Pts',(-1.15151930500006,11.6,-10.69611685));
#299374=CARTESIAN_POINT('Ctrl Pts',(-1.15107714100006,15.2,-10.698632773));
#299375=CARTESIAN_POINT('Ctrl Pts',(-1.15107714100006,11.6,-10.698632773));
#299376=CARTESIAN_POINT('Ctrl Pts',(-1.15063177100006,15.2,-10.701154289));
#299377=CARTESIAN_POINT('Ctrl Pts',(-1.15063177100006,11.6,-10.701154289));
#299378=CARTESIAN_POINT('Ctrl Pts',(-1.15018318700006,15.2,-10.703681383));
#299379=CARTESIAN_POINT('Ctrl Pts',(-1.15018318700006,11.6,-10.703681383));
#299380=CARTESIAN_POINT('Ctrl Pts',(-1.14973138200006,15.2,-10.706214044));
#299381=CARTESIAN_POINT('Ctrl Pts',(-1.14973138200006,11.6,-10.706214044));
#299382=CARTESIAN_POINT('Ctrl Pts',(-1.14927635100006,15.2,-10.708752257));
#299383=CARTESIAN_POINT('Ctrl Pts',(-1.14927635100006,11.6,-10.708752257));
#299384=CARTESIAN_POINT('Ctrl Pts',(-1.14881808500006,15.2,-10.711296011));
#299385=CARTESIAN_POINT('Ctrl Pts',(-1.14881808500006,11.6,-10.711296011));
#299386=CARTESIAN_POINT('Ctrl Pts',(-1.14835657800006,15.2,-10.713845292));
#299387=CARTESIAN_POINT('Ctrl Pts',(-1.14835657800006,11.6,-10.713845292));
#299388=CARTESIAN_POINT('Ctrl Pts',(-1.14789182500005,15.2,-10.716400088));
#299389=CARTESIAN_POINT('Ctrl Pts',(-1.14789182500005,11.6,-10.716400088));
#299390=CARTESIAN_POINT('Ctrl Pts',(-1.14742381600006,15.2,-10.718960385));
#299391=CARTESIAN_POINT('Ctrl Pts',(-1.14742381600006,11.6,-10.718960385));
#299392=CARTESIAN_POINT('Ctrl Pts',(-1.14695254600006,15.2,-10.721526171));
#299393=CARTESIAN_POINT('Ctrl Pts',(-1.14695254600006,11.6,-10.721526171));
#299394=CARTESIAN_POINT('Ctrl Pts',(-1.14647800900006,15.2,-10.724097433));
#299395=CARTESIAN_POINT('Ctrl Pts',(-1.14647800900006,11.6,-10.724097433));
#299396=CARTESIAN_POINT('Ctrl Pts',(-1.14600019700006,15.2,-10.726674158));
#299397=CARTESIAN_POINT('Ctrl Pts',(-1.14600019700006,11.6,-10.726674158));
#299398=CARTESIAN_POINT('Ctrl Pts',(-1.14551910300006,15.2,-10.729256334));
#299399=CARTESIAN_POINT('Ctrl Pts',(-1.14551910300006,11.6,-10.729256334));
#299400=CARTESIAN_POINT('Ctrl Pts',(-1.14503472200005,15.2,-10.731843947));
#299401=CARTESIAN_POINT('Ctrl Pts',(-1.14503472200005,11.6,-10.731843947));
#299402=CARTESIAN_POINT('Ctrl Pts',(-1.14454704700006,15.2,-10.734436985));
#299403=CARTESIAN_POINT('Ctrl Pts',(-1.14454704700006,11.6,-10.734436985));
#299404=CARTESIAN_POINT('Ctrl Pts',(-1.14405607000006,15.2,-10.737035436));
#299405=CARTESIAN_POINT('Ctrl Pts',(-1.14405607000006,11.6,-10.737035436));
#299406=CARTESIAN_POINT('Ctrl Pts',(-1.14356178700006,15.2,-10.739639287));
#299407=CARTESIAN_POINT('Ctrl Pts',(-1.14356178700006,11.6,-10.739639287));
#299408=CARTESIAN_POINT('Ctrl Pts',(-1.14306419000005,15.2,-10.742248524));
#299409=CARTESIAN_POINT('Ctrl Pts',(-1.14306419000005,11.6,-10.742248524));
#299410=CARTESIAN_POINT('Ctrl Pts',(-1.14256327100006,15.2,-10.744863136));
#299411=CARTESIAN_POINT('Ctrl Pts',(-1.14256327100006,11.6,-10.744863136));
#299412=CARTESIAN_POINT('Ctrl Pts',(-1.14205902600006,15.2,-10.74748311));
#299413=CARTESIAN_POINT('Ctrl Pts',(-1.14205902600006,11.6,-10.74748311));
#299414=CARTESIAN_POINT('Ctrl Pts',(-1.14155144800006,15.2,-10.750108433));
#299415=CARTESIAN_POINT('Ctrl Pts',(-1.14155144800006,11.6,-10.750108433));
#299416=CARTESIAN_POINT('Ctrl Pts',(-1.14104053000006,15.2,-10.752739094));
#299417=CARTESIAN_POINT('Ctrl Pts',(-1.14104053000006,11.6,-10.752739094));
#299418=CARTESIAN_POINT('Ctrl Pts',(-1.14052626500006,15.2,-10.755375079));
#299419=CARTESIAN_POINT('Ctrl Pts',(-1.14052626500006,11.6,-10.755375079));
#299420=CARTESIAN_POINT('Ctrl Pts',(-1.14000864800005,15.2,-10.758016376));
#299421=CARTESIAN_POINT('Ctrl Pts',(-1.14000864800005,11.6,-10.758016376));
#299422=CARTESIAN_POINT('Ctrl Pts',(-1.13948767300006,15.2,-10.760662972));
#299423=CARTESIAN_POINT('Ctrl Pts',(-1.13948767300006,11.6,-10.760662972));
#299424=CARTESIAN_POINT('Ctrl Pts',(-1.13896333200006,15.2,-10.763314856));
#299425=CARTESIAN_POINT('Ctrl Pts',(-1.13896333200006,11.6,-10.763314856));
#299426=CARTESIAN_POINT('Ctrl Pts',(-1.13843562000006,15.2,-10.765972015));
#299427=CARTESIAN_POINT('Ctrl Pts',(-1.13843562000006,11.6,-10.765972015));
#299428=CARTESIAN_POINT('Ctrl Pts',(-1.13790453000005,15.2,-10.768634436));
#299429=CARTESIAN_POINT('Ctrl Pts',(-1.13790453000005,11.6,-10.768634436));
#299430=CARTESIAN_POINT('Ctrl Pts',(-1.13737005500006,15.2,-10.771302109));
#299431=CARTESIAN_POINT('Ctrl Pts',(-1.13737005500006,11.6,-10.771302109));
#299432=CARTESIAN_POINT('Ctrl Pts',(-1.13683219200006,15.2,-10.773975018));
#299433=CARTESIAN_POINT('Ctrl Pts',(-1.13683219200006,11.6,-10.773975018));
#299434=CARTESIAN_POINT('Ctrl Pts',(-1.13629093200006,15.2,-10.776653154));
#299435=CARTESIAN_POINT('Ctrl Pts',(-1.13629093200006,11.6,-10.776653154));
#299436=CARTESIAN_POINT('Ctrl Pts',(-1.13574626900006,15.2,-10.779336503));
#299437=CARTESIAN_POINT('Ctrl Pts',(-1.13574626900006,11.6,-10.779336503));
#299438=CARTESIAN_POINT('Ctrl Pts',(-1.13519819700006,15.2,-10.782025053));
#299439=CARTESIAN_POINT('Ctrl Pts',(-1.13519819700006,11.6,-10.782025053));
#299440=CARTESIAN_POINT('Ctrl Pts',(-1.13464671100005,15.2,-10.784718793));
#299441=CARTESIAN_POINT('Ctrl Pts',(-1.13464671100005,11.6,-10.784718793));
#299442=CARTESIAN_POINT('Ctrl Pts',(-1.13409180400006,15.2,-10.78741771));
#299443=CARTESIAN_POINT('Ctrl Pts',(-1.13409180400006,11.6,-10.78741771));
#299444=CARTESIAN_POINT('Ctrl Pts',(-1.13353347000006,15.2,-10.790121791));
#299445=CARTESIAN_POINT('Ctrl Pts',(-1.13353347000006,11.6,-10.790121791));
#299446=CARTESIAN_POINT('Ctrl Pts',(-1.13297170400006,15.2,-10.792831026));
#299447=CARTESIAN_POINT('Ctrl Pts',(-1.13297170400006,11.6,-10.792831026));
#299448=CARTESIAN_POINT('Ctrl Pts',(-1.13240649900006,15.2,-10.795545401));
#299449=CARTESIAN_POINT('Ctrl Pts',(-1.13240649900006,11.6,-10.795545401));
#299450=CARTESIAN_POINT('Ctrl Pts',(-1.13183784800006,15.2,-10.798264905));
#299451=CARTESIAN_POINT('Ctrl Pts',(-1.13183784800006,11.6,-10.798264905));
#299452=CARTESIAN_POINT('Ctrl Pts',(-1.13126574700006,15.2,-10.800989525));
#299453=CARTESIAN_POINT('Ctrl Pts',(-1.13126574700006,11.6,-10.800989525));
#299454=CARTESIAN_POINT('Ctrl Pts',(-1.13069018800006,15.2,-10.803719251));
#299455=CARTESIAN_POINT('Ctrl Pts',(-1.13069018800006,11.6,-10.803719251));
#299456=CARTESIAN_POINT('Ctrl Pts',(-1.13011116700006,15.2,-10.806454068));
#299457=CARTESIAN_POINT('Ctrl Pts',(-1.13011116700006,11.6,-10.806454068));
#299458=CARTESIAN_POINT('Ctrl Pts',(-1.12952867800006,15.2,-10.809193966));
#299459=CARTESIAN_POINT('Ctrl Pts',(-1.12952867800006,11.6,-10.809193966));
#299460=CARTESIAN_POINT('Ctrl Pts',(-1.12894271500006,15.2,-10.811938934));
#299461=CARTESIAN_POINT('Ctrl Pts',(-1.12894271500006,11.6,-10.811938934));
#299462=CARTESIAN_POINT('Ctrl Pts',(-1.12835327000006,15.2,-10.814688959));
#299463=CARTESIAN_POINT('Ctrl Pts',(-1.12835327000006,11.6,-10.814688959));
#299464=CARTESIAN_POINT('Ctrl Pts',(-1.12776033900006,15.2,-10.817444029));
#299465=CARTESIAN_POINT('Ctrl Pts',(-1.12776033900006,11.6,-10.817444029));
#299466=CARTESIAN_POINT('Ctrl Pts',(-1.12716391600006,15.2,-10.820204131));
#299467=CARTESIAN_POINT('Ctrl Pts',(-1.12716391600006,11.6,-10.820204131));
#299468=CARTESIAN_POINT('Ctrl Pts',(-1.12656399600006,15.2,-10.822969255));
#299469=CARTESIAN_POINT('Ctrl Pts',(-1.12656399600006,11.6,-10.822969255));
#299470=CARTESIAN_POINT('Ctrl Pts',(-1.12596057300006,15.2,-10.82573939));
#299471=CARTESIAN_POINT('Ctrl Pts',(-1.12596057300006,11.6,-10.82573939));
#299472=CARTESIAN_POINT('Ctrl Pts',(-1.12535363900006,15.2,-10.828514521));
#299473=CARTESIAN_POINT('Ctrl Pts',(-1.12535363900006,11.6,-10.828514521));
#299474=CARTESIAN_POINT('Ctrl Pts',(-1.12474319100005,15.2,-10.831294639));
#299475=CARTESIAN_POINT('Ctrl Pts',(-1.12474319100005,11.6,-10.831294639));
#299476=CARTESIAN_POINT('Ctrl Pts',(-1.12412922300006,15.2,-10.834079731));
#299477=CARTESIAN_POINT('Ctrl Pts',(-1.12412922300006,11.6,-10.834079731));
#299478=CARTESIAN_POINT('Ctrl Pts',(-1.12351172700005,15.2,-10.836869786));
#299479=CARTESIAN_POINT('Ctrl Pts',(-1.12351172700005,11.6,-10.836869786));
#299480=CARTESIAN_POINT('Ctrl Pts',(-1.12289070100006,15.2,-10.839664792));
#299481=CARTESIAN_POINT('Ctrl Pts',(-1.12289070100006,11.6,-10.839664792));
#299482=CARTESIAN_POINT('Ctrl Pts',(-1.12226613600006,15.2,-10.842464738));
#299483=CARTESIAN_POINT('Ctrl Pts',(-1.12226613600006,11.6,-10.842464738));
#299484=CARTESIAN_POINT('Ctrl Pts',(-1.12163802800006,15.2,-10.845269611));
#299485=CARTESIAN_POINT('Ctrl Pts',(-1.12163802800006,11.6,-10.845269611));
#299486=CARTESIAN_POINT('Ctrl Pts',(-1.12100637100006,15.2,-10.848079399));
#299487=CARTESIAN_POINT('Ctrl Pts',(-1.12100637100006,11.6,-10.848079399));
#299488=CARTESIAN_POINT('Ctrl Pts',(-1.12037116000006,15.2,-10.850894093));
#299489=CARTESIAN_POINT('Ctrl Pts',(-1.12037116000006,11.6,-10.850894093));
#299490=CARTESIAN_POINT('Ctrl Pts',(-1.11973239000006,15.2,-10.85371368));
#299491=CARTESIAN_POINT('Ctrl Pts',(-1.11973239000006,11.6,-10.85371368));
#299492=CARTESIAN_POINT('Ctrl Pts',(-1.11909005400006,15.2,-10.856538148));
#299493=CARTESIAN_POINT('Ctrl Pts',(-1.11909005400006,11.6,-10.856538148));
#299494=CARTESIAN_POINT('Ctrl Pts',(-1.11844414600006,15.2,-10.859367486));
#299495=CARTESIAN_POINT('Ctrl Pts',(-1.11844414600006,11.6,-10.859367486));
#299496=CARTESIAN_POINT('Ctrl Pts',(-1.11779466300006,15.2,-10.862201683));
#299497=CARTESIAN_POINT('Ctrl Pts',(-1.11779466300006,11.6,-10.862201683));
#299498=CARTESIAN_POINT('Ctrl Pts',(-1.11714159900006,15.2,-10.865040726));
#299499=CARTESIAN_POINT('Ctrl Pts',(-1.11714159900006,11.6,-10.865040726));
#299500=CARTESIAN_POINT('Ctrl Pts',(-1.11648494600006,15.2,-10.867884606));
#299501=CARTESIAN_POINT('Ctrl Pts',(-1.11648494600006,11.6,-10.867884606));
#299502=CARTESIAN_POINT('Ctrl Pts',(-1.11582470100006,15.2,-10.870733309));
#299503=CARTESIAN_POINT('Ctrl Pts',(-1.11582470100006,11.6,-10.870733309));
#299504=CARTESIAN_POINT('Ctrl Pts',(-1.11516085700006,15.2,-10.873586825));
#299505=CARTESIAN_POINT('Ctrl Pts',(-1.11516085700006,11.6,-10.873586825));
#299506=CARTESIAN_POINT('Ctrl Pts',(-1.11449341200006,15.2,-10.876445142));
#299507=CARTESIAN_POINT('Ctrl Pts',(-1.11449341200006,11.6,-10.876445142));
#299508=CARTESIAN_POINT('Ctrl Pts',(-1.11382235600006,15.2,-10.87930825));
#299509=CARTESIAN_POINT('Ctrl Pts',(-1.11382235600006,11.6,-10.87930825));
#299510=CARTESIAN_POINT('Ctrl Pts',(-1.11314768700006,15.2,-10.882176135));
#299511=CARTESIAN_POINT('Ctrl Pts',(-1.11314768700006,11.6,-10.882176135));
#299512=CARTESIAN_POINT('Ctrl Pts',(-1.11246939900006,15.2,-10.885048789));
#299513=CARTESIAN_POINT('Ctrl Pts',(-1.11246939900006,11.6,-10.885048789));
#299514=CARTESIAN_POINT('Ctrl Pts',(-1.11178748600006,15.2,-10.887926198));
#299515=CARTESIAN_POINT('Ctrl Pts',(-1.11178748600006,11.6,-10.887926198));
#299516=CARTESIAN_POINT('Ctrl Pts',(-1.11110194300006,15.2,-10.890808352));
#299517=CARTESIAN_POINT('Ctrl Pts',(-1.11110194300006,11.6,-10.890808352));
#299518=CARTESIAN_POINT('Ctrl Pts',(-1.11041276500006,15.2,-10.893695239));
#299519=CARTESIAN_POINT('Ctrl Pts',(-1.11041276500006,11.6,-10.893695239));
#299520=CARTESIAN_POINT('Ctrl Pts',(-1.10971994600006,15.2,-10.89658685));
#299521=CARTESIAN_POINT('Ctrl Pts',(-1.10971994600006,11.6,-10.89658685));
#299522=CARTESIAN_POINT('Ctrl Pts',(-1.10902348300006,15.2,-10.899483171));
#299523=CARTESIAN_POINT('Ctrl Pts',(-1.10902348300006,11.6,-10.899483171));
#299524=CARTESIAN_POINT('Ctrl Pts',(-1.10832336800006,15.2,-10.902384191));
#299525=CARTESIAN_POINT('Ctrl Pts',(-1.10832336800006,11.6,-10.902384191));
#299526=CARTESIAN_POINT('Ctrl Pts',(-1.10761959700006,15.2,-10.905289901));
#299527=CARTESIAN_POINT('Ctrl Pts',(-1.10761959700006,11.6,-10.905289901));
#299528=CARTESIAN_POINT('Ctrl Pts',(-1.10691216600006,15.2,-10.908200288));
#299529=CARTESIAN_POINT('Ctrl Pts',(-1.10691216600006,11.6,-10.908200288));
#299530=CARTESIAN_POINT('Ctrl Pts',(-1.10620106800006,15.2,-10.911115343));
#299531=CARTESIAN_POINT('Ctrl Pts',(-1.10620106800006,11.6,-10.911115343));
#299532=CARTESIAN_POINT('Ctrl Pts',(-1.10548630000006,15.2,-10.914035053));
#299533=CARTESIAN_POINT('Ctrl Pts',(-1.10548630000006,11.6,-10.914035053));
#299534=CARTESIAN_POINT('Ctrl Pts',(-1.10476785400005,15.2,-10.916959406));
#299535=CARTESIAN_POINT('Ctrl Pts',(-1.10476785400005,11.6,-10.916959406));
#299536=CARTESIAN_POINT('Ctrl Pts',(-1.10404572800006,15.2,-10.919888394));
#299537=CARTESIAN_POINT('Ctrl Pts',(-1.10404572800006,11.6,-10.919888394));
#299538=CARTESIAN_POINT('Ctrl Pts',(-1.10331991600006,15.2,-10.922822003));
#299539=CARTESIAN_POINT('Ctrl Pts',(-1.10331991600006,11.6,-10.922822003));
#299540=CARTESIAN_POINT('Ctrl Pts',(-1.10259041100006,15.2,-10.925760224));
#299541=CARTESIAN_POINT('Ctrl Pts',(-1.10259041100006,11.6,-10.925760224));
#299542=CARTESIAN_POINT('Ctrl Pts',(-1.10185721000006,15.2,-10.928703044));
#299543=CARTESIAN_POINT('Ctrl Pts',(-1.10185721000006,11.6,-10.928703044));
#299544=CARTESIAN_POINT('Ctrl Pts',(-1.10112030900006,15.2,-10.931650455));
#299545=CARTESIAN_POINT('Ctrl Pts',(-1.10112030900006,11.6,-10.931650455));
#299546=CARTESIAN_POINT('Ctrl Pts',(-1.10037970000006,15.2,-10.934602443));
#299547=CARTESIAN_POINT('Ctrl Pts',(-1.10037970000006,11.6,-10.934602443));
#299548=CARTESIAN_POINT('Ctrl Pts',(-1.09963538000006,15.2,-10.937559));
#299549=CARTESIAN_POINT('Ctrl Pts',(-1.09963538000006,11.6,-10.937559));
#299550=CARTESIAN_POINT('Ctrl Pts',(-1.09888734500006,15.2,-10.940520113));
#299551=CARTESIAN_POINT('Ctrl Pts',(-1.09888734500006,11.6,-10.940520113));
#299552=CARTESIAN_POINT('Ctrl Pts',(-1.09813558800006,15.2,-10.943485771));
#299553=CARTESIAN_POINT('Ctrl Pts',(-1.09813558800006,11.6,-10.943485771));
#299554=CARTESIAN_POINT('Ctrl Pts',(-1.09738010500006,15.2,-10.946455964));
#299555=CARTESIAN_POINT('Ctrl Pts',(-1.09738010500006,11.6,-10.946455964));
#299556=CARTESIAN_POINT('Ctrl Pts',(-1.09662089100006,15.2,-10.949430681));
#299557=CARTESIAN_POINT('Ctrl Pts',(-1.09662089100006,11.6,-10.949430681));
#299558=CARTESIAN_POINT('Ctrl Pts',(-1.09585794200005,15.2,-10.952409912));
#299559=CARTESIAN_POINT('Ctrl Pts',(-1.09585794200005,11.6,-10.952409912));
#299560=CARTESIAN_POINT('Ctrl Pts',(-1.09509125200006,15.2,-10.955393644));
#299561=CARTESIAN_POINT('Ctrl Pts',(-1.09509125200006,11.6,-10.955393644));
#299562=CARTESIAN_POINT('Ctrl Pts',(-1.09432081700006,15.2,-10.958381868));
#299563=CARTESIAN_POINT('Ctrl Pts',(-1.09432081700006,11.6,-10.958381868));
#299564=CARTESIAN_POINT('Ctrl Pts',(-1.09354663200006,15.2,-10.961374573));
#299565=CARTESIAN_POINT('Ctrl Pts',(-1.09354663200006,11.6,-10.961374573));
#299566=CARTESIAN_POINT('Ctrl Pts',(-1.09276869100006,15.2,-10.964371748));
#299567=CARTESIAN_POINT('Ctrl Pts',(-1.09276869100006,11.6,-10.964371748));
#299568=CARTESIAN_POINT('Ctrl Pts',(-1.09198699200006,15.2,-10.967373381));
#299569=CARTESIAN_POINT('Ctrl Pts',(-1.09198699200006,11.6,-10.967373381));
#299570=CARTESIAN_POINT('Ctrl Pts',(-1.09120152700006,15.2,-10.970379465));
#299571=CARTESIAN_POINT('Ctrl Pts',(-1.09120152700006,11.6,-10.970379465));
#299572=CARTESIAN_POINT('Ctrl Pts',(-1.09041229400006,15.2,-10.973389985));
#299573=CARTESIAN_POINT('Ctrl Pts',(-1.09041229400006,11.6,-10.973389985));
#299574=CARTESIAN_POINT('Ctrl Pts',(-1.08961928800006,15.2,-10.976404933));
#299575=CARTESIAN_POINT('Ctrl Pts',(-1.08961928800006,11.6,-10.976404933));
#299576=CARTESIAN_POINT('Ctrl Pts',(-1.08882250300006,15.2,-10.979424298));
#299577=CARTESIAN_POINT('Ctrl Pts',(-1.08882250300006,11.6,-10.979424298));
#299578=CARTESIAN_POINT('Ctrl Pts',(-1.08802193400006,15.2,-10.982448068));
#299579=CARTESIAN_POINT('Ctrl Pts',(-1.08802193400006,11.6,-10.982448068));
#299580=CARTESIAN_POINT('Ctrl Pts',(-1.08721757800006,15.2,-10.985476233));
#299581=CARTESIAN_POINT('Ctrl Pts',(-1.08721757800006,11.6,-10.985476233));
#299582=CARTESIAN_POINT('Ctrl Pts',(-1.08640943000006,15.2,-10.988508784));
#299583=CARTESIAN_POINT('Ctrl Pts',(-1.08640943000006,11.6,-10.988508784));
#299584=CARTESIAN_POINT('Ctrl Pts',(-1.08559748500006,15.2,-10.991545708));
#299585=CARTESIAN_POINT('Ctrl Pts',(-1.08559748500006,11.6,-10.991545708));
#299586=CARTESIAN_POINT('Ctrl Pts',(-1.08478173800005,15.2,-10.994586996));
#299587=CARTESIAN_POINT('Ctrl Pts',(-1.08478173800005,11.6,-10.994586996));
#299588=CARTESIAN_POINT('Ctrl Pts',(-1.08396218500006,15.2,-10.997632637));
#299589=CARTESIAN_POINT('Ctrl Pts',(-1.08396218500006,11.6,-10.997632637));
#299590=CARTESIAN_POINT('Ctrl Pts',(-1.08313882200005,15.2,-11.000682622));
#299591=CARTESIAN_POINT('Ctrl Pts',(-1.08313882200005,11.6,-11.000682622));
#299592=CARTESIAN_POINT('Ctrl Pts',(-1.08231164200006,15.2,-11.003736938));
#299593=CARTESIAN_POINT('Ctrl Pts',(-1.08231164200006,11.6,-11.003736938));
#299594=CARTESIAN_POINT('Ctrl Pts',(-1.08148064400006,15.2,-11.006795575));
#299595=CARTESIAN_POINT('Ctrl Pts',(-1.08148064400006,11.6,-11.006795575));
#299596=CARTESIAN_POINT('Ctrl Pts',(-1.08064582200006,15.2,-11.009858524));
#299597=CARTESIAN_POINT('Ctrl Pts',(-1.08064582200006,11.6,-11.009858524));
#299598=CARTESIAN_POINT('Ctrl Pts',(-1.07980717000006,15.2,-11.012925773));
#299599=CARTESIAN_POINT('Ctrl Pts',(-1.07980717000006,11.6,-11.012925773));
#299600=CARTESIAN_POINT('Ctrl Pts',(-1.07896468700006,15.2,-11.015997313));
#299601=CARTESIAN_POINT('Ctrl Pts',(-1.07896468700006,11.6,-11.015997313));
#299602=CARTESIAN_POINT('Ctrl Pts',(-1.07811836400006,15.2,-11.019073132));
#299603=CARTESIAN_POINT('Ctrl Pts',(-1.07811836400006,11.6,-11.019073132));
#299604=CARTESIAN_POINT('Ctrl Pts',(-1.07726820100006,15.2,-11.022153221));
#299605=CARTESIAN_POINT('Ctrl Pts',(-1.07726820100006,11.6,-11.022153221));
#299606=CARTESIAN_POINT('Ctrl Pts',(-1.07641419000006,15.2,-11.025237569));
#299607=CARTESIAN_POINT('Ctrl Pts',(-1.07641419000006,11.6,-11.025237569));
#299608=CARTESIAN_POINT('Ctrl Pts',(-1.07555633000006,15.2,-11.028326166));
#299609=CARTESIAN_POINT('Ctrl Pts',(-1.07555633000006,11.6,-11.028326166));
#299610=CARTESIAN_POINT('Ctrl Pts',(-1.07469461400005,15.2,-11.031419001));
#299611=CARTESIAN_POINT('Ctrl Pts',(-1.07469461400005,11.6,-11.031419001));
#299612=CARTESIAN_POINT('Ctrl Pts',(-1.07382903800006,15.2,-11.034516065));
#299613=CARTESIAN_POINT('Ctrl Pts',(-1.07382903800006,11.6,-11.034516065));
#299614=CARTESIAN_POINT('Ctrl Pts',(-1.07295959900006,15.2,-11.037617345));
#299615=CARTESIAN_POINT('Ctrl Pts',(-1.07295959900006,11.6,-11.037617345));
#299616=CARTESIAN_POINT('Ctrl Pts',(-1.07208629100006,15.2,-11.040722834));
#299617=CARTESIAN_POINT('Ctrl Pts',(-1.07208629100006,11.6,-11.040722834));
#299618=CARTESIAN_POINT('Ctrl Pts',(-1.07120911100006,15.2,-11.04383252));
#299619=CARTESIAN_POINT('Ctrl Pts',(-1.07120911100006,11.6,-11.04383252));
#299620=CARTESIAN_POINT('Ctrl Pts',(-1.07032805400006,15.2,-11.046946393));
#299621=CARTESIAN_POINT('Ctrl Pts',(-1.07032805400006,11.6,-11.046946393));
#299622=CARTESIAN_POINT('Ctrl Pts',(-1.06944311600006,15.2,-11.050064443));
#299623=CARTESIAN_POINT('Ctrl Pts',(-1.06944311600006,11.6,-11.050064443));
#299624=CARTESIAN_POINT('Ctrl Pts',(-1.06855429400005,15.2,-11.05318666));
#299625=CARTESIAN_POINT('Ctrl Pts',(-1.06855429400005,11.6,-11.05318666));
#299626=CARTESIAN_POINT('Ctrl Pts',(-1.06766158100006,15.2,-11.056313032));
#299627=CARTESIAN_POINT('Ctrl Pts',(-1.06766158100006,11.6,-11.056313032));
#299628=CARTESIAN_POINT('Ctrl Pts',(-1.06676497400006,15.2,-11.059443552));
#299629=CARTESIAN_POINT('Ctrl Pts',(-1.06676497400006,11.6,-11.059443552));
#299630=CARTESIAN_POINT('Ctrl Pts',(-1.06586447000006,15.2,-11.062578207));
#299631=CARTESIAN_POINT('Ctrl Pts',(-1.06586447000006,11.6,-11.062578207));
#299632=CARTESIAN_POINT('Ctrl Pts',(-1.06496006400006,15.2,-11.065716988));
#299633=CARTESIAN_POINT('Ctrl Pts',(-1.06496006400006,11.6,-11.065716988));
#299634=CARTESIAN_POINT('Ctrl Pts',(-1.06405175100006,15.2,-11.068859886));
#299635=CARTESIAN_POINT('Ctrl Pts',(-1.06405175100006,11.6,-11.068859886));
#299636=CARTESIAN_POINT('Ctrl Pts',(-1.06313952800006,15.2,-11.072006888));
#299637=CARTESIAN_POINT('Ctrl Pts',(-1.06313952800006,11.6,-11.072006888));
#299638=CARTESIAN_POINT('Ctrl Pts',(-1.06222339100006,15.2,-11.075157987));
#299639=CARTESIAN_POINT('Ctrl Pts',(-1.06222339100006,11.6,-11.075157987));
#299640=CARTESIAN_POINT('Ctrl Pts',(-1.06130333400006,15.2,-11.07831317));
#299641=CARTESIAN_POINT('Ctrl Pts',(-1.06130333400006,11.6,-11.07831317));
#299642=CARTESIAN_POINT('Ctrl Pts',(-1.06037935500006,15.2,-11.08147243));
#299643=CARTESIAN_POINT('Ctrl Pts',(-1.06037935500006,11.6,-11.08147243));
#299644=CARTESIAN_POINT('Ctrl Pts',(-1.05945145000006,15.2,-11.084635755));
#299645=CARTESIAN_POINT('Ctrl Pts',(-1.05945145000006,11.6,-11.084635755));
#299646=CARTESIAN_POINT('Ctrl Pts',(-1.05851961200006,15.2,-11.087803135));
#299647=CARTESIAN_POINT('Ctrl Pts',(-1.05851961200006,11.6,-11.087803135));
#299648=CARTESIAN_POINT('Ctrl Pts',(-1.05758384000006,15.2,-11.090974562));
#299649=CARTESIAN_POINT('Ctrl Pts',(-1.05758384000006,11.6,-11.090974562));
#299650=CARTESIAN_POINT('Ctrl Pts',(-1.05664412900005,15.2,-11.094150024));
#299651=CARTESIAN_POINT('Ctrl Pts',(-1.05664412900005,11.6,-11.094150024));
#299652=CARTESIAN_POINT('Ctrl Pts',(-1.05570047500006,15.2,-11.09732951));
#299653=CARTESIAN_POINT('Ctrl Pts',(-1.05570047500006,11.6,-11.09732951));
#299654=CARTESIAN_POINT('Ctrl Pts',(-1.05475287400006,15.2,-11.100513013));
#299655=CARTESIAN_POINT('Ctrl Pts',(-1.05475287400006,11.6,-11.100513013));
#299656=CARTESIAN_POINT('Ctrl Pts',(-1.05380132100006,15.2,-11.103700521));
#299657=CARTESIAN_POINT('Ctrl Pts',(-1.05380132100006,11.6,-11.103700521));
#299658=CARTESIAN_POINT('Ctrl Pts',(-1.05284581400006,15.2,-11.106892026));
#299659=CARTESIAN_POINT('Ctrl Pts',(-1.05284581400006,11.6,-11.106892026));
#299660=CARTESIAN_POINT('Ctrl Pts',(-1.05188634700006,15.2,-11.110087516));
#299661=CARTESIAN_POINT('Ctrl Pts',(-1.05188634700006,11.6,-11.110087516));
#299662=CARTESIAN_POINT('Ctrl Pts',(-1.05092291800006,15.2,-11.113286981));
#299663=CARTESIAN_POINT('Ctrl Pts',(-1.05092291800006,11.6,-11.113286981));
#299664=CARTESIAN_POINT('Ctrl Pts',(-1.04995552100006,15.2,-11.116490413));
#299665=CARTESIAN_POINT('Ctrl Pts',(-1.04995552100006,11.6,-11.116490413));
#299666=CARTESIAN_POINT('Ctrl Pts',(-1.04898415400006,15.2,-11.119697801));
#299667=CARTESIAN_POINT('Ctrl Pts',(-1.04898415400006,11.6,-11.119697801));
#299668=CARTESIAN_POINT('Ctrl Pts',(-1.04800881300006,15.2,-11.122909136));
#299669=CARTESIAN_POINT('Ctrl Pts',(-1.04800881300006,11.6,-11.122909136));
#299670=CARTESIAN_POINT('Ctrl Pts',(-1.04702949200006,15.2,-11.126124407));
#299671=CARTESIAN_POINT('Ctrl Pts',(-1.04702949200006,11.6,-11.126124407));
#299672=CARTESIAN_POINT('Ctrl Pts',(-1.04604618900005,15.2,-11.129343605));
#299673=CARTESIAN_POINT('Ctrl Pts',(-1.04604618900005,11.6,-11.129343605));
#299674=CARTESIAN_POINT('Ctrl Pts',(-1.04505890000006,15.2,-11.13256672));
#299675=CARTESIAN_POINT('Ctrl Pts',(-1.04505890000006,11.6,-11.13256672));
#299676=CARTESIAN_POINT('Ctrl Pts',(-1.04406762000006,15.2,-11.135793742));
#299677=CARTESIAN_POINT('Ctrl Pts',(-1.04406762000006,11.6,-11.135793742));
#299678=CARTESIAN_POINT('Ctrl Pts',(-1.04307234700006,15.2,-11.139024662));
#299679=CARTESIAN_POINT('Ctrl Pts',(-1.04307234700006,11.6,-11.139024662));
#299680=CARTESIAN_POINT('Ctrl Pts',(-1.04207307600006,15.2,-11.142259468));
#299681=CARTESIAN_POINT('Ctrl Pts',(-1.04207307600006,11.6,-11.142259468));
#299682=CARTESIAN_POINT('Ctrl Pts',(-1.04106980400006,15.2,-11.145498154));
#299683=CARTESIAN_POINT('Ctrl Pts',(-1.04106980400006,11.6,-11.145498154));
#299684=CARTESIAN_POINT('Ctrl Pts',(-1.04006252600006,15.2,-11.148740707));
#299685=CARTESIAN_POINT('Ctrl Pts',(-1.04006252600006,11.6,-11.148740707));
#299686=CARTESIAN_POINT('Ctrl Pts',(-1.03905123800006,15.2,-11.151987119));
#299687=CARTESIAN_POINT('Ctrl Pts',(-1.03905123800006,11.6,-11.151987119));
#299688=CARTESIAN_POINT('Ctrl Pts',(-1.03803593800005,15.2,-11.155237381));
#299689=CARTESIAN_POINT('Ctrl Pts',(-1.03803593800005,11.6,-11.155237381));
#299690=CARTESIAN_POINT('Ctrl Pts',(-1.03701662100006,15.2,-11.158491481));
#299691=CARTESIAN_POINT('Ctrl Pts',(-1.03701662100006,11.6,-11.158491481));
#299692=CARTESIAN_POINT('Ctrl Pts',(-1.03599328400006,15.2,-11.16174941));
#299693=CARTESIAN_POINT('Ctrl Pts',(-1.03599328400006,11.6,-11.16174941));
#299694=CARTESIAN_POINT('Ctrl Pts',(-1.03496592300006,15.2,-11.165011161));
#299695=CARTESIAN_POINT('Ctrl Pts',(-1.03496592300006,11.6,-11.165011161));
#299696=CARTESIAN_POINT('Ctrl Pts',(-1.03393453400005,15.2,-11.168276721));
#299697=CARTESIAN_POINT('Ctrl Pts',(-1.03393453400005,11.6,-11.168276721));
#299698=CARTESIAN_POINT('Ctrl Pts',(-1.03289911500006,15.2,-11.171546082));
#299699=CARTESIAN_POINT('Ctrl Pts',(-1.03289911500006,11.6,-11.171546082));
#299700=CARTESIAN_POINT('Ctrl Pts',(-1.03185965900006,15.2,-11.174819234));
#299701=CARTESIAN_POINT('Ctrl Pts',(-1.03185965900006,11.6,-11.174819234));
#299702=CARTESIAN_POINT('Ctrl Pts',(-1.03081616500006,15.2,-11.178096168));
#299703=CARTESIAN_POINT('Ctrl Pts',(-1.03081616500006,11.6,-11.178096168));
#299704=CARTESIAN_POINT('Ctrl Pts',(-1.02976862900006,15.2,-11.181376874));
#299705=CARTESIAN_POINT('Ctrl Pts',(-1.02976862900006,11.6,-11.181376874));
#299706=CARTESIAN_POINT('Ctrl Pts',(-1.02871704700006,15.2,-11.184661341));
#299707=CARTESIAN_POINT('Ctrl Pts',(-1.02871704700006,11.6,-11.184661341));
#299708=CARTESIAN_POINT('Ctrl Pts',(-1.02766141600006,15.2,-11.187949563));
#299709=CARTESIAN_POINT('Ctrl Pts',(-1.02766141600006,11.6,-11.187949563));
#299710=CARTESIAN_POINT('Ctrl Pts',(-1.02660173100006,15.2,-11.191241529));
#299711=CARTESIAN_POINT('Ctrl Pts',(-1.02660173100006,11.6,-11.191241529));
#299712=CARTESIAN_POINT('Ctrl Pts',(-1.02553799000005,15.2,-11.194537226));
#299713=CARTESIAN_POINT('Ctrl Pts',(-1.02553799000005,11.6,-11.194537226));
#299714=CARTESIAN_POINT('Ctrl Pts',(-1.02447018800006,15.2,-11.19783665));
#299715=CARTESIAN_POINT('Ctrl Pts',(-1.02447018800006,11.6,-11.19783665));
#299716=CARTESIAN_POINT('Ctrl Pts',(-1.02339832300006,15.2,-11.201139788));
#299717=CARTESIAN_POINT('Ctrl Pts',(-1.02339832300006,11.6,-11.201139788));
#299718=CARTESIAN_POINT('Ctrl Pts',(-1.02232239100006,15.2,-11.204446633));
#299719=CARTESIAN_POINT('Ctrl Pts',(-1.02232239100006,11.6,-11.204446633));
#299720=CARTESIAN_POINT('Ctrl Pts',(-1.02124238700006,15.2,-11.207757173));
#299721=CARTESIAN_POINT('Ctrl Pts',(-1.02124238700006,11.6,-11.207757173));
#299722=CARTESIAN_POINT('Ctrl Pts',(-1.02015830900006,15.2,-11.2110714));
#299723=CARTESIAN_POINT('Ctrl Pts',(-1.02015830900006,11.6,-11.2110714));
#299724=CARTESIAN_POINT('Ctrl Pts',(-1.01907015400006,15.2,-11.214389304));
#299725=CARTESIAN_POINT('Ctrl Pts',(-1.01907015400006,11.6,-11.214389304));
#299726=CARTESIAN_POINT('Ctrl Pts',(-1.01797791800006,15.2,-11.217710877));
#299727=CARTESIAN_POINT('Ctrl Pts',(-1.01797791800006,11.6,-11.217710877));
#299728=CARTESIAN_POINT('Ctrl Pts',(-1.01688159500006,15.2,-11.221036107));
#299729=CARTESIAN_POINT('Ctrl Pts',(-1.01688159500006,11.6,-11.221036107));
#299730=CARTESIAN_POINT('Ctrl Pts',(-1.01578118600006,15.2,-11.224364987));
#299731=CARTESIAN_POINT('Ctrl Pts',(-1.01578118600006,11.6,-11.224364987));
#299732=CARTESIAN_POINT('Ctrl Pts',(-1.01467668500006,15.2,-11.227697507));
#299733=CARTESIAN_POINT('Ctrl Pts',(-1.01467668500006,11.6,-11.227697507));
#299734=CARTESIAN_POINT('Ctrl Pts',(-1.01356808900006,15.2,-11.231033658));
#299735=CARTESIAN_POINT('Ctrl Pts',(-1.01356808900006,11.6,-11.231033658));
#299736=CARTESIAN_POINT('Ctrl Pts',(-1.01245539400006,15.2,-11.234373429));
#299737=CARTESIAN_POINT('Ctrl Pts',(-1.01245539400006,11.6,-11.234373429));
#299738=CARTESIAN_POINT('Ctrl Pts',(-1.01133859700006,15.2,-11.237716813));
#299739=CARTESIAN_POINT('Ctrl Pts',(-1.01133859700006,11.6,-11.237716813));
#299740=CARTESIAN_POINT('Ctrl Pts',(-1.01021769600006,15.2,-11.241063799));
#299741=CARTESIAN_POINT('Ctrl Pts',(-1.01021769600006,11.6,-11.241063799));
#299742=CARTESIAN_POINT('Ctrl Pts',(-1.00909268600006,15.2,-11.244414379));
#299743=CARTESIAN_POINT('Ctrl Pts',(-1.00909268600006,11.6,-11.244414379));
#299744=CARTESIAN_POINT('Ctrl Pts',(-1.00796356300005,15.2,-11.247768543));
#299745=CARTESIAN_POINT('Ctrl Pts',(-1.00796356300005,11.6,-11.247768543));
#299746=CARTESIAN_POINT('Ctrl Pts',(-1.00683032600006,15.2,-11.251126281));
#299747=CARTESIAN_POINT('Ctrl Pts',(-1.00683032600006,11.6,-11.251126281));
#299748=CARTESIAN_POINT('Ctrl Pts',(-1.00569297000005,15.2,-11.254487585));
#299749=CARTESIAN_POINT('Ctrl Pts',(-1.00569297000005,11.6,-11.254487585));
#299750=CARTESIAN_POINT('Ctrl Pts',(-1.00455149300006,15.2,-11.257852446));
#299751=CARTESIAN_POINT('Ctrl Pts',(-1.00455149300006,11.6,-11.257852446));
#299752=CARTESIAN_POINT('Ctrl Pts',(-1.00340588900006,15.2,-11.261220853));
#299753=CARTESIAN_POINT('Ctrl Pts',(-1.00340588900006,11.6,-11.261220853));
#299754=CARTESIAN_POINT('Ctrl Pts',(-1.00225615900006,15.2,-11.264592799));
#299755=CARTESIAN_POINT('Ctrl Pts',(-1.00225615900006,11.6,-11.264592799));
#299756=CARTESIAN_POINT('Ctrl Pts',(-1.00110229600006,15.2,-11.267968274));
#299757=CARTESIAN_POINT('Ctrl Pts',(-1.00110229600006,11.6,-11.267968274));
#299758=CARTESIAN_POINT('Ctrl Pts',(-0.999944298000056,15.2,-11.271347269));
#299759=CARTESIAN_POINT('Ctrl Pts',(-0.999944298000056,11.6,-11.271347269));
#299760=CARTESIAN_POINT('Ctrl Pts',(-0.998782162000056,15.2,-11.274729773));
#299761=CARTESIAN_POINT('Ctrl Pts',(-0.998782162000056,11.6,-11.274729773));
#299762=CARTESIAN_POINT('Ctrl Pts',(-0.997615884000057,15.2,-11.278115779));
#299763=CARTESIAN_POINT('Ctrl Pts',(-0.997615884000057,11.6,-11.278115779));
#299764=CARTESIAN_POINT('Ctrl Pts',(-0.996445463000055,15.2,-11.281505277));
#299765=CARTESIAN_POINT('Ctrl Pts',(-0.996445463000055,11.6,-11.281505277));
#299766=CARTESIAN_POINT('Ctrl Pts',(-0.995270892000055,15.2,-11.284898258));
#299767=CARTESIAN_POINT('Ctrl Pts',(-0.995270892000055,11.6,-11.284898258));
#299768=CARTESIAN_POINT('Ctrl Pts',(-0.994092171000055,15.2,-11.288294715));
#299769=CARTESIAN_POINT('Ctrl Pts',(-0.994092171000055,11.6,-11.288294715));
#299770=CARTESIAN_POINT('Ctrl Pts',(-0.992909296000055,15.2,-11.291694635));
#299771=CARTESIAN_POINT('Ctrl Pts',(-0.992909296000055,11.6,-11.291694635));
#299772=CARTESIAN_POINT('Ctrl Pts',(-0.991722264000057,15.2,-11.295098011));
#299773=CARTESIAN_POINT('Ctrl Pts',(-0.991722264000057,11.6,-11.295098011));
#299774=CARTESIAN_POINT('Ctrl Pts',(-0.990531071000056,15.2,-11.298504835));
#299775=CARTESIAN_POINT('Ctrl Pts',(-0.990531071000056,11.6,-11.298504835));
#299776=CARTESIAN_POINT('Ctrl Pts',(-0.989335715000056,15.2,-11.301915096));
#299777=CARTESIAN_POINT('Ctrl Pts',(-0.989335715000056,11.6,-11.301915096));
#299778=CARTESIAN_POINT('Ctrl Pts',(-0.988136191000055,15.2,-11.305328786));
#299779=CARTESIAN_POINT('Ctrl Pts',(-0.988136191000055,11.6,-11.305328786));
#299780=CARTESIAN_POINT('Ctrl Pts',(-0.986932499000056,15.2,-11.308745895));
#299781=CARTESIAN_POINT('Ctrl Pts',(-0.986932499000056,11.6,-11.308745895));
#299782=CARTESIAN_POINT('Ctrl Pts',(-0.985724632000055,15.2,-11.312166416));
#299783=CARTESIAN_POINT('Ctrl Pts',(-0.985724632000055,11.6,-11.312166416));
#299784=CARTESIAN_POINT('Ctrl Pts',(-0.984512591000056,15.2,-11.315590339));
#299785=CARTESIAN_POINT('Ctrl Pts',(-0.984512591000056,11.6,-11.315590339));
#299786=CARTESIAN_POINT('Ctrl Pts',(-0.983296369000056,15.2,-11.319017654));
#299787=CARTESIAN_POINT('Ctrl Pts',(-0.983296369000056,11.6,-11.319017654));
#299788=CARTESIAN_POINT('Ctrl Pts',(-0.982075966000057,15.2,-11.322448353));
#299789=CARTESIAN_POINT('Ctrl Pts',(-0.982075966000057,11.6,-11.322448353));
#299790=CARTESIAN_POINT('Ctrl Pts',(-0.980851378000055,15.2,-11.325882426));
#299791=CARTESIAN_POINT('Ctrl Pts',(-0.980851378000055,11.6,-11.325882426));
#299792=CARTESIAN_POINT('Ctrl Pts',(-0.979622600000055,15.2,-11.329319866));
#299793=CARTESIAN_POINT('Ctrl Pts',(-0.979622600000055,11.6,-11.329319866));
#299794=CARTESIAN_POINT('Ctrl Pts',(-0.978389633000055,15.2,-11.332760663));
#299795=CARTESIAN_POINT('Ctrl Pts',(-0.978389633000055,11.6,-11.332760663));
#299796=CARTESIAN_POINT('Ctrl Pts',(-0.977152471000055,15.2,-11.336204808));
#299797=CARTESIAN_POINT('Ctrl Pts',(-0.977152471000055,11.6,-11.336204808));
#299798=CARTESIAN_POINT('Ctrl Pts',(-0.975911111000055,15.2,-11.339652292));
#299799=CARTESIAN_POINT('Ctrl Pts',(-0.975911111000055,11.6,-11.339652292));
#299800=CARTESIAN_POINT('Ctrl Pts',(-0.974665552000056,15.2,-11.343103107));
#299801=CARTESIAN_POINT('Ctrl Pts',(-0.974665552000056,11.6,-11.343103107));
#299802=CARTESIAN_POINT('Ctrl Pts',(-0.973415788000055,15.2,-11.346557243));
#299803=CARTESIAN_POINT('Ctrl Pts',(-0.973415788000055,11.6,-11.346557243));
#299804=CARTESIAN_POINT('Ctrl Pts',(-0.972161820000055,15.2,-11.350014692));
#299805=CARTESIAN_POINT('Ctrl Pts',(-0.972161820000055,11.6,-11.350014692));
#299806=CARTESIAN_POINT('Ctrl Pts',(-0.970903641000056,15.2,-11.353475444));
#299807=CARTESIAN_POINT('Ctrl Pts',(-0.970903641000056,11.6,-11.353475444));
#299808=CARTESIAN_POINT('Ctrl Pts',(-0.969641251000055,15.2,-11.356939492));
#299809=CARTESIAN_POINT('Ctrl Pts',(-0.969641251000055,11.6,-11.356939492));
#299810=CARTESIAN_POINT('Ctrl Pts',(-0.968374645000055,15.2,-11.360406825));
#299811=CARTESIAN_POINT('Ctrl Pts',(-0.968374645000055,11.6,-11.360406825));
#299812=CARTESIAN_POINT('Ctrl Pts',(-0.967103822000055,15.2,-11.363877435));
#299813=CARTESIAN_POINT('Ctrl Pts',(-0.967103822000055,11.6,-11.363877435));
#299814=CARTESIAN_POINT('Ctrl Pts',(-0.965828779000055,15.2,-11.367351314));
#299815=CARTESIAN_POINT('Ctrl Pts',(-0.965828779000055,11.6,-11.367351314));
#299816=CARTESIAN_POINT('Ctrl Pts',(-0.964549511000056,15.2,-11.370828453));
#299817=CARTESIAN_POINT('Ctrl Pts',(-0.964549511000056,11.6,-11.370828453));
#299818=CARTESIAN_POINT('Ctrl Pts',(-0.963266016000055,15.2,-11.374308843));
#299819=CARTESIAN_POINT('Ctrl Pts',(-0.963266016000055,11.6,-11.374308843));
#299820=CARTESIAN_POINT('Ctrl Pts',(-0.961978293000056,15.2,-11.377792477));
#299821=CARTESIAN_POINT('Ctrl Pts',(-0.961978293000056,11.6,-11.377792477));
#299822=CARTESIAN_POINT('Ctrl Pts',(-0.960686338000055,15.2,-11.381279343));
#299823=CARTESIAN_POINT('Ctrl Pts',(-0.960686338000055,11.6,-11.381279343));
#299824=CARTESIAN_POINT('Ctrl Pts',(-0.959390148000056,15.2,-11.384769435));
#299825=CARTESIAN_POINT('Ctrl Pts',(-0.959390148000056,11.6,-11.384769435));
#299826=CARTESIAN_POINT('Ctrl Pts',(-0.958089718000057,15.2,-11.388262743));
#299827=CARTESIAN_POINT('Ctrl Pts',(-0.958089718000057,11.6,-11.388262743));
#299828=CARTESIAN_POINT('Ctrl Pts',(-0.956785050000055,15.2,-11.391759258));
#299829=CARTESIAN_POINT('Ctrl Pts',(-0.956785050000055,11.6,-11.391759258));
#299830=CARTESIAN_POINT('Ctrl Pts',(-0.955476137000056,15.2,-11.39525897));
#299831=CARTESIAN_POINT('Ctrl Pts',(-0.955476137000056,11.6,-11.39525897));
#299832=CARTESIAN_POINT('Ctrl Pts',(-0.954162977000056,15.2,-11.398761871));
#299833=CARTESIAN_POINT('Ctrl Pts',(-0.954162977000056,11.6,-11.398761871));
#299834=CARTESIAN_POINT('Ctrl Pts',(-0.952845568000056,15.2,-11.402267952));
#299835=CARTESIAN_POINT('Ctrl Pts',(-0.952845568000056,11.6,-11.402267952));
#299836=CARTESIAN_POINT('Ctrl Pts',(-0.951523907000055,15.2,-11.405777207));
#299837=CARTESIAN_POINT('Ctrl Pts',(-0.951523907000055,11.6,-11.405777207));
#299838=CARTESIAN_POINT('Ctrl Pts',(-0.950197992000056,15.2,-11.409289625));
#299839=CARTESIAN_POINT('Ctrl Pts',(-0.950197992000056,11.6,-11.409289625));
#299840=CARTESIAN_POINT('Ctrl Pts',(-0.948867819000055,15.2,-11.4128052));
#299841=CARTESIAN_POINT('Ctrl Pts',(-0.948867819000055,11.6,-11.4128052));
#299842=CARTESIAN_POINT('Ctrl Pts',(-0.947533388000057,15.2,-11.416323924));
#299843=CARTESIAN_POINT('Ctrl Pts',(-0.947533388000057,11.6,-11.416323924));
#299844=CARTESIAN_POINT('Ctrl Pts',(-0.946194693000055,15.2,-11.419845789));
#299845=CARTESIAN_POINT('Ctrl Pts',(-0.946194693000055,11.6,-11.419845789));
#299846=CARTESIAN_POINT('Ctrl Pts',(-0.944851735000055,15.2,-11.423370784));
#299847=CARTESIAN_POINT('Ctrl Pts',(-0.944851735000055,11.6,-11.423370784));
#299848=CARTESIAN_POINT('Ctrl Pts',(-0.943504508000055,15.2,-11.426898902));
#299849=CARTESIAN_POINT('Ctrl Pts',(-0.943504508000055,11.6,-11.426898902));
#299850=CARTESIAN_POINT('Ctrl Pts',(-0.942153010000055,15.2,-11.430430131));
#299851=CARTESIAN_POINT('Ctrl Pts',(-0.942153010000055,11.6,-11.430430131));
#299852=CARTESIAN_POINT('Ctrl Pts',(-0.940797238000056,15.2,-11.433964459));
#299853=CARTESIAN_POINT('Ctrl Pts',(-0.940797238000056,11.6,-11.433964459));
#299854=CARTESIAN_POINT('Ctrl Pts',(-0.939437187000056,15.2,-11.437501879));
#299855=CARTESIAN_POINT('Ctrl Pts',(-0.939437187000056,11.6,-11.437501879));
#299856=CARTESIAN_POINT('Ctrl Pts',(-0.938072856000056,15.2,-11.441042379));
#299857=CARTESIAN_POINT('Ctrl Pts',(-0.938072856000056,11.6,-11.441042379));
#299858=CARTESIAN_POINT('Ctrl Pts',(-0.936704242000056,15.2,-11.444585951));
#299859=CARTESIAN_POINT('Ctrl Pts',(-0.936704242000056,11.6,-11.444585951));
#299860=CARTESIAN_POINT('Ctrl Pts',(-0.935331342000056,15.2,-11.448132592));
#299861=CARTESIAN_POINT('Ctrl Pts',(-0.935331342000056,11.6,-11.448132592));
#299862=CARTESIAN_POINT('Ctrl Pts',(-0.933954157000055,15.2,-11.451682295));
#299863=CARTESIAN_POINT('Ctrl Pts',(-0.933954157000055,11.6,-11.451682295));
#299864=CARTESIAN_POINT('Ctrl Pts',(-0.932572685000055,15.2,-11.45523506));
#299865=CARTESIAN_POINT('Ctrl Pts',(-0.932572685000055,11.6,-11.45523506));
#299866=CARTESIAN_POINT('Ctrl Pts',(-0.931464077000056,15.2,-11.45807972));
#299867=CARTESIAN_POINT('Ctrl Pts',(-0.931464077000056,11.6,-11.45807972));
#299868=CARTESIAN_POINT('Ctrl Pts',(-0.930630693000056,15.2,-11.460214591));
#299869=CARTESIAN_POINT('Ctrl Pts',(-0.930630693000056,11.6,-11.460214591));
#299870=CARTESIAN_POINT('Ctrl Pts',(-0.930074247000056,15.2,-11.461638451));
#299871=CARTESIAN_POINT('Ctrl Pts',(-0.930074247000056,11.6,-11.461638451));
#299872=CARTESIAN_POINT('Ctrl Pts',(-0.929795809000057,15.2,-11.462350534));
#299873=CARTESIAN_POINT('Ctrl Pts',(-0.929795809000057,11.6,-11.462350534));
#299874=CARTESIAN_POINT('Ctrl Pts',(-1.18690176600006,12.2,-10.306885524));
#299875=CARTESIAN_POINT('Ctrl Pts',(-1.18695287825247,12.2,-10.3086714504511));
#299876=CARTESIAN_POINT('Ctrl Pts',(-1.18700024431844,12.2,-10.3105146700777));
#299877=CARTESIAN_POINT('Ctrl Pts',(-1.18704320796202,12.2,-10.3124142312835));
#299878=CARTESIAN_POINT('Ctrl Pts',(-1.18708637879801,12.2,-10.3143229531337));
#299879=CARTESIAN_POINT('Ctrl Pts',(-1.18712509994175,12.2,-10.3162885639395));
#299880=CARTESIAN_POINT('Ctrl Pts',(-1.1871587090283,12.2,-10.3183101249039));
#299881=CARTESIAN_POINT('Ctrl Pts',(-1.1871923181118,12.2,-10.3203316856847));
#299882=CARTESIAN_POINT('Ctrl Pts',(-1.18722081733423,12.2,-10.322409198819));
#299883=CARTESIAN_POINT('Ctrl Pts',(-1.18724356650007,12.2,-10.3245417524916));
#299884=CARTESIAN_POINT('Ctrl Pts',(-1.18726631566591,12.2,-10.3266743061641));
#299885=CARTESIAN_POINT('Ctrl Pts',(-1.18728331741518,12.2,-10.3288618993474));
#299886=CARTESIAN_POINT('Ctrl Pts',(-1.18729394974902,12.2,-10.3311036472915));
#299887=CARTESIAN_POINT('Ctrl Pts',(-1.18730458208384,12.2,-10.3333453954392));
#299888=CARTESIAN_POINT('Ctrl Pts',(-1.18730884758373,12.2,-10.335641298191));
#299889=CARTESIAN_POINT('Ctrl Pts',(-1.18730614774977,12.2,-10.3379904903227));
#299890=CARTESIAN_POINT('Ctrl Pts',(-1.18730344791606,12.2,-10.3403396822409));
#299891=CARTESIAN_POINT('Ctrl Pts',(-1.18729378039953,12.2,-10.3427421643207));
#299892=CARTESIAN_POINT('Ctrl Pts',(-1.18727656873339,12.2,-10.3451970944927));
#299893=CARTESIAN_POINT('Ctrl Pts',(-1.18725935706726,12.2,-10.3476520246647));
#299894=CARTESIAN_POINT('Ctrl Pts',(-1.18723459815028,12.2,-10.3501594023475));
#299895=CARTESIAN_POINT('Ctrl Pts',(-1.18720173348516,12.2,-10.3527184083357));
#299896=CARTESIAN_POINT('Ctrl Pts',(-1.18716886881705,12.2,-10.3552774145562));
#299897=CARTESIAN_POINT('Ctrl Pts',(-1.18712789608962,12.2,-10.3578880464332));
#299898=CARTESIAN_POINT('Ctrl Pts',(-1.18707827150299,12.2,-10.3605495048317));
#299899=CARTESIAN_POINT('Ctrl Pts',(-1.18702864692087,12.2,-10.3632109629885));
#299900=CARTESIAN_POINT('Ctrl Pts',(-1.18697036877764,12.2,-10.3659232462155));
#299901=CARTESIAN_POINT('Ctrl Pts',(-1.18690291127969,12.2,-10.3686855726173));
#299902=CARTESIAN_POINT('Ctrl Pts',(-1.18683545378174,12.2,-10.3714478990192));
#299903=CARTESIAN_POINT('Ctrl Pts',(-1.18675881418451,12.2,-10.3742602688836));
#299904=CARTESIAN_POINT('Ctrl Pts',(-1.18667248268807,12.2,-10.3771219181108));
#299905=CARTESIAN_POINT('Ctrl Pts',(-1.18658615119163,12.2,-10.379983567338));
#299906=CARTESIAN_POINT('Ctrl Pts',(-1.18649012644043,12.2,-10.3828944944465));
#299907=CARTESIAN_POINT('Ctrl Pts',(-1.18638390927832,12.2,-10.385853953919));
#299908=CARTESIAN_POINT('Ctrl Pts',(-1.18627769210655,12.2,-10.3888134136604));
#299909=CARTESIAN_POINT('Ctrl Pts',(-1.18616128558383,12.2,-10.3918214053147));
#299910=CARTESIAN_POINT('Ctrl Pts',(-1.1860342042431,12.2,-10.39487719815));
#299911=CARTESIAN_POINT('Ctrl Pts',(-1.18590712291392,12.2,-10.3979329907077));
#299912=CARTESIAN_POINT('Ctrl Pts',(-1.18576936691205,12.2,-10.4010365852655));
#299913=CARTESIAN_POINT('Ctrl Pts',(-1.18562046775014,12.2,-10.4041872659985));
#299914=CARTESIAN_POINT('Ctrl Pts',(-1.18547156858824,12.2,-10.4073379467315));
#299915=CARTESIAN_POINT('Ctrl Pts',(-1.18531152576172,12.2,-10.410535714918));
#299916=CARTESIAN_POINT('Ctrl Pts',(-1.18513988276875,12.2,-10.4137798696303));
#299917=CARTESIAN_POINT('Ctrl Pts',(-1.18496823976018,12.2,-10.4170240246374));
#299918=CARTESIAN_POINT('Ctrl Pts',(-1.18478499820055,12.2,-10.4203145675565));
#299919=CARTESIAN_POINT('Ctrl Pts',(-1.18458971402272,12.2,-10.423650812657));
#299920=CARTESIAN_POINT('Ctrl Pts',(-1.18439442986262,12.2,-10.4269870574544));
#299921=CARTESIAN_POINT('Ctrl Pts',(-1.18418710221816,12.2,-10.4303690046824));
#299922=CARTESIAN_POINT('Ctrl Pts',(-1.18396730047518,12.2,-10.43379598349));
#299923=CARTESIAN_POINT('Ctrl Pts',(-1.18374749873219,12.2,-10.4372229622977));
#299924=CARTESIAN_POINT('Ctrl Pts',(-1.18351522376701,12.2,-10.4406949718391));
#299925=CARTESIAN_POINT('Ctrl Pts',(-1.1832700567768,12.2,-10.444211356625));
#299926=CARTESIAN_POINT('Ctrl Pts',(-1.18302488976432,12.2,-10.4477277417303));
#299927=CARTESIAN_POINT('Ctrl Pts',(-1.18276682798624,12.2,-10.4512885011114));
#299928=CARTESIAN_POINT('Ctrl Pts',(-1.18249546795713,12.2,-10.4548929895738));
#299929=CARTESIAN_POINT('Ctrl Pts',(-1.18222410795266,12.2,-10.4584974777087));
#299930=CARTESIAN_POINT('Ctrl Pts',(-1.18193944638091,12.2,-10.4621456945924));
#299931=CARTESIAN_POINT('Ctrl Pts',(-1.18164108847508,12.2,-10.4658370095416));
#299932=CARTESIAN_POINT('Ctrl Pts',(-1.18134273056926,12.2,-10.4695283244908));
#299933=CARTESIAN_POINT('Ctrl Pts',(-1.18103067595189,12.2,-10.473262737469));
#299934=CARTESIAN_POINT('Ctrl Pts',(-1.1807045372816,12.2,-10.4770396258513));
#299935=CARTESIAN_POINT('Ctrl Pts',(-1.18037839858167,12.2,-10.4808165145767));
#299936=CARTESIAN_POINT('Ctrl Pts',(-1.1800381776234,12.2,-10.4846358832492));
#299937=CARTESIAN_POINT('Ctrl Pts',(-1.17968349868642,12.2,-10.4884971177125));
#299938=CARTESIAN_POINT('Ctrl Pts',(-1.17932881978165,12.2,-10.4923583518251));
#299939=CARTESIAN_POINT('Ctrl Pts',(-1.17895967939607,12.2,-10.4962614543104));
#299940=CARTESIAN_POINT('Ctrl Pts',(-1.17857571749157,12.2,-10.5002058275184));
#299941=CARTESIAN_POINT('Ctrl Pts',(-1.17819175558708,12.2,-10.5041502007264));
#299942=CARTESIAN_POINT('Ctrl Pts',(-1.17779296731521,12.2,-10.5081358447371));
#299943=CARTESIAN_POINT('Ctrl Pts',(-1.17737899874758,12.2,-10.5121621710057));
#299944=CARTESIAN_POINT('Ctrl Pts',(-1.17703402492869,12.2,-10.5155174430181));
#299945=CARTESIAN_POINT('Ctrl Pts',(-1.17667850924008,12.2,-10.5189009680785));
#299946=CARTESIAN_POINT('Ctrl Pts',(-1.1763122502823,12.2,-10.5223124107853));
#299947=CARTESIAN_POINT('Ctrl Pts',(-1.17594599132453,12.2,-10.5257238534922));
#299948=CARTESIAN_POINT('Ctrl Pts',(-1.17556898840758,12.2,-10.5291632140324));
#299949=CARTESIAN_POINT('Ctrl Pts',(-1.17518104472529,12.2,-10.5326301642564));
#299950=CARTESIAN_POINT('Ctrl Pts',(-1.17479310104301,12.2,-10.5360971144804));
#299951=CARTESIAN_POINT('Ctrl Pts',(-1.17439421778898,12.2,-10.5395916512833));
#299952=CARTESIAN_POINT('Ctrl Pts',(-1.17398420077509,12.2,-10.5431134539916));
#299953=CARTESIAN_POINT('Ctrl Pts',(-1.1735741837612,12.2,-10.5466352566999));
#299954=CARTESIAN_POINT('Ctrl Pts',(-1.17315303389629,12.2,-10.55018432143));
#299955=CARTESIAN_POINT('Ctrl Pts',(-1.17272056174151,12.2,-10.5537603309602));
#299956=CARTESIAN_POINT('Ctrl Pts',(-1.17228808958674,12.2,-10.5573363404904));
#299957=CARTESIAN_POINT('Ctrl Pts',(-1.17184429560973,12.2,-10.5609392926138));
#299958=CARTESIAN_POINT('Ctrl Pts',(-1.17138899526191,12.2,-10.5645688729625));
#299959=CARTESIAN_POINT('Ctrl Pts',(-1.17093369491408,12.2,-10.5681984533111));
#299960=CARTESIAN_POINT('Ctrl Pts',(-1.17046688745822,12.2,-10.5718546597562));
#299961=CARTESIAN_POINT('Ctrl Pts',(-1.16998839294372,12.2,-10.5755371826743));
#299962=CARTESIAN_POINT('Ctrl Pts',(-1.16950989842922,12.2,-10.5792197055923));
#299963=CARTESIAN_POINT('Ctrl Pts',(-1.16901971706767,12.2,-10.5829285444452));
#299964=CARTESIAN_POINT('Ctrl Pts',(-1.16851767016676,12.2,-10.5866633917169));
#299965=CARTESIAN_POINT('Ctrl Pts',(-1.16791521390756,12.2,-10.5911452082802));
#299966=CARTESIAN_POINT('Ctrl Pts',(-1.16729567313537,12.2,-10.5956644770899));
#299967=CARTESIAN_POINT('Ctrl Pts',(-1.16665874874172,12.2,-10.6002206725085));
#299968=CARTESIAN_POINT('Ctrl Pts',(-1.1661279783944,12.2,-10.604017502162));
#299969=CARTESIAN_POINT('Ctrl Pts',(-1.16558513589678,12.2,-10.6078399757678));
#299970=CARTESIAN_POINT('Ctrl Pts',(-1.16503005228311,12.2,-10.6116877962021));
#299971=CARTESIAN_POINT('Ctrl Pts',(-1.16447496866945,12.2,-10.6155356166363));
#299972=CARTESIAN_POINT('Ctrl Pts',(-1.16390764256274,12.2,-10.6194087828815));
#299973=CARTESIAN_POINT('Ctrl Pts',(-1.1633279106871,12.2,-10.6233069992717));
#299974=CARTESIAN_POINT('Ctrl Pts',(-1.16274817881145,12.2,-10.6272052156619));
#299975=CARTESIAN_POINT('Ctrl Pts',(-1.16215604066112,12.2,-10.6311284828292));
#299976=CARTESIAN_POINT('Ctrl Pts',(-1.16155133295213,12.2,-10.6350765099833));
#299977=CARTESIAN_POINT('Ctrl Pts',(-1.16094662524314,12.2,-10.6390245371374));
#299978=CARTESIAN_POINT('Ctrl Pts',(-1.16032934929836,12.2,-10.6429973217769));
#299979=CARTESIAN_POINT('Ctrl Pts',(-1.15969934499214,12.2,-10.6469945805282));
#299980=CARTESIAN_POINT('Ctrl Pts',(-1.15906934068592,12.2,-10.6509918392795));
#299981=CARTESIAN_POINT('Ctrl Pts',(-1.1584266080187,12.2,-10.6550135687715));
#299982=CARTESIAN_POINT('Ctrl Pts',(-1.15777099270727,12.2,-10.659059485503));
#299983=CARTESIAN_POINT('Ctrl Pts',(-1.15711537739584,12.2,-10.6631054022346));
#299984=CARTESIAN_POINT('Ctrl Pts',(-1.15644687732867,12.2,-10.6671755075668));
#299985=CARTESIAN_POINT('Ctrl Pts',(-1.15576534211927,12.2,-10.6712695190271));
#299986=CARTESIAN_POINT('Ctrl Pts',(-1.15522011399633,12.2,-10.6745447279276));
#299987=CARTESIAN_POINT('Ctrl Pts',(-1.15466654389668,12.2,-10.6778352358539));
#299988=CARTESIAN_POINT('Ctrl Pts',(-1.15410455255429,12.2,-10.6811409039715));
#299989=CARTESIAN_POINT('Ctrl Pts',(-1.15354256113532,12.2,-10.6844465725396));
#299990=CARTESIAN_POINT('Ctrl Pts',(-1.15297215054114,12.2,-10.687767398726));
#299991=CARTESIAN_POINT('Ctrl Pts',(-1.15239324442437,12.2,-10.6911032422424));
#299992=CARTESIAN_POINT('Ctrl Pts',(-1.15166961181785,12.2,-10.6952730464107));
#299993=CARTESIAN_POINT('Ctrl Pts',(-1.15093270666971,12.2,-10.6994663145718));
#299994=CARTESIAN_POINT('Ctrl Pts',(-1.15018238166861,12.2,-10.7036827752681));
#299995=CARTESIAN_POINT('Ctrl Pts',(-1.1495821217168,12.2,-10.7070559435494));
#299996=CARTESIAN_POINT('Ctrl Pts',(-1.14897327395778,12.2,-10.7104439541788));
#299997=CARTESIAN_POINT('Ctrl Pts',(-1.14835576650882,12.2,-10.7138466704553));
#299998=CARTESIAN_POINT('Ctrl Pts',(-1.14773825897573,12.2,-10.7172493871953));
#299999=CARTESIAN_POINT('Ctrl Pts',(-1.14711209039999,12.2,-10.7206668089522));
#300000=CARTESIAN_POINT('Ctrl Pts',(-1.14647719016625,12.2,-10.7240987992564));
#300001=CARTESIAN_POINT('Ctrl Pts',(-1.14584229001901,12.2,-10.727530789093));
#300002=CARTESIAN_POINT('Ctrl Pts',(-1.1451986568661,12.2,-10.7309773469649));
#300003=CARTESIAN_POINT('Ctrl Pts',(-1.14454622158668,12.2,-10.7344383379588));
#300004=CARTESIAN_POINT('Ctrl Pts',(-1.14389378621836,12.2,-10.7378993294243));
#300005=CARTESIAN_POINT('Ctrl Pts',(-1.14323254940177,12.2,-10.7413747540387));
#300006=CARTESIAN_POINT('Ctrl Pts',(-1.14256243942022,12.2,-10.7448644767854));
#300007=CARTESIAN_POINT('Ctrl Pts',(-1.14189232952998,12.2,-10.7483541990566));
#300008=CARTESIAN_POINT('Ctrl Pts',(-1.14121334901333,12.2,-10.7518582199831));
#300009=CARTESIAN_POINT('Ctrl Pts',(-1.14052542709153,12.2,-10.7553764064812));
#300010=CARTESIAN_POINT('Ctrl Pts',(-1.139837505076,12.2,-10.7588945934586));
#300011=CARTESIAN_POINT('Ctrl Pts',(-1.13914064425914,12.2,-10.7624269452319));
#300012=CARTESIAN_POINT('Ctrl Pts',(-1.1384347754423,12.2,-10.765973330815));
#300013=CARTESIAN_POINT('Ctrl Pts',(-1.13772890672163,12.2,-10.7695197159149));
#300014=CARTESIAN_POINT('Ctrl Pts',(-1.13701403064168,12.2,-10.773080135087));
#300015=CARTESIAN_POINT('Ctrl Pts',(-1.13629008136845,12.2,-10.7766544566822));
#300016=CARTESIAN_POINT('Ctrl Pts',(-1.13556613199659,12.2,-10.7802287787645));
#300017=CARTESIAN_POINT('Ctrl Pts',(-1.13483310857954,12.2,-10.7838170034258));
#300018=CARTESIAN_POINT('Ctrl Pts',(-1.13409094725792,12.2,-10.7874190010274));
#300019=CARTESIAN_POINT('Ctrl Pts',(-1.13334878603741,12.2,-10.7910209981382));
#300020=CARTESIAN_POINT('Ctrl Pts',(-1.13259748752799,12.2,-10.7946367690074));
#300021=CARTESIAN_POINT('Ctrl Pts',(-1.1318369855911,12.2,-10.7982661834316));
#300022=CARTESIAN_POINT('Ctrl Pts',(-1.13107648355059,12.2,-10.8018955983502));
#300023=CARTESIAN_POINT('Ctrl Pts',(-1.13030677830366,12.2,-10.805538657284));
#300024=CARTESIAN_POINT('Ctrl Pts',(-1.12952780948343,12.2,-10.8091952334833));
#300025=CARTESIAN_POINT('Ctrl Pts',(-1.1287488406632,12.2,-10.8128518096826));
#300026=CARTESIAN_POINT('Ctrl Pts',(-1.12796060426689,12.2,-10.8165219040584));
#300027=CARTESIAN_POINT('Ctrl Pts',(-1.12716304161135,12.2,-10.8202053870939));
#300028=CARTESIAN_POINT('Ctrl Pts',(-1.12636547906449,12.2,-10.8238888696274));
#300029=CARTESIAN_POINT('Ctrl Pts',(-1.12555858903203,12.2,-10.8275857441339));
#300030=CARTESIAN_POINT('Ctrl Pts',(-1.12474231098398,12.2,-10.8312958825141));
#300031=CARTESIAN_POINT('Ctrl Pts',(-1.12392603282471,12.2,-10.8350060213998));
#300032=CARTESIAN_POINT('Ctrl Pts',(-1.12310036603225,12.2,-10.8387294255531));
#300033=CARTESIAN_POINT('Ctrl Pts',(-1.12226525009688,12.2,-10.8424659703692));
#300034=CARTESIAN_POINT('Ctrl Pts',(-1.12143013427529,12.2,-10.8462025146762));
#300035=CARTESIAN_POINT('Ctrl Pts',(-1.12058556989661,12.2,-10.8499521982037));
#300036=CARTESIAN_POINT('Ctrl Pts',(-1.11973149857816,12.2,-10.8537148999508));
#300037=CARTESIAN_POINT('Ctrl Pts',(-1.11887742714334,12.2,-10.8574776022106));
#300038=CARTESIAN_POINT('Ctrl Pts',(-1.11801384703482,12.2,-10.8612533213057));
#300039=CARTESIAN_POINT('Ctrl Pts',(-1.11714070166501,12.2,-10.8650419357581));
#300040=CARTESIAN_POINT('Ctrl Pts',(-1.11626755641416,12.2,-10.8688305496943));
#300041=CARTESIAN_POINT('Ctrl Pts',(-1.11538484398271,12.2,-10.8726320577176));
#300042=CARTESIAN_POINT('Ctrl Pts',(-1.11449250938962,12.2,-10.8764463394049));
#300043=CARTESIAN_POINT('Ctrl Pts',(-1.11360017467495,12.2,-10.880260621612));
#300044=CARTESIAN_POINT('Ctrl Pts',(-1.11269821636468,12.2,-10.8840876768928));
#300045=CARTESIAN_POINT('Ctrl Pts',(-1.11178657842548,12.2,-10.8879273845473));
#300046=CARTESIAN_POINT('Ctrl Pts',(-1.11087494061048,12.2,-10.8917670916787));
#300047=CARTESIAN_POINT('Ctrl Pts',(-1.10995362280469,12.2,-10.895619452441));
#300048=CARTESIAN_POINT('Ctrl Pts',(-1.10902257016848,12.2,-10.8994843452059));
#300049=CARTESIAN_POINT('Ctrl Pts',(-1.1080915174054,12.2,-10.9033492384974));
#300050=CARTESIAN_POINT('Ctrl Pts',(-1.10715072837752,12.2,-10.9072266649192));
#300051=CARTESIAN_POINT('Ctrl Pts',(-1.10620015038063,12.2,-10.9111165070764));
#300052=CARTESIAN_POINT('Ctrl Pts',(-1.10524957251325,12.2,-10.9150063487037));
#300053=CARTESIAN_POINT('Ctrl Pts',(-1.10428920475062,12.2,-10.9189086035368));
#300054=CARTESIAN_POINT('Ctrl Pts',(-1.10331899294205,12.2,-10.9228231553266));
#300055=CARTESIAN_POINT('Ctrl Pts',(-1.1021062280822,12.2,-10.9277163454639));
#300056=CARTESIAN_POINT('Ctrl Pts',(-1.10087808131704,12.2,-10.9326287483732));
#300057=CARTESIAN_POINT('Ctrl Pts',(-1.09963445138776,12.2,-10.9375601383716));
#300058=CARTESIAN_POINT('Ctrl Pts',(-1.0986395473901,12.2,-10.9415052505854));
#300059=CARTESIAN_POINT('Ctrl Pts',(-1.09763473318157,12.2,-10.9454625118544));
#300060=CARTESIAN_POINT('Ctrl Pts',(-1.09661995723274,12.2,-10.9494318094777));
#300061=CARTESIAN_POINT('Ctrl Pts',(-1.09535148736582,12.2,-10.9543934312364));
#300062=CARTESIAN_POINT('Ctrl Pts',(-1.09406745206026,12.2,-10.9593738575205));
#300063=CARTESIAN_POINT('Ctrl Pts',(-1.092767751365,12.2,-10.9643728628687));
#300064=CARTESIAN_POINT('Ctrl Pts',(-1.09120811058736,12.2,-10.9703716690685));
#300065=CARTESIAN_POINT('Ctrl Pts',(-1.08962591292817,12.2,-10.9763972332329));
#300066=CARTESIAN_POINT('Ctrl Pts',(-1.0880209873208,12.2,-10.9824491664286));
#300067=CARTESIAN_POINT('Ctrl Pts',(-1.0869510368187,12.2,-10.9864837889255));
#300068=CARTESIAN_POINT('Ctrl Pts',(-1.08587098690105,12.2,-10.9905301328751));
#300069=CARTESIAN_POINT('Ctrl Pts',(-1.08478078634185,12.2,-10.9945880848555));
#300070=CARTESIAN_POINT('Ctrl Pts',(-1.08369058593118,12.2,-10.9986460362831));
#300071=CARTESIAN_POINT('Ctrl Pts',(-1.08259023533267,12.2,-11.0027155968092));
#300072=CARTESIAN_POINT('Ctrl Pts',(-1.08147968809079,12.2,-11.0067966526415));
#300073=CARTESIAN_POINT('Ctrl Pts',(-1.08036914069759,12.2,-11.0108777090298));
#300074=CARTESIAN_POINT('Ctrl Pts',(-1.07924839501429,12.2,-11.0149702620389));
#300075=CARTESIAN_POINT('Ctrl Pts',(-1.07811740384087,12.2,-11.0190741998189));
#300076=CARTESIAN_POINT('Ctrl Pts',(-1.07698641282155,12.2,-11.0231781370397));
#300077=CARTESIAN_POINT('Ctrl Pts',(-1.07584517752686,12.2,-11.0272934596389));
#300078=CARTESIAN_POINT('Ctrl Pts',(-1.07469364917547,12.2,-11.0314200576179));
#300079=CARTESIAN_POINT('Ctrl Pts',(-1.07354212066718,12.2,-11.0355466561591));
#300080=CARTESIAN_POINT('Ctrl Pts',(-1.07238030022707,12.2,-11.0396845286402));
#300081=CARTESIAN_POINT('Ctrl Pts',(-1.07120814166251,12.2,-11.0438335670893));
#300082=CARTESIAN_POINT('Ctrl Pts',(-1.07003598325766,12.2,-11.047982604973));
#300083=CARTESIAN_POINT('Ctrl Pts',(-1.06885348792987,12.2,-11.0521428083879));
#300084=CARTESIAN_POINT('Ctrl Pts',(-1.06766060769512,12.2,-11.056314068268));
#300085=CARTESIAN_POINT('Ctrl Pts',(-1.06646772729784,12.2,-11.0604853287164));
#300086=CARTESIAN_POINT('Ctrl Pts',(-1.06526446461823,12.2,-11.0646676462495));
#300087=CARTESIAN_POINT('Ctrl Pts',(-1.06405077349099,12.2,-11.0688609120526));
#300088=CARTESIAN_POINT('Ctrl Pts',(-1.06283708252911,12.2,-11.0730541772845));
#300089=CARTESIAN_POINT('Ctrl Pts',(-1.0616129635194,12.2,-11.0772583904787));
#300090=CARTESIAN_POINT('Ctrl Pts',(-1.06037837367695,12.2,-11.0814734455775));
#300091=CARTESIAN_POINT('Ctrl Pts',(-1.05914378366628,12.2,-11.0856885012506));
#300092=CARTESIAN_POINT('Ctrl Pts',(-1.05789872042964,12.2,-11.0899143988024));
#300093=CARTESIAN_POINT('Ctrl Pts',(-1.0566431432501,12.2,-11.0941510300333));
#300094=CARTESIAN_POINT('Ctrl Pts',(-1.05538756607056,12.2,-11.0983876612642));
#300095=CARTESIAN_POINT('Ctrl Pts',(-1.05412147367313,12.2,-11.1026350272852));
#300096=CARTESIAN_POINT('Ctrl Pts',(-1.05284482382469,12.2,-11.1068930229628));
#300097=CARTESIAN_POINT('Ctrl Pts',(-1.05188733652533,12.2,-11.110086519431));
#300098=CARTESIAN_POINT('Ctrl Pts',(-1.05092391055972,12.2,-11.1132859934258));
#300099=CARTESIAN_POINT('Ctrl Pts',(-1.04995452829582,12.2,-11.1164914026369));
#300100=CARTESIAN_POINT('Ctrl Pts',(-1.04898514603192,12.2,-11.1196968118479));
#300101=CARTESIAN_POINT('Ctrl Pts',(-1.04800980859123,12.2,-11.1229081555005));
#300102=CARTESIAN_POINT('Ctrl Pts',(-1.04702849637637,12.2,-11.1261253890924));
#300103=CARTESIAN_POINT('Ctrl Pts',(-1.0460471841615,12.2,-11.1293426226844));
#300104=CARTESIAN_POINT('Ctrl Pts',(-1.04505989848068,12.2,-11.1325657464673));
#300105=CARTESIAN_POINT('Ctrl Pts',(-1.0440666217251,12.2,-11.135794716475));
#300106=CARTESIAN_POINT('Ctrl Pts',(-1.04307334496953,12.2,-11.1390236864826));
#300107=CARTESIAN_POINT('Ctrl Pts',(-1.04207407795586,12.2,-11.1422585019318));
#300108=CARTESIAN_POINT('Ctrl Pts',(-1.0410688026179,12.2,-11.1454991204385));
#300109=CARTESIAN_POINT('Ctrl Pts',(-1.04006352727995,12.2,-11.1487397389453));
#300110=CARTESIAN_POINT('Ctrl Pts',(-1.03905224281003,12.2,-11.1519861597272));
#300111=CARTESIAN_POINT('Ctrl Pts',(-1.03803493396353,12.2,-11.1552383398958));
#300112=CARTESIAN_POINT('Ctrl Pts',(-1.03667852204499,12.2,-11.1595745805146));
#300113=CARTESIAN_POINT('Ctrl Pts',(-1.03531139892148,12.2,-11.1639210583515));
#300114=CARTESIAN_POINT('Ctrl Pts',(-1.03393352634569,12.2,-11.1682776715896));
#300115=CARTESIAN_POINT('Ctrl Pts',(-1.03290012200771,12.2,-11.1715451312213));
#300116=CARTESIAN_POINT('Ctrl Pts',(-1.03186066979545,12.2,-11.1748182919858));
#300117=CARTESIAN_POINT('Ctrl Pts',(-1.0308151545001,12.2,-11.1780971109916));
#300118=CARTESIAN_POINT('Ctrl Pts',(-1.02976963920475,12.2,-11.1813759299975));
#300119=CARTESIAN_POINT('Ctrl Pts',(-1.02871806089299,12.2,-11.1846604057448));
#300120=CARTESIAN_POINT('Ctrl Pts',(-1.02766040264028,12.2,-11.1879504986248));
#300121=CARTESIAN_POINT('Ctrl Pts',(-1.02660274438757,12.2,-11.1912405915048));
#300122=CARTESIAN_POINT('Ctrl Pts',(-1.02553900620423,12.2,-11.1945362977003));
#300123=CARTESIAN_POINT('Ctrl Pts',(-1.02446917244036,12.2,-11.1978375779113));
#300124=CARTESIAN_POINT('Ctrl Pts',(-1.02339933867648,12.2,-11.2011388581223));
#300125=CARTESIAN_POINT('Ctrl Pts',(-1.02232340989583,12.2,-11.2044457113823));
#300126=CARTESIAN_POINT('Ctrl Pts',(-1.02124136872764,12.2,-11.2077580940112));
#300127=CARTESIAN_POINT('Ctrl Pts',(-1.02015932736289,12.2,-11.2110704772419));
#300128=CARTESIAN_POINT('Ctrl Pts',(-1.01907117593808,12.2,-11.2143883908241));
#300129=CARTESIAN_POINT('Ctrl Pts',(-1.01797689606987,12.2,-11.2177117920161));
#300130=CARTESIAN_POINT('Ctrl Pts',(-1.01688261640046,12.2,-11.2210351926045));
#300131=CARTESIAN_POINT('Ctrl Pts',(-1.01578220987305,12.2,-11.2243640805508));
#300132=CARTESIAN_POINT('Ctrl Pts',(-1.01467566112105,12.2,-11.2276984150968));
#300133=CARTESIAN_POINT('Ctrl Pts',(-1.01356911236905,12.2,-11.2310327496428));
#300134=CARTESIAN_POINT('Ctrl Pts',(-1.01245642023021,12.2,-11.234372529426));
#300135=CARTESIAN_POINT('Ctrl Pts',(-1.01133757097408,12.2,-11.237717713528));
#300136=CARTESIAN_POINT('Ctrl Pts',(-1.01021872171795,12.2,-11.24106289763));
#300137=CARTESIAN_POINT('Ctrl Pts',(-1.0090937146818,12.2,-11.2444134863703));
#300138=CARTESIAN_POINT('Ctrl Pts',(-1.00796253446779,12.2,-11.2477694365136));
#300139=CARTESIAN_POINT('Ctrl Pts',(-1.00683135425378,12.2,-11.2511253866569));
#300140=CARTESIAN_POINT('Ctrl Pts',(-1.00569400209922,12.2,-11.2544866990392));
#300141=CARTESIAN_POINT('Ctrl Pts',(-1.00455046143297,12.2,-11.2578533321664));
#300142=CARTESIAN_POINT('Ctrl Pts',(-1.00340692076673,12.2,-11.2612199652937));
#300143=CARTESIAN_POINT('Ctrl Pts',(-1.00225719315924,12.2,-11.2645919192038));
#300144=CARTESIAN_POINT('Ctrl Pts',(-1.00110126249375,12.2,-11.2679691532471));
#300145=CARTESIAN_POINT('Ctrl Pts',(-0.999945331618268,12.2,-11.2713463879039));
#300146=CARTESIAN_POINT('Ctrl Pts',(-0.998783197949374,12.2,-11.2747289010454));
#300147=CARTESIAN_POINT('Ctrl Pts',(-0.997614847945394,12.2,-11.2781166527468));
#300148=CARTESIAN_POINT('Ctrl Pts',(-0.996446498153665,12.2,-11.2815044038328));
#300149=CARTESIAN_POINT('Ctrl Pts',(-0.99527193062893,12.2,-11.2848973936268));
#300150=CARTESIAN_POINT('Ctrl Pts',(-0.99409113237962,12.2,-11.2882955811705));
#300151=CARTESIAN_POINT('Ctrl Pts',(-0.992910334130311,12.2,-11.2916937687141));
#300152=CARTESIAN_POINT('Ctrl Pts',(-0.991723304977775,12.2,-11.2950971526781));
#300153=CARTESIAN_POINT('Ctrl Pts',(-0.990530030224015,12.2,-11.2985056942781));
#300154=CARTESIAN_POINT('Ctrl Pts',(-0.988938997291261,12.2,-11.303050416205));
#300155=CARTESIAN_POINT('Ctrl Pts',(-0.987336860897517,12.2,-11.3076043045723));
#300156=CARTESIAN_POINT('Ctrl Pts',(-0.985723588697198,12.2,-11.3121672657539));
#300157=CARTESIAN_POINT('Ctrl Pts',(-0.98411031627707,12.2,-11.3167302275573));
#300158=CARTESIAN_POINT('Ctrl Pts',(-0.982485908194793,12.2,-11.3213022597531));
#300159=CARTESIAN_POINT('Ctrl Pts',(-0.980850330550103,12.2,-11.325883267725));
#300160=CARTESIAN_POINT('Ctrl Pts',(-0.979623647428009,12.2,-11.3293190233918));
#300161=CARTESIAN_POINT('Ctrl Pts',(-0.97839068277283,12.2,-11.3327598287168));
#300162=CARTESIAN_POINT('Ctrl Pts',(-0.97715142165174,12.2,-11.3362056423828));
#300163=CARTESIAN_POINT('Ctrl Pts',(-0.97591216053065,12.2,-11.3396514560488));
#300164=CARTESIAN_POINT('Ctrl Pts',(-0.974666603441903,12.2,-11.3431022787682));
#300165=CARTESIAN_POINT('Ctrl Pts',(-0.973414737175575,12.2,-11.3465580705648));
#300166=CARTESIAN_POINT('Ctrl Pts',(-0.972162870909247,12.2,-11.3500138623613));
#300167=CARTESIAN_POINT('Ctrl Pts',(-0.970904695512285,12.2,-11.3534746229377));
#300168=CARTESIAN_POINT('Ctrl Pts',(-0.969640197309087,12.2,-11.3569403125195));
#300169=CARTESIAN_POINT('Ctrl Pts',(-0.968375698876171,12.2,-11.3604060027308));
#300170=CARTESIAN_POINT('Ctrl Pts',(-0.967104878474818,12.2,-11.3638766210019));
#300171=CARTESIAN_POINT('Ctrl Pts',(-0.965827722496673,12.2,-11.3673521297576));
#300172=CARTESIAN_POINT('Ctrl Pts',(-0.964550566750545,12.2,-11.370827637882));
#300173=CARTESIAN_POINT('Ctrl Pts',(-0.963267074113089,12.2,-11.3743080363062));
#300174=CARTESIAN_POINT('Ctrl Pts',(-0.961977234867734,12.2,-11.37779328543));
#300175=CARTESIAN_POINT('Ctrl Pts',(-0.96068739562238,12.2,-11.3812785345537));
#300176=CARTESIAN_POINT('Ctrl Pts',(-0.959391207590864,12.2,-11.3847686341476));
#300177=CARTESIAN_POINT('Ctrl Pts',(-0.958088658423916,12.2,-11.3882635447448));
#300178=CARTESIAN_POINT('Ctrl Pts',(-0.956786109256967,12.2,-11.3917584553421));
#300179=CARTESIAN_POINT('Ctrl Pts',(-0.955477199409448,12.2,-11.3952581757582));
#300180=CARTESIAN_POINT('Ctrl Pts',(-0.95416191474296,12.2,-11.3987626660218));
#300181=CARTESIAN_POINT('Ctrl Pts',(-0.952846630076473,12.2,-11.4022671562854));
#300182=CARTESIAN_POINT('Ctrl Pts',(-0.951524971795942,12.2,-11.4057764180618));
#300183=CARTESIAN_POINT('Ctrl Pts',(-0.950196927678083,12.2,-11.4092904138504));
#300184=CARTESIAN_POINT('Ctrl Pts',(-0.948426202026765,12.2,-11.4139757419941));
#300185=CARTESIAN_POINT('Ctrl Pts',(-0.946644124846304,12.2,-11.4186694905582));
#300186=CARTESIAN_POINT('Ctrl Pts',(-0.944850667636712,12.2,-11.4233715650928));
#300187=CARTESIAN_POINT('Ctrl Pts',(-0.943505574851696,12.2,-11.4268981206734));
#300188=CARTESIAN_POINT('Ctrl Pts',(-0.942154079989061,12.2,-11.4304293588656));
#300189=CARTESIAN_POINT('Ctrl Pts',(-0.940796168282198,12.2,-11.4339652319615));
#300190=CARTESIAN_POINT('Ctrl Pts',(-0.939438256575334,12.2,-11.4375011050575));
#300191=CARTESIAN_POINT('Ctrl Pts',(-0.938073927574405,12.2,-11.4410416122428));
#300192=CARTESIAN_POINT('Ctrl Pts',(-0.936703170534677,12.2,-11.4445867182134));
#300193=CARTESIAN_POINT('Ctrl Pts',(-0.934418575385458,12.2,-11.4504952283791));
#300194=CARTESIAN_POINT('Ctrl Pts',(-0.932116123684424,12.2,-11.4564165140663));
#300195=CARTESIAN_POINT('Ctrl Pts',(-0.929795809339219,12.2,-11.4623505331326));
#300196=CARTESIAN_POINT('Origin',(-5.66257110645729E-14,15.4,-1.77635683940025E-14));
#300197=CARTESIAN_POINT('',(-3.28892417320473,12.2,-1.19707050039253));
#300198=CARTESIAN_POINT('',(-3.28892417320473,15.4,-1.19707050039253));
#300199=CARTESIAN_POINT('Origin',(-5.66257110645729E-14,12.2,-1.77635683940025E-14));
#300200=CARTESIAN_POINT('Origin',(2.60871324108541E-9,12.2,-1.77635683940025E-14));
#300201=CARTESIAN_POINT('Origin',(-5.66300478732629E-14,15.4,-1.77635683940025E-14));
#300202=CARTESIAN_POINT('',(1.49999999999995,17.9,-1.77635683940025E-14));
#300203=CARTESIAN_POINT('Origin',(-5.55198248486377E-14,17.9,-1.77635683940025E-14));
#300204=CARTESIAN_POINT('',(1.49999999999994,15.4,-1.79472654138746E-14));
#300205=CARTESIAN_POINT('',(1.49999999999994,15.4,-1.79472654138746E-14));
#300206=CARTESIAN_POINT('Origin',(-5.66300478732629E-14,15.4,-1.77635683940025E-14));
#300207=CARTESIAN_POINT('Origin',(-5.66300478732629E-14,15.4,-1.77635683940025E-14));
#300208=CARTESIAN_POINT('',(1.49999999999994,2.4,-1.91719121435528E-14));
#300209=CARTESIAN_POINT('Origin',(-6.24032076013137E-14,2.4,-1.93556091634249E-14));
#300210=CARTESIAN_POINT('',(1.49999999999994,-0.100000000000001,-1.11022302462516E-14));
#300211=CARTESIAN_POINT('',(1.49999999999994,15.4,-1.79472654138746E-14));
#300212=CARTESIAN_POINT('Origin',(-6.4401609045639E-14,-0.100000000000001,
-1.11022302462516E-14));
#300213=CARTESIAN_POINT('Origin',(-6.4401609045639E-14,-0.100000000000001,
-1.11022302462516E-14));
#300214=CARTESIAN_POINT('Origin',(-5.55198248486377E-14,17.9,-1.77635683940025E-14));
#300215=CARTESIAN_POINT('Origin',(-5.66300478732629E-14,12.2,-1.77635683940025E-14));
#300216=CARTESIAN_POINT('',(1.33499935591029,12.2,-3.76399246382145));
#300217=CARTESIAN_POINT('',(1.21174315076912,12.2,-3.41647530879655));
#300218=CARTESIAN_POINT('',(1.33499941799994,12.2,-3.76399244200002));
#300219=CARTESIAN_POINT('',(0.669813182999944,12.2,-3.56257986500002));
#300220=CARTESIAN_POINT('Origin',(-5.66300478732629E-14,12.2,-1.77635683940025E-14));
#300221=CARTESIAN_POINT('',(0.737948320677355,12.2,-3.92497529182648));
#300222=CARTESIAN_POINT('',(0.669813182999944,12.2,-3.56257986500002));
#300223=CARTESIAN_POINT('',(0.540411127999944,12.2,-4.71915837900001));
#300224=CARTESIAN_POINT('Ctrl Pts',(0.737948221040922,12.2,-3.92497531022196));
#300225=CARTESIAN_POINT('Ctrl Pts',(0.738035737340575,12.2,-3.92544932936902));
#300226=CARTESIAN_POINT('Ctrl Pts',(0.738181018754199,12.2,-3.92631728138919));
#300227=CARTESIAN_POINT('Ctrl Pts',(0.738670587243213,12.2,-3.92956818688039));
#300228=CARTESIAN_POINT('Ctrl Pts',(0.738954729183831,12.1999999999079,
-3.93174223113599));
#300229=CARTESIAN_POINT('Ctrl Pts',(0.740093274189603,12.1999999999079,
-3.94128424531577));
#300230=CARTESIAN_POINT('Ctrl Pts',(0.740740501657956,12.1999999999079,
-3.94930810735695));
#300231=CARTESIAN_POINT('Ctrl Pts',(0.742798149505974,12.1999999999079,
-3.98426650826332));
#300232=CARTESIAN_POINT('Ctrl Pts',(0.742372759528698,12.2,-4.01357561888738));
#300233=CARTESIAN_POINT('Ctrl Pts',(0.736437186727589,12.2,-4.119388050933));
#300234=CARTESIAN_POINT('Ctrl Pts',(0.721506350180841,12.2,-4.21805492592019));
#300235=CARTESIAN_POINT('Ctrl Pts',(0.653099662777896,12.2,-4.46559806981985));
#300236=CARTESIAN_POINT('Ctrl Pts',(0.601738439484085,12.2,-4.59476663244512));
#300237=CARTESIAN_POINT('Ctrl Pts',(0.540411128396557,12.2,-4.71915837919555));
#300238=CARTESIAN_POINT('',(0.204481245999943,12.2,-4.74559663400001));
#300239=CARTESIAN_POINT('Origin',(-5.66300478732629E-14,12.2,-1.77635683940025E-14));
#300240=CARTESIAN_POINT('',(-0.114861198664522,12.2,-3.99208010934835));
#300241=CARTESIAN_POINT('Ctrl Pts',(0.204481245999943,12.2,-4.74559663400001));
#300242=CARTESIAN_POINT('Ctrl Pts',(0.172553443581559,12.2,-4.7004103209369));
#300243=CARTESIAN_POINT('Ctrl Pts',(0.143344934273432,12.2,-4.65597464923193));
#300244=CARTESIAN_POINT('Ctrl Pts',(0.116780339324946,12.2,-4.61263536275873));
#300245=CARTESIAN_POINT('Ctrl Pts',(0.089774485485458,12.2,-4.56857617652711));
#300246=CARTESIAN_POINT('Ctrl Pts',(0.0655014911131988,12.2,-4.52565083217712));
#300247=CARTESIAN_POINT('Ctrl Pts',(0.0438412949943011,12.2,-4.48424707603364));
#300248=CARTESIAN_POINT('Ctrl Pts',(0.0230828477657351,12.2,-4.44456702501974));
#300249=CARTESIAN_POINT('Ctrl Pts',(0.00472433924867187,12.2000000000001,
-4.40628451809031));
#300250=CARTESIAN_POINT('Ctrl Pts',(-0.0113809795912018,12.2,-4.36976156125905));
#300251=CARTESIAN_POINT('Ctrl Pts',(-0.0270142158296342,12.1999999999999,
-4.33430917326561));
#300252=CARTESIAN_POINT('Ctrl Pts',(-0.0405241706954382,12.2,-4.30051460941323));
#300253=CARTESIAN_POINT('Ctrl Pts',(-0.0520879448806814,12.2,-4.26872928236361));
#300254=CARTESIAN_POINT('Ctrl Pts',(-0.06314037611749,12.2,-4.23834948283383));
#300255=CARTESIAN_POINT('Ctrl Pts',(-0.0724147466109138,12.2,-4.20980510629708));
#300256=CARTESIAN_POINT('Ctrl Pts',(-0.0801088059519884,12.2,-4.18342243520099));
#300257=CARTESIAN_POINT('Ctrl Pts',(-0.0874725000263822,12.2,-4.15817257550991));
#300258=CARTESIAN_POINT('Ctrl Pts',(-0.0933884292815516,12.1999999999999,
-4.13490270492306));
#300259=CARTESIAN_POINT('Ctrl Pts',(-0.0980736177886704,12.2,-4.11391792531568));
#300260=CARTESIAN_POINT('Ctrl Pts',(-0.102420051223164,12.2000000000001,
-4.09445041668451));
#300261=CARTESIAN_POINT('Ctrl Pts',(-0.105707231633019,12.2,-4.07694951907395));
#300262=CARTESIAN_POINT('Ctrl Pts',(-0.108148552352073,12.2,-4.06167605561997));
#300263=CARTESIAN_POINT('Ctrl Pts',(-0.110505994223923,12.2,-4.04692735751014));
#300264=CARTESIAN_POINT('Ctrl Pts',(-0.112074334131715,12.1999999999999,
-4.03425550678305));
#300265=CARTESIAN_POINT('Ctrl Pts',(-0.113087970038994,12.2,-4.02391341293629));
#300266=CARTESIAN_POINT('Ctrl Pts',(-0.114055851981257,12.2000000000001,
-4.01403814529079));
#300267=CARTESIAN_POINT('Ctrl Pts',(-0.114517612985473,12.2,-4.00628689124919));
#300268=CARTESIAN_POINT('Ctrl Pts',(-0.114721610728504,12.2,-4.0008988960201));
#300269=CARTESIAN_POINT('Ctrl Pts',(-0.11482360960002,12.2,-3.99820489840556));
#300270=CARTESIAN_POINT('Ctrl Pts',(-0.114861911538468,12.2,-3.99610203167409));
#300271=CARTESIAN_POINT('Ctrl Pts',(-0.114872546484935,12.2,-3.99462238128286));
#300272=CARTESIAN_POINT('Ctrl Pts',(-0.114877863958168,12.2,-3.99388255608725));
#300273=CARTESIAN_POINT('Ctrl Pts',(-0.11487632054625,12.2,-3.99329856060513));
#300274=CARTESIAN_POINT('Ctrl Pts',(-0.11487279171893,12.2,-3.99287456748994));
#300275=CARTESIAN_POINT('Ctrl Pts',(-0.114871027305269,12.2,-3.99266257093235));
#300276=CARTESIAN_POINT('Ctrl Pts',(-0.114868725248524,12.2,-3.99249054033208));
#300277=CARTESIAN_POINT('Ctrl Pts',(-0.114866622243977,12.2,-3.99235909393692));
#300278=CARTESIAN_POINT('Ctrl Pts',(-0.114865070454561,12.2,-3.99226210074452));
#300279=CARTESIAN_POINT('Ctrl Pts',(-0.114863611222235,12.2,-3.99218545762677));
#300280=CARTESIAN_POINT('Ctrl Pts',(-0.114862439806823,12.2,-3.99213426766888));
#300281=CARTESIAN_POINT('Ctrl Pts',(-0.114862023705324,12.2,-3.99211608435154));
#300282=CARTESIAN_POINT('Ctrl Pts',(-0.1148616317576,12.2,-3.99210051805137));
#300283=CARTESIAN_POINT('Ctrl Pts',(-0.11486123084618,12.2,-3.99208443600385));
#300284=CARTESIAN_POINT('',(-0.104256396000055,12.2,-3.62350046200001));
#300285=CARTESIAN_POINT('',(-0.114861017000055,12.2,-3.99207578600001));
#300286=CARTESIAN_POINT('',(-0.662370095000057,12.2,-3.56397122000002));
#300287=CARTESIAN_POINT('Origin',(-5.66300478732629E-14,12.2,-1.77635683940025E-14));
#300288=CARTESIAN_POINT('',(-0.729748298404982,12.2,-3.92650814146157));
#300289=CARTESIAN_POINT('',(-0.662370095000057,12.2,-3.56397122000002));
#300290=CARTESIAN_POINT('',(-1.20083826600006,12.2,-4.59570315100001));
#300291=CARTESIAN_POINT('Ctrl Pts',(-0.729748397137909,12.2,-3.92650812272649));
#300292=CARTESIAN_POINT('Ctrl Pts',(-0.729798979329332,12.2,-3.92677468824178));
#300293=CARTESIAN_POINT('Ctrl Pts',(-0.729853590824242,12.1999999999997,
-3.92704048095005));
#300294=CARTESIAN_POINT('Ctrl Pts',(-0.730025582708951,12.1999999999997,
-3.92786938784101));
#300295=CARTESIAN_POINT('Ctrl Pts',(-0.730155150278449,12.2,-3.92846502942454));
#300296=CARTESIAN_POINT('Ctrl Pts',(-0.730733246668206,12.2,-3.93104867134671));
#300297=CARTESIAN_POINT('Ctrl Pts',(-0.731253196319109,12.1999999999077,
-3.93317718551181));
#300298=CARTESIAN_POINT('Ctrl Pts',(-0.733639815031661,12.1999999999077,
-3.94249120885481));
#300299=CARTESIAN_POINT('Ctrl Pts',(-0.735934859520536,12.1999999999077,
-3.95020698257531));
#300300=CARTESIAN_POINT('Ctrl Pts',(-0.746644516032087,12.1999999999077,
-3.98354780293642));
#300301=CARTESIAN_POINT('Ctrl Pts',(-0.757632863640905,12.2,-4.01073278352797));
#300302=CARTESIAN_POINT('Ctrl Pts',(-0.801179313012322,12.2,-4.10678792979713));
#300303=CARTESIAN_POINT('Ctrl Pts',(-0.850601354606886,12.2,-4.19338450992101));
#300304=CARTESIAN_POINT('Ctrl Pts',(-1.00417815028429,12.2,-4.39999394708107));
#300305=CARTESIAN_POINT('Ctrl Pts',(-1.09878737824146,12.2,-4.50193041233648));
#300306=CARTESIAN_POINT('Ctrl Pts',(-1.20083826600006,12.2,-4.59570315100001));
#300307=CARTESIAN_POINT('',(-1.5236341523253,12.2,-4.49900421997614));
#300308=CARTESIAN_POINT('Origin',(-5.66300478732629E-14,12.2,-1.77635683940025E-14));
#300309=CARTESIAN_POINT('',(-1.54921060157246,12.2,-3.68101131236159));
#300310=CARTESIAN_POINT('Ctrl Pts',(-1.52363415300006,12.2,-4.49900422000002));
#300311=CARTESIAN_POINT('Ctrl Pts',(-1.53068793708627,12.2,-4.47085469189399));
#300312=CARTESIAN_POINT('Ctrl Pts',(-1.53711977389706,12.2,-4.4431686191827));
#300313=CARTESIAN_POINT('Ctrl Pts',(-1.54295573603177,12.2,-4.41598726777904));
#300314=CARTESIAN_POINT('Ctrl Pts',(-1.55441407633895,12.2,-4.36261934536915));
#300315=CARTESIAN_POINT('Ctrl Pts',(-1.56357351051339,12.2,-4.3111985843265));
#300316=CARTESIAN_POINT('Ctrl Pts',(-1.57067315083765,12.2,-4.26205308021928));
#300317=CARTESIAN_POINT('Ctrl Pts',(-1.57747688850023,12.2,-4.21495588909847));
#300318=CARTESIAN_POINT('Ctrl Pts',(-1.58238883909617,12.1999999999999,
-4.16994832068129));
#300319=CARTESIAN_POINT('Ctrl Pts',(-1.58566442677365,12.2,-4.127324038995));
#300320=CARTESIAN_POINT('Ctrl Pts',(-1.58883259252429,12.2,-4.0860976079907));
#300321=CARTESIAN_POINT('Ctrl Pts',(-1.59046974502133,12.2,-4.04710078678771));
#300322=CARTESIAN_POINT('Ctrl Pts',(-1.59085264474885,12.2,-4.01060305274178));
#300323=CARTESIAN_POINT('Ctrl Pts',(-1.59122369863281,12.2,-3.97523445621444));
#300324=CARTESIAN_POINT('Ctrl Pts',(-1.59041660073962,12.2,-3.94221277590855));
#300325=CARTESIAN_POINT('Ctrl Pts',(-1.58873062606297,12.2,-3.911786232773));
#300326=CARTESIAN_POINT('Ctrl Pts',(-1.58714775742718,12.2,-3.88322042956623));
#300327=CARTESIAN_POINT('Ctrl Pts',(-1.58479013109599,12.2,-3.85694208153543));
#300328=CARTESIAN_POINT('Ctrl Pts',(-1.58195002843682,12.2,-3.83315875411321));
#300329=CARTESIAN_POINT('Ctrl Pts',(-1.57910981659426,12.2,-3.80937451237743));
#300330=CARTESIAN_POINT('Ctrl Pts',(-1.57578641439816,12.1999999999999,
-3.7880854732337));
#300331=CARTESIAN_POINT('Ctrl Pts',(-1.5723245407617,12.2,-3.7695012212912));
#300332=CARTESIAN_POINT('Ctrl Pts',(-1.56921114460368,12.2000000000001,
-3.75278768848402));
#300333=CARTESIAN_POINT('Ctrl Pts',(-1.56598590621646,12.2,-3.73826182817511));
#300334=CARTESIAN_POINT('Ctrl Pts',(-1.56294413362489,12.2,-3.72607762949063));
#300335=CARTESIAN_POINT('Ctrl Pts',(-1.56002764522756,12.2,-3.71439527223861));
#300336=CARTESIAN_POINT('Ctrl Pts',(-1.55727941358539,12.2,-3.70486562365225));
#300337=CARTESIAN_POINT('Ctrl Pts',(-1.5550051743708,12.2,-3.69762600726247));
#300338=CARTESIAN_POINT('Ctrl Pts',(-1.55337212957192,12.2,-3.69242751371117));
#300339=CARTESIAN_POINT('Ctrl Pts',(-1.55198432092636,12.2,-3.6884098225594));
#300340=CARTESIAN_POINT('Ctrl Pts',(-1.55097251090944,12.2,-3.68562445599079));
#300341=CARTESIAN_POINT('Ctrl Pts',(-1.55046660590099,12.2,-3.68423177270649));
#300342=CARTESIAN_POINT('Ctrl Pts',(-1.55005495419322,12.2,-3.68314718213396));
#300343=CARTESIAN_POINT('Ctrl Pts',(-1.54975552508367,12.2,-3.68237719584491));
#300344=CARTESIAN_POINT('Ctrl Pts',(-1.5496058105289,12.2,-3.68199220270039));
#300345=CARTESIAN_POINT('Ctrl Pts',(-1.54948420123509,12.2,-3.68168586978067));
#300346=CARTESIAN_POINT('Ctrl Pts',(-1.54939298287873,12.2,-3.68145899258006));
#300347=CARTESIAN_POINT('Ctrl Pts',(-1.54933878915026,12.2,-3.68132420258933));
#300348=CARTESIAN_POINT('Ctrl Pts',(-1.54929551285811,12.2,-3.68121780149236));
#300349=CARTESIAN_POINT('Ctrl Pts',(-1.54926322330182,12.2,-3.68113891519218));
#300350=CARTESIAN_POINT('Ctrl Pts',(-1.54924619322756,12.2,-3.68109730918379));
#300351=CARTESIAN_POINT('Ctrl Pts',(-1.54923273601866,12.2,-3.68106468916976));
#300352=CARTESIAN_POINT('Ctrl Pts',(-1.54922180885574,12.2,-3.68103843225446));
#300353=CARTESIAN_POINT('Ctrl Pts',(-1.54921858151565,12.2,-3.68103067726846));
#300354=CARTESIAN_POINT('Ctrl Pts',(-1.54921541865686,12.2,-3.68102308221307));
#300355=CARTESIAN_POINT('Ctrl Pts',(-1.54921224493634,12.2,-3.68101546102655));
#300356=CARTESIAN_POINT('',(-1.40617553966606,12.2,-3.34115179986312));
#300357=CARTESIAN_POINT('',(-1.54920881800006,12.2,-3.68100722300001));
#300358=CARTESIAN_POINT('',(-1.90509662000005,12.2,-3.08402851200002));
#300359=CARTESIAN_POINT('Origin',(-5.66300478732629E-14,12.2,-1.77635683940025E-14));
#300360=CARTESIAN_POINT('',(-2.0988883662473,12.2,-3.39774430965258));
#300361=CARTESIAN_POINT('',(-1.90509662000005,12.2,-3.08402851200002));
#300362=CARTESIAN_POINT('',(-2.77990780000006,12.2,-3.85157274700001));
#300363=CARTESIAN_POINT('Ctrl Pts',(-2.09888845211281,12.2,-3.39774425618107));
#300364=CARTESIAN_POINT('Ctrl Pts',(-2.09903187832741,12.2,-3.39797457253771));
#300365=CARTESIAN_POINT('Ctrl Pts',(-2.09917885578644,12.1999999999997,
-3.39820266771551));
#300366=CARTESIAN_POINT('Ctrl Pts',(-2.09963895812251,12.1999999999997,
-3.39891392611081));
#300367=CARTESIAN_POINT('Ctrl Pts',(-2.09997452956103,12.2,-3.39942189887948));
#300368=CARTESIAN_POINT('Ctrl Pts',(-2.1014481628405,12.2,-3.40162410246599));
#300369=CARTESIAN_POINT('Ctrl Pts',(-2.10270249498751,12.1999999999079,
-3.40342177907669));
#300370=CARTESIAN_POINT('Ctrl Pts',(-2.10829027509302,12.1999999999079,
-3.41124149475554));
#300371=CARTESIAN_POINT('Ctrl Pts',(-2.11321950204324,12.1999999999079,
-3.41760963109163));
#300372=CARTESIAN_POINT('Ctrl Pts',(-2.13524297057016,12.1999999999079,
-3.44482145366327));
#300373=CARTESIAN_POINT('Ctrl Pts',(-2.15530017599741,12.2,-3.46619350428762));
#300374=CARTESIAN_POINT('Ctrl Pts',(-2.23100372376674,12.2,-3.54042209052579));
#300375=CARTESIAN_POINT('Ctrl Pts',(-2.30852269436843,12.2,-3.6032793024282));
#300376=CARTESIAN_POINT('Ctrl Pts',(-2.52588006333986,12.2,-3.74015282700682));
#300377=CARTESIAN_POINT('Ctrl Pts',(-2.65150240933442,12.2,-3.80124396329853));
#300378=CARTESIAN_POINT('Ctrl Pts',(-2.77990780000006,12.2,-3.85157274700001));
#300379=CARTESIAN_POINT('',(-3.04597431500006,12.2,-3.64479635500001));
#300380=CARTESIAN_POINT('Origin',(-5.66300478732629E-14,12.2,-1.77635683940025E-14));
#300381=CARTESIAN_POINT('',(-2.77433052545124,12.2,-2.87280140881169));
#300382=CARTESIAN_POINT('Ctrl Pts',(-3.04597431500006,12.2,-3.64479635500001));
#300383=CARTESIAN_POINT('Ctrl Pts',(-3.04202932086791,12.2,-3.61316355471933));
#300384=CARTESIAN_POINT('Ctrl Pts',(-3.03758633189924,12.2,-3.5823231881441));
#300385=CARTESIAN_POINT('Ctrl Pts',(-3.03269790848834,12.2,-3.55231409881095));
#300386=CARTESIAN_POINT('Ctrl Pts',(-3.02400453989956,12.2,-3.49894718423372));
#300387=CARTESIAN_POINT('Ctrl Pts',(-3.01390127476584,12.2,-3.44821094171571));
#300388=CARTESIAN_POINT('Ctrl Pts',(-3.0027266806269,12.2,-3.4003210931824));
#300389=CARTESIAN_POINT('Ctrl Pts',(-2.991920980653,12.2,-3.35401217774325));
#300390=CARTESIAN_POINT('Ctrl Pts',(-2.98011337707264,12.1999999999999,
-3.31036493482041));
#300391=CARTESIAN_POINT('Ctrl Pts',(-2.96765450987006,12.2,-3.26956247204393));
#300392=CARTESIAN_POINT('Ctrl Pts',(-2.95566474553295,12.2000000000001,
-3.2302963088279));
#300393=CARTESIAN_POINT('Ctrl Pts',(-2.94307169437058,12.2,-3.19366484089195));
#300394=CARTESIAN_POINT('Ctrl Pts',(-2.93023205633515,12.2,-3.15981818093772));
#300395=CARTESIAN_POINT('Ctrl Pts',(-2.91788975284348,12.2,-3.12728254806535));
#300396=CARTESIAN_POINT('Ctrl Pts',(-2.90531940526358,12.2,-3.09732026810663));
#300397=CARTESIAN_POINT('Ctrl Pts',(-2.89288201802745,12.2,-3.07005062301657));
#300398=CARTESIAN_POINT('Ctrl Pts',(-2.88095667512664,12.2,-3.04390366286261));
#300399=CARTESIAN_POINT('Ctrl Pts',(-2.869153369637,12.2,-3.02023230347142));
#300400=CARTESIAN_POINT('Ctrl Pts',(-2.85783471947781,12.2,-2.99912683090921));
#300401=CARTESIAN_POINT('Ctrl Pts',(-2.84681464370975,12.2,-2.97857809908297));
#300402=CARTESIAN_POINT('Ctrl Pts',(-2.83625357808533,12.2,-2.9604618568326));
#300403=CARTESIAN_POINT('Ctrl Pts',(-2.82653408044394,12.2,-2.94484495350539));
#300404=CARTESIAN_POINT('Ctrl Pts',(-2.81760443123926,12.2,-2.93049714732027));
#300405=CARTESIAN_POINT('Ctrl Pts',(-2.80938510198816,12.2,-2.91825898115459));
#300406=CARTESIAN_POINT('Ctrl Pts',(-2.80221596360782,12.2,-2.90816727129479));
#300407=CARTESIAN_POINT('Ctrl Pts',(-2.79537498136305,12.2,-2.89853749372491));
#300408=CARTESIAN_POINT('Ctrl Pts',(-2.78948989273483,12.2,-2.89086226716769));
#300409=CARTESIAN_POINT('Ctrl Pts',(-2.78489987364489,12.2,-2.88515831797985));
#300410=CARTESIAN_POINT('Ctrl Pts',(-2.78174647474832,12.2,-2.88123963556861));
#300411=CARTESIAN_POINT('Ctrl Pts',(-2.77920517936183,12.2,-2.87825107637023));
#300412=CARTESIAN_POINT('Ctrl Pts',(-2.77740054731802,12.2,-2.87619306749039));
#300413=CARTESIAN_POINT('Ctrl Pts',(-2.77649823129612,12.2,-2.87516406305046));
#300414=CARTESIAN_POINT('Ctrl Pts',(-2.77578028206434,12.2,-2.87436762379733));
#300415=CARTESIAN_POINT('Ctrl Pts',(-2.77526359373549,12.2,-2.87380336028058));
#300416=CARTESIAN_POINT('Ctrl Pts',(-2.77500524957107,12.2,-2.8735212285222));
#300417=CARTESIAN_POINT('Ctrl Pts',(-2.77479725418726,12.2,-2.87329713551082));
#300418=CARTESIAN_POINT('Ctrl Pts',(-2.77464175442408,12.2,-2.87313100117707));
#300419=CARTESIAN_POINT('Ctrl Pts',(-2.77454713595653,12.2,-2.87302991178797));
#300420=CARTESIAN_POINT('Ctrl Pts',(-2.77447240241418,12.2,-2.87295067082362));
#300421=CARTESIAN_POINT('Ctrl Pts',(-2.77441676535422,12.2,-2.87289196756005));
#300422=CARTESIAN_POINT('Ctrl Pts',(-2.77438698189278,12.2,-2.87286054270784));
#300423=CARTESIAN_POINT('Ctrl Pts',(-2.77436463441682,12.2,-2.87283711775074));
#300424=CARTESIAN_POINT('Ctrl Pts',(-2.77434525405922,12.2,-2.87281688981085));
#300425=CARTESIAN_POINT('Ctrl Pts',(-2.77434133962869,12.2,-2.87281280418626));
#300426=CARTESIAN_POINT('Ctrl Pts',(-2.77433745035311,12.2,-2.87280874625328));
#300427=CARTESIAN_POINT('Ctrl Pts',(-2.77433355875055,12.2,-2.87280468523913));
#300428=CARTESIAN_POINT('',(-2.51818288326644,12.2,-2.6075620736151));
#300429=CARTESIAN_POINT('',(-2.77432738300006,12.2,-2.87279823700001));
#300430=CARTESIAN_POINT('',(-2.89052929200006,12.2,-2.18757066500002));
#300431=CARTESIAN_POINT('Origin',(-5.66300478732629E-14,12.2,-1.77635683940025E-14));
#300432=CARTESIAN_POINT('',(-3.18456193007282,12.2,-2.41009628089888));
#300433=CARTESIAN_POINT('',(-2.89052929200006,12.2,-2.18757066500002));
#300434=CARTESIAN_POINT('',(-3.98353538000006,12.2,-2.58726610100001));
#300435=CARTESIAN_POINT('Ctrl Pts',(-3.18456199052765,12.2,-2.41009620039622));
#300436=CARTESIAN_POINT('Ctrl Pts',(-3.1847789483277,12.2,-2.41025912851954));
#300437=CARTESIAN_POINT('Ctrl Pts',(-3.18499837884731,12.1999999999997,
-2.41041875026477));
#300438=CARTESIAN_POINT('Ctrl Pts',(-3.18568371131526,12.1999999999997,
-2.41091530622894));
#300439=CARTESIAN_POINT('Ctrl Pts',(-3.18618024732525,12.2,-2.41126785644461));
#300440=CARTESIAN_POINT('Ctrl Pts',(-3.18834989044632,12.2,-2.41278901397985));
#300441=CARTESIAN_POINT('Ctrl Pts',(-3.19016802488907,12.1999999999079,
-2.41401161234104));
#300442=CARTESIAN_POINT('Ctrl Pts',(-3.19820687861432,12.1999999999079,
-2.41928710817222));
#300443=CARTESIAN_POINT('Ctrl Pts',(-3.20510075911968,12.1999999999079,
-2.42344270161732));
#300444=CARTESIAN_POINT('Ctrl Pts',(-3.23547872372625,12.1999999999079,
-2.44086791092227));
#300445=CARTESIAN_POINT('Ctrl Pts',(-3.26191056113451,12.2,-2.45355331330479));
#300446=CARTESIAN_POINT('Ctrl Pts',(-3.35901835635599,12.2,-2.49529406440199));
#300447=CARTESIAN_POINT('Ctrl Pts',(-3.45393334803369,12.2,-2.52595419545077));
#300448=CARTESIAN_POINT('Ctrl Pts',(-3.70638249798277,12.2,-2.57512980517529));
#300449=CARTESIAN_POINT('Ctrl Pts',(-3.84524313000394,12.2,-2.58671966873636));
#300450=CARTESIAN_POINT('Ctrl Pts',(-3.98353538000006,12.2,-2.58726610100001));
#300451=CARTESIAN_POINT('',(-4.15693876900006,12.2,-2.29833854600002));
#300452=CARTESIAN_POINT('Origin',(-5.66300478732629E-14,12.2,-1.77635683940025E-14));
#300453=CARTESIAN_POINT('',(-3.62476174783278,12.2,-1.676603759906));
#300454=CARTESIAN_POINT('Ctrl Pts',(-4.15693876900006,12.2,-2.29833854600002));
#300455=CARTESIAN_POINT('Ctrl Pts',(-4.14220958485318,12.2,-2.27096656816286));
#300456=CARTESIAN_POINT('Ctrl Pts',(-4.12731111776242,12.2,-2.24446827238719));
#300457=CARTESIAN_POINT('Ctrl Pts',(-4.11230167253419,12.2,-2.21885949074597));
#300458=CARTESIAN_POINT('Ctrl Pts',(-4.08477741829449,12.2,-2.17189822029633));
#300459=CARTESIAN_POINT('Ctrl Pts',(-4.05687943548038,12.2,-2.12793053560342));
#300460=CARTESIAN_POINT('Ctrl Pts',(-4.02900743847548,12.2,-2.08703684650124));
#300461=CARTESIAN_POINT('Ctrl Pts',(-4.00217614217277,12.2,-2.04767006955237));
#300462=CARTESIAN_POINT('Ctrl Pts',(-3.97536882407247,12.2,-2.01115220162154));
#300463=CARTESIAN_POINT('Ctrl Pts',(-3.94897945960632,12.2,-1.97752765018928));
#300464=CARTESIAN_POINT('Ctrl Pts',(-3.92350771750221,12.2,-1.94507230616052));
#300465=CARTESIAN_POINT('Ctrl Pts',(-3.89842521272531,12.2,-1.9153127559376));
#300466=CARTESIAN_POINT('Ctrl Pts',(-3.87412319315574,12.2,-1.88826042636132));
#300467=CARTESIAN_POINT('Ctrl Pts',(-3.85061722051365,12.2,-1.86209423399593));
#300468=CARTESIAN_POINT('Ctrl Pts',(-3.8278412423737,12.2,-1.83846102204754));
#300469=CARTESIAN_POINT('Ctrl Pts',(-3.80618677108186,12.2,-1.81734097964565));
#300470=CARTESIAN_POINT('Ctrl Pts',(-3.78529621739538,12.2,-1.79696600148473));
#300471=CARTESIAN_POINT('Ctrl Pts',(-3.76544921024321,12.2,-1.77893023451589));
#300472=CARTESIAN_POINT('Ctrl Pts',(-3.74703567838489,12.2,-1.76318404897607));
#300473=CARTESIAN_POINT('Ctrl Pts',(-3.72949948546344,12.2,-1.74818811286084));
#300474=CARTESIAN_POINT('Ctrl Pts',(-3.71326322431709,12.2,-1.73526896265244));
#300475=CARTESIAN_POINT('Ctrl Pts',(-3.69870203620881,12.2,-1.72435135611523));
#300476=CARTESIAN_POINT('Ctrl Pts',(-3.68525234134329,12.2,-1.71426711879234));
#300477=CARTESIAN_POINT('Ctrl Pts',(-3.67323171741993,12.2,-1.70589056673568));
#300478=CARTESIAN_POINT('Ctrl Pts',(-3.66297061081925,12.2,-1.69913275840808));
#300479=CARTESIAN_POINT('Ctrl Pts',(-3.6531381669103,12.2,-1.69265726079223));
#300480=CARTESIAN_POINT('Ctrl Pts',(-3.6449209883424,12.2,-1.68766836640196));
#300481=CARTESIAN_POINT('Ctrl Pts',(-3.63864585579863,12.2,-1.68405720735998));
#300482=CARTESIAN_POINT('Ctrl Pts',(-3.63442292860184,12.2,-1.68162703371441));
#300483=CARTESIAN_POINT('Ctrl Pts',(-3.63108021443716,12.2,-1.67982022145482));
#300484=CARTESIAN_POINT('Ctrl Pts',(-3.62872851541058,12.2,-1.6785941477588));
#300485=CARTESIAN_POINT('Ctrl Pts',(-3.62755266589729,12.2,-1.67798111091079));
#300486=CARTESIAN_POINT('Ctrl Pts',(-3.62662472212591,12.2,-1.67751313883082));
#300487=CARTESIAN_POINT('Ctrl Pts',(-3.62595954395709,12.2,-1.67718405449576));
#300488=CARTESIAN_POINT('Ctrl Pts',(-3.62562695487268,12.2,-1.67701951232824));
#300489=CARTESIAN_POINT('Ctrl Pts',(-3.62536007978653,12.2,-1.67688967842754));
#300490=CARTESIAN_POINT('Ctrl Pts',(-3.62516080538803,12.2,-1.67679374434236));
#300491=CARTESIAN_POINT('Ctrl Pts',(-3.62503846121203,12.2,-1.67673484577491));
#300492=CARTESIAN_POINT('Ctrl Pts',(-3.62494219413518,12.2,-1.67668893681862));
#300493=CARTESIAN_POINT('Ctrl Pts',(-3.62487062783168,12.2,-1.67665503599103));
#300494=CARTESIAN_POINT('Ctrl Pts',(-3.62483104884004,12.2,-1.67663628749479));
#300495=CARTESIAN_POINT('Ctrl Pts',(-3.62480232555704,12.2,-1.67662280367348));
#300496=CARTESIAN_POINT('Ctrl Pts',(-3.62477640670851,12.2,-1.67661069179204));
#300497=CARTESIAN_POINT('Ctrl Pts',(-3.62477285602412,12.2,-1.67660903255675));
#300498=CARTESIAN_POINT('Ctrl Pts',(-3.62476931425303,12.2,-1.6766073779349));
#300499=CARTESIAN_POINT('Ctrl Pts',(-3.62476577205416,12.2,-1.67660572288421));
#300500=CARTESIAN_POINT('',(-3.29009567465824,12.2,-1.52180664071691));
#300501=CARTESIAN_POINT('',(-3.62475766100006,12.2,-1.67660193100001));
#300502=CARTESIAN_POINT('',(-3.48557996500006,12.2,-0.995669277000015));
#300503=CARTESIAN_POINT('Origin',(-5.66300478732629E-14,12.2,-1.77635683940025E-14));
#300504=CARTESIAN_POINT('',(-3.84014275842517,12.2,-1.0969513940623));
#300505=CARTESIAN_POINT('',(-3.48557996500006,12.2,-0.995669277000015));
#300506=CARTESIAN_POINT('',(-4.64916443400006,12.2,-0.973534832000014));
#300507=CARTESIAN_POINT('Ctrl Pts',(-3.84014278600006,12.2,-1.09695129700001));
#300508=CARTESIAN_POINT('Ctrl Pts',(-3.84030898991399,12.2,-1.09699816032842));
#300509=CARTESIAN_POINT('Ctrl Pts',(-3.84140226785887,12.2,-1.0972932841756));
#300510=CARTESIAN_POINT('Ctrl Pts',(-3.84464780527484,12.2,-1.0980939631551));
#300511=CARTESIAN_POINT('Ctrl Pts',(-3.84678446778506,12.199999999908,-1.0985771363248));
#300512=CARTESIAN_POINT('Ctrl Pts',(-3.85618709028379,12.199999999908,-1.10059260222741));
#300513=CARTESIAN_POINT('Ctrl Pts',(-3.86411569097725,12.199999999908,-1.10197705056623));
#300514=CARTESIAN_POINT('Ctrl Pts',(-3.89873881818786,12.199999999908,-1.10725203377565));
#300515=CARTESIAN_POINT('Ctrl Pts',(-3.92796253029191,12.2,-1.10953219114214));
#300516=CARTESIAN_POINT('Ctrl Pts',(-4.0336650704685,12.2,-1.11337750310591));
#300517=CARTESIAN_POINT('Ctrl Pts',(-4.13324208872044,12.2,-1.10766588628757));
#300518=CARTESIAN_POINT('Ctrl Pts',(-4.38630470364963,12.2,-1.06234400779285));
#300519=CARTESIAN_POINT('Ctrl Pts',(-4.51963188083663,12.2,-1.02312808333993));
#300520=CARTESIAN_POINT('Ctrl Pts',(-4.64916443400006,12.2,-0.973534832000014));
#300521=CARTESIAN_POINT('',(-4.70648560700006,12.2,-0.641477381000013));
#300522=CARTESIAN_POINT('Origin',(-5.66300478732629E-14,12.2,-1.77635683940025E-14));
#300523=CARTESIAN_POINT('',(-3.98564879651336,12.2,-0.253971471173062));
#300524=CARTESIAN_POINT('Ctrl Pts',(-4.70648560700006,12.2,-0.641477381000013));
#300525=CARTESIAN_POINT('Ctrl Pts',(-4.67739030276498,12.2,-0.616593939557199));
#300526=CARTESIAN_POINT('Ctrl Pts',(-4.64853374448598,12.2,-0.593039396638165));
#300527=CARTESIAN_POINT('Ctrl Pts',(-4.62002995111684,12.2,-0.570801237698567));
#300528=CARTESIAN_POINT('Ctrl Pts',(-4.57760782927771,12.2,-0.537704243351314));
#300529=CARTESIAN_POINT('Ctrl Pts',(-4.53596732202362,12.2,-0.50752499617894));
#300530=CARTESIAN_POINT('Ctrl Pts',(-4.49551314177239,12.2,-0.480188970837284));
#300531=CARTESIAN_POINT('Ctrl Pts',(-4.45659866038684,12.2,-0.453893363246007));
#300532=CARTESIAN_POINT('Ctrl Pts',(-4.4187819253462,12.2,-0.430228847080283));
#300533=CARTESIAN_POINT('Ctrl Pts',(-4.38244840783252,12.2,-0.409089430305889));
#300534=CARTESIAN_POINT('Ctrl Pts',(-4.34725263625644,12.2,-0.388611972163751));
#300535=CARTESIAN_POINT('Ctrl Pts',(-4.31344857123307,12.2,-0.370504213207233));
#300536=CARTESIAN_POINT('Ctrl Pts',(-4.28141134962896,12.2,-0.354628570095604));
#300537=CARTESIAN_POINT('Ctrl Pts',(-4.2509814919226,12.2,-0.339549435991728));
#300538=CARTESIAN_POINT('Ctrl Pts',(-4.22214561332269,12.2,-0.326484236774195));
#300539=CARTESIAN_POINT('Ctrl Pts',(-4.19524842022594,12.2,-0.31527462050277));
#300540=CARTESIAN_POINT('Ctrl Pts',(-4.16917658132024,12.2,-0.304408977066588));
#300541=CARTESIAN_POINT('Ctrl Pts',(-4.14492611508931,12.2,-0.295287111378102));
#300542=CARTESIAN_POINT('Ctrl Pts',(-4.12283468744088,12.2,-0.287722175954538));
#300543=CARTESIAN_POINT('Ctrl Pts',(-4.10223155113375,12.2,-0.280666887443235));
#300544=CARTESIAN_POINT('Ctrl Pts',(-4.08350632160541,12.2,-0.274965900155463));
#300545=CARTESIAN_POINT('Ctrl Pts',(-4.06695477888446,12.2,-0.27042749044276));
#300546=CARTESIAN_POINT('Ctrl Pts',(-4.05123986161395,12.2,-0.26611848225076));
#300547=CARTESIAN_POINT('Ctrl Pts',(-4.03748433107584,12.2,-0.262857737210549));
#300548=CARTESIAN_POINT('Ctrl Pts',(-4.02596291487887,12.2,-0.260441305594084));
#300549=CARTESIAN_POINT('Ctrl Pts',(-4.01484311445685,12.2,-0.25810910642263));
#300550=CARTESIAN_POINT('Ctrl Pts',(-4.00580415854497,12.2,-0.256563801725764));
#300551=CARTESIAN_POINT('Ctrl Pts',(-3.9991163289497,12.2,-0.255579178475452));
#300552=CARTESIAN_POINT('Ctrl Pts',(-3.99497751304969,12.2,-0.254969836639529));
#300553=CARTESIAN_POINT('Ctrl Pts',(-3.99173960011373,12.2,-0.254574381557754));
#300554=CARTESIAN_POINT('Ctrl Pts',(-3.98947213811192,12.2,-0.25432920431917));
#300555=CARTESIAN_POINT('Ctrl Pts',(-3.98833840711101,12.2,-0.254206615699878));
#300556=CARTESIAN_POINT('Ctrl Pts',(-3.98744734802868,12.2,-0.254121478293377));
#300557=CARTESIAN_POINT('Ctrl Pts',(-3.98680815864947,12.2,-0.254064967079465));
#300558=CARTESIAN_POINT('Ctrl Pts',(-3.98648856395987,12.2,-0.254036711472509));
#300559=CARTESIAN_POINT('Ctrl Pts',(-3.9862319212959,12.2,-0.254015618895323));
#300560=CARTESIAN_POINT('Ctrl Pts',(-3.98603942619645,12.2,-0.254000520323441));
#300561=CARTESIAN_POINT('Ctrl Pts',(-3.98591562691842,12.2,-0.253990809986381));
#300562=CARTESIAN_POINT('Ctrl Pts',(-3.98581889125066,12.2,-0.253983577985231));
#300563=CARTESIAN_POINT('Ctrl Pts',(-3.98574755264139,12.2,-0.25397838826675));
#300564=CARTESIAN_POINT('Ctrl Pts',(-3.98570796707643,12.2,-0.253975508508647));
#300565=CARTESIAN_POINT('Ctrl Pts',(-3.98568085248347,12.2,-0.253973712859757));
#300566=CARTESIAN_POINT('Ctrl Pts',(-3.98565325097426,12.2,-0.2539718483819));
#300567=CARTESIAN_POINT('',(-3.61766281507283,12.2,-0.230522786376999));
#300568=CARTESIAN_POINT('',(-3.98564433200006,12.2,-0.253971243000013));
#300569=CARTESIAN_POINT('',(-3.60988374900006,12.2,0.330702762999984));
#300570=CARTESIAN_POINT('Origin',(-5.66300478732629E-14,12.2,-1.77635683940025E-14));
#300571=CARTESIAN_POINT('',(-3.9770910289505,12.2,0.364342856252411));
#300572=CARTESIAN_POINT('',(-3.60988374900006,12.2,0.330702762999984));
#300573=CARTESIAN_POINT('',(-4.68689806900006,12.2,0.771677711999987));
#300574=CARTESIAN_POINT('Ctrl Pts',(-3.97709101934974,12.2,0.364342957033298));
#300575=CARTESIAN_POINT('Ctrl Pts',(-3.97736112094161,12.2,0.364368687912379));
#300576=CARTESIAN_POINT('Ctrl Pts',(-3.97763081754438,12.1999999999997,
0.364398582405285));
#300577=CARTESIAN_POINT('Ctrl Pts',(-3.97847249976144,12.1999999999997,
0.364493406994217));
#300578=CARTESIAN_POINT('Ctrl Pts',(-3.97907662749092,12.2,0.364567350873792));
#300579=CARTESIAN_POINT('Ctrl Pts',(-3.98170542410654,12.2,0.364904961265897));
#300580=CARTESIAN_POINT('Ctrl Pts',(-3.98387379409812,12.199999999908,0.365226521130628));
#300581=CARTESIAN_POINT('Ctrl Pts',(-3.99336397358853,12.199999999908,0.366742885520348));
#300582=CARTESIAN_POINT('Ctrl Pts',(-4.0012579760989,12.199999999908,0.368316009283327));
#300583=CARTESIAN_POINT('Ctrl Pts',(-4.03544701617339,12.199999999908,0.375904201720463));
#300584=CARTESIAN_POINT('Ctrl Pts',(-4.06352360252377,12.2,0.384335203288191));
#300585=CARTESIAN_POINT('Ctrl Pts',(-4.16348965587543,12.2,0.418937988494843));
#300586=CARTESIAN_POINT('Ctrl Pts',(-4.25429273351133,12.2,0.460246281843015));
#300587=CARTESIAN_POINT('Ctrl Pts',(-4.47387858189227,12.2,0.593914841213743));
#300588=CARTESIAN_POINT('Ctrl Pts',(-4.5841592272997,12.2,0.67875964775583));
#300589=CARTESIAN_POINT('Ctrl Pts',(-4.68689806900006,12.2,0.771677711999987));
#300590=CARTESIAN_POINT('',(-4.62039548500006,12.2,1.10201885899999));
#300591=CARTESIAN_POINT('Origin',(-5.66300478732629E-14,12.2,-1.77635683940025E-14));
#300592=CARTESIAN_POINT('',(-3.80824764648564,12.2,1.20295971278735));
#300593=CARTESIAN_POINT('Ctrl Pts',(-4.62039548500006,12.2,1.10201885899999));
#300594=CARTESIAN_POINT('Ctrl Pts',(-4.49008798165083,12.2,1.14780973418869));
#300595=CARTESIAN_POINT('Ctrl Pts',(-4.35566622701388,12.2,1.18338092348667));
#300596=CARTESIAN_POINT('Ctrl Pts',(-4.10115788280569,12.2,1.22181532284944));
#300597=CARTESIAN_POINT('Ctrl Pts',(-4.00118301828606,12.2,1.22475245377806));
#300598=CARTESIAN_POINT('Ctrl Pts',(-3.89557234472372,12.2,1.21796341587231));
#300599=CARTESIAN_POINT('Ctrl Pts',(-3.86637307317564,12.2000000000748,
1.21486437588036));
#300600=CARTESIAN_POINT('Ctrl Pts',(-3.83190572787353,12.2000000000748,
1.20861681729509));
#300601=CARTESIAN_POINT('Ctrl Pts',(-3.82403373441455,12.2000000000748,
1.20701284847675));
#300602=CARTESIAN_POINT('Ctrl Pts',(-3.81473210800609,12.2000000000748,
1.20474214283786));
#300603=CARTESIAN_POINT('Ctrl Pts',(-3.81262693390849,12.2,1.2042031454596));
#300604=CARTESIAN_POINT('Ctrl Pts',(-3.81010330907745,12.2,1.20350407609351));
#300605=CARTESIAN_POINT('Ctrl Pts',(-3.80952866324519,12.2000000000005,
1.2033412192238));
#300606=CARTESIAN_POINT('Ctrl Pts',(-3.80885139391262,12.2000000000005,
1.20314218456492));
#300607=CARTESIAN_POINT('Ctrl Pts',(-3.80853382233514,12.2,1.20304885187476));
#300608=CARTESIAN_POINT('Ctrl Pts',(-3.80828031400006,12.2,1.20296984599999));
#300609=CARTESIAN_POINT('',(-3.45664454600006,12.2,1.09189444699998));
#300610=CARTESIAN_POINT('',(-3.80824765200006,12.2,1.20295966899999));
#300611=CARTESIAN_POINT('',(-3.24665273100006,12.2,1.61241156299999));
#300612=CARTESIAN_POINT('Origin',(-5.66300478732629E-14,12.2,-1.77635683940025E-14));
#300613=CARTESIAN_POINT('',(-3.57691111715103,12.2,1.7764305847426));
#300614=CARTESIAN_POINT('',(-3.24665273100006,12.2,1.61241156299999));
#300615=CARTESIAN_POINT('',(-4.09164014900006,12.2,2.41267090399998));
#300616=CARTESIAN_POINT('Ctrl Pts',(-3.57691107200006,12.2,1.77643067499998));
#300617=CARTESIAN_POINT('Ctrl Pts',(-3.57715363087875,12.2,1.77655225603397));
#300618=CARTESIAN_POINT('Ctrl Pts',(-3.57739432442841,12.1999999999997,
1.7766775413267));
#300619=CARTESIAN_POINT('Ctrl Pts',(-3.57814397713914,12.1999999999997,
1.77706952294413));
#300620=CARTESIAN_POINT('Ctrl Pts',(-3.57868088758371,12.2,1.77735684826631));
#300621=CARTESIAN_POINT('Ctrl Pts',(-3.58100948595218,12.2,1.77862090122509));
#300622=CARTESIAN_POINT('Ctrl Pts',(-3.58291519327722,12.1999999999079,
1.77970395294905));
#300623=CARTESIAN_POINT('Ctrl Pts',(-3.5912174593958,12.1999999999079,1.78454657405624));
#300624=CARTESIAN_POINT('Ctrl Pts',(-3.5980079172033,12.1999999999079,1.78886359039074));
#300625=CARTESIAN_POINT('Ctrl Pts',(-3.62715509725334,12.1999999999079,
1.80829521478595));
#300626=CARTESIAN_POINT('Ctrl Pts',(-3.65029150305341,12.2,1.82630146689454));
#300627=CARTESIAN_POINT('Ctrl Pts',(-3.73111669954928,12.2,1.89477220755472));
#300628=CARTESIAN_POINT('Ctrl Pts',(-3.8008635540934,12.2,1.96614323281364));
#300629=CARTESIAN_POINT('Ctrl Pts',(-3.95725251061657,12.2,2.17000168930957));
#300630=CARTESIAN_POINT('Ctrl Pts',(-4.02964978479197,12.2,2.28940052844448));
#300631=CARTESIAN_POINT('Ctrl Pts',(-4.09164014979821,12.2,2.41267090359861));
#300632=CARTESIAN_POINT('',(-3.91029535000006,12.2,2.69668134599998));
#300633=CARTESIAN_POINT('Origin',(-5.66300478732629E-14,12.2,-1.77635683940025E-14));
#300634=CARTESIAN_POINT('',(-3.11652947055878,12.2,2.49742704586989));
#300635=CARTESIAN_POINT('Ctrl Pts',(-3.91029535000006,12.2,2.69668134599998));
#300636=CARTESIAN_POINT('Ctrl Pts',(-3.87704667375992,12.2,2.69562795448002));
#300637=CARTESIAN_POINT('Ctrl Pts',(-3.844607186862,12.2,2.69395488001898));
#300638=CARTESIAN_POINT('Ctrl Pts',(-3.81302641540527,12.2,2.69171777261672));
#300639=CARTESIAN_POINT('Ctrl Pts',(-3.75925183787251,12.2,2.68790850831115));
#300640=CARTESIAN_POINT('Ctrl Pts',(-3.70796856982792,12.2,2.68246255129163));
#300641=CARTESIAN_POINT('Ctrl Pts',(-3.65942186526007,12.2,2.67569751949168));
#300642=CARTESIAN_POINT('Ctrl Pts',(-3.61272377880615,12.2,2.66919009447346));
#300643=CARTESIAN_POINT('Ctrl Pts',(-3.56855790143124,12.2,2.66146197193717));
#300644=CARTESIAN_POINT('Ctrl Pts',(-3.52713481762616,12.2,2.65284046259447));
#300645=CARTESIAN_POINT('Ctrl Pts',(-3.48684973136383,12.2,2.644455808057));
#300646=CARTESIAN_POINT('Ctrl Pts',(-3.44915895619017,12.2,2.63522588786816));
#300647=CARTESIAN_POINT('Ctrl Pts',(-3.41424704813716,12.2,2.62549768671105));
#300648=CARTESIAN_POINT('Ctrl Pts',(-3.38050173090573,12.2,2.6160945560188));
#300649=CARTESIAN_POINT('Ctrl Pts',(-3.34935281231531,12.2,2.60622559506111));
#300650=CARTESIAN_POINT('Ctrl Pts',(-3.32095662401592,12.2,2.59625133524797));
#300651=CARTESIAN_POINT('Ctrl Pts',(-3.29395175854877,12.2,2.58676578241432));
#300652=CARTESIAN_POINT('Ctrl Pts',(-3.26943656002086,12.2,2.57718480265262));
#300653=CARTESIAN_POINT('Ctrl Pts',(-3.24753462597801,12.2,2.56786486200729));
#300654=CARTESIAN_POINT('Ctrl Pts',(-3.22645411420113,12.2,2.5588944615783));
#300655=CARTESIAN_POINT('Ctrl Pts',(-3.20779462551826,12.2,2.5501655301266));
#300656=CARTESIAN_POINT('Ctrl Pts',(-3.19165465935819,12.2,2.54204381384399));
#300657=CARTESIAN_POINT('Ctrl Pts',(-3.176799307833,12.2,2.53456852243573));
#300658=CARTESIAN_POINT('Ctrl Pts',(-3.16407839268306,12.2,2.52760760821054));
#300659=CARTESIAN_POINT('Ctrl Pts',(-3.15355800067279,12.2,2.52148949437163));
#300660=CARTESIAN_POINT('Ctrl Pts',(-3.14350736635935,12.2,2.51564456722226));
#300661=CARTESIAN_POINT('Ctrl Pts',(-3.13546519137256,12.2,2.5105685062388));
#300662=CARTESIAN_POINT('Ctrl Pts',(-3.12947823622448,12.2,2.50659179575057));
#300663=CARTESIAN_POINT('Ctrl Pts',(-3.12539205517989,12.2,2.50387763494345));
#300664=CARTESIAN_POINT('Ctrl Pts',(-3.12226302098882,12.2,2.50167644123223));
#300665=CARTESIAN_POINT('Ctrl Pts',(-3.12010253332815,12.2,2.50010760672021));
#300666=CARTESIAN_POINT('Ctrl Pts',(-3.11902228949781,12.2,2.4993231894642));
#300667=CARTESIAN_POINT('Ctrl Pts',(-3.11818413389332,12.2,2.49869705722392));
#300668=CARTESIAN_POINT('Ctrl Pts',(-3.11758918392009,12.2,2.49824543008379));
#300669=CARTESIAN_POINT('Ctrl Pts',(-3.11729170893347,12.2,2.49801961651373));
#300670=CARTESIAN_POINT('Ctrl Pts',(-3.11705503249409,12.2,2.49783745985302));
#300671=CARTESIAN_POINT('Ctrl Pts',(-3.11687927028665,12.2,2.49770102503292));
#300672=CARTESIAN_POINT('Ctrl Pts',(-3.11677151728329,12.2,2.49761738212787));
#300673=CARTESIAN_POINT('Ctrl Pts',(-3.11668713186045,12.2,2.49755136519769));
#300674=CARTESIAN_POINT('Ctrl Pts',(-3.11662457182833,12.2,2.49750218397371));
#300675=CARTESIAN_POINT('Ctrl Pts',(-3.11659040942531,12.2,2.49747532738912));
#300676=CARTESIAN_POINT('Ctrl Pts',(-3.11656553206438,12.2,2.49745561966817));
#300677=CARTESIAN_POINT('Ctrl Pts',(-3.11654335547073,12.2,2.49743798830104));
#300678=CARTESIAN_POINT('Ctrl Pts',(-3.11653990011135,12.2,2.49743524113839));
#300679=CARTESIAN_POINT('Ctrl Pts',(-3.11653645629695,12.2,2.4974325028997));
#300680=CARTESIAN_POINT('Ctrl Pts',(-3.11653301183405,12.2,2.49742976420877));
#300681=CARTESIAN_POINT('',(-2.82878727700006,12.2,2.26684528399999));
#300682=CARTESIAN_POINT('',(-3.11652602300006,12.2,2.49742420999999));
#300683=CARTESIAN_POINT('',(-2.44494327000006,12.2,2.67635524699998));
#300684=CARTESIAN_POINT('Origin',(-5.66300478732629E-14,12.2,-1.77635683940025E-14));
#300685=CARTESIAN_POINT('',(-2.69364953994162,12.2,2.94860152033068));
#300686=CARTESIAN_POINT('',(-2.44494327000006,12.2,2.67635524699998));
#300687=CARTESIAN_POINT('',(-2.94378355400006,12.2,3.72781952199999));
#300688=CARTESIAN_POINT('Ctrl Pts',(-2.69364946515999,12.2,2.94860158817627));
#300689=CARTESIAN_POINT('Ctrl Pts',(-2.69383177439424,12.2,2.94880253537606));
#300690=CARTESIAN_POINT('Ctrl Pts',(-2.69401090483053,12.1999999999997,
2.94900635440571));
#300691=CARTESIAN_POINT('Ctrl Pts',(-2.69456846309778,12.1999999999997,
2.94964281651214));
#300692=CARTESIAN_POINT('Ctrl Pts',(-2.69496497063731,12.2,2.95010428156435));
#300693=CARTESIAN_POINT('Ctrl Pts',(-2.69668033191381,12.2,2.95212492184448));
#300694=CARTESIAN_POINT('Ctrl Pts',(-2.69806509480641,12.1999999999079,
2.95382201005389));
#300695=CARTESIAN_POINT('Ctrl Pts',(-2.70406029290256,12.1999999999079,
2.96134042105594));
#300696=CARTESIAN_POINT('Ctrl Pts',(-2.70883395520956,12.1999999999079,
2.96782105431918));
#300697=CARTESIAN_POINT('Ctrl Pts',(-2.72898834256397,12.1999999999079,
2.99646249251351));
#300698=CARTESIAN_POINT('Ctrl Pts',(-2.74405879664829,12.2,3.02161189257851));
#300699=CARTESIAN_POINT('Ctrl Pts',(-2.79448036335615,12.2,3.11426835608687));
#300700=CARTESIAN_POINT('Ctrl Pts',(-2.83379571846681,12.2,3.2058879483145));
#300701=CARTESIAN_POINT('Ctrl Pts',(-2.90612983688009,12.2,3.45297987201336));
#300702=CARTESIAN_POINT('Ctrl Pts',(-2.9304772130833,12.2,3.59014359399116));
#300703=CARTESIAN_POINT('Ctrl Pts',(-2.94378355400006,12.2,3.72781952199999));
#300704=CARTESIAN_POINT('',(-2.67208816000006,12.2,3.92714207399998));
#300705=CARTESIAN_POINT('Origin',(-5.66300478732629E-14,12.2,-1.77635683940025E-14));
#300706=CARTESIAN_POINT('',(-2.00390023382555,12.2,3.45459781463392));
#300707=CARTESIAN_POINT('Ctrl Pts',(-2.67208816000006,12.2,3.92714207399998));
#300708=CARTESIAN_POINT('Ctrl Pts',(-2.54470272548118,12.2,3.87309341167482));
#300709=CARTESIAN_POINT('Ctrl Pts',(-2.42161063813132,12.2,3.80890442524401));
#300710=CARTESIAN_POINT('Ctrl Pts',(-2.20787373403996,12.2,3.66600708574621));
#300711=CARTESIAN_POINT('Ctrl Pts',(-2.13195690805562,12.2,3.60084568574312));
#300712=CARTESIAN_POINT('Ctrl Pts',(-2.0583252666406,12.2,3.52451513065958));
#300713=CARTESIAN_POINT('Ctrl Pts',(-2.0388379215194,12.2000000000748,3.50255771474838));
#300714=CARTESIAN_POINT('Ctrl Pts',(-2.01046851767774,12.2000000000748,
3.46541597332446));
#300715=CARTESIAN_POINT('Ctrl Pts',(-2.00486827616945,12.2,3.45625245717719));
#300716=CARTESIAN_POINT('Ctrl Pts',(-2.00390029233317,12.2,3.45459778040704));
#300717=CARTESIAN_POINT('',(-1.81888661200006,12.2,3.13564610499999));
#300718=CARTESIAN_POINT('',(-2.00390028500005,12.2,3.45459777499999));
#300719=CARTESIAN_POINT('',(-1.31303067400006,12.2,3.37884232399999));
#300720=CARTESIAN_POINT('Origin',(-5.66300478732629E-14,12.2,-1.77635683940025E-14));
#300721=CARTESIAN_POINT('',(-1.44659566557757,12.2,3.72254748089793));
#300722=CARTESIAN_POINT('',(-1.31303067400006,12.2,3.37884232399999));
#300723=CARTESIAN_POINT('',(-1.39835267900006,12.2,4.53950545599999));
#300724=CARTESIAN_POINT('Ctrl Pts',(-1.44659557109088,12.2,3.72254751723615));
#300725=CARTESIAN_POINT('Ctrl Pts',(-1.44669296442588,12.2,3.72280075945341));
#300726=CARTESIAN_POINT('Ctrl Pts',(-1.4467863863064,12.1999999999997,3.72305551966744));
#300727=CARTESIAN_POINT('Ctrl Pts',(-1.44707664467613,12.1999999999997,
3.72385115239218));
#300728=CARTESIAN_POINT('Ctrl Pts',(-1.44727952399059,12.2,3.72442428851802));
#300729=CARTESIAN_POINT('Ctrl Pts',(-1.44814961145563,12.2,3.72692957023441));
#300730=CARTESIAN_POINT('Ctrl Pts',(-1.44882811640487,12.199999999908,3.72901348813528));
#300731=CARTESIAN_POINT('Ctrl Pts',(-1.45170124179413,12.199999999908,3.73818584407418));
#300732=CARTESIAN_POINT('Ctrl Pts',(-1.45381079932822,12.199999999908,3.74595029799757));
#300733=CARTESIAN_POINT('Ctrl Pts',(-1.46226030946429,12.199999999908,3.77994874903547));
#300734=CARTESIAN_POINT('Ctrl Pts',(-1.46722768673953,12.2,3.80884656437798));
#300735=CARTESIAN_POINT('Ctrl Pts',(-1.48078731749073,12.2,3.91357120575646));
#300736=CARTESIAN_POINT('Ctrl Pts',(-1.4843227561384,12.2,4.01323730435706));
#300737=CARTESIAN_POINT('Ctrl Pts',(-1.46252018784725,12.2,4.26968072123177));
#300738=CARTESIAN_POINT('Ctrl Pts',(-1.43552455444774,12.2,4.40687162494879));
#300739=CARTESIAN_POINT('Ctrl Pts',(-1.39835267900006,12.2,4.53950545599998));
#300740=CARTESIAN_POINT('',(-1.07300065765139,12.2,4.62722050353667));
#300741=CARTESIAN_POINT('Origin',(-5.66300478732629E-14,12.2,-1.77635683940025E-14));
#300742=CARTESIAN_POINT('',(-0.620636653770277,12.2,3.9452088280328));
#300743=CARTESIAN_POINT('Ctrl Pts',(-1.07300065706596,12.2,4.62722050309264));
#300744=CARTESIAN_POINT('Ctrl Pts',(-1.0507849572306,12.2,4.60564108152845));
#300745=CARTESIAN_POINT('Ctrl Pts',(-1.02944940026969,12.2,4.58413736641884));
#300746=CARTESIAN_POINT('Ctrl Pts',(-1.00899345236455,12.2,4.56276913341815));
#300747=CARTESIAN_POINT('Ctrl Pts',(-0.971388421889957,12.2,4.52348701083426));
#300748=CARTESIAN_POINT('Ctrl Pts',(-0.936758198137158,12.2,4.48466285825686));
#300749=CARTESIAN_POINT('Ctrl Pts',(-0.905070969024602,12.2,4.44670166000136));
#300750=CARTESIAN_POINT('Ctrl Pts',(-0.874654520745516,12.2,4.41026285308488));
#300751=CARTESIAN_POINT('Ctrl Pts',(-0.846949885617722,12.2,4.37461914823072));
#300752=CARTESIAN_POINT('Ctrl Pts',(-0.821892991659933,12.2,4.34015678120677));
#300753=CARTESIAN_POINT('Ctrl Pts',(-0.797601978032624,12.2,4.30674777894103));
#300754=CARTESIAN_POINT('Ctrl Pts',(-0.77579954999807,12.2,4.27444890333346));
#300755=CARTESIAN_POINT('Ctrl Pts',(-0.756389823805907,12.2,4.24363974821588));
#300756=CARTESIAN_POINT('Ctrl Pts',(-0.737708294855191,12.2,4.21398646420878));
#300757=CARTESIAN_POINT('Ctrl Pts',(-0.721243540586764,12.2,4.18571311401967));
#300758=CARTESIAN_POINT('Ctrl Pts',(-0.706871483729886,12.2,4.15918547425683));
#300759=CARTESIAN_POINT('Ctrl Pts',(-0.693077220900548,12.2,4.13372431453733));
#300760=CARTESIAN_POINT('Ctrl Pts',(-0.681211010007532,12.2,4.10987120057421));
#300761=CARTESIAN_POINT('Ctrl Pts',(-0.671123604797768,12.2,4.08797668630482));
#300762=CARTESIAN_POINT('Ctrl Pts',(-0.66135402368667,12.2,4.06677200297993));
#300763=CARTESIAN_POINT('Ctrl Pts',(-0.653253266385538,12.2,4.04740423646243));
#300764=CARTESIAN_POINT('Ctrl Pts',(-0.646643456602352,12.2,4.03022032450418));
#300765=CARTESIAN_POINT('Ctrl Pts',(-0.640601123809652,12.2,4.01451171591513));
#300766=CARTESIAN_POINT('Ctrl Pts',(-0.635804690486196,12.2,4.00062807843892));
#300767=CARTESIAN_POINT('Ctrl Pts',(-0.632080686925434,12.2,3.98885955077024));
#300768=CARTESIAN_POINT('Ctrl Pts',(-0.628517809363524,12.2,3.97760021052436));
#300769=CARTESIAN_POINT('Ctrl Pts',(-0.625936885444006,12.2,3.9682766719032));
#300770=CARTESIAN_POINT('Ctrl Pts',(-0.624147610493951,12.2,3.96116869451554));
#300771=CARTESIAN_POINT('Ctrl Pts',(-0.622908591722011,12.2,3.95624663521237));
#300772=CARTESIAN_POINT('Ctrl Pts',(-0.622048443669106,12.2,3.95238744701319));
#300773=CARTESIAN_POINT('Ctrl Pts',(-0.621490912601253,12.2,3.94969285919901));
#300774=CARTESIAN_POINT('Ctrl Pts',(-0.621212147067327,12.2,3.94834556529192));
#300775=CARTESIAN_POINT('Ctrl Pts',(-0.621008857541319,12.2,3.94728953113019));
#300776=CARTESIAN_POINT('Ctrl Pts',(-0.620870323783881,12.2,3.94653829591385));
#300777=CARTESIAN_POINT('Ctrl Pts',(-0.620801056905161,12.2,3.94616267830568));
#300778=CARTESIAN_POINT('Ctrl Pts',(-0.620747955427695,12.2,3.94586327661587));
#300779=CARTESIAN_POINT('Ctrl Pts',(-0.620709628879688,12.2,3.94564180448601));
#300780=CARTESIAN_POINT('Ctrl Pts',(-0.620685910104493,12.2,3.94550474419926));
#300781=CARTESIAN_POINT('Ctrl Pts',(-0.620667909838897,12.2,3.94539829416118));
#300782=CARTESIAN_POINT('Ctrl Pts',(-0.620654939939172,12.2,3.94532036311127));
#300783=CARTESIAN_POINT('Ctrl Pts',(-0.620646952117413,12.2,3.94527236741744));
#300784=CARTESIAN_POINT('Ctrl Pts',(-0.620641950349572,12.2,3.94524125295544));
#300785=CARTESIAN_POINT('Ctrl Pts',(-0.620636729615096,12.2,3.94520886906205));
#300786=CARTESIAN_POINT('',(-0.563335230000056,12.2,3.58096054499998));
#300787=CARTESIAN_POINT('',(-0.620636721000055,12.2,3.94520881799998));
#300788=CARTESIAN_POINT('',(-0.00378600900005522,12.2,3.62499802299999));
#300789=CARTESIAN_POINT('Origin',(-5.66300478732629E-14,12.2,-1.77635683940025E-14));
#300790=CARTESIAN_POINT('',(-0.0041710307407783,12.2,3.99374277690018));
#300791=CARTESIAN_POINT('',(-0.00378600900005522,12.2,3.62499802299999));
#300792=CARTESIAN_POINT('',(0.335933474325597,12.2,4.73810602455833));
#300793=CARTESIAN_POINT('Ctrl Pts',(-0.00417093000005587,12.2,3.99374277699999));
#300794=CARTESIAN_POINT('Ctrl Pts',(-0.00417024165288169,12.2,3.99401409886674));
#300795=CARTESIAN_POINT('Ctrl Pts',(-0.00416534981364848,12.1999999999997,
3.99428540196681));
#300796=CARTESIAN_POINT('Ctrl Pts',(-0.00414859876650465,12.1999999999997,
3.99513161023346));
#300797=CARTESIAN_POINT('Ctrl Pts',(-0.00413071236587515,12.2,3.99574033513076));
#300798=CARTESIAN_POINT('Ctrl Pts',(-0.0040371607748202,12.2,3.99838724109435));
#300799=CARTESIAN_POINT('Ctrl Pts',(-0.00391727435201773,12.1999999999079,
4.00057359205342));
#300800=CARTESIAN_POINT('Ctrl Pts',(-0.00328249533119052,12.1999999999079,
4.01017095407316));
#300801=CARTESIAN_POINT('Ctrl Pts',(-0.0024444871704632,12.1999999999079,
4.01817466079553));
#300802=CARTESIAN_POINT('Ctrl Pts',(0.00195733879072123,12.1999999999079,
4.05292260177391));
#300803=CARTESIAN_POINT('Ctrl Pts',(0.00776259300637182,12.2,4.08165749006985));
#300804=CARTESIAN_POINT('Ctrl Pts',(0.0330060981399338,12.2,4.18443935972204));
#300805=CARTESIAN_POINT('Ctrl Pts',(0.0657739729375395,12.2,4.27866713336303));
#300806=CARTESIAN_POINT('Ctrl Pts',(0.178614829390611,12.2,4.50965703821246));
#300807=CARTESIAN_POINT('Ctrl Pts',(0.253251233611231,12.2,4.62771303457587));
#300808=CARTESIAN_POINT('Ctrl Pts',(0.335933474999944,12.2,4.73810602399999));
#300809=CARTESIAN_POINT('',(0.671001528968269,12.2,4.70236716444468));
#300810=CARTESIAN_POINT('Origin',(-5.66300478732629E-14,12.2,-1.77635683940025E-14));
#300811=CARTESIAN_POINT('',(0.846447363903509,12.2,3.90299749089007));
#300812=CARTESIAN_POINT('Ctrl Pts',(0.671001528999944,12.2,4.70236716399998));
#300813=CARTESIAN_POINT('Ctrl Pts',(0.689750617970205,12.2,4.66152111816135));
#300814=CARTESIAN_POINT('Ctrl Pts',(0.706827850453991,12.2,4.62149223703923));
#300815=CARTESIAN_POINT('Ctrl Pts',(0.722304674338832,12.2,4.58245379874695));
#300816=CARTESIAN_POINT('Ctrl Pts',(0.741807263919132,12.2,4.53326084769089));
#300817=CARTESIAN_POINT('Ctrl Pts',(0.758767324969944,12.2,4.48564127013701));
#300818=CARTESIAN_POINT('Ctrl Pts',(0.773369417859129,12.2,4.43995898600264));
#300819=CARTESIAN_POINT('Ctrl Pts',(0.787377131758578,12.2,4.39613620174263));
#300820=CARTESIAN_POINT('Ctrl Pts',(0.79921477102076,12.2,4.35409623312068));
#300821=CARTESIAN_POINT('Ctrl Pts',(0.809089552047529,12.2,4.31417337674083));
#300822=CARTESIAN_POINT('Ctrl Pts',(0.818602810828708,12.2,4.2757121224613));
#300823=CARTESIAN_POINT('Ctrl Pts',(0.826294080583583,12.2,4.23921581476659));
#300824=CARTESIAN_POINT('Ctrl Pts',(0.832393390803862,12.2,4.20499530620236));
#300825=CARTESIAN_POINT('Ctrl Pts',(0.838252673463236,12.2,4.17212148519901));
#300826=CARTESIAN_POINT('Ctrl Pts',(0.842642574720562,12.2,4.14134786481141));
#300827=CARTESIAN_POINT('Ctrl Pts',(0.845812337415013,12.2,4.11296125522075));
#300828=CARTESIAN_POINT('Ctrl Pts',(0.848839496067851,12.2,4.0858517271171));
#300829=CARTESIAN_POINT('Ctrl Pts',(0.850753570419483,12.2,4.06091921258366));
#300830=CARTESIAN_POINT('Ctrl Pts',(0.851817032964709,12.2,4.03842413570375));
#300831=CARTESIAN_POINT('Ctrl Pts',(0.852808803672242,12.2,4.01744553291857));
#300832=CARTESIAN_POINT('Ctrl Pts',(0.853060701605771,12.2,3.99858680463442));
#300833=CARTESIAN_POINT('Ctrl Pts',(0.852827866970706,12.2,3.98206865845845));
#300834=CARTESIAN_POINT('Ctrl Pts',(0.852604043162,12.2,3.96618977347707));
#300835=CARTESIAN_POINT('Ctrl Pts',(0.85193190637898,12.2,3.95247375923966));
#300836=CARTESIAN_POINT('Ctrl Pts',(0.851081822358656,12.2,3.94112639931417));
#300837=CARTESIAN_POINT('Ctrl Pts',(0.850268518793122,12.2,3.93027000386836));
#300838=CARTESIAN_POINT('Ctrl Pts',(0.849291970755508,12.2,3.92158163117595));
#300839=CARTESIAN_POINT('Ctrl Pts',(0.848434785939518,12.2,3.91525181550474));
#300840=CARTESIAN_POINT('Ctrl Pts',(0.84791939618732,12.2,3.91144595932368));
#300841=CARTESIAN_POINT('Ctrl Pts',(0.847448067511482,12.2,3.90849293832927));
#300842=CARTESIAN_POINT('Ctrl Pts',(0.847091867570908,12.2,3.90643638947668));
#300843=CARTESIAN_POINT('Ctrl Pts',(0.846913767600621,12.2,3.90540811505039));
#300844=CARTESIAN_POINT('Ctrl Pts',(0.846764561790633,12.2,3.90460397331201));
#300845=CARTESIAN_POINT('Ctrl Pts',(0.846653981297917,12.2,3.90402963828343));
#300846=CARTESIAN_POINT('Ctrl Pts',(0.846598691051559,12.2,3.90374247076914));
#300847=CARTESIAN_POINT('Ctrl Pts',(0.846553019198255,12.2,3.90351273146421));
#300848=CARTESIAN_POINT('Ctrl Pts',(0.846518305619912,12.2,3.90334117504919));
#300849=CARTESIAN_POINT('Ctrl Pts',(0.846494840731448,12.2,3.90322521027874));
#300850=CARTESIAN_POINT('Ctrl Pts',(0.846476253679565,12.2,3.90313481853468));
#300851=CARTESIAN_POINT('Ctrl Pts',(0.846463233076636,12.2,3.90307263461551));
#300852=CARTESIAN_POINT('Ctrl Pts',(0.84645699120915,12.2,3.90304282464548));
#300853=CARTESIAN_POINT('Ctrl Pts',(0.846452319816075,12.2,3.90302108760437));
#300854=CARTESIAN_POINT('Ctrl Pts',(0.846447309728966,12.2,3.90299755605768));
#300855=CARTESIAN_POINT('',(0.768297694750895,12.2,3.54264641972273));
#300856=CARTESIAN_POINT('',(0.846447299999944,12.2,3.90299750499998));
#300857=CARTESIAN_POINT('',(1.30596997799994,12.2,3.38157765299999));
#300858=CARTESIAN_POINT('Origin',(-5.66300478732629E-14,12.2,-1.77635683940025E-14));
#300859=CARTESIAN_POINT('',(1.43881692432775,12.2,3.72556098059384));
#300860=CARTESIAN_POINT('',(1.30596997799994,12.2,3.38157765299999));
#300861=CARTESIAN_POINT('',(2.02484994999994,12.2,4.29679911999998));
#300862=CARTESIAN_POINT('Ctrl Pts',(1.43881701800443,12.2,3.72556094401147));
#300863=CARTESIAN_POINT('Ctrl Pts',(1.43891571542436,12.2,3.72581367906159));
#300864=CARTESIAN_POINT('Ctrl Pts',(1.43901824239838,12.1999999999997,3.72606491060791));
#300865=CARTESIAN_POINT('Ctrl Pts',(1.43933918812595,12.1999999999997,3.72684706398779));
#300866=CARTESIAN_POINT('Ctrl Pts',(1.43957531344741,12.2,3.72740719862251));
#300867=CARTESIAN_POINT('Ctrl Pts',(1.44062068239649,12.2,3.72984614017064));
#300868=CARTESIAN_POINT('Ctrl Pts',(1.44152373669993,12.1999999999078,3.73184446484589));
#300869=CARTESIAN_POINT('Ctrl Pts',(1.44557809881245,12.1999999999078,3.74055478896382));
#300870=CARTESIAN_POINT('Ctrl Pts',(1.44925055570118,12.1999999999078,3.74771538267329));
#300871=CARTESIAN_POINT('Ctrl Pts',(1.46590832509403,12.1999999999078,3.77852819662625));
#300872=CARTESIAN_POINT('Ctrl Pts',(1.48170041768112,12.2,3.80322417128525));
#300873=CARTESIAN_POINT('Ctrl Pts',(1.54222286540467,12.2,3.88973841319805));
#300874=CARTESIAN_POINT('Ctrl Pts',(1.60672952262203,12.2,3.96575969106281));
#300875=CARTESIAN_POINT('Ctrl Pts',(1.79561314049852,12.2,4.14059190618597));
#300876=CARTESIAN_POINT('Ctrl Pts',(1.9075685457603,12.2,4.22353887709006));
#300877=CARTESIAN_POINT('Ctrl Pts',(2.02484995028062,12.2,4.29679911955065));
#300878=CARTESIAN_POINT('',(2.32438124132219,12.2,4.14243308298023));
#300879=CARTESIAN_POINT('Origin',(-5.66300478732629E-14,12.2,-1.77635683940025E-14));
#300880=CARTESIAN_POINT('',(2.19921397760577,12.2,3.33366471456779));
#300881=CARTESIAN_POINT('Ctrl Pts',(2.32438124099994,12.2,4.14243308299998));
#300882=CARTESIAN_POINT('Ctrl Pts',(2.33276945463597,12.2,4.00447590820319));
#300883=CARTESIAN_POINT('Ctrl Pts',(2.33018902391579,12.2,3.86552790147597));
#300884=CARTESIAN_POINT('Ctrl Pts',(2.29756209278249,12.2,3.61065448254086));
#300885=CARTESIAN_POINT('Ctrl Pts',(2.27310042612445,12.2,3.51362648008036));
#300886=CARTESIAN_POINT('Ctrl Pts',(2.2375381345951,12.2,3.41353790557386));
#300887=CARTESIAN_POINT('Ctrl Pts',(2.22657068478963,12.2000000000756,3.38631279890763));
#300888=CARTESIAN_POINT('Ctrl Pts',(2.21112646047588,12.2000000000756,3.35486547673215));
#300889=CARTESIAN_POINT('Ctrl Pts',(2.20743003282668,12.2000000000756,3.34773476935894));
#300890=CARTESIAN_POINT('Ctrl Pts',(2.20270375929611,12.2000000000756,3.33941537254005));
#300891=CARTESIAN_POINT('Ctrl Pts',(2.20160840104712,12.2,3.33753660556523));
#300892=CARTESIAN_POINT('Ctrl Pts',(2.20024479446,12.2,3.33529963498368));
#300893=CARTESIAN_POINT('Ctrl Pts',(2.19993114734272,12.2000000000005,3.33479192891932));
#300894=CARTESIAN_POINT('Ctrl Pts',(2.19957309575045,12.2000000000005,3.33422465248725));
#300895=CARTESIAN_POINT('Ctrl Pts',(2.19936920503646,12.2,3.33390204975526));
#300896=CARTESIAN_POINT('Ctrl Pts',(2.19921392137674,12.2,3.33366475136423));
#300897=CARTESIAN_POINT('',(1.99616775954023,12.2,3.02587826526674));
#300898=CARTESIAN_POINT('',(2.19921392199994,12.2,3.33366475199998));
#300899=CARTESIAN_POINT('',(2.43934748299994,12.2,2.68145648099999));
#300900=CARTESIAN_POINT('Origin',(-5.66300478732629E-14,12.2,-1.77635683940025E-14));
#300901=CARTESIAN_POINT('',(2.68748468083623,12.2,2.9542215299112));
#300902=CARTESIAN_POINT('',(2.43934748299994,12.2,2.68145648099999));
#300903=CARTESIAN_POINT('',(3.44029922199995,12.2,3.27518568399999));
#300904=CARTESIAN_POINT('Ctrl Pts',(2.68748475499994,12.2,2.95422146199999));
#300905=CARTESIAN_POINT('Ctrl Pts',(2.68766810418239,12.2,2.95442145981663));
#300906=CARTESIAN_POINT('Ctrl Pts',(2.68785444461358,12.1999999999997,2.95461870580728));
#300907=CARTESIAN_POINT('Ctrl Pts',(2.68843649977677,12.1999999999997,2.95523235155731));
#300908=CARTESIAN_POINT('Ctrl Pts',(2.68885952550013,12.2,2.95566986667335));
#300909=CARTESIAN_POINT('Ctrl Pts',(2.6907140028693,12.2,2.95756511229716));
#300910=CARTESIAN_POINT('Ctrl Pts',(2.69227789133226,12.1999999999079,2.95910224681046));
#300911=CARTESIAN_POINT('Ctrl Pts',(2.69920541755507,12.1999999999079,2.96576016437954));
#300912=CARTESIAN_POINT('Ctrl Pts',(2.70521670352856,12.1999999999079,2.97111070509354));
#300913=CARTESIAN_POINT('Ctrl Pts',(2.73188047686284,12.1999999999079,2.99382533939136));
#300914=CARTESIAN_POINT('Ctrl Pts',(2.75552513406558,12.2,3.01114739782507));
#300915=CARTESIAN_POINT('Ctrl Pts',(2.84363361994914,12.2,3.07023822782865));
#300916=CARTESIAN_POINT('Ctrl Pts',(2.93139608331567,12.2,3.11776816464238));
#300917=CARTESIAN_POINT('Ctrl Pts',(3.17016487496149,12.2,3.21235683542494));
#300918=CARTESIAN_POINT('Ctrl Pts',(3.30518397689249,12.2,3.24937563452363));
#300919=CARTESIAN_POINT('Ctrl Pts',(3.44029922199995,12.2,3.27518568399999));
#300920=CARTESIAN_POINT('',(3.66384038699994,12.2,3.02304045899999));
#300921=CARTESIAN_POINT('Origin',(-5.66300478732629E-14,12.2,-1.77635683940025E-14));
#300922=CARTESIAN_POINT('',(3.25496455695711,12.2,2.31410204699751));
#300923=CARTESIAN_POINT('Ctrl Pts',(3.66384038663958,12.2,3.0230404588706));
#300924=CARTESIAN_POINT('Ctrl Pts',(3.65004021639256,12.2,2.97979079468028));
#300925=CARTESIAN_POINT('Ctrl Pts',(3.6355410673424,12.2,2.93830654304683));
#300926=CARTESIAN_POINT('Ctrl Pts',(3.62051781872112,12.2,2.89867000875219));
#300927=CARTESIAN_POINT('Ctrl Pts',(3.60181539509289,12.2,2.84932653623033));
#300928=CARTESIAN_POINT('Ctrl Pts',(3.58230031128659,12.2,2.80284793622846));
#300929=CARTESIAN_POINT('Ctrl Pts',(3.56235203927954,12.2,2.75937773445781));
#300930=CARTESIAN_POINT('Ctrl Pts',(3.54321245661152,12.2,2.71766978501283));
#300931=CARTESIAN_POINT('Ctrl Pts',(3.52367400370563,12.2,2.67873141952692));
#300932=CARTESIAN_POINT('Ctrl Pts',(3.50411306518538,12.2,2.64266933700222));
#300933=CARTESIAN_POINT('Ctrl Pts',(3.48530900365763,12.2,2.60800261495761));
#300934=CARTESIAN_POINT('Ctrl Pts',(3.46648405527645,12.2,2.57599404382551));
#300935=CARTESIAN_POINT('Ctrl Pts',(3.4480130972279,12.2,2.54671742996617));
#300936=CARTESIAN_POINT('Ctrl Pts',(3.43017328439979,12.2,2.51844118624785));
#300937=CARTESIAN_POINT('Ctrl Pts',(3.41266347568383,12.2,2.49271356238918));
#300938=CARTESIAN_POINT('Ctrl Pts',(3.39586256226689,12.2,2.46957875447664));
#300939=CARTESIAN_POINT('Ctrl Pts',(3.37963335056515,12.2,2.44723117812919));
#300940=CARTESIAN_POINT('Ctrl Pts',(3.36406534738878,12.2,2.42730316202406));
#300941=CARTESIAN_POINT('Ctrl Pts',(3.3495426582697,12.2,2.40981071661852));
#300942=CARTESIAN_POINT('Ctrl Pts',(3.33613594551948,12.2,2.39366245448001));
#300943=CARTESIAN_POINT('Ctrl Pts',(3.32362008334591,12.2,2.37958984249667));
#300944=CARTESIAN_POINT('Ctrl Pts',(3.3123355631942,12.2,2.36758366996853));
#300945=CARTESIAN_POINT('Ctrl Pts',(3.30155454011509,12.2,2.35611319347705));
#300946=CARTESIAN_POINT('Ctrl Pts',(3.29189718479154,12.2,2.34652900741971));
#300947=CARTESIAN_POINT('Ctrl Pts',(3.28369897633022,12.2,2.33880100197491));
#300948=CARTESIAN_POINT('Ctrl Pts',(3.27585943539416,12.2,2.33141109290826));
#300949=CARTESIAN_POINT('Ctrl Pts',(3.26935383400655,12.2,2.3257186557819));
#300950=CARTESIAN_POINT('Ctrl Pts',(3.26451584584619,12.2,2.32167436186622));
#300951=CARTESIAN_POINT('Ctrl Pts',(3.26162365731134,12.2,2.31925665018384));
#300952=CARTESIAN_POINT('Ctrl Pts',(3.25932822240677,12.2,2.31742748566471));
#300953=CARTESIAN_POINT('Ctrl Pts',(3.25770916214891,12.2,2.31617162237947));
#300954=CARTESIAN_POINT('Ctrl Pts',(3.25689963201998,12.2,2.31554369073685));
#300955=CARTESIAN_POINT('Ctrl Pts',(3.25625928522045,12.2,2.3150590283412));
#300956=CARTESIAN_POINT('Ctrl Pts',(3.25579882407171,12.2,2.31471533066125));
#300957=CARTESIAN_POINT('Ctrl Pts',(3.25556859349734,12.2,2.31454348182128));
#300958=CARTESIAN_POINT('Ctrl Pts',(3.25538328548142,12.2,2.31440688227762));
#300959=CARTESIAN_POINT('Ctrl Pts',(3.2552443668341,12.2,2.31430519881979));
#300960=CARTESIAN_POINT('Ctrl Pts',(3.25514984661369,12.2,2.31423601341501));
#300961=CARTESIAN_POINT('Ctrl Pts',(3.25507590025553,12.2,2.31418223108013));
#300962=CARTESIAN_POINT('Ctrl Pts',(3.25502519035787,12.2,2.31414564573923));
#300963=CARTESIAN_POINT('Ctrl Pts',(3.25500137069604,12.2,2.31412846072234));
#300964=CARTESIAN_POINT('Ctrl Pts',(3.25498365476425,12.2,2.31411582124383));
#300965=CARTESIAN_POINT('Ctrl Pts',(3.25496456102782,12.2,2.3141021319611));
#300966=CARTESIAN_POINT('',(2.95444430678277,12.2,2.10044848453536));
#300967=CARTESIAN_POINT('',(3.25496451799994,12.2,2.31410210199999));
#300968=CARTESIAN_POINT('',(3.24327759199994,12.2,1.61918975399999));
#300969=CARTESIAN_POINT('Origin',(-5.66300478732629E-14,12.2,-1.77635683940025E-14));
#300970=CARTESIAN_POINT('',(3.57319274026315,12.2,1.78389809210464));
#300971=CARTESIAN_POINT('',(3.24327759199994,12.2,1.61918975399999));
#300972=CARTESIAN_POINT('',(4.39111701799995,12.2,1.81124027399999));
#300973=CARTESIAN_POINT('Ctrl Pts',(3.57320811899994,12.2,1.78390558399999));
#300974=CARTESIAN_POINT('Ctrl Pts',(3.573471434563,12.2,1.78403581721233));
#300975=CARTESIAN_POINT('Ctrl Pts',(3.57385384963781,12.1999999999998,1.78421671185872));
#300976=CARTESIAN_POINT('Ctrl Pts',(3.57444583390415,12.1999999999998,1.78449699969217));
#300977=CARTESIAN_POINT('Ctrl Pts',(3.57499885979161,12.2,1.78475240106916));
#300978=CARTESIAN_POINT('Ctrl Pts',(3.57741451025376,12.2,1.78585050902155));
#300979=CARTESIAN_POINT('Ctrl Pts',(3.57942953936059,12.1999999999353,1.78671951455766));
#300980=CARTESIAN_POINT('Ctrl Pts',(3.58830406673956,12.1999999999353,1.79042908219111));
#300981=CARTESIAN_POINT('Ctrl Pts',(3.59584781630494,12.1999999999353,1.79324846166707));
#300982=CARTESIAN_POINT('Ctrl Pts',(3.62895086887599,12.1999999999353,1.80480706665112));
#300983=CARTESIAN_POINT('Ctrl Pts',(3.65729094241754,12.2,1.81242373874791));
#300984=CARTESIAN_POINT('Ctrl Pts',(3.76042940298413,12.2,1.83560201230679));
#300985=CARTESIAN_POINT('Ctrl Pts',(3.85943144621604,12.2,1.84831099332293));
#300986=CARTESIAN_POINT('Ctrl Pts',(4.11673089669352,12.2,1.85021299219715));
#300987=CARTESIAN_POINT('Ctrl Pts',(4.2554861848505,12.2,1.83603990528381));
#300988=CARTESIAN_POINT('Ctrl Pts',(4.39111701799995,12.2,1.81124027399999));
#300989=CARTESIAN_POINT('',(4.50847758599994,12.2,1.49536946999998));
#300990=CARTESIAN_POINT('Origin',(-5.66300478732629E-14,12.2,-1.77635683940025E-14));
#300991=CARTESIAN_POINT('',(3.87111413641841,12.2,0.982007073016362));
#300992=CARTESIAN_POINT('Ctrl Pts',(4.50847758599994,12.2,1.49536947099998));
#300993=CARTESIAN_POINT('Ctrl Pts',(4.42189143693061,12.2,1.38796023687308));
#300994=CARTESIAN_POINT('Ctrl Pts',(4.32625365229783,12.2,1.28685002287302));
#300995=CARTESIAN_POINT('Ctrl Pts',(4.13004445467292,12.2,1.12014543536591));
#300996=CARTESIAN_POINT('Ctrl Pts',(4.04660568678907,12.2,1.06503627533653));
#300997=CARTESIAN_POINT('Ctrl Pts',(3.95325368265746,12.2,1.01521924022475));
#300998=CARTESIAN_POINT('Ctrl Pts',(3.92680090281939,12.2000000000757,1.00248483664623));
#300999=CARTESIAN_POINT('Ctrl Pts',(3.89420290683788,12.2000000000757,0.989650213179769));
#301000=CARTESIAN_POINT('Ctrl Pts',(3.88666701235301,12.2000000000757,0.98687056215581));
#301001=CARTESIAN_POINT('Ctrl Pts',(3.8775671417713,12.2000000000757,0.983905758842116));
#301002=CARTESIAN_POINT('Ctrl Pts',(3.87549245275233,12.2,0.983255419398263));
#301003=CARTESIAN_POINT('Ctrl Pts',(3.87297812162379,12.2,0.982521063410915));
#301004=CARTESIAN_POINT('Ctrl Pts',(3.87240393490892,12.2000000000005,0.982357051593943));
#301005=CARTESIAN_POINT('Ctrl Pts',(3.87161345090973,12.2000000000005,0.982139498976519));
#301006=CARTESIAN_POINT('Ctrl Pts',(3.87136421885209,12.2,0.982071645256235));
#301007=CARTESIAN_POINT('Ctrl Pts',(3.87111411939993,12.2,0.982007138999299));
#301008=CARTESIAN_POINT('',(3.51370678013976,12.2,0.891341496431592));
#301009=CARTESIAN_POINT('',(3.87111411999994,12.2,0.982007138999985));
#301010=CARTESIAN_POINT('',(3.60918509199994,12.2,0.338242477999984));
#301011=CARTESIAN_POINT('Origin',(-5.66300478732629E-14,12.2,-1.77635683940025E-14));
#301012=CARTESIAN_POINT('',(3.97632131980427,12.2,0.372649332160937));
#301013=CARTESIAN_POINT('',(3.60918509199994,12.2,0.338242477999984));
#301014=CARTESIAN_POINT('',(4.74889012999994,12.2,0.102676828999986));
#301015=CARTESIAN_POINT('Ctrl Pts',(3.97632132878368,12.2,0.372649232070297));
#301016=CARTESIAN_POINT('Ctrl Pts',(3.97659156631608,12.2,0.372673475831972));
#301017=CARTESIAN_POINT('Ctrl Pts',(3.97686215349336,12.1999999999997,0.372693740160113));
#301018=CARTESIAN_POINT('Ctrl Pts',(3.97770753758359,12.1999999999997,0.372755234620468));
#301019=CARTESIAN_POINT('Ctrl Pts',(3.97831516441626,12.2,0.372793558096753));
#301020=CARTESIAN_POINT('Ctrl Pts',(3.98096065091767,12.2,0.372944703878524));
#301021=CARTESIAN_POINT('Ctrl Pts',(3.98315053462491,12.1999999999078,0.373027030774091));
#301022=CARTESIAN_POINT('Ctrl Pts',(3.99275999528421,12.1999999999078,0.373280365470712));
#301023=CARTESIAN_POINT('Ctrl Pts',(4.00080741751491,12.1999999999078,0.373184467362426));
#301024=CARTESIAN_POINT('Ctrl Pts',(4.03581303640557,12.1999999999078,0.372007587291399));
#301025=CARTESIAN_POINT('Ctrl Pts',(4.06496098547899,12.2,0.368878531427779));
#301026=CARTESIAN_POINT('Ctrl Pts',(4.16957554102918,12.2,0.353234892688601));
#301027=CARTESIAN_POINT('Ctrl Pts',(4.26641642627047,12.2,0.329317758609609));
#301028=CARTESIAN_POINT('Ctrl Pts',(4.5068681474629,12.2,0.238257898338845));
#301029=CARTESIAN_POINT('Ctrl Pts',(4.63107293515098,12.2,0.174983763566832));
#301030=CARTESIAN_POINT('Ctrl Pts',(4.74889012955414,12.2,0.102676828273587));
#301031=CARTESIAN_POINT('',(4.74421990499994,12.2,-0.234259451000014));
#301032=CARTESIAN_POINT('Origin',(-5.66300478732629E-14,12.2,-1.77635683940025E-14));
#301033=CARTESIAN_POINT('',(3.9644482997684,12.2,-0.482713394198715));
#301034=CARTESIAN_POINT('Ctrl Pts',(4.74421990499994,12.2,-0.234259451000014));
#301035=CARTESIAN_POINT('Ctrl Pts',(4.71280838274439,12.2,-0.252358422706553));
#301036=CARTESIAN_POINT('Ctrl Pts',(4.68182628481682,12.2,-0.269325626376228));
#301037=CARTESIAN_POINT('Ctrl Pts',(4.65136663428666,12.2,-0.285188901941369));
#301038=CARTESIAN_POINT('Ctrl Pts',(4.60376418654431,12.2,-0.309980084143681));
#301039=CARTESIAN_POINT('Ctrl Pts',(4.55743821394982,12.2,-0.33207332577565));
#301040=CARTESIAN_POINT('Ctrl Pts',(4.51276566604218,12.2,-0.351611995871092));
#301041=CARTESIAN_POINT('Ctrl Pts',(4.46966970825717,12.2,-0.370461104351526));
#301042=CARTESIAN_POINT('Ctrl Pts',(4.42811254063867,12.2,-0.386932586665946));
#301043=CARTESIAN_POINT('Ctrl Pts',(4.38844978019863,12.2,-0.40119795231803));
#301044=CARTESIAN_POINT('Ctrl Pts',(4.35014417590209,12.2,-0.414975194389727));
#301045=CARTESIAN_POINT('Ctrl Pts',(4.31360554684493,12.2,-0.426694489899858));
#301046=CARTESIAN_POINT('Ctrl Pts',(4.27917057492761,12.2,-0.436554070185109));
#301047=CARTESIAN_POINT('Ctrl Pts',(4.24599813772591,12.2,-0.446052155696343));
#301048=CARTESIAN_POINT('Ctrl Pts',(4.21477788342143,12.2,-0.453824144641168));
#301049=CARTESIAN_POINT('Ctrl Pts',(4.18582653151251,12.2,-0.460092073302094));
#301050=CARTESIAN_POINT('Ctrl Pts',(4.15829129016377,12.2,-0.466053415935704));
#301051=CARTESIAN_POINT('Ctrl Pts',(4.13280837037226,12.2,-0.470654038415366));
#301052=CARTESIAN_POINT('Ctrl Pts',(4.10966513089301,12.2,-0.474129271609313));
#301053=CARTESIAN_POINT('Ctrl Pts',(4.08747104362572,12.2,-0.477461978288073));
#301054=CARTESIAN_POINT('Ctrl Pts',(4.06742854151838,12.2,-0.47975942539362));
#301055=CARTESIAN_POINT('Ctrl Pts',(4.04980584225301,12.2,-0.48127457959937));
#301056=CARTESIAN_POINT('Ctrl Pts',(4.03332992873515,12.2,-0.482691136125943));
#301057=CARTESIAN_POINT('Ctrl Pts',(4.01896907893941,12.2,-0.483423742151229));
#301058=CARTESIAN_POINT('Ctrl Pts',(4.00695638984246,12.2,-0.483722451718041));
#301059=CARTESIAN_POINT('Ctrl Pts',(3.99549310337372,12.2,-0.484007499745812));
#301060=CARTESIAN_POINT('Ctrl Pts',(3.98616799207043,12.2,-0.483897081035411));
#301061=CARTESIAN_POINT('Ctrl Pts',(3.97919795030351,12.2,-0.483652861953002));
#301062=CARTESIAN_POINT('Ctrl Pts',(3.97461628623507,12.2,-0.483492327793793));
#301063=CARTESIAN_POINT('Ctrl Pts',(3.97105251234585,12.2,-0.483274855533071));
#301064=CARTESIAN_POINT('Ctrl Pts',(3.96857238495118,12.2,-0.483087409556649));
#301065=CARTESIAN_POINT('Ctrl Pts',(3.96733232125385,12.2,-0.482993686568438));
#301066=CARTESIAN_POINT('Ctrl Pts',(3.96636321862757,12.2,-0.482907633051564));
#301067=CARTESIAN_POINT('Ctrl Pts',(3.96567368282888,12.2,-0.482841249840966));
#301068=CARTESIAN_POINT('Ctrl Pts',(3.96532891492954,12.2,-0.482808058235667));
#301069=CARTESIAN_POINT('Ctrl Pts',(3.965054037478,12.2,-0.482779787357501));
#301070=CARTESIAN_POINT('Ctrl Pts',(3.96485014744288,12.2,-0.48275801329454));
#301071=CARTESIAN_POINT('Ctrl Pts',(3.96472015919018,12.2,-0.482744131437113));
#301072=CARTESIAN_POINT('Ctrl Pts',(3.96461946383355,12.2,-0.482732997352684));
#301073=CARTESIAN_POINT('Ctrl Pts',(3.96454657132337,12.2,-0.482724755568015));
#301074=CARTESIAN_POINT('Ctrl Pts',(3.96450512999067,12.2,-0.482720069894005));
#301075=CARTESIAN_POINT('Ctrl Pts',(3.96447771970708,12.2,-0.482716794149493));
#301076=CARTESIAN_POINT('Ctrl Pts',(3.96444835997019,12.2,-0.482713334252444));
#301077=CARTESIAN_POINT('',(3.5984236820905,12.2,-0.438146098542558));
#301078=CARTESIAN_POINT('',(3.96444830899994,12.2,-0.482713328000015));
#301079=CARTESIAN_POINT('',(3.48765214499994,12.2,-0.988386318000014));
#301080=CARTESIAN_POINT('Origin',(-5.66300478732629E-14,12.2,-1.77635683940025E-14));
#301081=CARTESIAN_POINT('',(3.84242567103147,12.2,-1.0889277859801));
#301082=CARTESIAN_POINT('',(3.48765214499994,12.2,-0.988386318000014));
#301083=CARTESIAN_POINT('',(4.46529931499995,12.2,-1.61975369200002));
#301084=CARTESIAN_POINT('Ctrl Pts',(3.84242564315659,12.2,-1.088927883045));
#301085=CARTESIAN_POINT('Ctrl Pts',(3.84268642756792,12.2,-1.0890027745344));
#301086=CARTESIAN_POINT('Ctrl Pts',(3.84294603075642,12.1999999999997,-1.089081747968));
#301087=CARTESIAN_POINT('Ctrl Pts',(3.84375517486719,12.1999999999997,-1.08932937765328));
#301088=CARTESIAN_POINT('Ctrl Pts',(3.84433532277453,12.2,-1.08951302470086));
#301089=CARTESIAN_POINT('Ctrl Pts',(3.84685853713855,12.2,-1.09032831431401));
#301090=CARTESIAN_POINT('Ctrl Pts',(3.84893005724474,12.1999999999081,-1.09104255104995));
#301091=CARTESIAN_POINT('Ctrl Pts',(3.85798372485354,12.1999999999081,-1.09427822963628));
#301092=CARTESIAN_POINT('Ctrl Pts',(3.86545613666242,12.1999999999081,-1.09727610859554));
#301093=CARTESIAN_POINT('Ctrl Pts',(3.89766100957131,12.1999999999081,-1.111014062726));
#301094=CARTESIAN_POINT('Ctrl Pts',(3.92371080997547,12.2,-1.12446042846844));
#301095=CARTESIAN_POINT('Ctrl Pts',(4.01543103001572,12.2,-1.17673704252015));
#301096=CARTESIAN_POINT('Ctrl Pts',(4.09709048001922,12.2,-1.2339590057417));
#301097=CARTESIAN_POINT('Ctrl Pts',(4.28857034295747,12.2,-1.40587505111375));
#301098=CARTESIAN_POINT('Ctrl Pts',(4.38130822209624,12.2,-1.50944072497096));
#301099=CARTESIAN_POINT('Ctrl Pts',(4.46529931499995,12.2,-1.61975369200002));
#301100=CARTESIAN_POINT('',(4.33922903699994,12.2,-1.93225033600001));
#301101=CARTESIAN_POINT('Origin',(-5.66300478732629E-14,12.2,-1.77635683940025E-14));
#301102=CARTESIAN_POINT('',(3.52236175392628,12.2,-1.88224074466015));
#301103=CARTESIAN_POINT('Ctrl Pts',(4.33922903699994,12.2,-1.93225033600001));
#301104=CARTESIAN_POINT('Ctrl Pts',(4.29900656514174,12.2,-1.93845813259177));
#301105=CARTESIAN_POINT('Ctrl Pts',(4.25980390494279,12.2,-1.94353103969836));
#301106=CARTESIAN_POINT('Ctrl Pts',(4.22172995537545,12.2,-1.94755436125775));
#301107=CARTESIAN_POINT('Ctrl Pts',(4.16871119947665,12.2,-1.95315691907179));
#301108=CARTESIAN_POINT('Ctrl Pts',(4.11788223931045,12.2,-1.9567229568601));
#301109=CARTESIAN_POINT('Ctrl Pts',(4.06954307521643,12.2,-1.95852644618014));
#301110=CARTESIAN_POINT('Ctrl Pts',(4.02325836860018,12.2,-1.96025328559965));
#301111=CARTESIAN_POINT('Ctrl Pts',(3.97925644296878,12.2,-1.96036409029778));
#301112=CARTESIAN_POINT('Ctrl Pts',(3.93780116827124,12.2,-1.95914487990857));
#301113=CARTESIAN_POINT('Ctrl Pts',(3.89739186390891,12.2,-1.95795643177842));
#301114=CARTESIAN_POINT('Ctrl Pts',(3.8594024213275,12.2,-1.95550391043724));
#301115=CARTESIAN_POINT('Ctrl Pts',(3.82407655579394,12.2,-1.95209965533137));
#301116=CARTESIAN_POINT('Ctrl Pts',(3.78997061682712,12.2,-1.94881296114527));
#301117=CARTESIAN_POINT('Ctrl Pts',(3.75834756381887,12.2,-1.94463885468989));
#301118=CARTESIAN_POINT('Ctrl Pts',(3.72942509982425,12.2,-1.9399073151758));
#301119=CARTESIAN_POINT('Ctrl Pts',(3.70208784783339,12.2,-1.9354351067213));
#301120=CARTESIAN_POINT('Ctrl Pts',(3.67716330263961,12.2,-1.93046473194123));
#301121=CARTESIAN_POINT('Ctrl Pts',(3.65483308074296,12.2,-1.92532209267641));
#301122=CARTESIAN_POINT('Ctrl Pts',(3.63387548666265,12.2,-1.92049556893149));
#301123=CARTESIAN_POINT('Ctrl Pts',(3.61520310657084,12.2,-1.91551717163214));
#301124=CARTESIAN_POINT('Ctrl Pts',(3.59896359240005,12.2,-1.91070096211013));
#301125=CARTESIAN_POINT('Ctrl Pts',(3.58357139066594,12.2,-1.9061360430013));
#301126=CARTESIAN_POINT('Ctrl Pts',(3.57036483791297,12.2,-1.90171657509177));
#301127=CARTESIAN_POINT('Ctrl Pts',(3.55946707966078,12.2,-1.89775407406141));
#301128=CARTESIAN_POINT('Ctrl Pts',(3.54893209458809,12.2,-1.89392347989339));
#301129=CARTESIAN_POINT('Ctrl Pts',(3.54055478815737,12.2,-1.89051943439848));
#301130=CARTESIAN_POINT('Ctrl Pts',(3.53444369477347,12.2,-1.88787100387636));
#301131=CARTESIAN_POINT('Ctrl Pts',(3.53065572913985,12.2,-1.88622937231052));
#301132=CARTESIAN_POINT('Ctrl Pts',(3.52773843948522,12.2,-1.88487898787886));
#301133=CARTESIAN_POINT('Ctrl Pts',(3.52571707879089,12.2,-1.88390942517561));
#301134=CARTESIAN_POINT('Ctrl Pts',(3.52470639844372,12.2,-1.88342464382399));
#301135=CARTESIAN_POINT('Ctrl Pts',(3.52391969356645,12.2,-1.88303518981985));
#301136=CARTESIAN_POINT('Ctrl Pts',(3.52336008261798,12.2,-1.88275326165307));
#301137=CARTESIAN_POINT('Ctrl Pts',(3.52308027714375,12.2,-1.88261229756968));
#301138=CARTESIAN_POINT('Ctrl Pts',(3.52285723827716,12.2,-1.88249818746355));
#301139=CARTESIAN_POINT('Ctrl Pts',(3.52269136250471,12.2,-1.88241256318214));
#301140=CARTESIAN_POINT('Ctrl Pts',(3.52258193395062,12.2,-1.88235607668522));
#301141=CARTESIAN_POINT('Ctrl Pts',(3.52249703884443,12.2,-1.88231188564555));
#301142=CARTESIAN_POINT('Ctrl Pts',(3.52243726950848,12.2,-1.88228053212193));
#301143=CARTESIAN_POINT('Ctrl Pts',(3.52240643831652,12.2,-1.88226435883692));
#301144=CARTESIAN_POINT('Ctrl Pts',(3.5223850376344,12.2,-1.88225299025455));
#301145=CARTESIAN_POINT('Ctrl Pts',(3.52236183191156,12.2,-1.88224071016707));
#301146=CARTESIAN_POINT('',(3.19715352623975,12.2,-1.70845963654418));
#301147=CARTESIAN_POINT('',(3.52236178599994,12.2,-1.88224068600002));
#301148=CARTESIAN_POINT('',(2.89509245023569,12.2,-2.18152806526552));
#301149=CARTESIAN_POINT('Origin',(-5.66300478732629E-14,12.2,-1.77635683940025E-14));
#301150=CARTESIAN_POINT('',(3.1895891437794,12.2,-2.40343917166473));
#301151=CARTESIAN_POINT('',(2.89509244999994,12.2,-2.18152806500001));
#301152=CARTESIAN_POINT('',(3.57864508499994,12.2,-3.12342750100001));
#301153=CARTESIAN_POINT('Ctrl Pts',(3.18958908299994,12.2,-2.40343925200001));
#301154=CARTESIAN_POINT('Ctrl Pts',(3.18972664483265,12.2,-2.40354363799686));
#301155=CARTESIAN_POINT('Ctrl Pts',(3.19053877007493,12.2,-2.40417145281639));
#301156=CARTESIAN_POINT('Ctrl Pts',(3.19321480642603,12.2,-2.40634490153556));
#301157=CARTESIAN_POINT('Ctrl Pts',(3.19488796455418,12.1999999999079,-2.40775871102333));
#301158=CARTESIAN_POINT('Ctrl Pts',(3.20216212621672,12.1999999999079,-2.41404710203839));
#301159=CARTESIAN_POINT('Ctrl Pts',(3.20804455305006,12.1999999999079,-2.41953932649126));
#301160=CARTESIAN_POINT('Ctrl Pts',(3.23312051415152,12.1999999999079,-2.44399161344329));
#301161=CARTESIAN_POINT('Ctrl Pts',(3.25255277588417,12.2,-2.46594012204941));
#301162=CARTESIAN_POINT('Ctrl Pts',(3.31934274303239,12.2,-2.54800138031337));
#301163=CARTESIAN_POINT('Ctrl Pts',(3.37479477908212,12.2,-2.63092698918229));
#301164=CARTESIAN_POINT('Ctrl Pts',(3.49112749819354,12.2,-2.86017974548445));
#301165=CARTESIAN_POINT('Ctrl Pts',(3.54028648814989,12.2,-2.99060729942287));
#301166=CARTESIAN_POINT('Ctrl Pts',(3.57864508499994,12.2,-3.12342750100001));
#301167=CARTESIAN_POINT('',(3.34820124399994,12.2,-3.36928010500001));
#301168=CARTESIAN_POINT('Origin',(-5.66300478732629E-14,12.2,-1.77635683940025E-14));
#301169=CARTESIAN_POINT('',(2.60456073403712,12.2,-3.02756105307893));
#301170=CARTESIAN_POINT('Ctrl Pts',(3.34820124399994,12.2,-3.36928010500001));
#301171=CARTESIAN_POINT('Ctrl Pts',(3.31610338031493,12.2,-3.36222132135304));
#301172=CARTESIAN_POINT('Ctrl Pts',(3.28489316543702,12.2,-3.35471299742094));
#301173=CARTESIAN_POINT('Ctrl Pts',(3.25460746644452,12.2,-3.34681680642958));
#301174=CARTESIAN_POINT('Ctrl Pts',(3.20231260989431,12.2,-3.33318231262812));
#301175=CARTESIAN_POINT('Ctrl Pts',(3.15277628079259,12.2,-3.31839009953227));
#301176=CARTESIAN_POINT('Ctrl Pts',(3.10618228623555,12.2,-3.30279915010095));
#301177=CARTESIAN_POINT('Ctrl Pts',(3.06109729991451,12.2,-3.28771313422004));
#301178=CARTESIAN_POINT('Ctrl Pts',(3.01876729021624,12.2000000000001,-3.27187911778594));
#301179=CARTESIAN_POINT('Ctrl Pts',(2.97934262927457,12.2,-3.2556658918671));
#301180=CARTESIAN_POINT('Ctrl Pts',(2.94147455473056,12.1999999999999,-3.2400928055544));
#301181=CARTESIAN_POINT('Ctrl Pts',(2.90628704421913,12.2,-3.22416976229994));
#301182=CARTESIAN_POINT('Ctrl Pts',(2.87389618604026,12.2,-3.20826646750966));
#301183=CARTESIAN_POINT('Ctrl Pts',(2.84258537401118,12.2,-3.19289345481974));
#301184=CARTESIAN_POINT('Ctrl Pts',(2.81388796074758,12.2,-3.17753868749481));
#301185=CARTESIAN_POINT('Ctrl Pts',(2.78789027600534,12.2,-3.16257980667675));
#301186=CARTESIAN_POINT('Ctrl Pts',(2.76293364575501,12.2,-3.14821994112579));
#301187=CARTESIAN_POINT('Ctrl Pts',(2.74046502013137,12.1999999999999,-3.13422463962054));
#301188=CARTESIAN_POINT('Ctrl Pts',(2.72054127763874,12.2,-3.12097215534773));
#301189=CARTESIAN_POINT('Ctrl Pts',(2.70141897153072,12.2000000000001,-3.1082527548109));
#301190=CARTESIAN_POINT('Ctrl Pts',(2.68464109606858,12.2,-3.0962173287529));
#301191=CARTESIAN_POINT('Ctrl Pts',(2.67023747516043,12.2,-3.08524559523614));
#301192=CARTESIAN_POINT('Ctrl Pts',(2.65700458237695,12.2,-3.0751656456039));
#301193=CARTESIAN_POINT('Ctrl Pts',(2.64577568833732,12.2,-3.06598350134236));
#301194=CARTESIAN_POINT('Ctrl Pts',(2.63655542330602,12.2,-3.05803422841789));
#301195=CARTESIAN_POINT('Ctrl Pts',(2.6277125659735,12.2,-3.050410338418));
#301196=CARTESIAN_POINT('Ctrl Pts',(2.62071741312198,12.2,-3.04392007669833));
#301197=CARTESIAN_POINT('Ctrl Pts',(2.61555497849679,12.2,-3.03890099424192));
#301198=CARTESIAN_POINT('Ctrl Pts',(2.61203910333727,12.2,-3.03548274905079));
#301199=CARTESIAN_POINT('Ctrl Pts',(2.60937292520829,12.2,-3.032747694406));
#301200=CARTESIAN_POINT('Ctrl Pts',(2.60754559550129,12.2,-3.03081602249089));
#301201=CARTESIAN_POINT('Ctrl Pts',(2.60663193064778,12.2,-3.02985018653334));
#301202=CARTESIAN_POINT('Ctrl Pts',(2.6059279015729,12.2,-3.02908537937573));
#301203=CARTESIAN_POINT('Ctrl Pts',(2.60543160098027,12.2,-3.02853785707786));
#301204=CARTESIAN_POINT('Ctrl Pts',(2.60518345068395,12.2,-3.02826409592892));
#301205=CARTESIAN_POINT('Ctrl Pts',(2.60498722709952,12.2,-3.02804467705542));
#301206=CARTESIAN_POINT('Ctrl Pts',(2.60484265807629,12.2,-3.02788168440645));
#301207=CARTESIAN_POINT('Ctrl Pts',(2.60475225973617,12.2,-3.02777976585854));
#301208=CARTESIAN_POINT('Ctrl Pts',(2.60468246168515,12.2,-3.02770047411044));
#301209=CARTESIAN_POINT('Ctrl Pts',(2.60463169836712,12.2,-3.02764248669049));
#301210=CARTESIAN_POINT('Ctrl Pts',(2.60460127874204,12.2,-3.02760773806407));
#301211=CARTESIAN_POINT('Ctrl Pts',(2.60458156576711,12.2,-3.0275849736035));
#301212=CARTESIAN_POINT('Ctrl Pts',(2.60456081971581,12.2,-3.02756104824639));
#301213=CARTESIAN_POINT('',(2.36409006999994,12.2,-2.74803623300001));
#301214=CARTESIAN_POINT('',(2.60456078499995,12.2,-3.02756100900002));
#301215=CARTESIAN_POINT('',(1.91153447899994,12.2,-3.08004235900002));
#301216=CARTESIAN_POINT('Origin',(-5.66300478732629E-14,12.2,-1.77635683940025E-14));
#301217=CARTESIAN_POINT('',(2.10598092973928,12.2,-3.39335277979123));
#301218=CARTESIAN_POINT('',(1.91153447899994,12.2,-3.08004235900002));
#301219=CARTESIAN_POINT('',(2.20867500599994,12.2,-4.20526511800002));
#301220=CARTESIAN_POINT('Ctrl Pts',(2.10598084399995,12.2,-3.39335283300001));
#301221=CARTESIAN_POINT('Ctrl Pts',(2.10612311054997,12.2,-3.39358400226231));
#301222=CARTESIAN_POINT('Ctrl Pts',(2.10626187270212,12.1999999999997,-3.39381731953339));
#301223=CARTESIAN_POINT('Ctrl Pts',(2.10669328388901,12.1999999999997,-3.39454590594761));
#301224=CARTESIAN_POINT('Ctrl Pts',(2.10699833127559,12.2,-3.39507253151456));
#301225=CARTESIAN_POINT('Ctrl Pts',(2.1083141818034,12.2,-3.39737572880188));
#301226=CARTESIAN_POINT('Ctrl Pts',(2.10936495438345,12.199999999924,-3.39930115367447));
#301227=CARTESIAN_POINT('Ctrl Pts',(2.11387550924077,12.199999999924,-3.40779148964373));
#301228=CARTESIAN_POINT('Ctrl Pts',(2.11737859461051,12.199999999924,-3.41504199950801));
#301229=CARTESIAN_POINT('Ctrl Pts',(2.13193416739489,12.199999999924,-3.44691753809593));
#301230=CARTESIAN_POINT('Ctrl Pts',(2.14212952196091,12.2,-3.47441825103592));
#301231=CARTESIAN_POINT('Ctrl Pts',(2.17477097005074,12.2,-3.57510296880395));
#301232=CARTESIAN_POINT('Ctrl Pts',(2.19652755494506,12.2,-3.67250735829484));
#301233=CARTESIAN_POINT('Ctrl Pts',(2.2221638801155,12.2,-3.92833258330708));
#301234=CARTESIAN_POINT('Ctrl Pts',(2.22086610698297,12.2,-4.06779136454917));
#301235=CARTESIAN_POINT('Ctrl Pts',(2.20867500608793,12.2,-4.20526511800782));
#301236=CARTESIAN_POINT('',(1.90498031899994,12.2,-4.35126992700001));
#301237=CARTESIAN_POINT('Origin',(-5.66300478732629E-14,12.2,-1.77635683940025E-14));
#301238=CARTESIAN_POINT('Ctrl Pts',(1.90498031853915,12.2,-4.3512699276941));
#301239=CARTESIAN_POINT('Ctrl Pts',(1.87731122367178,12.2,-4.33290102593718));
#301240=CARTESIAN_POINT('Ctrl Pts',(1.85065313309167,12.2,-4.31443155952546));
#301241=CARTESIAN_POINT('Ctrl Pts',(1.82501865469772,12.2,-4.29593456725834));
#301242=CARTESIAN_POINT('Ctrl Pts',(1.7814207545479,12.2,-4.26447576362908));
#301243=CARTESIAN_POINT('Ctrl Pts',(1.74078589202437,12.2,-4.23293703601144));
#301244=CARTESIAN_POINT('Ctrl Pts',(1.70315507361045,12.2,-4.20171407893944));
#301245=CARTESIAN_POINT('Ctrl Pts',(1.66677641164637,12.2,-4.17153005826926));
#301246=CARTESIAN_POINT('Ctrl Pts',(1.63320539722488,12.2000000000001,-4.14164105433643));
#301247=CARTESIAN_POINT('Ctrl Pts',(1.60244892133047,12.2,-4.11243861538496));
#301248=CARTESIAN_POINT('Ctrl Pts',(1.57273511323079,12.1999999999999,-4.08422616120049));
#301249=CARTESIAN_POINT('Ctrl Pts',(1.54564845580195,12.2,-4.0566544282747));
#301250=CARTESIAN_POINT('Ctrl Pts',(1.52116372005999,12.2,-4.03011018221668));
#301251=CARTESIAN_POINT('Ctrl Pts',(1.49762025163875,12.2,-4.004586377287));
#301252=CARTESIAN_POINT('Ctrl Pts',(1.47648269596018,12.2,-3.98001248487298));
#301253=CARTESIAN_POINT('Ctrl Pts',(1.45769623267052,12.2,-3.95676577818292));
#301254=CARTESIAN_POINT('Ctrl Pts',(1.43938836702436,12.2,-3.93411129680262));
#301255=CARTESIAN_POINT('Ctrl Pts',(1.42331361287325,12.1999999999999,-3.91271697766841));
#301256=CARTESIAN_POINT('Ctrl Pts',(1.40938606434272,12.2,-3.8929672821972));
#301257=CARTESIAN_POINT('Ctrl Pts',(1.39615307577568,12.2000000000001,-3.87420249428061));
#301258=CARTESIAN_POINT('Ctrl Pts',(1.38485861700844,12.2,-3.85692219250991));
#301259=CARTESIAN_POINT('Ctrl Pts',(1.37539340264988,12.2,-3.84149117465438));
#301260=CARTESIAN_POINT('Ctrl Pts',(1.36665980231613,12.2,-3.82725289778206));
#301261=CARTESIAN_POINT('Ctrl Pts',(1.3594835944762,12.2,-3.81458902219661));
#301262=CARTESIAN_POINT('Ctrl Pts',(1.35374651900545,12.2,-3.803817745772));
#301263=CARTESIAN_POINT('Ctrl Pts',(1.34830700444303,12.2,-3.79360513565971));
#301264=CARTESIAN_POINT('Ctrl Pts',(1.34416138735862,12.2,-3.78509367744774));
#301265=CARTESIAN_POINT('Ctrl Pts',(1.34117666537531,12.2,-3.7785860725486));
#301266=CARTESIAN_POINT('Ctrl Pts',(1.3391254676793,12.2,-3.77411383551939));
#301267=CARTESIAN_POINT('Ctrl Pts',(1.33762190934237,12.2,-3.77058860390923));
#301268=CARTESIAN_POINT('Ctrl Pts',(1.33661222385445,12.2,-3.76811909717029));
#301269=CARTESIAN_POINT('Ctrl Pts',(1.33610738111049,12.2,-3.76688434380082));
#301270=CARTESIAN_POINT('Ctrl Pts',(1.33572585904822,12.2,-3.76591366201497));
#301271=CARTESIAN_POINT('Ctrl Pts',(1.33545997377132,12.2,-3.76522160098899));
#301272=CARTESIAN_POINT('Ctrl Pts',(1.33532703113287,12.2,-3.764875570476));
#301273=CARTESIAN_POINT('Ctrl Pts',(1.33522298535505,12.2,-3.76459921215659));
#301274=CARTESIAN_POINT('Ctrl Pts',(1.33514682354475,12.2,-3.7643943808242));
#301275=CARTESIAN_POINT('Ctrl Pts',(1.33509927145191,12.2,-3.76426649312701));
#301276=CARTESIAN_POINT('Ctrl Pts',(1.33506277162764,12.2,-3.76416716393628));
#301277=CARTESIAN_POINT('Ctrl Pts',(1.33503630943865,12.2,-3.76409459607695));
#301278=CARTESIAN_POINT('Ctrl Pts',(1.3350203884622,12.2,-3.76405093562315));
#301279=CARTESIAN_POINT('Ctrl Pts',(1.33501018614367,12.2,-3.76402242543819));
#301280=CARTESIAN_POINT('Ctrl Pts',(1.33499943628452,12.2,-3.76399249025695));
#301281=CARTESIAN_POINT('',(-3.28892417320473,12.2,-1.19707050039253));
#301282=CARTESIAN_POINT('Origin',(-5.66300478732629E-14,12.2,-1.77635683940025E-14));
#301283=CARTESIAN_POINT('Origin',(-5.66300478732629E-14,5.2,-1.77635683940025E-14));
#301284=CARTESIAN_POINT('',(0.235377287932295,2.4,-2.99075200114047));
#301285=CARTESIAN_POINT('Origin',(-5.66300478732629E-14,2.4,-1.81064694828012E-14));
#301286=CARTESIAN_POINT('',(0.235377287932295,2.7,-2.99075200114047));
#301287=CARTESIAN_POINT('',(0.235377287932296,5.2,-2.99075200114047));
#301288=CARTESIAN_POINT('Origin',(-5.66300478732629E-14,2.7,-1.80697300804299E-14));
#301289=CARTESIAN_POINT('Origin',(-5.66300478732629E-14,2.4,-1.77268289916312E-14));
#301290=CARTESIAN_POINT('Origin',(-5.66300478732629E-14,15.2,-1.77635683940025E-14));
#301291=CARTESIAN_POINT('',(-1.39835267900006,2.7,4.53950545599999));
#301292=CARTESIAN_POINT('',(-1.39835267900006,12.2,4.53950545599999));
#301293=CARTESIAN_POINT('',(-1.07300065800006,2.7,4.62722050399999));
#301294=CARTESIAN_POINT('Origin',(-5.66300478732629E-14,2.7,-1.92943768261394E-14));
#301295=CARTESIAN_POINT('',(-1.07300065800006,12.2,4.62722050399999));
#301296=CARTESIAN_POINT('Ctrl Pts',(-1.39835267900006,12.2,4.53950545599999));
#301297=CARTESIAN_POINT('Ctrl Pts',(-1.39835267900006,5.2,4.53950545599999));
#301298=CARTESIAN_POINT('Ctrl Pts',(-1.39835267900006,2.2,4.53950545599999));
#301299=CARTESIAN_POINT('Ctrl Pts',(-1.39849651400006,12.2,4.53899223499998));
#301300=CARTESIAN_POINT('Ctrl Pts',(-1.39849651400006,5.2,4.53899223499998));
#301301=CARTESIAN_POINT('Ctrl Pts',(-1.39849651400006,2.2,4.53899223499998));
#301302=CARTESIAN_POINT('Ctrl Pts',(-1.39878382700006,12.2,4.53796604699999));
#301303=CARTESIAN_POINT('Ctrl Pts',(-1.39878382700006,5.2,4.53796604699999));
#301304=CARTESIAN_POINT('Ctrl Pts',(-1.39878382700006,2.2,4.53796604699999));
#301305=CARTESIAN_POINT('Ctrl Pts',(-1.39921373200006,12.2,4.53642752199999));
#301306=CARTESIAN_POINT('Ctrl Pts',(-1.39921373200006,5.2,4.53642752199999));
#301307=CARTESIAN_POINT('Ctrl Pts',(-1.39921373200006,2.2,4.53642752199999));
#301308=CARTESIAN_POINT('Ctrl Pts',(-1.39978480400006,12.2,4.53437767499998));
#301309=CARTESIAN_POINT('Ctrl Pts',(-1.39978480400006,5.2,4.53437767499998));
#301310=CARTESIAN_POINT('Ctrl Pts',(-1.39978480400006,2.2,4.53437767499998));
#301311=CARTESIAN_POINT('Ctrl Pts',(-1.40049509300006,12.2,4.53181789599999));
#301312=CARTESIAN_POINT('Ctrl Pts',(-1.40049509300006,5.2,4.53181789599999));
#301313=CARTESIAN_POINT('Ctrl Pts',(-1.40049509300006,2.2,4.53181789599999));
#301314=CARTESIAN_POINT('Ctrl Pts',(-1.40120182900006,12.2,4.52926064799998));
#301315=CARTESIAN_POINT('Ctrl Pts',(-1.40120182900006,5.2,4.52926064799998));
#301316=CARTESIAN_POINT('Ctrl Pts',(-1.40120182900006,2.2,4.52926064799998));
#301317=CARTESIAN_POINT('Ctrl Pts',(-1.40190501200006,12.2,4.52670593299998));
#301318=CARTESIAN_POINT('Ctrl Pts',(-1.40190501200006,5.2,4.52670593299998));
#301319=CARTESIAN_POINT('Ctrl Pts',(-1.40190501200006,2.2,4.52670593299998));
#301320=CARTESIAN_POINT('Ctrl Pts',(-1.40260464700006,12.2,4.52415375599998));
#301321=CARTESIAN_POINT('Ctrl Pts',(-1.40260464700006,5.2,4.52415375599998));
#301322=CARTESIAN_POINT('Ctrl Pts',(-1.40260464700006,2.2,4.52415375599998));
#301323=CARTESIAN_POINT('Ctrl Pts',(-1.40330073300006,12.2,4.52160412099998));
#301324=CARTESIAN_POINT('Ctrl Pts',(-1.40330073300006,5.2,4.52160412099998));
#301325=CARTESIAN_POINT('Ctrl Pts',(-1.40330073300006,2.2,4.52160412099998));
#301326=CARTESIAN_POINT('Ctrl Pts',(-1.40399327800006,12.2,4.51905703499998));
#301327=CARTESIAN_POINT('Ctrl Pts',(-1.40399327800006,5.2,4.51905703499998));
#301328=CARTESIAN_POINT('Ctrl Pts',(-1.40399327800006,2.2,4.51905703499998));
#301329=CARTESIAN_POINT('Ctrl Pts',(-1.40468228400006,12.2,4.51651250799999));
#301330=CARTESIAN_POINT('Ctrl Pts',(-1.40468228400006,5.2,4.51651250799999));
#301331=CARTESIAN_POINT('Ctrl Pts',(-1.40468228400006,2.2,4.51651250799999));
#301332=CARTESIAN_POINT('Ctrl Pts',(-1.40536775800006,12.2,4.51397054699999));
#301333=CARTESIAN_POINT('Ctrl Pts',(-1.40536775800006,5.2,4.51397054699999));
#301334=CARTESIAN_POINT('Ctrl Pts',(-1.40536775800006,2.2,4.51397054699999));
#301335=CARTESIAN_POINT('Ctrl Pts',(-1.40604970300006,12.2,4.51143116199999));
#301336=CARTESIAN_POINT('Ctrl Pts',(-1.40604970300006,5.2,4.51143116199999));
#301337=CARTESIAN_POINT('Ctrl Pts',(-1.40604970300006,2.2,4.51143116199999));
#301338=CARTESIAN_POINT('Ctrl Pts',(-1.40672812800006,12.2,4.50889436399999));
#301339=CARTESIAN_POINT('Ctrl Pts',(-1.40672812800006,5.2,4.50889436399999));
#301340=CARTESIAN_POINT('Ctrl Pts',(-1.40672812800006,2.2,4.50889436399999));
#301341=CARTESIAN_POINT('Ctrl Pts',(-1.40740303600006,12.2,4.50636015799999));
#301342=CARTESIAN_POINT('Ctrl Pts',(-1.40740303600006,5.2,4.50636015799999));
#301343=CARTESIAN_POINT('Ctrl Pts',(-1.40740303600006,2.2,4.50636015799999));
#301344=CARTESIAN_POINT('Ctrl Pts',(-1.40807443200006,12.2,4.50382855499999));
#301345=CARTESIAN_POINT('Ctrl Pts',(-1.40807443200006,5.2,4.50382855499999));
#301346=CARTESIAN_POINT('Ctrl Pts',(-1.40807443200006,2.2,4.50382855499999));
#301347=CARTESIAN_POINT('Ctrl Pts',(-1.40874231900006,12.2,4.50129955899998));
#301348=CARTESIAN_POINT('Ctrl Pts',(-1.40874231900006,5.2,4.50129955899998));
#301349=CARTESIAN_POINT('Ctrl Pts',(-1.40874231900006,2.2,4.50129955899998));
#301350=CARTESIAN_POINT('Ctrl Pts',(-1.40940670100006,12.2,4.49877317899999));
#301351=CARTESIAN_POINT('Ctrl Pts',(-1.40940670100006,5.2,4.49877317899999));
#301352=CARTESIAN_POINT('Ctrl Pts',(-1.40940670100006,2.2,4.49877317899999));
#301353=CARTESIAN_POINT('Ctrl Pts',(-1.41006758200006,12.2,4.49624941999998));
#301354=CARTESIAN_POINT('Ctrl Pts',(-1.41006758200006,5.2,4.49624941999998));
#301355=CARTESIAN_POINT('Ctrl Pts',(-1.41006758200006,2.2,4.49624941999998));
#301356=CARTESIAN_POINT('Ctrl Pts',(-1.41072496700006,12.2,4.49372828999999));
#301357=CARTESIAN_POINT('Ctrl Pts',(-1.41072496700006,5.2,4.49372828999999));
#301358=CARTESIAN_POINT('Ctrl Pts',(-1.41072496700006,2.2,4.49372828999999));
#301359=CARTESIAN_POINT('Ctrl Pts',(-1.41137886000006,12.2,4.49120979499998));
#301360=CARTESIAN_POINT('Ctrl Pts',(-1.41137886000006,5.2,4.49120979499998));
#301361=CARTESIAN_POINT('Ctrl Pts',(-1.41137886000006,2.2,4.49120979499998));
#301362=CARTESIAN_POINT('Ctrl Pts',(-1.41202926500006,12.2,4.48869394399999));
#301363=CARTESIAN_POINT('Ctrl Pts',(-1.41202926500006,5.2,4.48869394399999));
#301364=CARTESIAN_POINT('Ctrl Pts',(-1.41202926500006,2.2,4.48869394399999));
#301365=CARTESIAN_POINT('Ctrl Pts',(-1.41267618800006,12.2,4.48618074299999));
#301366=CARTESIAN_POINT('Ctrl Pts',(-1.41267618800006,5.2,4.48618074299999));
#301367=CARTESIAN_POINT('Ctrl Pts',(-1.41267618800006,2.2,4.48618074299999));
#301368=CARTESIAN_POINT('Ctrl Pts',(-1.41331963200006,12.2,4.48367020199999));
#301369=CARTESIAN_POINT('Ctrl Pts',(-1.41331963200006,5.2,4.48367020199999));
#301370=CARTESIAN_POINT('Ctrl Pts',(-1.41331963200006,2.2,4.48367020199999));
#301371=CARTESIAN_POINT('Ctrl Pts',(-1.41395960300006,12.2,4.48116232799999));
#301372=CARTESIAN_POINT('Ctrl Pts',(-1.41395960300006,5.2,4.48116232799999));
#301373=CARTESIAN_POINT('Ctrl Pts',(-1.41395960300006,2.2,4.48116232799999));
#301374=CARTESIAN_POINT('Ctrl Pts',(-1.41459610500006,12.2,4.47865712799998));
#301375=CARTESIAN_POINT('Ctrl Pts',(-1.41459610500006,5.2,4.47865712799998));
#301376=CARTESIAN_POINT('Ctrl Pts',(-1.41459610500006,2.2,4.47865712799998));
#301377=CARTESIAN_POINT('Ctrl Pts',(-1.41522914200006,12.2,4.47615460999998));
#301378=CARTESIAN_POINT('Ctrl Pts',(-1.41522914200006,5.2,4.47615460999998));
#301379=CARTESIAN_POINT('Ctrl Pts',(-1.41522914200006,2.2,4.47615460999998));
#301380=CARTESIAN_POINT('Ctrl Pts',(-1.41585872000006,12.2,4.47365478099999));
#301381=CARTESIAN_POINT('Ctrl Pts',(-1.41585872000006,5.2,4.47365478099999));
#301382=CARTESIAN_POINT('Ctrl Pts',(-1.41585872000006,2.2,4.47365478099999));
#301383=CARTESIAN_POINT('Ctrl Pts',(-1.41648484200006,12.2,4.47115764999998));
#301384=CARTESIAN_POINT('Ctrl Pts',(-1.41648484200006,5.2,4.47115764999998));
#301385=CARTESIAN_POINT('Ctrl Pts',(-1.41648484200006,2.2,4.47115764999998));
#301386=CARTESIAN_POINT('Ctrl Pts',(-1.41710751400006,12.2,4.46866322199998));
#301387=CARTESIAN_POINT('Ctrl Pts',(-1.41710751400006,5.2,4.46866322199998));
#301388=CARTESIAN_POINT('Ctrl Pts',(-1.41710751400006,2.2,4.46866322199998));
#301389=CARTESIAN_POINT('Ctrl Pts',(-1.41772673900006,12.2,4.46617150599998));
#301390=CARTESIAN_POINT('Ctrl Pts',(-1.41772673900006,5.2,4.46617150599998));
#301391=CARTESIAN_POINT('Ctrl Pts',(-1.41772673900006,2.2,4.46617150599998));
#301392=CARTESIAN_POINT('Ctrl Pts',(-1.41834252300006,12.2,4.46368250799999));
#301393=CARTESIAN_POINT('Ctrl Pts',(-1.41834252300006,5.2,4.46368250799999));
#301394=CARTESIAN_POINT('Ctrl Pts',(-1.41834252300006,2.2,4.46368250799999));
#301395=CARTESIAN_POINT('Ctrl Pts',(-1.41895486900006,12.2,4.46119623799999));
#301396=CARTESIAN_POINT('Ctrl Pts',(-1.41895486900006,5.2,4.46119623799999));
#301397=CARTESIAN_POINT('Ctrl Pts',(-1.41895486900006,2.2,4.46119623799999));
#301398=CARTESIAN_POINT('Ctrl Pts',(-1.41956378300006,12.2,4.45871269999999));
#301399=CARTESIAN_POINT('Ctrl Pts',(-1.41956378300006,5.2,4.45871269999999));
#301400=CARTESIAN_POINT('Ctrl Pts',(-1.41956378300006,2.2,4.45871269999999));
#301401=CARTESIAN_POINT('Ctrl Pts',(-1.42016927000006,12.2,4.45623190599999));
#301402=CARTESIAN_POINT('Ctrl Pts',(-1.42016927000006,5.2,4.45623190599999));
#301403=CARTESIAN_POINT('Ctrl Pts',(-1.42016927000006,2.2,4.45623190599999));
#301404=CARTESIAN_POINT('Ctrl Pts',(-1.42077133300006,12.2,4.45375385999998));
#301405=CARTESIAN_POINT('Ctrl Pts',(-1.42077133300006,5.2,4.45375385999998));
#301406=CARTESIAN_POINT('Ctrl Pts',(-1.42077133300006,2.2,4.45375385999998));
#301407=CARTESIAN_POINT('Ctrl Pts',(-1.42136997900006,12.2,4.45127857099998));
#301408=CARTESIAN_POINT('Ctrl Pts',(-1.42136997900006,5.2,4.45127857099998));
#301409=CARTESIAN_POINT('Ctrl Pts',(-1.42136997900006,2.2,4.45127857099998));
#301410=CARTESIAN_POINT('Ctrl Pts',(-1.42196521100006,12.2,4.44880604699998));
#301411=CARTESIAN_POINT('Ctrl Pts',(-1.42196521100006,5.2,4.44880604699998));
#301412=CARTESIAN_POINT('Ctrl Pts',(-1.42196521100006,2.2,4.44880604699998));
#301413=CARTESIAN_POINT('Ctrl Pts',(-1.42255703400005,12.2,4.44633629399998));
#301414=CARTESIAN_POINT('Ctrl Pts',(-1.42255703400005,5.2,4.44633629399998));
#301415=CARTESIAN_POINT('Ctrl Pts',(-1.42255703400005,2.2,4.44633629399998));
#301416=CARTESIAN_POINT('Ctrl Pts',(-1.42314545400006,12.2,4.44386931899999));
#301417=CARTESIAN_POINT('Ctrl Pts',(-1.42314545400006,5.2,4.44386931899999));
#301418=CARTESIAN_POINT('Ctrl Pts',(-1.42314545400006,2.2,4.44386931899999));
#301419=CARTESIAN_POINT('Ctrl Pts',(-1.42373047400006,12.2,4.44140513299998));
#301420=CARTESIAN_POINT('Ctrl Pts',(-1.42373047400006,5.2,4.44140513299998));
#301421=CARTESIAN_POINT('Ctrl Pts',(-1.42373047400006,2.2,4.44140513299998));
#301422=CARTESIAN_POINT('Ctrl Pts',(-1.42431210000006,12.2,4.43894374199999));
#301423=CARTESIAN_POINT('Ctrl Pts',(-1.42431210000006,5.2,4.43894374199999));
#301424=CARTESIAN_POINT('Ctrl Pts',(-1.42431210000006,2.2,4.43894374199999));
#301425=CARTESIAN_POINT('Ctrl Pts',(-1.42489033600006,12.2,4.43648515099999));
#301426=CARTESIAN_POINT('Ctrl Pts',(-1.42489033600006,5.2,4.43648515099999));
#301427=CARTESIAN_POINT('Ctrl Pts',(-1.42489033600006,2.2,4.43648515099999));
#301428=CARTESIAN_POINT('Ctrl Pts',(-1.42546518700006,12.2,4.43402936999998));
#301429=CARTESIAN_POINT('Ctrl Pts',(-1.42546518700006,5.2,4.43402936999998));
#301430=CARTESIAN_POINT('Ctrl Pts',(-1.42546518700006,2.2,4.43402936999998));
#301431=CARTESIAN_POINT('Ctrl Pts',(-1.42603665900006,12.2,4.43157640599999));
#301432=CARTESIAN_POINT('Ctrl Pts',(-1.42603665900006,5.2,4.43157640599999));
#301433=CARTESIAN_POINT('Ctrl Pts',(-1.42603665900006,2.2,4.43157640599999));
#301434=CARTESIAN_POINT('Ctrl Pts',(-1.42660475600006,12.2,4.42912626699999));
#301435=CARTESIAN_POINT('Ctrl Pts',(-1.42660475600006,5.2,4.42912626699999));
#301436=CARTESIAN_POINT('Ctrl Pts',(-1.42660475600006,2.2,4.42912626699999));
#301437=CARTESIAN_POINT('Ctrl Pts',(-1.42716948100006,12.2,4.42667895999998));
#301438=CARTESIAN_POINT('Ctrl Pts',(-1.42716948100006,5.2,4.42667895999998));
#301439=CARTESIAN_POINT('Ctrl Pts',(-1.42716948100006,2.2,4.42667895999998));
#301440=CARTESIAN_POINT('Ctrl Pts',(-1.42773084300006,12.2,4.42423449199998));
#301441=CARTESIAN_POINT('Ctrl Pts',(-1.42773084300006,5.2,4.42423449199998));
#301442=CARTESIAN_POINT('Ctrl Pts',(-1.42773084300006,2.2,4.42423449199998));
#301443=CARTESIAN_POINT('Ctrl Pts',(-1.42828884300006,12.2,4.42179287099999));
#301444=CARTESIAN_POINT('Ctrl Pts',(-1.42828884300006,5.2,4.42179287099999));
#301445=CARTESIAN_POINT('Ctrl Pts',(-1.42828884300006,2.2,4.42179287099999));
#301446=CARTESIAN_POINT('Ctrl Pts',(-1.42884348800006,12.2,4.41935410599999));
#301447=CARTESIAN_POINT('Ctrl Pts',(-1.42884348800006,5.2,4.41935410599999));
#301448=CARTESIAN_POINT('Ctrl Pts',(-1.42884348800006,2.2,4.41935410599999));
#301449=CARTESIAN_POINT('Ctrl Pts',(-1.42939478200006,12.2,4.41691820299998));
#301450=CARTESIAN_POINT('Ctrl Pts',(-1.42939478200006,5.2,4.41691820299998));
#301451=CARTESIAN_POINT('Ctrl Pts',(-1.42939478200006,2.2,4.41691820299998));
#301452=CARTESIAN_POINT('Ctrl Pts',(-1.42994273000006,12.2,4.41448516999999));
#301453=CARTESIAN_POINT('Ctrl Pts',(-1.42994273000006,5.2,4.41448516999999));
#301454=CARTESIAN_POINT('Ctrl Pts',(-1.42994273000006,2.2,4.41448516999999));
#301455=CARTESIAN_POINT('Ctrl Pts',(-1.43048733900006,12.2,4.41205501499999));
#301456=CARTESIAN_POINT('Ctrl Pts',(-1.43048733900006,5.2,4.41205501499999));
#301457=CARTESIAN_POINT('Ctrl Pts',(-1.43048733900006,2.2,4.41205501499999));
#301458=CARTESIAN_POINT('Ctrl Pts',(-1.43102861100005,12.2,4.40962774299998));
#301459=CARTESIAN_POINT('Ctrl Pts',(-1.43102861100005,5.2,4.40962774299998));
#301460=CARTESIAN_POINT('Ctrl Pts',(-1.43102861100005,2.2,4.40962774299998));
#301461=CARTESIAN_POINT('Ctrl Pts',(-1.43156655300006,12.2,4.40720336599998));
#301462=CARTESIAN_POINT('Ctrl Pts',(-1.43156655300006,5.2,4.40720336599998));
#301463=CARTESIAN_POINT('Ctrl Pts',(-1.43156655300006,2.2,4.40720336599998));
#301464=CARTESIAN_POINT('Ctrl Pts',(-1.43210116800006,12.2,4.40478188799998));
#301465=CARTESIAN_POINT('Ctrl Pts',(-1.43210116800006,5.2,4.40478188799998));
#301466=CARTESIAN_POINT('Ctrl Pts',(-1.43210116800006,2.2,4.40478188799998));
#301467=CARTESIAN_POINT('Ctrl Pts',(-1.43263246300006,12.2,4.40236331799999));
#301468=CARTESIAN_POINT('Ctrl Pts',(-1.43263246300006,5.2,4.40236331799999));
#301469=CARTESIAN_POINT('Ctrl Pts',(-1.43263246300006,2.2,4.40236331799999));
#301470=CARTESIAN_POINT('Ctrl Pts',(-1.43316044400006,12.2,4.39994766299999));
#301471=CARTESIAN_POINT('Ctrl Pts',(-1.43316044400006,5.2,4.39994766299999));
#301472=CARTESIAN_POINT('Ctrl Pts',(-1.43316044400006,2.2,4.39994766299999));
#301473=CARTESIAN_POINT('Ctrl Pts',(-1.43368511200006,12.2,4.39753493199999));
#301474=CARTESIAN_POINT('Ctrl Pts',(-1.43368511200006,5.2,4.39753493199999));
#301475=CARTESIAN_POINT('Ctrl Pts',(-1.43368511200006,2.2,4.39753493199999));
#301476=CARTESIAN_POINT('Ctrl Pts',(-1.43420647600006,12.2,4.39512513099999));
#301477=CARTESIAN_POINT('Ctrl Pts',(-1.43420647600006,5.2,4.39512513099999));
#301478=CARTESIAN_POINT('Ctrl Pts',(-1.43420647600006,2.2,4.39512513099999));
#301479=CARTESIAN_POINT('Ctrl Pts',(-1.43472454000006,12.2,4.39271826799998));
#301480=CARTESIAN_POINT('Ctrl Pts',(-1.43472454000006,5.2,4.39271826799998));
#301481=CARTESIAN_POINT('Ctrl Pts',(-1.43472454000006,2.2,4.39271826799998));
#301482=CARTESIAN_POINT('Ctrl Pts',(-1.43523930800006,12.2,4.39031435099999));
#301483=CARTESIAN_POINT('Ctrl Pts',(-1.43523930800006,5.2,4.39031435099999));
#301484=CARTESIAN_POINT('Ctrl Pts',(-1.43523930800006,2.2,4.39031435099999));
#301485=CARTESIAN_POINT('Ctrl Pts',(-1.43575078600006,12.2,4.38791338599999));
#301486=CARTESIAN_POINT('Ctrl Pts',(-1.43575078600006,5.2,4.38791338599999));
#301487=CARTESIAN_POINT('Ctrl Pts',(-1.43575078600006,2.2,4.38791338599999));
#301488=CARTESIAN_POINT('Ctrl Pts',(-1.43625898000006,12.2,4.38551538399999));
#301489=CARTESIAN_POINT('Ctrl Pts',(-1.43625898000006,5.2,4.38551538399999));
#301490=CARTESIAN_POINT('Ctrl Pts',(-1.43625898000006,2.2,4.38551538399999));
#301491=CARTESIAN_POINT('Ctrl Pts',(-1.43676389300005,12.2,4.38312034899998));
#301492=CARTESIAN_POINT('Ctrl Pts',(-1.43676389300005,5.2,4.38312034899998));
#301493=CARTESIAN_POINT('Ctrl Pts',(-1.43676389300005,2.2,4.38312034899998));
#301494=CARTESIAN_POINT('Ctrl Pts',(-1.43726553200006,12.2,4.38072828999999));
#301495=CARTESIAN_POINT('Ctrl Pts',(-1.43726553200006,5.2,4.38072828999999));
#301496=CARTESIAN_POINT('Ctrl Pts',(-1.43726553200006,2.2,4.38072828999999));
#301497=CARTESIAN_POINT('Ctrl Pts',(-1.43776390200006,12.2,4.37833921599999));
#301498=CARTESIAN_POINT('Ctrl Pts',(-1.43776390200006,5.2,4.37833921599999));
#301499=CARTESIAN_POINT('Ctrl Pts',(-1.43776390200006,2.2,4.37833921599999));
#301500=CARTESIAN_POINT('Ctrl Pts',(-1.43825900700006,12.2,4.37595313299998));
#301501=CARTESIAN_POINT('Ctrl Pts',(-1.43825900700006,5.2,4.37595313299998));
#301502=CARTESIAN_POINT('Ctrl Pts',(-1.43825900700006,2.2,4.37595313299998));
#301503=CARTESIAN_POINT('Ctrl Pts',(-1.43875085400005,12.2,4.37357004899999));
#301504=CARTESIAN_POINT('Ctrl Pts',(-1.43875085400005,5.2,4.37357004899999));
#301505=CARTESIAN_POINT('Ctrl Pts',(-1.43875085400005,2.2,4.37357004899999));
#301506=CARTESIAN_POINT('Ctrl Pts',(-1.43923944700005,12.2,4.37118997099999));
#301507=CARTESIAN_POINT('Ctrl Pts',(-1.43923944700005,5.2,4.37118997099999));
#301508=CARTESIAN_POINT('Ctrl Pts',(-1.43923944700005,2.2,4.37118997099999));
#301509=CARTESIAN_POINT('Ctrl Pts',(-1.43972479200006,12.2,4.36881290699999));
#301510=CARTESIAN_POINT('Ctrl Pts',(-1.43972479200006,5.2,4.36881290699999));
#301511=CARTESIAN_POINT('Ctrl Pts',(-1.43972479200006,2.2,4.36881290699999));
#301512=CARTESIAN_POINT('Ctrl Pts',(-1.44020689300006,12.2,4.36643886499999));
#301513=CARTESIAN_POINT('Ctrl Pts',(-1.44020689300006,5.2,4.36643886499999));
#301514=CARTESIAN_POINT('Ctrl Pts',(-1.44020689300006,2.2,4.36643886499999));
#301515=CARTESIAN_POINT('Ctrl Pts',(-1.44068575700006,12.2,4.36406785199999));
#301516=CARTESIAN_POINT('Ctrl Pts',(-1.44068575700006,5.2,4.36406785199999));
#301517=CARTESIAN_POINT('Ctrl Pts',(-1.44068575700006,2.2,4.36406785199999));
#301518=CARTESIAN_POINT('Ctrl Pts',(-1.44116138800006,12.2,4.36169987799998));
#301519=CARTESIAN_POINT('Ctrl Pts',(-1.44116138800006,5.2,4.36169987799998));
#301520=CARTESIAN_POINT('Ctrl Pts',(-1.44116138800006,2.2,4.36169987799998));
#301521=CARTESIAN_POINT('Ctrl Pts',(-1.44163379200006,12.2,4.35933494699999));
#301522=CARTESIAN_POINT('Ctrl Pts',(-1.44163379200006,5.2,4.35933494699999));
#301523=CARTESIAN_POINT('Ctrl Pts',(-1.44163379200006,2.2,4.35933494699999));
#301524=CARTESIAN_POINT('Ctrl Pts',(-1.44210297400006,12.2,4.35697306899999));
#301525=CARTESIAN_POINT('Ctrl Pts',(-1.44210297400006,5.2,4.35697306899999));
#301526=CARTESIAN_POINT('Ctrl Pts',(-1.44210297400006,2.2,4.35697306899999));
#301527=CARTESIAN_POINT('Ctrl Pts',(-1.44256894100006,12.2,4.35461424899999));
#301528=CARTESIAN_POINT('Ctrl Pts',(-1.44256894100006,5.2,4.35461424899999));
#301529=CARTESIAN_POINT('Ctrl Pts',(-1.44256894100006,2.2,4.35461424899999));
#301530=CARTESIAN_POINT('Ctrl Pts',(-1.44303169500006,12.2,4.35225849899999));
#301531=CARTESIAN_POINT('Ctrl Pts',(-1.44303169500006,5.2,4.35225849899999));
#301532=CARTESIAN_POINT('Ctrl Pts',(-1.44303169500006,2.2,4.35225849899999));
#301533=CARTESIAN_POINT('Ctrl Pts',(-1.44349124500006,12.2,4.34990582299999));
#301534=CARTESIAN_POINT('Ctrl Pts',(-1.44349124500006,5.2,4.34990582299999));
#301535=CARTESIAN_POINT('Ctrl Pts',(-1.44349124500006,2.2,4.34990582299999));
#301536=CARTESIAN_POINT('Ctrl Pts',(-1.44394759500006,12.2,4.34755622899999));
#301537=CARTESIAN_POINT('Ctrl Pts',(-1.44394759500006,5.2,4.34755622899999));
#301538=CARTESIAN_POINT('Ctrl Pts',(-1.44394759500006,2.2,4.34755622899999));
#301539=CARTESIAN_POINT('Ctrl Pts',(-1.44440074900006,12.2,4.34520972699998));
#301540=CARTESIAN_POINT('Ctrl Pts',(-1.44440074900006,5.2,4.34520972699998));
#301541=CARTESIAN_POINT('Ctrl Pts',(-1.44440074900006,2.2,4.34520972699998));
#301542=CARTESIAN_POINT('Ctrl Pts',(-1.44485071400006,12.2,4.34286632199999));
#301543=CARTESIAN_POINT('Ctrl Pts',(-1.44485071400006,5.2,4.34286632199999));
#301544=CARTESIAN_POINT('Ctrl Pts',(-1.44485071400006,2.2,4.34286632199999));
#301545=CARTESIAN_POINT('Ctrl Pts',(-1.44529749600006,12.2,4.34052602399999));
#301546=CARTESIAN_POINT('Ctrl Pts',(-1.44529749600006,5.2,4.34052602399999));
#301547=CARTESIAN_POINT('Ctrl Pts',(-1.44529749600006,2.2,4.34052602399999));
#301548=CARTESIAN_POINT('Ctrl Pts',(-1.44574109900006,12.2,4.33818883899999));
#301549=CARTESIAN_POINT('Ctrl Pts',(-1.44574109900006,5.2,4.33818883899999));
#301550=CARTESIAN_POINT('Ctrl Pts',(-1.44574109900006,2.2,4.33818883899999));
#301551=CARTESIAN_POINT('Ctrl Pts',(-1.44618153000006,12.2,4.33585477399999));
#301552=CARTESIAN_POINT('Ctrl Pts',(-1.44618153000006,5.2,4.33585477399999));
#301553=CARTESIAN_POINT('Ctrl Pts',(-1.44618153000006,2.2,4.33585477399999));
#301554=CARTESIAN_POINT('Ctrl Pts',(-1.44661879400006,12.2,4.33352383899998));
#301555=CARTESIAN_POINT('Ctrl Pts',(-1.44661879400006,5.2,4.33352383899998));
#301556=CARTESIAN_POINT('Ctrl Pts',(-1.44661879400006,2.2,4.33352383899998));
#301557=CARTESIAN_POINT('Ctrl Pts',(-1.44705289500005,12.2,4.33119603999998));
#301558=CARTESIAN_POINT('Ctrl Pts',(-1.44705289500005,5.2,4.33119603999998));
#301559=CARTESIAN_POINT('Ctrl Pts',(-1.44705289500005,2.2,4.33119603999998));
#301560=CARTESIAN_POINT('Ctrl Pts',(-1.44748384100006,12.2,4.32887138499999));
#301561=CARTESIAN_POINT('Ctrl Pts',(-1.44748384100006,5.2,4.32887138499999));
#301562=CARTESIAN_POINT('Ctrl Pts',(-1.44748384100006,2.2,4.32887138499999));
#301563=CARTESIAN_POINT('Ctrl Pts',(-1.44791163700006,12.2,4.32654988099999));
#301564=CARTESIAN_POINT('Ctrl Pts',(-1.44791163700006,5.2,4.32654988099999));
#301565=CARTESIAN_POINT('Ctrl Pts',(-1.44791163700006,2.2,4.32654988099999));
#301566=CARTESIAN_POINT('Ctrl Pts',(-1.44833628700006,12.2,4.32423153699999));
#301567=CARTESIAN_POINT('Ctrl Pts',(-1.44833628700006,5.2,4.32423153699999));
#301568=CARTESIAN_POINT('Ctrl Pts',(-1.44833628700006,2.2,4.32423153699999));
#301569=CARTESIAN_POINT('Ctrl Pts',(-1.44875779800006,12.2,4.32191636099999));
#301570=CARTESIAN_POINT('Ctrl Pts',(-1.44875779800006,5.2,4.32191636099999));
#301571=CARTESIAN_POINT('Ctrl Pts',(-1.44875779800006,2.2,4.32191636099999));
#301572=CARTESIAN_POINT('Ctrl Pts',(-1.44917617600006,12.2,4.31960435799999));
#301573=CARTESIAN_POINT('Ctrl Pts',(-1.44917617600006,5.2,4.31960435799999));
#301574=CARTESIAN_POINT('Ctrl Pts',(-1.44917617600006,2.2,4.31960435799999));
#301575=CARTESIAN_POINT('Ctrl Pts',(-1.44959142400006,12.2,4.31729553799999));
#301576=CARTESIAN_POINT('Ctrl Pts',(-1.44959142400006,5.2,4.31729553799999));
#301577=CARTESIAN_POINT('Ctrl Pts',(-1.44959142400006,2.2,4.31729553799999));
#301578=CARTESIAN_POINT('Ctrl Pts',(-1.45000355200006,12.2,4.31498990799999));
#301579=CARTESIAN_POINT('Ctrl Pts',(-1.45000355200006,5.2,4.31498990799999));
#301580=CARTESIAN_POINT('Ctrl Pts',(-1.45000355200006,2.2,4.31498990799999));
#301581=CARTESIAN_POINT('Ctrl Pts',(-1.45041256300006,12.2,4.31268747599999));
#301582=CARTESIAN_POINT('Ctrl Pts',(-1.45041256300006,5.2,4.31268747599999));
#301583=CARTESIAN_POINT('Ctrl Pts',(-1.45041256300006,2.2,4.31268747599999));
#301584=CARTESIAN_POINT('Ctrl Pts',(-1.45081846300006,12.2,4.31038824899999));
#301585=CARTESIAN_POINT('Ctrl Pts',(-1.45081846300006,5.2,4.31038824899999));
#301586=CARTESIAN_POINT('Ctrl Pts',(-1.45081846300006,2.2,4.31038824899999));
#301587=CARTESIAN_POINT('Ctrl Pts',(-1.45122125700005,12.2,4.30809223499999));
#301588=CARTESIAN_POINT('Ctrl Pts',(-1.45122125700005,5.2,4.30809223499999));
#301589=CARTESIAN_POINT('Ctrl Pts',(-1.45122125700005,2.2,4.30809223499999));
#301590=CARTESIAN_POINT('Ctrl Pts',(-1.45162095300006,12.2,4.30579944199999));
#301591=CARTESIAN_POINT('Ctrl Pts',(-1.45162095300006,5.2,4.30579944199999));
#301592=CARTESIAN_POINT('Ctrl Pts',(-1.45162095300006,2.2,4.30579944199999));
#301593=CARTESIAN_POINT('Ctrl Pts',(-1.45201755400006,12.2,4.30350987799999));
#301594=CARTESIAN_POINT('Ctrl Pts',(-1.45201755400006,5.2,4.30350987799999));
#301595=CARTESIAN_POINT('Ctrl Pts',(-1.45201755400006,2.2,4.30350987799999));
#301596=CARTESIAN_POINT('Ctrl Pts',(-1.45241106800006,12.2,4.30122354899999));
#301597=CARTESIAN_POINT('Ctrl Pts',(-1.45241106800006,5.2,4.30122354899999));
#301598=CARTESIAN_POINT('Ctrl Pts',(-1.45241106800006,2.2,4.30122354899999));
#301599=CARTESIAN_POINT('Ctrl Pts',(-1.45280150000006,12.2,4.29894046499999));
#301600=CARTESIAN_POINT('Ctrl Pts',(-1.45280150000006,5.2,4.29894046499999));
#301601=CARTESIAN_POINT('Ctrl Pts',(-1.45280150000006,2.2,4.29894046499999));
#301602=CARTESIAN_POINT('Ctrl Pts',(-1.45318885600005,12.2,4.29666063199999));
#301603=CARTESIAN_POINT('Ctrl Pts',(-1.45318885600005,5.2,4.29666063199999));
#301604=CARTESIAN_POINT('Ctrl Pts',(-1.45318885600005,2.2,4.29666063199999));
#301605=CARTESIAN_POINT('Ctrl Pts',(-1.45357314000006,12.2,4.29438405699998));
#301606=CARTESIAN_POINT('Ctrl Pts',(-1.45357314000006,5.2,4.29438405699998));
#301607=CARTESIAN_POINT('Ctrl Pts',(-1.45357314000006,2.2,4.29438405699998));
#301608=CARTESIAN_POINT('Ctrl Pts',(-1.45395436100006,12.2,4.29211075099998));
#301609=CARTESIAN_POINT('Ctrl Pts',(-1.45395436100006,5.2,4.29211075099998));
#301610=CARTESIAN_POINT('Ctrl Pts',(-1.45395436100006,2.2,4.29211075099998));
#301611=CARTESIAN_POINT('Ctrl Pts',(-1.45433252400006,12.2,4.28984071899999));
#301612=CARTESIAN_POINT('Ctrl Pts',(-1.45433252400006,5.2,4.28984071899999));
#301613=CARTESIAN_POINT('Ctrl Pts',(-1.45433252400006,2.2,4.28984071899999));
#301614=CARTESIAN_POINT('Ctrl Pts',(-1.45470763300006,12.2,4.28757396799998));
#301615=CARTESIAN_POINT('Ctrl Pts',(-1.45470763300006,5.2,4.28757396799998));
#301616=CARTESIAN_POINT('Ctrl Pts',(-1.45470763300006,2.2,4.28757396799998));
#301617=CARTESIAN_POINT('Ctrl Pts',(-1.45507969700006,12.2,4.28531050899998));
#301618=CARTESIAN_POINT('Ctrl Pts',(-1.45507969700006,5.2,4.28531050899998));
#301619=CARTESIAN_POINT('Ctrl Pts',(-1.45507969700006,2.2,4.28531050899998));
#301620=CARTESIAN_POINT('Ctrl Pts',(-1.45544871800006,12.2,4.28305034699999));
#301621=CARTESIAN_POINT('Ctrl Pts',(-1.45544871800006,5.2,4.28305034699999));
#301622=CARTESIAN_POINT('Ctrl Pts',(-1.45544871800006,2.2,4.28305034699999));
#301623=CARTESIAN_POINT('Ctrl Pts',(-1.45581470400006,12.2,4.28079348999999));
#301624=CARTESIAN_POINT('Ctrl Pts',(-1.45581470400006,5.2,4.28079348999999));
#301625=CARTESIAN_POINT('Ctrl Pts',(-1.45581470400006,2.2,4.28079348999999));
#301626=CARTESIAN_POINT('Ctrl Pts',(-1.45617766300006,12.2,4.27853994599998));
#301627=CARTESIAN_POINT('Ctrl Pts',(-1.45617766300006,5.2,4.27853994599998));
#301628=CARTESIAN_POINT('Ctrl Pts',(-1.45617766300006,2.2,4.27853994599998));
#301629=CARTESIAN_POINT('Ctrl Pts',(-1.45653759900006,12.2,4.27628972399998));
#301630=CARTESIAN_POINT('Ctrl Pts',(-1.45653759900006,5.2,4.27628972399998));
#301631=CARTESIAN_POINT('Ctrl Pts',(-1.45653759900006,2.2,4.27628972399998));
#301632=CARTESIAN_POINT('Ctrl Pts',(-1.45689451600005,12.2,4.27404282999999));
#301633=CARTESIAN_POINT('Ctrl Pts',(-1.45689451600005,5.2,4.27404282999999));
#301634=CARTESIAN_POINT('Ctrl Pts',(-1.45689451600005,2.2,4.27404282999999));
#301635=CARTESIAN_POINT('Ctrl Pts',(-1.45724842400006,12.2,4.27179927199998));
#301636=CARTESIAN_POINT('Ctrl Pts',(-1.45724842400006,5.2,4.27179927199998));
#301637=CARTESIAN_POINT('Ctrl Pts',(-1.45724842400006,2.2,4.27179927199998));
#301638=CARTESIAN_POINT('Ctrl Pts',(-1.45759932700006,12.2,4.26955905899998));
#301639=CARTESIAN_POINT('Ctrl Pts',(-1.45759932700006,5.2,4.26955905899998));
#301640=CARTESIAN_POINT('Ctrl Pts',(-1.45759932700006,2.2,4.26955905899998));
#301641=CARTESIAN_POINT('Ctrl Pts',(-1.45794723000006,12.2,4.26732219699999));
#301642=CARTESIAN_POINT('Ctrl Pts',(-1.45794723000006,5.2,4.26732219699999));
#301643=CARTESIAN_POINT('Ctrl Pts',(-1.45794723000006,2.2,4.26732219699999));
#301644=CARTESIAN_POINT('Ctrl Pts',(-1.45829214100006,12.2,4.26508869499998));
#301645=CARTESIAN_POINT('Ctrl Pts',(-1.45829214100006,5.2,4.26508869499998));
#301646=CARTESIAN_POINT('Ctrl Pts',(-1.45829214100006,2.2,4.26508869499998));
#301647=CARTESIAN_POINT('Ctrl Pts',(-1.45863406500006,12.2,4.26285855999998));
#301648=CARTESIAN_POINT('Ctrl Pts',(-1.45863406500006,5.2,4.26285855999998));
#301649=CARTESIAN_POINT('Ctrl Pts',(-1.45863406500006,2.2,4.26285855999998));
#301650=CARTESIAN_POINT('Ctrl Pts',(-1.45897301000006,12.2,4.26063179999999));
#301651=CARTESIAN_POINT('Ctrl Pts',(-1.45897301000006,5.2,4.26063179999999));
#301652=CARTESIAN_POINT('Ctrl Pts',(-1.45897301000006,2.2,4.26063179999999));
#301653=CARTESIAN_POINT('Ctrl Pts',(-1.45930898000006,12.2,4.25840842299999));
#301654=CARTESIAN_POINT('Ctrl Pts',(-1.45930898000006,5.2,4.25840842299999));
#301655=CARTESIAN_POINT('Ctrl Pts',(-1.45930898000006,2.2,4.25840842299999));
#301656=CARTESIAN_POINT('Ctrl Pts',(-1.45964198100006,12.2,4.25618843599998));
#301657=CARTESIAN_POINT('Ctrl Pts',(-1.45964198100006,5.2,4.25618843599998));
#301658=CARTESIAN_POINT('Ctrl Pts',(-1.45964198100006,2.2,4.25618843599998));
#301659=CARTESIAN_POINT('Ctrl Pts',(-1.45997202100006,12.2,4.25397184699998));
#301660=CARTESIAN_POINT('Ctrl Pts',(-1.45997202100006,5.2,4.25397184699998));
#301661=CARTESIAN_POINT('Ctrl Pts',(-1.45997202100006,2.2,4.25397184699998));
#301662=CARTESIAN_POINT('Ctrl Pts',(-1.46029910500006,12.2,4.25175866399999));
#301663=CARTESIAN_POINT('Ctrl Pts',(-1.46029910500006,5.2,4.25175866399999));
#301664=CARTESIAN_POINT('Ctrl Pts',(-1.46029910500006,2.2,4.25175866399999));
#301665=CARTESIAN_POINT('Ctrl Pts',(-1.46062324000006,12.2,4.24954889499999));
#301666=CARTESIAN_POINT('Ctrl Pts',(-1.46062324000006,5.2,4.24954889499999));
#301667=CARTESIAN_POINT('Ctrl Pts',(-1.46062324000006,2.2,4.24954889499999));
#301668=CARTESIAN_POINT('Ctrl Pts',(-1.46094443100006,12.2,4.24734254799999));
#301669=CARTESIAN_POINT('Ctrl Pts',(-1.46094443100006,5.2,4.24734254799999));
#301670=CARTESIAN_POINT('Ctrl Pts',(-1.46094443100006,2.2,4.24734254799999));
#301671=CARTESIAN_POINT('Ctrl Pts',(-1.46126268600006,12.2,4.24513962999999));
#301672=CARTESIAN_POINT('Ctrl Pts',(-1.46126268600006,5.2,4.24513962999999));
#301673=CARTESIAN_POINT('Ctrl Pts',(-1.46126268600006,2.2,4.24513962999999));
#301674=CARTESIAN_POINT('Ctrl Pts',(-1.46157800900006,12.2,4.24294014899999));
#301675=CARTESIAN_POINT('Ctrl Pts',(-1.46157800900006,5.2,4.24294014899999));
#301676=CARTESIAN_POINT('Ctrl Pts',(-1.46157800900006,2.2,4.24294014899999));
#301677=CARTESIAN_POINT('Ctrl Pts',(-1.46189040800005,12.2,4.24074411199998));
#301678=CARTESIAN_POINT('Ctrl Pts',(-1.46189040800005,5.2,4.24074411199998));
#301679=CARTESIAN_POINT('Ctrl Pts',(-1.46189040800005,2.2,4.24074411199998));
#301680=CARTESIAN_POINT('Ctrl Pts',(-1.46219988800006,12.2,4.23855152799998));
#301681=CARTESIAN_POINT('Ctrl Pts',(-1.46219988800006,5.2,4.23855152799998));
#301682=CARTESIAN_POINT('Ctrl Pts',(-1.46219988800006,2.2,4.23855152799998));
#301683=CARTESIAN_POINT('Ctrl Pts',(-1.46250645800006,12.2,4.23636240399999));
#301684=CARTESIAN_POINT('Ctrl Pts',(-1.46250645800006,5.2,4.23636240399999));
#301685=CARTESIAN_POINT('Ctrl Pts',(-1.46250645800006,2.2,4.23636240399999));
#301686=CARTESIAN_POINT('Ctrl Pts',(-1.46281012200006,12.2,4.23417674899999));
#301687=CARTESIAN_POINT('Ctrl Pts',(-1.46281012200006,5.2,4.23417674899999));
#301688=CARTESIAN_POINT('Ctrl Pts',(-1.46281012200006,2.2,4.23417674899999));
#301689=CARTESIAN_POINT('Ctrl Pts',(-1.46311088700006,12.2,4.23199456799999));
#301690=CARTESIAN_POINT('Ctrl Pts',(-1.46311088700006,5.2,4.23199456799999));
#301691=CARTESIAN_POINT('Ctrl Pts',(-1.46311088700006,2.2,4.23199456799999));
#301692=CARTESIAN_POINT('Ctrl Pts',(-1.46340875900006,12.2,4.22981587199998));
#301693=CARTESIAN_POINT('Ctrl Pts',(-1.46340875900006,5.2,4.22981587199998));
#301694=CARTESIAN_POINT('Ctrl Pts',(-1.46340875900006,2.2,4.22981587199998));
#301695=CARTESIAN_POINT('Ctrl Pts',(-1.46370374500005,12.2,4.22764066699998));
#301696=CARTESIAN_POINT('Ctrl Pts',(-1.46370374500005,5.2,4.22764066699998));
#301697=CARTESIAN_POINT('Ctrl Pts',(-1.46370374500005,2.2,4.22764066699998));
#301698=CARTESIAN_POINT('Ctrl Pts',(-1.46399585200006,12.2,4.22546895999999));
#301699=CARTESIAN_POINT('Ctrl Pts',(-1.46399585200006,5.2,4.22546895999999));
#301700=CARTESIAN_POINT('Ctrl Pts',(-1.46399585200006,2.2,4.22546895999999));
#301701=CARTESIAN_POINT('Ctrl Pts',(-1.46428508500006,12.2,4.22330076099998));
#301702=CARTESIAN_POINT('Ctrl Pts',(-1.46428508500006,5.2,4.22330076099998));
#301703=CARTESIAN_POINT('Ctrl Pts',(-1.46428508500006,2.2,4.22330076099998));
#301704=CARTESIAN_POINT('Ctrl Pts',(-1.46457145100006,12.2,4.22113607699998));
#301705=CARTESIAN_POINT('Ctrl Pts',(-1.46457145100006,5.2,4.22113607699998));
#301706=CARTESIAN_POINT('Ctrl Pts',(-1.46457145100006,2.2,4.22113607699998));
#301707=CARTESIAN_POINT('Ctrl Pts',(-1.46485495700006,12.2,4.21897491499998));
#301708=CARTESIAN_POINT('Ctrl Pts',(-1.46485495700006,5.2,4.21897491499998));
#301709=CARTESIAN_POINT('Ctrl Pts',(-1.46485495700006,2.2,4.21897491499998));
#301710=CARTESIAN_POINT('Ctrl Pts',(-1.46513560900006,12.2,4.21681728399999));
#301711=CARTESIAN_POINT('Ctrl Pts',(-1.46513560900006,5.2,4.21681728399999));
#301712=CARTESIAN_POINT('Ctrl Pts',(-1.46513560900006,2.2,4.21681728399999));
#301713=CARTESIAN_POINT('Ctrl Pts',(-1.46541341300006,12.2,4.21466318899999));
#301714=CARTESIAN_POINT('Ctrl Pts',(-1.46541341300006,5.2,4.21466318899999));
#301715=CARTESIAN_POINT('Ctrl Pts',(-1.46541341300006,2.2,4.21466318899999));
#301716=CARTESIAN_POINT('Ctrl Pts',(-1.46568837800006,12.2,4.21251264099999));
#301717=CARTESIAN_POINT('Ctrl Pts',(-1.46568837800006,5.2,4.21251264099999));
#301718=CARTESIAN_POINT('Ctrl Pts',(-1.46568837800006,2.2,4.21251264099999));
#301719=CARTESIAN_POINT('Ctrl Pts',(-1.46596050800005,12.2,4.21036564699998));
#301720=CARTESIAN_POINT('Ctrl Pts',(-1.46596050800005,5.2,4.21036564699998));
#301721=CARTESIAN_POINT('Ctrl Pts',(-1.46596050800005,2.2,4.21036564699998));
#301722=CARTESIAN_POINT('Ctrl Pts',(-1.46622981100006,12.2,4.20822221299999));
#301723=CARTESIAN_POINT('Ctrl Pts',(-1.46622981100006,5.2,4.20822221299999));
#301724=CARTESIAN_POINT('Ctrl Pts',(-1.46622981100006,2.2,4.20822221299999));
#301725=CARTESIAN_POINT('Ctrl Pts',(-1.46649629200006,12.2,4.20608234999998));
#301726=CARTESIAN_POINT('Ctrl Pts',(-1.46649629200006,5.2,4.20608234999998));
#301727=CARTESIAN_POINT('Ctrl Pts',(-1.46649629200006,2.2,4.20608234999998));
#301728=CARTESIAN_POINT('Ctrl Pts',(-1.46675996000006,12.2,4.20394606199999));
#301729=CARTESIAN_POINT('Ctrl Pts',(-1.46675996000006,5.2,4.20394606199999));
#301730=CARTESIAN_POINT('Ctrl Pts',(-1.46675996000006,2.2,4.20394606199999));
#301731=CARTESIAN_POINT('Ctrl Pts',(-1.46702082000005,12.2,4.20181335999998));
#301732=CARTESIAN_POINT('Ctrl Pts',(-1.46702082000005,5.2,4.20181335999998));
#301733=CARTESIAN_POINT('Ctrl Pts',(-1.46702082000005,2.2,4.20181335999998));
#301734=CARTESIAN_POINT('Ctrl Pts',(-1.46727887800005,12.2,4.19968425099999));
#301735=CARTESIAN_POINT('Ctrl Pts',(-1.46727887800005,5.2,4.19968425099999));
#301736=CARTESIAN_POINT('Ctrl Pts',(-1.46727887800005,2.2,4.19968425099999));
#301737=CARTESIAN_POINT('Ctrl Pts',(-1.46753414300006,12.2,4.19755874099998));
#301738=CARTESIAN_POINT('Ctrl Pts',(-1.46753414300006,5.2,4.19755874099998));
#301739=CARTESIAN_POINT('Ctrl Pts',(-1.46753414300006,2.2,4.19755874099998));
#301740=CARTESIAN_POINT('Ctrl Pts',(-1.46778662100005,12.2,4.19543684099998));
#301741=CARTESIAN_POINT('Ctrl Pts',(-1.46778662100005,5.2,4.19543684099998));
#301742=CARTESIAN_POINT('Ctrl Pts',(-1.46778662100005,2.2,4.19543684099998));
#301743=CARTESIAN_POINT('Ctrl Pts',(-1.46803631800006,12.2,4.19331855599999));
#301744=CARTESIAN_POINT('Ctrl Pts',(-1.46803631800006,5.2,4.19331855599999));
#301745=CARTESIAN_POINT('Ctrl Pts',(-1.46803631800006,2.2,4.19331855599999));
#301746=CARTESIAN_POINT('Ctrl Pts',(-1.46828324000006,12.2,4.19120389499999));
#301747=CARTESIAN_POINT('Ctrl Pts',(-1.46828324000006,5.2,4.19120389499999));
#301748=CARTESIAN_POINT('Ctrl Pts',(-1.46828324000006,2.2,4.19120389499999));
#301749=CARTESIAN_POINT('Ctrl Pts',(-1.46852739600006,12.2,4.18909286499999));
#301750=CARTESIAN_POINT('Ctrl Pts',(-1.46852739600006,5.2,4.18909286499999));
#301751=CARTESIAN_POINT('Ctrl Pts',(-1.46852739600006,2.2,4.18909286499999));
#301752=CARTESIAN_POINT('Ctrl Pts',(-1.46876879100006,12.2,4.18698547499999));
#301753=CARTESIAN_POINT('Ctrl Pts',(-1.46876879100006,5.2,4.18698547499999));
#301754=CARTESIAN_POINT('Ctrl Pts',(-1.46876879100006,2.2,4.18698547499999));
#301755=CARTESIAN_POINT('Ctrl Pts',(-1.46900743300006,12.2,4.18488173199999));
#301756=CARTESIAN_POINT('Ctrl Pts',(-1.46900743300006,5.2,4.18488173199999));
#301757=CARTESIAN_POINT('Ctrl Pts',(-1.46900743300006,2.2,4.18488173199999));
#301758=CARTESIAN_POINT('Ctrl Pts',(-1.46924332800006,12.2,4.18278164499998));
#301759=CARTESIAN_POINT('Ctrl Pts',(-1.46924332800006,5.2,4.18278164499998));
#301760=CARTESIAN_POINT('Ctrl Pts',(-1.46924332800006,2.2,4.18278164499998));
#301761=CARTESIAN_POINT('Ctrl Pts',(-1.46947648300006,12.2,4.18068521899999));
#301762=CARTESIAN_POINT('Ctrl Pts',(-1.46947648300006,5.2,4.18068521899999));
#301763=CARTESIAN_POINT('Ctrl Pts',(-1.46947648300006,2.2,4.18068521899999));
#301764=CARTESIAN_POINT('Ctrl Pts',(-1.46970690600006,12.2,4.17859246499999));
#301765=CARTESIAN_POINT('Ctrl Pts',(-1.46970690600006,5.2,4.17859246499999));
#301766=CARTESIAN_POINT('Ctrl Pts',(-1.46970690600006,2.2,4.17859246499999));
#301767=CARTESIAN_POINT('Ctrl Pts',(-1.46993460300005,12.2,4.17650338999999));
#301768=CARTESIAN_POINT('Ctrl Pts',(-1.46993460300005,5.2,4.17650338999999));
#301769=CARTESIAN_POINT('Ctrl Pts',(-1.46993460300005,2.2,4.17650338999999));
#301770=CARTESIAN_POINT('Ctrl Pts',(-1.47015957900006,12.2,4.17441800099999));
#301771=CARTESIAN_POINT('Ctrl Pts',(-1.47015957900006,5.2,4.17441800099999));
#301772=CARTESIAN_POINT('Ctrl Pts',(-1.47015957900006,2.2,4.17441800099999));
#301773=CARTESIAN_POINT('Ctrl Pts',(-1.47038184500005,12.2,4.17233630599998));
#301774=CARTESIAN_POINT('Ctrl Pts',(-1.47038184500005,5.2,4.17233630599998));
#301775=CARTESIAN_POINT('Ctrl Pts',(-1.47038184500005,2.2,4.17233630599998));
#301776=CARTESIAN_POINT('Ctrl Pts',(-1.47060140500006,12.2,4.17025831399998));
#301777=CARTESIAN_POINT('Ctrl Pts',(-1.47060140500006,5.2,4.17025831399998));
#301778=CARTESIAN_POINT('Ctrl Pts',(-1.47060140500006,2.2,4.17025831399998));
#301779=CARTESIAN_POINT('Ctrl Pts',(-1.47081826800005,12.2,4.16818403099998));
#301780=CARTESIAN_POINT('Ctrl Pts',(-1.47081826800005,5.2,4.16818403099998));
#301781=CARTESIAN_POINT('Ctrl Pts',(-1.47081826800005,2.2,4.16818403099998));
#301782=CARTESIAN_POINT('Ctrl Pts',(-1.47103243800006,12.2,4.16611346599999));
#301783=CARTESIAN_POINT('Ctrl Pts',(-1.47103243800006,5.2,4.16611346599999));
#301784=CARTESIAN_POINT('Ctrl Pts',(-1.47103243800006,2.2,4.16611346599999));
#301785=CARTESIAN_POINT('Ctrl Pts',(-1.47124392500006,12.2,4.16404662599999));
#301786=CARTESIAN_POINT('Ctrl Pts',(-1.47124392500006,5.2,4.16404662599999));
#301787=CARTESIAN_POINT('Ctrl Pts',(-1.47124392500006,2.2,4.16404662599999));
#301788=CARTESIAN_POINT('Ctrl Pts',(-1.47145273500006,12.2,4.16198351999999));
#301789=CARTESIAN_POINT('Ctrl Pts',(-1.47145273500006,5.2,4.16198351999999));
#301790=CARTESIAN_POINT('Ctrl Pts',(-1.47145273500006,2.2,4.16198351999999));
#301791=CARTESIAN_POINT('Ctrl Pts',(-1.47165887500006,12.2,4.15992415599998));
#301792=CARTESIAN_POINT('Ctrl Pts',(-1.47165887500006,5.2,4.15992415599998));
#301793=CARTESIAN_POINT('Ctrl Pts',(-1.47165887500006,2.2,4.15992415599998));
#301794=CARTESIAN_POINT('Ctrl Pts',(-1.47186235200006,12.2,4.15786854099998));
#301795=CARTESIAN_POINT('Ctrl Pts',(-1.47186235200006,5.2,4.15786854099998));
#301796=CARTESIAN_POINT('Ctrl Pts',(-1.47186235200006,2.2,4.15786854099998));
#301797=CARTESIAN_POINT('Ctrl Pts',(-1.47206317400006,12.2,4.15581668199999));
#301798=CARTESIAN_POINT('Ctrl Pts',(-1.47206317400006,5.2,4.15581668199999));
#301799=CARTESIAN_POINT('Ctrl Pts',(-1.47206317400006,2.2,4.15581668199999));
#301800=CARTESIAN_POINT('Ctrl Pts',(-1.47226134800006,12.2,4.15376858899998));
#301801=CARTESIAN_POINT('Ctrl Pts',(-1.47226134800006,5.2,4.15376858899998));
#301802=CARTESIAN_POINT('Ctrl Pts',(-1.47226134800006,2.2,4.15376858899998));
#301803=CARTESIAN_POINT('Ctrl Pts',(-1.47245687900006,12.2,4.15172426699999));
#301804=CARTESIAN_POINT('Ctrl Pts',(-1.47245687900006,5.2,4.15172426699999));
#301805=CARTESIAN_POINT('Ctrl Pts',(-1.47245687900006,2.2,4.15172426699999));
#301806=CARTESIAN_POINT('Ctrl Pts',(-1.47264977700006,12.2,4.14968372799999));
#301807=CARTESIAN_POINT('Ctrl Pts',(-1.47264977700006,5.2,4.14968372799999));
#301808=CARTESIAN_POINT('Ctrl Pts',(-1.47264977700006,2.2,4.14968372799999));
#301809=CARTESIAN_POINT('Ctrl Pts',(-1.47284004700006,12.2,4.14764697499999));
#301810=CARTESIAN_POINT('Ctrl Pts',(-1.47284004700006,5.2,4.14764697499999));
#301811=CARTESIAN_POINT('Ctrl Pts',(-1.47284004700006,2.2,4.14764697499999));
#301812=CARTESIAN_POINT('Ctrl Pts',(-1.47302769900006,12.2,4.14561402099999));
#301813=CARTESIAN_POINT('Ctrl Pts',(-1.47302769900006,5.2,4.14561402099999));
#301814=CARTESIAN_POINT('Ctrl Pts',(-1.47302769900006,2.2,4.14561402099999));
#301815=CARTESIAN_POINT('Ctrl Pts',(-1.47321273700006,12.2,4.14358486899999));
#301816=CARTESIAN_POINT('Ctrl Pts',(-1.47321273700006,5.2,4.14358486899999));
#301817=CARTESIAN_POINT('Ctrl Pts',(-1.47321273700006,2.2,4.14358486899999));
#301818=CARTESIAN_POINT('Ctrl Pts',(-1.47339517100006,12.2,4.14155952999998));
#301819=CARTESIAN_POINT('Ctrl Pts',(-1.47339517100006,5.2,4.14155952999998));
#301820=CARTESIAN_POINT('Ctrl Pts',(-1.47339517100006,2.2,4.14155952999998));
#301821=CARTESIAN_POINT('Ctrl Pts',(-1.47357500700006,12.2,4.13953801099999));
#301822=CARTESIAN_POINT('Ctrl Pts',(-1.47357500700006,5.2,4.13953801099999));
#301823=CARTESIAN_POINT('Ctrl Pts',(-1.47357500700006,2.2,4.13953801099999));
#301824=CARTESIAN_POINT('Ctrl Pts',(-1.47375225100006,12.2,4.13752031899998));
#301825=CARTESIAN_POINT('Ctrl Pts',(-1.47375225100006,5.2,4.13752031899998));
#301826=CARTESIAN_POINT('Ctrl Pts',(-1.47375225100006,2.2,4.13752031899998));
#301827=CARTESIAN_POINT('Ctrl Pts',(-1.47392691400006,12.2,4.13550646399998));
#301828=CARTESIAN_POINT('Ctrl Pts',(-1.47392691400006,5.2,4.13550646399998));
#301829=CARTESIAN_POINT('Ctrl Pts',(-1.47392691400006,2.2,4.13550646399998));
#301830=CARTESIAN_POINT('Ctrl Pts',(-1.47409900000006,12.2,4.13349645099998));
#301831=CARTESIAN_POINT('Ctrl Pts',(-1.47409900000006,5.2,4.13349645099998));
#301832=CARTESIAN_POINT('Ctrl Pts',(-1.47409900000006,2.2,4.13349645099998));
#301833=CARTESIAN_POINT('Ctrl Pts',(-1.47426851800006,12.2,4.13149029099999));
#301834=CARTESIAN_POINT('Ctrl Pts',(-1.47426851800006,5.2,4.13149029099999));
#301835=CARTESIAN_POINT('Ctrl Pts',(-1.47426851800006,2.2,4.13149029099999));
#301836=CARTESIAN_POINT('Ctrl Pts',(-1.47443547500006,12.2,4.12948798899999));
#301837=CARTESIAN_POINT('Ctrl Pts',(-1.47443547500006,5.2,4.12948798899999));
#301838=CARTESIAN_POINT('Ctrl Pts',(-1.47443547500006,2.2,4.12948798899999));
#301839=CARTESIAN_POINT('Ctrl Pts',(-1.47459987800006,12.2,4.12748955499998));
#301840=CARTESIAN_POINT('Ctrl Pts',(-1.47459987800006,5.2,4.12748955499998));
#301841=CARTESIAN_POINT('Ctrl Pts',(-1.47459987800006,2.2,4.12748955499998));
#301842=CARTESIAN_POINT('Ctrl Pts',(-1.47476173500006,12.2,4.12549499699999));
#301843=CARTESIAN_POINT('Ctrl Pts',(-1.47476173500006,5.2,4.12549499699999));
#301844=CARTESIAN_POINT('Ctrl Pts',(-1.47476173500006,2.2,4.12549499699999));
#301845=CARTESIAN_POINT('Ctrl Pts',(-1.47492105400006,12.2,4.12350432099998));
#301846=CARTESIAN_POINT('Ctrl Pts',(-1.47492105400006,5.2,4.12350432099998));
#301847=CARTESIAN_POINT('Ctrl Pts',(-1.47492105400006,2.2,4.12350432099998));
#301848=CARTESIAN_POINT('Ctrl Pts',(-1.47507784200006,12.2,4.12151753499998));
#301849=CARTESIAN_POINT('Ctrl Pts',(-1.47507784200006,5.2,4.12151753499998));
#301850=CARTESIAN_POINT('Ctrl Pts',(-1.47507784200006,2.2,4.12151753499998));
#301851=CARTESIAN_POINT('Ctrl Pts',(-1.47523210600006,12.2,4.11953464899998));
#301852=CARTESIAN_POINT('Ctrl Pts',(-1.47523210600006,5.2,4.11953464899998));
#301853=CARTESIAN_POINT('Ctrl Pts',(-1.47523210600006,2.2,4.11953464899998));
#301854=CARTESIAN_POINT('Ctrl Pts',(-1.47538385400006,12.2,4.11755566899998));
#301855=CARTESIAN_POINT('Ctrl Pts',(-1.47538385400006,5.2,4.11755566899998));
#301856=CARTESIAN_POINT('Ctrl Pts',(-1.47538385400006,2.2,4.11755566899998));
#301857=CARTESIAN_POINT('Ctrl Pts',(-1.47553309400006,12.2,4.11558060499999));
#301858=CARTESIAN_POINT('Ctrl Pts',(-1.47553309400006,5.2,4.11558060499999));
#301859=CARTESIAN_POINT('Ctrl Pts',(-1.47553309400006,2.2,4.11558060499999));
#301860=CARTESIAN_POINT('Ctrl Pts',(-1.47567983300006,12.2,4.11360946199999));
#301861=CARTESIAN_POINT('Ctrl Pts',(-1.47567983300006,5.2,4.11360946199999));
#301862=CARTESIAN_POINT('Ctrl Pts',(-1.47567983300006,2.2,4.11360946199999));
#301863=CARTESIAN_POINT('Ctrl Pts',(-1.47582407900006,12.2,4.11164225099999));
#301864=CARTESIAN_POINT('Ctrl Pts',(-1.47582407900006,5.2,4.11164225099999));
#301865=CARTESIAN_POINT('Ctrl Pts',(-1.47582407900006,2.2,4.11164225099999));
#301866=CARTESIAN_POINT('Ctrl Pts',(-1.47596583900006,12.2,4.10967897699998));
#301867=CARTESIAN_POINT('Ctrl Pts',(-1.47596583900006,5.2,4.10967897699998));
#301868=CARTESIAN_POINT('Ctrl Pts',(-1.47596583900006,2.2,4.10967897699998));
#301869=CARTESIAN_POINT('Ctrl Pts',(-1.47610512100006,12.2,4.10771964899999));
#301870=CARTESIAN_POINT('Ctrl Pts',(-1.47610512100006,5.2,4.10771964899999));
#301871=CARTESIAN_POINT('Ctrl Pts',(-1.47610512100006,2.2,4.10771964899999));
#301872=CARTESIAN_POINT('Ctrl Pts',(-1.47624193300006,12.2,4.10576427599998));
#301873=CARTESIAN_POINT('Ctrl Pts',(-1.47624193300006,5.2,4.10576427599998));
#301874=CARTESIAN_POINT('Ctrl Pts',(-1.47624193300006,2.2,4.10576427599998));
#301875=CARTESIAN_POINT('Ctrl Pts',(-1.47637628300005,12.2,4.10381286499998));
#301876=CARTESIAN_POINT('Ctrl Pts',(-1.47637628300005,5.2,4.10381286499998));
#301877=CARTESIAN_POINT('Ctrl Pts',(-1.47637628300005,2.2,4.10381286499998));
#301878=CARTESIAN_POINT('Ctrl Pts',(-1.47650817800006,12.2,4.10186542299999));
#301879=CARTESIAN_POINT('Ctrl Pts',(-1.47650817800006,5.2,4.10186542299999));
#301880=CARTESIAN_POINT('Ctrl Pts',(-1.47650817800006,2.2,4.10186542299999));
#301881=CARTESIAN_POINT('Ctrl Pts',(-1.47663762600006,12.2,4.09992195999998));
#301882=CARTESIAN_POINT('Ctrl Pts',(-1.47663762600006,5.2,4.09992195999998));
#301883=CARTESIAN_POINT('Ctrl Pts',(-1.47663762600006,2.2,4.09992195999998));
#301884=CARTESIAN_POINT('Ctrl Pts',(-1.47676463500006,12.2,4.09798248299998));
#301885=CARTESIAN_POINT('Ctrl Pts',(-1.47676463500006,5.2,4.09798248299998));
#301886=CARTESIAN_POINT('Ctrl Pts',(-1.47676463500006,2.2,4.09798248299998));
#301887=CARTESIAN_POINT('Ctrl Pts',(-1.47688921300006,12.2,4.09604699899998));
#301888=CARTESIAN_POINT('Ctrl Pts',(-1.47688921300006,5.2,4.09604699899998));
#301889=CARTESIAN_POINT('Ctrl Pts',(-1.47688921300006,2.2,4.09604699899998));
#301890=CARTESIAN_POINT('Ctrl Pts',(-1.47701136600006,12.2,4.09411551599998));
#301891=CARTESIAN_POINT('Ctrl Pts',(-1.47701136600006,5.2,4.09411551599998));
#301892=CARTESIAN_POINT('Ctrl Pts',(-1.47701136600006,2.2,4.09411551599998));
#301893=CARTESIAN_POINT('Ctrl Pts',(-1.47713110400006,12.2,4.09218804399998));
#301894=CARTESIAN_POINT('Ctrl Pts',(-1.47713110400006,5.2,4.09218804399998));
#301895=CARTESIAN_POINT('Ctrl Pts',(-1.47713110400006,2.2,4.09218804399998));
#301896=CARTESIAN_POINT('Ctrl Pts',(-1.47724843400006,12.2,4.09026458899999));
#301897=CARTESIAN_POINT('Ctrl Pts',(-1.47724843400006,5.2,4.09026458899999));
#301898=CARTESIAN_POINT('Ctrl Pts',(-1.47724843400006,2.2,4.09026458899999));
#301899=CARTESIAN_POINT('Ctrl Pts',(-1.47736336500006,12.2,4.08834515899999));
#301900=CARTESIAN_POINT('Ctrl Pts',(-1.47736336500006,5.2,4.08834515899999));
#301901=CARTESIAN_POINT('Ctrl Pts',(-1.47736336500006,2.2,4.08834515899999));
#301902=CARTESIAN_POINT('Ctrl Pts',(-1.47747590400006,12.2,4.08642976299999));
#301903=CARTESIAN_POINT('Ctrl Pts',(-1.47747590400006,5.2,4.08642976299999));
#301904=CARTESIAN_POINT('Ctrl Pts',(-1.47747590400006,2.2,4.08642976299999));
#301905=CARTESIAN_POINT('Ctrl Pts',(-1.47758605800006,12.2,4.08451840899998));
#301906=CARTESIAN_POINT('Ctrl Pts',(-1.47758605800006,5.2,4.08451840899998));
#301907=CARTESIAN_POINT('Ctrl Pts',(-1.47758605800006,2.2,4.08451840899998));
#301908=CARTESIAN_POINT('Ctrl Pts',(-1.47769383700005,12.2,4.08261110299998));
#301909=CARTESIAN_POINT('Ctrl Pts',(-1.47769383700005,5.2,4.08261110299998));
#301910=CARTESIAN_POINT('Ctrl Pts',(-1.47769383700005,2.2,4.08261110299998));
#301911=CARTESIAN_POINT('Ctrl Pts',(-1.47779924700006,12.2,4.08070785499999));
#301912=CARTESIAN_POINT('Ctrl Pts',(-1.47779924700006,5.2,4.08070785499999));
#301913=CARTESIAN_POINT('Ctrl Pts',(-1.47779924700006,2.2,4.08070785499999));
#301914=CARTESIAN_POINT('Ctrl Pts',(-1.47790229800006,12.2,4.07880867199999));
#301915=CARTESIAN_POINT('Ctrl Pts',(-1.47790229800006,5.2,4.07880867199999));
#301916=CARTESIAN_POINT('Ctrl Pts',(-1.47790229800006,2.2,4.07880867199999));
#301917=CARTESIAN_POINT('Ctrl Pts',(-1.47800299600006,12.2,4.07691356199999));
#301918=CARTESIAN_POINT('Ctrl Pts',(-1.47800299600006,5.2,4.07691356199999));
#301919=CARTESIAN_POINT('Ctrl Pts',(-1.47800299600006,2.2,4.07691356199999));
#301920=CARTESIAN_POINT('Ctrl Pts',(-1.47810135000006,12.2,4.07502253299998));
#301921=CARTESIAN_POINT('Ctrl Pts',(-1.47810135000006,5.2,4.07502253299998));
#301922=CARTESIAN_POINT('Ctrl Pts',(-1.47810135000006,2.2,4.07502253299998));
#301923=CARTESIAN_POINT('Ctrl Pts',(-1.47819737000006,12.2,4.07313559299999));
#301924=CARTESIAN_POINT('Ctrl Pts',(-1.47819737000006,5.2,4.07313559299999));
#301925=CARTESIAN_POINT('Ctrl Pts',(-1.47819737000006,2.2,4.07313559299999));
#301926=CARTESIAN_POINT('Ctrl Pts',(-1.47829106100006,12.2,4.07125274999999));
#301927=CARTESIAN_POINT('Ctrl Pts',(-1.47829106100006,5.2,4.07125274999999));
#301928=CARTESIAN_POINT('Ctrl Pts',(-1.47829106100006,2.2,4.07125274999999));
#301929=CARTESIAN_POINT('Ctrl Pts',(-1.47838243300006,12.2,4.06937401199999));
#301930=CARTESIAN_POINT('Ctrl Pts',(-1.47838243300006,5.2,4.06937401199999));
#301931=CARTESIAN_POINT('Ctrl Pts',(-1.47838243300006,2.2,4.06937401199999));
#301932=CARTESIAN_POINT('Ctrl Pts',(-1.47847149200006,12.2,4.06749938699999));
#301933=CARTESIAN_POINT('Ctrl Pts',(-1.47847149200006,5.2,4.06749938699999));
#301934=CARTESIAN_POINT('Ctrl Pts',(-1.47847149200006,2.2,4.06749938699999));
#301935=CARTESIAN_POINT('Ctrl Pts',(-1.47855825000006,12.2,4.06562888299998));
#301936=CARTESIAN_POINT('Ctrl Pts',(-1.47855825000006,5.2,4.06562888299998));
#301937=CARTESIAN_POINT('Ctrl Pts',(-1.47855825000006,2.2,4.06562888299998));
#301938=CARTESIAN_POINT('Ctrl Pts',(-1.47864271200006,12.2,4.06376250799998));
#301939=CARTESIAN_POINT('Ctrl Pts',(-1.47864271200006,5.2,4.06376250799998));
#301940=CARTESIAN_POINT('Ctrl Pts',(-1.47864271200006,2.2,4.06376250799998));
#301941=CARTESIAN_POINT('Ctrl Pts',(-1.47872488800005,12.2,4.06190026899999));
#301942=CARTESIAN_POINT('Ctrl Pts',(-1.47872488800005,5.2,4.06190026899999));
#301943=CARTESIAN_POINT('Ctrl Pts',(-1.47872488800005,2.2,4.06190026899999));
#301944=CARTESIAN_POINT('Ctrl Pts',(-1.47880478500006,12.2,4.06004217499999));
#301945=CARTESIAN_POINT('Ctrl Pts',(-1.47880478500006,5.2,4.06004217499999));
#301946=CARTESIAN_POINT('Ctrl Pts',(-1.47880478500006,2.2,4.06004217499999));
#301947=CARTESIAN_POINT('Ctrl Pts',(-1.47888241200006,12.2,4.05818823399999));
#301948=CARTESIAN_POINT('Ctrl Pts',(-1.47888241200006,5.2,4.05818823399999));
#301949=CARTESIAN_POINT('Ctrl Pts',(-1.47888241200006,2.2,4.05818823399999));
#301950=CARTESIAN_POINT('Ctrl Pts',(-1.47895777700006,12.2,4.05633845299998));
#301951=CARTESIAN_POINT('Ctrl Pts',(-1.47895777700006,5.2,4.05633845299998));
#301952=CARTESIAN_POINT('Ctrl Pts',(-1.47895777700006,2.2,4.05633845299998));
#301953=CARTESIAN_POINT('Ctrl Pts',(-1.47903088800006,12.2,4.05449284099999));
#301954=CARTESIAN_POINT('Ctrl Pts',(-1.47903088800006,5.2,4.05449284099999));
#301955=CARTESIAN_POINT('Ctrl Pts',(-1.47903088800006,2.2,4.05449284099999));
#301956=CARTESIAN_POINT('Ctrl Pts',(-1.47910175500006,12.2,4.05265140599998));
#301957=CARTESIAN_POINT('Ctrl Pts',(-1.47910175500006,5.2,4.05265140599998));
#301958=CARTESIAN_POINT('Ctrl Pts',(-1.47910175500006,2.2,4.05265140599998));
#301959=CARTESIAN_POINT('Ctrl Pts',(-1.47917038600006,12.2,4.05081415599999));
#301960=CARTESIAN_POINT('Ctrl Pts',(-1.47917038600006,5.2,4.05081415599999));
#301961=CARTESIAN_POINT('Ctrl Pts',(-1.47917038600006,2.2,4.05081415599999));
#301962=CARTESIAN_POINT('Ctrl Pts',(-1.47923678600006,12.2,4.04898109799999));
#301963=CARTESIAN_POINT('Ctrl Pts',(-1.47923678600006,5.2,4.04898109799999));
#301964=CARTESIAN_POINT('Ctrl Pts',(-1.47923678600006,2.2,4.04898109799999));
#301965=CARTESIAN_POINT('Ctrl Pts',(-1.47930096900006,12.2,4.04715224099998));
#301966=CARTESIAN_POINT('Ctrl Pts',(-1.47930096900006,5.2,4.04715224099998));
#301967=CARTESIAN_POINT('Ctrl Pts',(-1.47930096900006,2.2,4.04715224099998));
#301968=CARTESIAN_POINT('Ctrl Pts',(-1.47936293900006,12.2,4.04532759199999));
#301969=CARTESIAN_POINT('Ctrl Pts',(-1.47936293900006,5.2,4.04532759199999));
#301970=CARTESIAN_POINT('Ctrl Pts',(-1.47936293900006,2.2,4.04532759199999));
#301971=CARTESIAN_POINT('Ctrl Pts',(-1.47942270700006,12.2,4.04350715999998));
#301972=CARTESIAN_POINT('Ctrl Pts',(-1.47942270700006,5.2,4.04350715999998));
#301973=CARTESIAN_POINT('Ctrl Pts',(-1.47942270700006,2.2,4.04350715999998));
#301974=CARTESIAN_POINT('Ctrl Pts',(-1.47948028000006,12.2,4.04169095299999));
#301975=CARTESIAN_POINT('Ctrl Pts',(-1.47948028000006,5.2,4.04169095299999));
#301976=CARTESIAN_POINT('Ctrl Pts',(-1.47948028000006,2.2,4.04169095299999));
#301977=CARTESIAN_POINT('Ctrl Pts',(-1.47953566800005,12.2,4.03987897799999));
#301978=CARTESIAN_POINT('Ctrl Pts',(-1.47953566800005,5.2,4.03987897799999));
#301979=CARTESIAN_POINT('Ctrl Pts',(-1.47953566800005,2.2,4.03987897799999));
#301980=CARTESIAN_POINT('Ctrl Pts',(-1.47958887800006,12.2,4.03807124299998));
#301981=CARTESIAN_POINT('Ctrl Pts',(-1.47958887800006,5.2,4.03807124299998));
#301982=CARTESIAN_POINT('Ctrl Pts',(-1.47958887800006,2.2,4.03807124299998));
#301983=CARTESIAN_POINT('Ctrl Pts',(-1.47963992000006,12.2,4.03626775699998));
#301984=CARTESIAN_POINT('Ctrl Pts',(-1.47963992000006,5.2,4.03626775699998));
#301985=CARTESIAN_POINT('Ctrl Pts',(-1.47963992000006,2.2,4.03626775699998));
#301986=CARTESIAN_POINT('Ctrl Pts',(-1.47968880200006,12.2,4.03446852799998));
#301987=CARTESIAN_POINT('Ctrl Pts',(-1.47968880200006,5.2,4.03446852799998));
#301988=CARTESIAN_POINT('Ctrl Pts',(-1.47968880200006,2.2,4.03446852799998));
#301989=CARTESIAN_POINT('Ctrl Pts',(-1.47973553200006,12.2,4.03267356299998));
#301990=CARTESIAN_POINT('Ctrl Pts',(-1.47973553200006,5.2,4.03267356299998));
#301991=CARTESIAN_POINT('Ctrl Pts',(-1.47973553200006,2.2,4.03267356299998));
#301992=CARTESIAN_POINT('Ctrl Pts',(-1.47978012000006,12.2,4.03088287099998));
#301993=CARTESIAN_POINT('Ctrl Pts',(-1.47978012000006,5.2,4.03088287099998));
#301994=CARTESIAN_POINT('Ctrl Pts',(-1.47978012000006,2.2,4.03088287099998));
#301995=CARTESIAN_POINT('Ctrl Pts',(-1.47982257300006,12.2,4.02909645899998));
#301996=CARTESIAN_POINT('Ctrl Pts',(-1.47982257300006,5.2,4.02909645899998));
#301997=CARTESIAN_POINT('Ctrl Pts',(-1.47982257300006,2.2,4.02909645899998));
#301998=CARTESIAN_POINT('Ctrl Pts',(-1.47986290300006,12.2,4.02731433599998));
#301999=CARTESIAN_POINT('Ctrl Pts',(-1.47986290300006,5.2,4.02731433599998));
#302000=CARTESIAN_POINT('Ctrl Pts',(-1.47986290300006,2.2,4.02731433599998));
#302001=CARTESIAN_POINT('Ctrl Pts',(-1.47990111500006,12.2,4.02553650999998));
#302002=CARTESIAN_POINT('Ctrl Pts',(-1.47990111500006,5.2,4.02553650999998));
#302003=CARTESIAN_POINT('Ctrl Pts',(-1.47990111500006,2.2,4.02553650999998));
#302004=CARTESIAN_POINT('Ctrl Pts',(-1.47993722000006,12.2,4.02376298799999));
#302005=CARTESIAN_POINT('Ctrl Pts',(-1.47993722000006,5.2,4.02376298799999));
#302006=CARTESIAN_POINT('Ctrl Pts',(-1.47993722000006,2.2,4.02376298799999));
#302007=CARTESIAN_POINT('Ctrl Pts',(-1.47997122500006,12.2,4.02199377799998));
#302008=CARTESIAN_POINT('Ctrl Pts',(-1.47997122500006,5.2,4.02199377799998));
#302009=CARTESIAN_POINT('Ctrl Pts',(-1.47997122500006,2.2,4.02199377799998));
#302010=CARTESIAN_POINT('Ctrl Pts',(-1.48000314100006,12.2,4.02022888899998));
#302011=CARTESIAN_POINT('Ctrl Pts',(-1.48000314100006,5.2,4.02022888899998));
#302012=CARTESIAN_POINT('Ctrl Pts',(-1.48000314100006,2.2,4.02022888899998));
#302013=CARTESIAN_POINT('Ctrl Pts',(-1.48003297500006,12.2,4.01846832999999));
#302014=CARTESIAN_POINT('Ctrl Pts',(-1.48003297500006,5.2,4.01846832999999));
#302015=CARTESIAN_POINT('Ctrl Pts',(-1.48003297500006,2.2,4.01846832999999));
#302016=CARTESIAN_POINT('Ctrl Pts',(-1.48006073700006,12.2,4.01671210599999));
#302017=CARTESIAN_POINT('Ctrl Pts',(-1.48006073700006,5.2,4.01671210599999));
#302018=CARTESIAN_POINT('Ctrl Pts',(-1.48006073700006,2.2,4.01671210599999));
#302019=CARTESIAN_POINT('Ctrl Pts',(-1.48008643700006,12.2,4.01496022799999));
#302020=CARTESIAN_POINT('Ctrl Pts',(-1.48008643700006,5.2,4.01496022799999));
#302021=CARTESIAN_POINT('Ctrl Pts',(-1.48008643700006,2.2,4.01496022799999));
#302022=CARTESIAN_POINT('Ctrl Pts',(-1.48011008100006,12.2,4.01321270199999));
#302023=CARTESIAN_POINT('Ctrl Pts',(-1.48011008100006,5.2,4.01321270199999));
#302024=CARTESIAN_POINT('Ctrl Pts',(-1.48011008100006,2.2,4.01321270199999));
#302025=CARTESIAN_POINT('Ctrl Pts',(-1.48013168000006,12.2,4.01146953699998));
#302026=CARTESIAN_POINT('Ctrl Pts',(-1.48013168000006,5.2,4.01146953699998));
#302027=CARTESIAN_POINT('Ctrl Pts',(-1.48013168000006,2.2,4.01146953699998));
#302028=CARTESIAN_POINT('Ctrl Pts',(-1.48015124300006,12.2,4.00973074099999));
#302029=CARTESIAN_POINT('Ctrl Pts',(-1.48015124300006,5.2,4.00973074099999));
#302030=CARTESIAN_POINT('Ctrl Pts',(-1.48015124300006,2.2,4.00973074099999));
#302031=CARTESIAN_POINT('Ctrl Pts',(-1.48016877800006,12.2,4.00799632099999));
#302032=CARTESIAN_POINT('Ctrl Pts',(-1.48016877800006,5.2,4.00799632099999));
#302033=CARTESIAN_POINT('Ctrl Pts',(-1.48016877800006,2.2,4.00799632099999));
#302034=CARTESIAN_POINT('Ctrl Pts',(-1.48018429500006,12.2,4.00626628699998));
#302035=CARTESIAN_POINT('Ctrl Pts',(-1.48018429500006,5.2,4.00626628699998));
#302036=CARTESIAN_POINT('Ctrl Pts',(-1.48018429500006,2.2,4.00626628699998));
#302037=CARTESIAN_POINT('Ctrl Pts',(-1.48019780300006,12.2,4.00454064499999));
#302038=CARTESIAN_POINT('Ctrl Pts',(-1.48019780300006,5.2,4.00454064499999));
#302039=CARTESIAN_POINT('Ctrl Pts',(-1.48019780300006,2.2,4.00454064499999));
#302040=CARTESIAN_POINT('Ctrl Pts',(-1.48020931000006,12.2,4.00281940399999));
#302041=CARTESIAN_POINT('Ctrl Pts',(-1.48020931000006,5.2,4.00281940399999));
#302042=CARTESIAN_POINT('Ctrl Pts',(-1.48020931000006,2.2,4.00281940399999));
#302043=CARTESIAN_POINT('Ctrl Pts',(-1.48021882600006,12.2,4.00110257199999));
#302044=CARTESIAN_POINT('Ctrl Pts',(-1.48021882600006,5.2,4.00110257199999));
#302045=CARTESIAN_POINT('Ctrl Pts',(-1.48021882600006,2.2,4.00110257199999));
#302046=CARTESIAN_POINT('Ctrl Pts',(-1.48022636200006,12.2,3.99939015799998));
#302047=CARTESIAN_POINT('Ctrl Pts',(-1.48022636200006,5.2,3.99939015799998));
#302048=CARTESIAN_POINT('Ctrl Pts',(-1.48022636200006,2.2,3.99939015799998));
#302049=CARTESIAN_POINT('Ctrl Pts',(-1.48023192300006,12.2,3.99768216799998));
#302050=CARTESIAN_POINT('Ctrl Pts',(-1.48023192300006,5.2,3.99768216799998));
#302051=CARTESIAN_POINT('Ctrl Pts',(-1.48023192300006,2.2,3.99768216799998));
#302052=CARTESIAN_POINT('Ctrl Pts',(-1.48023552100006,12.2,3.99597861199998));
#302053=CARTESIAN_POINT('Ctrl Pts',(-1.48023552100006,5.2,3.99597861199998));
#302054=CARTESIAN_POINT('Ctrl Pts',(-1.48023552100006,2.2,3.99597861199998));
#302055=CARTESIAN_POINT('Ctrl Pts',(-1.48023716600005,12.2,3.99427949599998));
#302056=CARTESIAN_POINT('Ctrl Pts',(-1.48023716600005,5.2,3.99427949599998));
#302057=CARTESIAN_POINT('Ctrl Pts',(-1.48023716600005,2.2,3.99427949599998));
#302058=CARTESIAN_POINT('Ctrl Pts',(-1.48023686500006,12.2,3.99258482999999));
#302059=CARTESIAN_POINT('Ctrl Pts',(-1.48023686500006,5.2,3.99258482999999));
#302060=CARTESIAN_POINT('Ctrl Pts',(-1.48023686500006,2.2,3.99258482999999));
#302061=CARTESIAN_POINT('Ctrl Pts',(-1.48023462900006,12.2,3.99089462199999));
#302062=CARTESIAN_POINT('Ctrl Pts',(-1.48023462900006,5.2,3.99089462199999));
#302063=CARTESIAN_POINT('Ctrl Pts',(-1.48023462900006,2.2,3.99089462199999));
#302064=CARTESIAN_POINT('Ctrl Pts',(-1.48023046600006,12.2,3.98920887799999));
#302065=CARTESIAN_POINT('Ctrl Pts',(-1.48023046600006,5.2,3.98920887799999));
#302066=CARTESIAN_POINT('Ctrl Pts',(-1.48023046600006,2.2,3.98920887799999));
#302067=CARTESIAN_POINT('Ctrl Pts',(-1.48022438700006,12.2,3.98752760799999));
#302068=CARTESIAN_POINT('Ctrl Pts',(-1.48022438700006,5.2,3.98752760799999));
#302069=CARTESIAN_POINT('Ctrl Pts',(-1.48022438700006,2.2,3.98752760799999));
#302070=CARTESIAN_POINT('Ctrl Pts',(-1.48021639900006,12.2,3.98585081899999));
#302071=CARTESIAN_POINT('Ctrl Pts',(-1.48021639900006,5.2,3.98585081899999));
#302072=CARTESIAN_POINT('Ctrl Pts',(-1.48021639900006,2.2,3.98585081899999));
#302073=CARTESIAN_POINT('Ctrl Pts',(-1.48020651400006,12.2,3.98417852099998));
#302074=CARTESIAN_POINT('Ctrl Pts',(-1.48020651400006,5.2,3.98417852099998));
#302075=CARTESIAN_POINT('Ctrl Pts',(-1.48020651400006,2.2,3.98417852099998));
#302076=CARTESIAN_POINT('Ctrl Pts',(-1.48019474000006,12.2,3.98251071999999));
#302077=CARTESIAN_POINT('Ctrl Pts',(-1.48019474000006,5.2,3.98251071999999));
#302078=CARTESIAN_POINT('Ctrl Pts',(-1.48019474000006,2.2,3.98251071999999));
#302079=CARTESIAN_POINT('Ctrl Pts',(-1.48018108700006,12.2,3.98084742399998));
#302080=CARTESIAN_POINT('Ctrl Pts',(-1.48018108700006,5.2,3.98084742399998));
#302081=CARTESIAN_POINT('Ctrl Pts',(-1.48018108700006,2.2,3.98084742399998));
#302082=CARTESIAN_POINT('Ctrl Pts',(-1.48016556400006,12.2,3.97918864299999));
#302083=CARTESIAN_POINT('Ctrl Pts',(-1.48016556400006,5.2,3.97918864299999));
#302084=CARTESIAN_POINT('Ctrl Pts',(-1.48016556400006,2.2,3.97918864299999));
#302085=CARTESIAN_POINT('Ctrl Pts',(-1.48014818000005,12.2,3.97753438199998));
#302086=CARTESIAN_POINT('Ctrl Pts',(-1.48014818000005,5.2,3.97753438199998));
#302087=CARTESIAN_POINT('Ctrl Pts',(-1.48014818000005,2.2,3.97753438199998));
#302088=CARTESIAN_POINT('Ctrl Pts',(-1.48012894600006,12.2,3.97588465299999));
#302089=CARTESIAN_POINT('Ctrl Pts',(-1.48012894600006,5.2,3.97588465299999));
#302090=CARTESIAN_POINT('Ctrl Pts',(-1.48012894600006,2.2,3.97588465299999));
#302091=CARTESIAN_POINT('Ctrl Pts',(-1.48010787200006,12.2,3.97423945999999));
#302092=CARTESIAN_POINT('Ctrl Pts',(-1.48010787200006,5.2,3.97423945999999));
#302093=CARTESIAN_POINT('Ctrl Pts',(-1.48010787200006,2.2,3.97423945999999));
#302094=CARTESIAN_POINT('Ctrl Pts',(-1.48008496500006,12.2,3.97259881399999));
#302095=CARTESIAN_POINT('Ctrl Pts',(-1.48008496500006,5.2,3.97259881399999));
#302096=CARTESIAN_POINT('Ctrl Pts',(-1.48008496500006,2.2,3.97259881399999));
#302097=CARTESIAN_POINT('Ctrl Pts',(-1.48006023600006,12.2,3.97096272199998));
#302098=CARTESIAN_POINT('Ctrl Pts',(-1.48006023600006,5.2,3.97096272199998));
#302099=CARTESIAN_POINT('Ctrl Pts',(-1.48006023600006,2.2,3.97096272199998));
#302100=CARTESIAN_POINT('Ctrl Pts',(-1.48003369600006,12.2,3.96933119299998));
#302101=CARTESIAN_POINT('Ctrl Pts',(-1.48003369600006,5.2,3.96933119299998));
#302102=CARTESIAN_POINT('Ctrl Pts',(-1.48003369600006,2.2,3.96933119299998));
#302103=CARTESIAN_POINT('Ctrl Pts',(-1.48000535300006,12.2,3.96770423299999));
#302104=CARTESIAN_POINT('Ctrl Pts',(-1.48000535300006,5.2,3.96770423299999));
#302105=CARTESIAN_POINT('Ctrl Pts',(-1.48000535300006,2.2,3.96770423299999));
#302106=CARTESIAN_POINT('Ctrl Pts',(-1.47997521700006,12.2,3.96608185299999));
#302107=CARTESIAN_POINT('Ctrl Pts',(-1.47997521700006,5.2,3.96608185299999));
#302108=CARTESIAN_POINT('Ctrl Pts',(-1.47997521700006,2.2,3.96608185299999));
#302109=CARTESIAN_POINT('Ctrl Pts',(-1.47994329900005,12.2,3.96446405799999));
#302110=CARTESIAN_POINT('Ctrl Pts',(-1.47994329900005,5.2,3.96446405799999));
#302111=CARTESIAN_POINT('Ctrl Pts',(-1.47994329900005,2.2,3.96446405799999));
#302112=CARTESIAN_POINT('Ctrl Pts',(-1.47990960800006,12.2,3.96285085899999));
#302113=CARTESIAN_POINT('Ctrl Pts',(-1.47990960800006,5.2,3.96285085899999));
#302114=CARTESIAN_POINT('Ctrl Pts',(-1.47990960800006,2.2,3.96285085899999));
#302115=CARTESIAN_POINT('Ctrl Pts',(-1.47987415200006,12.2,3.96124226199999));
#302116=CARTESIAN_POINT('Ctrl Pts',(-1.47987415200006,5.2,3.96124226199999));
#302117=CARTESIAN_POINT('Ctrl Pts',(-1.47987415200006,2.2,3.96124226199999));
#302118=CARTESIAN_POINT('Ctrl Pts',(-1.47983694400006,12.2,3.95963827599999));
#302119=CARTESIAN_POINT('Ctrl Pts',(-1.47983694400006,5.2,3.95963827599999));
#302120=CARTESIAN_POINT('Ctrl Pts',(-1.47983694400006,2.2,3.95963827599999));
#302121=CARTESIAN_POINT('Ctrl Pts',(-1.47979799200006,12.2,3.95803890899998));
#302122=CARTESIAN_POINT('Ctrl Pts',(-1.47979799200006,5.2,3.95803890899998));
#302123=CARTESIAN_POINT('Ctrl Pts',(-1.47979799200006,2.2,3.95803890899998));
#302124=CARTESIAN_POINT('Ctrl Pts',(-1.47975730600006,12.2,3.95644416899999));
#302125=CARTESIAN_POINT('Ctrl Pts',(-1.47975730600006,5.2,3.95644416899999));
#302126=CARTESIAN_POINT('Ctrl Pts',(-1.47975730600006,2.2,3.95644416899999));
#302127=CARTESIAN_POINT('Ctrl Pts',(-1.47971489600006,12.2,3.95485406399998));
#302128=CARTESIAN_POINT('Ctrl Pts',(-1.47971489600006,5.2,3.95485406399998));
#302129=CARTESIAN_POINT('Ctrl Pts',(-1.47971489600006,2.2,3.95485406399998));
#302130=CARTESIAN_POINT('Ctrl Pts',(-1.47967077300006,12.2,3.95326860199999));
#302131=CARTESIAN_POINT('Ctrl Pts',(-1.47967077300006,5.2,3.95326860199999));
#302132=CARTESIAN_POINT('Ctrl Pts',(-1.47967077300006,2.2,3.95326860199999));
#302133=CARTESIAN_POINT('Ctrl Pts',(-1.47962494700006,12.2,3.95168779099999));
#302134=CARTESIAN_POINT('Ctrl Pts',(-1.47962494700006,5.2,3.95168779099999));
#302135=CARTESIAN_POINT('Ctrl Pts',(-1.47962494700006,2.2,3.95168779099999));
#302136=CARTESIAN_POINT('Ctrl Pts',(-1.47957742600005,12.2,3.95011164099999));
#302137=CARTESIAN_POINT('Ctrl Pts',(-1.47957742600005,5.2,3.95011164099999));
#302138=CARTESIAN_POINT('Ctrl Pts',(-1.47957742600005,2.2,3.95011164099999));
#302139=CARTESIAN_POINT('Ctrl Pts',(-1.47952822100006,12.2,3.94854015799999));
#302140=CARTESIAN_POINT('Ctrl Pts',(-1.47952822100006,5.2,3.94854015799999));
#302141=CARTESIAN_POINT('Ctrl Pts',(-1.47952822100006,2.2,3.94854015799999));
#302142=CARTESIAN_POINT('Ctrl Pts',(-1.47947734300006,12.2,3.94697334999999));
#302143=CARTESIAN_POINT('Ctrl Pts',(-1.47947734300006,5.2,3.94697334999999));
#302144=CARTESIAN_POINT('Ctrl Pts',(-1.47947734300006,2.2,3.94697334999999));
#302145=CARTESIAN_POINT('Ctrl Pts',(-1.47942480100006,12.2,3.94541122599998));
#302146=CARTESIAN_POINT('Ctrl Pts',(-1.47942480100006,5.2,3.94541122599998));
#302147=CARTESIAN_POINT('Ctrl Pts',(-1.47942480100006,2.2,3.94541122599998));
#302148=CARTESIAN_POINT('Ctrl Pts',(-1.47937060600006,12.2,3.94385379399999));
#302149=CARTESIAN_POINT('Ctrl Pts',(-1.47937060600006,5.2,3.94385379399999));
#302150=CARTESIAN_POINT('Ctrl Pts',(-1.47937060600006,2.2,3.94385379399999));
#302151=CARTESIAN_POINT('Ctrl Pts',(-1.47931476800006,12.2,3.94230106299998));
#302152=CARTESIAN_POINT('Ctrl Pts',(-1.47931476800006,5.2,3.94230106299998));
#302153=CARTESIAN_POINT('Ctrl Pts',(-1.47931476800006,2.2,3.94230106299998));
#302154=CARTESIAN_POINT('Ctrl Pts',(-1.47925729700006,12.2,3.94075303899999));
#302155=CARTESIAN_POINT('Ctrl Pts',(-1.47925729700006,5.2,3.94075303899999));
#302156=CARTESIAN_POINT('Ctrl Pts',(-1.47925729700006,2.2,3.94075303899999));
#302157=CARTESIAN_POINT('Ctrl Pts',(-1.47919820300006,12.2,3.93920973199998));
#302158=CARTESIAN_POINT('Ctrl Pts',(-1.47919820300006,5.2,3.93920973199998));
#302159=CARTESIAN_POINT('Ctrl Pts',(-1.47919820300006,2.2,3.93920973199998));
#302160=CARTESIAN_POINT('Ctrl Pts',(-1.47913749800006,12.2,3.93767114899998));
#302161=CARTESIAN_POINT('Ctrl Pts',(-1.47913749800006,5.2,3.93767114899998));
#302162=CARTESIAN_POINT('Ctrl Pts',(-1.47913749800006,2.2,3.93767114899998));
#302163=CARTESIAN_POINT('Ctrl Pts',(-1.47907519000006,12.2,3.93613729899998));
#302164=CARTESIAN_POINT('Ctrl Pts',(-1.47907519000006,5.2,3.93613729899998));
#302165=CARTESIAN_POINT('Ctrl Pts',(-1.47907519000006,2.2,3.93613729899998));
#302166=CARTESIAN_POINT('Ctrl Pts',(-1.47901129000006,12.2,3.93460818899998));
#302167=CARTESIAN_POINT('Ctrl Pts',(-1.47901129000006,5.2,3.93460818899998));
#302168=CARTESIAN_POINT('Ctrl Pts',(-1.47901129000006,2.2,3.93460818899998));
#302169=CARTESIAN_POINT('Ctrl Pts',(-1.47894580800006,12.2,3.93308382899999));
#302170=CARTESIAN_POINT('Ctrl Pts',(-1.47894580800006,5.2,3.93308382899999));
#302171=CARTESIAN_POINT('Ctrl Pts',(-1.47894580800006,2.2,3.93308382899999));
#302172=CARTESIAN_POINT('Ctrl Pts',(-1.47887875600005,12.2,3.93156422499998));
#302173=CARTESIAN_POINT('Ctrl Pts',(-1.47887875600005,5.2,3.93156422499998));
#302174=CARTESIAN_POINT('Ctrl Pts',(-1.47887875600005,2.2,3.93156422499998));
#302175=CARTESIAN_POINT('Ctrl Pts',(-1.47881014300006,12.2,3.93004938699999));
#302176=CARTESIAN_POINT('Ctrl Pts',(-1.47881014300006,5.2,3.93004938699999));
#302177=CARTESIAN_POINT('Ctrl Pts',(-1.47881014300006,2.2,3.93004938699999));
#302178=CARTESIAN_POINT('Ctrl Pts',(-1.47873998000006,12.2,3.92853932199999));
#302179=CARTESIAN_POINT('Ctrl Pts',(-1.47873998000006,5.2,3.92853932199999));
#302180=CARTESIAN_POINT('Ctrl Pts',(-1.47873998000006,2.2,3.92853932199999));
#302181=CARTESIAN_POINT('Ctrl Pts',(-1.47866827700006,12.2,3.92703403799998));
#302182=CARTESIAN_POINT('Ctrl Pts',(-1.47866827700006,5.2,3.92703403799998));
#302183=CARTESIAN_POINT('Ctrl Pts',(-1.47866827700006,2.2,3.92703403799998));
#302184=CARTESIAN_POINT('Ctrl Pts',(-1.47859504600006,12.2,3.92553354499999));
#302185=CARTESIAN_POINT('Ctrl Pts',(-1.47859504600006,5.2,3.92553354499999));
#302186=CARTESIAN_POINT('Ctrl Pts',(-1.47859504600006,2.2,3.92553354499999));
#302187=CARTESIAN_POINT('Ctrl Pts',(-1.47852029600006,12.2,3.92403784899999));
#302188=CARTESIAN_POINT('Ctrl Pts',(-1.47852029600006,5.2,3.92403784899999));
#302189=CARTESIAN_POINT('Ctrl Pts',(-1.47852029600006,2.2,3.92403784899999));
#302190=CARTESIAN_POINT('Ctrl Pts',(-1.47844403800006,12.2,3.92254695799998));
#302191=CARTESIAN_POINT('Ctrl Pts',(-1.47844403800006,5.2,3.92254695799998));
#302192=CARTESIAN_POINT('Ctrl Pts',(-1.47844403800006,2.2,3.92254695799998));
#302193=CARTESIAN_POINT('Ctrl Pts',(-1.47836628300006,12.2,3.92106088199998));
#302194=CARTESIAN_POINT('Ctrl Pts',(-1.47836628300006,5.2,3.92106088199998));
#302195=CARTESIAN_POINT('Ctrl Pts',(-1.47836628300006,2.2,3.92106088199998));
#302196=CARTESIAN_POINT('Ctrl Pts',(-1.47828704000006,12.2,3.91957962799999));
#302197=CARTESIAN_POINT('Ctrl Pts',(-1.47828704000006,5.2,3.91957962799999));
#302198=CARTESIAN_POINT('Ctrl Pts',(-1.47828704000006,2.2,3.91957962799999));
#302199=CARTESIAN_POINT('Ctrl Pts',(-1.47820632300006,12.2,3.91810320499999));
#302200=CARTESIAN_POINT('Ctrl Pts',(-1.47820632300006,5.2,3.91810320499999));
#302201=CARTESIAN_POINT('Ctrl Pts',(-1.47820632300006,2.2,3.91810320499999));
#302202=CARTESIAN_POINT('Ctrl Pts',(-1.47812414000006,12.2,3.91663161999999));
#302203=CARTESIAN_POINT('Ctrl Pts',(-1.47812414000006,5.2,3.91663161999999));
#302204=CARTESIAN_POINT('Ctrl Pts',(-1.47812414000006,2.2,3.91663161999999));
#302205=CARTESIAN_POINT('Ctrl Pts',(-1.47804050300006,12.2,3.91516488099998));
#302206=CARTESIAN_POINT('Ctrl Pts',(-1.47804050300006,5.2,3.91516488099998));
#302207=CARTESIAN_POINT('Ctrl Pts',(-1.47804050300006,2.2,3.91516488099998));
#302208=CARTESIAN_POINT('Ctrl Pts',(-1.47795542200006,12.2,3.91370299799998));
#302209=CARTESIAN_POINT('Ctrl Pts',(-1.47795542200006,5.2,3.91370299799998));
#302210=CARTESIAN_POINT('Ctrl Pts',(-1.47795542200006,2.2,3.91370299799998));
#302211=CARTESIAN_POINT('Ctrl Pts',(-1.47786890800006,12.2,3.91224597799999));
#302212=CARTESIAN_POINT('Ctrl Pts',(-1.47786890800006,5.2,3.91224597799999));
#302213=CARTESIAN_POINT('Ctrl Pts',(-1.47786890800006,2.2,3.91224597799999));
#302214=CARTESIAN_POINT('Ctrl Pts',(-1.47778097200006,12.2,3.91079382799998));
#302215=CARTESIAN_POINT('Ctrl Pts',(-1.47778097200006,5.2,3.91079382799998));
#302216=CARTESIAN_POINT('Ctrl Pts',(-1.47778097200006,2.2,3.91079382799998));
#302217=CARTESIAN_POINT('Ctrl Pts',(-1.47769162500005,12.2,3.90934655899999));
#302218=CARTESIAN_POINT('Ctrl Pts',(-1.47769162500005,5.2,3.90934655899999));
#302219=CARTESIAN_POINT('Ctrl Pts',(-1.47769162500005,2.2,3.90934655899999));
#302220=CARTESIAN_POINT('Ctrl Pts',(-1.47760087800005,12.2,3.90790417599998));
#302221=CARTESIAN_POINT('Ctrl Pts',(-1.47760087800005,5.2,3.90790417599998));
#302222=CARTESIAN_POINT('Ctrl Pts',(-1.47760087800005,2.2,3.90790417599998));
#302223=CARTESIAN_POINT('Ctrl Pts',(-1.47750874100006,12.2,3.90646668999998));
#302224=CARTESIAN_POINT('Ctrl Pts',(-1.47750874100006,5.2,3.90646668999998));
#302225=CARTESIAN_POINT('Ctrl Pts',(-1.47750874100006,2.2,3.90646668999998));
#302226=CARTESIAN_POINT('Ctrl Pts',(-1.47741522700006,12.2,3.90503410799998));
#302227=CARTESIAN_POINT('Ctrl Pts',(-1.47741522700006,5.2,3.90503410799998));
#302228=CARTESIAN_POINT('Ctrl Pts',(-1.47741522700006,2.2,3.90503410799998));
#302229=CARTESIAN_POINT('Ctrl Pts',(-1.47732034500006,12.2,3.90360643799998));
#302230=CARTESIAN_POINT('Ctrl Pts',(-1.47732034500006,5.2,3.90360643799998));
#302231=CARTESIAN_POINT('Ctrl Pts',(-1.47732034500006,2.2,3.90360643799998));
#302232=CARTESIAN_POINT('Ctrl Pts',(-1.47722410700006,12.2,3.90218368799999));
#302233=CARTESIAN_POINT('Ctrl Pts',(-1.47722410700006,5.2,3.90218368799999));
#302234=CARTESIAN_POINT('Ctrl Pts',(-1.47722410700006,2.2,3.90218368799999));
#302235=CARTESIAN_POINT('Ctrl Pts',(-1.47712652400006,12.2,3.90076586599999));
#302236=CARTESIAN_POINT('Ctrl Pts',(-1.47712652400006,5.2,3.90076586599999));
#302237=CARTESIAN_POINT('Ctrl Pts',(-1.47712652400006,2.2,3.90076586599999));
#302238=CARTESIAN_POINT('Ctrl Pts',(-1.47702760700006,12.2,3.89935298299999));
#302239=CARTESIAN_POINT('Ctrl Pts',(-1.47702760700006,5.2,3.89935298299999));
#302240=CARTESIAN_POINT('Ctrl Pts',(-1.47702760700006,2.2,3.89935298299999));
#302241=CARTESIAN_POINT('Ctrl Pts',(-1.47692736800005,12.2,3.89794504199998));
#302242=CARTESIAN_POINT('Ctrl Pts',(-1.47692736800005,5.2,3.89794504199998));
#302243=CARTESIAN_POINT('Ctrl Pts',(-1.47692736800005,2.2,3.89794504199998));
#302244=CARTESIAN_POINT('Ctrl Pts',(-1.47682581600006,12.2,3.89654205599999));
#302245=CARTESIAN_POINT('Ctrl Pts',(-1.47682581600006,5.2,3.89654205599999));
#302246=CARTESIAN_POINT('Ctrl Pts',(-1.47682581600006,2.2,3.89654205599999));
#302247=CARTESIAN_POINT('Ctrl Pts',(-1.47672296500006,12.2,3.89514403099999));
#302248=CARTESIAN_POINT('Ctrl Pts',(-1.47672296500006,5.2,3.89514403099999));
#302249=CARTESIAN_POINT('Ctrl Pts',(-1.47672296500006,2.2,3.89514403099999));
#302250=CARTESIAN_POINT('Ctrl Pts',(-1.47661882400006,12.2,3.89375097499999));
#302251=CARTESIAN_POINT('Ctrl Pts',(-1.47661882400006,5.2,3.89375097499999));
#302252=CARTESIAN_POINT('Ctrl Pts',(-1.47661882400006,2.2,3.89375097499999));
#302253=CARTESIAN_POINT('Ctrl Pts',(-1.47651340600006,12.2,3.89236289699999));
#302254=CARTESIAN_POINT('Ctrl Pts',(-1.47651340600006,5.2,3.89236289699999));
#302255=CARTESIAN_POINT('Ctrl Pts',(-1.47651340600006,2.2,3.89236289699999));
#302256=CARTESIAN_POINT('Ctrl Pts',(-1.47640672200006,12.2,3.89097980499999));
#302257=CARTESIAN_POINT('Ctrl Pts',(-1.47640672200006,5.2,3.89097980499999));
#302258=CARTESIAN_POINT('Ctrl Pts',(-1.47640672200006,2.2,3.89097980499999));
#302259=CARTESIAN_POINT('Ctrl Pts',(-1.47629878100005,12.2,3.88960170699999));
#302260=CARTESIAN_POINT('Ctrl Pts',(-1.47629878100005,5.2,3.88960170699999));
#302261=CARTESIAN_POINT('Ctrl Pts',(-1.47629878100005,2.2,3.88960170699999));
#302262=CARTESIAN_POINT('Ctrl Pts',(-1.47618959800006,12.2,3.88822861099998));
#302263=CARTESIAN_POINT('Ctrl Pts',(-1.47618959800006,5.2,3.88822861099998));
#302264=CARTESIAN_POINT('Ctrl Pts',(-1.47618959800006,2.2,3.88822861099998));
#302265=CARTESIAN_POINT('Ctrl Pts',(-1.47607918100006,12.2,3.88686052599999));
#302266=CARTESIAN_POINT('Ctrl Pts',(-1.47607918100006,5.2,3.88686052599999));
#302267=CARTESIAN_POINT('Ctrl Pts',(-1.47607918100006,2.2,3.88686052599999));
#302268=CARTESIAN_POINT('Ctrl Pts',(-1.47596754500006,12.2,3.88549745999998));
#302269=CARTESIAN_POINT('Ctrl Pts',(-1.47596754500006,5.2,3.88549745999998));
#302270=CARTESIAN_POINT('Ctrl Pts',(-1.47596754500006,2.2,3.88549745999998));
#302271=CARTESIAN_POINT('Ctrl Pts',(-1.47585469900006,12.2,3.88413941999998));
#302272=CARTESIAN_POINT('Ctrl Pts',(-1.47585469900006,5.2,3.88413941999998));
#302273=CARTESIAN_POINT('Ctrl Pts',(-1.47585469900006,2.2,3.88413941999998));
#302274=CARTESIAN_POINT('Ctrl Pts',(-1.47574065500006,12.2,3.88278641599998));
#302275=CARTESIAN_POINT('Ctrl Pts',(-1.47574065500006,5.2,3.88278641599998));
#302276=CARTESIAN_POINT('Ctrl Pts',(-1.47574065500006,2.2,3.88278641599998));
#302277=CARTESIAN_POINT('Ctrl Pts',(-1.47562542500006,12.2,3.88143845599998));
#302278=CARTESIAN_POINT('Ctrl Pts',(-1.47562542500006,5.2,3.88143845599998));
#302279=CARTESIAN_POINT('Ctrl Pts',(-1.47562542500006,2.2,3.88143845599998));
#302280=CARTESIAN_POINT('Ctrl Pts',(-1.47550902100006,12.2,3.88009554599999));
#302281=CARTESIAN_POINT('Ctrl Pts',(-1.47550902100006,5.2,3.88009554599999));
#302282=CARTESIAN_POINT('Ctrl Pts',(-1.47550902100006,2.2,3.88009554599999));
#302283=CARTESIAN_POINT('Ctrl Pts',(-1.47539145400006,12.2,3.87875769699999));
#302284=CARTESIAN_POINT('Ctrl Pts',(-1.47539145400006,5.2,3.87875769699999));
#302285=CARTESIAN_POINT('Ctrl Pts',(-1.47539145400006,2.2,3.87875769699999));
#302286=CARTESIAN_POINT('Ctrl Pts',(-1.47527273500006,12.2,3.87742491599998));
#302287=CARTESIAN_POINT('Ctrl Pts',(-1.47527273500006,5.2,3.87742491599998));
#302288=CARTESIAN_POINT('Ctrl Pts',(-1.47527273500006,2.2,3.87742491599998));
#302289=CARTESIAN_POINT('Ctrl Pts',(-1.47515287800006,12.2,3.87609721099999));
#302290=CARTESIAN_POINT('Ctrl Pts',(-1.47515287800006,5.2,3.87609721099999));
#302291=CARTESIAN_POINT('Ctrl Pts',(-1.47515287800006,2.2,3.87609721099999));
#302292=CARTESIAN_POINT('Ctrl Pts',(-1.47503189200005,12.2,3.87477459099999));
#302293=CARTESIAN_POINT('Ctrl Pts',(-1.47503189200005,5.2,3.87477459099999));
#302294=CARTESIAN_POINT('Ctrl Pts',(-1.47503189200005,2.2,3.87477459099999));
#302295=CARTESIAN_POINT('Ctrl Pts',(-1.47490979000006,12.2,3.87345706399999));
#302296=CARTESIAN_POINT('Ctrl Pts',(-1.47490979000006,5.2,3.87345706399999));
#302297=CARTESIAN_POINT('Ctrl Pts',(-1.47490979000006,2.2,3.87345706399999));
#302298=CARTESIAN_POINT('Ctrl Pts',(-1.47478658500006,12.2,3.87214463699999));
#302299=CARTESIAN_POINT('Ctrl Pts',(-1.47478658500006,5.2,3.87214463699999));
#302300=CARTESIAN_POINT('Ctrl Pts',(-1.47478658500006,2.2,3.87214463699999));
#302301=CARTESIAN_POINT('Ctrl Pts',(-1.47466228700006,12.2,3.87083732099998));
#302302=CARTESIAN_POINT('Ctrl Pts',(-1.47466228700006,5.2,3.87083732099998));
#302303=CARTESIAN_POINT('Ctrl Pts',(-1.47466228700006,2.2,3.87083732099998));
#302304=CARTESIAN_POINT('Ctrl Pts',(-1.47453690800006,12.2,3.86953512199998));
#302305=CARTESIAN_POINT('Ctrl Pts',(-1.47453690800006,5.2,3.86953512199998));
#302306=CARTESIAN_POINT('Ctrl Pts',(-1.47453690800006,2.2,3.86953512199998));
#302307=CARTESIAN_POINT('Ctrl Pts',(-1.47441046100006,12.2,3.86823804799998));
#302308=CARTESIAN_POINT('Ctrl Pts',(-1.47441046100006,5.2,3.86823804799998));
#302309=CARTESIAN_POINT('Ctrl Pts',(-1.47441046100006,2.2,3.86823804799998));
#302310=CARTESIAN_POINT('Ctrl Pts',(-1.47428295900006,12.2,3.86694610899998));
#302311=CARTESIAN_POINT('Ctrl Pts',(-1.47428295900006,5.2,3.86694610899998));
#302312=CARTESIAN_POINT('Ctrl Pts',(-1.47428295900006,2.2,3.86694610899998));
#302313=CARTESIAN_POINT('Ctrl Pts',(-1.47415441200006,12.2,3.86565931099998));
#302314=CARTESIAN_POINT('Ctrl Pts',(-1.47415441200006,5.2,3.86565931099998));
#302315=CARTESIAN_POINT('Ctrl Pts',(-1.47415441200006,2.2,3.86565931099998));
#302316=CARTESIAN_POINT('Ctrl Pts',(-1.47402483300006,12.2,3.86437766499999));
#302317=CARTESIAN_POINT('Ctrl Pts',(-1.47402483300006,5.2,3.86437766499999));
#302318=CARTESIAN_POINT('Ctrl Pts',(-1.47402483300006,2.2,3.86437766499999));
#302319=CARTESIAN_POINT('Ctrl Pts',(-1.47389423200006,12.2,3.86310117799999));
#302320=CARTESIAN_POINT('Ctrl Pts',(-1.47389423200006,5.2,3.86310117799999));
#302321=CARTESIAN_POINT('Ctrl Pts',(-1.47389423200006,2.2,3.86310117799999));
#302322=CARTESIAN_POINT('Ctrl Pts',(-1.47376262400006,12.2,3.86182985599999));
#302323=CARTESIAN_POINT('Ctrl Pts',(-1.47376262400006,5.2,3.86182985599999));
#302324=CARTESIAN_POINT('Ctrl Pts',(-1.47376262400006,2.2,3.86182985599999));
#302325=CARTESIAN_POINT('Ctrl Pts',(-1.47363002000006,12.2,3.86056371099999));
#302326=CARTESIAN_POINT('Ctrl Pts',(-1.47363002000006,5.2,3.86056371099999));
#302327=CARTESIAN_POINT('Ctrl Pts',(-1.47363002000006,2.2,3.86056371099999));
#302328=CARTESIAN_POINT('Ctrl Pts',(-1.47349643200006,12.2,3.85930274899999));
#302329=CARTESIAN_POINT('Ctrl Pts',(-1.47349643200006,5.2,3.85930274899999));
#302330=CARTESIAN_POINT('Ctrl Pts',(-1.47349643200006,2.2,3.85930274899999));
#302331=CARTESIAN_POINT('Ctrl Pts',(-1.47336187400006,12.2,3.85804697899999));
#302332=CARTESIAN_POINT('Ctrl Pts',(-1.47336187400006,5.2,3.85804697899999));
#302333=CARTESIAN_POINT('Ctrl Pts',(-1.47336187400006,2.2,3.85804697899999));
#302334=CARTESIAN_POINT('Ctrl Pts',(-1.47322635500006,12.2,3.85679640999999));
#302335=CARTESIAN_POINT('Ctrl Pts',(-1.47322635500006,5.2,3.85679640999999));
#302336=CARTESIAN_POINT('Ctrl Pts',(-1.47322635500006,2.2,3.85679640999999));
#302337=CARTESIAN_POINT('Ctrl Pts',(-1.47308989000006,12.2,3.85555104799998));
#302338=CARTESIAN_POINT('Ctrl Pts',(-1.47308989000006,5.2,3.85555104799998));
#302339=CARTESIAN_POINT('Ctrl Pts',(-1.47308989000006,2.2,3.85555104799998));
#302340=CARTESIAN_POINT('Ctrl Pts',(-1.47295249000006,12.2,3.85431090299999));
#302341=CARTESIAN_POINT('Ctrl Pts',(-1.47295249000006,5.2,3.85431090299999));
#302342=CARTESIAN_POINT('Ctrl Pts',(-1.47295249000006,2.2,3.85431090299999));
#302343=CARTESIAN_POINT('Ctrl Pts',(-1.47281416900006,12.2,3.85307598399999));
#302344=CARTESIAN_POINT('Ctrl Pts',(-1.47281416900006,5.2,3.85307598399999));
#302345=CARTESIAN_POINT('Ctrl Pts',(-1.47281416900006,2.2,3.85307598399999));
#302346=CARTESIAN_POINT('Ctrl Pts',(-1.47267493700006,12.2,3.85184629699998));
#302347=CARTESIAN_POINT('Ctrl Pts',(-1.47267493700006,5.2,3.85184629699998));
#302348=CARTESIAN_POINT('Ctrl Pts',(-1.47267493700006,2.2,3.85184629699998));
#302349=CARTESIAN_POINT('Ctrl Pts',(-1.47253480800006,12.2,3.85062185299999));
#302350=CARTESIAN_POINT('Ctrl Pts',(-1.47253480800006,5.2,3.85062185299999));
#302351=CARTESIAN_POINT('Ctrl Pts',(-1.47253480800006,2.2,3.85062185299999));
#302352=CARTESIAN_POINT('Ctrl Pts',(-1.47239379500006,12.2,3.84940265599998));
#302353=CARTESIAN_POINT('Ctrl Pts',(-1.47239379500006,5.2,3.84940265599998));
#302354=CARTESIAN_POINT('Ctrl Pts',(-1.47239379500006,2.2,3.84940265599998));
#302355=CARTESIAN_POINT('Ctrl Pts',(-1.47225191000006,12.2,3.84818871999999));
#302356=CARTESIAN_POINT('Ctrl Pts',(-1.47225191000006,5.2,3.84818871999999));
#302357=CARTESIAN_POINT('Ctrl Pts',(-1.47225191000006,2.2,3.84818871999999));
#302358=CARTESIAN_POINT('Ctrl Pts',(-1.47210916400006,12.2,3.84698004899998));
#302359=CARTESIAN_POINT('Ctrl Pts',(-1.47210916400006,5.2,3.84698004899998));
#302360=CARTESIAN_POINT('Ctrl Pts',(-1.47210916400006,2.2,3.84698004899998));
#302361=CARTESIAN_POINT('Ctrl Pts',(-1.47196557200005,12.2,3.84577665299998));
#302362=CARTESIAN_POINT('Ctrl Pts',(-1.47196557200005,5.2,3.84577665299998));
#302363=CARTESIAN_POINT('Ctrl Pts',(-1.47196557200005,2.2,3.84577665299998));
#302364=CARTESIAN_POINT('Ctrl Pts',(-1.47182114600006,12.2,3.84457853999999));
#302365=CARTESIAN_POINT('Ctrl Pts',(-1.47182114600006,5.2,3.84457853999999));
#302366=CARTESIAN_POINT('Ctrl Pts',(-1.47182114600006,2.2,3.84457853999999));
#302367=CARTESIAN_POINT('Ctrl Pts',(-1.47167589900006,12.2,3.84338571799999));
#302368=CARTESIAN_POINT('Ctrl Pts',(-1.47167589900006,5.2,3.84338571799999));
#302369=CARTESIAN_POINT('Ctrl Pts',(-1.47167589900006,2.2,3.84338571799999));
#302370=CARTESIAN_POINT('Ctrl Pts',(-1.47152984200006,12.2,3.84219819599998));
#302371=CARTESIAN_POINT('Ctrl Pts',(-1.47152984200006,5.2,3.84219819599998));
#302372=CARTESIAN_POINT('Ctrl Pts',(-1.47152984200006,2.2,3.84219819599998));
#302373=CARTESIAN_POINT('Ctrl Pts',(-1.47138298900006,12.2,3.84101598099999));
#302374=CARTESIAN_POINT('Ctrl Pts',(-1.47138298900006,5.2,3.84101598099999));
#302375=CARTESIAN_POINT('Ctrl Pts',(-1.47138298900006,2.2,3.84101598099999));
#302376=CARTESIAN_POINT('Ctrl Pts',(-1.47123535300006,12.2,3.83983908399999));
#302377=CARTESIAN_POINT('Ctrl Pts',(-1.47123535300006,5.2,3.83983908399999));
#302378=CARTESIAN_POINT('Ctrl Pts',(-1.47123535300006,2.2,3.83983908399999));
#302379=CARTESIAN_POINT('Ctrl Pts',(-1.47108694700006,12.2,3.83866750899998));
#302380=CARTESIAN_POINT('Ctrl Pts',(-1.47108694700006,5.2,3.83866750899998));
#302381=CARTESIAN_POINT('Ctrl Pts',(-1.47108694700006,2.2,3.83866750899998));
#302382=CARTESIAN_POINT('Ctrl Pts',(-1.47093778500005,12.2,3.83750126899999));
#302383=CARTESIAN_POINT('Ctrl Pts',(-1.47093778500005,5.2,3.83750126899999));
#302384=CARTESIAN_POINT('Ctrl Pts',(-1.47093778500005,2.2,3.83750126899999));
#302385=CARTESIAN_POINT('Ctrl Pts',(-1.47078787700006,12.2,3.83634036799998));
#302386=CARTESIAN_POINT('Ctrl Pts',(-1.47078787700006,5.2,3.83634036799998));
#302387=CARTESIAN_POINT('Ctrl Pts',(-1.47078787700006,2.2,3.83634036799998));
#302388=CARTESIAN_POINT('Ctrl Pts',(-1.47063723800006,12.2,3.83518481799998));
#302389=CARTESIAN_POINT('Ctrl Pts',(-1.47063723800006,5.2,3.83518481799998));
#302390=CARTESIAN_POINT('Ctrl Pts',(-1.47063723800006,2.2,3.83518481799998));
#302391=CARTESIAN_POINT('Ctrl Pts',(-1.47048588000006,12.2,3.83403462499999));
#302392=CARTESIAN_POINT('Ctrl Pts',(-1.47048588000006,5.2,3.83403462499999));
#302393=CARTESIAN_POINT('Ctrl Pts',(-1.47048588000006,2.2,3.83403462499999));
#302394=CARTESIAN_POINT('Ctrl Pts',(-1.47033381800005,12.2,3.83288979899999));
#302395=CARTESIAN_POINT('Ctrl Pts',(-1.47033381800005,5.2,3.83288979899999));
#302396=CARTESIAN_POINT('Ctrl Pts',(-1.47033381800005,2.2,3.83288979899999));
#302397=CARTESIAN_POINT('Ctrl Pts',(-1.47018106300006,12.2,3.83175034699998));
#302398=CARTESIAN_POINT('Ctrl Pts',(-1.47018106300006,5.2,3.83175034699998));
#302399=CARTESIAN_POINT('Ctrl Pts',(-1.47018106300006,2.2,3.83175034699998));
#302400=CARTESIAN_POINT('Ctrl Pts',(-1.47002762900006,12.2,3.83061627699998));
#302401=CARTESIAN_POINT('Ctrl Pts',(-1.47002762900006,5.2,3.83061627699998));
#302402=CARTESIAN_POINT('Ctrl Pts',(-1.47002762900006,2.2,3.83061627699998));
#302403=CARTESIAN_POINT('Ctrl Pts',(-1.46987352900006,12.2,3.82948759799999));
#302404=CARTESIAN_POINT('Ctrl Pts',(-1.46987352900006,5.2,3.82948759799999));
#302405=CARTESIAN_POINT('Ctrl Pts',(-1.46987352900006,2.2,3.82948759799999));
#302406=CARTESIAN_POINT('Ctrl Pts',(-1.46971877700006,12.2,3.82836431999999));
#302407=CARTESIAN_POINT('Ctrl Pts',(-1.46971877700006,5.2,3.82836431999999));
#302408=CARTESIAN_POINT('Ctrl Pts',(-1.46971877700006,2.2,3.82836431999999));
#302409=CARTESIAN_POINT('Ctrl Pts',(-1.46956338500006,12.2,3.82724644799998));
#302410=CARTESIAN_POINT('Ctrl Pts',(-1.46956338500006,5.2,3.82724644799998));
#302411=CARTESIAN_POINT('Ctrl Pts',(-1.46956338500006,2.2,3.82724644799998));
#302412=CARTESIAN_POINT('Ctrl Pts',(-1.46940736800006,12.2,3.82613399199998));
#302413=CARTESIAN_POINT('Ctrl Pts',(-1.46940736800006,5.2,3.82613399199998));
#302414=CARTESIAN_POINT('Ctrl Pts',(-1.46940736800006,2.2,3.82613399199998));
#302415=CARTESIAN_POINT('Ctrl Pts',(-1.46925073800006,12.2,3.82502696099999));
#302416=CARTESIAN_POINT('Ctrl Pts',(-1.46925073800006,5.2,3.82502696099999));
#302417=CARTESIAN_POINT('Ctrl Pts',(-1.46925073800006,2.2,3.82502696099999));
#302418=CARTESIAN_POINT('Ctrl Pts',(-1.46909350800006,12.2,3.82392536299999));
#302419=CARTESIAN_POINT('Ctrl Pts',(-1.46909350800006,5.2,3.82392536299999));
#302420=CARTESIAN_POINT('Ctrl Pts',(-1.46909350800006,2.2,3.82392536299999));
#302421=CARTESIAN_POINT('Ctrl Pts',(-1.46893569400006,12.2,3.82282920599998));
#302422=CARTESIAN_POINT('Ctrl Pts',(-1.46893569400006,5.2,3.82282920599998));
#302423=CARTESIAN_POINT('Ctrl Pts',(-1.46893569400006,2.2,3.82282920599998));
#302424=CARTESIAN_POINT('Ctrl Pts',(-1.46877730700006,12.2,3.82173849699999));
#302425=CARTESIAN_POINT('Ctrl Pts',(-1.46877730700006,5.2,3.82173849699999));
#302426=CARTESIAN_POINT('Ctrl Pts',(-1.46877730700006,2.2,3.82173849699999));
#302427=CARTESIAN_POINT('Ctrl Pts',(-1.46861836100006,12.2,3.82065324699998));
#302428=CARTESIAN_POINT('Ctrl Pts',(-1.46861836100006,5.2,3.82065324699998));
#302429=CARTESIAN_POINT('Ctrl Pts',(-1.46861836100006,2.2,3.82065324699998));
#302430=CARTESIAN_POINT('Ctrl Pts',(-1.46845887000006,12.2,3.81957346299998));
#302431=CARTESIAN_POINT('Ctrl Pts',(-1.46845887000006,5.2,3.81957346299998));
#302432=CARTESIAN_POINT('Ctrl Pts',(-1.46845887000006,2.2,3.81957346299998));
#302433=CARTESIAN_POINT('Ctrl Pts',(-1.46829884900006,12.2,3.81849915399999));
#302434=CARTESIAN_POINT('Ctrl Pts',(-1.46829884900006,5.2,3.81849915399999));
#302435=CARTESIAN_POINT('Ctrl Pts',(-1.46829884900006,2.2,3.81849915399999));
#302436=CARTESIAN_POINT('Ctrl Pts',(-1.46813830800006,12.2,3.81743032699998));
#302437=CARTESIAN_POINT('Ctrl Pts',(-1.46813830800006,5.2,3.81743032699998));
#302438=CARTESIAN_POINT('Ctrl Pts',(-1.46813830800006,2.2,3.81743032699998));
#302439=CARTESIAN_POINT('Ctrl Pts',(-1.46797726500006,12.2,3.81636699099998));
#302440=CARTESIAN_POINT('Ctrl Pts',(-1.46797726500006,5.2,3.81636699099998));
#302441=CARTESIAN_POINT('Ctrl Pts',(-1.46797726500006,2.2,3.81636699099998));
#302442=CARTESIAN_POINT('Ctrl Pts',(-1.46781573100006,12.2,3.81530915599999));
#302443=CARTESIAN_POINT('Ctrl Pts',(-1.46781573100006,5.2,3.81530915599999));
#302444=CARTESIAN_POINT('Ctrl Pts',(-1.46781573100006,2.2,3.81530915599999));
#302445=CARTESIAN_POINT('Ctrl Pts',(-1.46765372000006,12.2,3.81425682799998));
#302446=CARTESIAN_POINT('Ctrl Pts',(-1.46765372000006,5.2,3.81425682799998));
#302447=CARTESIAN_POINT('Ctrl Pts',(-1.46765372000006,2.2,3.81425682799998));
#302448=CARTESIAN_POINT('Ctrl Pts',(-1.46749124700006,12.2,3.81321001499998));
#302449=CARTESIAN_POINT('Ctrl Pts',(-1.46749124700006,5.2,3.81321001499998));
#302450=CARTESIAN_POINT('Ctrl Pts',(-1.46749124700006,2.2,3.81321001499998));
#302451=CARTESIAN_POINT('Ctrl Pts',(-1.46732832600006,12.2,3.81216872799998));
#302452=CARTESIAN_POINT('Ctrl Pts',(-1.46732832600006,5.2,3.81216872799998));
#302453=CARTESIAN_POINT('Ctrl Pts',(-1.46732832600006,2.2,3.81216872799998));
#302454=CARTESIAN_POINT('Ctrl Pts',(-1.46716496900006,12.2,3.81113297399998));
#302455=CARTESIAN_POINT('Ctrl Pts',(-1.46716496900006,5.2,3.81113297399998));
#302456=CARTESIAN_POINT('Ctrl Pts',(-1.46716496900006,2.2,3.81113297399998));
#302457=CARTESIAN_POINT('Ctrl Pts',(-1.46700119300006,12.2,3.81010276099998));
#302458=CARTESIAN_POINT('Ctrl Pts',(-1.46700119300006,5.2,3.81010276099998));
#302459=CARTESIAN_POINT('Ctrl Pts',(-1.46700119300006,2.2,3.81010276099998));
#302460=CARTESIAN_POINT('Ctrl Pts',(-1.46683700900006,12.2,3.80907809799999));
#302461=CARTESIAN_POINT('Ctrl Pts',(-1.46683700900006,5.2,3.80907809799999));
#302462=CARTESIAN_POINT('Ctrl Pts',(-1.46683700900006,2.2,3.80907809799999));
#302463=CARTESIAN_POINT('Ctrl Pts',(-1.46667243200006,12.2,3.80805899299999));
#302464=CARTESIAN_POINT('Ctrl Pts',(-1.46667243200006,5.2,3.80805899299999));
#302465=CARTESIAN_POINT('Ctrl Pts',(-1.46667243200006,2.2,3.80805899299999));
#302466=CARTESIAN_POINT('Ctrl Pts',(-1.46650747700006,12.2,3.80704545499999));
#302467=CARTESIAN_POINT('Ctrl Pts',(-1.46650747700006,5.2,3.80704545499999));
#302468=CARTESIAN_POINT('Ctrl Pts',(-1.46650747700006,2.2,3.80704545499999));
#302469=CARTESIAN_POINT('Ctrl Pts',(-1.46634215800006,12.2,3.80603749199998));
#302470=CARTESIAN_POINT('Ctrl Pts',(-1.46634215800006,5.2,3.80603749199998));
#302471=CARTESIAN_POINT('Ctrl Pts',(-1.46634215800006,2.2,3.80603749199998));
#302472=CARTESIAN_POINT('Ctrl Pts',(-1.46617648900006,12.2,3.80503511099998));
#302473=CARTESIAN_POINT('Ctrl Pts',(-1.46617648900006,5.2,3.80503511099998));
#302474=CARTESIAN_POINT('Ctrl Pts',(-1.46617648900006,2.2,3.80503511099998));
#302475=CARTESIAN_POINT('Ctrl Pts',(-1.46601048300006,12.2,3.80403832299999));
#302476=CARTESIAN_POINT('Ctrl Pts',(-1.46601048300006,5.2,3.80403832299999));
#302477=CARTESIAN_POINT('Ctrl Pts',(-1.46601048300006,2.2,3.80403832299999));
#302478=CARTESIAN_POINT('Ctrl Pts',(-1.46584415700006,12.2,3.80304713499999));
#302479=CARTESIAN_POINT('Ctrl Pts',(-1.46584415700006,5.2,3.80304713499999));
#302480=CARTESIAN_POINT('Ctrl Pts',(-1.46584415700006,2.2,3.80304713499999));
#302481=CARTESIAN_POINT('Ctrl Pts',(-1.46567752200006,12.2,3.80206155499998));
#302482=CARTESIAN_POINT('Ctrl Pts',(-1.46567752200006,5.2,3.80206155499998));
#302483=CARTESIAN_POINT('Ctrl Pts',(-1.46567752200006,2.2,3.80206155499998));
#302484=CARTESIAN_POINT('Ctrl Pts',(-1.46551059500006,12.2,3.80108159299999));
#302485=CARTESIAN_POINT('Ctrl Pts',(-1.46551059500006,5.2,3.80108159299999));
#302486=CARTESIAN_POINT('Ctrl Pts',(-1.46551059500006,2.2,3.80108159299999));
#302487=CARTESIAN_POINT('Ctrl Pts',(-1.46534339000006,12.2,3.80010725399998));
#302488=CARTESIAN_POINT('Ctrl Pts',(-1.46534339000006,5.2,3.80010725399998));
#302489=CARTESIAN_POINT('Ctrl Pts',(-1.46534339000006,2.2,3.80010725399998));
#302490=CARTESIAN_POINT('Ctrl Pts',(-1.46517592200005,12.2,3.79913855099999));
#302491=CARTESIAN_POINT('Ctrl Pts',(-1.46517592200005,5.2,3.79913855099999));
#302492=CARTESIAN_POINT('Ctrl Pts',(-1.46517592200005,2.2,3.79913855099999));
#302493=CARTESIAN_POINT('Ctrl Pts',(-1.46500820400006,12.2,3.79817548899998));
#302494=CARTESIAN_POINT('Ctrl Pts',(-1.46500820400006,5.2,3.79817548899998));
#302495=CARTESIAN_POINT('Ctrl Pts',(-1.46500820400006,2.2,3.79817548899998));
#302496=CARTESIAN_POINT('Ctrl Pts',(-1.46484025100006,12.2,3.79721807799999));
#302497=CARTESIAN_POINT('Ctrl Pts',(-1.46484025100006,5.2,3.79721807799999));
#302498=CARTESIAN_POINT('Ctrl Pts',(-1.46484025100006,2.2,3.79721807799999));
#302499=CARTESIAN_POINT('Ctrl Pts',(-1.46467207800006,12.2,3.79626632699999));
#302500=CARTESIAN_POINT('Ctrl Pts',(-1.46467207800006,5.2,3.79626632699999));
#302501=CARTESIAN_POINT('Ctrl Pts',(-1.46467207800006,2.2,3.79626632699999));
#302502=CARTESIAN_POINT('Ctrl Pts',(-1.46450369900006,12.2,3.79532024099999));
#302503=CARTESIAN_POINT('Ctrl Pts',(-1.46450369900006,5.2,3.79532024099999));
#302504=CARTESIAN_POINT('Ctrl Pts',(-1.46450369900006,2.2,3.79532024099999));
#302505=CARTESIAN_POINT('Ctrl Pts',(-1.46433513000006,12.2,3.79437983299999));
#302506=CARTESIAN_POINT('Ctrl Pts',(-1.46433513000006,5.2,3.79437983299999));
#302507=CARTESIAN_POINT('Ctrl Pts',(-1.46433513000006,2.2,3.79437983299999));
#302508=CARTESIAN_POINT('Ctrl Pts',(-1.46416638600006,12.2,3.79344510799999));
#302509=CARTESIAN_POINT('Ctrl Pts',(-1.46416638600006,5.2,3.79344510799999));
#302510=CARTESIAN_POINT('Ctrl Pts',(-1.46416638600006,2.2,3.79344510799999));
#302511=CARTESIAN_POINT('Ctrl Pts',(-1.46399748000006,12.2,3.79251607599999));
#302512=CARTESIAN_POINT('Ctrl Pts',(-1.46399748000006,5.2,3.79251607599999));
#302513=CARTESIAN_POINT('Ctrl Pts',(-1.46399748000006,2.2,3.79251607599999));
#302514=CARTESIAN_POINT('Ctrl Pts',(-1.46382842800006,12.2,3.79159274499998));
#302515=CARTESIAN_POINT('Ctrl Pts',(-1.46382842800006,5.2,3.79159274499998));
#302516=CARTESIAN_POINT('Ctrl Pts',(-1.46382842800006,2.2,3.79159274499998));
#302517=CARTESIAN_POINT('Ctrl Pts',(-1.46365924500006,12.2,3.79067512299999));
#302518=CARTESIAN_POINT('Ctrl Pts',(-1.46365924500006,5.2,3.79067512299999));
#302519=CARTESIAN_POINT('Ctrl Pts',(-1.46365924500006,2.2,3.79067512299999));
#302520=CARTESIAN_POINT('Ctrl Pts',(-1.46348994600006,12.2,3.78976321999998));
#302521=CARTESIAN_POINT('Ctrl Pts',(-1.46348994600006,5.2,3.78976321999998));
#302522=CARTESIAN_POINT('Ctrl Pts',(-1.46348994600006,2.2,3.78976321999998));
#302523=CARTESIAN_POINT('Ctrl Pts',(-1.46332054500006,12.2,3.78885704299999));
#302524=CARTESIAN_POINT('Ctrl Pts',(-1.46332054500006,5.2,3.78885704299999));
#302525=CARTESIAN_POINT('Ctrl Pts',(-1.46332054500006,2.2,3.78885704299999));
#302526=CARTESIAN_POINT('Ctrl Pts',(-1.46315105800006,12.2,3.78795660099998));
#302527=CARTESIAN_POINT('Ctrl Pts',(-1.46315105800006,5.2,3.78795660099998));
#302528=CARTESIAN_POINT('Ctrl Pts',(-1.46315105800006,2.2,3.78795660099998));
#302529=CARTESIAN_POINT('Ctrl Pts',(-1.46298150100006,12.2,3.78706190199999));
#302530=CARTESIAN_POINT('Ctrl Pts',(-1.46298150100006,5.2,3.78706190199999));
#302531=CARTESIAN_POINT('Ctrl Pts',(-1.46298150100006,2.2,3.78706190199999));
#302532=CARTESIAN_POINT('Ctrl Pts',(-1.46281188800006,12.2,3.78617295499998));
#302533=CARTESIAN_POINT('Ctrl Pts',(-1.46281188800006,5.2,3.78617295499998));
#302534=CARTESIAN_POINT('Ctrl Pts',(-1.46281188800006,2.2,3.78617295499998));
#302535=CARTESIAN_POINT('Ctrl Pts',(-1.46264223400006,12.2,3.78528976799998));
#302536=CARTESIAN_POINT('Ctrl Pts',(-1.46264223400006,5.2,3.78528976799998));
#302537=CARTESIAN_POINT('Ctrl Pts',(-1.46264223400006,2.2,3.78528976799998));
#302538=CARTESIAN_POINT('Ctrl Pts',(-1.46247255500006,12.2,3.78441234999999));
#302539=CARTESIAN_POINT('Ctrl Pts',(-1.46247255500006,5.2,3.78441234999999));
#302540=CARTESIAN_POINT('Ctrl Pts',(-1.46247255500006,2.2,3.78441234999999));
#302541=CARTESIAN_POINT('Ctrl Pts',(-1.46230286600006,12.2,3.78354070899999));
#302542=CARTESIAN_POINT('Ctrl Pts',(-1.46230286600006,5.2,3.78354070899999));
#302543=CARTESIAN_POINT('Ctrl Pts',(-1.46230286600006,2.2,3.78354070899999));
#302544=CARTESIAN_POINT('Ctrl Pts',(-1.46213318200005,12.2,3.78267485399999));
#302545=CARTESIAN_POINT('Ctrl Pts',(-1.46213318200005,5.2,3.78267485399999));
#302546=CARTESIAN_POINT('Ctrl Pts',(-1.46213318200005,2.2,3.78267485399999));
#302547=CARTESIAN_POINT('Ctrl Pts',(-1.46196352000006,12.2,3.78181479199998));
#302548=CARTESIAN_POINT('Ctrl Pts',(-1.46196352000006,5.2,3.78181479199998));
#302549=CARTESIAN_POINT('Ctrl Pts',(-1.46196352000006,2.2,3.78181479199998));
#302550=CARTESIAN_POINT('Ctrl Pts',(-1.46179389300006,12.2,3.78096053299998));
#302551=CARTESIAN_POINT('Ctrl Pts',(-1.46179389300006,5.2,3.78096053299998));
#302552=CARTESIAN_POINT('Ctrl Pts',(-1.46179389300006,2.2,3.78096053299998));
#302553=CARTESIAN_POINT('Ctrl Pts',(-1.46162431900006,12.2,3.78011208499998));
#302554=CARTESIAN_POINT('Ctrl Pts',(-1.46162431900006,5.2,3.78011208499998));
#302555=CARTESIAN_POINT('Ctrl Pts',(-1.46162431900006,2.2,3.78011208499998));
#302556=CARTESIAN_POINT('Ctrl Pts',(-1.46145481200006,12.2,3.77926945699999));
#302557=CARTESIAN_POINT('Ctrl Pts',(-1.46145481200006,5.2,3.77926945699999));
#302558=CARTESIAN_POINT('Ctrl Pts',(-1.46145481200006,2.2,3.77926945699999));
#302559=CARTESIAN_POINT('Ctrl Pts',(-1.46128538900006,12.2,3.77843265599999));
#302560=CARTESIAN_POINT('Ctrl Pts',(-1.46128538900006,5.2,3.77843265599999));
#302561=CARTESIAN_POINT('Ctrl Pts',(-1.46128538900006,2.2,3.77843265599999));
#302562=CARTESIAN_POINT('Ctrl Pts',(-1.46111606400006,12.2,3.77760169299999));
#302563=CARTESIAN_POINT('Ctrl Pts',(-1.46111606400006,5.2,3.77760169299999));
#302564=CARTESIAN_POINT('Ctrl Pts',(-1.46111606400006,2.2,3.77760169299999));
#302565=CARTESIAN_POINT('Ctrl Pts',(-1.46094685400006,12.2,3.77677657299999));
#302566=CARTESIAN_POINT('Ctrl Pts',(-1.46094685400006,5.2,3.77677657299999));
#302567=CARTESIAN_POINT('Ctrl Pts',(-1.46094685400006,2.2,3.77677657299999));
#302568=CARTESIAN_POINT('Ctrl Pts',(-1.46077777400005,12.2,3.77595730799998));
#302569=CARTESIAN_POINT('Ctrl Pts',(-1.46077777400005,5.2,3.77595730799998));
#302570=CARTESIAN_POINT('Ctrl Pts',(-1.46077777400005,2.2,3.77595730799998));
#302571=CARTESIAN_POINT('Ctrl Pts',(-1.46060884100006,12.2,3.77514390399998));
#302572=CARTESIAN_POINT('Ctrl Pts',(-1.46060884100006,5.2,3.77514390399998));
#302573=CARTESIAN_POINT('Ctrl Pts',(-1.46060884100006,2.2,3.77514390399998));
#302574=CARTESIAN_POINT('Ctrl Pts',(-1.46044006900006,12.2,3.77433637099998));
#302575=CARTESIAN_POINT('Ctrl Pts',(-1.46044006900006,5.2,3.77433637099998));
#302576=CARTESIAN_POINT('Ctrl Pts',(-1.46044006900006,2.2,3.77433637099998));
#302577=CARTESIAN_POINT('Ctrl Pts',(-1.46027147600006,12.2,3.77353471599999));
#302578=CARTESIAN_POINT('Ctrl Pts',(-1.46027147600006,5.2,3.77353471599999));
#302579=CARTESIAN_POINT('Ctrl Pts',(-1.46027147600006,2.2,3.77353471599999));
#302580=CARTESIAN_POINT('Ctrl Pts',(-1.46010307700006,12.2,3.77273894899999));
#302581=CARTESIAN_POINT('Ctrl Pts',(-1.46010307700006,5.2,3.77273894899999));
#302582=CARTESIAN_POINT('Ctrl Pts',(-1.46010307700006,2.2,3.77273894899999));
#302583=CARTESIAN_POINT('Ctrl Pts',(-1.45993488800006,12.2,3.77194907799999));
#302584=CARTESIAN_POINT('Ctrl Pts',(-1.45993488800006,5.2,3.77194907799999));
#302585=CARTESIAN_POINT('Ctrl Pts',(-1.45993488800006,2.2,3.77194907799999));
#302586=CARTESIAN_POINT('Ctrl Pts',(-1.45976692500006,12.2,3.77116511099998));
#302587=CARTESIAN_POINT('Ctrl Pts',(-1.45976692500006,5.2,3.77116511099998));
#302588=CARTESIAN_POINT('Ctrl Pts',(-1.45976692500006,2.2,3.77116511099998));
#302589=CARTESIAN_POINT('Ctrl Pts',(-1.45959920500006,12.2,3.77038705699999));
#302590=CARTESIAN_POINT('Ctrl Pts',(-1.45959920500006,5.2,3.77038705699999));
#302591=CARTESIAN_POINT('Ctrl Pts',(-1.45959920500006,2.2,3.77038705699999));
#302592=CARTESIAN_POINT('Ctrl Pts',(-1.45943174500006,12.2,3.76961492499999));
#302593=CARTESIAN_POINT('Ctrl Pts',(-1.45943174500006,5.2,3.76961492499999));
#302594=CARTESIAN_POINT('Ctrl Pts',(-1.45943174500006,2.2,3.76961492499999));
#302595=CARTESIAN_POINT('Ctrl Pts',(-1.45926455800006,12.2,3.76884872199999));
#302596=CARTESIAN_POINT('Ctrl Pts',(-1.45926455800006,5.2,3.76884872199999));
#302597=CARTESIAN_POINT('Ctrl Pts',(-1.45926455800006,2.2,3.76884872199999));
#302598=CARTESIAN_POINT('Ctrl Pts',(-1.45909766400006,12.2,3.76808845899999));
#302599=CARTESIAN_POINT('Ctrl Pts',(-1.45909766400006,5.2,3.76808845899999));
#302600=CARTESIAN_POINT('Ctrl Pts',(-1.45909766400006,2.2,3.76808845899999));
#302601=CARTESIAN_POINT('Ctrl Pts',(-1.45893107700006,12.2,3.76733414199999));
#302602=CARTESIAN_POINT('Ctrl Pts',(-1.45893107700006,5.2,3.76733414199999));
#302603=CARTESIAN_POINT('Ctrl Pts',(-1.45893107700006,2.2,3.76733414199999));
#302604=CARTESIAN_POINT('Ctrl Pts',(-1.45876481400006,12.2,3.76658578099998));
#302605=CARTESIAN_POINT('Ctrl Pts',(-1.45876481400006,5.2,3.76658578099998));
#302606=CARTESIAN_POINT('Ctrl Pts',(-1.45876481400006,2.2,3.76658578099998));
#302607=CARTESIAN_POINT('Ctrl Pts',(-1.45859889200006,12.2,3.76584338299998));
#302608=CARTESIAN_POINT('Ctrl Pts',(-1.45859889200006,5.2,3.76584338299998));
#302609=CARTESIAN_POINT('Ctrl Pts',(-1.45859889200006,2.2,3.76584338299998));
#302610=CARTESIAN_POINT('Ctrl Pts',(-1.45843332800006,12.2,3.76510695899999));
#302611=CARTESIAN_POINT('Ctrl Pts',(-1.45843332800006,5.2,3.76510695899999));
#302612=CARTESIAN_POINT('Ctrl Pts',(-1.45843332800006,2.2,3.76510695899999));
#302613=CARTESIAN_POINT('Ctrl Pts',(-1.45826813800006,12.2,3.76437651499998));
#302614=CARTESIAN_POINT('Ctrl Pts',(-1.45826813800006,5.2,3.76437651499998));
#302615=CARTESIAN_POINT('Ctrl Pts',(-1.45826813800006,2.2,3.76437651499998));
#302616=CARTESIAN_POINT('Ctrl Pts',(-1.45810333700006,12.2,3.76365206099998));
#302617=CARTESIAN_POINT('Ctrl Pts',(-1.45810333700006,5.2,3.76365206099998));
#302618=CARTESIAN_POINT('Ctrl Pts',(-1.45810333700006,2.2,3.76365206099998));
#302619=CARTESIAN_POINT('Ctrl Pts',(-1.45793894500006,12.2,3.76293360499999));
#302620=CARTESIAN_POINT('Ctrl Pts',(-1.45793894500006,5.2,3.76293360499999));
#302621=CARTESIAN_POINT('Ctrl Pts',(-1.45793894500006,2.2,3.76293360499999));
#302622=CARTESIAN_POINT('Ctrl Pts',(-1.45777497700006,12.2,3.76222115699999));
#302623=CARTESIAN_POINT('Ctrl Pts',(-1.45777497700006,5.2,3.76222115699999));
#302624=CARTESIAN_POINT('Ctrl Pts',(-1.45777497700006,2.2,3.76222115699999));
#302625=CARTESIAN_POINT('Ctrl Pts',(-1.45761145000006,12.2,3.76151472299998));
#302626=CARTESIAN_POINT('Ctrl Pts',(-1.45761145000006,5.2,3.76151472299998));
#302627=CARTESIAN_POINT('Ctrl Pts',(-1.45761145000006,2.2,3.76151472299998));
#302628=CARTESIAN_POINT('Ctrl Pts',(-1.45744838100006,12.2,3.76081431299998));
#302629=CARTESIAN_POINT('Ctrl Pts',(-1.45744838100006,5.2,3.76081431299998));
#302630=CARTESIAN_POINT('Ctrl Pts',(-1.45744838100006,2.2,3.76081431299998));
#302631=CARTESIAN_POINT('Ctrl Pts',(-1.45728578700006,12.2,3.76011993699999));
#302632=CARTESIAN_POINT('Ctrl Pts',(-1.45728578700006,5.2,3.76011993699999));
#302633=CARTESIAN_POINT('Ctrl Pts',(-1.45728578700006,2.2,3.76011993699999));
#302634=CARTESIAN_POINT('Ctrl Pts',(-1.45712368400006,12.2,3.75943159999998));
#302635=CARTESIAN_POINT('Ctrl Pts',(-1.45712368400006,5.2,3.75943159999998));
#302636=CARTESIAN_POINT('Ctrl Pts',(-1.45712368400006,2.2,3.75943159999998));
#302637=CARTESIAN_POINT('Ctrl Pts',(-1.45696209200006,12.2,3.75874931399999));
#302638=CARTESIAN_POINT('Ctrl Pts',(-1.45696209200006,5.2,3.75874931399999));
#302639=CARTESIAN_POINT('Ctrl Pts',(-1.45696209200006,2.2,3.75874931399999));
#302640=CARTESIAN_POINT('Ctrl Pts',(-1.45680102500006,12.2,3.75807308599998));
#302641=CARTESIAN_POINT('Ctrl Pts',(-1.45680102500006,5.2,3.75807308599998));
#302642=CARTESIAN_POINT('Ctrl Pts',(-1.45680102500006,2.2,3.75807308599998));
#302643=CARTESIAN_POINT('Ctrl Pts',(-1.45664050200006,12.2,3.75740292399998));
#302644=CARTESIAN_POINT('Ctrl Pts',(-1.45664050200006,5.2,3.75740292399998));
#302645=CARTESIAN_POINT('Ctrl Pts',(-1.45664050200006,2.2,3.75740292399998));
#302646=CARTESIAN_POINT('Ctrl Pts',(-1.45648053900006,12.2,3.75673883699999));
#302647=CARTESIAN_POINT('Ctrl Pts',(-1.45648053900006,5.2,3.75673883699999));
#302648=CARTESIAN_POINT('Ctrl Pts',(-1.45648053900006,2.2,3.75673883699999));
#302649=CARTESIAN_POINT('Ctrl Pts',(-1.45632115500006,12.2,3.75608083599998));
#302650=CARTESIAN_POINT('Ctrl Pts',(-1.45632115500006,5.2,3.75608083599998));
#302651=CARTESIAN_POINT('Ctrl Pts',(-1.45632115500006,2.2,3.75608083599998));
#302652=CARTESIAN_POINT('Ctrl Pts',(-1.45616236600006,12.2,3.75542892599999));
#302653=CARTESIAN_POINT('Ctrl Pts',(-1.45616236600006,5.2,3.75542892599999));
#302654=CARTESIAN_POINT('Ctrl Pts',(-1.45616236600006,2.2,3.75542892599999));
#302655=CARTESIAN_POINT('Ctrl Pts',(-1.45600419000006,12.2,3.75478311699998));
#302656=CARTESIAN_POINT('Ctrl Pts',(-1.45600419000006,5.2,3.75478311699998));
#302657=CARTESIAN_POINT('Ctrl Pts',(-1.45600419000006,2.2,3.75478311699998));
#302658=CARTESIAN_POINT('Ctrl Pts',(-1.45584664500006,12.2,3.75414341799999));
#302659=CARTESIAN_POINT('Ctrl Pts',(-1.45584664500006,5.2,3.75414341799999));
#302660=CARTESIAN_POINT('Ctrl Pts',(-1.45584664500006,2.2,3.75414341799999));
#302661=CARTESIAN_POINT('Ctrl Pts',(-1.45568974700006,12.2,3.75350983799999));
#302662=CARTESIAN_POINT('Ctrl Pts',(-1.45568974700006,5.2,3.75350983799999));
#302663=CARTESIAN_POINT('Ctrl Pts',(-1.45568974700006,2.2,3.75350983799999));
#302664=CARTESIAN_POINT('Ctrl Pts',(-1.45553351600006,12.2,3.75288238399998));
#302665=CARTESIAN_POINT('Ctrl Pts',(-1.45553351600006,5.2,3.75288238399998));
#302666=CARTESIAN_POINT('Ctrl Pts',(-1.45553351600006,2.2,3.75288238399998));
#302667=CARTESIAN_POINT('Ctrl Pts',(-1.45537796700006,12.2,3.75226106499999));
#302668=CARTESIAN_POINT('Ctrl Pts',(-1.45537796700006,5.2,3.75226106499999));
#302669=CARTESIAN_POINT('Ctrl Pts',(-1.45537796700006,2.2,3.75226106499999));
#302670=CARTESIAN_POINT('Ctrl Pts',(-1.45522312000006,12.2,3.75164589099998));
#302671=CARTESIAN_POINT('Ctrl Pts',(-1.45522312000006,5.2,3.75164589099998));
#302672=CARTESIAN_POINT('Ctrl Pts',(-1.45522312000006,2.2,3.75164589099998));
#302673=CARTESIAN_POINT('Ctrl Pts',(-1.45506899100006,12.2,3.75103686899998));
#302674=CARTESIAN_POINT('Ctrl Pts',(-1.45506899100006,5.2,3.75103686899998));
#302675=CARTESIAN_POINT('Ctrl Pts',(-1.45506899100006,2.2,3.75103686899998));
#302676=CARTESIAN_POINT('Ctrl Pts',(-1.45491559900006,12.2,3.75043400999999));
#302677=CARTESIAN_POINT('Ctrl Pts',(-1.45491559900006,5.2,3.75043400999999));
#302678=CARTESIAN_POINT('Ctrl Pts',(-1.45491559900006,2.2,3.75043400999999));
#302679=CARTESIAN_POINT('Ctrl Pts',(-1.45476296300005,12.2,3.74983731899999));
#302680=CARTESIAN_POINT('Ctrl Pts',(-1.45476296300005,5.2,3.74983731899999));
#302681=CARTESIAN_POINT('Ctrl Pts',(-1.45476296300005,2.2,3.74983731899999));
#302682=CARTESIAN_POINT('Ctrl Pts',(-1.45461109900006,12.2,3.74924680899999));
#302683=CARTESIAN_POINT('Ctrl Pts',(-1.45461109900006,5.2,3.74924680899999));
#302684=CARTESIAN_POINT('Ctrl Pts',(-1.45461109900006,2.2,3.74924680899999));
#302685=CARTESIAN_POINT('Ctrl Pts',(-1.45446002600006,12.2,3.74866248399999));
#302686=CARTESIAN_POINT('Ctrl Pts',(-1.45446002600006,5.2,3.74866248399999));
#302687=CARTESIAN_POINT('Ctrl Pts',(-1.45446002600006,2.2,3.74866248399999));
#302688=CARTESIAN_POINT('Ctrl Pts',(-1.45430976300006,12.2,3.74808435499999));
#302689=CARTESIAN_POINT('Ctrl Pts',(-1.45430976300006,5.2,3.74808435499999));
#302690=CARTESIAN_POINT('Ctrl Pts',(-1.45430976300006,2.2,3.74808435499999));
#302691=CARTESIAN_POINT('Ctrl Pts',(-1.45416032600005,12.2,3.74751243199999));
#302692=CARTESIAN_POINT('Ctrl Pts',(-1.45416032600005,5.2,3.74751243199999));
#302693=CARTESIAN_POINT('Ctrl Pts',(-1.45416032600005,2.2,3.74751243199999));
#302694=CARTESIAN_POINT('Ctrl Pts',(-1.45401173500006,12.2,3.74694672099999));
#302695=CARTESIAN_POINT('Ctrl Pts',(-1.45401173500006,5.2,3.74694672099999));
#302696=CARTESIAN_POINT('Ctrl Pts',(-1.45401173500006,2.2,3.74694672099999));
#302697=CARTESIAN_POINT('Ctrl Pts',(-1.45386400800006,12.2,3.74638723199999));
#302698=CARTESIAN_POINT('Ctrl Pts',(-1.45386400800006,5.2,3.74638723199999));
#302699=CARTESIAN_POINT('Ctrl Pts',(-1.45386400800006,2.2,3.74638723199999));
#302700=CARTESIAN_POINT('Ctrl Pts',(-1.45371716300006,12.2,3.74583397399999));
#302701=CARTESIAN_POINT('Ctrl Pts',(-1.45371716300006,5.2,3.74583397399999));
#302702=CARTESIAN_POINT('Ctrl Pts',(-1.45371716300006,2.2,3.74583397399999));
#302703=CARTESIAN_POINT('Ctrl Pts',(-1.45357121900005,12.2,3.74528695499999));
#302704=CARTESIAN_POINT('Ctrl Pts',(-1.45357121900005,5.2,3.74528695499999));
#302705=CARTESIAN_POINT('Ctrl Pts',(-1.45357121900005,2.2,3.74528695499999));
#302706=CARTESIAN_POINT('Ctrl Pts',(-1.45342619400005,12.2,3.74474618299999));
#302707=CARTESIAN_POINT('Ctrl Pts',(-1.45342619400005,5.2,3.74474618299999));
#302708=CARTESIAN_POINT('Ctrl Pts',(-1.45342619400005,2.2,3.74474618299999));
#302709=CARTESIAN_POINT('Ctrl Pts',(-1.45328210800006,12.2,3.74421166899998));
#302710=CARTESIAN_POINT('Ctrl Pts',(-1.45328210800006,5.2,3.74421166899998));
#302711=CARTESIAN_POINT('Ctrl Pts',(-1.45328210800006,2.2,3.74421166899998));
#302712=CARTESIAN_POINT('Ctrl Pts',(-1.45313897700006,12.2,3.74368341899999));
#302713=CARTESIAN_POINT('Ctrl Pts',(-1.45313897700006,5.2,3.74368341899999));
#302714=CARTESIAN_POINT('Ctrl Pts',(-1.45313897700006,2.2,3.74368341899999));
#302715=CARTESIAN_POINT('Ctrl Pts',(-1.45299682300006,12.2,3.74316144299998));
#302716=CARTESIAN_POINT('Ctrl Pts',(-1.45299682300006,5.2,3.74316144299998));
#302717=CARTESIAN_POINT('Ctrl Pts',(-1.45299682300006,2.2,3.74316144299998));
#302718=CARTESIAN_POINT('Ctrl Pts',(-1.45285566200006,12.2,3.74264574899998));
#302719=CARTESIAN_POINT('Ctrl Pts',(-1.45285566200006,5.2,3.74264574899998));
#302720=CARTESIAN_POINT('Ctrl Pts',(-1.45285566200006,2.2,3.74264574899998));
#302721=CARTESIAN_POINT('Ctrl Pts',(-1.45271551400006,12.2,3.74213634699998));
#302722=CARTESIAN_POINT('Ctrl Pts',(-1.45271551400006,5.2,3.74213634699998));
#302723=CARTESIAN_POINT('Ctrl Pts',(-1.45271551400006,2.2,3.74213634699998));
#302724=CARTESIAN_POINT('Ctrl Pts',(-1.45257639800006,12.2,3.74163324399999));
#302725=CARTESIAN_POINT('Ctrl Pts',(-1.45257639800006,5.2,3.74163324399999));
#302726=CARTESIAN_POINT('Ctrl Pts',(-1.45257639800006,2.2,3.74163324399999));
#302727=CARTESIAN_POINT('Ctrl Pts',(-1.45243833400006,12.2,3.74113645099998));
#302728=CARTESIAN_POINT('Ctrl Pts',(-1.45243833400006,5.2,3.74113645099998));
#302729=CARTESIAN_POINT('Ctrl Pts',(-1.45243833400006,2.2,3.74113645099998));
#302730=CARTESIAN_POINT('Ctrl Pts',(-1.45230133900006,12.2,3.74064597399999));
#302731=CARTESIAN_POINT('Ctrl Pts',(-1.45230133900006,5.2,3.74064597399999));
#302732=CARTESIAN_POINT('Ctrl Pts',(-1.45230133900006,2.2,3.74064597399999));
#302733=CARTESIAN_POINT('Ctrl Pts',(-1.45216543300006,12.2,3.74016182299999));
#302734=CARTESIAN_POINT('Ctrl Pts',(-1.45216543300006,5.2,3.74016182299999));
#302735=CARTESIAN_POINT('Ctrl Pts',(-1.45216543300006,2.2,3.74016182299999));
#302736=CARTESIAN_POINT('Ctrl Pts',(-1.45203063700006,12.2,3.73968400799999));
#302737=CARTESIAN_POINT('Ctrl Pts',(-1.45203063700006,5.2,3.73968400799999));
#302738=CARTESIAN_POINT('Ctrl Pts',(-1.45203063700006,2.2,3.73968400799999));
#302739=CARTESIAN_POINT('Ctrl Pts',(-1.45189696700006,12.2,3.73921253499999));
#302740=CARTESIAN_POINT('Ctrl Pts',(-1.45189696700006,5.2,3.73921253499999));
#302741=CARTESIAN_POINT('Ctrl Pts',(-1.45189696700006,2.2,3.73921253499999));
#302742=CARTESIAN_POINT('Ctrl Pts',(-1.45176444400006,12.2,3.73874741399998));
#302743=CARTESIAN_POINT('Ctrl Pts',(-1.45176444400006,5.2,3.73874741399998));
#302744=CARTESIAN_POINT('Ctrl Pts',(-1.45176444400006,2.2,3.73874741399998));
#302745=CARTESIAN_POINT('Ctrl Pts',(-1.45163308900006,12.2,3.73828865499998));
#302746=CARTESIAN_POINT('Ctrl Pts',(-1.45163308900006,5.2,3.73828865499998));
#302747=CARTESIAN_POINT('Ctrl Pts',(-1.45163308900006,2.2,3.73828865499998));
#302748=CARTESIAN_POINT('Ctrl Pts',(-1.45150291900006,12.2,3.73783626399998));
#302749=CARTESIAN_POINT('Ctrl Pts',(-1.45150291900006,5.2,3.73783626399998));
#302750=CARTESIAN_POINT('Ctrl Pts',(-1.45150291900006,2.2,3.73783626399998));
#302751=CARTESIAN_POINT('Ctrl Pts',(-1.45137395500006,12.2,3.73739025199999));
#302752=CARTESIAN_POINT('Ctrl Pts',(-1.45137395500006,5.2,3.73739025199999));
#302753=CARTESIAN_POINT('Ctrl Pts',(-1.45137395500006,2.2,3.73739025199999));
#302754=CARTESIAN_POINT('Ctrl Pts',(-1.45124621600006,12.2,3.73695062699999));
#302755=CARTESIAN_POINT('Ctrl Pts',(-1.45124621600006,5.2,3.73695062699999));
#302756=CARTESIAN_POINT('Ctrl Pts',(-1.45124621600006,2.2,3.73695062699999));
#302757=CARTESIAN_POINT('Ctrl Pts',(-1.45111972300006,12.2,3.73651739899999));
#302758=CARTESIAN_POINT('Ctrl Pts',(-1.45111972300006,5.2,3.73651739899999));
#302759=CARTESIAN_POINT('Ctrl Pts',(-1.45111972300006,2.2,3.73651739899999));
#302760=CARTESIAN_POINT('Ctrl Pts',(-1.45099449400006,12.2,3.73609057399998));
#302761=CARTESIAN_POINT('Ctrl Pts',(-1.45099449400006,5.2,3.73609057399998));
#302762=CARTESIAN_POINT('Ctrl Pts',(-1.45099449400006,2.2,3.73609057399998));
#302763=CARTESIAN_POINT('Ctrl Pts',(-1.45087055000006,12.2,3.73567016199999));
#302764=CARTESIAN_POINT('Ctrl Pts',(-1.45087055000006,5.2,3.73567016199999));
#302765=CARTESIAN_POINT('Ctrl Pts',(-1.45087055000006,2.2,3.73567016199999));
#302766=CARTESIAN_POINT('Ctrl Pts',(-1.45074791000006,12.2,3.73525617299999));
#302767=CARTESIAN_POINT('Ctrl Pts',(-1.45074791000006,5.2,3.73525617299999));
#302768=CARTESIAN_POINT('Ctrl Pts',(-1.45074791000006,2.2,3.73525617299999));
#302769=CARTESIAN_POINT('Ctrl Pts',(-1.45062659500006,12.2,3.73484861399999));
#302770=CARTESIAN_POINT('Ctrl Pts',(-1.45062659500006,5.2,3.73484861399999));
#302771=CARTESIAN_POINT('Ctrl Pts',(-1.45062659500006,2.2,3.73484861399999));
#302772=CARTESIAN_POINT('Ctrl Pts',(-1.45050662500006,12.2,3.73444749499999));
#302773=CARTESIAN_POINT('Ctrl Pts',(-1.45050662500006,5.2,3.73444749499999));
#302774=CARTESIAN_POINT('Ctrl Pts',(-1.45050662500006,2.2,3.73444749499999));
#302775=CARTESIAN_POINT('Ctrl Pts',(-1.45038802000006,12.2,3.73405282499998));
#302776=CARTESIAN_POINT('Ctrl Pts',(-1.45038802000006,5.2,3.73405282499998));
#302777=CARTESIAN_POINT('Ctrl Pts',(-1.45038802000006,2.2,3.73405282499998));
#302778=CARTESIAN_POINT('Ctrl Pts',(-1.45027080000006,12.2,3.73366461099998));
#302779=CARTESIAN_POINT('Ctrl Pts',(-1.45027080000006,5.2,3.73366461099998));
#302780=CARTESIAN_POINT('Ctrl Pts',(-1.45027080000006,2.2,3.73366461099998));
#302781=CARTESIAN_POINT('Ctrl Pts',(-1.45015498500006,12.2,3.73328286299999));
#302782=CARTESIAN_POINT('Ctrl Pts',(-1.45015498500006,5.2,3.73328286299999));
#302783=CARTESIAN_POINT('Ctrl Pts',(-1.45015498500006,2.2,3.73328286299999));
#302784=CARTESIAN_POINT('Ctrl Pts',(-1.45004059600006,12.2,3.73290758999998));
#302785=CARTESIAN_POINT('Ctrl Pts',(-1.45004059600006,5.2,3.73290758999998));
#302786=CARTESIAN_POINT('Ctrl Pts',(-1.45004059600006,2.2,3.73290758999998));
#302787=CARTESIAN_POINT('Ctrl Pts',(-1.44992765300006,12.2,3.73253880099998));
#302788=CARTESIAN_POINT('Ctrl Pts',(-1.44992765300006,5.2,3.73253880099998));
#302789=CARTESIAN_POINT('Ctrl Pts',(-1.44992765300006,2.2,3.73253880099998));
#302790=CARTESIAN_POINT('Ctrl Pts',(-1.44981617800006,12.2,3.73217650299999));
#302791=CARTESIAN_POINT('Ctrl Pts',(-1.44981617800006,5.2,3.73217650299999));
#302792=CARTESIAN_POINT('Ctrl Pts',(-1.44981617800006,2.2,3.73217650299999));
#302793=CARTESIAN_POINT('Ctrl Pts',(-1.44970619000006,12.2,3.73182070599999));
#302794=CARTESIAN_POINT('Ctrl Pts',(-1.44970619000006,5.2,3.73182070599999));
#302795=CARTESIAN_POINT('Ctrl Pts',(-1.44970619000006,2.2,3.73182070599999));
#302796=CARTESIAN_POINT('Ctrl Pts',(-1.44959771000006,12.2,3.73147141999999));
#302797=CARTESIAN_POINT('Ctrl Pts',(-1.44959771000006,5.2,3.73147141999999));
#302798=CARTESIAN_POINT('Ctrl Pts',(-1.44959771000006,2.2,3.73147141999999));
#302799=CARTESIAN_POINT('Ctrl Pts',(-1.44949075900006,12.2,3.73112865199998));
#302800=CARTESIAN_POINT('Ctrl Pts',(-1.44949075900006,5.2,3.73112865199998));
#302801=CARTESIAN_POINT('Ctrl Pts',(-1.44949075900006,2.2,3.73112865199998));
#302802=CARTESIAN_POINT('Ctrl Pts',(-1.44938535800006,12.2,3.73079241199999));
#302803=CARTESIAN_POINT('Ctrl Pts',(-1.44938535800006,5.2,3.73079241199999));
#302804=CARTESIAN_POINT('Ctrl Pts',(-1.44938535800006,2.2,3.73079241199999));
#302805=CARTESIAN_POINT('Ctrl Pts',(-1.44928152800005,12.2,3.73046270799998));
#302806=CARTESIAN_POINT('Ctrl Pts',(-1.44928152800005,5.2,3.73046270799998));
#302807=CARTESIAN_POINT('Ctrl Pts',(-1.44928152800005,2.2,3.73046270799998));
#302808=CARTESIAN_POINT('Ctrl Pts',(-1.44917928900006,12.2,3.73013954999998));
#302809=CARTESIAN_POINT('Ctrl Pts',(-1.44917928900006,5.2,3.73013954999998));
#302810=CARTESIAN_POINT('Ctrl Pts',(-1.44917928900006,2.2,3.73013954999998));
#302811=CARTESIAN_POINT('Ctrl Pts',(-1.44907866400006,12.2,3.72982294399999));
#302812=CARTESIAN_POINT('Ctrl Pts',(-1.44907866400006,5.2,3.72982294399999));
#302813=CARTESIAN_POINT('Ctrl Pts',(-1.44907866400006,2.2,3.72982294399999));
#302814=CARTESIAN_POINT('Ctrl Pts',(-1.44897967300005,12.2,3.72951290199998));
#302815=CARTESIAN_POINT('Ctrl Pts',(-1.44897967300005,5.2,3.72951290199998));
#302816=CARTESIAN_POINT('Ctrl Pts',(-1.44897967300005,2.2,3.72951290199998));
#302817=CARTESIAN_POINT('Ctrl Pts',(-1.44888233700006,12.2,3.72920943199999));
#302818=CARTESIAN_POINT('Ctrl Pts',(-1.44888233700006,5.2,3.72920943199999));
#302819=CARTESIAN_POINT('Ctrl Pts',(-1.44888233700006,2.2,3.72920943199999));
#302820=CARTESIAN_POINT('Ctrl Pts',(-1.44878667900006,12.2,3.72891254199998));
#302821=CARTESIAN_POINT('Ctrl Pts',(-1.44878667900006,5.2,3.72891254199998));
#302822=CARTESIAN_POINT('Ctrl Pts',(-1.44878667900006,2.2,3.72891254199998));
#302823=CARTESIAN_POINT('Ctrl Pts',(-1.44869271700006,12.2,3.72862224099999));
#302824=CARTESIAN_POINT('Ctrl Pts',(-1.44869271700006,5.2,3.72862224099999));
#302825=CARTESIAN_POINT('Ctrl Pts',(-1.44869271700006,2.2,3.72862224099999));
#302826=CARTESIAN_POINT('Ctrl Pts',(-1.44860047700006,12.2,3.72833853899999));
#302827=CARTESIAN_POINT('Ctrl Pts',(-1.44860047700006,5.2,3.72833853899999));
#302828=CARTESIAN_POINT('Ctrl Pts',(-1.44860047700006,2.2,3.72833853899999));
#302829=CARTESIAN_POINT('Ctrl Pts',(-1.44850997700006,12.2,3.72806144399998));
#302830=CARTESIAN_POINT('Ctrl Pts',(-1.44850997700006,5.2,3.72806144399998));
#302831=CARTESIAN_POINT('Ctrl Pts',(-1.44850997700006,2.2,3.72806144399998));
#302832=CARTESIAN_POINT('Ctrl Pts',(-1.44842123900006,12.2,3.72779096499999));
#302833=CARTESIAN_POINT('Ctrl Pts',(-1.44842123900006,5.2,3.72779096499999));
#302834=CARTESIAN_POINT('Ctrl Pts',(-1.44842123900006,2.2,3.72779096499999));
#302835=CARTESIAN_POINT('Ctrl Pts',(-1.44833428800006,12.2,3.72752711099999));
#302836=CARTESIAN_POINT('Ctrl Pts',(-1.44833428800006,5.2,3.72752711099999));
#302837=CARTESIAN_POINT('Ctrl Pts',(-1.44833428800006,2.2,3.72752711099999));
#302838=CARTESIAN_POINT('Ctrl Pts',(-1.44824914200006,12.2,3.72726989099998));
#302839=CARTESIAN_POINT('Ctrl Pts',(-1.44824914200006,5.2,3.72726989099998));
#302840=CARTESIAN_POINT('Ctrl Pts',(-1.44824914200006,2.2,3.72726989099998));
#302841=CARTESIAN_POINT('Ctrl Pts',(-1.44816582500006,12.2,3.72701931299999));
#302842=CARTESIAN_POINT('Ctrl Pts',(-1.44816582500006,5.2,3.72701931299999));
#302843=CARTESIAN_POINT('Ctrl Pts',(-1.44816582500006,2.2,3.72701931299999));
#302844=CARTESIAN_POINT('Ctrl Pts',(-1.44808435900006,12.2,3.72677538699998));
#302845=CARTESIAN_POINT('Ctrl Pts',(-1.44808435900006,5.2,3.72677538699998));
#302846=CARTESIAN_POINT('Ctrl Pts',(-1.44808435900006,2.2,3.72677538699998));
#302847=CARTESIAN_POINT('Ctrl Pts',(-1.44800476500005,12.2,3.72653812199999));
#302848=CARTESIAN_POINT('Ctrl Pts',(-1.44800476500005,5.2,3.72653812199999));
#302849=CARTESIAN_POINT('Ctrl Pts',(-1.44800476500005,2.2,3.72653812199999));
#302850=CARTESIAN_POINT('Ctrl Pts',(-1.44792706600006,12.2,3.72630752599999));
#302851=CARTESIAN_POINT('Ctrl Pts',(-1.44792706600006,5.2,3.72630752599999));
#302852=CARTESIAN_POINT('Ctrl Pts',(-1.44792706600006,2.2,3.72630752599999));
#302853=CARTESIAN_POINT('Ctrl Pts',(-1.44785128400006,12.2,3.72608360799998));
#302854=CARTESIAN_POINT('Ctrl Pts',(-1.44785128400006,5.2,3.72608360799998));
#302855=CARTESIAN_POINT('Ctrl Pts',(-1.44785128400006,2.2,3.72608360799998));
#302856=CARTESIAN_POINT('Ctrl Pts',(-1.44777744200006,12.2,3.72586637799999));
#302857=CARTESIAN_POINT('Ctrl Pts',(-1.44777744200006,5.2,3.72586637799999));
#302858=CARTESIAN_POINT('Ctrl Pts',(-1.44777744200006,2.2,3.72586637799999));
#302859=CARTESIAN_POINT('Ctrl Pts',(-1.44770556100006,12.2,3.72565584299998));
#302860=CARTESIAN_POINT('Ctrl Pts',(-1.44770556100006,5.2,3.72565584299998));
#302861=CARTESIAN_POINT('Ctrl Pts',(-1.44770556100006,2.2,3.72565584299998));
#302862=CARTESIAN_POINT('Ctrl Pts',(-1.44763566500006,12.2,3.72545201299998));
#302863=CARTESIAN_POINT('Ctrl Pts',(-1.44763566500006,5.2,3.72545201299998));
#302864=CARTESIAN_POINT('Ctrl Pts',(-1.44763566500006,2.2,3.72545201299998));
#302865=CARTESIAN_POINT('Ctrl Pts',(-1.44756777600006,12.2,3.72525489799998));
#302866=CARTESIAN_POINT('Ctrl Pts',(-1.44756777600006,5.2,3.72525489799998));
#302867=CARTESIAN_POINT('Ctrl Pts',(-1.44756777600006,2.2,3.72525489799998));
#302868=CARTESIAN_POINT('Ctrl Pts',(-1.44750191600005,12.2,3.72506450599998));
#302869=CARTESIAN_POINT('Ctrl Pts',(-1.44750191600005,5.2,3.72506450599998));
#302870=CARTESIAN_POINT('Ctrl Pts',(-1.44750191600005,2.2,3.72506450599998));
#302871=CARTESIAN_POINT('Ctrl Pts',(-1.44743811100006,12.2,3.72488084599999));
#302872=CARTESIAN_POINT('Ctrl Pts',(-1.44743811100006,5.2,3.72488084599999));
#302873=CARTESIAN_POINT('Ctrl Pts',(-1.44743811100006,2.2,3.72488084599999));
#302874=CARTESIAN_POINT('Ctrl Pts',(-1.44737638100006,12.2,3.72470392699999));
#302875=CARTESIAN_POINT('Ctrl Pts',(-1.44737638100006,5.2,3.72470392699999));
#302876=CARTESIAN_POINT('Ctrl Pts',(-1.44737638100006,2.2,3.72470392699999));
#302877=CARTESIAN_POINT('Ctrl Pts',(-1.44731675000005,12.2,3.72453375899998));
#302878=CARTESIAN_POINT('Ctrl Pts',(-1.44731675000005,5.2,3.72453375899998));
#302879=CARTESIAN_POINT('Ctrl Pts',(-1.44731675000005,2.2,3.72453375899998));
#302880=CARTESIAN_POINT('Ctrl Pts',(-1.44725923900006,12.2,3.72437034899999));
#302881=CARTESIAN_POINT('Ctrl Pts',(-1.44725923900006,5.2,3.72437034899999));
#302882=CARTESIAN_POINT('Ctrl Pts',(-1.44725923900006,2.2,3.72437034899999));
#302883=CARTESIAN_POINT('Ctrl Pts',(-1.44720387400006,12.2,3.72421370599999));
#302884=CARTESIAN_POINT('Ctrl Pts',(-1.44720387400006,5.2,3.72421370599999));
#302885=CARTESIAN_POINT('Ctrl Pts',(-1.44720387400006,2.2,3.72421370599999));
#302886=CARTESIAN_POINT('Ctrl Pts',(-1.44715067400006,12.2,3.72406384099998));
#302887=CARTESIAN_POINT('Ctrl Pts',(-1.44715067400006,5.2,3.72406384099998));
#302888=CARTESIAN_POINT('Ctrl Pts',(-1.44715067400006,2.2,3.72406384099998));
#302889=CARTESIAN_POINT('Ctrl Pts',(-1.44709966700006,12.2,3.72392076099998));
#302890=CARTESIAN_POINT('Ctrl Pts',(-1.44709966700006,5.2,3.72392076099998));
#302891=CARTESIAN_POINT('Ctrl Pts',(-1.44709966700006,2.2,3.72392076099998));
#302892=CARTESIAN_POINT('Ctrl Pts',(-1.44705087400006,12.2,3.72378447599999));
#302893=CARTESIAN_POINT('Ctrl Pts',(-1.44705087400006,5.2,3.72378447599999));
#302894=CARTESIAN_POINT('Ctrl Pts',(-1.44705087400006,2.2,3.72378447599999));
#302895=CARTESIAN_POINT('Ctrl Pts',(-1.44700432100006,12.2,3.72365499499999));
#302896=CARTESIAN_POINT('Ctrl Pts',(-1.44700432100006,5.2,3.72365499499999));
#302897=CARTESIAN_POINT('Ctrl Pts',(-1.44700432100006,2.2,3.72365499499999));
#302898=CARTESIAN_POINT('Ctrl Pts',(-1.44696003400006,12.2,3.72353232799998));
#302899=CARTESIAN_POINT('Ctrl Pts',(-1.44696003400006,5.2,3.72353232799998));
#302900=CARTESIAN_POINT('Ctrl Pts',(-1.44696003400006,2.2,3.72353232799998));
#302901=CARTESIAN_POINT('Ctrl Pts',(-1.44691803400006,12.2,3.72341648399999));
#302902=CARTESIAN_POINT('Ctrl Pts',(-1.44691803400006,5.2,3.72341648399999));
#302903=CARTESIAN_POINT('Ctrl Pts',(-1.44691803400006,2.2,3.72341648399999));
#302904=CARTESIAN_POINT('Ctrl Pts',(-1.44687834300006,12.2,3.72330747199998));
#302905=CARTESIAN_POINT('Ctrl Pts',(-1.44687834300006,5.2,3.72330747199998));
#302906=CARTESIAN_POINT('Ctrl Pts',(-1.44687834300006,2.2,3.72330747199998));
#302907=CARTESIAN_POINT('Ctrl Pts',(-1.44684098300006,12.2,3.72320529699999));
#302908=CARTESIAN_POINT('Ctrl Pts',(-1.44684098300006,5.2,3.72320529699999));
#302909=CARTESIAN_POINT('Ctrl Pts',(-1.44684098300006,2.2,3.72320529699999));
#302910=CARTESIAN_POINT('Ctrl Pts',(-1.44680597500006,12.2,3.72310996999998));
#302911=CARTESIAN_POINT('Ctrl Pts',(-1.44680597500006,5.2,3.72310996999998));
#302912=CARTESIAN_POINT('Ctrl Pts',(-1.44680597500006,2.2,3.72310996999998));
#302913=CARTESIAN_POINT('Ctrl Pts',(-1.44677334500006,12.2,3.72302149899999));
#302914=CARTESIAN_POINT('Ctrl Pts',(-1.44677334500006,5.2,3.72302149899999));
#302915=CARTESIAN_POINT('Ctrl Pts',(-1.44677334500006,2.2,3.72302149899999));
#302916=CARTESIAN_POINT('Ctrl Pts',(-1.44674311900006,12.2,3.72293989599999));
#302917=CARTESIAN_POINT('Ctrl Pts',(-1.44674311900006,5.2,3.72293989599999));
#302918=CARTESIAN_POINT('Ctrl Pts',(-1.44674311900006,2.2,3.72293989599999));
#302919=CARTESIAN_POINT('Ctrl Pts',(-1.44671532800006,12.2,3.72286516999999));
#302920=CARTESIAN_POINT('Ctrl Pts',(-1.44671532800006,5.2,3.72286516999999));
#302921=CARTESIAN_POINT('Ctrl Pts',(-1.44671532800006,2.2,3.72286516999999));
#302922=CARTESIAN_POINT('Ctrl Pts',(-1.44669000500006,12.2,3.72279733399999));
#302923=CARTESIAN_POINT('Ctrl Pts',(-1.44669000500006,5.2,3.72279733399999));
#302924=CARTESIAN_POINT('Ctrl Pts',(-1.44669000500006,2.2,3.72279733399999));
#302925=CARTESIAN_POINT('Ctrl Pts',(-1.44666717300006,12.2,3.72273639799998));
#302926=CARTESIAN_POINT('Ctrl Pts',(-1.44666717300006,5.2,3.72273639799998));
#302927=CARTESIAN_POINT('Ctrl Pts',(-1.44666717300006,2.2,3.72273639799998));
#302928=CARTESIAN_POINT('Ctrl Pts',(-1.44664685600006,12.2,3.72268236899998));
#302929=CARTESIAN_POINT('Ctrl Pts',(-1.44664685600006,5.2,3.72268236899998));
#302930=CARTESIAN_POINT('Ctrl Pts',(-1.44664685600006,2.2,3.72268236899998));
#302931=CARTESIAN_POINT('Ctrl Pts',(-1.44662715937635,12.2,3.72263020704428));
#302932=CARTESIAN_POINT('Ctrl Pts',(-1.44662715937635,5.2,3.72263020704428));
#302933=CARTESIAN_POINT('Ctrl Pts',(-1.44662715937635,2.2,3.72263020704428));
#302934=CARTESIAN_POINT('Ctrl Pts',(-1.44661362254973,12.2,3.72259457946533));
#302935=CARTESIAN_POINT('Ctrl Pts',(-1.44661362254973,5.2,3.72259457946533));
#302936=CARTESIAN_POINT('Ctrl Pts',(-1.44661362254973,2.2,3.72259457946533));
#302937=CARTESIAN_POINT('Ctrl Pts',(-1.44660465484929,12.2,3.72257112803267));
#302938=CARTESIAN_POINT('Ctrl Pts',(-1.44660465484929,5.2,3.72257112803267));
#302939=CARTESIAN_POINT('Ctrl Pts',(-1.44660465484929,2.2,3.72257112803267));
#302940=CARTESIAN_POINT('Ctrl Pts',(-1.44659903765901,12.2,3.7225565310091));
#302941=CARTESIAN_POINT('Ctrl Pts',(-1.44659903765901,5.2,3.7225565310091));
#302942=CARTESIAN_POINT('Ctrl Pts',(-1.44659903765901,2.2,3.7225565310091));
#302943=CARTESIAN_POINT('Ctrl Pts',(-1.44659557100006,12.2,3.72254751699998));
#302944=CARTESIAN_POINT('Ctrl Pts',(-1.44659557100006,5.2,3.72254751699998));
#302945=CARTESIAN_POINT('Ctrl Pts',(-1.44659557100006,2.2,3.72254751699998));
#302946=CARTESIAN_POINT('',(-1.44659576000006,2.7,3.72254744499998));
#302947=CARTESIAN_POINT('',(-1.44659576000006,12.2,3.72254744499998));
#302948=CARTESIAN_POINT('Ctrl Pts',(-1.39835267900006,2.7,4.53950545599999));
#302949=CARTESIAN_POINT('Ctrl Pts',(-1.46128293091346,2.7,4.3149625643711));
#302950=CARTESIAN_POINT('Ctrl Pts',(-1.48231430522207,2.7,4.12307648969267));
#302951=CARTESIAN_POINT('Ctrl Pts',(-1.47777222782857,2.7,3.81654919462578));
#302952=CARTESIAN_POINT('Ctrl Pts',(-1.4509749893252,2.7,3.73439048105048));
#302953=CARTESIAN_POINT('Ctrl Pts',(-1.44671500473292,2.7,3.72286373140579));
#302954=CARTESIAN_POINT('Ctrl Pts',(-1.44665623704781,2.7,3.72270526090141));
#302955=CARTESIAN_POINT('Ctrl Pts',(-1.44659557100006,2.7,3.72254751699998));
#302956=CARTESIAN_POINT('Origin',(-1.44657717200006,15.2,3.72249961199999));
#302957=CARTESIAN_POINT('',(-1.31303067400006,2.7,3.37884232399999));
#302958=CARTESIAN_POINT('',(-1.31303067400006,2.2,3.37884232399999));
#302959=CARTESIAN_POINT('',(-0.723288586352956,2.7,1.86124980586285));
#302960=CARTESIAN_POINT('Origin',(-5.66300478732629E-14,15.2,-1.77635683940025E-14));
#302961=CARTESIAN_POINT('',(-1.81888661200006,2.7,3.13564610499998));
#302962=CARTESIAN_POINT('',(-1.81888661200006,12.2,3.13564610499999));
#302963=CARTESIAN_POINT('Origin',(-5.66300478732629E-14,2.7,-1.92943768261394E-14));
#302964=CARTESIAN_POINT('Origin',(-5.66300478732629E-14,15.2,-1.77635683940025E-14));
#302965=CARTESIAN_POINT('',(-2.00390017000006,2.7,3.45459784199999));
#302966=CARTESIAN_POINT('',(-2.00390017000006,12.2,3.45459784199999));
#302967=CARTESIAN_POINT('',(-5.6975542132353E-14,2.7,-1.86987664562669E-14));
#302968=CARTESIAN_POINT('Ctrl Pts',(-2.00390028800005,12.2,3.45459777299999));
#302969=CARTESIAN_POINT('Ctrl Pts',(-2.00390028800005,5.2,3.45459777299999));
#302970=CARTESIAN_POINT('Ctrl Pts',(-2.00390028800005,2.2,3.45459777299999));
#302971=CARTESIAN_POINT('Ctrl Pts',(-2.00390374300006,12.2,3.45460367899998));
#302972=CARTESIAN_POINT('Ctrl Pts',(-2.00390374300006,5.2,3.45460367899998));
#302973=CARTESIAN_POINT('Ctrl Pts',(-2.00390374300006,2.2,3.45460367899998));
#302974=CARTESIAN_POINT('Ctrl Pts',(-2.00391042944521,12.2,3.45461510030709));
#302975=CARTESIAN_POINT('Ctrl Pts',(-2.00391042944521,5.2,3.45461510030709));
#302976=CARTESIAN_POINT('Ctrl Pts',(-2.00391042944521,2.2,3.45461510030709));
#302977=CARTESIAN_POINT('Ctrl Pts',(-2.00392033978938,12.2,3.4546320379243));
#302978=CARTESIAN_POINT('Ctrl Pts',(-2.00392033978938,5.2,3.4546320379243));
#302979=CARTESIAN_POINT('Ctrl Pts',(-2.00392033978938,2.2,3.4546320379243));
#302980=CARTESIAN_POINT('Ctrl Pts',(-2.00393346686492,12.2,3.45465453404064));
#302981=CARTESIAN_POINT('Ctrl Pts',(-2.00393346686492,5.2,3.45465453404064));
#302982=CARTESIAN_POINT('Ctrl Pts',(-2.00393346686492,2.2,3.45465453404064));
#302983=CARTESIAN_POINT('Ctrl Pts',(-2.00395653200005,12.2,3.45469348599998));
#302984=CARTESIAN_POINT('Ctrl Pts',(-2.00395653200005,5.2,3.45469348599998));
#302985=CARTESIAN_POINT('Ctrl Pts',(-2.00395653200005,2.2,3.45469348599998));
#302986=CARTESIAN_POINT('Ctrl Pts',(-2.00398222000006,12.2,3.45473680799999));
#302987=CARTESIAN_POINT('Ctrl Pts',(-2.00398222000006,5.2,3.45473680799999));
#302988=CARTESIAN_POINT('Ctrl Pts',(-2.00398222000006,2.2,3.45473680799999));
#302989=CARTESIAN_POINT('Ctrl Pts',(-2.00401172800006,12.2,3.45478641899999));
#302990=CARTESIAN_POINT('Ctrl Pts',(-2.00401172800006,5.2,3.45478641899999));
#302991=CARTESIAN_POINT('Ctrl Pts',(-2.00401172800006,2.2,3.45478641899999));
#302992=CARTESIAN_POINT('Ctrl Pts',(-2.00404506100006,12.2,3.45484230499999));
#302993=CARTESIAN_POINT('Ctrl Pts',(-2.00404506100006,5.2,3.45484230499999));
#302994=CARTESIAN_POINT('Ctrl Pts',(-2.00404506100006,2.2,3.45484230499999));
#302995=CARTESIAN_POINT('Ctrl Pts',(-2.00408222600006,12.2,3.45490444799999));
#302996=CARTESIAN_POINT('Ctrl Pts',(-2.00408222600006,5.2,3.45490444799999));
#302997=CARTESIAN_POINT('Ctrl Pts',(-2.00408222600006,2.2,3.45490444799999));
#302998=CARTESIAN_POINT('Ctrl Pts',(-2.00412323200006,12.2,3.45497281999998));
#302999=CARTESIAN_POINT('Ctrl Pts',(-2.00412323200006,5.2,3.45497281999998));
#303000=CARTESIAN_POINT('Ctrl Pts',(-2.00412323200006,2.2,3.45497281999998));
#303001=CARTESIAN_POINT('Ctrl Pts',(-2.00416808800005,12.2,3.45504738999999));
#303002=CARTESIAN_POINT('Ctrl Pts',(-2.00416808800005,5.2,3.45504738999999));
#303003=CARTESIAN_POINT('Ctrl Pts',(-2.00416808800005,2.2,3.45504738999999));
#303004=CARTESIAN_POINT('Ctrl Pts',(-2.00421680500006,12.2,3.45512812799999));
#303005=CARTESIAN_POINT('Ctrl Pts',(-2.00421680500006,5.2,3.45512812799999));
#303006=CARTESIAN_POINT('Ctrl Pts',(-2.00421680500006,2.2,3.45512812799999));
#303007=CARTESIAN_POINT('Ctrl Pts',(-2.00426939400006,12.2,3.45521500299999));
#303008=CARTESIAN_POINT('Ctrl Pts',(-2.00426939400006,5.2,3.45521500299999));
#303009=CARTESIAN_POINT('Ctrl Pts',(-2.00426939400006,2.2,3.45521500299999));
#303010=CARTESIAN_POINT('Ctrl Pts',(-2.00432586000006,12.2,3.45530799099999));
#303011=CARTESIAN_POINT('Ctrl Pts',(-2.00432586000006,5.2,3.45530799099999));
#303012=CARTESIAN_POINT('Ctrl Pts',(-2.00432586000006,2.2,3.45530799099999));
#303013=CARTESIAN_POINT('Ctrl Pts',(-2.00438621300006,12.2,3.45540706999999));
#303014=CARTESIAN_POINT('Ctrl Pts',(-2.00438621300006,5.2,3.45540706999999));
#303015=CARTESIAN_POINT('Ctrl Pts',(-2.00438621300006,2.2,3.45540706999999));
#303016=CARTESIAN_POINT('Ctrl Pts',(-2.00445045700006,12.2,3.45551221899999));
#303017=CARTESIAN_POINT('Ctrl Pts',(-2.00445045700006,5.2,3.45551221899999));
#303018=CARTESIAN_POINT('Ctrl Pts',(-2.00445045700006,2.2,3.45551221899999));
#303019=CARTESIAN_POINT('Ctrl Pts',(-2.00451860300006,12.2,3.45562341599998));
#303020=CARTESIAN_POINT('Ctrl Pts',(-2.00451860300006,5.2,3.45562341599998));
#303021=CARTESIAN_POINT('Ctrl Pts',(-2.00451860300006,2.2,3.45562341599998));
#303022=CARTESIAN_POINT('Ctrl Pts',(-2.00459065500006,12.2,3.45574063699999));
#303023=CARTESIAN_POINT('Ctrl Pts',(-2.00459065500006,5.2,3.45574063699999));
#303024=CARTESIAN_POINT('Ctrl Pts',(-2.00459065500006,2.2,3.45574063699999));
#303025=CARTESIAN_POINT('Ctrl Pts',(-2.00466662200005,12.2,3.45586385799999));
#303026=CARTESIAN_POINT('Ctrl Pts',(-2.00466662200005,5.2,3.45586385799999));
#303027=CARTESIAN_POINT('Ctrl Pts',(-2.00466662200005,2.2,3.45586385799999));
#303028=CARTESIAN_POINT('Ctrl Pts',(-2.00474651300006,12.2,3.45599305199999));
#303029=CARTESIAN_POINT('Ctrl Pts',(-2.00474651300006,5.2,3.45599305199999));
#303030=CARTESIAN_POINT('Ctrl Pts',(-2.00474651300006,2.2,3.45599305199999));
#303031=CARTESIAN_POINT('Ctrl Pts',(-2.00483033600006,12.2,3.45612819499999));
#303032=CARTESIAN_POINT('Ctrl Pts',(-2.00483033600006,5.2,3.45612819499999));
#303033=CARTESIAN_POINT('Ctrl Pts',(-2.00483033600006,2.2,3.45612819499999));
#303034=CARTESIAN_POINT('Ctrl Pts',(-2.00491809800006,12.2,3.45626926299998));
#303035=CARTESIAN_POINT('Ctrl Pts',(-2.00491809800006,5.2,3.45626926299998));
#303036=CARTESIAN_POINT('Ctrl Pts',(-2.00491809800006,2.2,3.45626926299998));
#303037=CARTESIAN_POINT('Ctrl Pts',(-2.00500980600005,12.2,3.45641623299999));
#303038=CARTESIAN_POINT('Ctrl Pts',(-2.00500980600005,5.2,3.45641623299999));
#303039=CARTESIAN_POINT('Ctrl Pts',(-2.00500980600005,2.2,3.45641623299999));
#303040=CARTESIAN_POINT('Ctrl Pts',(-2.00510546900006,12.2,3.45656907899999));
#303041=CARTESIAN_POINT('Ctrl Pts',(-2.00510546900006,5.2,3.45656907899999));
#303042=CARTESIAN_POINT('Ctrl Pts',(-2.00510546900006,2.2,3.45656907899999));
#303043=CARTESIAN_POINT('Ctrl Pts',(-2.00520509200006,12.2,3.45672777999999));
#303044=CARTESIAN_POINT('Ctrl Pts',(-2.00520509200006,5.2,3.45672777999999));
#303045=CARTESIAN_POINT('Ctrl Pts',(-2.00520509200006,2.2,3.45672777999999));
#303046=CARTESIAN_POINT('Ctrl Pts',(-2.00530868400006,12.2,3.45689231299998));
#303047=CARTESIAN_POINT('Ctrl Pts',(-2.00530868400006,5.2,3.45689231299998));
#303048=CARTESIAN_POINT('Ctrl Pts',(-2.00530868400006,2.2,3.45689231299998));
#303049=CARTESIAN_POINT('Ctrl Pts',(-2.00541625000006,12.2,3.45706265199999));
#303050=CARTESIAN_POINT('Ctrl Pts',(-2.00541625000006,5.2,3.45706265199999));
#303051=CARTESIAN_POINT('Ctrl Pts',(-2.00541625000006,2.2,3.45706265199999));
#303052=CARTESIAN_POINT('Ctrl Pts',(-2.00552780100006,12.2,3.45723877799998));
#303053=CARTESIAN_POINT('Ctrl Pts',(-2.00552780100006,5.2,3.45723877799998));
#303054=CARTESIAN_POINT('Ctrl Pts',(-2.00552780100006,2.2,3.45723877799998));
#303055=CARTESIAN_POINT('Ctrl Pts',(-2.00564334200006,12.2,3.45742066199998));
#303056=CARTESIAN_POINT('Ctrl Pts',(-2.00564334200006,5.2,3.45742066199998));
#303057=CARTESIAN_POINT('Ctrl Pts',(-2.00564334200006,2.2,3.45742066199998));
#303058=CARTESIAN_POINT('Ctrl Pts',(-2.00576288000006,12.2,3.45760828499999));
#303059=CARTESIAN_POINT('Ctrl Pts',(-2.00576288000006,5.2,3.45760828499999));
#303060=CARTESIAN_POINT('Ctrl Pts',(-2.00576288000006,2.2,3.45760828499999));
#303061=CARTESIAN_POINT('Ctrl Pts',(-2.00588642200006,12.2,3.45780162099998));
#303062=CARTESIAN_POINT('Ctrl Pts',(-2.00588642200006,5.2,3.45780162099998));
#303063=CARTESIAN_POINT('Ctrl Pts',(-2.00588642200006,2.2,3.45780162099998));
#303064=CARTESIAN_POINT('Ctrl Pts',(-2.00601397600006,12.2,3.45800064899999));
#303065=CARTESIAN_POINT('Ctrl Pts',(-2.00601397600006,5.2,3.45800064899999));
#303066=CARTESIAN_POINT('Ctrl Pts',(-2.00601397600006,2.2,3.45800064899999));
#303067=CARTESIAN_POINT('Ctrl Pts',(-2.00614554900006,12.2,3.45820534399999));
#303068=CARTESIAN_POINT('Ctrl Pts',(-2.00614554900006,5.2,3.45820534399999));
#303069=CARTESIAN_POINT('Ctrl Pts',(-2.00614554900006,2.2,3.45820534399999));
#303070=CARTESIAN_POINT('Ctrl Pts',(-2.00628114700006,12.2,3.45841568499999));
#303071=CARTESIAN_POINT('Ctrl Pts',(-2.00628114700006,5.2,3.45841568499999));
#303072=CARTESIAN_POINT('Ctrl Pts',(-2.00628114700006,2.2,3.45841568499999));
#303073=CARTESIAN_POINT('Ctrl Pts',(-2.00642077800006,12.2,3.45863164899999));
#303074=CARTESIAN_POINT('Ctrl Pts',(-2.00642077800006,5.2,3.45863164899999));
#303075=CARTESIAN_POINT('Ctrl Pts',(-2.00642077800006,2.2,3.45863164899999));
#303076=CARTESIAN_POINT('Ctrl Pts',(-2.00656444800006,12.2,3.45885321099999));
#303077=CARTESIAN_POINT('Ctrl Pts',(-2.00656444800006,5.2,3.45885321099999));
#303078=CARTESIAN_POINT('Ctrl Pts',(-2.00656444800006,2.2,3.45885321099999));
#303079=CARTESIAN_POINT('Ctrl Pts',(-2.00671216400006,12.2,3.45908034999999));
#303080=CARTESIAN_POINT('Ctrl Pts',(-2.00671216400006,5.2,3.45908034999999));
#303081=CARTESIAN_POINT('Ctrl Pts',(-2.00671216400006,2.2,3.45908034999999));
#303082=CARTESIAN_POINT('Ctrl Pts',(-2.00686393300006,12.2,3.45931304199999));
#303083=CARTESIAN_POINT('Ctrl Pts',(-2.00686393300006,5.2,3.45931304199999));
#303084=CARTESIAN_POINT('Ctrl Pts',(-2.00686393300006,2.2,3.45931304199999));
#303085=CARTESIAN_POINT('Ctrl Pts',(-2.00701976100006,12.2,3.45955126599998));
#303086=CARTESIAN_POINT('Ctrl Pts',(-2.00701976100006,5.2,3.45955126599998));
#303087=CARTESIAN_POINT('Ctrl Pts',(-2.00701976100006,2.2,3.45955126599998));
#303088=CARTESIAN_POINT('Ctrl Pts',(-2.00717965500006,12.2,3.45979499899999));
#303089=CARTESIAN_POINT('Ctrl Pts',(-2.00717965500006,5.2,3.45979499899999));
#303090=CARTESIAN_POINT('Ctrl Pts',(-2.00717965500006,2.2,3.45979499899999));
#303091=CARTESIAN_POINT('Ctrl Pts',(-2.00734362100006,12.2,3.46004421799999));
#303092=CARTESIAN_POINT('Ctrl Pts',(-2.00734362100006,5.2,3.46004421799999));
#303093=CARTESIAN_POINT('Ctrl Pts',(-2.00734362100006,2.2,3.46004421799999));
#303094=CARTESIAN_POINT('Ctrl Pts',(-2.00751166900006,12.2,3.46029890099998));
#303095=CARTESIAN_POINT('Ctrl Pts',(-2.00751166900006,5.2,3.46029890099998));
#303096=CARTESIAN_POINT('Ctrl Pts',(-2.00751166900006,2.2,3.46029890099998));
#303097=CARTESIAN_POINT('Ctrl Pts',(-2.00768380000006,12.2,3.46055902599999));
#303098=CARTESIAN_POINT('Ctrl Pts',(-2.00768380000006,5.2,3.46055902599999));
#303099=CARTESIAN_POINT('Ctrl Pts',(-2.00768380000006,2.2,3.46055902599999));
#303100=CARTESIAN_POINT('Ctrl Pts',(-2.00786002500006,12.2,3.46082456999999));
#303101=CARTESIAN_POINT('Ctrl Pts',(-2.00786002500006,5.2,3.46082456999999));
#303102=CARTESIAN_POINT('Ctrl Pts',(-2.00786002500006,2.2,3.46082456999999));
#303103=CARTESIAN_POINT('Ctrl Pts',(-2.00804034800006,12.2,3.46109550999999));
#303104=CARTESIAN_POINT('Ctrl Pts',(-2.00804034800006,5.2,3.46109550999999));
#303105=CARTESIAN_POINT('Ctrl Pts',(-2.00804034800006,2.2,3.46109550999999));
#303106=CARTESIAN_POINT('Ctrl Pts',(-2.00822477600005,12.2,3.46137182599998));
#303107=CARTESIAN_POINT('Ctrl Pts',(-2.00822477600005,5.2,3.46137182599998));
#303108=CARTESIAN_POINT('Ctrl Pts',(-2.00822477600005,2.2,3.46137182599998));
#303109=CARTESIAN_POINT('Ctrl Pts',(-2.00841331600006,12.2,3.46165349399998));
#303110=CARTESIAN_POINT('Ctrl Pts',(-2.00841331600006,5.2,3.46165349399998));
#303111=CARTESIAN_POINT('Ctrl Pts',(-2.00841331600006,2.2,3.46165349399998));
#303112=CARTESIAN_POINT('Ctrl Pts',(-2.00860597300006,12.2,3.46194049399998));
#303113=CARTESIAN_POINT('Ctrl Pts',(-2.00860597300006,5.2,3.46194049399998));
#303114=CARTESIAN_POINT('Ctrl Pts',(-2.00860597300006,2.2,3.46194049399998));
#303115=CARTESIAN_POINT('Ctrl Pts',(-2.00880275500006,12.2,3.46223280199998));
#303116=CARTESIAN_POINT('Ctrl Pts',(-2.00880275500006,5.2,3.46223280199998));
#303117=CARTESIAN_POINT('Ctrl Pts',(-2.00880275500006,2.2,3.46223280199998));
#303118=CARTESIAN_POINT('Ctrl Pts',(-2.00900366600006,12.2,3.46253039699998));
#303119=CARTESIAN_POINT('Ctrl Pts',(-2.00900366600006,5.2,3.46253039699998));
#303120=CARTESIAN_POINT('Ctrl Pts',(-2.00900366600006,2.2,3.46253039699998));
#303121=CARTESIAN_POINT('Ctrl Pts',(-2.00920871300006,12.2,3.46283325799998));
#303122=CARTESIAN_POINT('Ctrl Pts',(-2.00920871300006,5.2,3.46283325799998));
#303123=CARTESIAN_POINT('Ctrl Pts',(-2.00920871300006,2.2,3.46283325799998));
#303124=CARTESIAN_POINT('Ctrl Pts',(-2.00941790300006,12.2,3.46314136199998));
#303125=CARTESIAN_POINT('Ctrl Pts',(-2.00941790300006,5.2,3.46314136199998));
#303126=CARTESIAN_POINT('Ctrl Pts',(-2.00941790300006,2.2,3.46314136199998));
#303127=CARTESIAN_POINT('Ctrl Pts',(-2.00963124100006,12.2,3.46345468799999));
#303128=CARTESIAN_POINT('Ctrl Pts',(-2.00963124100006,5.2,3.46345468799999));
#303129=CARTESIAN_POINT('Ctrl Pts',(-2.00963124100006,2.2,3.46345468799999));
#303130=CARTESIAN_POINT('Ctrl Pts',(-2.00984873400006,12.2,3.46377321299999));
#303131=CARTESIAN_POINT('Ctrl Pts',(-2.00984873400006,5.2,3.46377321299999));
#303132=CARTESIAN_POINT('Ctrl Pts',(-2.00984873400006,2.2,3.46377321299999));
#303133=CARTESIAN_POINT('Ctrl Pts',(-2.01007038700005,12.2,3.46409691799998));
#303134=CARTESIAN_POINT('Ctrl Pts',(-2.01007038700005,5.2,3.46409691799998));
#303135=CARTESIAN_POINT('Ctrl Pts',(-2.01007038700005,2.2,3.46409691799998));
#303136=CARTESIAN_POINT('Ctrl Pts',(-2.01029620600006,12.2,3.46442577899998));
#303137=CARTESIAN_POINT('Ctrl Pts',(-2.01029620600006,5.2,3.46442577899998));
#303138=CARTESIAN_POINT('Ctrl Pts',(-2.01029620600006,2.2,3.46442577899998));
#303139=CARTESIAN_POINT('Ctrl Pts',(-2.01052619700006,12.2,3.46475977699999));
#303140=CARTESIAN_POINT('Ctrl Pts',(-2.01052619700006,5.2,3.46475977699999));
#303141=CARTESIAN_POINT('Ctrl Pts',(-2.01052619700006,2.2,3.46475977699999));
#303142=CARTESIAN_POINT('Ctrl Pts',(-2.01076036700006,12.2,3.46509888899998));
#303143=CARTESIAN_POINT('Ctrl Pts',(-2.01076036700006,5.2,3.46509888899998));
#303144=CARTESIAN_POINT('Ctrl Pts',(-2.01076036700006,2.2,3.46509888899998));
#303145=CARTESIAN_POINT('Ctrl Pts',(-2.01099872000006,12.2,3.46544309399999));
#303146=CARTESIAN_POINT('Ctrl Pts',(-2.01099872000006,5.2,3.46544309399999));
#303147=CARTESIAN_POINT('Ctrl Pts',(-2.01099872000006,2.2,3.46544309399999));
#303148=CARTESIAN_POINT('Ctrl Pts',(-2.01124126300006,12.2,3.46579237099998));
#303149=CARTESIAN_POINT('Ctrl Pts',(-2.01124126300006,5.2,3.46579237099998));
#303150=CARTESIAN_POINT('Ctrl Pts',(-2.01124126300006,2.2,3.46579237099998));
#303151=CARTESIAN_POINT('Ctrl Pts',(-2.01148800000006,12.2,3.46614669899999));
#303152=CARTESIAN_POINT('Ctrl Pts',(-2.01148800000006,5.2,3.46614669899999));
#303153=CARTESIAN_POINT('Ctrl Pts',(-2.01148800000006,2.2,3.46614669899999));
#303154=CARTESIAN_POINT('Ctrl Pts',(-2.01173893900005,12.2,3.46650605599999));
#303155=CARTESIAN_POINT('Ctrl Pts',(-2.01173893900005,5.2,3.46650605599999));
#303156=CARTESIAN_POINT('Ctrl Pts',(-2.01173893900005,2.2,3.46650605599999));
#303157=CARTESIAN_POINT('Ctrl Pts',(-2.01199408500006,12.2,3.46687042099998));
#303158=CARTESIAN_POINT('Ctrl Pts',(-2.01199408500006,5.2,3.46687042099998));
#303159=CARTESIAN_POINT('Ctrl Pts',(-2.01199408500006,2.2,3.46687042099998));
#303160=CARTESIAN_POINT('Ctrl Pts',(-2.01225344200005,12.2,3.46723977499998));
#303161=CARTESIAN_POINT('Ctrl Pts',(-2.01225344200005,5.2,3.46723977499998));
#303162=CARTESIAN_POINT('Ctrl Pts',(-2.01225344200005,2.2,3.46723977499998));
#303163=CARTESIAN_POINT('Ctrl Pts',(-2.01251701700006,12.2,3.46761409499998));
#303164=CARTESIAN_POINT('Ctrl Pts',(-2.01251701700006,5.2,3.46761409499998));
#303165=CARTESIAN_POINT('Ctrl Pts',(-2.01251701700006,2.2,3.46761409499998));
#303166=CARTESIAN_POINT('Ctrl Pts',(-2.01278481500006,12.2,3.46799336099998));
#303167=CARTESIAN_POINT('Ctrl Pts',(-2.01278481500006,5.2,3.46799336099998));
#303168=CARTESIAN_POINT('Ctrl Pts',(-2.01278481500006,2.2,3.46799336099998));
#303169=CARTESIAN_POINT('Ctrl Pts',(-2.01305684200006,12.2,3.46837755199999));
#303170=CARTESIAN_POINT('Ctrl Pts',(-2.01305684200006,5.2,3.46837755199999));
#303171=CARTESIAN_POINT('Ctrl Pts',(-2.01305684200006,2.2,3.46837755199999));
#303172=CARTESIAN_POINT('Ctrl Pts',(-2.01333310200006,12.2,3.46876664699998));
#303173=CARTESIAN_POINT('Ctrl Pts',(-2.01333310200006,5.2,3.46876664699998));
#303174=CARTESIAN_POINT('Ctrl Pts',(-2.01333310200006,2.2,3.46876664699998));
#303175=CARTESIAN_POINT('Ctrl Pts',(-2.01361360100006,12.2,3.46916062499999));
#303176=CARTESIAN_POINT('Ctrl Pts',(-2.01361360100006,5.2,3.46916062499999));
#303177=CARTESIAN_POINT('Ctrl Pts',(-2.01361360100006,2.2,3.46916062499999));
#303178=CARTESIAN_POINT('Ctrl Pts',(-2.01389834600006,12.2,3.46955946699998));
#303179=CARTESIAN_POINT('Ctrl Pts',(-2.01389834600006,5.2,3.46955946699998));
#303180=CARTESIAN_POINT('Ctrl Pts',(-2.01389834600006,2.2,3.46955946699998));
#303181=CARTESIAN_POINT('Ctrl Pts',(-2.01418734100006,12.2,3.46996315099998));
#303182=CARTESIAN_POINT('Ctrl Pts',(-2.01418734100006,5.2,3.46996315099998));
#303183=CARTESIAN_POINT('Ctrl Pts',(-2.01418734100006,2.2,3.46996315099998));
#303184=CARTESIAN_POINT('Ctrl Pts',(-2.01448059000006,12.2,3.47037165699999));
#303185=CARTESIAN_POINT('Ctrl Pts',(-2.01448059000006,5.2,3.47037165699999));
#303186=CARTESIAN_POINT('Ctrl Pts',(-2.01448059000006,2.2,3.47037165699999));
#303187=CARTESIAN_POINT('Ctrl Pts',(-2.01477810100006,12.2,3.47078496399998));
#303188=CARTESIAN_POINT('Ctrl Pts',(-2.01477810100006,5.2,3.47078496399998));
#303189=CARTESIAN_POINT('Ctrl Pts',(-2.01477810100006,2.2,3.47078496399998));
#303190=CARTESIAN_POINT('Ctrl Pts',(-2.01507987500006,12.2,3.47120305099998));
#303191=CARTESIAN_POINT('Ctrl Pts',(-2.01507987500006,5.2,3.47120305099998));
#303192=CARTESIAN_POINT('Ctrl Pts',(-2.01507987500006,2.2,3.47120305099998));
#303193=CARTESIAN_POINT('Ctrl Pts',(-2.01538592200006,12.2,3.47162589999999));
#303194=CARTESIAN_POINT('Ctrl Pts',(-2.01538592200006,5.2,3.47162589999999));
#303195=CARTESIAN_POINT('Ctrl Pts',(-2.01538592200006,2.2,3.47162589999999));
#303196=CARTESIAN_POINT('Ctrl Pts',(-2.01569624400005,12.2,3.47205348999999));
#303197=CARTESIAN_POINT('Ctrl Pts',(-2.01569624400005,5.2,3.47205348999999));
#303198=CARTESIAN_POINT('Ctrl Pts',(-2.01569624400005,2.2,3.47205348999999));
#303199=CARTESIAN_POINT('Ctrl Pts',(-2.01601084700005,12.2,3.47248579799999));
#303200=CARTESIAN_POINT('Ctrl Pts',(-2.01601084700005,5.2,3.47248579799999));
#303201=CARTESIAN_POINT('Ctrl Pts',(-2.01601084700005,2.2,3.47248579799999));
#303202=CARTESIAN_POINT('Ctrl Pts',(-2.01632973500006,12.2,3.47292280699998));
#303203=CARTESIAN_POINT('Ctrl Pts',(-2.01632973500006,5.2,3.47292280699998));
#303204=CARTESIAN_POINT('Ctrl Pts',(-2.01632973500006,2.2,3.47292280699998));
#303205=CARTESIAN_POINT('Ctrl Pts',(-2.01665291500006,12.2,3.47336449599998));
#303206=CARTESIAN_POINT('Ctrl Pts',(-2.01665291500006,5.2,3.47336449599998));
#303207=CARTESIAN_POINT('Ctrl Pts',(-2.01665291500006,2.2,3.47336449599998));
#303208=CARTESIAN_POINT('Ctrl Pts',(-2.01698039000005,12.2,3.47381084599999));
#303209=CARTESIAN_POINT('Ctrl Pts',(-2.01698039000005,5.2,3.47381084599999));
#303210=CARTESIAN_POINT('Ctrl Pts',(-2.01698039000005,2.2,3.47381084599999));
#303211=CARTESIAN_POINT('Ctrl Pts',(-2.01731216500006,12.2,3.47426183399998));
#303212=CARTESIAN_POINT('Ctrl Pts',(-2.01731216500006,5.2,3.47426183399998));
#303213=CARTESIAN_POINT('Ctrl Pts',(-2.01731216500006,2.2,3.47426183399998));
#303214=CARTESIAN_POINT('Ctrl Pts',(-2.01764824700006,12.2,3.47471744199999));
#303215=CARTESIAN_POINT('Ctrl Pts',(-2.01764824700006,5.2,3.47471744199999));
#303216=CARTESIAN_POINT('Ctrl Pts',(-2.01764824700006,2.2,3.47471744199999));
#303217=CARTESIAN_POINT('Ctrl Pts',(-2.01798863800006,12.2,3.47517765199999));
#303218=CARTESIAN_POINT('Ctrl Pts',(-2.01798863800006,5.2,3.47517765199999));
#303219=CARTESIAN_POINT('Ctrl Pts',(-2.01798863800006,2.2,3.47517765199999));
#303220=CARTESIAN_POINT('Ctrl Pts',(-2.01833334400006,12.2,3.47564244099999));
#303221=CARTESIAN_POINT('Ctrl Pts',(-2.01833334400006,5.2,3.47564244099999));
#303222=CARTESIAN_POINT('Ctrl Pts',(-2.01833334400006,2.2,3.47564244099999));
#303223=CARTESIAN_POINT('Ctrl Pts',(-2.01868237000005,12.2,3.47611178899999));
#303224=CARTESIAN_POINT('Ctrl Pts',(-2.01868237000005,5.2,3.47611178899999));
#303225=CARTESIAN_POINT('Ctrl Pts',(-2.01868237000005,2.2,3.47611178899999));
#303226=CARTESIAN_POINT('Ctrl Pts',(-2.01903572100006,12.2,3.47658567899998));
#303227=CARTESIAN_POINT('Ctrl Pts',(-2.01903572100006,5.2,3.47658567899998));
#303228=CARTESIAN_POINT('Ctrl Pts',(-2.01903572100006,2.2,3.47658567899998));
#303229=CARTESIAN_POINT('Ctrl Pts',(-2.01939340100005,12.2,3.47706408999999));
#303230=CARTESIAN_POINT('Ctrl Pts',(-2.01939340100005,5.2,3.47706408999999));
#303231=CARTESIAN_POINT('Ctrl Pts',(-2.01939340100005,2.2,3.47706408999999));
#303232=CARTESIAN_POINT('Ctrl Pts',(-2.01975541400006,12.2,3.47754700199999));
#303233=CARTESIAN_POINT('Ctrl Pts',(-2.01975541400006,5.2,3.47754700199999));
#303234=CARTESIAN_POINT('Ctrl Pts',(-2.01975541400006,2.2,3.47754700199999));
#303235=CARTESIAN_POINT('Ctrl Pts',(-2.02012176600005,12.2,3.47803439599998));
#303236=CARTESIAN_POINT('Ctrl Pts',(-2.02012176600005,5.2,3.47803439599998));
#303237=CARTESIAN_POINT('Ctrl Pts',(-2.02012176600005,2.2,3.47803439599998));
#303238=CARTESIAN_POINT('Ctrl Pts',(-2.02049246100006,12.2,3.47852625099998));
#303239=CARTESIAN_POINT('Ctrl Pts',(-2.02049246100006,5.2,3.47852625099998));
#303240=CARTESIAN_POINT('Ctrl Pts',(-2.02049246100006,2.2,3.47852625099998));
#303241=CARTESIAN_POINT('Ctrl Pts',(-2.02086750300006,12.2,3.47902254999998));
#303242=CARTESIAN_POINT('Ctrl Pts',(-2.02086750300006,5.2,3.47902254999998));
#303243=CARTESIAN_POINT('Ctrl Pts',(-2.02086750300006,2.2,3.47902254999998));
#303244=CARTESIAN_POINT('Ctrl Pts',(-2.02124689700006,12.2,3.47952327299998));
#303245=CARTESIAN_POINT('Ctrl Pts',(-2.02124689700006,5.2,3.47952327299998));
#303246=CARTESIAN_POINT('Ctrl Pts',(-2.02124689700006,2.2,3.47952327299998));
#303247=CARTESIAN_POINT('Ctrl Pts',(-2.02163064700006,12.2,3.48002839899999));
#303248=CARTESIAN_POINT('Ctrl Pts',(-2.02163064700006,5.2,3.48002839899999));
#303249=CARTESIAN_POINT('Ctrl Pts',(-2.02163064700006,2.2,3.48002839899999));
#303250=CARTESIAN_POINT('Ctrl Pts',(-2.02201875900006,12.2,3.48053790899999));
#303251=CARTESIAN_POINT('Ctrl Pts',(-2.02201875900006,5.2,3.48053790899999));
#303252=CARTESIAN_POINT('Ctrl Pts',(-2.02201875900006,2.2,3.48053790899999));
#303253=CARTESIAN_POINT('Ctrl Pts',(-2.02241123400006,12.2,3.48105178599998));
#303254=CARTESIAN_POINT('Ctrl Pts',(-2.02241123400006,5.2,3.48105178599998));
#303255=CARTESIAN_POINT('Ctrl Pts',(-2.02241123400006,2.2,3.48105178599998));
#303256=CARTESIAN_POINT('Ctrl Pts',(-2.02280808000005,12.2,3.48157000899998));
#303257=CARTESIAN_POINT('Ctrl Pts',(-2.02280808000005,5.2,3.48157000899998));
#303258=CARTESIAN_POINT('Ctrl Pts',(-2.02280808000005,2.2,3.48157000899998));
#303259=CARTESIAN_POINT('Ctrl Pts',(-2.02320930000006,12.2,3.48209255899998));
#303260=CARTESIAN_POINT('Ctrl Pts',(-2.02320930000006,5.2,3.48209255899998));
#303261=CARTESIAN_POINT('Ctrl Pts',(-2.02320930000006,2.2,3.48209255899998));
#303262=CARTESIAN_POINT('Ctrl Pts',(-2.02361489700006,12.2,3.48261941699998));
#303263=CARTESIAN_POINT('Ctrl Pts',(-2.02361489700006,5.2,3.48261941699998));
#303264=CARTESIAN_POINT('Ctrl Pts',(-2.02361489700006,2.2,3.48261941699998));
#303265=CARTESIAN_POINT('Ctrl Pts',(-2.02402487700006,12.2,3.48315056399999));
#303266=CARTESIAN_POINT('Ctrl Pts',(-2.02402487700006,5.2,3.48315056399999));
#303267=CARTESIAN_POINT('Ctrl Pts',(-2.02402487700006,2.2,3.48315056399999));
#303268=CARTESIAN_POINT('Ctrl Pts',(-2.02443924200006,12.2,3.48368597999999));
#303269=CARTESIAN_POINT('Ctrl Pts',(-2.02443924200006,5.2,3.48368597999999));
#303270=CARTESIAN_POINT('Ctrl Pts',(-2.02443924200006,2.2,3.48368597999999));
#303271=CARTESIAN_POINT('Ctrl Pts',(-2.02485799900006,12.2,3.48422564899998));
#303272=CARTESIAN_POINT('Ctrl Pts',(-2.02485799900006,5.2,3.48422564899998));
#303273=CARTESIAN_POINT('Ctrl Pts',(-2.02485799900006,2.2,3.48422564899998));
#303274=CARTESIAN_POINT('Ctrl Pts',(-2.02528115000006,12.2,3.48476954899999));
#303275=CARTESIAN_POINT('Ctrl Pts',(-2.02528115000006,5.2,3.48476954899999));
#303276=CARTESIAN_POINT('Ctrl Pts',(-2.02528115000006,2.2,3.48476954899999));
#303277=CARTESIAN_POINT('Ctrl Pts',(-2.02570870000006,12.2,3.48531766099998));
#303278=CARTESIAN_POINT('Ctrl Pts',(-2.02570870000006,5.2,3.48531766099998));
#303279=CARTESIAN_POINT('Ctrl Pts',(-2.02570870000006,2.2,3.48531766099998));
#303280=CARTESIAN_POINT('Ctrl Pts',(-2.02614065300006,12.2,3.48586996899999));
#303281=CARTESIAN_POINT('Ctrl Pts',(-2.02614065300006,5.2,3.48586996899999));
#303282=CARTESIAN_POINT('Ctrl Pts',(-2.02614065300006,2.2,3.48586996899999));
#303283=CARTESIAN_POINT('Ctrl Pts',(-2.02657701300006,12.2,3.48642645299999));
#303284=CARTESIAN_POINT('Ctrl Pts',(-2.02657701300006,5.2,3.48642645299999));
#303285=CARTESIAN_POINT('Ctrl Pts',(-2.02657701300006,2.2,3.48642645299999));
#303286=CARTESIAN_POINT('Ctrl Pts',(-2.02701778400006,12.2,3.48698709399999));
#303287=CARTESIAN_POINT('Ctrl Pts',(-2.02701778400006,5.2,3.48698709399999));
#303288=CARTESIAN_POINT('Ctrl Pts',(-2.02701778400006,2.2,3.48698709399999));
#303289=CARTESIAN_POINT('Ctrl Pts',(-2.02746296900005,12.2,3.48755187299999));
#303290=CARTESIAN_POINT('Ctrl Pts',(-2.02746296900005,5.2,3.48755187299999));
#303291=CARTESIAN_POINT('Ctrl Pts',(-2.02746296900005,2.2,3.48755187299999));
#303292=CARTESIAN_POINT('Ctrl Pts',(-2.02791257300006,12.2,3.48812077099999));
#303293=CARTESIAN_POINT('Ctrl Pts',(-2.02791257300006,5.2,3.48812077099999));
#303294=CARTESIAN_POINT('Ctrl Pts',(-2.02791257300006,2.2,3.48812077099999));
#303295=CARTESIAN_POINT('Ctrl Pts',(-2.02836659900006,12.2,3.48869377099999));
#303296=CARTESIAN_POINT('Ctrl Pts',(-2.02836659900006,5.2,3.48869377099999));
#303297=CARTESIAN_POINT('Ctrl Pts',(-2.02836659900006,2.2,3.48869377099999));
#303298=CARTESIAN_POINT('Ctrl Pts',(-2.02882505200006,12.2,3.48927085299999));
#303299=CARTESIAN_POINT('Ctrl Pts',(-2.02882505200006,5.2,3.48927085299999));
#303300=CARTESIAN_POINT('Ctrl Pts',(-2.02882505200006,2.2,3.48927085299999));
#303301=CARTESIAN_POINT('Ctrl Pts',(-2.02928793500006,12.2,3.48985199999999));
#303302=CARTESIAN_POINT('Ctrl Pts',(-2.02928793500006,5.2,3.48985199999999));
#303303=CARTESIAN_POINT('Ctrl Pts',(-2.02928793500006,2.2,3.48985199999999));
#303304=CARTESIAN_POINT('Ctrl Pts',(-2.02975525200006,12.2,3.49043719299999));
#303305=CARTESIAN_POINT('Ctrl Pts',(-2.02975525200006,5.2,3.49043719299999));
#303306=CARTESIAN_POINT('Ctrl Pts',(-2.02975525200006,2.2,3.49043719299999));
#303307=CARTESIAN_POINT('Ctrl Pts',(-2.03022700700005,12.2,3.49102641199998));
#303308=CARTESIAN_POINT('Ctrl Pts',(-2.03022700700005,5.2,3.49102641199998));
#303309=CARTESIAN_POINT('Ctrl Pts',(-2.03022700700005,2.2,3.49102641199998));
#303310=CARTESIAN_POINT('Ctrl Pts',(-2.03070320300006,12.2,3.49161964199999));
#303311=CARTESIAN_POINT('Ctrl Pts',(-2.03070320300006,5.2,3.49161964199999));
#303312=CARTESIAN_POINT('Ctrl Pts',(-2.03070320300006,2.2,3.49161964199999));
#303313=CARTESIAN_POINT('Ctrl Pts',(-2.03118384500006,12.2,3.49221686199999));
#303314=CARTESIAN_POINT('Ctrl Pts',(-2.03118384500006,5.2,3.49221686199999));
#303315=CARTESIAN_POINT('Ctrl Pts',(-2.03118384500006,2.2,3.49221686199999));
#303316=CARTESIAN_POINT('Ctrl Pts',(-2.03166893600006,12.2,3.49281805499999));
#303317=CARTESIAN_POINT('Ctrl Pts',(-2.03166893600006,5.2,3.49281805499999));
#303318=CARTESIAN_POINT('Ctrl Pts',(-2.03166893600006,2.2,3.49281805499999));
#303319=CARTESIAN_POINT('Ctrl Pts',(-2.03215847800006,12.2,3.49342320099999));
#303320=CARTESIAN_POINT('Ctrl Pts',(-2.03215847800006,5.2,3.49342320099999));
#303321=CARTESIAN_POINT('Ctrl Pts',(-2.03215847800006,2.2,3.49342320099999));
#303322=CARTESIAN_POINT('Ctrl Pts',(-2.03265247700006,12.2,3.49403228499998));
#303323=CARTESIAN_POINT('Ctrl Pts',(-2.03265247700006,5.2,3.49403228499998));
#303324=CARTESIAN_POINT('Ctrl Pts',(-2.03265247700006,2.2,3.49403228499998));
#303325=CARTESIAN_POINT('Ctrl Pts',(-2.03315093500006,12.2,3.49464528699999));
#303326=CARTESIAN_POINT('Ctrl Pts',(-2.03315093500006,5.2,3.49464528699999));
#303327=CARTESIAN_POINT('Ctrl Pts',(-2.03315093500006,2.2,3.49464528699999));
#303328=CARTESIAN_POINT('Ctrl Pts',(-2.03365385700006,12.2,3.49526218799999));
#303329=CARTESIAN_POINT('Ctrl Pts',(-2.03365385700006,5.2,3.49526218799999));
#303330=CARTESIAN_POINT('Ctrl Pts',(-2.03365385700006,2.2,3.49526218799999));
#303331=CARTESIAN_POINT('Ctrl Pts',(-2.03416124500006,12.2,3.49588297199999));
#303332=CARTESIAN_POINT('Ctrl Pts',(-2.03416124500006,5.2,3.49588297199999));
#303333=CARTESIAN_POINT('Ctrl Pts',(-2.03416124500006,2.2,3.49588297199999));
#303334=CARTESIAN_POINT('Ctrl Pts',(-2.03467310300006,12.2,3.49650761999998));
#303335=CARTESIAN_POINT('Ctrl Pts',(-2.03467310300006,5.2,3.49650761999998));
#303336=CARTESIAN_POINT('Ctrl Pts',(-2.03467310300006,2.2,3.49650761999998));
#303337=CARTESIAN_POINT('Ctrl Pts',(-2.03518943400006,12.2,3.49713611399999));
#303338=CARTESIAN_POINT('Ctrl Pts',(-2.03518943400006,5.2,3.49713611399999));
#303339=CARTESIAN_POINT('Ctrl Pts',(-2.03518943400006,2.2,3.49713611399999));
#303340=CARTESIAN_POINT('Ctrl Pts',(-2.03571024300006,12.2,3.49776843699999));
#303341=CARTESIAN_POINT('Ctrl Pts',(-2.03571024300006,5.2,3.49776843699999));
#303342=CARTESIAN_POINT('Ctrl Pts',(-2.03571024300006,2.2,3.49776843699999));
#303343=CARTESIAN_POINT('Ctrl Pts',(-2.03623553100006,12.2,3.49840457099998));
#303344=CARTESIAN_POINT('Ctrl Pts',(-2.03623553100006,5.2,3.49840457099998));
#303345=CARTESIAN_POINT('Ctrl Pts',(-2.03623553100006,2.2,3.49840457099998));
#303346=CARTESIAN_POINT('Ctrl Pts',(-2.03676530300006,12.2,3.49904449799999));
#303347=CARTESIAN_POINT('Ctrl Pts',(-2.03676530300006,5.2,3.49904449799999));
#303348=CARTESIAN_POINT('Ctrl Pts',(-2.03676530300006,2.2,3.49904449799999));
#303349=CARTESIAN_POINT('Ctrl Pts',(-2.03729956200006,12.2,3.49968819899999));
#303350=CARTESIAN_POINT('Ctrl Pts',(-2.03729956200006,5.2,3.49968819899999));
#303351=CARTESIAN_POINT('Ctrl Pts',(-2.03729956200006,2.2,3.49968819899999));
#303352=CARTESIAN_POINT('Ctrl Pts',(-2.03783831100006,12.2,3.50033565799999));
#303353=CARTESIAN_POINT('Ctrl Pts',(-2.03783831100006,5.2,3.50033565799999));
#303354=CARTESIAN_POINT('Ctrl Pts',(-2.03783831100006,2.2,3.50033565799999));
#303355=CARTESIAN_POINT('Ctrl Pts',(-2.03838155400006,12.2,3.50098685599999));
#303356=CARTESIAN_POINT('Ctrl Pts',(-2.03838155400006,5.2,3.50098685599999));
#303357=CARTESIAN_POINT('Ctrl Pts',(-2.03838155400006,2.2,3.50098685599999));
#303358=CARTESIAN_POINT('Ctrl Pts',(-2.03892929300005,12.2,3.50164177699998));
#303359=CARTESIAN_POINT('Ctrl Pts',(-2.03892929300005,5.2,3.50164177699998));
#303360=CARTESIAN_POINT('Ctrl Pts',(-2.03892929300005,2.2,3.50164177699998));
#303361=CARTESIAN_POINT('Ctrl Pts',(-2.03948153100006,12.2,3.50230040299999));
#303362=CARTESIAN_POINT('Ctrl Pts',(-2.03948153100006,5.2,3.50230040299999));
#303363=CARTESIAN_POINT('Ctrl Pts',(-2.03948153100006,2.2,3.50230040299999));
#303364=CARTESIAN_POINT('Ctrl Pts',(-2.04003827300005,12.2,3.50296271599999));
#303365=CARTESIAN_POINT('Ctrl Pts',(-2.04003827300005,5.2,3.50296271599999));
#303366=CARTESIAN_POINT('Ctrl Pts',(-2.04003827300005,2.2,3.50296271599999));
#303367=CARTESIAN_POINT('Ctrl Pts',(-2.04059952000006,12.2,3.50362869699998));
#303368=CARTESIAN_POINT('Ctrl Pts',(-2.04059952000006,5.2,3.50362869699998));
#303369=CARTESIAN_POINT('Ctrl Pts',(-2.04059952000006,2.2,3.50362869699998));
#303370=CARTESIAN_POINT('Ctrl Pts',(-2.04116527700006,12.2,3.50429833199998));
#303371=CARTESIAN_POINT('Ctrl Pts',(-2.04116527700006,5.2,3.50429833199998));
#303372=CARTESIAN_POINT('Ctrl Pts',(-2.04116527700006,2.2,3.50429833199998));
#303373=CARTESIAN_POINT('Ctrl Pts',(-2.04173554600006,12.2,3.50497160199998));
#303374=CARTESIAN_POINT('Ctrl Pts',(-2.04173554600006,5.2,3.50497160199998));
#303375=CARTESIAN_POINT('Ctrl Pts',(-2.04173554600006,2.2,3.50497160199998));
#303376=CARTESIAN_POINT('Ctrl Pts',(-2.04231033000006,12.2,3.50564848799999));
#303377=CARTESIAN_POINT('Ctrl Pts',(-2.04231033000006,5.2,3.50564848799999));
#303378=CARTESIAN_POINT('Ctrl Pts',(-2.04231033000006,2.2,3.50564848799999));
#303379=CARTESIAN_POINT('Ctrl Pts',(-2.04288963300006,12.2,3.50632897599999));
#303380=CARTESIAN_POINT('Ctrl Pts',(-2.04288963300006,5.2,3.50632897599999));
#303381=CARTESIAN_POINT('Ctrl Pts',(-2.04288963300006,2.2,3.50632897599999));
#303382=CARTESIAN_POINT('Ctrl Pts',(-2.04347345600006,12.2,3.50701304499999));
#303383=CARTESIAN_POINT('Ctrl Pts',(-2.04347345600006,5.2,3.50701304499999));
#303384=CARTESIAN_POINT('Ctrl Pts',(-2.04347345600006,2.2,3.50701304499999));
#303385=CARTESIAN_POINT('Ctrl Pts',(-2.04406180300006,12.2,3.50770068099998));
#303386=CARTESIAN_POINT('Ctrl Pts',(-2.04406180300006,5.2,3.50770068099998));
#303387=CARTESIAN_POINT('Ctrl Pts',(-2.04406180300006,2.2,3.50770068099998));
#303388=CARTESIAN_POINT('Ctrl Pts',(-2.04465467800006,12.2,3.50839186499999));
#303389=CARTESIAN_POINT('Ctrl Pts',(-2.04465467800006,5.2,3.50839186499999));
#303390=CARTESIAN_POINT('Ctrl Pts',(-2.04465467800006,2.2,3.50839186499999));
#303391=CARTESIAN_POINT('Ctrl Pts',(-2.04525208200006,12.2,3.50908657999998));
#303392=CARTESIAN_POINT('Ctrl Pts',(-2.04525208200006,5.2,3.50908657999998));
#303393=CARTESIAN_POINT('Ctrl Pts',(-2.04525208200006,2.2,3.50908657999998));
#303394=CARTESIAN_POINT('Ctrl Pts',(-2.04585401900006,12.2,3.50978480999999));
#303395=CARTESIAN_POINT('Ctrl Pts',(-2.04585401900006,5.2,3.50978480999999));
#303396=CARTESIAN_POINT('Ctrl Pts',(-2.04585401900006,2.2,3.50978480999999));
#303397=CARTESIAN_POINT('Ctrl Pts',(-2.04646049200006,12.2,3.51048653799998));
#303398=CARTESIAN_POINT('Ctrl Pts',(-2.04646049200006,5.2,3.51048653799998));
#303399=CARTESIAN_POINT('Ctrl Pts',(-2.04646049200006,2.2,3.51048653799998));
#303400=CARTESIAN_POINT('Ctrl Pts',(-2.04707150300006,12.2,3.51119174499999));
#303401=CARTESIAN_POINT('Ctrl Pts',(-2.04707150300006,5.2,3.51119174499999));
#303402=CARTESIAN_POINT('Ctrl Pts',(-2.04707150300006,2.2,3.51119174499999));
#303403=CARTESIAN_POINT('Ctrl Pts',(-2.04768705500005,12.2,3.51190041499999));
#303404=CARTESIAN_POINT('Ctrl Pts',(-2.04768705500005,5.2,3.51190041499999));
#303405=CARTESIAN_POINT('Ctrl Pts',(-2.04768705500005,2.2,3.51190041499999));
#303406=CARTESIAN_POINT('Ctrl Pts',(-2.04830715100006,12.2,3.51261253299998));
#303407=CARTESIAN_POINT('Ctrl Pts',(-2.04830715100006,5.2,3.51261253299998));
#303408=CARTESIAN_POINT('Ctrl Pts',(-2.04830715100006,2.2,3.51261253299998));
#303409=CARTESIAN_POINT('Ctrl Pts',(-2.04893179400006,12.2,3.51332807899999));
#303410=CARTESIAN_POINT('Ctrl Pts',(-2.04893179400006,5.2,3.51332807899999));
#303411=CARTESIAN_POINT('Ctrl Pts',(-2.04893179400006,2.2,3.51332807899999));
#303412=CARTESIAN_POINT('Ctrl Pts',(-2.04956098500006,12.2,3.51404703799999));
#303413=CARTESIAN_POINT('Ctrl Pts',(-2.04956098500006,5.2,3.51404703799999));
#303414=CARTESIAN_POINT('Ctrl Pts',(-2.04956098500006,2.2,3.51404703799999));
#303415=CARTESIAN_POINT('Ctrl Pts',(-2.05019473000006,12.2,3.51476939299998));
#303416=CARTESIAN_POINT('Ctrl Pts',(-2.05019473000006,5.2,3.51476939299998));
#303417=CARTESIAN_POINT('Ctrl Pts',(-2.05019473000006,2.2,3.51476939299998));
#303418=CARTESIAN_POINT('Ctrl Pts',(-2.05083302700006,12.2,3.51549512699999));
#303419=CARTESIAN_POINT('Ctrl Pts',(-2.05083302700006,5.2,3.51549512699999));
#303420=CARTESIAN_POINT('Ctrl Pts',(-2.05083302700006,2.2,3.51549512699999));
#303421=CARTESIAN_POINT('Ctrl Pts',(-2.05147588300005,12.2,3.51622422299998));
#303422=CARTESIAN_POINT('Ctrl Pts',(-2.05147588300005,5.2,3.51622422299998));
#303423=CARTESIAN_POINT('Ctrl Pts',(-2.05147588300005,2.2,3.51622422299998));
#303424=CARTESIAN_POINT('Ctrl Pts',(-2.05212329700006,12.2,3.51695666399999));
#303425=CARTESIAN_POINT('Ctrl Pts',(-2.05212329700006,5.2,3.51695666399999));
#303426=CARTESIAN_POINT('Ctrl Pts',(-2.05212329700006,2.2,3.51695666399999));
#303427=CARTESIAN_POINT('Ctrl Pts',(-2.05277527500006,12.2,3.51769243499999));
#303428=CARTESIAN_POINT('Ctrl Pts',(-2.05277527500006,5.2,3.51769243499999));
#303429=CARTESIAN_POINT('Ctrl Pts',(-2.05277527500006,2.2,3.51769243499999));
#303430=CARTESIAN_POINT('Ctrl Pts',(-2.05343181700006,12.2,3.51843151799999));
#303431=CARTESIAN_POINT('Ctrl Pts',(-2.05343181700006,5.2,3.51843151799999));
#303432=CARTESIAN_POINT('Ctrl Pts',(-2.05343181700006,2.2,3.51843151799999));
#303433=CARTESIAN_POINT('Ctrl Pts',(-2.05409292700006,12.2,3.51917389699998));
#303434=CARTESIAN_POINT('Ctrl Pts',(-2.05409292700006,5.2,3.51917389699998));
#303435=CARTESIAN_POINT('Ctrl Pts',(-2.05409292700006,2.2,3.51917389699998));
#303436=CARTESIAN_POINT('Ctrl Pts',(-2.05475860500006,12.2,3.51991955499999));
#303437=CARTESIAN_POINT('Ctrl Pts',(-2.05475860500006,5.2,3.51991955499999));
#303438=CARTESIAN_POINT('Ctrl Pts',(-2.05475860500006,2.2,3.51991955499999));
#303439=CARTESIAN_POINT('Ctrl Pts',(-2.05542885700006,12.2,3.52066847499999));
#303440=CARTESIAN_POINT('Ctrl Pts',(-2.05542885700006,5.2,3.52066847499999));
#303441=CARTESIAN_POINT('Ctrl Pts',(-2.05542885700006,2.2,3.52066847499999));
#303442=CARTESIAN_POINT('Ctrl Pts',(-2.05610368200006,12.2,3.52142064199998));
#303443=CARTESIAN_POINT('Ctrl Pts',(-2.05610368200006,5.2,3.52142064199998));
#303444=CARTESIAN_POINT('Ctrl Pts',(-2.05610368200006,2.2,3.52142064199998));
#303445=CARTESIAN_POINT('Ctrl Pts',(-2.05678308500006,12.2,3.52217603899999));
#303446=CARTESIAN_POINT('Ctrl Pts',(-2.05678308500006,5.2,3.52217603899999));
#303447=CARTESIAN_POINT('Ctrl Pts',(-2.05678308500006,2.2,3.52217603899999));
#303448=CARTESIAN_POINT('Ctrl Pts',(-2.05746706600006,12.2,3.52293464899999));
#303449=CARTESIAN_POINT('Ctrl Pts',(-2.05746706600006,5.2,3.52293464899999));
#303450=CARTESIAN_POINT('Ctrl Pts',(-2.05746706600006,2.2,3.52293464899999));
#303451=CARTESIAN_POINT('Ctrl Pts',(-2.05815563000006,12.2,3.52369645699999));
#303452=CARTESIAN_POINT('Ctrl Pts',(-2.05815563000006,5.2,3.52369645699999));
#303453=CARTESIAN_POINT('Ctrl Pts',(-2.05815563000006,2.2,3.52369645699999));
#303454=CARTESIAN_POINT('Ctrl Pts',(-2.05884877800006,12.2,3.52446144499999));
#303455=CARTESIAN_POINT('Ctrl Pts',(-2.05884877800006,5.2,3.52446144499999));
#303456=CARTESIAN_POINT('Ctrl Pts',(-2.05884877800006,2.2,3.52446144499999));
#303457=CARTESIAN_POINT('Ctrl Pts',(-2.05954651100006,12.2,3.52522959799998));
#303458=CARTESIAN_POINT('Ctrl Pts',(-2.05954651100006,5.2,3.52522959799998));
#303459=CARTESIAN_POINT('Ctrl Pts',(-2.05954651100006,2.2,3.52522959799998));
#303460=CARTESIAN_POINT('Ctrl Pts',(-2.06024883300006,12.2,3.52600089799999));
#303461=CARTESIAN_POINT('Ctrl Pts',(-2.06024883300006,5.2,3.52600089799999));
#303462=CARTESIAN_POINT('Ctrl Pts',(-2.06024883300006,2.2,3.52600089799999));
#303463=CARTESIAN_POINT('Ctrl Pts',(-2.06095574500006,12.2,3.52677533199999));
#303464=CARTESIAN_POINT('Ctrl Pts',(-2.06095574500006,5.2,3.52677533199999));
#303465=CARTESIAN_POINT('Ctrl Pts',(-2.06095574500006,2.2,3.52677533199999));
#303466=CARTESIAN_POINT('Ctrl Pts',(-2.06166725100006,12.2,3.52755288099999));
#303467=CARTESIAN_POINT('Ctrl Pts',(-2.06166725100006,5.2,3.52755288099999));
#303468=CARTESIAN_POINT('Ctrl Pts',(-2.06166725100006,2.2,3.52755288099999));
#303469=CARTESIAN_POINT('Ctrl Pts',(-2.06238335200006,12.2,3.52833352999999));
#303470=CARTESIAN_POINT('Ctrl Pts',(-2.06238335200006,5.2,3.52833352999999));
#303471=CARTESIAN_POINT('Ctrl Pts',(-2.06238335200006,2.2,3.52833352999999));
#303472=CARTESIAN_POINT('Ctrl Pts',(-2.06310404900006,12.2,3.52911726299999));
#303473=CARTESIAN_POINT('Ctrl Pts',(-2.06310404900006,5.2,3.52911726299999));
#303474=CARTESIAN_POINT('Ctrl Pts',(-2.06310404900006,2.2,3.52911726299999));
#303475=CARTESIAN_POINT('Ctrl Pts',(-2.06382934600006,12.2,3.52990406399999));
#303476=CARTESIAN_POINT('Ctrl Pts',(-2.06382934600006,5.2,3.52990406399999));
#303477=CARTESIAN_POINT('Ctrl Pts',(-2.06382934600006,2.2,3.52990406399999));
#303478=CARTESIAN_POINT('Ctrl Pts',(-2.06455924400006,12.2,3.53069391599998));
#303479=CARTESIAN_POINT('Ctrl Pts',(-2.06455924400006,5.2,3.53069391599998));
#303480=CARTESIAN_POINT('Ctrl Pts',(-2.06455924400006,2.2,3.53069391599998));
#303481=CARTESIAN_POINT('Ctrl Pts',(-2.06529374600006,12.2,3.53148680299999));
#303482=CARTESIAN_POINT('Ctrl Pts',(-2.06529374600006,5.2,3.53148680299999));
#303483=CARTESIAN_POINT('Ctrl Pts',(-2.06529374600006,2.2,3.53148680299999));
#303484=CARTESIAN_POINT('Ctrl Pts',(-2.06603285300006,12.2,3.53228271099999));
#303485=CARTESIAN_POINT('Ctrl Pts',(-2.06603285300006,5.2,3.53228271099999));
#303486=CARTESIAN_POINT('Ctrl Pts',(-2.06603285300006,2.2,3.53228271099999));
#303487=CARTESIAN_POINT('Ctrl Pts',(-2.06677656700006,12.2,3.53308162299999));
#303488=CARTESIAN_POINT('Ctrl Pts',(-2.06677656700006,5.2,3.53308162299999));
#303489=CARTESIAN_POINT('Ctrl Pts',(-2.06677656700006,2.2,3.53308162299999));
#303490=CARTESIAN_POINT('Ctrl Pts',(-2.06752489200006,12.2,3.53388352199998));
#303491=CARTESIAN_POINT('Ctrl Pts',(-2.06752489200006,5.2,3.53388352199998));
#303492=CARTESIAN_POINT('Ctrl Pts',(-2.06752489200006,2.2,3.53388352199998));
#303493=CARTESIAN_POINT('Ctrl Pts',(-2.06827782600006,12.2,3.53468839399999));
#303494=CARTESIAN_POINT('Ctrl Pts',(-2.06827782600006,5.2,3.53468839399999));
#303495=CARTESIAN_POINT('Ctrl Pts',(-2.06827782600006,2.2,3.53468839399999));
#303496=CARTESIAN_POINT('Ctrl Pts',(-2.06903537500006,12.2,3.53549622199999));
#303497=CARTESIAN_POINT('Ctrl Pts',(-2.06903537500006,5.2,3.53549622199999));
#303498=CARTESIAN_POINT('Ctrl Pts',(-2.06903537500006,2.2,3.53549622199999));
#303499=CARTESIAN_POINT('Ctrl Pts',(-2.06979753900006,12.2,3.53630699099998));
#303500=CARTESIAN_POINT('Ctrl Pts',(-2.06979753900006,5.2,3.53630699099998));
#303501=CARTESIAN_POINT('Ctrl Pts',(-2.06979753900006,2.2,3.53630699099998));
#303502=CARTESIAN_POINT('Ctrl Pts',(-2.07056432000006,12.2,3.53712068399999));
#303503=CARTESIAN_POINT('Ctrl Pts',(-2.07056432000006,5.2,3.53712068399999));
#303504=CARTESIAN_POINT('Ctrl Pts',(-2.07056432000006,2.2,3.53712068399999));
#303505=CARTESIAN_POINT('Ctrl Pts',(-2.07133572000005,12.2,3.53793728699999));
#303506=CARTESIAN_POINT('Ctrl Pts',(-2.07133572000005,5.2,3.53793728699999));
#303507=CARTESIAN_POINT('Ctrl Pts',(-2.07133572000005,2.2,3.53793728699999));
#303508=CARTESIAN_POINT('Ctrl Pts',(-2.07211174100005,12.2,3.53875678399999));
#303509=CARTESIAN_POINT('Ctrl Pts',(-2.07211174100005,5.2,3.53875678399999));
#303510=CARTESIAN_POINT('Ctrl Pts',(-2.07211174100005,2.2,3.53875678399999));
#303511=CARTESIAN_POINT('Ctrl Pts',(-2.07289238500006,12.2,3.53957915799998));
#303512=CARTESIAN_POINT('Ctrl Pts',(-2.07289238500006,5.2,3.53957915799998));
#303513=CARTESIAN_POINT('Ctrl Pts',(-2.07289238500006,2.2,3.53957915799998));
#303514=CARTESIAN_POINT('Ctrl Pts',(-2.07367765300006,12.2,3.54040439499999));
#303515=CARTESIAN_POINT('Ctrl Pts',(-2.07367765300006,5.2,3.54040439499999));
#303516=CARTESIAN_POINT('Ctrl Pts',(-2.07367765300006,2.2,3.54040439499999));
#303517=CARTESIAN_POINT('Ctrl Pts',(-2.07446754800006,12.2,3.54123247799999));
#303518=CARTESIAN_POINT('Ctrl Pts',(-2.07446754800006,5.2,3.54123247799999));
#303519=CARTESIAN_POINT('Ctrl Pts',(-2.07446754800006,2.2,3.54123247799999));
#303520=CARTESIAN_POINT('Ctrl Pts',(-2.07526207000006,12.2,3.54206339399998));
#303521=CARTESIAN_POINT('Ctrl Pts',(-2.07526207000006,5.2,3.54206339399998));
#303522=CARTESIAN_POINT('Ctrl Pts',(-2.07526207000006,2.2,3.54206339399998));
#303523=CARTESIAN_POINT('Ctrl Pts',(-2.07606122200006,12.2,3.54289712399999));
#303524=CARTESIAN_POINT('Ctrl Pts',(-2.07606122200006,5.2,3.54289712399999));
#303525=CARTESIAN_POINT('Ctrl Pts',(-2.07606122200006,2.2,3.54289712399999));
#303526=CARTESIAN_POINT('Ctrl Pts',(-2.07686500500006,12.2,3.54373365599999));
#303527=CARTESIAN_POINT('Ctrl Pts',(-2.07686500500006,5.2,3.54373365599999));
#303528=CARTESIAN_POINT('Ctrl Pts',(-2.07686500500006,2.2,3.54373365599999));
#303529=CARTESIAN_POINT('Ctrl Pts',(-2.07767342200006,12.2,3.54457297199998));
#303530=CARTESIAN_POINT('Ctrl Pts',(-2.07767342200006,5.2,3.54457297199998));
#303531=CARTESIAN_POINT('Ctrl Pts',(-2.07767342200006,2.2,3.54457297199998));
#303532=CARTESIAN_POINT('Ctrl Pts',(-2.07848647300006,12.2,3.54541505699999));
#303533=CARTESIAN_POINT('Ctrl Pts',(-2.07848647300006,5.2,3.54541505699999));
#303534=CARTESIAN_POINT('Ctrl Pts',(-2.07848647300006,2.2,3.54541505699999));
#303535=CARTESIAN_POINT('Ctrl Pts',(-2.07930416100006,12.2,3.54625989799998));
#303536=CARTESIAN_POINT('Ctrl Pts',(-2.07930416100006,5.2,3.54625989799998));
#303537=CARTESIAN_POINT('Ctrl Pts',(-2.07930416100006,2.2,3.54625989799998));
#303538=CARTESIAN_POINT('Ctrl Pts',(-2.08012648600006,12.2,3.54710747599999));
#303539=CARTESIAN_POINT('Ctrl Pts',(-2.08012648600006,5.2,3.54710747599999));
#303540=CARTESIAN_POINT('Ctrl Pts',(-2.08012648600006,2.2,3.54710747599999));
#303541=CARTESIAN_POINT('Ctrl Pts',(-2.08095345200006,12.2,3.54795777899999));
#303542=CARTESIAN_POINT('Ctrl Pts',(-2.08095345200006,5.2,3.54795777899999));
#303543=CARTESIAN_POINT('Ctrl Pts',(-2.08095345200006,2.2,3.54795777899999));
#303544=CARTESIAN_POINT('Ctrl Pts',(-2.08178505800006,12.2,3.54881078999998));
#303545=CARTESIAN_POINT('Ctrl Pts',(-2.08178505800006,5.2,3.54881078999998));
#303546=CARTESIAN_POINT('Ctrl Pts',(-2.08178505800006,2.2,3.54881078999998));
#303547=CARTESIAN_POINT('Ctrl Pts',(-2.08262130700006,12.2,3.54966649399999));
#303548=CARTESIAN_POINT('Ctrl Pts',(-2.08262130700006,5.2,3.54966649399999));
#303549=CARTESIAN_POINT('Ctrl Pts',(-2.08262130700006,2.2,3.54966649399999));
#303550=CARTESIAN_POINT('Ctrl Pts',(-2.08346219900006,12.2,3.55052487699999));
#303551=CARTESIAN_POINT('Ctrl Pts',(-2.08346219900006,5.2,3.55052487699999));
#303552=CARTESIAN_POINT('Ctrl Pts',(-2.08346219900006,2.2,3.55052487699999));
#303553=CARTESIAN_POINT('Ctrl Pts',(-2.08430773800006,12.2,3.55138592199998));
#303554=CARTESIAN_POINT('Ctrl Pts',(-2.08430773800006,5.2,3.55138592199998));
#303555=CARTESIAN_POINT('Ctrl Pts',(-2.08430773800006,2.2,3.55138592199998));
#303556=CARTESIAN_POINT('Ctrl Pts',(-2.08515792300005,12.2,3.55224961399998));
#303557=CARTESIAN_POINT('Ctrl Pts',(-2.08515792300005,5.2,3.55224961399998));
#303558=CARTESIAN_POINT('Ctrl Pts',(-2.08515792300005,2.2,3.55224961399998));
#303559=CARTESIAN_POINT('Ctrl Pts',(-2.08601275700006,12.2,3.55311593999998));
#303560=CARTESIAN_POINT('Ctrl Pts',(-2.08601275700006,5.2,3.55311593999998));
#303561=CARTESIAN_POINT('Ctrl Pts',(-2.08601275700006,2.2,3.55311593999998));
#303562=CARTESIAN_POINT('Ctrl Pts',(-2.08687224100006,12.2,3.55398488399998));
#303563=CARTESIAN_POINT('Ctrl Pts',(-2.08687224100006,5.2,3.55398488399998));
#303564=CARTESIAN_POINT('Ctrl Pts',(-2.08687224100006,2.2,3.55398488399998));
#303565=CARTESIAN_POINT('Ctrl Pts',(-2.08773637600005,12.2,3.55485642999999));
#303566=CARTESIAN_POINT('Ctrl Pts',(-2.08773637600005,5.2,3.55485642999999));
#303567=CARTESIAN_POINT('Ctrl Pts',(-2.08773637600005,2.2,3.55485642999999));
#303568=CARTESIAN_POINT('Ctrl Pts',(-2.08860516300006,12.2,3.55573056299999));
#303569=CARTESIAN_POINT('Ctrl Pts',(-2.08860516300006,5.2,3.55573056299999));
#303570=CARTESIAN_POINT('Ctrl Pts',(-2.08860516300006,2.2,3.55573056299999));
#303571=CARTESIAN_POINT('Ctrl Pts',(-2.08947860600006,12.2,3.55660726999999));
#303572=CARTESIAN_POINT('Ctrl Pts',(-2.08947860600006,5.2,3.55660726999999));
#303573=CARTESIAN_POINT('Ctrl Pts',(-2.08947860600006,2.2,3.55660726999999));
#303574=CARTESIAN_POINT('Ctrl Pts',(-2.09035670200006,12.2,3.55748653299998));
#303575=CARTESIAN_POINT('Ctrl Pts',(-2.09035670200006,5.2,3.55748653299998));
#303576=CARTESIAN_POINT('Ctrl Pts',(-2.09035670200006,2.2,3.55748653299998));
#303577=CARTESIAN_POINT('Ctrl Pts',(-2.09123945700005,12.2,3.55836833999999));
#303578=CARTESIAN_POINT('Ctrl Pts',(-2.09123945700005,5.2,3.55836833999999));
#303579=CARTESIAN_POINT('Ctrl Pts',(-2.09123945700005,2.2,3.55836833999999));
#303580=CARTESIAN_POINT('Ctrl Pts',(-2.09212686800006,12.2,3.55925267499998));
#303581=CARTESIAN_POINT('Ctrl Pts',(-2.09212686800006,5.2,3.55925267499998));
#303582=CARTESIAN_POINT('Ctrl Pts',(-2.09212686800006,2.2,3.55925267499998));
#303583=CARTESIAN_POINT('Ctrl Pts',(-2.09301893900005,12.2,3.56013952299998));
#303584=CARTESIAN_POINT('Ctrl Pts',(-2.09301893900005,5.2,3.56013952299998));
#303585=CARTESIAN_POINT('Ctrl Pts',(-2.09301893900005,2.2,3.56013952299998));
#303586=CARTESIAN_POINT('Ctrl Pts',(-2.09391567000006,12.2,3.56102886999999));
#303587=CARTESIAN_POINT('Ctrl Pts',(-2.09391567000006,5.2,3.56102886999999));
#303588=CARTESIAN_POINT('Ctrl Pts',(-2.09391567000006,2.2,3.56102886999999));
#303589=CARTESIAN_POINT('Ctrl Pts',(-2.09481706300005,12.2,3.56192070099999));
#303590=CARTESIAN_POINT('Ctrl Pts',(-2.09481706300005,5.2,3.56192070099999));
#303591=CARTESIAN_POINT('Ctrl Pts',(-2.09481706300005,2.2,3.56192070099999));
#303592=CARTESIAN_POINT('Ctrl Pts',(-2.09572311800006,12.2,3.56281500099998));
#303593=CARTESIAN_POINT('Ctrl Pts',(-2.09572311800006,5.2,3.56281500099998));
#303594=CARTESIAN_POINT('Ctrl Pts',(-2.09572311800006,2.2,3.56281500099998));
#303595=CARTESIAN_POINT('Ctrl Pts',(-2.09663383700006,12.2,3.56371175399998));
#303596=CARTESIAN_POINT('Ctrl Pts',(-2.09663383700006,5.2,3.56371175399998));
#303597=CARTESIAN_POINT('Ctrl Pts',(-2.09663383700006,2.2,3.56371175399998));
#303598=CARTESIAN_POINT('Ctrl Pts',(-2.09754922100006,12.2,3.56461094699998));
#303599=CARTESIAN_POINT('Ctrl Pts',(-2.09754922100006,5.2,3.56461094699998));
#303600=CARTESIAN_POINT('Ctrl Pts',(-2.09754922100006,2.2,3.56461094699998));
#303601=CARTESIAN_POINT('Ctrl Pts',(-2.09846927300006,12.2,3.56551256499999));
#303602=CARTESIAN_POINT('Ctrl Pts',(-2.09846927300006,5.2,3.56551256499999));
#303603=CARTESIAN_POINT('Ctrl Pts',(-2.09846927300006,2.2,3.56551256499999));
#303604=CARTESIAN_POINT('Ctrl Pts',(-2.09939399000006,12.2,3.56641659399998));
#303605=CARTESIAN_POINT('Ctrl Pts',(-2.09939399000006,5.2,3.56641659399998));
#303606=CARTESIAN_POINT('Ctrl Pts',(-2.09939399000006,2.2,3.56641659399998));
#303607=CARTESIAN_POINT('Ctrl Pts',(-2.10032337800006,12.2,3.56732301899999));
#303608=CARTESIAN_POINT('Ctrl Pts',(-2.10032337800006,5.2,3.56732301899999));
#303609=CARTESIAN_POINT('Ctrl Pts',(-2.10032337800006,2.2,3.56732301899999));
#303610=CARTESIAN_POINT('Ctrl Pts',(-2.10125743300006,12.2,3.56823182499999));
#303611=CARTESIAN_POINT('Ctrl Pts',(-2.10125743300006,5.2,3.56823182499999));
#303612=CARTESIAN_POINT('Ctrl Pts',(-2.10125743300006,2.2,3.56823182499999));
#303613=CARTESIAN_POINT('Ctrl Pts',(-2.10219615900006,12.2,3.56914299699999));
#303614=CARTESIAN_POINT('Ctrl Pts',(-2.10219615900006,5.2,3.56914299699999));
#303615=CARTESIAN_POINT('Ctrl Pts',(-2.10219615900006,2.2,3.56914299699999));
#303616=CARTESIAN_POINT('Ctrl Pts',(-2.10313955700005,12.2,3.57005652199998));
#303617=CARTESIAN_POINT('Ctrl Pts',(-2.10313955700005,5.2,3.57005652199998));
#303618=CARTESIAN_POINT('Ctrl Pts',(-2.10313955700005,2.2,3.57005652199998));
#303619=CARTESIAN_POINT('Ctrl Pts',(-2.10408762800005,12.2,3.57097238399999));
#303620=CARTESIAN_POINT('Ctrl Pts',(-2.10408762800005,5.2,3.57097238399999));
#303621=CARTESIAN_POINT('Ctrl Pts',(-2.10408762800005,2.2,3.57097238399999));
#303622=CARTESIAN_POINT('Ctrl Pts',(-2.10504037200006,12.2,3.57189057099998));
#303623=CARTESIAN_POINT('Ctrl Pts',(-2.10504037200006,5.2,3.57189057099998));
#303624=CARTESIAN_POINT('Ctrl Pts',(-2.10504037200006,2.2,3.57189057099998));
#303625=CARTESIAN_POINT('Ctrl Pts',(-2.10599779100006,12.2,3.57281106599999));
#303626=CARTESIAN_POINT('Ctrl Pts',(-2.10599779100006,5.2,3.57281106599999));
#303627=CARTESIAN_POINT('Ctrl Pts',(-2.10599779100006,2.2,3.57281106599999));
#303628=CARTESIAN_POINT('Ctrl Pts',(-2.10695988400006,12.2,3.57373385599999));
#303629=CARTESIAN_POINT('Ctrl Pts',(-2.10695988400006,5.2,3.57373385599999));
#303630=CARTESIAN_POINT('Ctrl Pts',(-2.10695988400006,2.2,3.57373385599999));
#303631=CARTESIAN_POINT('Ctrl Pts',(-2.10792665500006,12.2,3.57465892499999));
#303632=CARTESIAN_POINT('Ctrl Pts',(-2.10792665500006,5.2,3.57465892499999));
#303633=CARTESIAN_POINT('Ctrl Pts',(-2.10792665500006,2.2,3.57465892499999));
#303634=CARTESIAN_POINT('Ctrl Pts',(-2.10889810200006,12.2,3.57558626199998));
#303635=CARTESIAN_POINT('Ctrl Pts',(-2.10889810200006,5.2,3.57558626199998));
#303636=CARTESIAN_POINT('Ctrl Pts',(-2.10889810200006,2.2,3.57558626199998));
#303637=CARTESIAN_POINT('Ctrl Pts',(-2.10987422800006,12.2,3.57651584899998));
#303638=CARTESIAN_POINT('Ctrl Pts',(-2.10987422800006,5.2,3.57651584899998));
#303639=CARTESIAN_POINT('Ctrl Pts',(-2.10987422800006,2.2,3.57651584899998));
#303640=CARTESIAN_POINT('Ctrl Pts',(-2.11085503200006,12.2,3.57744767599999));
#303641=CARTESIAN_POINT('Ctrl Pts',(-2.11085503200006,5.2,3.57744767599999));
#303642=CARTESIAN_POINT('Ctrl Pts',(-2.11085503200006,2.2,3.57744767599999));
#303643=CARTESIAN_POINT('Ctrl Pts',(-2.11184051600006,12.2,3.57838172399998));
#303644=CARTESIAN_POINT('Ctrl Pts',(-2.11184051600006,5.2,3.57838172399998));
#303645=CARTESIAN_POINT('Ctrl Pts',(-2.11184051600006,2.2,3.57838172399998));
#303646=CARTESIAN_POINT('Ctrl Pts',(-2.11283068000006,12.2,3.57931798199999));
#303647=CARTESIAN_POINT('Ctrl Pts',(-2.11283068000006,5.2,3.57931798199999));
#303648=CARTESIAN_POINT('Ctrl Pts',(-2.11283068000006,2.2,3.57931798199999));
#303649=CARTESIAN_POINT('Ctrl Pts',(-2.11382552700006,12.2,3.58025643499998));
#303650=CARTESIAN_POINT('Ctrl Pts',(-2.11382552700006,5.2,3.58025643499998));
#303651=CARTESIAN_POINT('Ctrl Pts',(-2.11382552700006,2.2,3.58025643499998));
#303652=CARTESIAN_POINT('Ctrl Pts',(-2.11482505400005,12.2,3.58119706899998));
#303653=CARTESIAN_POINT('Ctrl Pts',(-2.11482505400005,5.2,3.58119706899998));
#303654=CARTESIAN_POINT('Ctrl Pts',(-2.11482505400005,2.2,3.58119706899998));
#303655=CARTESIAN_POINT('Ctrl Pts',(-2.11582926500005,12.2,3.58213986899998));
#303656=CARTESIAN_POINT('Ctrl Pts',(-2.11582926500005,5.2,3.58213986899998));
#303657=CARTESIAN_POINT('Ctrl Pts',(-2.11582926500005,2.2,3.58213986899998));
#303658=CARTESIAN_POINT('Ctrl Pts',(-2.11683815900006,12.2,3.58308482299999));
#303659=CARTESIAN_POINT('Ctrl Pts',(-2.11683815900006,5.2,3.58308482299999));
#303660=CARTESIAN_POINT('Ctrl Pts',(-2.11683815900006,2.2,3.58308482299999));
#303661=CARTESIAN_POINT('Ctrl Pts',(-2.11785173800005,12.2,3.58403191499999));
#303662=CARTESIAN_POINT('Ctrl Pts',(-2.11785173800005,5.2,3.58403191499999));
#303663=CARTESIAN_POINT('Ctrl Pts',(-2.11785173800005,2.2,3.58403191499999));
#303664=CARTESIAN_POINT('Ctrl Pts',(-2.11887000200006,12.2,3.58498113199998));
#303665=CARTESIAN_POINT('Ctrl Pts',(-2.11887000200006,5.2,3.58498113199998));
#303666=CARTESIAN_POINT('Ctrl Pts',(-2.11887000200006,2.2,3.58498113199998));
#303667=CARTESIAN_POINT('Ctrl Pts',(-2.11989295200006,12.2,3.58593245999998));
#303668=CARTESIAN_POINT('Ctrl Pts',(-2.11989295200006,5.2,3.58593245999998));
#303669=CARTESIAN_POINT('Ctrl Pts',(-2.11989295200006,2.2,3.58593245999998));
#303670=CARTESIAN_POINT('Ctrl Pts',(-2.12092058700006,12.2,3.58688588399998));
#303671=CARTESIAN_POINT('Ctrl Pts',(-2.12092058700006,5.2,3.58688588399998));
#303672=CARTESIAN_POINT('Ctrl Pts',(-2.12092058700006,2.2,3.58688588399998));
#303673=CARTESIAN_POINT('Ctrl Pts',(-2.12195291000006,12.2,3.58784139099999));
#303674=CARTESIAN_POINT('Ctrl Pts',(-2.12195291000006,5.2,3.58784139099999));
#303675=CARTESIAN_POINT('Ctrl Pts',(-2.12195291000006,2.2,3.58784139099999));
#303676=CARTESIAN_POINT('Ctrl Pts',(-2.12298992100005,12.2,3.58879896799999));
#303677=CARTESIAN_POINT('Ctrl Pts',(-2.12298992100005,5.2,3.58879896799999));
#303678=CARTESIAN_POINT('Ctrl Pts',(-2.12298992100005,2.2,3.58879896799999));
#303679=CARTESIAN_POINT('Ctrl Pts',(-2.12403161800006,12.2,3.58975859899999));
#303680=CARTESIAN_POINT('Ctrl Pts',(-2.12403161800006,5.2,3.58975859899999));
#303681=CARTESIAN_POINT('Ctrl Pts',(-2.12403161800006,2.2,3.58975859899999));
#303682=CARTESIAN_POINT('Ctrl Pts',(-2.12507800500005,12.2,3.59072027199999));
#303683=CARTESIAN_POINT('Ctrl Pts',(-2.12507800500005,5.2,3.59072027199999));
#303684=CARTESIAN_POINT('Ctrl Pts',(-2.12507800500005,2.2,3.59072027199999));
#303685=CARTESIAN_POINT('Ctrl Pts',(-2.12612908200006,12.2,3.59168397199999));
#303686=CARTESIAN_POINT('Ctrl Pts',(-2.12612908200006,5.2,3.59168397199999));
#303687=CARTESIAN_POINT('Ctrl Pts',(-2.12612908200006,2.2,3.59168397199999));
#303688=CARTESIAN_POINT('Ctrl Pts',(-2.12718484700006,12.2,3.59264968499998));
#303689=CARTESIAN_POINT('Ctrl Pts',(-2.12718484700006,5.2,3.59264968499998));
#303690=CARTESIAN_POINT('Ctrl Pts',(-2.12718484700006,2.2,3.59264968499998));
#303691=CARTESIAN_POINT('Ctrl Pts',(-2.12824530300006,12.2,3.59361739899998));
#303692=CARTESIAN_POINT('Ctrl Pts',(-2.12824530300006,5.2,3.59361739899998));
#303693=CARTESIAN_POINT('Ctrl Pts',(-2.12824530300006,2.2,3.59361739899998));
#303694=CARTESIAN_POINT('Ctrl Pts',(-2.12931045000006,12.2,3.59458709999998));
#303695=CARTESIAN_POINT('Ctrl Pts',(-2.12931045000006,5.2,3.59458709999998));
#303696=CARTESIAN_POINT('Ctrl Pts',(-2.12931045000006,2.2,3.59458709999998));
#303697=CARTESIAN_POINT('Ctrl Pts',(-2.13038028900006,12.2,3.59555877199998));
#303698=CARTESIAN_POINT('Ctrl Pts',(-2.13038028900006,5.2,3.59555877199998));
#303699=CARTESIAN_POINT('Ctrl Pts',(-2.13038028900006,2.2,3.59555877199998));
#303700=CARTESIAN_POINT('Ctrl Pts',(-2.13145481800006,12.2,3.59653240399999));
#303701=CARTESIAN_POINT('Ctrl Pts',(-2.13145481800006,5.2,3.59653240399999));
#303702=CARTESIAN_POINT('Ctrl Pts',(-2.13145481800006,2.2,3.59653240399999));
#303703=CARTESIAN_POINT('Ctrl Pts',(-2.13253404000006,12.2,3.59750797899999));
#303704=CARTESIAN_POINT('Ctrl Pts',(-2.13253404000006,5.2,3.59750797899999));
#303705=CARTESIAN_POINT('Ctrl Pts',(-2.13253404000006,2.2,3.59750797899999));
#303706=CARTESIAN_POINT('Ctrl Pts',(-2.13361795400006,12.2,3.59848548799999));
#303707=CARTESIAN_POINT('Ctrl Pts',(-2.13361795400006,5.2,3.59848548799999));
#303708=CARTESIAN_POINT('Ctrl Pts',(-2.13361795400006,2.2,3.59848548799999));
#303709=CARTESIAN_POINT('Ctrl Pts',(-2.13470656200006,12.2,3.59946491399998));
#303710=CARTESIAN_POINT('Ctrl Pts',(-2.13470656200006,5.2,3.59946491399998));
#303711=CARTESIAN_POINT('Ctrl Pts',(-2.13470656200006,2.2,3.59946491399998));
#303712=CARTESIAN_POINT('Ctrl Pts',(-2.13579986300005,12.2,3.60044624499999));
#303713=CARTESIAN_POINT('Ctrl Pts',(-2.13579986300005,5.2,3.60044624499999));
#303714=CARTESIAN_POINT('Ctrl Pts',(-2.13579986300005,2.2,3.60044624499999));
#303715=CARTESIAN_POINT('Ctrl Pts',(-2.13689785700006,12.2,3.60142946699998));
#303716=CARTESIAN_POINT('Ctrl Pts',(-2.13689785700006,5.2,3.60142946699998));
#303717=CARTESIAN_POINT('Ctrl Pts',(-2.13689785700006,2.2,3.60142946699998));
#303718=CARTESIAN_POINT('Ctrl Pts',(-2.13800054500005,12.2,3.60241456599999));
#303719=CARTESIAN_POINT('Ctrl Pts',(-2.13800054500005,5.2,3.60241456599999));
#303720=CARTESIAN_POINT('Ctrl Pts',(-2.13800054500005,2.2,3.60241456599999));
#303721=CARTESIAN_POINT('Ctrl Pts',(-2.13910792800006,12.2,3.60340152899998));
#303722=CARTESIAN_POINT('Ctrl Pts',(-2.13910792800006,5.2,3.60340152899998));
#303723=CARTESIAN_POINT('Ctrl Pts',(-2.13910792800006,2.2,3.60340152899998));
#303724=CARTESIAN_POINT('Ctrl Pts',(-2.14022000500006,12.2,3.60439034299999));
#303725=CARTESIAN_POINT('Ctrl Pts',(-2.14022000500006,5.2,3.60439034299999));
#303726=CARTESIAN_POINT('Ctrl Pts',(-2.14022000500006,2.2,3.60439034299999));
#303727=CARTESIAN_POINT('Ctrl Pts',(-2.14133677700006,12.2,3.60538099399999));
#303728=CARTESIAN_POINT('Ctrl Pts',(-2.14133677700006,5.2,3.60538099399999));
#303729=CARTESIAN_POINT('Ctrl Pts',(-2.14133677700006,2.2,3.60538099399999));
#303730=CARTESIAN_POINT('Ctrl Pts',(-2.14245824500006,12.2,3.60637346799999));
#303731=CARTESIAN_POINT('Ctrl Pts',(-2.14245824500006,5.2,3.60637346799999));
#303732=CARTESIAN_POINT('Ctrl Pts',(-2.14245824500006,2.2,3.60637346799999));
#303733=CARTESIAN_POINT('Ctrl Pts',(-2.14358440700006,12.2,3.60736775199998));
#303734=CARTESIAN_POINT('Ctrl Pts',(-2.14358440700006,5.2,3.60736775199998));
#303735=CARTESIAN_POINT('Ctrl Pts',(-2.14358440700006,2.2,3.60736775199998));
#303736=CARTESIAN_POINT('Ctrl Pts',(-2.14471526600006,12.2,3.60836383499999));
#303737=CARTESIAN_POINT('Ctrl Pts',(-2.14471526600006,5.2,3.60836383499999));
#303738=CARTESIAN_POINT('Ctrl Pts',(-2.14471526600006,2.2,3.60836383499999));
#303739=CARTESIAN_POINT('Ctrl Pts',(-2.14585082000006,12.2,3.60936169999999));
#303740=CARTESIAN_POINT('Ctrl Pts',(-2.14585082000006,5.2,3.60936169999999));
#303741=CARTESIAN_POINT('Ctrl Pts',(-2.14585082000006,2.2,3.60936169999999));
#303742=CARTESIAN_POINT('Ctrl Pts',(-2.14699107100006,12.2,3.61036133599999));
#303743=CARTESIAN_POINT('Ctrl Pts',(-2.14699107100006,5.2,3.61036133599999));
#303744=CARTESIAN_POINT('Ctrl Pts',(-2.14699107100006,2.2,3.61036133599999));
#303745=CARTESIAN_POINT('Ctrl Pts',(-2.14813601800006,12.2,3.61136272899999));
#303746=CARTESIAN_POINT('Ctrl Pts',(-2.14813601800006,5.2,3.61136272899999));
#303747=CARTESIAN_POINT('Ctrl Pts',(-2.14813601800006,2.2,3.61136272899999));
#303748=CARTESIAN_POINT('Ctrl Pts',(-2.14928566100005,12.2,3.61236586599999));
#303749=CARTESIAN_POINT('Ctrl Pts',(-2.14928566100005,5.2,3.61236586599999));
#303750=CARTESIAN_POINT('Ctrl Pts',(-2.14928566100005,2.2,3.61236586599999));
#303751=CARTESIAN_POINT('Ctrl Pts',(-2.15044000000006,12.2,3.61337073399999));
#303752=CARTESIAN_POINT('Ctrl Pts',(-2.15044000000006,5.2,3.61337073399999));
#303753=CARTESIAN_POINT('Ctrl Pts',(-2.15044000000006,2.2,3.61337073399999));
#303754=CARTESIAN_POINT('Ctrl Pts',(-2.15159903600005,12.2,3.61437731899999));
#303755=CARTESIAN_POINT('Ctrl Pts',(-2.15159903600005,5.2,3.61437731899999));
#303756=CARTESIAN_POINT('Ctrl Pts',(-2.15159903600005,2.2,3.61437731899999));
#303757=CARTESIAN_POINT('Ctrl Pts',(-2.15276276900005,12.2,3.61538560899999));
#303758=CARTESIAN_POINT('Ctrl Pts',(-2.15276276900005,5.2,3.61538560899999));
#303759=CARTESIAN_POINT('Ctrl Pts',(-2.15276276900005,2.2,3.61538560899999));
#303760=CARTESIAN_POINT('Ctrl Pts',(-2.15393119800006,12.2,3.61639558899999));
#303761=CARTESIAN_POINT('Ctrl Pts',(-2.15393119800006,5.2,3.61639558899999));
#303762=CARTESIAN_POINT('Ctrl Pts',(-2.15393119800006,2.2,3.61639558899999));
#303763=CARTESIAN_POINT('Ctrl Pts',(-2.15510432500006,12.2,3.61740724799999));
#303764=CARTESIAN_POINT('Ctrl Pts',(-2.15510432500006,5.2,3.61740724799999));
#303765=CARTESIAN_POINT('Ctrl Pts',(-2.15510432500006,2.2,3.61740724799999));
#303766=CARTESIAN_POINT('Ctrl Pts',(-2.15628214900006,12.2,3.61842057199999));
#303767=CARTESIAN_POINT('Ctrl Pts',(-2.15628214900006,5.2,3.61842057199999));
#303768=CARTESIAN_POINT('Ctrl Pts',(-2.15628214900006,2.2,3.61842057199999));
#303769=CARTESIAN_POINT('Ctrl Pts',(-2.15746466900006,12.2,3.61943554799999));
#303770=CARTESIAN_POINT('Ctrl Pts',(-2.15746466900006,5.2,3.61943554799999));
#303771=CARTESIAN_POINT('Ctrl Pts',(-2.15746466900006,2.2,3.61943554799999));
#303772=CARTESIAN_POINT('Ctrl Pts',(-2.15865188700006,12.2,3.62045216299999));
#303773=CARTESIAN_POINT('Ctrl Pts',(-2.15865188700006,5.2,3.62045216299999));
#303774=CARTESIAN_POINT('Ctrl Pts',(-2.15865188700006,2.2,3.62045216299999));
#303775=CARTESIAN_POINT('Ctrl Pts',(-2.15984380100006,12.2,3.62147040399999));
#303776=CARTESIAN_POINT('Ctrl Pts',(-2.15984380100006,5.2,3.62147040399999));
#303777=CARTESIAN_POINT('Ctrl Pts',(-2.15984380100006,2.2,3.62147040399999));
#303778=CARTESIAN_POINT('Ctrl Pts',(-2.16104041300006,12.2,3.62249025699998));
#303779=CARTESIAN_POINT('Ctrl Pts',(-2.16104041300006,5.2,3.62249025699998));
#303780=CARTESIAN_POINT('Ctrl Pts',(-2.16104041300006,2.2,3.62249025699998));
#303781=CARTESIAN_POINT('Ctrl Pts',(-2.16224172200006,12.2,3.62351171199998));
#303782=CARTESIAN_POINT('Ctrl Pts',(-2.16224172200006,5.2,3.62351171199998));
#303783=CARTESIAN_POINT('Ctrl Pts',(-2.16224172200006,2.2,3.62351171199998));
#303784=CARTESIAN_POINT('Ctrl Pts',(-2.16344772600006,12.2,3.62453475299999));
#303785=CARTESIAN_POINT('Ctrl Pts',(-2.16344772600006,5.2,3.62453475299999));
#303786=CARTESIAN_POINT('Ctrl Pts',(-2.16344772600006,2.2,3.62453475299999));
#303787=CARTESIAN_POINT('Ctrl Pts',(-2.16465842900006,12.2,3.62555936799998));
#303788=CARTESIAN_POINT('Ctrl Pts',(-2.16465842900006,5.2,3.62555936799998));
#303789=CARTESIAN_POINT('Ctrl Pts',(-2.16465842900006,2.2,3.62555936799998));
#303790=CARTESIAN_POINT('Ctrl Pts',(-2.16587382700005,12.2,3.62658554399999));
#303791=CARTESIAN_POINT('Ctrl Pts',(-2.16587382700005,5.2,3.62658554399999));
#303792=CARTESIAN_POINT('Ctrl Pts',(-2.16587382700005,2.2,3.62658554399999));
#303793=CARTESIAN_POINT('Ctrl Pts',(-2.16709392200006,12.2,3.62761326999999));
#303794=CARTESIAN_POINT('Ctrl Pts',(-2.16709392200006,5.2,3.62761326999999));
#303795=CARTESIAN_POINT('Ctrl Pts',(-2.16709392200006,2.2,3.62761326999999));
#303796=CARTESIAN_POINT('Ctrl Pts',(-2.16831871400006,12.2,3.62864252999999));
#303797=CARTESIAN_POINT('Ctrl Pts',(-2.16831871400006,5.2,3.62864252999999));
#303798=CARTESIAN_POINT('Ctrl Pts',(-2.16831871400006,2.2,3.62864252999999));
#303799=CARTESIAN_POINT('Ctrl Pts',(-2.16954820200006,12.2,3.62967331299998));
#303800=CARTESIAN_POINT('Ctrl Pts',(-2.16954820200006,5.2,3.62967331299998));
#303801=CARTESIAN_POINT('Ctrl Pts',(-2.16954820200006,2.2,3.62967331299998));
#303802=CARTESIAN_POINT('Ctrl Pts',(-2.17078238700006,12.2,3.63070560699998));
#303803=CARTESIAN_POINT('Ctrl Pts',(-2.17078238700006,5.2,3.63070560699998));
#303804=CARTESIAN_POINT('Ctrl Pts',(-2.17078238700006,2.2,3.63070560699998));
#303805=CARTESIAN_POINT('Ctrl Pts',(-2.17202126700006,12.2,3.63173939899998));
#303806=CARTESIAN_POINT('Ctrl Pts',(-2.17202126700006,5.2,3.63173939899998));
#303807=CARTESIAN_POINT('Ctrl Pts',(-2.17202126700006,2.2,3.63173939899998));
#303808=CARTESIAN_POINT('Ctrl Pts',(-2.17326484300005,12.2,3.63277467399998));
#303809=CARTESIAN_POINT('Ctrl Pts',(-2.17326484300005,5.2,3.63277467399998));
#303810=CARTESIAN_POINT('Ctrl Pts',(-2.17326484300005,2.2,3.63277467399998));
#303811=CARTESIAN_POINT('Ctrl Pts',(-2.17451311500006,12.2,3.63381142099998));
#303812=CARTESIAN_POINT('Ctrl Pts',(-2.17451311500006,5.2,3.63381142099998));
#303813=CARTESIAN_POINT('Ctrl Pts',(-2.17451311500006,2.2,3.63381142099998));
#303814=CARTESIAN_POINT('Ctrl Pts',(-2.17576608200006,12.2,3.63484962799999));
#303815=CARTESIAN_POINT('Ctrl Pts',(-2.17576608200006,5.2,3.63484962799999));
#303816=CARTESIAN_POINT('Ctrl Pts',(-2.17576608200006,2.2,3.63484962799999));
#303817=CARTESIAN_POINT('Ctrl Pts',(-2.17702374500006,12.2,3.63588928099999));
#303818=CARTESIAN_POINT('Ctrl Pts',(-2.17702374500006,5.2,3.63588928099999));
#303819=CARTESIAN_POINT('Ctrl Pts',(-2.17702374500006,2.2,3.63588928099999));
#303820=CARTESIAN_POINT('Ctrl Pts',(-2.17828610200006,12.2,3.63693036799998));
#303821=CARTESIAN_POINT('Ctrl Pts',(-2.17828610200006,5.2,3.63693036799998));
#303822=CARTESIAN_POINT('Ctrl Pts',(-2.17828610200006,2.2,3.63693036799998));
#303823=CARTESIAN_POINT('Ctrl Pts',(-2.17955315300005,12.2,3.63797287599999));
#303824=CARTESIAN_POINT('Ctrl Pts',(-2.17955315300005,5.2,3.63797287599999));
#303825=CARTESIAN_POINT('Ctrl Pts',(-2.17955315300005,2.2,3.63797287599999));
#303826=CARTESIAN_POINT('Ctrl Pts',(-2.18082490000006,12.2,3.63901679299998));
#303827=CARTESIAN_POINT('Ctrl Pts',(-2.18082490000006,5.2,3.63901679299998));
#303828=CARTESIAN_POINT('Ctrl Pts',(-2.18082490000006,2.2,3.63901679299998));
#303829=CARTESIAN_POINT('Ctrl Pts',(-2.18210134000006,12.2,3.64006210699999));
#303830=CARTESIAN_POINT('Ctrl Pts',(-2.18210134000006,5.2,3.64006210699999));
#303831=CARTESIAN_POINT('Ctrl Pts',(-2.18210134000006,2.2,3.64006210699999));
#303832=CARTESIAN_POINT('Ctrl Pts',(-2.18338247300006,12.2,3.64110880499998));
#303833=CARTESIAN_POINT('Ctrl Pts',(-2.18338247300006,5.2,3.64110880499998));
#303834=CARTESIAN_POINT('Ctrl Pts',(-2.18338247300006,2.2,3.64110880499998));
#303835=CARTESIAN_POINT('Ctrl Pts',(-2.18466830000006,12.2,3.64215687199999));
#303836=CARTESIAN_POINT('Ctrl Pts',(-2.18466830000006,5.2,3.64215687199999));
#303837=CARTESIAN_POINT('Ctrl Pts',(-2.18466830000006,2.2,3.64215687199999));
#303838=CARTESIAN_POINT('Ctrl Pts',(-2.18595882000006,12.2,3.64320629899999));
#303839=CARTESIAN_POINT('Ctrl Pts',(-2.18595882000006,5.2,3.64320629899999));
#303840=CARTESIAN_POINT('Ctrl Pts',(-2.18595882000006,2.2,3.64320629899999));
#303841=CARTESIAN_POINT('Ctrl Pts',(-2.18725403300006,12.2,3.64425707199998));
#303842=CARTESIAN_POINT('Ctrl Pts',(-2.18725403300006,5.2,3.64425707199998));
#303843=CARTESIAN_POINT('Ctrl Pts',(-2.18725403300006,2.2,3.64425707199998));
#303844=CARTESIAN_POINT('Ctrl Pts',(-2.18855393700006,12.2,3.64530917899998));
#303845=CARTESIAN_POINT('Ctrl Pts',(-2.18855393700006,5.2,3.64530917899998));
#303846=CARTESIAN_POINT('Ctrl Pts',(-2.18855393700006,2.2,3.64530917899998));
#303847=CARTESIAN_POINT('Ctrl Pts',(-2.18985853500006,12.2,3.64636260699999));
#303848=CARTESIAN_POINT('Ctrl Pts',(-2.18985853500006,5.2,3.64636260699999));
#303849=CARTESIAN_POINT('Ctrl Pts',(-2.18985853500006,2.2,3.64636260699999));
#303850=CARTESIAN_POINT('Ctrl Pts',(-2.19116782200006,12.2,3.64741734399999));
#303851=CARTESIAN_POINT('Ctrl Pts',(-2.19116782200006,5.2,3.64741734399999));
#303852=CARTESIAN_POINT('Ctrl Pts',(-2.19116782200006,2.2,3.64741734399999));
#303853=CARTESIAN_POINT('Ctrl Pts',(-2.19248180100006,12.2,3.64847337799999));
#303854=CARTESIAN_POINT('Ctrl Pts',(-2.19248180100006,5.2,3.64847337799999));
#303855=CARTESIAN_POINT('Ctrl Pts',(-2.19248180100006,2.2,3.64847337799999));
#303856=CARTESIAN_POINT('Ctrl Pts',(-2.19380047100006,12.2,3.64953069599999));
#303857=CARTESIAN_POINT('Ctrl Pts',(-2.19380047100006,5.2,3.64953069599999));
#303858=CARTESIAN_POINT('Ctrl Pts',(-2.19380047100006,2.2,3.64953069599999));
#303859=CARTESIAN_POINT('Ctrl Pts',(-2.19512383000006,12.2,3.65058928599999));
#303860=CARTESIAN_POINT('Ctrl Pts',(-2.19512383000006,5.2,3.65058928599999));
#303861=CARTESIAN_POINT('Ctrl Pts',(-2.19512383000006,2.2,3.65058928599999));
#303862=CARTESIAN_POINT('Ctrl Pts',(-2.19645187900006,12.2,3.65164913499999));
#303863=CARTESIAN_POINT('Ctrl Pts',(-2.19645187900006,5.2,3.65164913499999));
#303864=CARTESIAN_POINT('Ctrl Pts',(-2.19645187900006,2.2,3.65164913499999));
#303865=CARTESIAN_POINT('Ctrl Pts',(-2.19778461700006,12.2,3.65271023199998));
#303866=CARTESIAN_POINT('Ctrl Pts',(-2.19778461700006,5.2,3.65271023199998));
#303867=CARTESIAN_POINT('Ctrl Pts',(-2.19778461700006,2.2,3.65271023199998));
#303868=CARTESIAN_POINT('Ctrl Pts',(-2.19912204400006,12.2,3.65377256399999));
#303869=CARTESIAN_POINT('Ctrl Pts',(-2.19912204400006,5.2,3.65377256399999));
#303870=CARTESIAN_POINT('Ctrl Pts',(-2.19912204400006,2.2,3.65377256399999));
#303871=CARTESIAN_POINT('Ctrl Pts',(-2.20046415900006,12.2,3.65483611899998));
#303872=CARTESIAN_POINT('Ctrl Pts',(-2.20046415900006,5.2,3.65483611899998));
#303873=CARTESIAN_POINT('Ctrl Pts',(-2.20046415900006,2.2,3.65483611899998));
#303874=CARTESIAN_POINT('Ctrl Pts',(-2.20181096100006,12.2,3.65590088399999));
#303875=CARTESIAN_POINT('Ctrl Pts',(-2.20181096100006,5.2,3.65590088399999));
#303876=CARTESIAN_POINT('Ctrl Pts',(-2.20181096100006,2.2,3.65590088399999));
#303877=CARTESIAN_POINT('Ctrl Pts',(-2.20316245000005,12.2,3.65696684799998));
#303878=CARTESIAN_POINT('Ctrl Pts',(-2.20316245000005,5.2,3.65696684799998));
#303879=CARTESIAN_POINT('Ctrl Pts',(-2.20316245000005,2.2,3.65696684799998));
#303880=CARTESIAN_POINT('Ctrl Pts',(-2.20451862500005,12.2,3.65803399899999));
#303881=CARTESIAN_POINT('Ctrl Pts',(-2.20451862500005,5.2,3.65803399899999));
#303882=CARTESIAN_POINT('Ctrl Pts',(-2.20451862500005,2.2,3.65803399899999));
#303883=CARTESIAN_POINT('Ctrl Pts',(-2.20587948700006,12.2,3.65910232399998));
#303884=CARTESIAN_POINT('Ctrl Pts',(-2.20587948700006,5.2,3.65910232399998));
#303885=CARTESIAN_POINT('Ctrl Pts',(-2.20587948700006,2.2,3.65910232399998));
#303886=CARTESIAN_POINT('Ctrl Pts',(-2.20724503300006,12.2,3.66017180999999));
#303887=CARTESIAN_POINT('Ctrl Pts',(-2.20724503300006,5.2,3.66017180999999));
#303888=CARTESIAN_POINT('Ctrl Pts',(-2.20724503300006,2.2,3.66017180999999));
#303889=CARTESIAN_POINT('Ctrl Pts',(-2.20861526400005,12.2,3.66124244699999));
#303890=CARTESIAN_POINT('Ctrl Pts',(-2.20861526400005,5.2,3.66124244699999));
#303891=CARTESIAN_POINT('Ctrl Pts',(-2.20861526400005,2.2,3.66124244699999));
#303892=CARTESIAN_POINT('Ctrl Pts',(-2.20999017900006,12.2,3.66231422099998));
#303893=CARTESIAN_POINT('Ctrl Pts',(-2.20999017900006,5.2,3.66231422099998));
#303894=CARTESIAN_POINT('Ctrl Pts',(-2.20999017900006,2.2,3.66231422099998));
#303895=CARTESIAN_POINT('Ctrl Pts',(-2.21136977600006,12.2,3.66338712199998));
#303896=CARTESIAN_POINT('Ctrl Pts',(-2.21136977600006,5.2,3.66338712199998));
#303897=CARTESIAN_POINT('Ctrl Pts',(-2.21136977600006,2.2,3.66338712199998));
#303898=CARTESIAN_POINT('Ctrl Pts',(-2.21275405700006,12.2,3.66446113599999));
#303899=CARTESIAN_POINT('Ctrl Pts',(-2.21275405700006,5.2,3.66446113599999));
#303900=CARTESIAN_POINT('Ctrl Pts',(-2.21275405700006,2.2,3.66446113599999));
#303901=CARTESIAN_POINT('Ctrl Pts',(-2.21414301900006,12.2,3.66553625199998));
#303902=CARTESIAN_POINT('Ctrl Pts',(-2.21414301900006,5.2,3.66553625199998));
#303903=CARTESIAN_POINT('Ctrl Pts',(-2.21414301900006,2.2,3.66553625199998));
#303904=CARTESIAN_POINT('Ctrl Pts',(-2.21553666200006,12.2,3.66661245899999));
#303905=CARTESIAN_POINT('Ctrl Pts',(-2.21553666200006,5.2,3.66661245899999));
#303906=CARTESIAN_POINT('Ctrl Pts',(-2.21553666200006,2.2,3.66661245899999));
#303907=CARTESIAN_POINT('Ctrl Pts',(-2.21693498600006,12.2,3.66768974299998));
#303908=CARTESIAN_POINT('Ctrl Pts',(-2.21693498600006,5.2,3.66768974299998));
#303909=CARTESIAN_POINT('Ctrl Pts',(-2.21693498600006,2.2,3.66768974299998));
#303910=CARTESIAN_POINT('Ctrl Pts',(-2.21833799000006,12.2,3.66876809299999));
#303911=CARTESIAN_POINT('Ctrl Pts',(-2.21833799000006,5.2,3.66876809299999));
#303912=CARTESIAN_POINT('Ctrl Pts',(-2.21833799000006,2.2,3.66876809299999));
#303913=CARTESIAN_POINT('Ctrl Pts',(-2.21974567200005,12.2,3.66984749699999));
#303914=CARTESIAN_POINT('Ctrl Pts',(-2.21974567200005,5.2,3.66984749699999));
#303915=CARTESIAN_POINT('Ctrl Pts',(-2.21974567200005,2.2,3.66984749699999));
#303916=CARTESIAN_POINT('Ctrl Pts',(-2.22115803300006,12.2,3.67092794299998));
#303917=CARTESIAN_POINT('Ctrl Pts',(-2.22115803300006,5.2,3.67092794299998));
#303918=CARTESIAN_POINT('Ctrl Pts',(-2.22115803300006,2.2,3.67092794299998));
#303919=CARTESIAN_POINT('Ctrl Pts',(-2.22257507100006,12.2,3.67200941999998));
#303920=CARTESIAN_POINT('Ctrl Pts',(-2.22257507100006,5.2,3.67200941999998));
#303921=CARTESIAN_POINT('Ctrl Pts',(-2.22257507100006,2.2,3.67200941999998));
#303922=CARTESIAN_POINT('Ctrl Pts',(-2.22399678600006,12.2,3.67309191499999));
#303923=CARTESIAN_POINT('Ctrl Pts',(-2.22399678600006,5.2,3.67309191499999));
#303924=CARTESIAN_POINT('Ctrl Pts',(-2.22399678600006,2.2,3.67309191499999));
#303925=CARTESIAN_POINT('Ctrl Pts',(-2.22542317600006,12.2,3.67417541699999));
#303926=CARTESIAN_POINT('Ctrl Pts',(-2.22542317600006,5.2,3.67417541699999));
#303927=CARTESIAN_POINT('Ctrl Pts',(-2.22542317600006,2.2,3.67417541699999));
#303928=CARTESIAN_POINT('Ctrl Pts',(-2.22685424200006,12.2,3.67525991399998));
#303929=CARTESIAN_POINT('Ctrl Pts',(-2.22685424200006,5.2,3.67525991399998));
#303930=CARTESIAN_POINT('Ctrl Pts',(-2.22685424200006,2.2,3.67525991399998));
#303931=CARTESIAN_POINT('Ctrl Pts',(-2.22828998300006,12.2,3.67634539399998));
#303932=CARTESIAN_POINT('Ctrl Pts',(-2.22828998300006,5.2,3.67634539399998));
#303933=CARTESIAN_POINT('Ctrl Pts',(-2.22828998300006,2.2,3.67634539399998));
#303934=CARTESIAN_POINT('Ctrl Pts',(-2.22973039500005,12.2,3.67743184499999));
#303935=CARTESIAN_POINT('Ctrl Pts',(-2.22973039500005,5.2,3.67743184499999));
#303936=CARTESIAN_POINT('Ctrl Pts',(-2.22973039500005,2.2,3.67743184499999));
#303937=CARTESIAN_POINT('Ctrl Pts',(-2.23117548100006,12.2,3.67851925599999));
#303938=CARTESIAN_POINT('Ctrl Pts',(-2.23117548100006,5.2,3.67851925599999));
#303939=CARTESIAN_POINT('Ctrl Pts',(-2.23117548100006,2.2,3.67851925599999));
#303940=CARTESIAN_POINT('Ctrl Pts',(-2.23262523900006,12.2,3.67960761499998));
#303941=CARTESIAN_POINT('Ctrl Pts',(-2.23262523900006,5.2,3.67960761499998));
#303942=CARTESIAN_POINT('Ctrl Pts',(-2.23262523900006,2.2,3.67960761499998));
#303943=CARTESIAN_POINT('Ctrl Pts',(-2.23407966600006,12.2,3.68069690999998));
#303944=CARTESIAN_POINT('Ctrl Pts',(-2.23407966600006,5.2,3.68069690999998));
#303945=CARTESIAN_POINT('Ctrl Pts',(-2.23407966600006,2.2,3.68069690999998));
#303946=CARTESIAN_POINT('Ctrl Pts',(-2.23553876500006,12.2,3.68178712899999));
#303947=CARTESIAN_POINT('Ctrl Pts',(-2.23553876500006,5.2,3.68178712899999));
#303948=CARTESIAN_POINT('Ctrl Pts',(-2.23553876500006,2.2,3.68178712899999));
#303949=CARTESIAN_POINT('Ctrl Pts',(-2.23700253100006,12.2,3.68287826199998));
#303950=CARTESIAN_POINT('Ctrl Pts',(-2.23700253100006,5.2,3.68287826199998));
#303951=CARTESIAN_POINT('Ctrl Pts',(-2.23700253100006,2.2,3.68287826199998));
#303952=CARTESIAN_POINT('Ctrl Pts',(-2.23847096600006,12.2,3.68397029499998));
#303953=CARTESIAN_POINT('Ctrl Pts',(-2.23847096600006,5.2,3.68397029499998));
#303954=CARTESIAN_POINT('Ctrl Pts',(-2.23847096600006,2.2,3.68397029499998));
#303955=CARTESIAN_POINT('Ctrl Pts',(-2.23994406800006,12.2,3.68506321899999));
#303956=CARTESIAN_POINT('Ctrl Pts',(-2.23994406800006,5.2,3.68506321899999));
#303957=CARTESIAN_POINT('Ctrl Pts',(-2.23994406800006,2.2,3.68506321899999));
#303958=CARTESIAN_POINT('Ctrl Pts',(-2.24142183500006,12.2,3.68615701999998));
#303959=CARTESIAN_POINT('Ctrl Pts',(-2.24142183500006,5.2,3.68615701999998));
#303960=CARTESIAN_POINT('Ctrl Pts',(-2.24142183500006,2.2,3.68615701999998));
#303961=CARTESIAN_POINT('Ctrl Pts',(-2.24290426800006,12.2,3.68725168899999));
#303962=CARTESIAN_POINT('Ctrl Pts',(-2.24290426800006,5.2,3.68725168899999));
#303963=CARTESIAN_POINT('Ctrl Pts',(-2.24290426800006,2.2,3.68725168899999));
#303964=CARTESIAN_POINT('Ctrl Pts',(-2.24439136500005,12.2,3.68834721199998));
#303965=CARTESIAN_POINT('Ctrl Pts',(-2.24439136500005,5.2,3.68834721199998));
#303966=CARTESIAN_POINT('Ctrl Pts',(-2.24439136500005,2.2,3.68834721199998));
#303967=CARTESIAN_POINT('Ctrl Pts',(-2.24588312600006,12.2,3.68944357799998));
#303968=CARTESIAN_POINT('Ctrl Pts',(-2.24588312600006,5.2,3.68944357799998));
#303969=CARTESIAN_POINT('Ctrl Pts',(-2.24588312600006,2.2,3.68944357799998));
#303970=CARTESIAN_POINT('Ctrl Pts',(-2.24737954800006,12.2,3.69054077599999));
#303971=CARTESIAN_POINT('Ctrl Pts',(-2.24737954800006,5.2,3.69054077599999));
#303972=CARTESIAN_POINT('Ctrl Pts',(-2.24737954800006,2.2,3.69054077599999));
#303973=CARTESIAN_POINT('Ctrl Pts',(-2.24888063100006,12.2,3.69163879499999));
#303974=CARTESIAN_POINT('Ctrl Pts',(-2.24888063100006,5.2,3.69163879499999));
#303975=CARTESIAN_POINT('Ctrl Pts',(-2.24888063100006,2.2,3.69163879499999));
#303976=CARTESIAN_POINT('Ctrl Pts',(-2.25038637400006,12.2,3.69273762399998));
#303977=CARTESIAN_POINT('Ctrl Pts',(-2.25038637400006,5.2,3.69273762399998));
#303978=CARTESIAN_POINT('Ctrl Pts',(-2.25038637400006,2.2,3.69273762399998));
#303979=CARTESIAN_POINT('Ctrl Pts',(-2.25189677600006,12.2,3.69383724899999));
#303980=CARTESIAN_POINT('Ctrl Pts',(-2.25189677600006,5.2,3.69383724899999));
#303981=CARTESIAN_POINT('Ctrl Pts',(-2.25189677600006,2.2,3.69383724899999));
#303982=CARTESIAN_POINT('Ctrl Pts',(-2.25341183700006,12.2,3.69493766099998));
#303983=CARTESIAN_POINT('Ctrl Pts',(-2.25341183700006,5.2,3.69493766099998));
#303984=CARTESIAN_POINT('Ctrl Pts',(-2.25341183700006,2.2,3.69493766099998));
#303985=CARTESIAN_POINT('Ctrl Pts',(-2.25493155300006,12.2,3.69603884699998));
#303986=CARTESIAN_POINT('Ctrl Pts',(-2.25493155300006,5.2,3.69603884699998));
#303987=CARTESIAN_POINT('Ctrl Pts',(-2.25493155300006,2.2,3.69603884699998));
#303988=CARTESIAN_POINT('Ctrl Pts',(-2.25645592500006,12.2,3.69714079599999));
#303989=CARTESIAN_POINT('Ctrl Pts',(-2.25645592500006,5.2,3.69714079599999));
#303990=CARTESIAN_POINT('Ctrl Pts',(-2.25645592500006,2.2,3.69714079599999));
#303991=CARTESIAN_POINT('Ctrl Pts',(-2.25798495200006,12.2,3.69824349899999));
#303992=CARTESIAN_POINT('Ctrl Pts',(-2.25798495200006,5.2,3.69824349899999));
#303993=CARTESIAN_POINT('Ctrl Pts',(-2.25798495200006,2.2,3.69824349899999));
#303994=CARTESIAN_POINT('Ctrl Pts',(-2.25951863300006,12.2,3.69934694199999));
#303995=CARTESIAN_POINT('Ctrl Pts',(-2.25951863300006,5.2,3.69934694199999));
#303996=CARTESIAN_POINT('Ctrl Pts',(-2.25951863300006,2.2,3.69934694199999));
#303997=CARTESIAN_POINT('Ctrl Pts',(-2.26105696600006,12.2,3.70045111299999));
#303998=CARTESIAN_POINT('Ctrl Pts',(-2.26105696600006,5.2,3.70045111299999));
#303999=CARTESIAN_POINT('Ctrl Pts',(-2.26105696600006,2.2,3.70045111299999));
#304000=CARTESIAN_POINT('Ctrl Pts',(-2.26259995000006,12.2,3.70155600399999));
#304001=CARTESIAN_POINT('Ctrl Pts',(-2.26259995000006,5.2,3.70155600399999));
#304002=CARTESIAN_POINT('Ctrl Pts',(-2.26259995000006,2.2,3.70155600399999));
#304003=CARTESIAN_POINT('Ctrl Pts',(-2.26414758400006,12.2,3.70266159999999));
#304004=CARTESIAN_POINT('Ctrl Pts',(-2.26414758400006,5.2,3.70266159999999));
#304005=CARTESIAN_POINT('Ctrl Pts',(-2.26414758400006,2.2,3.70266159999999));
#304006=CARTESIAN_POINT('Ctrl Pts',(-2.26569986700006,12.2,3.70376789299999));
#304007=CARTESIAN_POINT('Ctrl Pts',(-2.26569986700006,5.2,3.70376789299999));
#304008=CARTESIAN_POINT('Ctrl Pts',(-2.26569986700006,2.2,3.70376789299999));
#304009=CARTESIAN_POINT('Ctrl Pts',(-2.26725679800006,12.2,3.70487486999998));
#304010=CARTESIAN_POINT('Ctrl Pts',(-2.26725679800006,5.2,3.70487486999998));
#304011=CARTESIAN_POINT('Ctrl Pts',(-2.26725679800006,2.2,3.70487486999998));
#304012=CARTESIAN_POINT('Ctrl Pts',(-2.26881837400006,12.2,3.70598251999999));
#304013=CARTESIAN_POINT('Ctrl Pts',(-2.26881837400006,5.2,3.70598251999999));
#304014=CARTESIAN_POINT('Ctrl Pts',(-2.26881837400006,2.2,3.70598251999999));
#304015=CARTESIAN_POINT('Ctrl Pts',(-2.27038459700006,12.2,3.70709083299998));
#304016=CARTESIAN_POINT('Ctrl Pts',(-2.27038459700006,5.2,3.70709083299998));
#304017=CARTESIAN_POINT('Ctrl Pts',(-2.27038459700006,2.2,3.70709083299998));
#304018=CARTESIAN_POINT('Ctrl Pts',(-2.27195546200006,12.2,3.70819979599998));
#304019=CARTESIAN_POINT('Ctrl Pts',(-2.27195546200006,5.2,3.70819979599998));
#304020=CARTESIAN_POINT('Ctrl Pts',(-2.27195546200006,2.2,3.70819979599998));
#304021=CARTESIAN_POINT('Ctrl Pts',(-2.27353097200006,12.2,3.70930939799998));
#304022=CARTESIAN_POINT('Ctrl Pts',(-2.27353097200006,5.2,3.70930939799998));
#304023=CARTESIAN_POINT('Ctrl Pts',(-2.27353097200006,2.2,3.70930939799998));
#304024=CARTESIAN_POINT('Ctrl Pts',(-2.27511112200005,12.2,3.71041962899999));
#304025=CARTESIAN_POINT('Ctrl Pts',(-2.27511112200005,5.2,3.71041962899999));
#304026=CARTESIAN_POINT('Ctrl Pts',(-2.27511112200005,2.2,3.71041962899999));
#304027=CARTESIAN_POINT('Ctrl Pts',(-2.27669591200006,12.2,3.71153047699998));
#304028=CARTESIAN_POINT('Ctrl Pts',(-2.27669591200006,5.2,3.71153047699998));
#304029=CARTESIAN_POINT('Ctrl Pts',(-2.27669591200006,2.2,3.71153047699998));
#304030=CARTESIAN_POINT('Ctrl Pts',(-2.27828534100006,12.2,3.71264193299999));
#304031=CARTESIAN_POINT('Ctrl Pts',(-2.27828534100006,5.2,3.71264193299999));
#304032=CARTESIAN_POINT('Ctrl Pts',(-2.27828534100006,2.2,3.71264193299999));
#304033=CARTESIAN_POINT('Ctrl Pts',(-2.27987940700006,12.2,3.71375398199999));
#304034=CARTESIAN_POINT('Ctrl Pts',(-2.27987940700006,5.2,3.71375398199999));
#304035=CARTESIAN_POINT('Ctrl Pts',(-2.27987940700006,2.2,3.71375398199999));
#304036=CARTESIAN_POINT('Ctrl Pts',(-2.28147811000006,12.2,3.71486661699999));
#304037=CARTESIAN_POINT('Ctrl Pts',(-2.28147811000006,5.2,3.71486661699999));
#304038=CARTESIAN_POINT('Ctrl Pts',(-2.28147811000006,2.2,3.71486661699999));
#304039=CARTESIAN_POINT('Ctrl Pts',(-2.28308144900006,12.2,3.71597982399998));
#304040=CARTESIAN_POINT('Ctrl Pts',(-2.28308144900006,5.2,3.71597982399998));
#304041=CARTESIAN_POINT('Ctrl Pts',(-2.28308144900006,2.2,3.71597982399998));
#304042=CARTESIAN_POINT('Ctrl Pts',(-2.28468942000006,12.2,3.71709359399999));
#304043=CARTESIAN_POINT('Ctrl Pts',(-2.28468942000006,5.2,3.71709359399999));
#304044=CARTESIAN_POINT('Ctrl Pts',(-2.28468942000006,2.2,3.71709359399999));
#304045=CARTESIAN_POINT('Ctrl Pts',(-2.28630202400006,12.2,3.71820791499999));
#304046=CARTESIAN_POINT('Ctrl Pts',(-2.28630202400006,5.2,3.71820791499999));
#304047=CARTESIAN_POINT('Ctrl Pts',(-2.28630202400006,2.2,3.71820791499999));
#304048=CARTESIAN_POINT('Ctrl Pts',(-2.28791925900006,12.2,3.71932277699998));
#304049=CARTESIAN_POINT('Ctrl Pts',(-2.28791925900006,5.2,3.71932277699998));
#304050=CARTESIAN_POINT('Ctrl Pts',(-2.28791925900006,2.2,3.71932277699998));
#304051=CARTESIAN_POINT('Ctrl Pts',(-2.28954112300006,12.2,3.72043816699998));
#304052=CARTESIAN_POINT('Ctrl Pts',(-2.28954112300006,5.2,3.72043816699998));
#304053=CARTESIAN_POINT('Ctrl Pts',(-2.28954112300006,2.2,3.72043816699998));
#304054=CARTESIAN_POINT('Ctrl Pts',(-2.29116761500006,12.2,3.72155407499999));
#304055=CARTESIAN_POINT('Ctrl Pts',(-2.29116761500006,5.2,3.72155407499999));
#304056=CARTESIAN_POINT('Ctrl Pts',(-2.29116761500006,2.2,3.72155407499999));
#304057=CARTESIAN_POINT('Ctrl Pts',(-2.29279873500006,12.2,3.72267049199999));
#304058=CARTESIAN_POINT('Ctrl Pts',(-2.29279873500006,5.2,3.72267049199999));
#304059=CARTESIAN_POINT('Ctrl Pts',(-2.29279873500006,2.2,3.72267049199999));
#304060=CARTESIAN_POINT('Ctrl Pts',(-2.29443447900006,12.2,3.72378740399999));
#304061=CARTESIAN_POINT('Ctrl Pts',(-2.29443447900006,5.2,3.72378740399999));
#304062=CARTESIAN_POINT('Ctrl Pts',(-2.29443447900006,2.2,3.72378740399999));
#304063=CARTESIAN_POINT('Ctrl Pts',(-2.29607484800006,12.2,3.72490480199998));
#304064=CARTESIAN_POINT('Ctrl Pts',(-2.29607484800006,5.2,3.72490480199998));
#304065=CARTESIAN_POINT('Ctrl Pts',(-2.29607484800006,2.2,3.72490480199998));
#304066=CARTESIAN_POINT('Ctrl Pts',(-2.29771983800005,12.2,3.72602267599999));
#304067=CARTESIAN_POINT('Ctrl Pts',(-2.29771983800005,5.2,3.72602267599999));
#304068=CARTESIAN_POINT('Ctrl Pts',(-2.29771983800005,2.2,3.72602267599999));
#304069=CARTESIAN_POINT('Ctrl Pts',(-2.29936945000006,12.2,3.72714101299999));
#304070=CARTESIAN_POINT('Ctrl Pts',(-2.29936945000006,5.2,3.72714101299999));
#304071=CARTESIAN_POINT('Ctrl Pts',(-2.29936945000006,2.2,3.72714101299999));
#304072=CARTESIAN_POINT('Ctrl Pts',(-2.30102368200006,12.2,3.72825980299999));
#304073=CARTESIAN_POINT('Ctrl Pts',(-2.30102368200006,5.2,3.72825980299999));
#304074=CARTESIAN_POINT('Ctrl Pts',(-2.30102368200006,2.2,3.72825980299999));
#304075=CARTESIAN_POINT('Ctrl Pts',(-2.30268253100005,12.2,3.72937903599999));
#304076=CARTESIAN_POINT('Ctrl Pts',(-2.30268253100005,5.2,3.72937903599999));
#304077=CARTESIAN_POINT('Ctrl Pts',(-2.30268253100005,2.2,3.72937903599999));
#304078=CARTESIAN_POINT('Ctrl Pts',(-2.30434599700006,12.2,3.73049869999999));
#304079=CARTESIAN_POINT('Ctrl Pts',(-2.30434599700006,5.2,3.73049869999999));
#304080=CARTESIAN_POINT('Ctrl Pts',(-2.30434599700006,2.2,3.73049869999999));
#304081=CARTESIAN_POINT('Ctrl Pts',(-2.30601407800005,12.2,3.73161878499998));
#304082=CARTESIAN_POINT('Ctrl Pts',(-2.30601407800005,5.2,3.73161878499998));
#304083=CARTESIAN_POINT('Ctrl Pts',(-2.30601407800005,2.2,3.73161878499998));
#304084=CARTESIAN_POINT('Ctrl Pts',(-2.30768677300006,12.2,3.73273928099999));
#304085=CARTESIAN_POINT('Ctrl Pts',(-2.30768677300006,5.2,3.73273928099999));
#304086=CARTESIAN_POINT('Ctrl Pts',(-2.30768677300006,2.2,3.73273928099999));
#304087=CARTESIAN_POINT('Ctrl Pts',(-2.30936408000006,12.2,3.73386017499998));
#304088=CARTESIAN_POINT('Ctrl Pts',(-2.30936408000006,5.2,3.73386017499998));
#304089=CARTESIAN_POINT('Ctrl Pts',(-2.30936408000006,2.2,3.73386017499998));
#304090=CARTESIAN_POINT('Ctrl Pts',(-2.31104599700005,12.2,3.73498145799999));
#304091=CARTESIAN_POINT('Ctrl Pts',(-2.31104599700005,5.2,3.73498145799999));
#304092=CARTESIAN_POINT('Ctrl Pts',(-2.31104599700005,2.2,3.73498145799999));
#304093=CARTESIAN_POINT('Ctrl Pts',(-2.31273252300006,12.2,3.73610311999999));
#304094=CARTESIAN_POINT('Ctrl Pts',(-2.31273252300006,5.2,3.73610311999999));
#304095=CARTESIAN_POINT('Ctrl Pts',(-2.31273252300006,2.2,3.73610311999999));
#304096=CARTESIAN_POINT('Ctrl Pts',(-2.31442365600006,12.2,3.73722514799999));
#304097=CARTESIAN_POINT('Ctrl Pts',(-2.31442365600006,5.2,3.73722514799999));
#304098=CARTESIAN_POINT('Ctrl Pts',(-2.31442365600006,2.2,3.73722514799999));
#304099=CARTESIAN_POINT('Ctrl Pts',(-2.31611939500006,12.2,3.73834753399999));
#304100=CARTESIAN_POINT('Ctrl Pts',(-2.31611939500006,5.2,3.73834753399999));
#304101=CARTESIAN_POINT('Ctrl Pts',(-2.31611939500006,2.2,3.73834753399999));
#304102=CARTESIAN_POINT('Ctrl Pts',(-2.31781973900006,12.2,3.73947026499999));
#304103=CARTESIAN_POINT('Ctrl Pts',(-2.31781973900006,5.2,3.73947026499999));
#304104=CARTESIAN_POINT('Ctrl Pts',(-2.31781973900006,2.2,3.73947026499999));
#304105=CARTESIAN_POINT('Ctrl Pts',(-2.31952468500006,12.2,3.74059333199998));
#304106=CARTESIAN_POINT('Ctrl Pts',(-2.31952468500006,5.2,3.74059333199998));
#304107=CARTESIAN_POINT('Ctrl Pts',(-2.31952468500006,2.2,3.74059333199998));
#304108=CARTESIAN_POINT('Ctrl Pts',(-2.32123423200005,12.2,3.74171672399999));
#304109=CARTESIAN_POINT('Ctrl Pts',(-2.32123423200005,5.2,3.74171672399999));
#304110=CARTESIAN_POINT('Ctrl Pts',(-2.32123423200005,2.2,3.74171672399999));
#304111=CARTESIAN_POINT('Ctrl Pts',(-2.32294837900006,12.2,3.74284042999999));
#304112=CARTESIAN_POINT('Ctrl Pts',(-2.32294837900006,5.2,3.74284042999999));
#304113=CARTESIAN_POINT('Ctrl Pts',(-2.32294837900006,2.2,3.74284042999999));
#304114=CARTESIAN_POINT('Ctrl Pts',(-2.32466712300006,12.2,3.74396443999998));
#304115=CARTESIAN_POINT('Ctrl Pts',(-2.32466712300006,5.2,3.74396443999998));
#304116=CARTESIAN_POINT('Ctrl Pts',(-2.32466712300006,2.2,3.74396443999998));
#304117=CARTESIAN_POINT('Ctrl Pts',(-2.32639046300006,12.2,3.74508874299998));
#304118=CARTESIAN_POINT('Ctrl Pts',(-2.32639046300006,5.2,3.74508874299998));
#304119=CARTESIAN_POINT('Ctrl Pts',(-2.32639046300006,2.2,3.74508874299998));
#304120=CARTESIAN_POINT('Ctrl Pts',(-2.32811839800006,12.2,3.74621332899999));
#304121=CARTESIAN_POINT('Ctrl Pts',(-2.32811839800006,5.2,3.74621332899999));
#304122=CARTESIAN_POINT('Ctrl Pts',(-2.32811839800006,2.2,3.74621332899999));
#304123=CARTESIAN_POINT('Ctrl Pts',(-2.32985092500006,12.2,3.74733818699998));
#304124=CARTESIAN_POINT('Ctrl Pts',(-2.32985092500006,5.2,3.74733818699998));
#304125=CARTESIAN_POINT('Ctrl Pts',(-2.32985092500006,2.2,3.74733818699998));
#304126=CARTESIAN_POINT('Ctrl Pts',(-2.33158804400006,12.2,3.74846330799999));
#304127=CARTESIAN_POINT('Ctrl Pts',(-2.33158804400006,5.2,3.74846330799999));
#304128=CARTESIAN_POINT('Ctrl Pts',(-2.33158804400006,2.2,3.74846330799999));
#304129=CARTESIAN_POINT('Ctrl Pts',(-2.33332975200006,12.2,3.74958867799998));
#304130=CARTESIAN_POINT('Ctrl Pts',(-2.33332975200006,5.2,3.74958867799998));
#304131=CARTESIAN_POINT('Ctrl Pts',(-2.33332975200006,2.2,3.74958867799998));
#304132=CARTESIAN_POINT('Ctrl Pts',(-2.33507604800006,12.2,3.75071429099999));
#304133=CARTESIAN_POINT('Ctrl Pts',(-2.33507604800006,5.2,3.75071429099999));
#304134=CARTESIAN_POINT('Ctrl Pts',(-2.33507604800006,2.2,3.75071429099999));
#304135=CARTESIAN_POINT('Ctrl Pts',(-2.33682693000006,12.2,3.75184013399998));
#304136=CARTESIAN_POINT('Ctrl Pts',(-2.33682693000006,5.2,3.75184013399998));
#304137=CARTESIAN_POINT('Ctrl Pts',(-2.33682693000006,2.2,3.75184013399998));
#304138=CARTESIAN_POINT('Ctrl Pts',(-2.33858239600006,12.2,3.75296619599998));
#304139=CARTESIAN_POINT('Ctrl Pts',(-2.33858239600006,5.2,3.75296619599998));
#304140=CARTESIAN_POINT('Ctrl Pts',(-2.33858239600006,2.2,3.75296619599998));
#304141=CARTESIAN_POINT('Ctrl Pts',(-2.34034244400006,12.2,3.75409246799999));
#304142=CARTESIAN_POINT('Ctrl Pts',(-2.34034244400006,5.2,3.75409246799999));
#304143=CARTESIAN_POINT('Ctrl Pts',(-2.34034244400006,2.2,3.75409246799999));
#304144=CARTESIAN_POINT('Ctrl Pts',(-2.34210707400006,12.2,3.75521893999998));
#304145=CARTESIAN_POINT('Ctrl Pts',(-2.34210707400006,5.2,3.75521893999998));
#304146=CARTESIAN_POINT('Ctrl Pts',(-2.34210707400006,2.2,3.75521893999998));
#304147=CARTESIAN_POINT('Ctrl Pts',(-2.34387628200006,12.2,3.75634560099999));
#304148=CARTESIAN_POINT('Ctrl Pts',(-2.34387628200006,5.2,3.75634560099999));
#304149=CARTESIAN_POINT('Ctrl Pts',(-2.34387628200006,2.2,3.75634560099999));
#304150=CARTESIAN_POINT('Ctrl Pts',(-2.34565006800006,12.2,3.75747243999999));
#304151=CARTESIAN_POINT('Ctrl Pts',(-2.34565006800006,5.2,3.75747243999999));
#304152=CARTESIAN_POINT('Ctrl Pts',(-2.34565006800006,2.2,3.75747243999999));
#304153=CARTESIAN_POINT('Ctrl Pts',(-2.34742842800005,12.2,3.75859944799998));
#304154=CARTESIAN_POINT('Ctrl Pts',(-2.34742842800005,5.2,3.75859944799998));
#304155=CARTESIAN_POINT('Ctrl Pts',(-2.34742842800005,2.2,3.75859944799998));
#304156=CARTESIAN_POINT('Ctrl Pts',(-2.34921136300006,12.2,3.75972661399998));
#304157=CARTESIAN_POINT('Ctrl Pts',(-2.34921136300006,5.2,3.75972661399998));
#304158=CARTESIAN_POINT('Ctrl Pts',(-2.34921136300006,2.2,3.75972661399998));
#304159=CARTESIAN_POINT('Ctrl Pts',(-2.35099887000006,12.2,3.76085392699999));
#304160=CARTESIAN_POINT('Ctrl Pts',(-2.35099887000006,5.2,3.76085392699999));
#304161=CARTESIAN_POINT('Ctrl Pts',(-2.35099887000006,2.2,3.76085392699999));
#304162=CARTESIAN_POINT('Ctrl Pts',(-2.35279094600005,12.2,3.76198137799998));
#304163=CARTESIAN_POINT('Ctrl Pts',(-2.35279094600005,5.2,3.76198137799998));
#304164=CARTESIAN_POINT('Ctrl Pts',(-2.35279094600005,2.2,3.76198137799998));
#304165=CARTESIAN_POINT('Ctrl Pts',(-2.35458759100006,12.2,3.76310895699999));
#304166=CARTESIAN_POINT('Ctrl Pts',(-2.35458759100006,5.2,3.76310895699999));
#304167=CARTESIAN_POINT('Ctrl Pts',(-2.35458759100006,2.2,3.76310895699999));
#304168=CARTESIAN_POINT('Ctrl Pts',(-2.35638880100006,12.2,3.76423665199999));
#304169=CARTESIAN_POINT('Ctrl Pts',(-2.35638880100006,5.2,3.76423665199999));
#304170=CARTESIAN_POINT('Ctrl Pts',(-2.35638880100006,2.2,3.76423665199999));
#304171=CARTESIAN_POINT('Ctrl Pts',(-2.35819457700006,12.2,3.76536445399999));
#304172=CARTESIAN_POINT('Ctrl Pts',(-2.35819457700006,5.2,3.76536445399999));
#304173=CARTESIAN_POINT('Ctrl Pts',(-2.35819457700006,2.2,3.76536445399999));
#304174=CARTESIAN_POINT('Ctrl Pts',(-2.36000491500006,12.2,3.76649235399999));
#304175=CARTESIAN_POINT('Ctrl Pts',(-2.36000491500006,5.2,3.76649235399999));
#304176=CARTESIAN_POINT('Ctrl Pts',(-2.36000491500006,2.2,3.76649235399999));
#304177=CARTESIAN_POINT('Ctrl Pts',(-2.36181981300006,12.2,3.76762033899999));
#304178=CARTESIAN_POINT('Ctrl Pts',(-2.36181981300006,5.2,3.76762033899999));
#304179=CARTESIAN_POINT('Ctrl Pts',(-2.36181981300006,2.2,3.76762033899999));
#304180=CARTESIAN_POINT('Ctrl Pts',(-2.36363927100005,12.2,3.76874840099998));
#304181=CARTESIAN_POINT('Ctrl Pts',(-2.36363927100005,5.2,3.76874840099998));
#304182=CARTESIAN_POINT('Ctrl Pts',(-2.36363927100005,2.2,3.76874840099998));
#304183=CARTESIAN_POINT('Ctrl Pts',(-2.36546328500005,12.2,3.76987652899999));
#304184=CARTESIAN_POINT('Ctrl Pts',(-2.36546328500005,5.2,3.76987652899999));
#304185=CARTESIAN_POINT('Ctrl Pts',(-2.36546328500005,2.2,3.76987652899999));
#304186=CARTESIAN_POINT('Ctrl Pts',(-2.36729185500006,12.2,3.77100471299999));
#304187=CARTESIAN_POINT('Ctrl Pts',(-2.36729185500006,5.2,3.77100471299999));
#304188=CARTESIAN_POINT('Ctrl Pts',(-2.36729185500006,2.2,3.77100471299999));
#304189=CARTESIAN_POINT('Ctrl Pts',(-2.36912497900006,12.2,3.77213294399999));
#304190=CARTESIAN_POINT('Ctrl Pts',(-2.36912497900006,5.2,3.77213294399999));
#304191=CARTESIAN_POINT('Ctrl Pts',(-2.36912497900006,2.2,3.77213294399999));
#304192=CARTESIAN_POINT('Ctrl Pts',(-2.37096265200006,12.2,3.77326120999999));
#304193=CARTESIAN_POINT('Ctrl Pts',(-2.37096265200006,5.2,3.77326120999999));
#304194=CARTESIAN_POINT('Ctrl Pts',(-2.37096265200006,2.2,3.77326120999999));
#304195=CARTESIAN_POINT('Ctrl Pts',(-2.37280487500006,12.2,3.77438950199998));
#304196=CARTESIAN_POINT('Ctrl Pts',(-2.37280487500006,5.2,3.77438950199998));
#304197=CARTESIAN_POINT('Ctrl Pts',(-2.37280487500006,2.2,3.77438950199998));
#304198=CARTESIAN_POINT('Ctrl Pts',(-2.37465164600006,12.2,3.77551780999998));
#304199=CARTESIAN_POINT('Ctrl Pts',(-2.37465164600006,5.2,3.77551780999998));
#304200=CARTESIAN_POINT('Ctrl Pts',(-2.37465164600006,2.2,3.77551780999998));
#304201=CARTESIAN_POINT('Ctrl Pts',(-2.37650296200006,12.2,3.77664612399998));
#304202=CARTESIAN_POINT('Ctrl Pts',(-2.37650296200006,5.2,3.77664612399998));
#304203=CARTESIAN_POINT('Ctrl Pts',(-2.37650296200006,2.2,3.77664612399998));
#304204=CARTESIAN_POINT('Ctrl Pts',(-2.37835882100006,12.2,3.77777443399999));
#304205=CARTESIAN_POINT('Ctrl Pts',(-2.37835882100006,5.2,3.77777443399999));
#304206=CARTESIAN_POINT('Ctrl Pts',(-2.37835882100006,2.2,3.77777443399999));
#304207=CARTESIAN_POINT('Ctrl Pts',(-2.38021922100006,12.2,3.77890272899998));
#304208=CARTESIAN_POINT('Ctrl Pts',(-2.38021922100006,5.2,3.77890272899998));
#304209=CARTESIAN_POINT('Ctrl Pts',(-2.38021922100006,2.2,3.77890272899998));
#304210=CARTESIAN_POINT('Ctrl Pts',(-2.38208416100006,12.2,3.78003099999999));
#304211=CARTESIAN_POINT('Ctrl Pts',(-2.38208416100006,5.2,3.78003099999999));
#304212=CARTESIAN_POINT('Ctrl Pts',(-2.38208416100006,2.2,3.78003099999999));
#304213=CARTESIAN_POINT('Ctrl Pts',(-2.38395363900006,12.2,3.78115923799999));
#304214=CARTESIAN_POINT('Ctrl Pts',(-2.38395363900006,5.2,3.78115923799999));
#304215=CARTESIAN_POINT('Ctrl Pts',(-2.38395363900006,2.2,3.78115923799999));
#304216=CARTESIAN_POINT('Ctrl Pts',(-2.38582765100006,12.2,3.78228743199998));
#304217=CARTESIAN_POINT('Ctrl Pts',(-2.38582765100006,5.2,3.78228743199998));
#304218=CARTESIAN_POINT('Ctrl Pts',(-2.38582765100006,2.2,3.78228743199998));
#304219=CARTESIAN_POINT('Ctrl Pts',(-2.38770619700006,12.2,3.78341556999998));
#304220=CARTESIAN_POINT('Ctrl Pts',(-2.38770619700006,5.2,3.78341556999998));
#304221=CARTESIAN_POINT('Ctrl Pts',(-2.38770619700006,2.2,3.78341556999998));
#304222=CARTESIAN_POINT('Ctrl Pts',(-2.38958927400006,12.2,3.78454364599998));
#304223=CARTESIAN_POINT('Ctrl Pts',(-2.38958927400006,5.2,3.78454364599998));
#304224=CARTESIAN_POINT('Ctrl Pts',(-2.38958927400006,2.2,3.78454364599998));
#304225=CARTESIAN_POINT('Ctrl Pts',(-2.39147688100006,12.2,3.78567164799998));
#304226=CARTESIAN_POINT('Ctrl Pts',(-2.39147688100006,5.2,3.78567164799998));
#304227=CARTESIAN_POINT('Ctrl Pts',(-2.39147688100006,2.2,3.78567164799998));
#304228=CARTESIAN_POINT('Ctrl Pts',(-2.39336901400006,12.2,3.78679956599999));
#304229=CARTESIAN_POINT('Ctrl Pts',(-2.39336901400006,5.2,3.78679956599999));
#304230=CARTESIAN_POINT('Ctrl Pts',(-2.39336901400006,2.2,3.78679956599999));
#304231=CARTESIAN_POINT('Ctrl Pts',(-2.39526567400006,12.2,3.78792739099998));
#304232=CARTESIAN_POINT('Ctrl Pts',(-2.39526567400006,5.2,3.78792739099998));
#304233=CARTESIAN_POINT('Ctrl Pts',(-2.39526567400006,2.2,3.78792739099998));
#304234=CARTESIAN_POINT('Ctrl Pts',(-2.39716685500006,12.2,3.78905511199999));
#304235=CARTESIAN_POINT('Ctrl Pts',(-2.39716685500006,5.2,3.78905511199999));
#304236=CARTESIAN_POINT('Ctrl Pts',(-2.39716685500006,2.2,3.78905511199999));
#304237=CARTESIAN_POINT('Ctrl Pts',(-2.39907255800006,12.2,3.79018271999998));
#304238=CARTESIAN_POINT('Ctrl Pts',(-2.39907255800006,5.2,3.79018271999998));
#304239=CARTESIAN_POINT('Ctrl Pts',(-2.39907255800006,2.2,3.79018271999998));
#304240=CARTESIAN_POINT('Ctrl Pts',(-2.40098277900006,12.2,3.79131020599999));
#304241=CARTESIAN_POINT('Ctrl Pts',(-2.40098277900006,5.2,3.79131020599999));
#304242=CARTESIAN_POINT('Ctrl Pts',(-2.40098277900006,2.2,3.79131020599999));
#304243=CARTESIAN_POINT('Ctrl Pts',(-2.40289751700006,12.2,3.79243755799998));
#304244=CARTESIAN_POINT('Ctrl Pts',(-2.40289751700006,5.2,3.79243755799998));
#304245=CARTESIAN_POINT('Ctrl Pts',(-2.40289751700006,2.2,3.79243755799998));
#304246=CARTESIAN_POINT('Ctrl Pts',(-2.40481677100005,12.2,3.79356476899999));
#304247=CARTESIAN_POINT('Ctrl Pts',(-2.40481677100005,5.2,3.79356476899999));
#304248=CARTESIAN_POINT('Ctrl Pts',(-2.40481677100005,2.2,3.79356476899999));
#304249=CARTESIAN_POINT('Ctrl Pts',(-2.40674053600006,12.2,3.79469182699999));
#304250=CARTESIAN_POINT('Ctrl Pts',(-2.40674053600006,5.2,3.79469182699999));
#304251=CARTESIAN_POINT('Ctrl Pts',(-2.40674053600006,2.2,3.79469182699999));
#304252=CARTESIAN_POINT('Ctrl Pts',(-2.40866881100006,12.2,3.79581872299998));
#304253=CARTESIAN_POINT('Ctrl Pts',(-2.40866881100006,5.2,3.79581872299998));
#304254=CARTESIAN_POINT('Ctrl Pts',(-2.40866881100006,2.2,3.79581872299998));
#304255=CARTESIAN_POINT('Ctrl Pts',(-2.41060159600006,12.2,3.79694544699999));
#304256=CARTESIAN_POINT('Ctrl Pts',(-2.41060159600006,5.2,3.79694544699999));
#304257=CARTESIAN_POINT('Ctrl Pts',(-2.41060159600006,2.2,3.79694544699999));
#304258=CARTESIAN_POINT('Ctrl Pts',(-2.41253888500006,12.2,3.79807198999998));
#304259=CARTESIAN_POINT('Ctrl Pts',(-2.41253888500006,5.2,3.79807198999998));
#304260=CARTESIAN_POINT('Ctrl Pts',(-2.41253888500006,2.2,3.79807198999998));
#304261=CARTESIAN_POINT('Ctrl Pts',(-2.41448067900006,12.2,3.79919834299999));
#304262=CARTESIAN_POINT('Ctrl Pts',(-2.41448067900006,5.2,3.79919834299999));
#304263=CARTESIAN_POINT('Ctrl Pts',(-2.41448067900006,2.2,3.79919834299999));
#304264=CARTESIAN_POINT('Ctrl Pts',(-2.41642697400006,12.2,3.80032449399998));
#304265=CARTESIAN_POINT('Ctrl Pts',(-2.41642697400006,5.2,3.80032449399998));
#304266=CARTESIAN_POINT('Ctrl Pts',(-2.41642697400006,2.2,3.80032449399998));
#304267=CARTESIAN_POINT('Ctrl Pts',(-2.41837776900006,12.2,3.80145043399998));
#304268=CARTESIAN_POINT('Ctrl Pts',(-2.41837776900006,5.2,3.80145043399998));
#304269=CARTESIAN_POINT('Ctrl Pts',(-2.41837776900006,2.2,3.80145043399998));
#304270=CARTESIAN_POINT('Ctrl Pts',(-2.42033306000006,12.2,3.80257615499998));
#304271=CARTESIAN_POINT('Ctrl Pts',(-2.42033306000006,5.2,3.80257615499998));
#304272=CARTESIAN_POINT('Ctrl Pts',(-2.42033306000006,2.2,3.80257615499998));
#304273=CARTESIAN_POINT('Ctrl Pts',(-2.42229284800006,12.2,3.80370164699999));
#304274=CARTESIAN_POINT('Ctrl Pts',(-2.42229284800006,5.2,3.80370164699999));
#304275=CARTESIAN_POINT('Ctrl Pts',(-2.42229284800006,2.2,3.80370164699999));
#304276=CARTESIAN_POINT('Ctrl Pts',(-2.42425712700005,12.2,3.80482689899999));
#304277=CARTESIAN_POINT('Ctrl Pts',(-2.42425712700005,5.2,3.80482689899999));
#304278=CARTESIAN_POINT('Ctrl Pts',(-2.42425712700005,2.2,3.80482689899999));
#304279=CARTESIAN_POINT('Ctrl Pts',(-2.42622589800006,12.2,3.80595190299999));
#304280=CARTESIAN_POINT('Ctrl Pts',(-2.42622589800006,5.2,3.80595190299999));
#304281=CARTESIAN_POINT('Ctrl Pts',(-2.42622589800006,2.2,3.80595190299999));
#304282=CARTESIAN_POINT('Ctrl Pts',(-2.42819915600006,12.2,3.80707664799999));
#304283=CARTESIAN_POINT('Ctrl Pts',(-2.42819915600006,5.2,3.80707664799999));
#304284=CARTESIAN_POINT('Ctrl Pts',(-2.42819915600006,2.2,3.80707664799999));
#304285=CARTESIAN_POINT('Ctrl Pts',(-2.43017690100006,12.2,3.80820112499999));
#304286=CARTESIAN_POINT('Ctrl Pts',(-2.43017690100006,5.2,3.80820112499999));
#304287=CARTESIAN_POINT('Ctrl Pts',(-2.43017690100006,2.2,3.80820112499999));
#304288=CARTESIAN_POINT('Ctrl Pts',(-2.43215912900005,12.2,3.80932532399999));
#304289=CARTESIAN_POINT('Ctrl Pts',(-2.43215912900005,5.2,3.80932532399999));
#304290=CARTESIAN_POINT('Ctrl Pts',(-2.43215912900005,2.2,3.80932532399999));
#304291=CARTESIAN_POINT('Ctrl Pts',(-2.43414584000006,12.2,3.81044923799998));
#304292=CARTESIAN_POINT('Ctrl Pts',(-2.43414584000006,5.2,3.81044923799998));
#304293=CARTESIAN_POINT('Ctrl Pts',(-2.43414584000006,2.2,3.81044923799998));
#304294=CARTESIAN_POINT('Ctrl Pts',(-2.43613703000006,12.2,3.81157285399999));
#304295=CARTESIAN_POINT('Ctrl Pts',(-2.43613703000006,5.2,3.81157285399999));
#304296=CARTESIAN_POINT('Ctrl Pts',(-2.43613703000006,2.2,3.81157285399999));
#304297=CARTESIAN_POINT('Ctrl Pts',(-2.43813269600006,12.2,3.81269616399998));
#304298=CARTESIAN_POINT('Ctrl Pts',(-2.43813269600006,5.2,3.81269616399998));
#304299=CARTESIAN_POINT('Ctrl Pts',(-2.43813269600006,2.2,3.81269616399998));
#304300=CARTESIAN_POINT('Ctrl Pts',(-2.44013283600006,12.2,3.81381915999999));
#304301=CARTESIAN_POINT('Ctrl Pts',(-2.44013283600006,5.2,3.81381915999999));
#304302=CARTESIAN_POINT('Ctrl Pts',(-2.44013283600006,2.2,3.81381915999999));
#304303=CARTESIAN_POINT('Ctrl Pts',(-2.44213745000006,12.2,3.81494182999998));
#304304=CARTESIAN_POINT('Ctrl Pts',(-2.44213745000006,5.2,3.81494182999998));
#304305=CARTESIAN_POINT('Ctrl Pts',(-2.44213745000006,2.2,3.81494182999998));
#304306=CARTESIAN_POINT('Ctrl Pts',(-2.44414653200006,12.2,3.81606416499999));
#304307=CARTESIAN_POINT('Ctrl Pts',(-2.44414653200006,5.2,3.81606416499999));
#304308=CARTESIAN_POINT('Ctrl Pts',(-2.44414653200006,2.2,3.81606416499999));
#304309=CARTESIAN_POINT('Ctrl Pts',(-2.44616008300006,12.2,3.81718615699998));
#304310=CARTESIAN_POINT('Ctrl Pts',(-2.44616008300006,5.2,3.81718615699998));
#304311=CARTESIAN_POINT('Ctrl Pts',(-2.44616008300006,2.2,3.81718615699998));
#304312=CARTESIAN_POINT('Ctrl Pts',(-2.44817810000006,12.2,3.81830779599999));
#304313=CARTESIAN_POINT('Ctrl Pts',(-2.44817810000006,5.2,3.81830779599999));
#304314=CARTESIAN_POINT('Ctrl Pts',(-2.44817810000006,2.2,3.81830779599999));
#304315=CARTESIAN_POINT('Ctrl Pts',(-2.45020057900006,12.2,3.81942907299998));
#304316=CARTESIAN_POINT('Ctrl Pts',(-2.45020057900006,5.2,3.81942907299998));
#304317=CARTESIAN_POINT('Ctrl Pts',(-2.45020057900006,2.2,3.81942907299998));
#304318=CARTESIAN_POINT('Ctrl Pts',(-2.45222751900006,12.2,3.82054997699999));
#304319=CARTESIAN_POINT('Ctrl Pts',(-2.45222751900006,5.2,3.82054997699999));
#304320=CARTESIAN_POINT('Ctrl Pts',(-2.45222751900006,2.2,3.82054997699999));
#304321=CARTESIAN_POINT('Ctrl Pts',(-2.45425891600005,12.2,3.82167049999998));
#304322=CARTESIAN_POINT('Ctrl Pts',(-2.45425891600005,5.2,3.82167049999998));
#304323=CARTESIAN_POINT('Ctrl Pts',(-2.45425891600005,2.2,3.82167049999998));
#304324=CARTESIAN_POINT('Ctrl Pts',(-2.45629477100006,12.2,3.82279063299999));
#304325=CARTESIAN_POINT('Ctrl Pts',(-2.45629477100006,5.2,3.82279063299999));
#304326=CARTESIAN_POINT('Ctrl Pts',(-2.45629477100006,2.2,3.82279063299999));
#304327=CARTESIAN_POINT('Ctrl Pts',(-2.45833507800006,12.2,3.82391036599999));
#304328=CARTESIAN_POINT('Ctrl Pts',(-2.45833507800006,5.2,3.82391036599999));
#304329=CARTESIAN_POINT('Ctrl Pts',(-2.45833507800006,2.2,3.82391036599999));
#304330=CARTESIAN_POINT('Ctrl Pts',(-2.46037983700006,12.2,3.82502968999999));
#304331=CARTESIAN_POINT('Ctrl Pts',(-2.46037983700006,5.2,3.82502968999999));
#304332=CARTESIAN_POINT('Ctrl Pts',(-2.46037983700006,2.2,3.82502968999999));
#304333=CARTESIAN_POINT('Ctrl Pts',(-2.46242904400006,12.2,3.82614859499999));
#304334=CARTESIAN_POINT('Ctrl Pts',(-2.46242904400006,5.2,3.82614859499999));
#304335=CARTESIAN_POINT('Ctrl Pts',(-2.46242904400006,2.2,3.82614859499999));
#304336=CARTESIAN_POINT('Ctrl Pts',(-2.46448269700006,12.2,3.82726707199998));
#304337=CARTESIAN_POINT('Ctrl Pts',(-2.46448269700006,5.2,3.82726707199998));
#304338=CARTESIAN_POINT('Ctrl Pts',(-2.46448269700006,2.2,3.82726707199998));
#304339=CARTESIAN_POINT('Ctrl Pts',(-2.46654079500006,12.2,3.82838511199999));
#304340=CARTESIAN_POINT('Ctrl Pts',(-2.46654079500006,5.2,3.82838511199999));
#304341=CARTESIAN_POINT('Ctrl Pts',(-2.46654079500006,2.2,3.82838511199999));
#304342=CARTESIAN_POINT('Ctrl Pts',(-2.46860333300006,12.2,3.82950270699999));
#304343=CARTESIAN_POINT('Ctrl Pts',(-2.46860333300006,5.2,3.82950270699999));
#304344=CARTESIAN_POINT('Ctrl Pts',(-2.46860333300006,2.2,3.82950270699999));
#304345=CARTESIAN_POINT('Ctrl Pts',(-2.47067031100006,12.2,3.83061984499999));
#304346=CARTESIAN_POINT('Ctrl Pts',(-2.47067031100006,5.2,3.83061984499999));
#304347=CARTESIAN_POINT('Ctrl Pts',(-2.47067031100006,2.2,3.83061984499999));
#304348=CARTESIAN_POINT('Ctrl Pts',(-2.47274172400005,12.2,3.83173651899998));
#304349=CARTESIAN_POINT('Ctrl Pts',(-2.47274172400005,5.2,3.83173651899998));
#304350=CARTESIAN_POINT('Ctrl Pts',(-2.47274172400005,2.2,3.83173651899998));
#304351=CARTESIAN_POINT('Ctrl Pts',(-2.47481757200006,12.2,3.83285271899998));
#304352=CARTESIAN_POINT('Ctrl Pts',(-2.47481757200006,5.2,3.83285271899998));
#304353=CARTESIAN_POINT('Ctrl Pts',(-2.47481757200006,2.2,3.83285271899998));
#304354=CARTESIAN_POINT('Ctrl Pts',(-2.47689785200006,12.2,3.83396843499998));
#304355=CARTESIAN_POINT('Ctrl Pts',(-2.47689785200006,5.2,3.83396843499998));
#304356=CARTESIAN_POINT('Ctrl Pts',(-2.47689785200006,2.2,3.83396843499998));
#304357=CARTESIAN_POINT('Ctrl Pts',(-2.47898256100005,12.2,3.83508365999998));
#304358=CARTESIAN_POINT('Ctrl Pts',(-2.47898256100005,5.2,3.83508365999998));
#304359=CARTESIAN_POINT('Ctrl Pts',(-2.47898256100005,2.2,3.83508365999998));
#304360=CARTESIAN_POINT('Ctrl Pts',(-2.48107169600006,12.2,3.83619838299998));
#304361=CARTESIAN_POINT('Ctrl Pts',(-2.48107169600006,5.2,3.83619838299998));
#304362=CARTESIAN_POINT('Ctrl Pts',(-2.48107169600006,2.2,3.83619838299998));
#304363=CARTESIAN_POINT('Ctrl Pts',(-2.48316525500006,12.2,3.83731259599998));
#304364=CARTESIAN_POINT('Ctrl Pts',(-2.48316525500006,5.2,3.83731259599998));
#304365=CARTESIAN_POINT('Ctrl Pts',(-2.48316525500006,2.2,3.83731259599998));
#304366=CARTESIAN_POINT('Ctrl Pts',(-2.48526323500006,12.2,3.83842628899998));
#304367=CARTESIAN_POINT('Ctrl Pts',(-2.48526323500006,5.2,3.83842628899998));
#304368=CARTESIAN_POINT('Ctrl Pts',(-2.48526323500006,2.2,3.83842628899998));
#304369=CARTESIAN_POINT('Ctrl Pts',(-2.48736563500006,12.2,3.83953945299999));
#304370=CARTESIAN_POINT('Ctrl Pts',(-2.48736563500006,5.2,3.83953945299999));
#304371=CARTESIAN_POINT('Ctrl Pts',(-2.48736563500006,2.2,3.83953945299999));
#304372=CARTESIAN_POINT('Ctrl Pts',(-2.48947245100006,12.2,3.84065207999999));
#304373=CARTESIAN_POINT('Ctrl Pts',(-2.48947245100006,5.2,3.84065207999999));
#304374=CARTESIAN_POINT('Ctrl Pts',(-2.48947245100006,2.2,3.84065207999999));
#304375=CARTESIAN_POINT('Ctrl Pts',(-2.49158368100006,12.2,3.84176415999999));
#304376=CARTESIAN_POINT('Ctrl Pts',(-2.49158368100006,5.2,3.84176415999999));
#304377=CARTESIAN_POINT('Ctrl Pts',(-2.49158368100006,2.2,3.84176415999999));
#304378=CARTESIAN_POINT('Ctrl Pts',(-2.49369932300006,12.2,3.84287568299998));
#304379=CARTESIAN_POINT('Ctrl Pts',(-2.49369932300006,5.2,3.84287568299998));
#304380=CARTESIAN_POINT('Ctrl Pts',(-2.49369932300006,2.2,3.84287568299998));
#304381=CARTESIAN_POINT('Ctrl Pts',(-2.49581937300006,12.2,3.84398664099999));
#304382=CARTESIAN_POINT('Ctrl Pts',(-2.49581937300006,5.2,3.84398664099999));
#304383=CARTESIAN_POINT('Ctrl Pts',(-2.49581937300006,2.2,3.84398664099999));
#304384=CARTESIAN_POINT('Ctrl Pts',(-2.49794383000005,12.2,3.84509702499999));
#304385=CARTESIAN_POINT('Ctrl Pts',(-2.49794383000005,5.2,3.84509702499999));
#304386=CARTESIAN_POINT('Ctrl Pts',(-2.49794383000005,2.2,3.84509702499999));
#304387=CARTESIAN_POINT('Ctrl Pts',(-2.50007269000006,12.2,3.84620682699998));
#304388=CARTESIAN_POINT('Ctrl Pts',(-2.50007269000006,5.2,3.84620682699998));
#304389=CARTESIAN_POINT('Ctrl Pts',(-2.50007269000006,2.2,3.84620682699998));
#304390=CARTESIAN_POINT('Ctrl Pts',(-2.50220595100005,12.2,3.84731603599998));
#304391=CARTESIAN_POINT('Ctrl Pts',(-2.50220595100005,5.2,3.84731603599998));
#304392=CARTESIAN_POINT('Ctrl Pts',(-2.50220595100005,2.2,3.84731603599998));
#304393=CARTESIAN_POINT('Ctrl Pts',(-2.50434361100006,12.2,3.84842464399998));
#304394=CARTESIAN_POINT('Ctrl Pts',(-2.50434361100006,5.2,3.84842464399998));
#304395=CARTESIAN_POINT('Ctrl Pts',(-2.50434361100006,2.2,3.84842464399998));
#304396=CARTESIAN_POINT('Ctrl Pts',(-2.50648566700006,12.2,3.84953264199999));
#304397=CARTESIAN_POINT('Ctrl Pts',(-2.50648566700006,5.2,3.84953264199999));
#304398=CARTESIAN_POINT('Ctrl Pts',(-2.50648566700006,2.2,3.84953264199999));
#304399=CARTESIAN_POINT('Ctrl Pts',(-2.50863211600006,12.2,3.85064002099998));
#304400=CARTESIAN_POINT('Ctrl Pts',(-2.50863211600006,5.2,3.85064002099998));
#304401=CARTESIAN_POINT('Ctrl Pts',(-2.50863211600006,2.2,3.85064002099998));
#304402=CARTESIAN_POINT('Ctrl Pts',(-2.51078295600006,12.2,3.85174677299998));
#304403=CARTESIAN_POINT('Ctrl Pts',(-2.51078295600006,5.2,3.85174677299998));
#304404=CARTESIAN_POINT('Ctrl Pts',(-2.51078295600006,2.2,3.85174677299998));
#304405=CARTESIAN_POINT('Ctrl Pts',(-2.51293818400006,12.2,3.85285288799999));
#304406=CARTESIAN_POINT('Ctrl Pts',(-2.51293818400006,5.2,3.85285288799999));
#304407=CARTESIAN_POINT('Ctrl Pts',(-2.51293818400006,2.2,3.85285288799999));
#304408=CARTESIAN_POINT('Ctrl Pts',(-2.51509779700006,12.2,3.85395835599999));
#304409=CARTESIAN_POINT('Ctrl Pts',(-2.51509779700006,5.2,3.85395835599999));
#304410=CARTESIAN_POINT('Ctrl Pts',(-2.51509779700006,2.2,3.85395835599999));
#304411=CARTESIAN_POINT('Ctrl Pts',(-2.51726179300006,12.2,3.85506317199999));
#304412=CARTESIAN_POINT('Ctrl Pts',(-2.51726179300006,5.2,3.85506317199999));
#304413=CARTESIAN_POINT('Ctrl Pts',(-2.51726179300006,2.2,3.85506317199999));
#304414=CARTESIAN_POINT('Ctrl Pts',(-2.51943016900006,12.2,3.85616732199999));
#304415=CARTESIAN_POINT('Ctrl Pts',(-2.51943016900006,5.2,3.85616732199999));
#304416=CARTESIAN_POINT('Ctrl Pts',(-2.51943016900006,2.2,3.85616732199999));
#304417=CARTESIAN_POINT('Ctrl Pts',(-2.52160292300006,12.2,3.85727079999998));
#304418=CARTESIAN_POINT('Ctrl Pts',(-2.52160292300006,5.2,3.85727079999998));
#304419=CARTESIAN_POINT('Ctrl Pts',(-2.52160292300006,2.2,3.85727079999998));
#304420=CARTESIAN_POINT('Ctrl Pts',(-2.52378005200006,12.2,3.85837359799999));
#304421=CARTESIAN_POINT('Ctrl Pts',(-2.52378005200006,5.2,3.85837359799999));
#304422=CARTESIAN_POINT('Ctrl Pts',(-2.52378005200006,2.2,3.85837359799999));
#304423=CARTESIAN_POINT('Ctrl Pts',(-2.52596155200006,12.2,3.85947570499999));
#304424=CARTESIAN_POINT('Ctrl Pts',(-2.52596155200006,5.2,3.85947570499999));
#304425=CARTESIAN_POINT('Ctrl Pts',(-2.52596155200006,2.2,3.85947570499999));
#304426=CARTESIAN_POINT('Ctrl Pts',(-2.52814742100006,12.2,3.86057711399998));
#304427=CARTESIAN_POINT('Ctrl Pts',(-2.52814742100006,5.2,3.86057711399998));
#304428=CARTESIAN_POINT('Ctrl Pts',(-2.52814742100006,2.2,3.86057711399998));
#304429=CARTESIAN_POINT('Ctrl Pts',(-2.53033765900006,12.2,3.86167781499999));
#304430=CARTESIAN_POINT('Ctrl Pts',(-2.53033765900006,5.2,3.86167781499999));
#304431=CARTESIAN_POINT('Ctrl Pts',(-2.53033765900006,2.2,3.86167781499999));
#304432=CARTESIAN_POINT('Ctrl Pts',(-2.53253225900006,12.2,3.86277779999999));
#304433=CARTESIAN_POINT('Ctrl Pts',(-2.53253225900006,5.2,3.86277779999999));
#304434=CARTESIAN_POINT('Ctrl Pts',(-2.53253225900006,2.2,3.86277779999999));
#304435=CARTESIAN_POINT('Ctrl Pts',(-2.53473122100006,12.2,3.86387705899998));
#304436=CARTESIAN_POINT('Ctrl Pts',(-2.53473122100006,5.2,3.86387705899998));
#304437=CARTESIAN_POINT('Ctrl Pts',(-2.53473122100006,2.2,3.86387705899998));
#304438=CARTESIAN_POINT('Ctrl Pts',(-2.53693454100006,12.2,3.86497558399999));
#304439=CARTESIAN_POINT('Ctrl Pts',(-2.53693454100006,5.2,3.86497558399999));
#304440=CARTESIAN_POINT('Ctrl Pts',(-2.53693454100006,2.2,3.86497558399999));
#304441=CARTESIAN_POINT('Ctrl Pts',(-2.53914221700006,12.2,3.86607336699999));
#304442=CARTESIAN_POINT('Ctrl Pts',(-2.53914221700006,5.2,3.86607336699999));
#304443=CARTESIAN_POINT('Ctrl Pts',(-2.53914221700006,2.2,3.86607336699999));
#304444=CARTESIAN_POINT('Ctrl Pts',(-2.54135424600006,12.2,3.86717039899998));
#304445=CARTESIAN_POINT('Ctrl Pts',(-2.54135424600006,5.2,3.86717039899998));
#304446=CARTESIAN_POINT('Ctrl Pts',(-2.54135424600006,2.2,3.86717039899998));
#304447=CARTESIAN_POINT('Ctrl Pts',(-2.54357062600006,12.2,3.86826666999998));
#304448=CARTESIAN_POINT('Ctrl Pts',(-2.54357062600006,5.2,3.86826666999998));
#304449=CARTESIAN_POINT('Ctrl Pts',(-2.54357062600006,2.2,3.86826666999998));
#304450=CARTESIAN_POINT('Ctrl Pts',(-2.54579135400005,12.2,3.86936217299999));
#304451=CARTESIAN_POINT('Ctrl Pts',(-2.54579135400005,5.2,3.86936217299999));
#304452=CARTESIAN_POINT('Ctrl Pts',(-2.54579135400005,2.2,3.86936217299999));
#304453=CARTESIAN_POINT('Ctrl Pts',(-2.54801642600006,12.2,3.87045689799999));
#304454=CARTESIAN_POINT('Ctrl Pts',(-2.54801642600006,5.2,3.87045689799999));
#304455=CARTESIAN_POINT('Ctrl Pts',(-2.54801642600006,2.2,3.87045689799999));
#304456=CARTESIAN_POINT('Ctrl Pts',(-2.55024583900005,12.2,3.87155083699999));
#304457=CARTESIAN_POINT('Ctrl Pts',(-2.55024583900005,5.2,3.87155083699999));
#304458=CARTESIAN_POINT('Ctrl Pts',(-2.55024583900005,2.2,3.87155083699999));
#304459=CARTESIAN_POINT('Ctrl Pts',(-2.55247959300006,12.2,3.87264398099998));
#304460=CARTESIAN_POINT('Ctrl Pts',(-2.55247959300006,5.2,3.87264398099998));
#304461=CARTESIAN_POINT('Ctrl Pts',(-2.55247959300006,2.2,3.87264398099998));
#304462=CARTESIAN_POINT('Ctrl Pts',(-2.55471768200006,12.2,3.87373632199999));
#304463=CARTESIAN_POINT('Ctrl Pts',(-2.55471768200006,5.2,3.87373632199999));
#304464=CARTESIAN_POINT('Ctrl Pts',(-2.55471768200006,2.2,3.87373632199999));
#304465=CARTESIAN_POINT('Ctrl Pts',(-2.55696010600006,12.2,3.87482785099999));
#304466=CARTESIAN_POINT('Ctrl Pts',(-2.55696010600006,5.2,3.87482785099999));
#304467=CARTESIAN_POINT('Ctrl Pts',(-2.55696010600006,2.2,3.87482785099999));
#304468=CARTESIAN_POINT('Ctrl Pts',(-2.55920686100006,12.2,3.87591855899998));
#304469=CARTESIAN_POINT('Ctrl Pts',(-2.55920686100006,5.2,3.87591855899998));
#304470=CARTESIAN_POINT('Ctrl Pts',(-2.55920686100006,2.2,3.87591855899998));
#304471=CARTESIAN_POINT('Ctrl Pts',(-2.56145794300005,12.2,3.87700843799998));
#304472=CARTESIAN_POINT('Ctrl Pts',(-2.56145794300005,5.2,3.87700843799998));
#304473=CARTESIAN_POINT('Ctrl Pts',(-2.56145794300005,2.2,3.87700843799998));
#304474=CARTESIAN_POINT('Ctrl Pts',(-2.56371335000006,12.2,3.87809747899999));
#304475=CARTESIAN_POINT('Ctrl Pts',(-2.56371335000006,5.2,3.87809747899999));
#304476=CARTESIAN_POINT('Ctrl Pts',(-2.56371335000006,2.2,3.87809747899999));
#304477=CARTESIAN_POINT('Ctrl Pts',(-2.56597308000006,12.2,3.87918567399999));
#304478=CARTESIAN_POINT('Ctrl Pts',(-2.56597308000006,5.2,3.87918567399999));
#304479=CARTESIAN_POINT('Ctrl Pts',(-2.56597308000006,2.2,3.87918567399999));
#304480=CARTESIAN_POINT('Ctrl Pts',(-2.56823713000006,12.2,3.88027301299999));
#304481=CARTESIAN_POINT('Ctrl Pts',(-2.56823713000006,5.2,3.88027301299999));
#304482=CARTESIAN_POINT('Ctrl Pts',(-2.56823713000006,2.2,3.88027301299999));
#304483=CARTESIAN_POINT('Ctrl Pts',(-2.57050549600006,12.2,3.88135948999999));
#304484=CARTESIAN_POINT('Ctrl Pts',(-2.57050549600006,5.2,3.88135948999999));
#304485=CARTESIAN_POINT('Ctrl Pts',(-2.57050549600006,2.2,3.88135948999999));
#304486=CARTESIAN_POINT('Ctrl Pts',(-2.57277817600006,12.2,3.88244509499999));
#304487=CARTESIAN_POINT('Ctrl Pts',(-2.57277817600006,5.2,3.88244509499999));
#304488=CARTESIAN_POINT('Ctrl Pts',(-2.57277817600006,2.2,3.88244509499999));
#304489=CARTESIAN_POINT('Ctrl Pts',(-2.57505516700005,12.2,3.88352981899998));
#304490=CARTESIAN_POINT('Ctrl Pts',(-2.57505516700005,5.2,3.88352981899998));
#304491=CARTESIAN_POINT('Ctrl Pts',(-2.57505516700005,2.2,3.88352981899998));
#304492=CARTESIAN_POINT('Ctrl Pts',(-2.57733646600005,12.2,3.88461365399999));
#304493=CARTESIAN_POINT('Ctrl Pts',(-2.57733646600005,5.2,3.88461365399999));
#304494=CARTESIAN_POINT('Ctrl Pts',(-2.57733646600005,2.2,3.88461365399999));
#304495=CARTESIAN_POINT('Ctrl Pts',(-2.57962207000006,12.2,3.88569659099999));
#304496=CARTESIAN_POINT('Ctrl Pts',(-2.57962207000006,5.2,3.88569659099999));
#304497=CARTESIAN_POINT('Ctrl Pts',(-2.57962207000006,2.2,3.88569659099999));
#304498=CARTESIAN_POINT('Ctrl Pts',(-2.58191197600006,12.2,3.88677862299998));
#304499=CARTESIAN_POINT('Ctrl Pts',(-2.58191197600006,5.2,3.88677862299998));
#304500=CARTESIAN_POINT('Ctrl Pts',(-2.58191197600006,2.2,3.88677862299998));
#304501=CARTESIAN_POINT('Ctrl Pts',(-2.58420618300006,12.2,3.88785973999998));
#304502=CARTESIAN_POINT('Ctrl Pts',(-2.58420618300006,5.2,3.88785973999998));
#304503=CARTESIAN_POINT('Ctrl Pts',(-2.58420618300006,2.2,3.88785973999998));
#304504=CARTESIAN_POINT('Ctrl Pts',(-2.58650468600006,12.2,3.88893993399999));
#304505=CARTESIAN_POINT('Ctrl Pts',(-2.58650468600006,5.2,3.88893993399999));
#304506=CARTESIAN_POINT('Ctrl Pts',(-2.58650468600006,2.2,3.88893993399999));
#304507=CARTESIAN_POINT('Ctrl Pts',(-2.58880748100006,12.2,3.89001919799998));
#304508=CARTESIAN_POINT('Ctrl Pts',(-2.58880748100006,5.2,3.89001919799998));
#304509=CARTESIAN_POINT('Ctrl Pts',(-2.58880748100006,2.2,3.89001919799998));
#304510=CARTESIAN_POINT('Ctrl Pts',(-2.59111456800006,12.2,3.89109752099999));
#304511=CARTESIAN_POINT('Ctrl Pts',(-2.59111456800006,5.2,3.89109752099999));
#304512=CARTESIAN_POINT('Ctrl Pts',(-2.59111456800006,2.2,3.89109752099999));
#304513=CARTESIAN_POINT('Ctrl Pts',(-2.59342594300006,12.2,3.89217489699998));
#304514=CARTESIAN_POINT('Ctrl Pts',(-2.59342594300006,5.2,3.89217489699998));
#304515=CARTESIAN_POINT('Ctrl Pts',(-2.59342594300006,2.2,3.89217489699998));
#304516=CARTESIAN_POINT('Ctrl Pts',(-2.59574160300006,12.2,3.89325131699999));
#304517=CARTESIAN_POINT('Ctrl Pts',(-2.59574160300006,5.2,3.89325131699999));
#304518=CARTESIAN_POINT('Ctrl Pts',(-2.59574160300006,2.2,3.89325131699999));
#304519=CARTESIAN_POINT('Ctrl Pts',(-2.59806154400006,12.2,3.89432677199999));
#304520=CARTESIAN_POINT('Ctrl Pts',(-2.59806154400006,5.2,3.89432677199999));
#304521=CARTESIAN_POINT('Ctrl Pts',(-2.59806154400006,2.2,3.89432677199999));
#304522=CARTESIAN_POINT('Ctrl Pts',(-2.60038576400006,12.2,3.89540125299998));
#304523=CARTESIAN_POINT('Ctrl Pts',(-2.60038576400006,5.2,3.89540125299998));
#304524=CARTESIAN_POINT('Ctrl Pts',(-2.60038576400006,2.2,3.89540125299998));
#304525=CARTESIAN_POINT('Ctrl Pts',(-2.60271426100006,12.2,3.89647475399999));
#304526=CARTESIAN_POINT('Ctrl Pts',(-2.60271426100006,5.2,3.89647475399999));
#304527=CARTESIAN_POINT('Ctrl Pts',(-2.60271426100006,2.2,3.89647475399999));
#304528=CARTESIAN_POINT('Ctrl Pts',(-2.60504703000006,12.2,3.89754726299999));
#304529=CARTESIAN_POINT('Ctrl Pts',(-2.60504703000006,5.2,3.89754726299999));
#304530=CARTESIAN_POINT('Ctrl Pts',(-2.60504703000006,2.2,3.89754726299999));
#304531=CARTESIAN_POINT('Ctrl Pts',(-2.60738406800006,12.2,3.89861877599999));
#304532=CARTESIAN_POINT('Ctrl Pts',(-2.60738406800006,5.2,3.89861877599999));
#304533=CARTESIAN_POINT('Ctrl Pts',(-2.60738406800006,2.2,3.89861877599999));
#304534=CARTESIAN_POINT('Ctrl Pts',(-2.60972537500006,12.2,3.89968928099999));
#304535=CARTESIAN_POINT('Ctrl Pts',(-2.60972537500006,5.2,3.89968928099999));
#304536=CARTESIAN_POINT('Ctrl Pts',(-2.60972537500006,2.2,3.89968928099999));
#304537=CARTESIAN_POINT('Ctrl Pts',(-2.61207094500006,12.2,3.90075877199998));
#304538=CARTESIAN_POINT('Ctrl Pts',(-2.61207094500006,5.2,3.90075877199998));
#304539=CARTESIAN_POINT('Ctrl Pts',(-2.61207094500006,2.2,3.90075877199998));
#304540=CARTESIAN_POINT('Ctrl Pts',(-2.61442077600006,12.2,3.90182724099999));
#304541=CARTESIAN_POINT('Ctrl Pts',(-2.61442077600006,5.2,3.90182724099999));
#304542=CARTESIAN_POINT('Ctrl Pts',(-2.61442077600006,2.2,3.90182724099999));
#304543=CARTESIAN_POINT('Ctrl Pts',(-2.61677486500006,12.2,3.90289467799998));
#304544=CARTESIAN_POINT('Ctrl Pts',(-2.61677486500006,5.2,3.90289467799998));
#304545=CARTESIAN_POINT('Ctrl Pts',(-2.61677486500006,2.2,3.90289467799998));
#304546=CARTESIAN_POINT('Ctrl Pts',(-2.61913321100006,12.2,3.90396107699999));
#304547=CARTESIAN_POINT('Ctrl Pts',(-2.61913321100006,5.2,3.90396107699999));
#304548=CARTESIAN_POINT('Ctrl Pts',(-2.61913321100006,2.2,3.90396107699999));
#304549=CARTESIAN_POINT('Ctrl Pts',(-2.62149580800005,12.2,3.90502642799999));
#304550=CARTESIAN_POINT('Ctrl Pts',(-2.62149580800005,5.2,3.90502642799999));
#304551=CARTESIAN_POINT('Ctrl Pts',(-2.62149580800005,2.2,3.90502642799999));
#304552=CARTESIAN_POINT('Ctrl Pts',(-2.62386265300006,12.2,3.90609072399998));
#304553=CARTESIAN_POINT('Ctrl Pts',(-2.62386265300006,5.2,3.90609072399998));
#304554=CARTESIAN_POINT('Ctrl Pts',(-2.62386265300006,2.2,3.90609072399998));
#304555=CARTESIAN_POINT('Ctrl Pts',(-2.62623374500006,12.2,3.90715395499999));
#304556=CARTESIAN_POINT('Ctrl Pts',(-2.62623374500006,5.2,3.90715395499999));
#304557=CARTESIAN_POINT('Ctrl Pts',(-2.62623374500006,2.2,3.90715395499999));
#304558=CARTESIAN_POINT('Ctrl Pts',(-2.62860907900006,12.2,3.90821611299998));
#304559=CARTESIAN_POINT('Ctrl Pts',(-2.62860907900006,5.2,3.90821611299998));
#304560=CARTESIAN_POINT('Ctrl Pts',(-2.62860907900006,2.2,3.90821611299998));
#304561=CARTESIAN_POINT('Ctrl Pts',(-2.63098865200006,12.2,3.90927718999999));
#304562=CARTESIAN_POINT('Ctrl Pts',(-2.63098865200006,5.2,3.90927718999999));
#304563=CARTESIAN_POINT('Ctrl Pts',(-2.63098865200006,2.2,3.90927718999999));
#304564=CARTESIAN_POINT('Ctrl Pts',(-2.63337246200006,12.2,3.91033717599999));
#304565=CARTESIAN_POINT('Ctrl Pts',(-2.63337246200006,5.2,3.91033717599999));
#304566=CARTESIAN_POINT('Ctrl Pts',(-2.63337246200006,2.2,3.91033717599999));
#304567=CARTESIAN_POINT('Ctrl Pts',(-2.63576050600005,12.2,3.91139606699999));
#304568=CARTESIAN_POINT('Ctrl Pts',(-2.63576050600005,5.2,3.91139606699999));
#304569=CARTESIAN_POINT('Ctrl Pts',(-2.63576050600005,2.2,3.91139606699999));
#304570=CARTESIAN_POINT('Ctrl Pts',(-2.63815278000005,12.2,3.91245385499998));
#304571=CARTESIAN_POINT('Ctrl Pts',(-2.63815278000005,5.2,3.91245385499998));
#304572=CARTESIAN_POINT('Ctrl Pts',(-2.63815278000005,2.2,3.91245385499998));
#304573=CARTESIAN_POINT('Ctrl Pts',(-2.64054928300005,12.2,3.91351052999998));
#304574=CARTESIAN_POINT('Ctrl Pts',(-2.64054928300005,5.2,3.91351052999998));
#304575=CARTESIAN_POINT('Ctrl Pts',(-2.64054928300005,2.2,3.91351052999998));
#304576=CARTESIAN_POINT('Ctrl Pts',(-2.64295001200006,12.2,3.91456608699999));
#304577=CARTESIAN_POINT('Ctrl Pts',(-2.64295001200006,5.2,3.91456608699999));
#304578=CARTESIAN_POINT('Ctrl Pts',(-2.64295001200006,2.2,3.91456608699999));
#304579=CARTESIAN_POINT('Ctrl Pts',(-2.64535496200006,12.2,3.91562051599998));
#304580=CARTESIAN_POINT('Ctrl Pts',(-2.64535496200006,5.2,3.91562051599998));
#304581=CARTESIAN_POINT('Ctrl Pts',(-2.64535496200006,2.2,3.91562051599998));
#304582=CARTESIAN_POINT('Ctrl Pts',(-2.64776413100006,12.2,3.91667381099998));
#304583=CARTESIAN_POINT('Ctrl Pts',(-2.64776413100006,5.2,3.91667381099998));
#304584=CARTESIAN_POINT('Ctrl Pts',(-2.64776413100006,2.2,3.91667381099998));
#304585=CARTESIAN_POINT('Ctrl Pts',(-2.65017751500006,12.2,3.91772595899998));
#304586=CARTESIAN_POINT('Ctrl Pts',(-2.65017751500006,5.2,3.91772595899998));
#304587=CARTESIAN_POINT('Ctrl Pts',(-2.65017751500006,2.2,3.91772595899998));
#304588=CARTESIAN_POINT('Ctrl Pts',(-2.65259511000006,12.2,3.91877695099998));
#304589=CARTESIAN_POINT('Ctrl Pts',(-2.65259511000006,5.2,3.91877695099998));
#304590=CARTESIAN_POINT('Ctrl Pts',(-2.65259511000006,2.2,3.91877695099998));
#304591=CARTESIAN_POINT('Ctrl Pts',(-2.65501691200006,12.2,3.91982677899998));
#304592=CARTESIAN_POINT('Ctrl Pts',(-2.65501691200006,5.2,3.91982677899998));
#304593=CARTESIAN_POINT('Ctrl Pts',(-2.65501691200006,2.2,3.91982677899998));
#304594=CARTESIAN_POINT('Ctrl Pts',(-2.65744291800006,12.2,3.92087542999998));
#304595=CARTESIAN_POINT('Ctrl Pts',(-2.65744291800006,5.2,3.92087542999998));
#304596=CARTESIAN_POINT('Ctrl Pts',(-2.65744291800006,2.2,3.92087542999998));
#304597=CARTESIAN_POINT('Ctrl Pts',(-2.65987312500005,12.2,3.92192289899998));
#304598=CARTESIAN_POINT('Ctrl Pts',(-2.65987312500005,5.2,3.92192289899998));
#304599=CARTESIAN_POINT('Ctrl Pts',(-2.65987312500005,2.2,3.92192289899998));
#304600=CARTESIAN_POINT('Ctrl Pts',(-2.66230753100006,12.2,3.92296918099999));
#304601=CARTESIAN_POINT('Ctrl Pts',(-2.66230753100006,5.2,3.92296918099999));
#304602=CARTESIAN_POINT('Ctrl Pts',(-2.66230753100006,2.2,3.92296918099999));
#304603=CARTESIAN_POINT('Ctrl Pts',(-2.66474613200006,12.2,3.92401427099998));
#304604=CARTESIAN_POINT('Ctrl Pts',(-2.66474613200006,5.2,3.92401427099998));
#304605=CARTESIAN_POINT('Ctrl Pts',(-2.66474613200006,2.2,3.92401427099998));
#304606=CARTESIAN_POINT('Ctrl Pts',(-2.66718893010949,12.2,3.92505816704675));
#304607=CARTESIAN_POINT('Ctrl Pts',(-2.66718893010949,5.2,3.92505816704675));
#304608=CARTESIAN_POINT('Ctrl Pts',(-2.66718893010949,2.2,3.92505816704675));
#304609=CARTESIAN_POINT('Ctrl Pts',(-2.6691465242193,12.2,3.92589232709341));
#304610=CARTESIAN_POINT('Ctrl Pts',(-2.6691465242193,5.2,3.92589232709341));
#304611=CARTESIAN_POINT('Ctrl Pts',(-2.6691465242193,2.2,3.92589232709341));
#304612=CARTESIAN_POINT('Ctrl Pts',(-2.67061660832935,12.2,3.92651741014));
#304613=CARTESIAN_POINT('Ctrl Pts',(-2.67061660832935,5.2,3.92651741014));
#304614=CARTESIAN_POINT('Ctrl Pts',(-2.67061660832935,2.2,3.92651741014));
#304615=CARTESIAN_POINT('Ctrl Pts',(-2.67159750343949,12.2,3.92693389218658));
#304616=CARTESIAN_POINT('Ctrl Pts',(-2.67159750343949,5.2,3.92693389218658));
#304617=CARTESIAN_POINT('Ctrl Pts',(-2.67159750343949,2.2,3.92693389218658));
#304618=CARTESIAN_POINT('Ctrl Pts',(-2.67208816000006,12.2,3.92714207399998));
#304619=CARTESIAN_POINT('Ctrl Pts',(-2.67208816000006,5.2,3.92714207399998));
#304620=CARTESIAN_POINT('Ctrl Pts',(-2.67208816000006,2.2,3.92714207399998));
#304621=CARTESIAN_POINT('',(-2.67208816000006,2.7,3.92714207399998));
#304622=CARTESIAN_POINT('',(-2.67208816000006,12.2,3.92714207399998));
#304623=CARTESIAN_POINT('Ctrl Pts',(-2.00390028800005,2.7,3.45459777299999));
#304624=CARTESIAN_POINT('Ctrl Pts',(-2.00531915316731,2.7,3.4570231905594));
#304625=CARTESIAN_POINT('Ctrl Pts',(-2.01694587943621,2.70000000004265,
3.47600453024496));
#304626=CARTESIAN_POINT('Ctrl Pts',(-2.07286963137762,2.70000000004265,
3.54137416856458));
#304627=CARTESIAN_POINT('Ctrl Pts',(-2.11342407259217,2.7,3.58245428063435));
#304628=CARTESIAN_POINT('Ctrl Pts',(-2.28821013174135,2.7,3.72952114371137));
#304629=CARTESIAN_POINT('Ctrl Pts',(-2.45288578684387,2.7,3.83413618920365));
#304630=CARTESIAN_POINT('Ctrl Pts',(-2.67208816000006,2.7,3.92714207399998));
#304631=CARTESIAN_POINT('Origin',(-5.66300478732629E-14,15.2,-1.77635683940025E-14));
#304632=CARTESIAN_POINT('',(-2.94378355400006,2.7,3.72781952199999));
#304633=CARTESIAN_POINT('',(-2.94378355400006,12.2,3.72781952199999));
#304634=CARTESIAN_POINT('Origin',(-5.66300478732629E-14,2.7,-1.92943768261394E-14));
#304635=CARTESIAN_POINT('Ctrl Pts',(-2.94378355400006,12.2,3.72781952199999));
#304636=CARTESIAN_POINT('Ctrl Pts',(-2.94378355400006,5.2,3.72781952199999));
#304637=CARTESIAN_POINT('Ctrl Pts',(-2.94378355400006,2.2,3.72781952199999));
#304638=CARTESIAN_POINT('Ctrl Pts',(-2.94373227900006,12.2,3.72728899799998));
#304639=CARTESIAN_POINT('Ctrl Pts',(-2.94373227900006,5.2,3.72728899799998));
#304640=CARTESIAN_POINT('Ctrl Pts',(-2.94373227900006,2.2,3.72728899799998));
#304641=CARTESIAN_POINT('Ctrl Pts',(-2.94362949000006,12.2,3.72622831699999));
#304642=CARTESIAN_POINT('Ctrl Pts',(-2.94362949000006,5.2,3.72622831699999));
#304643=CARTESIAN_POINT('Ctrl Pts',(-2.94362949000006,2.2,3.72622831699999));
#304644=CARTESIAN_POINT('Ctrl Pts',(-2.94347458500006,12.2,3.72463838599998));
#304645=CARTESIAN_POINT('Ctrl Pts',(-2.94347458500006,5.2,3.72463838599998));
#304646=CARTESIAN_POINT('Ctrl Pts',(-2.94347458500006,2.2,3.72463838599998));
#304647=CARTESIAN_POINT('Ctrl Pts',(-2.94326660500006,12.2,3.72252066499998));
#304648=CARTESIAN_POINT('Ctrl Pts',(-2.94326660500006,5.2,3.72252066499998));
#304649=CARTESIAN_POINT('Ctrl Pts',(-2.94326660500006,2.2,3.72252066499998));
#304650=CARTESIAN_POINT('Ctrl Pts',(-2.94300422900006,12.2,3.71987715499999));
#304651=CARTESIAN_POINT('Ctrl Pts',(-2.94300422900006,5.2,3.71987715499999));
#304652=CARTESIAN_POINT('Ctrl Pts',(-2.94300422900006,2.2,3.71987715499999));
#304653=CARTESIAN_POINT('Ctrl Pts',(-2.94273945600006,12.2,3.71723729099998));
#304654=CARTESIAN_POINT('Ctrl Pts',(-2.94273945600006,5.2,3.71723729099998));
#304655=CARTESIAN_POINT('Ctrl Pts',(-2.94273945600006,2.2,3.71723729099998));
#304656=CARTESIAN_POINT('Ctrl Pts',(-2.94247228600006,12.2,3.71460107099999));
#304657=CARTESIAN_POINT('Ctrl Pts',(-2.94247228600006,5.2,3.71460107099999));
#304658=CARTESIAN_POINT('Ctrl Pts',(-2.94247228600006,2.2,3.71460107099999));
#304659=CARTESIAN_POINT('Ctrl Pts',(-2.94220272300006,12.2,3.71196849999999));
#304660=CARTESIAN_POINT('Ctrl Pts',(-2.94220272300006,5.2,3.71196849999999));
#304661=CARTESIAN_POINT('Ctrl Pts',(-2.94220272300006,2.2,3.71196849999999));
#304662=CARTESIAN_POINT('Ctrl Pts',(-2.94193076900005,12.2,3.70933957999998));
#304663=CARTESIAN_POINT('Ctrl Pts',(-2.94193076900005,5.2,3.70933957999998));
#304664=CARTESIAN_POINT('Ctrl Pts',(-2.94193076900005,2.2,3.70933957999998));
#304665=CARTESIAN_POINT('Ctrl Pts',(-2.94165643500006,12.2,3.70671431799998));
#304666=CARTESIAN_POINT('Ctrl Pts',(-2.94165643500006,5.2,3.70671431799998));
#304667=CARTESIAN_POINT('Ctrl Pts',(-2.94165643500006,2.2,3.70671431799998));
#304668=CARTESIAN_POINT('Ctrl Pts',(-2.94137972400006,12.2,3.70409271899998));
#304669=CARTESIAN_POINT('Ctrl Pts',(-2.94137972400006,5.2,3.70409271899998));
#304670=CARTESIAN_POINT('Ctrl Pts',(-2.94137972400006,2.2,3.70409271899998));
#304671=CARTESIAN_POINT('Ctrl Pts',(-2.94110064700006,12.2,3.70147478899998));
#304672=CARTESIAN_POINT('Ctrl Pts',(-2.94110064700006,5.2,3.70147478899998));
#304673=CARTESIAN_POINT('Ctrl Pts',(-2.94110064700006,2.2,3.70147478899998));
#304674=CARTESIAN_POINT('Ctrl Pts',(-2.94081921200006,12.2,3.69886053599998));
#304675=CARTESIAN_POINT('Ctrl Pts',(-2.94081921200006,5.2,3.69886053599998));
#304676=CARTESIAN_POINT('Ctrl Pts',(-2.94081921200006,2.2,3.69886053599998));
#304677=CARTESIAN_POINT('Ctrl Pts',(-2.94053542700006,12.2,3.69624996699999));
#304678=CARTESIAN_POINT('Ctrl Pts',(-2.94053542700006,5.2,3.69624996699999));
#304679=CARTESIAN_POINT('Ctrl Pts',(-2.94053542700006,2.2,3.69624996699999));
#304680=CARTESIAN_POINT('Ctrl Pts',(-2.94024929900006,12.2,3.69364308599998));
#304681=CARTESIAN_POINT('Ctrl Pts',(-2.94024929900006,5.2,3.69364308599998));
#304682=CARTESIAN_POINT('Ctrl Pts',(-2.94024929900006,2.2,3.69364308599998));
#304683=CARTESIAN_POINT('Ctrl Pts',(-2.93996083600006,12.2,3.69103989999999));
#304684=CARTESIAN_POINT('Ctrl Pts',(-2.93996083600006,5.2,3.69103989999999));
#304685=CARTESIAN_POINT('Ctrl Pts',(-2.93996083600006,2.2,3.69103989999999));
#304686=CARTESIAN_POINT('Ctrl Pts',(-2.93967004300006,12.2,3.68844041299998));
#304687=CARTESIAN_POINT('Ctrl Pts',(-2.93967004300006,5.2,3.68844041299998));
#304688=CARTESIAN_POINT('Ctrl Pts',(-2.93967004300006,2.2,3.68844041299998));
#304689=CARTESIAN_POINT('Ctrl Pts',(-2.93937692700006,12.2,3.68584463099998));
#304690=CARTESIAN_POINT('Ctrl Pts',(-2.93937692700006,5.2,3.68584463099998));
#304691=CARTESIAN_POINT('Ctrl Pts',(-2.93937692700006,2.2,3.68584463099998));
#304692=CARTESIAN_POINT('Ctrl Pts',(-2.93908149400006,12.2,3.68325255699999));
#304693=CARTESIAN_POINT('Ctrl Pts',(-2.93908149400006,5.2,3.68325255699999));
#304694=CARTESIAN_POINT('Ctrl Pts',(-2.93908149400006,2.2,3.68325255699999));
#304695=CARTESIAN_POINT('Ctrl Pts',(-2.93878375000005,12.2,3.68066419899999));
#304696=CARTESIAN_POINT('Ctrl Pts',(-2.93878375000005,5.2,3.68066419899999));
#304697=CARTESIAN_POINT('Ctrl Pts',(-2.93878375000005,2.2,3.68066419899999));
#304698=CARTESIAN_POINT('Ctrl Pts',(-2.93848370200006,12.2,3.67807955899998));
#304699=CARTESIAN_POINT('Ctrl Pts',(-2.93848370200006,5.2,3.67807955899998));
#304700=CARTESIAN_POINT('Ctrl Pts',(-2.93848370200006,2.2,3.67807955899998));
#304701=CARTESIAN_POINT('Ctrl Pts',(-2.93818135600006,12.2,3.67549864399999));
#304702=CARTESIAN_POINT('Ctrl Pts',(-2.93818135600006,5.2,3.67549864399999));
#304703=CARTESIAN_POINT('Ctrl Pts',(-2.93818135600006,2.2,3.67549864399999));
#304704=CARTESIAN_POINT('Ctrl Pts',(-2.93787672200006,12.2,3.67292145899999));
#304705=CARTESIAN_POINT('Ctrl Pts',(-2.93787672200006,5.2,3.67292145899999));
#304706=CARTESIAN_POINT('Ctrl Pts',(-2.93787672200006,2.2,3.67292145899999));
#304707=CARTESIAN_POINT('Ctrl Pts',(-2.93756980300006,12.2,3.67034801099998));
#304708=CARTESIAN_POINT('Ctrl Pts',(-2.93756980300006,5.2,3.67034801099998));
#304709=CARTESIAN_POINT('Ctrl Pts',(-2.93756980300006,2.2,3.67034801099998));
#304710=CARTESIAN_POINT('Ctrl Pts',(-2.93726060900006,12.2,3.66777830299998));
#304711=CARTESIAN_POINT('Ctrl Pts',(-2.93726060900006,5.2,3.66777830299998));
#304712=CARTESIAN_POINT('Ctrl Pts',(-2.93726060900006,2.2,3.66777830299998));
#304713=CARTESIAN_POINT('Ctrl Pts',(-2.93694914700006,12.2,3.66521234299999));
#304714=CARTESIAN_POINT('Ctrl Pts',(-2.93694914700006,5.2,3.66521234299999));
#304715=CARTESIAN_POINT('Ctrl Pts',(-2.93694914700006,2.2,3.66521234299999));
#304716=CARTESIAN_POINT('Ctrl Pts',(-2.93663542300005,12.2,3.66265013499999));
#304717=CARTESIAN_POINT('Ctrl Pts',(-2.93663542300005,5.2,3.66265013499999));
#304718=CARTESIAN_POINT('Ctrl Pts',(-2.93663542300005,2.2,3.66265013499999));
#304719=CARTESIAN_POINT('Ctrl Pts',(-2.93631944400006,12.2,3.66009168499998));
#304720=CARTESIAN_POINT('Ctrl Pts',(-2.93631944400006,5.2,3.66009168499998));
#304721=CARTESIAN_POINT('Ctrl Pts',(-2.93631944400006,2.2,3.66009168499998));
#304722=CARTESIAN_POINT('Ctrl Pts',(-2.93600121800006,12.2,3.65753699699999));
#304723=CARTESIAN_POINT('Ctrl Pts',(-2.93600121800006,5.2,3.65753699699999));
#304724=CARTESIAN_POINT('Ctrl Pts',(-2.93600121800006,2.2,3.65753699699999));
#304725=CARTESIAN_POINT('Ctrl Pts',(-2.93568075100006,12.2,3.65498607799999));
#304726=CARTESIAN_POINT('Ctrl Pts',(-2.93568075100006,5.2,3.65498607799999));
#304727=CARTESIAN_POINT('Ctrl Pts',(-2.93568075100006,2.2,3.65498607799999));
#304728=CARTESIAN_POINT('Ctrl Pts',(-2.93535804900006,12.2,3.65243893199998));
#304729=CARTESIAN_POINT('Ctrl Pts',(-2.93535804900006,5.2,3.65243893199998));
#304730=CARTESIAN_POINT('Ctrl Pts',(-2.93535804900006,2.2,3.65243893199998));
#304731=CARTESIAN_POINT('Ctrl Pts',(-2.93503312000006,12.2,3.64989556399999));
#304732=CARTESIAN_POINT('Ctrl Pts',(-2.93503312000006,5.2,3.64989556399999));
#304733=CARTESIAN_POINT('Ctrl Pts',(-2.93503312000006,2.2,3.64989556399999));
#304734=CARTESIAN_POINT('Ctrl Pts',(-2.93470597200006,12.2,3.64735597999999));
#304735=CARTESIAN_POINT('Ctrl Pts',(-2.93470597200006,5.2,3.64735597999999));
#304736=CARTESIAN_POINT('Ctrl Pts',(-2.93470597200006,2.2,3.64735597999999));
#304737=CARTESIAN_POINT('Ctrl Pts',(-2.93437661100006,12.2,3.64482018699999));
#304738=CARTESIAN_POINT('Ctrl Pts',(-2.93437661100006,5.2,3.64482018699999));
#304739=CARTESIAN_POINT('Ctrl Pts',(-2.93437661100006,2.2,3.64482018699999));
#304740=CARTESIAN_POINT('Ctrl Pts',(-2.93404504400006,12.2,3.64228818699999));
#304741=CARTESIAN_POINT('Ctrl Pts',(-2.93404504400006,5.2,3.64228818699999));
#304742=CARTESIAN_POINT('Ctrl Pts',(-2.93404504400006,2.2,3.64228818699999));
#304743=CARTESIAN_POINT('Ctrl Pts',(-2.93371127800006,12.2,3.63975998699999));
#304744=CARTESIAN_POINT('Ctrl Pts',(-2.93371127800006,5.2,3.63975998699999));
#304745=CARTESIAN_POINT('Ctrl Pts',(-2.93371127800006,2.2,3.63975998699999));
#304746=CARTESIAN_POINT('Ctrl Pts',(-2.93337532100006,12.2,3.63723559299999));
#304747=CARTESIAN_POINT('Ctrl Pts',(-2.93337532100006,5.2,3.63723559299999));
#304748=CARTESIAN_POINT('Ctrl Pts',(-2.93337532100006,2.2,3.63723559299999));
#304749=CARTESIAN_POINT('Ctrl Pts',(-2.93303717900006,12.2,3.63471500999999));
#304750=CARTESIAN_POINT('Ctrl Pts',(-2.93303717900006,5.2,3.63471500999999));
#304751=CARTESIAN_POINT('Ctrl Pts',(-2.93303717900006,2.2,3.63471500999999));
#304752=CARTESIAN_POINT('Ctrl Pts',(-2.93269686000006,12.2,3.63219824299998));
#304753=CARTESIAN_POINT('Ctrl Pts',(-2.93269686000006,5.2,3.63219824299998));
#304754=CARTESIAN_POINT('Ctrl Pts',(-2.93269686000006,2.2,3.63219824299998));
#304755=CARTESIAN_POINT('Ctrl Pts',(-2.93235437200006,12.2,3.62968529699998));
#304756=CARTESIAN_POINT('Ctrl Pts',(-2.93235437200006,5.2,3.62968529699998));
#304757=CARTESIAN_POINT('Ctrl Pts',(-2.93235437200006,2.2,3.62968529699998));
#304758=CARTESIAN_POINT('Ctrl Pts',(-2.93200972000006,12.2,3.62717617799999));
#304759=CARTESIAN_POINT('Ctrl Pts',(-2.93200972000006,5.2,3.62717617799999));
#304760=CARTESIAN_POINT('Ctrl Pts',(-2.93200972000006,2.2,3.62717617799999));
#304761=CARTESIAN_POINT('Ctrl Pts',(-2.93166291300006,12.2,3.62467089099999));
#304762=CARTESIAN_POINT('Ctrl Pts',(-2.93166291300006,5.2,3.62467089099999));
#304763=CARTESIAN_POINT('Ctrl Pts',(-2.93166291300006,2.2,3.62467089099999));
#304764=CARTESIAN_POINT('Ctrl Pts',(-2.93131395600006,12.2,3.62216943999999));
#304765=CARTESIAN_POINT('Ctrl Pts',(-2.93131395600006,5.2,3.62216943999999));
#304766=CARTESIAN_POINT('Ctrl Pts',(-2.93131395600006,2.2,3.62216943999999));
#304767=CARTESIAN_POINT('Ctrl Pts',(-2.93096285900006,12.2,3.61967183199998));
#304768=CARTESIAN_POINT('Ctrl Pts',(-2.93096285900006,5.2,3.61967183199998));
#304769=CARTESIAN_POINT('Ctrl Pts',(-2.93096285900006,2.2,3.61967183199998));
#304770=CARTESIAN_POINT('Ctrl Pts',(-2.93060962800006,12.2,3.61717807199998));
#304771=CARTESIAN_POINT('Ctrl Pts',(-2.93060962800006,5.2,3.61717807199998));
#304772=CARTESIAN_POINT('Ctrl Pts',(-2.93060962800006,2.2,3.61717807199998));
#304773=CARTESIAN_POINT('Ctrl Pts',(-2.93025426900006,12.2,3.61468816499999));
#304774=CARTESIAN_POINT('Ctrl Pts',(-2.93025426900006,5.2,3.61468816499999));
#304775=CARTESIAN_POINT('Ctrl Pts',(-2.93025426900006,2.2,3.61468816499999));
#304776=CARTESIAN_POINT('Ctrl Pts',(-2.92989679200006,12.2,3.61220211699998));
#304777=CARTESIAN_POINT('Ctrl Pts',(-2.92989679200006,5.2,3.61220211699998));
#304778=CARTESIAN_POINT('Ctrl Pts',(-2.92989679200006,2.2,3.61220211699998));
#304779=CARTESIAN_POINT('Ctrl Pts',(-2.92953720100006,12.2,3.60971993199998));
#304780=CARTESIAN_POINT('Ctrl Pts',(-2.92953720100006,5.2,3.60971993199998));
#304781=CARTESIAN_POINT('Ctrl Pts',(-2.92953720100006,2.2,3.60971993199998));
#304782=CARTESIAN_POINT('Ctrl Pts',(-2.92917550600006,12.2,3.60724161599999));
#304783=CARTESIAN_POINT('Ctrl Pts',(-2.92917550600006,5.2,3.60724161599999));
#304784=CARTESIAN_POINT('Ctrl Pts',(-2.92917550600006,2.2,3.60724161599999));
#304785=CARTESIAN_POINT('Ctrl Pts',(-2.92881171300006,12.2,3.60476717399998));
#304786=CARTESIAN_POINT('Ctrl Pts',(-2.92881171300006,5.2,3.60476717399998));
#304787=CARTESIAN_POINT('Ctrl Pts',(-2.92881171300006,2.2,3.60476717399998));
#304788=CARTESIAN_POINT('Ctrl Pts',(-2.92844583100006,12.2,3.60229661199998));
#304789=CARTESIAN_POINT('Ctrl Pts',(-2.92844583100006,5.2,3.60229661199998));
#304790=CARTESIAN_POINT('Ctrl Pts',(-2.92844583100006,2.2,3.60229661199998));
#304791=CARTESIAN_POINT('Ctrl Pts',(-2.92807786400005,12.2,3.59982993399999));
#304792=CARTESIAN_POINT('Ctrl Pts',(-2.92807786400005,5.2,3.59982993399999));
#304793=CARTESIAN_POINT('Ctrl Pts',(-2.92807786400005,2.2,3.59982993399999));
#304794=CARTESIAN_POINT('Ctrl Pts',(-2.92770782300006,12.2,3.59736714599999));
#304795=CARTESIAN_POINT('Ctrl Pts',(-2.92770782300006,5.2,3.59736714599999));
#304796=CARTESIAN_POINT('Ctrl Pts',(-2.92770782300006,2.2,3.59736714599999));
#304797=CARTESIAN_POINT('Ctrl Pts',(-2.92733571200006,12.2,3.59490825399998));
#304798=CARTESIAN_POINT('Ctrl Pts',(-2.92733571200006,5.2,3.59490825399998));
#304799=CARTESIAN_POINT('Ctrl Pts',(-2.92733571200006,2.2,3.59490825399998));
#304800=CARTESIAN_POINT('Ctrl Pts',(-2.92696154200006,12.2,3.59245326099998));
#304801=CARTESIAN_POINT('Ctrl Pts',(-2.92696154200006,5.2,3.59245326099998));
#304802=CARTESIAN_POINT('Ctrl Pts',(-2.92696154200006,2.2,3.59245326099998));
#304803=CARTESIAN_POINT('Ctrl Pts',(-2.92658531800006,12.2,3.59000217499998));
#304804=CARTESIAN_POINT('Ctrl Pts',(-2.92658531800006,5.2,3.59000217499998));
#304805=CARTESIAN_POINT('Ctrl Pts',(-2.92658531800006,2.2,3.59000217499998));
#304806=CARTESIAN_POINT('Ctrl Pts',(-2.92620704700005,12.2,3.58755499999998));
#304807=CARTESIAN_POINT('Ctrl Pts',(-2.92620704700005,5.2,3.58755499999998));
#304808=CARTESIAN_POINT('Ctrl Pts',(-2.92620704700005,2.2,3.58755499999998));
#304809=CARTESIAN_POINT('Ctrl Pts',(-2.92582673900006,12.2,3.58511173999998));
#304810=CARTESIAN_POINT('Ctrl Pts',(-2.92582673900006,5.2,3.58511173999998));
#304811=CARTESIAN_POINT('Ctrl Pts',(-2.92582673900006,2.2,3.58511173999998));
#304812=CARTESIAN_POINT('Ctrl Pts',(-2.92544440000006,12.2,3.58267240299998));
#304813=CARTESIAN_POINT('Ctrl Pts',(-2.92544440000006,5.2,3.58267240299998));
#304814=CARTESIAN_POINT('Ctrl Pts',(-2.92544440000006,2.2,3.58267240299998));
#304815=CARTESIAN_POINT('Ctrl Pts',(-2.92506003600006,12.2,3.58023699199999));
#304816=CARTESIAN_POINT('Ctrl Pts',(-2.92506003600006,5.2,3.58023699199999));
#304817=CARTESIAN_POINT('Ctrl Pts',(-2.92506003600006,2.2,3.58023699199999));
#304818=CARTESIAN_POINT('Ctrl Pts',(-2.92467365700006,12.2,3.57780551299999));
#304819=CARTESIAN_POINT('Ctrl Pts',(-2.92467365700006,5.2,3.57780551299999));
#304820=CARTESIAN_POINT('Ctrl Pts',(-2.92467365700006,2.2,3.57780551299999));
#304821=CARTESIAN_POINT('Ctrl Pts',(-2.92428526900005,12.2,3.57537797099998));
#304822=CARTESIAN_POINT('Ctrl Pts',(-2.92428526900005,5.2,3.57537797099998));
#304823=CARTESIAN_POINT('Ctrl Pts',(-2.92428526900005,2.2,3.57537797099998));
#304824=CARTESIAN_POINT('Ctrl Pts',(-2.92389488000006,12.2,3.57295437199999));
#304825=CARTESIAN_POINT('Ctrl Pts',(-2.92389488000006,5.2,3.57295437199999));
#304826=CARTESIAN_POINT('Ctrl Pts',(-2.92389488000006,2.2,3.57295437199999));
#304827=CARTESIAN_POINT('Ctrl Pts',(-2.92350249700006,12.2,3.57053471999999));
#304828=CARTESIAN_POINT('Ctrl Pts',(-2.92350249700006,5.2,3.57053471999999));
#304829=CARTESIAN_POINT('Ctrl Pts',(-2.92350249700006,2.2,3.57053471999999));
#304830=CARTESIAN_POINT('Ctrl Pts',(-2.92310812900006,12.2,3.56811902099999));
#304831=CARTESIAN_POINT('Ctrl Pts',(-2.92310812900006,5.2,3.56811902099999));
#304832=CARTESIAN_POINT('Ctrl Pts',(-2.92310812900006,2.2,3.56811902099999));
#304833=CARTESIAN_POINT('Ctrl Pts',(-2.92271178200005,12.2,3.56570727999999));
#304834=CARTESIAN_POINT('Ctrl Pts',(-2.92271178200005,5.2,3.56570727999999));
#304835=CARTESIAN_POINT('Ctrl Pts',(-2.92271178200005,2.2,3.56570727999999));
#304836=CARTESIAN_POINT('Ctrl Pts',(-2.92231346500006,12.2,3.56329950299998));
#304837=CARTESIAN_POINT('Ctrl Pts',(-2.92231346500006,5.2,3.56329950299998));
#304838=CARTESIAN_POINT('Ctrl Pts',(-2.92231346500006,2.2,3.56329950299998));
#304839=CARTESIAN_POINT('Ctrl Pts',(-2.92191318400006,12.2,3.56089569299999));
#304840=CARTESIAN_POINT('Ctrl Pts',(-2.92191318400006,5.2,3.56089569299999));
#304841=CARTESIAN_POINT('Ctrl Pts',(-2.92191318400006,2.2,3.56089569299999));
#304842=CARTESIAN_POINT('Ctrl Pts',(-2.92151094800006,12.2,3.55849585699998));
#304843=CARTESIAN_POINT('Ctrl Pts',(-2.92151094800006,5.2,3.55849585699998));
#304844=CARTESIAN_POINT('Ctrl Pts',(-2.92151094800006,2.2,3.55849585699998));
#304845=CARTESIAN_POINT('Ctrl Pts',(-2.92110676400006,12.2,3.55610000199999));
#304846=CARTESIAN_POINT('Ctrl Pts',(-2.92110676400006,5.2,3.55610000199999));
#304847=CARTESIAN_POINT('Ctrl Pts',(-2.92110676400006,2.2,3.55610000199999));
#304848=CARTESIAN_POINT('Ctrl Pts',(-2.92070064000006,12.2,3.55370812899999));
#304849=CARTESIAN_POINT('Ctrl Pts',(-2.92070064000006,5.2,3.55370812899999));
#304850=CARTESIAN_POINT('Ctrl Pts',(-2.92070064000006,2.2,3.55370812899999));
#304851=CARTESIAN_POINT('Ctrl Pts',(-2.92029258400006,12.2,3.55132024499999));
#304852=CARTESIAN_POINT('Ctrl Pts',(-2.92029258400006,5.2,3.55132024499999));
#304853=CARTESIAN_POINT('Ctrl Pts',(-2.92029258400006,2.2,3.55132024499999));
#304854=CARTESIAN_POINT('Ctrl Pts',(-2.91988260200006,12.2,3.54893635699998));
#304855=CARTESIAN_POINT('Ctrl Pts',(-2.91988260200006,5.2,3.54893635699998));
#304856=CARTESIAN_POINT('Ctrl Pts',(-2.91988260200006,2.2,3.54893635699998));
#304857=CARTESIAN_POINT('Ctrl Pts',(-2.91947070300006,12.2,3.54655646799999));
#304858=CARTESIAN_POINT('Ctrl Pts',(-2.91947070300006,5.2,3.54655646799999));
#304859=CARTESIAN_POINT('Ctrl Pts',(-2.91947070300006,2.2,3.54655646799999));
#304860=CARTESIAN_POINT('Ctrl Pts',(-2.91905689500005,12.2,3.54418058299999));
#304861=CARTESIAN_POINT('Ctrl Pts',(-2.91905689500005,5.2,3.54418058299999));
#304862=CARTESIAN_POINT('Ctrl Pts',(-2.91905689500005,2.2,3.54418058299999));
#304863=CARTESIAN_POINT('Ctrl Pts',(-2.91864118600006,12.2,3.54180870899999));
#304864=CARTESIAN_POINT('Ctrl Pts',(-2.91864118600006,5.2,3.54180870899999));
#304865=CARTESIAN_POINT('Ctrl Pts',(-2.91864118600006,2.2,3.54180870899999));
#304866=CARTESIAN_POINT('Ctrl Pts',(-2.91822358300006,12.2,3.53944084999998));
#304867=CARTESIAN_POINT('Ctrl Pts',(-2.91822358300006,5.2,3.53944084999998));
#304868=CARTESIAN_POINT('Ctrl Pts',(-2.91822358300006,2.2,3.53944084999998));
#304869=CARTESIAN_POINT('Ctrl Pts',(-2.91780409400006,12.2,3.53707701099999));
#304870=CARTESIAN_POINT('Ctrl Pts',(-2.91780409400006,5.2,3.53707701099999));
#304871=CARTESIAN_POINT('Ctrl Pts',(-2.91780409400006,2.2,3.53707701099999));
#304872=CARTESIAN_POINT('Ctrl Pts',(-2.91738272700006,12.2,3.53471719699999));
#304873=CARTESIAN_POINT('Ctrl Pts',(-2.91738272700006,5.2,3.53471719699999));
#304874=CARTESIAN_POINT('Ctrl Pts',(-2.91738272700006,2.2,3.53471719699999));
#304875=CARTESIAN_POINT('Ctrl Pts',(-2.91695948900006,12.2,3.53236141499998));
#304876=CARTESIAN_POINT('Ctrl Pts',(-2.91695948900006,5.2,3.53236141499998));
#304877=CARTESIAN_POINT('Ctrl Pts',(-2.91695948900006,2.2,3.53236141499998));
#304878=CARTESIAN_POINT('Ctrl Pts',(-2.91653438800005,12.2,3.53000966899998));
#304879=CARTESIAN_POINT('Ctrl Pts',(-2.91653438800005,5.2,3.53000966899998));
#304880=CARTESIAN_POINT('Ctrl Pts',(-2.91653438800005,2.2,3.53000966899998));
#304881=CARTESIAN_POINT('Ctrl Pts',(-2.91610743300006,12.2,3.52766196299999));
#304882=CARTESIAN_POINT('Ctrl Pts',(-2.91610743300006,5.2,3.52766196299999));
#304883=CARTESIAN_POINT('Ctrl Pts',(-2.91610743300006,2.2,3.52766196299999));
#304884=CARTESIAN_POINT('Ctrl Pts',(-2.91567863100005,12.2,3.52531830299998));
#304885=CARTESIAN_POINT('Ctrl Pts',(-2.91567863100005,5.2,3.52531830299998));
#304886=CARTESIAN_POINT('Ctrl Pts',(-2.91567863100005,2.2,3.52531830299998));
#304887=CARTESIAN_POINT('Ctrl Pts',(-2.91524799000006,12.2,3.52297869399998));
#304888=CARTESIAN_POINT('Ctrl Pts',(-2.91524799000006,5.2,3.52297869399998));
#304889=CARTESIAN_POINT('Ctrl Pts',(-2.91524799000006,2.2,3.52297869399998));
#304890=CARTESIAN_POINT('Ctrl Pts',(-2.91481551900006,12.2,3.52064314199998));
#304891=CARTESIAN_POINT('Ctrl Pts',(-2.91481551900006,5.2,3.52064314199998));
#304892=CARTESIAN_POINT('Ctrl Pts',(-2.91481551900006,2.2,3.52064314199998));
#304893=CARTESIAN_POINT('Ctrl Pts',(-2.91438122300006,12.2,3.51831165199999));
#304894=CARTESIAN_POINT('Ctrl Pts',(-2.91438122300006,5.2,3.51831165199999));
#304895=CARTESIAN_POINT('Ctrl Pts',(-2.91438122300006,2.2,3.51831165199999));
#304896=CARTESIAN_POINT('Ctrl Pts',(-2.91394511400005,12.2,3.51598422799999));
#304897=CARTESIAN_POINT('Ctrl Pts',(-2.91394511400005,5.2,3.51598422799999));
#304898=CARTESIAN_POINT('Ctrl Pts',(-2.91394511400005,2.2,3.51598422799999));
#304899=CARTESIAN_POINT('Ctrl Pts',(-2.91350719600006,12.2,3.51366087699999));
#304900=CARTESIAN_POINT('Ctrl Pts',(-2.91350719600006,5.2,3.51366087699999));
#304901=CARTESIAN_POINT('Ctrl Pts',(-2.91350719600006,2.2,3.51366087699999));
#304902=CARTESIAN_POINT('Ctrl Pts',(-2.91306748000005,12.2,3.51134160099999));
#304903=CARTESIAN_POINT('Ctrl Pts',(-2.91306748000005,5.2,3.51134160099999));
#304904=CARTESIAN_POINT('Ctrl Pts',(-2.91306748000005,2.2,3.51134160099999));
#304905=CARTESIAN_POINT('Ctrl Pts',(-2.91262597100005,12.2,3.50902640899999));
#304906=CARTESIAN_POINT('Ctrl Pts',(-2.91262597100005,5.2,3.50902640899999));
#304907=CARTESIAN_POINT('Ctrl Pts',(-2.91262597100005,2.2,3.50902640899999));
#304908=CARTESIAN_POINT('Ctrl Pts',(-2.91218268100006,12.2,3.50671530299999));
#304909=CARTESIAN_POINT('Ctrl Pts',(-2.91218268100006,5.2,3.50671530299999));
#304910=CARTESIAN_POINT('Ctrl Pts',(-2.91218268100006,2.2,3.50671530299999));
#304911=CARTESIAN_POINT('Ctrl Pts',(-2.91173761400006,12.2,3.50440828999999));
#304912=CARTESIAN_POINT('Ctrl Pts',(-2.91173761400006,5.2,3.50440828999999));
#304913=CARTESIAN_POINT('Ctrl Pts',(-2.91173761400006,2.2,3.50440828999999));
#304914=CARTESIAN_POINT('Ctrl Pts',(-2.91129078100006,12.2,3.50210537399998));
#304915=CARTESIAN_POINT('Ctrl Pts',(-2.91129078100006,5.2,3.50210537399998));
#304916=CARTESIAN_POINT('Ctrl Pts',(-2.91129078100006,2.2,3.50210537399998));
#304917=CARTESIAN_POINT('Ctrl Pts',(-2.91084218900005,12.2,3.49980655999998));
#304918=CARTESIAN_POINT('Ctrl Pts',(-2.91084218900005,5.2,3.49980655999998));
#304919=CARTESIAN_POINT('Ctrl Pts',(-2.91084218900005,2.2,3.49980655999998));
#304920=CARTESIAN_POINT('Ctrl Pts',(-2.91039184500006,12.2,3.49751185399998));
#304921=CARTESIAN_POINT('Ctrl Pts',(-2.91039184500006,5.2,3.49751185399998));
#304922=CARTESIAN_POINT('Ctrl Pts',(-2.91039184500006,2.2,3.49751185399998));
#304923=CARTESIAN_POINT('Ctrl Pts',(-2.90993975900005,12.2,3.49522126099998));
#304924=CARTESIAN_POINT('Ctrl Pts',(-2.90993975900005,5.2,3.49522126099998));
#304925=CARTESIAN_POINT('Ctrl Pts',(-2.90993975900005,2.2,3.49522126099998));
#304926=CARTESIAN_POINT('Ctrl Pts',(-2.90948593800006,12.2,3.49293478699998));
#304927=CARTESIAN_POINT('Ctrl Pts',(-2.90948593800006,5.2,3.49293478699998));
#304928=CARTESIAN_POINT('Ctrl Pts',(-2.90948593800006,2.2,3.49293478699998));
#304929=CARTESIAN_POINT('Ctrl Pts',(-2.90903039100006,12.2,3.49065243299999));
#304930=CARTESIAN_POINT('Ctrl Pts',(-2.90903039100006,5.2,3.49065243299999));
#304931=CARTESIAN_POINT('Ctrl Pts',(-2.90903039100006,2.2,3.49065243299999));
#304932=CARTESIAN_POINT('Ctrl Pts',(-2.90857312500005,12.2,3.48837420999998));
#304933=CARTESIAN_POINT('Ctrl Pts',(-2.90857312500005,5.2,3.48837420999998));
#304934=CARTESIAN_POINT('Ctrl Pts',(-2.90857312500005,2.2,3.48837420999998));
#304935=CARTESIAN_POINT('Ctrl Pts',(-2.90811414800006,12.2,3.48610011899999));
#304936=CARTESIAN_POINT('Ctrl Pts',(-2.90811414800006,5.2,3.48610011899999));
#304937=CARTESIAN_POINT('Ctrl Pts',(-2.90811414800006,2.2,3.48610011899999));
#304938=CARTESIAN_POINT('Ctrl Pts',(-2.90765347000006,12.2,3.48383016499999));
#304939=CARTESIAN_POINT('Ctrl Pts',(-2.90765347000006,5.2,3.48383016499999));
#304940=CARTESIAN_POINT('Ctrl Pts',(-2.90765347000006,2.2,3.48383016499999));
#304941=CARTESIAN_POINT('Ctrl Pts',(-2.90719109800006,12.2,3.48156435399999));
#304942=CARTESIAN_POINT('Ctrl Pts',(-2.90719109800006,5.2,3.48156435399999));
#304943=CARTESIAN_POINT('Ctrl Pts',(-2.90719109800006,2.2,3.48156435399999));
#304944=CARTESIAN_POINT('Ctrl Pts',(-2.90672704000006,12.2,3.47930269299999));
#304945=CARTESIAN_POINT('Ctrl Pts',(-2.90672704000006,5.2,3.47930269299999));
#304946=CARTESIAN_POINT('Ctrl Pts',(-2.90672704000006,2.2,3.47930269299999));
#304947=CARTESIAN_POINT('Ctrl Pts',(-2.90626130400006,12.2,3.47704518499998));
#304948=CARTESIAN_POINT('Ctrl Pts',(-2.90626130400006,5.2,3.47704518499998));
#304949=CARTESIAN_POINT('Ctrl Pts',(-2.90626130400006,2.2,3.47704518499998));
#304950=CARTESIAN_POINT('Ctrl Pts',(-2.90579390000006,12.2,3.47479183399999));
#304951=CARTESIAN_POINT('Ctrl Pts',(-2.90579390000006,5.2,3.47479183399999));
#304952=CARTESIAN_POINT('Ctrl Pts',(-2.90579390000006,2.2,3.47479183399999));
#304953=CARTESIAN_POINT('Ctrl Pts',(-2.90532483500006,12.2,3.47254264799999));
#304954=CARTESIAN_POINT('Ctrl Pts',(-2.90532483500006,5.2,3.47254264799999));
#304955=CARTESIAN_POINT('Ctrl Pts',(-2.90532483500006,2.2,3.47254264799999));
#304956=CARTESIAN_POINT('Ctrl Pts',(-2.90485411700006,12.2,3.47029762999998));
#304957=CARTESIAN_POINT('Ctrl Pts',(-2.90485411700006,5.2,3.47029762999998));
#304958=CARTESIAN_POINT('Ctrl Pts',(-2.90485411700006,2.2,3.47029762999998));
#304959=CARTESIAN_POINT('Ctrl Pts',(-2.90438175500006,12.2,3.46805678499998));
#304960=CARTESIAN_POINT('Ctrl Pts',(-2.90438175500006,5.2,3.46805678499998));
#304961=CARTESIAN_POINT('Ctrl Pts',(-2.90438175500006,2.2,3.46805678499998));
#304962=CARTESIAN_POINT('Ctrl Pts',(-2.90390775600006,12.2,3.46582011999998));
#304963=CARTESIAN_POINT('Ctrl Pts',(-2.90390775600006,5.2,3.46582011999998));
#304964=CARTESIAN_POINT('Ctrl Pts',(-2.90390775600006,2.2,3.46582011999998));
#304965=CARTESIAN_POINT('Ctrl Pts',(-2.90343213100006,12.2,3.46358763699998));
#304966=CARTESIAN_POINT('Ctrl Pts',(-2.90343213100006,5.2,3.46358763699998));
#304967=CARTESIAN_POINT('Ctrl Pts',(-2.90343213100006,2.2,3.46358763699998));
#304968=CARTESIAN_POINT('Ctrl Pts',(-2.90295488600006,12.2,3.46135934399998));
#304969=CARTESIAN_POINT('Ctrl Pts',(-2.90295488600006,5.2,3.46135934399998));
#304970=CARTESIAN_POINT('Ctrl Pts',(-2.90295488600006,2.2,3.46135934399998));
#304971=CARTESIAN_POINT('Ctrl Pts',(-2.90247603100006,12.2,3.45913524399998));
#304972=CARTESIAN_POINT('Ctrl Pts',(-2.90247603100006,5.2,3.45913524399998));
#304973=CARTESIAN_POINT('Ctrl Pts',(-2.90247603100006,2.2,3.45913524399998));
#304974=CARTESIAN_POINT('Ctrl Pts',(-2.90199557400005,12.2,3.45691534299998));
#304975=CARTESIAN_POINT('Ctrl Pts',(-2.90199557400005,5.2,3.45691534299998));
#304976=CARTESIAN_POINT('Ctrl Pts',(-2.90199557400005,2.2,3.45691534299998));
#304977=CARTESIAN_POINT('Ctrl Pts',(-2.90151352200006,12.2,3.45469964499999));
#304978=CARTESIAN_POINT('Ctrl Pts',(-2.90151352200006,5.2,3.45469964499999));
#304979=CARTESIAN_POINT('Ctrl Pts',(-2.90151352200006,2.2,3.45469964499999));
#304980=CARTESIAN_POINT('Ctrl Pts',(-2.90102988400006,12.2,3.45248815599999));
#304981=CARTESIAN_POINT('Ctrl Pts',(-2.90102988400006,5.2,3.45248815599999));
#304982=CARTESIAN_POINT('Ctrl Pts',(-2.90102988400006,2.2,3.45248815599999));
#304983=CARTESIAN_POINT('Ctrl Pts',(-2.90054467100005,12.2,3.45028088099999));
#304984=CARTESIAN_POINT('Ctrl Pts',(-2.90054467100005,5.2,3.45028088099999));
#304985=CARTESIAN_POINT('Ctrl Pts',(-2.90054467100005,2.2,3.45028088099999));
#304986=CARTESIAN_POINT('Ctrl Pts',(-2.90005788800006,12.2,3.44807782499998));
#304987=CARTESIAN_POINT('Ctrl Pts',(-2.90005788800006,5.2,3.44807782499998));
#304988=CARTESIAN_POINT('Ctrl Pts',(-2.90005788800006,2.2,3.44807782499998));
#304989=CARTESIAN_POINT('Ctrl Pts',(-2.89956954600005,12.2,3.44587899199999));
#304990=CARTESIAN_POINT('Ctrl Pts',(-2.89956954600005,5.2,3.44587899199999));
#304991=CARTESIAN_POINT('Ctrl Pts',(-2.89956954600005,2.2,3.44587899199999));
#304992=CARTESIAN_POINT('Ctrl Pts',(-2.89907965200006,12.2,3.44368438899998));
#304993=CARTESIAN_POINT('Ctrl Pts',(-2.89907965200006,5.2,3.44368438899998));
#304994=CARTESIAN_POINT('Ctrl Pts',(-2.89907965200006,2.2,3.44368438899998));
#304995=CARTESIAN_POINT('Ctrl Pts',(-2.89858821500005,12.2,3.44149401799999));
#304996=CARTESIAN_POINT('Ctrl Pts',(-2.89858821500005,5.2,3.44149401799999));
#304997=CARTESIAN_POINT('Ctrl Pts',(-2.89858821500005,2.2,3.44149401799999));
#304998=CARTESIAN_POINT('Ctrl Pts',(-2.89809524300006,12.2,3.43930788699998));
#304999=CARTESIAN_POINT('Ctrl Pts',(-2.89809524300006,5.2,3.43930788699998));
#305000=CARTESIAN_POINT('Ctrl Pts',(-2.89809524300006,2.2,3.43930788699998));
#305001=CARTESIAN_POINT('Ctrl Pts',(-2.89760074700005,12.2,3.43712599899998));
#305002=CARTESIAN_POINT('Ctrl Pts',(-2.89760074700005,5.2,3.43712599899998));
#305003=CARTESIAN_POINT('Ctrl Pts',(-2.89760074700005,2.2,3.43712599899998));
#305004=CARTESIAN_POINT('Ctrl Pts',(-2.89710473200006,12.2,3.43494835999999));
#305005=CARTESIAN_POINT('Ctrl Pts',(-2.89710473200006,5.2,3.43494835999999));
#305006=CARTESIAN_POINT('Ctrl Pts',(-2.89710473200006,2.2,3.43494835999999));
#305007=CARTESIAN_POINT('Ctrl Pts',(-2.89660720900006,12.2,3.43277497499999));
#305008=CARTESIAN_POINT('Ctrl Pts',(-2.89660720900006,5.2,3.43277497499999));
#305009=CARTESIAN_POINT('Ctrl Pts',(-2.89660720900006,2.2,3.43277497499999));
#305010=CARTESIAN_POINT('Ctrl Pts',(-2.89610818700006,12.2,3.43060584799999));
#305011=CARTESIAN_POINT('Ctrl Pts',(-2.89610818700006,5.2,3.43060584799999));
#305012=CARTESIAN_POINT('Ctrl Pts',(-2.89610818700006,2.2,3.43060584799999));
#305013=CARTESIAN_POINT('Ctrl Pts',(-2.89560767300005,12.2,3.42844098499998));
#305014=CARTESIAN_POINT('Ctrl Pts',(-2.89560767300005,5.2,3.42844098499998));
#305015=CARTESIAN_POINT('Ctrl Pts',(-2.89560767300005,2.2,3.42844098499998));
#305016=CARTESIAN_POINT('Ctrl Pts',(-2.89510567700006,12.2,3.42628038999998));
#305017=CARTESIAN_POINT('Ctrl Pts',(-2.89510567700006,5.2,3.42628038999998));
#305018=CARTESIAN_POINT('Ctrl Pts',(-2.89510567700006,2.2,3.42628038999998));
#305019=CARTESIAN_POINT('Ctrl Pts',(-2.89460220700006,12.2,3.42412406899999));
#305020=CARTESIAN_POINT('Ctrl Pts',(-2.89460220700006,5.2,3.42412406899999));
#305021=CARTESIAN_POINT('Ctrl Pts',(-2.89460220700006,2.2,3.42412406899999));
#305022=CARTESIAN_POINT('Ctrl Pts',(-2.89409727200006,12.2,3.42197202599999));
#305023=CARTESIAN_POINT('Ctrl Pts',(-2.89409727200006,5.2,3.42197202599999));
#305024=CARTESIAN_POINT('Ctrl Pts',(-2.89409727200006,2.2,3.42197202599999));
#305025=CARTESIAN_POINT('Ctrl Pts',(-2.89359087900006,12.2,3.41982426699998));
#305026=CARTESIAN_POINT('Ctrl Pts',(-2.89359087900006,5.2,3.41982426699998));
#305027=CARTESIAN_POINT('Ctrl Pts',(-2.89359087900006,2.2,3.41982426699998));
#305028=CARTESIAN_POINT('Ctrl Pts',(-2.89308304000006,12.2,3.41768079499998));
#305029=CARTESIAN_POINT('Ctrl Pts',(-2.89308304000006,5.2,3.41768079499998));
#305030=CARTESIAN_POINT('Ctrl Pts',(-2.89308304000006,2.2,3.41768079499998));
#305031=CARTESIAN_POINT('Ctrl Pts',(-2.89257376100006,12.2,3.41554161799999));
#305032=CARTESIAN_POINT('Ctrl Pts',(-2.89257376100006,5.2,3.41554161799999));
#305033=CARTESIAN_POINT('Ctrl Pts',(-2.89257376100006,2.2,3.41554161799999));
#305034=CARTESIAN_POINT('Ctrl Pts',(-2.89206305300006,12.2,3.41340673799999));
#305035=CARTESIAN_POINT('Ctrl Pts',(-2.89206305300006,5.2,3.41340673799999));
#305036=CARTESIAN_POINT('Ctrl Pts',(-2.89206305300006,2.2,3.41340673799999));
#305037=CARTESIAN_POINT('Ctrl Pts',(-2.89155092300006,12.2,3.41127616099998));
#305038=CARTESIAN_POINT('Ctrl Pts',(-2.89155092300006,5.2,3.41127616099998));
#305039=CARTESIAN_POINT('Ctrl Pts',(-2.89155092300006,2.2,3.41127616099998));
#305040=CARTESIAN_POINT('Ctrl Pts',(-2.89103738100006,12.2,3.40914989399998));
#305041=CARTESIAN_POINT('Ctrl Pts',(-2.89103738100006,5.2,3.40914989399998));
#305042=CARTESIAN_POINT('Ctrl Pts',(-2.89103738100006,2.2,3.40914989399998));
#305043=CARTESIAN_POINT('Ctrl Pts',(-2.89052243500006,12.2,3.40702793799998));
#305044=CARTESIAN_POINT('Ctrl Pts',(-2.89052243500006,5.2,3.40702793799998));
#305045=CARTESIAN_POINT('Ctrl Pts',(-2.89052243500006,2.2,3.40702793799998));
#305046=CARTESIAN_POINT('Ctrl Pts',(-2.89000609500006,12.2,3.40491029899999));
#305047=CARTESIAN_POINT('Ctrl Pts',(-2.89000609500006,5.2,3.40491029899999));
#305048=CARTESIAN_POINT('Ctrl Pts',(-2.89000609500006,2.2,3.40491029899999));
#305049=CARTESIAN_POINT('Ctrl Pts',(-2.88948836900006,12.2,3.40279698399998));
#305050=CARTESIAN_POINT('Ctrl Pts',(-2.88948836900006,5.2,3.40279698399998));
#305051=CARTESIAN_POINT('Ctrl Pts',(-2.88948836900006,2.2,3.40279698399998));
#305052=CARTESIAN_POINT('Ctrl Pts',(-2.88896926500006,12.2,3.40068799699999));
#305053=CARTESIAN_POINT('Ctrl Pts',(-2.88896926500006,5.2,3.40068799699999));
#305054=CARTESIAN_POINT('Ctrl Pts',(-2.88896926500006,2.2,3.40068799699999));
#305055=CARTESIAN_POINT('Ctrl Pts',(-2.88844879500005,12.2,3.39858334199998));
#305056=CARTESIAN_POINT('Ctrl Pts',(-2.88844879500005,5.2,3.39858334199998));
#305057=CARTESIAN_POINT('Ctrl Pts',(-2.88844879500005,2.2,3.39858334199998));
#305058=CARTESIAN_POINT('Ctrl Pts',(-2.88792696500006,12.2,3.39648302499998));
#305059=CARTESIAN_POINT('Ctrl Pts',(-2.88792696500006,5.2,3.39648302499998));
#305060=CARTESIAN_POINT('Ctrl Pts',(-2.88792696500006,2.2,3.39648302499998));
#305061=CARTESIAN_POINT('Ctrl Pts',(-2.88740378400006,12.2,3.39438704899998));
#305062=CARTESIAN_POINT('Ctrl Pts',(-2.88740378400006,5.2,3.39438704899998));
#305063=CARTESIAN_POINT('Ctrl Pts',(-2.88740378400006,2.2,3.39438704899998));
#305064=CARTESIAN_POINT('Ctrl Pts',(-2.88687926300006,12.2,3.39229542199998));
#305065=CARTESIAN_POINT('Ctrl Pts',(-2.88687926300006,5.2,3.39229542199998));
#305066=CARTESIAN_POINT('Ctrl Pts',(-2.88687926300006,2.2,3.39229542199998));
#305067=CARTESIAN_POINT('Ctrl Pts',(-2.88635341000006,12.2,3.39020814599999));
#305068=CARTESIAN_POINT('Ctrl Pts',(-2.88635341000006,5.2,3.39020814599999));
#305069=CARTESIAN_POINT('Ctrl Pts',(-2.88635341000006,2.2,3.39020814599999));
#305070=CARTESIAN_POINT('Ctrl Pts',(-2.88582623400006,12.2,3.38812522599999));
#305071=CARTESIAN_POINT('Ctrl Pts',(-2.88582623400006,5.2,3.38812522599999));
#305072=CARTESIAN_POINT('Ctrl Pts',(-2.88582623400006,2.2,3.38812522599999));
#305073=CARTESIAN_POINT('Ctrl Pts',(-2.88529774300006,12.2,3.38604666899998));
#305074=CARTESIAN_POINT('Ctrl Pts',(-2.88529774300006,5.2,3.38604666899998));
#305075=CARTESIAN_POINT('Ctrl Pts',(-2.88529774300006,2.2,3.38604666899998));
#305076=CARTESIAN_POINT('Ctrl Pts',(-2.88476794800005,12.2,3.38397247899999));
#305077=CARTESIAN_POINT('Ctrl Pts',(-2.88476794800005,5.2,3.38397247899999));
#305078=CARTESIAN_POINT('Ctrl Pts',(-2.88476794800005,2.2,3.38397247899999));
#305079=CARTESIAN_POINT('Ctrl Pts',(-2.88423685700006,12.2,3.38190265899998));
#305080=CARTESIAN_POINT('Ctrl Pts',(-2.88423685700006,5.2,3.38190265899998));
#305081=CARTESIAN_POINT('Ctrl Pts',(-2.88423685700006,2.2,3.38190265899998));
#305082=CARTESIAN_POINT('Ctrl Pts',(-2.88370448000005,12.2,3.37983721699998));
#305083=CARTESIAN_POINT('Ctrl Pts',(-2.88370448000005,5.2,3.37983721699998));
#305084=CARTESIAN_POINT('Ctrl Pts',(-2.88370448000005,2.2,3.37983721699998));
#305085=CARTESIAN_POINT('Ctrl Pts',(-2.88317082500006,12.2,3.37777615499999));
#305086=CARTESIAN_POINT('Ctrl Pts',(-2.88317082500006,5.2,3.37777615499999));
#305087=CARTESIAN_POINT('Ctrl Pts',(-2.88317082500006,2.2,3.37777615499999));
#305088=CARTESIAN_POINT('Ctrl Pts',(-2.88263590100006,12.2,3.37571947899999));
#305089=CARTESIAN_POINT('Ctrl Pts',(-2.88263590100006,5.2,3.37571947899999));
#305090=CARTESIAN_POINT('Ctrl Pts',(-2.88263590100006,2.2,3.37571947899999));
#305091=CARTESIAN_POINT('Ctrl Pts',(-2.88209971800006,12.2,3.37366719499999));
#305092=CARTESIAN_POINT('Ctrl Pts',(-2.88209971800006,5.2,3.37366719499999));
#305093=CARTESIAN_POINT('Ctrl Pts',(-2.88209971800006,2.2,3.37366719499999));
#305094=CARTESIAN_POINT('Ctrl Pts',(-2.88156228600006,12.2,3.37161930599999));
#305095=CARTESIAN_POINT('Ctrl Pts',(-2.88156228600006,5.2,3.37161930599999));
#305096=CARTESIAN_POINT('Ctrl Pts',(-2.88156228600006,2.2,3.37161930599999));
#305097=CARTESIAN_POINT('Ctrl Pts',(-2.88102361300006,12.2,3.36957581699998));
#305098=CARTESIAN_POINT('Ctrl Pts',(-2.88102361300006,5.2,3.36957581699998));
#305099=CARTESIAN_POINT('Ctrl Pts',(-2.88102361300006,2.2,3.36957581699998));
#305100=CARTESIAN_POINT('Ctrl Pts',(-2.88048370700006,12.2,3.36753673399999));
#305101=CARTESIAN_POINT('Ctrl Pts',(-2.88048370700006,5.2,3.36753673399999));
#305102=CARTESIAN_POINT('Ctrl Pts',(-2.88048370700006,2.2,3.36753673399999));
#305103=CARTESIAN_POINT('Ctrl Pts',(-2.87994257900006,12.2,3.36550206099999));
#305104=CARTESIAN_POINT('Ctrl Pts',(-2.87994257900006,5.2,3.36550206099999));
#305105=CARTESIAN_POINT('Ctrl Pts',(-2.87994257900006,2.2,3.36550206099999));
#305106=CARTESIAN_POINT('Ctrl Pts',(-2.87940023900005,12.2,3.36347180199999));
#305107=CARTESIAN_POINT('Ctrl Pts',(-2.87940023900005,5.2,3.36347180199999));
#305108=CARTESIAN_POINT('Ctrl Pts',(-2.87940023900005,2.2,3.36347180199999));
#305109=CARTESIAN_POINT('Ctrl Pts',(-2.87885669500006,12.2,3.36144596399999));
#305110=CARTESIAN_POINT('Ctrl Pts',(-2.87885669500006,5.2,3.36144596399999));
#305111=CARTESIAN_POINT('Ctrl Pts',(-2.87885669500006,2.2,3.36144596399999));
#305112=CARTESIAN_POINT('Ctrl Pts',(-2.87831195600006,12.2,3.35942454999999));
#305113=CARTESIAN_POINT('Ctrl Pts',(-2.87831195600006,5.2,3.35942454999999));
#305114=CARTESIAN_POINT('Ctrl Pts',(-2.87831195600006,2.2,3.35942454999999));
#305115=CARTESIAN_POINT('Ctrl Pts',(-2.87776603200005,12.2,3.35740756499998));
#305116=CARTESIAN_POINT('Ctrl Pts',(-2.87776603200005,5.2,3.35740756499998));
#305117=CARTESIAN_POINT('Ctrl Pts',(-2.87776603200005,2.2,3.35740756499998));
#305118=CARTESIAN_POINT('Ctrl Pts',(-2.87721893300006,12.2,3.35539501399998));
#305119=CARTESIAN_POINT('Ctrl Pts',(-2.87721893300006,5.2,3.35539501399998));
#305120=CARTESIAN_POINT('Ctrl Pts',(-2.87721893300006,2.2,3.35539501399998));
#305121=CARTESIAN_POINT('Ctrl Pts',(-2.87667066700006,12.2,3.35338690199999));
#305122=CARTESIAN_POINT('Ctrl Pts',(-2.87667066700006,5.2,3.35338690199999));
#305123=CARTESIAN_POINT('Ctrl Pts',(-2.87667066700006,2.2,3.35338690199999));
#305124=CARTESIAN_POINT('Ctrl Pts',(-2.87612124500006,12.2,3.35138323399998));
#305125=CARTESIAN_POINT('Ctrl Pts',(-2.87612124500006,5.2,3.35138323399998));
#305126=CARTESIAN_POINT('Ctrl Pts',(-2.87612124500006,2.2,3.35138323399998));
#305127=CARTESIAN_POINT('Ctrl Pts',(-2.87557067400006,12.2,3.34938401399998));
#305128=CARTESIAN_POINT('Ctrl Pts',(-2.87557067400006,5.2,3.34938401399998));
#305129=CARTESIAN_POINT('Ctrl Pts',(-2.87557067400006,2.2,3.34938401399998));
#305130=CARTESIAN_POINT('Ctrl Pts',(-2.87501896500005,12.2,3.34738924799999));
#305131=CARTESIAN_POINT('Ctrl Pts',(-2.87501896500005,5.2,3.34738924799999));
#305132=CARTESIAN_POINT('Ctrl Pts',(-2.87501896500005,2.2,3.34738924799999));
#305133=CARTESIAN_POINT('Ctrl Pts',(-2.87446612800006,12.2,3.34539893899999));
#305134=CARTESIAN_POINT('Ctrl Pts',(-2.87446612800006,5.2,3.34539893899999));
#305135=CARTESIAN_POINT('Ctrl Pts',(-2.87446612800006,2.2,3.34539893899999));
#305136=CARTESIAN_POINT('Ctrl Pts',(-2.87391217200006,12.2,3.34341309299998));
#305137=CARTESIAN_POINT('Ctrl Pts',(-2.87391217200006,5.2,3.34341309299998));
#305138=CARTESIAN_POINT('Ctrl Pts',(-2.87391217200006,2.2,3.34341309299998));
#305139=CARTESIAN_POINT('Ctrl Pts',(-2.87335710600006,12.2,3.34143171399998));
#305140=CARTESIAN_POINT('Ctrl Pts',(-2.87335710600006,5.2,3.34143171399998));
#305141=CARTESIAN_POINT('Ctrl Pts',(-2.87335710600006,2.2,3.34143171399998));
#305142=CARTESIAN_POINT('Ctrl Pts',(-2.87280094100006,12.2,3.33945480699998));
#305143=CARTESIAN_POINT('Ctrl Pts',(-2.87280094100006,5.2,3.33945480699998));
#305144=CARTESIAN_POINT('Ctrl Pts',(-2.87280094100006,2.2,3.33945480699998));
#305145=CARTESIAN_POINT('Ctrl Pts',(-2.87224368400006,12.2,3.33748237699999));
#305146=CARTESIAN_POINT('Ctrl Pts',(-2.87224368400006,5.2,3.33748237699999));
#305147=CARTESIAN_POINT('Ctrl Pts',(-2.87224368400006,2.2,3.33748237699999));
#305148=CARTESIAN_POINT('Ctrl Pts',(-2.87168534700006,12.2,3.33551442899999));
#305149=CARTESIAN_POINT('Ctrl Pts',(-2.87168534700006,5.2,3.33551442899999));
#305150=CARTESIAN_POINT('Ctrl Pts',(-2.87168534700006,2.2,3.33551442899999));
#305151=CARTESIAN_POINT('Ctrl Pts',(-2.87112593900006,12.2,3.33355096799998));
#305152=CARTESIAN_POINT('Ctrl Pts',(-2.87112593900006,5.2,3.33355096799998));
#305153=CARTESIAN_POINT('Ctrl Pts',(-2.87112593900006,2.2,3.33355096799998));
#305154=CARTESIAN_POINT('Ctrl Pts',(-2.87056546800006,12.2,3.33159199699999));
#305155=CARTESIAN_POINT('Ctrl Pts',(-2.87056546800006,5.2,3.33159199699999));
#305156=CARTESIAN_POINT('Ctrl Pts',(-2.87056546800006,2.2,3.33159199699999));
#305157=CARTESIAN_POINT('Ctrl Pts',(-2.87000394500006,12.2,3.32963752199999));
#305158=CARTESIAN_POINT('Ctrl Pts',(-2.87000394500006,5.2,3.32963752199999));
#305159=CARTESIAN_POINT('Ctrl Pts',(-2.87000394500006,2.2,3.32963752199999));
#305160=CARTESIAN_POINT('Ctrl Pts',(-2.86944138000006,12.2,3.32768754699998));
#305161=CARTESIAN_POINT('Ctrl Pts',(-2.86944138000006,5.2,3.32768754699998));
#305162=CARTESIAN_POINT('Ctrl Pts',(-2.86944138000006,2.2,3.32768754699998));
#305163=CARTESIAN_POINT('Ctrl Pts',(-2.86887778300006,12.2,3.32574207799999));
#305164=CARTESIAN_POINT('Ctrl Pts',(-2.86887778300006,5.2,3.32574207799999));
#305165=CARTESIAN_POINT('Ctrl Pts',(-2.86887778300006,2.2,3.32574207799999));
#305166=CARTESIAN_POINT('Ctrl Pts',(-2.86831316100006,12.2,3.32380111699998));
#305167=CARTESIAN_POINT('Ctrl Pts',(-2.86831316100006,5.2,3.32380111699998));
#305168=CARTESIAN_POINT('Ctrl Pts',(-2.86831316100006,2.2,3.32380111699998));
#305169=CARTESIAN_POINT('Ctrl Pts',(-2.86774752600006,12.2,3.32186467299999));
#305170=CARTESIAN_POINT('Ctrl Pts',(-2.86774752600006,5.2,3.32186467299999));
#305171=CARTESIAN_POINT('Ctrl Pts',(-2.86774752600006,2.2,3.32186467299999));
#305172=CARTESIAN_POINT('Ctrl Pts',(-2.86718088800006,12.2,3.31993274599999));
#305173=CARTESIAN_POINT('Ctrl Pts',(-2.86718088800006,5.2,3.31993274599999));
#305174=CARTESIAN_POINT('Ctrl Pts',(-2.86718088800006,2.2,3.31993274599999));
#305175=CARTESIAN_POINT('Ctrl Pts',(-2.86661325600006,12.2,3.31800534399999));
#305176=CARTESIAN_POINT('Ctrl Pts',(-2.86661325600006,5.2,3.31800534399999));
#305177=CARTESIAN_POINT('Ctrl Pts',(-2.86661325600006,2.2,3.31800534399999));
#305178=CARTESIAN_POINT('Ctrl Pts',(-2.86604464000006,12.2,3.31608247099999));
#305179=CARTESIAN_POINT('Ctrl Pts',(-2.86604464000006,5.2,3.31608247099999));
#305180=CARTESIAN_POINT('Ctrl Pts',(-2.86604464000006,2.2,3.31608247099999));
#305181=CARTESIAN_POINT('Ctrl Pts',(-2.86547505000006,12.2,3.31416412999998));
#305182=CARTESIAN_POINT('Ctrl Pts',(-2.86547505000006,5.2,3.31416412999998));
#305183=CARTESIAN_POINT('Ctrl Pts',(-2.86547505000006,2.2,3.31416412999998));
#305184=CARTESIAN_POINT('Ctrl Pts',(-2.86490449600006,12.2,3.31225032799999));
#305185=CARTESIAN_POINT('Ctrl Pts',(-2.86490449600006,5.2,3.31225032799999));
#305186=CARTESIAN_POINT('Ctrl Pts',(-2.86490449600006,2.2,3.31225032799999));
#305187=CARTESIAN_POINT('Ctrl Pts',(-2.86433298600006,12.2,3.31034106699998));
#305188=CARTESIAN_POINT('Ctrl Pts',(-2.86433298600006,5.2,3.31034106699998));
#305189=CARTESIAN_POINT('Ctrl Pts',(-2.86433298600006,2.2,3.31034106699998));
#305190=CARTESIAN_POINT('Ctrl Pts',(-2.86376053200006,12.2,3.30843635499999));
#305191=CARTESIAN_POINT('Ctrl Pts',(-2.86376053200006,5.2,3.30843635499999));
#305192=CARTESIAN_POINT('Ctrl Pts',(-2.86376053200006,2.2,3.30843635499999));
#305193=CARTESIAN_POINT('Ctrl Pts',(-2.86318714300006,12.2,3.30653619399998));
#305194=CARTESIAN_POINT('Ctrl Pts',(-2.86318714300006,5.2,3.30653619399998));
#305195=CARTESIAN_POINT('Ctrl Pts',(-2.86318714300006,2.2,3.30653619399998));
#305196=CARTESIAN_POINT('Ctrl Pts',(-2.86261282900006,12.2,3.30464058799999));
#305197=CARTESIAN_POINT('Ctrl Pts',(-2.86261282900006,5.2,3.30464058799999));
#305198=CARTESIAN_POINT('Ctrl Pts',(-2.86261282900006,2.2,3.30464058799999));
#305199=CARTESIAN_POINT('Ctrl Pts',(-2.86203760000005,12.2,3.30274954499998));
#305200=CARTESIAN_POINT('Ctrl Pts',(-2.86203760000005,5.2,3.30274954499998));
#305201=CARTESIAN_POINT('Ctrl Pts',(-2.86203760000005,2.2,3.30274954499998));
#305202=CARTESIAN_POINT('Ctrl Pts',(-2.86146146600006,12.2,3.30086306599998));
#305203=CARTESIAN_POINT('Ctrl Pts',(-2.86146146600006,5.2,3.30086306599998));
#305204=CARTESIAN_POINT('Ctrl Pts',(-2.86146146600006,2.2,3.30086306599998));
#305205=CARTESIAN_POINT('Ctrl Pts',(-2.86088443800006,12.2,3.29898115899999));
#305206=CARTESIAN_POINT('Ctrl Pts',(-2.86088443800006,5.2,3.29898115899999));
#305207=CARTESIAN_POINT('Ctrl Pts',(-2.86088443800006,2.2,3.29898115899999));
#305208=CARTESIAN_POINT('Ctrl Pts',(-2.86030652300005,12.2,3.29710382599998));
#305209=CARTESIAN_POINT('Ctrl Pts',(-2.86030652300005,5.2,3.29710382599998));
#305210=CARTESIAN_POINT('Ctrl Pts',(-2.86030652300005,2.2,3.29710382599998));
#305211=CARTESIAN_POINT('Ctrl Pts',(-2.85972773500006,12.2,3.29523107299998));
#305212=CARTESIAN_POINT('Ctrl Pts',(-2.85972773500006,5.2,3.29523107299998));
#305213=CARTESIAN_POINT('Ctrl Pts',(-2.85972773500006,2.2,3.29523107299998));
#305214=CARTESIAN_POINT('Ctrl Pts',(-2.85914808100005,12.2,3.29336290299998));
#305215=CARTESIAN_POINT('Ctrl Pts',(-2.85914808100005,5.2,3.29336290299998));
#305216=CARTESIAN_POINT('Ctrl Pts',(-2.85914808100005,2.2,3.29336290299998));
#305217=CARTESIAN_POINT('Ctrl Pts',(-2.85856757300006,12.2,3.29149932199999));
#305218=CARTESIAN_POINT('Ctrl Pts',(-2.85856757300006,5.2,3.29149932199999));
#305219=CARTESIAN_POINT('Ctrl Pts',(-2.85856757300006,2.2,3.29149932199999));
#305220=CARTESIAN_POINT('Ctrl Pts',(-2.85798621900006,12.2,3.28964033399998));
#305221=CARTESIAN_POINT('Ctrl Pts',(-2.85798621900006,5.2,3.28964033399998));
#305222=CARTESIAN_POINT('Ctrl Pts',(-2.85798621900006,2.2,3.28964033399998));
#305223=CARTESIAN_POINT('Ctrl Pts',(-2.85740403200006,12.2,3.28778594499998));
#305224=CARTESIAN_POINT('Ctrl Pts',(-2.85740403200006,5.2,3.28778594499998));
#305225=CARTESIAN_POINT('Ctrl Pts',(-2.85740403200006,2.2,3.28778594499998));
#305226=CARTESIAN_POINT('Ctrl Pts',(-2.85682101900006,12.2,3.28593615699998));
#305227=CARTESIAN_POINT('Ctrl Pts',(-2.85682101900006,5.2,3.28593615699998));
#305228=CARTESIAN_POINT('Ctrl Pts',(-2.85682101900006,2.2,3.28593615699998));
#305229=CARTESIAN_POINT('Ctrl Pts',(-2.85623719200006,12.2,3.28409097699998));
#305230=CARTESIAN_POINT('Ctrl Pts',(-2.85623719200006,5.2,3.28409097699998));
#305231=CARTESIAN_POINT('Ctrl Pts',(-2.85623719200006,2.2,3.28409097699998));
#305232=CARTESIAN_POINT('Ctrl Pts',(-2.85565256200006,12.2,3.28225040699999));
#305233=CARTESIAN_POINT('Ctrl Pts',(-2.85565256200006,5.2,3.28225040699999));
#305234=CARTESIAN_POINT('Ctrl Pts',(-2.85565256200006,2.2,3.28225040699999));
#305235=CARTESIAN_POINT('Ctrl Pts',(-2.85506713700005,12.2,3.28041445499998));
#305236=CARTESIAN_POINT('Ctrl Pts',(-2.85506713700005,5.2,3.28041445499998));
#305237=CARTESIAN_POINT('Ctrl Pts',(-2.85506713700005,2.2,3.28041445499998));
#305238=CARTESIAN_POINT('Ctrl Pts',(-2.85448092800006,12.2,3.27858312199999));
#305239=CARTESIAN_POINT('Ctrl Pts',(-2.85448092800006,5.2,3.27858312199999));
#305240=CARTESIAN_POINT('Ctrl Pts',(-2.85448092800006,2.2,3.27858312199999));
#305241=CARTESIAN_POINT('Ctrl Pts',(-2.85389394600006,12.2,3.27675641499999));
#305242=CARTESIAN_POINT('Ctrl Pts',(-2.85389394600006,5.2,3.27675641499999));
#305243=CARTESIAN_POINT('Ctrl Pts',(-2.85389394600006,2.2,3.27675641499999));
#305244=CARTESIAN_POINT('Ctrl Pts',(-2.85330620200006,12.2,3.27493433699999));
#305245=CARTESIAN_POINT('Ctrl Pts',(-2.85330620200006,5.2,3.27493433699999));
#305246=CARTESIAN_POINT('Ctrl Pts',(-2.85330620200006,2.2,3.27493433699999));
#305247=CARTESIAN_POINT('Ctrl Pts',(-2.85271770300006,12.2,3.27311689299999));
#305248=CARTESIAN_POINT('Ctrl Pts',(-2.85271770300006,5.2,3.27311689299999));
#305249=CARTESIAN_POINT('Ctrl Pts',(-2.85271770300006,2.2,3.27311689299999));
#305250=CARTESIAN_POINT('Ctrl Pts',(-2.85212846300006,12.2,3.27130408899999));
#305251=CARTESIAN_POINT('Ctrl Pts',(-2.85212846300006,5.2,3.27130408899999));
#305252=CARTESIAN_POINT('Ctrl Pts',(-2.85212846300006,2.2,3.27130408899999));
#305253=CARTESIAN_POINT('Ctrl Pts',(-2.85153849100006,12.2,3.26949592699999));
#305254=CARTESIAN_POINT('Ctrl Pts',(-2.85153849100006,5.2,3.26949592699999));
#305255=CARTESIAN_POINT('Ctrl Pts',(-2.85153849100006,2.2,3.26949592699999));
#305256=CARTESIAN_POINT('Ctrl Pts',(-2.85094779600006,12.2,3.26769241299999));
#305257=CARTESIAN_POINT('Ctrl Pts',(-2.85094779600006,5.2,3.26769241299999));
#305258=CARTESIAN_POINT('Ctrl Pts',(-2.85094779600006,2.2,3.26769241299999));
#305259=CARTESIAN_POINT('Ctrl Pts',(-2.85035639200005,12.2,3.26589355199999));
#305260=CARTESIAN_POINT('Ctrl Pts',(-2.85035639200005,5.2,3.26589355199999));
#305261=CARTESIAN_POINT('Ctrl Pts',(-2.85035639200005,2.2,3.26589355199999));
#305262=CARTESIAN_POINT('Ctrl Pts',(-2.84976428500006,12.2,3.26409934599998));
#305263=CARTESIAN_POINT('Ctrl Pts',(-2.84976428500006,5.2,3.26409934599998));
#305264=CARTESIAN_POINT('Ctrl Pts',(-2.84976428500006,2.2,3.26409934599998));
#305265=CARTESIAN_POINT('Ctrl Pts',(-2.84917148800006,12.2,3.26230980199998));
#305266=CARTESIAN_POINT('Ctrl Pts',(-2.84917148800006,5.2,3.26230980199998));
#305267=CARTESIAN_POINT('Ctrl Pts',(-2.84917148800006,2.2,3.26230980199998));
#305268=CARTESIAN_POINT('Ctrl Pts',(-2.84857801100005,12.2,3.26052492399998));
#305269=CARTESIAN_POINT('Ctrl Pts',(-2.84857801100005,5.2,3.26052492399998));
#305270=CARTESIAN_POINT('Ctrl Pts',(-2.84857801100005,2.2,3.26052492399998));
#305271=CARTESIAN_POINT('Ctrl Pts',(-2.84798386500006,12.2,3.25874471599998));
#305272=CARTESIAN_POINT('Ctrl Pts',(-2.84798386500006,5.2,3.25874471599998));
#305273=CARTESIAN_POINT('Ctrl Pts',(-2.84798386500006,2.2,3.25874471599998));
#305274=CARTESIAN_POINT('Ctrl Pts',(-2.84738906000006,12.2,3.25696918299998));
#305275=CARTESIAN_POINT('Ctrl Pts',(-2.84738906000006,5.2,3.25696918299998));
#305276=CARTESIAN_POINT('Ctrl Pts',(-2.84738906000006,2.2,3.25696918299998));
#305277=CARTESIAN_POINT('Ctrl Pts',(-2.84679360500005,12.2,3.25519832899998));
#305278=CARTESIAN_POINT('Ctrl Pts',(-2.84679360500005,5.2,3.25519832899998));
#305279=CARTESIAN_POINT('Ctrl Pts',(-2.84679360500005,2.2,3.25519832899998));
#305280=CARTESIAN_POINT('Ctrl Pts',(-2.84619751300006,12.2,3.25343215699998));
#305281=CARTESIAN_POINT('Ctrl Pts',(-2.84619751300006,5.2,3.25343215699998));
#305282=CARTESIAN_POINT('Ctrl Pts',(-2.84619751300006,2.2,3.25343215699998));
#305283=CARTESIAN_POINT('Ctrl Pts',(-2.84560079400006,12.2,3.25167067399998));
#305284=CARTESIAN_POINT('Ctrl Pts',(-2.84560079400006,5.2,3.25167067399998));
#305285=CARTESIAN_POINT('Ctrl Pts',(-2.84560079400006,2.2,3.25167067399998));
#305286=CARTESIAN_POINT('Ctrl Pts',(-2.84500345900006,12.2,3.24991388399998));
#305287=CARTESIAN_POINT('Ctrl Pts',(-2.84500345900006,5.2,3.24991388399998));
#305288=CARTESIAN_POINT('Ctrl Pts',(-2.84500345900006,2.2,3.24991388399998));
#305289=CARTESIAN_POINT('Ctrl Pts',(-2.84440551700006,12.2,3.24816178999999));
#305290=CARTESIAN_POINT('Ctrl Pts',(-2.84440551700006,5.2,3.24816178999999));
#305291=CARTESIAN_POINT('Ctrl Pts',(-2.84440551700006,2.2,3.24816178999999));
#305292=CARTESIAN_POINT('Ctrl Pts',(-2.84380697900006,12.2,3.24641439699998));
#305293=CARTESIAN_POINT('Ctrl Pts',(-2.84380697900006,5.2,3.24641439699998));
#305294=CARTESIAN_POINT('Ctrl Pts',(-2.84380697900006,2.2,3.24641439699998));
#305295=CARTESIAN_POINT('Ctrl Pts',(-2.84320785800006,12.2,3.24467170999998));
#305296=CARTESIAN_POINT('Ctrl Pts',(-2.84320785800006,5.2,3.24467170999998));
#305297=CARTESIAN_POINT('Ctrl Pts',(-2.84320785800006,2.2,3.24467170999998));
#305298=CARTESIAN_POINT('Ctrl Pts',(-2.84260816200006,12.2,3.24293373299999));
#305299=CARTESIAN_POINT('Ctrl Pts',(-2.84260816200006,5.2,3.24293373299999));
#305300=CARTESIAN_POINT('Ctrl Pts',(-2.84260816200006,2.2,3.24293373299999));
#305301=CARTESIAN_POINT('Ctrl Pts',(-2.84200790300006,12.2,3.24120046999998));
#305302=CARTESIAN_POINT('Ctrl Pts',(-2.84200790300006,5.2,3.24120046999998));
#305303=CARTESIAN_POINT('Ctrl Pts',(-2.84200790300006,2.2,3.24120046999998));
#305304=CARTESIAN_POINT('Ctrl Pts',(-2.84140709100006,12.2,3.23947192599999));
#305305=CARTESIAN_POINT('Ctrl Pts',(-2.84140709100006,5.2,3.23947192599999));
#305306=CARTESIAN_POINT('Ctrl Pts',(-2.84140709100006,2.2,3.23947192599999));
#305307=CARTESIAN_POINT('Ctrl Pts',(-2.84080573800006,12.2,3.23774810599998));
#305308=CARTESIAN_POINT('Ctrl Pts',(-2.84080573800006,5.2,3.23774810599998));
#305309=CARTESIAN_POINT('Ctrl Pts',(-2.84080573800006,2.2,3.23774810599998));
#305310=CARTESIAN_POINT('Ctrl Pts',(-2.84020385300006,12.2,3.23602901199998));
#305311=CARTESIAN_POINT('Ctrl Pts',(-2.84020385300006,5.2,3.23602901199998));
#305312=CARTESIAN_POINT('Ctrl Pts',(-2.84020385300006,2.2,3.23602901199998));
#305313=CARTESIAN_POINT('Ctrl Pts',(-2.83960144900006,12.2,3.23431465199998));
#305314=CARTESIAN_POINT('Ctrl Pts',(-2.83960144900006,5.2,3.23431465199998));
#305315=CARTESIAN_POINT('Ctrl Pts',(-2.83960144900006,2.2,3.23431465199998));
#305316=CARTESIAN_POINT('Ctrl Pts',(-2.83899853600006,12.2,3.23260502699998));
#305317=CARTESIAN_POINT('Ctrl Pts',(-2.83899853600006,5.2,3.23260502699998));
#305318=CARTESIAN_POINT('Ctrl Pts',(-2.83899853600006,2.2,3.23260502699998));
#305319=CARTESIAN_POINT('Ctrl Pts',(-2.83839512400006,12.2,3.23090014199998));
#305320=CARTESIAN_POINT('Ctrl Pts',(-2.83839512400006,5.2,3.23090014199998));
#305321=CARTESIAN_POINT('Ctrl Pts',(-2.83839512400006,2.2,3.23090014199998));
#305322=CARTESIAN_POINT('Ctrl Pts',(-2.83779122500006,12.2,3.22920000399999));
#305323=CARTESIAN_POINT('Ctrl Pts',(-2.83779122500006,5.2,3.22920000399999));
#305324=CARTESIAN_POINT('Ctrl Pts',(-2.83779122500006,2.2,3.22920000399999));
#305325=CARTESIAN_POINT('Ctrl Pts',(-2.83718684900006,12.2,3.22750461399998));
#305326=CARTESIAN_POINT('Ctrl Pts',(-2.83718684900006,5.2,3.22750461399998));
#305327=CARTESIAN_POINT('Ctrl Pts',(-2.83718684900006,2.2,3.22750461399998));
#305328=CARTESIAN_POINT('Ctrl Pts',(-2.83658200700006,12.2,3.22581397899998));
#305329=CARTESIAN_POINT('Ctrl Pts',(-2.83658200700006,5.2,3.22581397899998));
#305330=CARTESIAN_POINT('Ctrl Pts',(-2.83658200700006,2.2,3.22581397899998));
#305331=CARTESIAN_POINT('Ctrl Pts',(-2.83597671200006,12.2,3.22412810099999));
#305332=CARTESIAN_POINT('Ctrl Pts',(-2.83597671200006,5.2,3.22412810099999));
#305333=CARTESIAN_POINT('Ctrl Pts',(-2.83597671200006,2.2,3.22412810099999));
#305334=CARTESIAN_POINT('Ctrl Pts',(-2.83537097200006,12.2,3.22244698499999));
#305335=CARTESIAN_POINT('Ctrl Pts',(-2.83537097200006,5.2,3.22244698499999));
#305336=CARTESIAN_POINT('Ctrl Pts',(-2.83537097200006,2.2,3.22244698499999));
#305337=CARTESIAN_POINT('Ctrl Pts',(-2.83476480100005,12.2,3.22077063699999));
#305338=CARTESIAN_POINT('Ctrl Pts',(-2.83476480100005,5.2,3.22077063699999));
#305339=CARTESIAN_POINT('Ctrl Pts',(-2.83476480100005,2.2,3.22077063699999));
#305340=CARTESIAN_POINT('Ctrl Pts',(-2.83415820700006,12.2,3.21909905899999));
#305341=CARTESIAN_POINT('Ctrl Pts',(-2.83415820700006,5.2,3.21909905899999));
#305342=CARTESIAN_POINT('Ctrl Pts',(-2.83415820700006,2.2,3.21909905899999));
#305343=CARTESIAN_POINT('Ctrl Pts',(-2.83355120500006,12.2,3.21743225699999));
#305344=CARTESIAN_POINT('Ctrl Pts',(-2.83355120500006,5.2,3.21743225699999));
#305345=CARTESIAN_POINT('Ctrl Pts',(-2.83355120500006,2.2,3.21743225699999));
#305346=CARTESIAN_POINT('Ctrl Pts',(-2.83294380200006,12.2,3.21577023399998));
#305347=CARTESIAN_POINT('Ctrl Pts',(-2.83294380200006,5.2,3.21577023399998));
#305348=CARTESIAN_POINT('Ctrl Pts',(-2.83294380200006,2.2,3.21577023399998));
#305349=CARTESIAN_POINT('Ctrl Pts',(-2.83233601100005,12.2,3.21411299499999));
#305350=CARTESIAN_POINT('Ctrl Pts',(-2.83233601100005,5.2,3.21411299499999));
#305351=CARTESIAN_POINT('Ctrl Pts',(-2.83233601100005,2.2,3.21411299499999));
#305352=CARTESIAN_POINT('Ctrl Pts',(-2.83172784300006,12.2,3.21246054399998));
#305353=CARTESIAN_POINT('Ctrl Pts',(-2.83172784300006,5.2,3.21246054399998));
#305354=CARTESIAN_POINT('Ctrl Pts',(-2.83172784300006,2.2,3.21246054399998));
#305355=CARTESIAN_POINT('Ctrl Pts',(-2.83111930900006,12.2,3.21081288599999));
#305356=CARTESIAN_POINT('Ctrl Pts',(-2.83111930900006,5.2,3.21081288599999));
#305357=CARTESIAN_POINT('Ctrl Pts',(-2.83111930900006,2.2,3.21081288599999));
#305358=CARTESIAN_POINT('Ctrl Pts',(-2.83051042200006,12.2,3.20917002399998));
#305359=CARTESIAN_POINT('Ctrl Pts',(-2.83051042200006,5.2,3.20917002399998));
#305360=CARTESIAN_POINT('Ctrl Pts',(-2.83051042200006,2.2,3.20917002399998));
#305361=CARTESIAN_POINT('Ctrl Pts',(-2.82990119000006,12.2,3.20753196299999));
#305362=CARTESIAN_POINT('Ctrl Pts',(-2.82990119000006,5.2,3.20753196299999));
#305363=CARTESIAN_POINT('Ctrl Pts',(-2.82990119000006,2.2,3.20753196299999));
#305364=CARTESIAN_POINT('Ctrl Pts',(-2.82929162700006,12.2,3.20589870799999));
#305365=CARTESIAN_POINT('Ctrl Pts',(-2.82929162700006,5.2,3.20589870799999));
#305366=CARTESIAN_POINT('Ctrl Pts',(-2.82929162700006,2.2,3.20589870799999));
#305367=CARTESIAN_POINT('Ctrl Pts',(-2.82868174300006,12.2,3.20427026199999));
#305368=CARTESIAN_POINT('Ctrl Pts',(-2.82868174300006,5.2,3.20427026199999));
#305369=CARTESIAN_POINT('Ctrl Pts',(-2.82868174300006,2.2,3.20427026199999));
#305370=CARTESIAN_POINT('Ctrl Pts',(-2.82807155000006,12.2,3.20264662899999));
#305371=CARTESIAN_POINT('Ctrl Pts',(-2.82807155000006,5.2,3.20264662899999));
#305372=CARTESIAN_POINT('Ctrl Pts',(-2.82807155000006,2.2,3.20264662899999));
#305373=CARTESIAN_POINT('Ctrl Pts',(-2.82746105800005,12.2,3.20102781399999));
#305374=CARTESIAN_POINT('Ctrl Pts',(-2.82746105800005,5.2,3.20102781399999));
#305375=CARTESIAN_POINT('Ctrl Pts',(-2.82746105800005,2.2,3.20102781399999));
#305376=CARTESIAN_POINT('Ctrl Pts',(-2.82685028000006,12.2,3.19941382199998));
#305377=CARTESIAN_POINT('Ctrl Pts',(-2.82685028000006,5.2,3.19941382199998));
#305378=CARTESIAN_POINT('Ctrl Pts',(-2.82685028000006,2.2,3.19941382199998));
#305379=CARTESIAN_POINT('Ctrl Pts',(-2.82623922700005,12.2,3.19780465599998));
#305380=CARTESIAN_POINT('Ctrl Pts',(-2.82623922700005,5.2,3.19780465599998));
#305381=CARTESIAN_POINT('Ctrl Pts',(-2.82623922700005,2.2,3.19780465599998));
#305382=CARTESIAN_POINT('Ctrl Pts',(-2.82562791000006,12.2,3.19620032099999));
#305383=CARTESIAN_POINT('Ctrl Pts',(-2.82562791000006,5.2,3.19620032099999));
#305384=CARTESIAN_POINT('Ctrl Pts',(-2.82562791000006,2.2,3.19620032099999));
#305385=CARTESIAN_POINT('Ctrl Pts',(-2.82501634000006,12.2,3.19460081899998));
#305386=CARTESIAN_POINT('Ctrl Pts',(-2.82501634000006,5.2,3.19460081899998));
#305387=CARTESIAN_POINT('Ctrl Pts',(-2.82501634000006,2.2,3.19460081899998));
#305388=CARTESIAN_POINT('Ctrl Pts',(-2.82440452900006,12.2,3.19300615799998));
#305389=CARTESIAN_POINT('Ctrl Pts',(-2.82440452900006,5.2,3.19300615799998));
#305390=CARTESIAN_POINT('Ctrl Pts',(-2.82440452900006,2.2,3.19300615799998));
#305391=CARTESIAN_POINT('Ctrl Pts',(-2.82379248900006,12.2,3.19141633799998));
#305392=CARTESIAN_POINT('Ctrl Pts',(-2.82379248900006,5.2,3.19141633799998));
#305393=CARTESIAN_POINT('Ctrl Pts',(-2.82379248900006,2.2,3.19141633799998));
#305394=CARTESIAN_POINT('Ctrl Pts',(-2.82318023000005,12.2,3.18983136699998));
#305395=CARTESIAN_POINT('Ctrl Pts',(-2.82318023000005,5.2,3.18983136699998));
#305396=CARTESIAN_POINT('Ctrl Pts',(-2.82318023000005,2.2,3.18983136699998));
#305397=CARTESIAN_POINT('Ctrl Pts',(-2.82256776600006,12.2,3.18825124699998));
#305398=CARTESIAN_POINT('Ctrl Pts',(-2.82256776600006,5.2,3.18825124699998));
#305399=CARTESIAN_POINT('Ctrl Pts',(-2.82256776600006,2.2,3.18825124699998));
#305400=CARTESIAN_POINT('Ctrl Pts',(-2.82195510700006,12.2,3.18667598099999));
#305401=CARTESIAN_POINT('Ctrl Pts',(-2.82195510700006,5.2,3.18667598099999));
#305402=CARTESIAN_POINT('Ctrl Pts',(-2.82195510700006,2.2,3.18667598099999));
#305403=CARTESIAN_POINT('Ctrl Pts',(-2.82134226500005,12.2,3.18510557699998));
#305404=CARTESIAN_POINT('Ctrl Pts',(-2.82134226500005,5.2,3.18510557699998));
#305405=CARTESIAN_POINT('Ctrl Pts',(-2.82134226500005,2.2,3.18510557699998));
#305406=CARTESIAN_POINT('Ctrl Pts',(-2.82072925100006,12.2,3.18354003499999));
#305407=CARTESIAN_POINT('Ctrl Pts',(-2.82072925100006,5.2,3.18354003499999));
#305408=CARTESIAN_POINT('Ctrl Pts',(-2.82072925100006,2.2,3.18354003499999));
#305409=CARTESIAN_POINT('Ctrl Pts',(-2.82011607700006,12.2,3.18197936199999));
#305410=CARTESIAN_POINT('Ctrl Pts',(-2.82011607700006,5.2,3.18197936199999));
#305411=CARTESIAN_POINT('Ctrl Pts',(-2.82011607700006,2.2,3.18197936199999));
#305412=CARTESIAN_POINT('Ctrl Pts',(-2.81950275500006,12.2,3.18042356099999));
#305413=CARTESIAN_POINT('Ctrl Pts',(-2.81950275500006,5.2,3.18042356099999));
#305414=CARTESIAN_POINT('Ctrl Pts',(-2.81950275500006,2.2,3.18042356099999));
#305415=CARTESIAN_POINT('Ctrl Pts',(-2.81888929700005,12.2,3.17887263499999));
#305416=CARTESIAN_POINT('Ctrl Pts',(-2.81888929700005,5.2,3.17887263499999));
#305417=CARTESIAN_POINT('Ctrl Pts',(-2.81888929700005,2.2,3.17887263499999));
#305418=CARTESIAN_POINT('Ctrl Pts',(-2.81827571400005,12.2,3.17732658999999));
#305419=CARTESIAN_POINT('Ctrl Pts',(-2.81827571400005,5.2,3.17732658999999));
#305420=CARTESIAN_POINT('Ctrl Pts',(-2.81827571400005,2.2,3.17732658999999));
#305421=CARTESIAN_POINT('Ctrl Pts',(-2.81766201800006,12.2,3.17578542999998));
#305422=CARTESIAN_POINT('Ctrl Pts',(-2.81766201800006,5.2,3.17578542999998));
#305423=CARTESIAN_POINT('Ctrl Pts',(-2.81766201800006,2.2,3.17578542999998));
#305424=CARTESIAN_POINT('Ctrl Pts',(-2.81704822000005,12.2,3.17424915799998));
#305425=CARTESIAN_POINT('Ctrl Pts',(-2.81704822000005,5.2,3.17424915799998));
#305426=CARTESIAN_POINT('Ctrl Pts',(-2.81704822000005,2.2,3.17424915799998));
#305427=CARTESIAN_POINT('Ctrl Pts',(-2.81643433500005,12.2,3.17271777899998));
#305428=CARTESIAN_POINT('Ctrl Pts',(-2.81643433500005,5.2,3.17271777899998));
#305429=CARTESIAN_POINT('Ctrl Pts',(-2.81643433500005,2.2,3.17271777899998));
#305430=CARTESIAN_POINT('Ctrl Pts',(-2.81582037000006,12.2,3.17119129599998));
#305431=CARTESIAN_POINT('Ctrl Pts',(-2.81582037000006,5.2,3.17119129599998));
#305432=CARTESIAN_POINT('Ctrl Pts',(-2.81582037000006,2.2,3.17119129599998));
#305433=CARTESIAN_POINT('Ctrl Pts',(-2.81520634200006,12.2,3.16966971399999));
#305434=CARTESIAN_POINT('Ctrl Pts',(-2.81520634200006,5.2,3.16966971399999));
#305435=CARTESIAN_POINT('Ctrl Pts',(-2.81520634200006,2.2,3.16966971399999));
#305436=CARTESIAN_POINT('Ctrl Pts',(-2.81459225800006,12.2,3.16815303599999));
#305437=CARTESIAN_POINT('Ctrl Pts',(-2.81459225800006,5.2,3.16815303599999));
#305438=CARTESIAN_POINT('Ctrl Pts',(-2.81459225800006,2.2,3.16815303599999));
#305439=CARTESIAN_POINT('Ctrl Pts',(-2.81397813400006,12.2,3.16664126899998));
#305440=CARTESIAN_POINT('Ctrl Pts',(-2.81397813400006,5.2,3.16664126899998));
#305441=CARTESIAN_POINT('Ctrl Pts',(-2.81397813400006,2.2,3.16664126899998));
#305442=CARTESIAN_POINT('Ctrl Pts',(-2.81336398000006,12.2,3.16513441199999));
#305443=CARTESIAN_POINT('Ctrl Pts',(-2.81336398000006,5.2,3.16513441199999));
#305444=CARTESIAN_POINT('Ctrl Pts',(-2.81336398000006,2.2,3.16513441199999));
#305445=CARTESIAN_POINT('Ctrl Pts',(-2.81274980700006,12.2,3.16363247299999));
#305446=CARTESIAN_POINT('Ctrl Pts',(-2.81274980700006,5.2,3.16363247299999));
#305447=CARTESIAN_POINT('Ctrl Pts',(-2.81274980700006,2.2,3.16363247299999));
#305448=CARTESIAN_POINT('Ctrl Pts',(-2.81213563000006,12.2,3.16213545599999));
#305449=CARTESIAN_POINT('Ctrl Pts',(-2.81213563000006,5.2,3.16213545599999));
#305450=CARTESIAN_POINT('Ctrl Pts',(-2.81213563000006,2.2,3.16213545599999));
#305451=CARTESIAN_POINT('Ctrl Pts',(-2.81152145800006,12.2,3.16064336299998));
#305452=CARTESIAN_POINT('Ctrl Pts',(-2.81152145800006,5.2,3.16064336299998));
#305453=CARTESIAN_POINT('Ctrl Pts',(-2.81152145800006,2.2,3.16064336299998));
#305454=CARTESIAN_POINT('Ctrl Pts',(-2.81090730500006,12.2,3.15915619899998));
#305455=CARTESIAN_POINT('Ctrl Pts',(-2.81090730500006,5.2,3.15915619899998));
#305456=CARTESIAN_POINT('Ctrl Pts',(-2.81090730500006,2.2,3.15915619899998));
#305457=CARTESIAN_POINT('Ctrl Pts',(-2.81029318300006,12.2,3.15767396799998));
#305458=CARTESIAN_POINT('Ctrl Pts',(-2.81029318300006,5.2,3.15767396799998));
#305459=CARTESIAN_POINT('Ctrl Pts',(-2.81029318300006,2.2,3.15767396799998));
#305460=CARTESIAN_POINT('Ctrl Pts',(-2.80967910300005,12.2,3.15619667399999));
#305461=CARTESIAN_POINT('Ctrl Pts',(-2.80967910300005,5.2,3.15619667399999));
#305462=CARTESIAN_POINT('Ctrl Pts',(-2.80967910300005,2.2,3.15619667399999));
#305463=CARTESIAN_POINT('Ctrl Pts',(-2.80906507800006,12.2,3.15472431999999));
#305464=CARTESIAN_POINT('Ctrl Pts',(-2.80906507800006,5.2,3.15472431999999));
#305465=CARTESIAN_POINT('Ctrl Pts',(-2.80906507800006,2.2,3.15472431999999));
#305466=CARTESIAN_POINT('Ctrl Pts',(-2.80845112000006,12.2,3.15325691099999));
#305467=CARTESIAN_POINT('Ctrl Pts',(-2.80845112000006,5.2,3.15325691099999));
#305468=CARTESIAN_POINT('Ctrl Pts',(-2.80845112000006,2.2,3.15325691099999));
#305469=CARTESIAN_POINT('Ctrl Pts',(-2.80783724200006,12.2,3.15179445199998));
#305470=CARTESIAN_POINT('Ctrl Pts',(-2.80783724200006,5.2,3.15179445199998));
#305471=CARTESIAN_POINT('Ctrl Pts',(-2.80783724200006,2.2,3.15179445199998));
#305472=CARTESIAN_POINT('Ctrl Pts',(-2.80722345500005,12.2,3.15033694399999));
#305473=CARTESIAN_POINT('Ctrl Pts',(-2.80722345500005,5.2,3.15033694399999));
#305474=CARTESIAN_POINT('Ctrl Pts',(-2.80722345500005,2.2,3.15033694399999));
#305475=CARTESIAN_POINT('Ctrl Pts',(-2.80660977100006,12.2,3.14888439299998));
#305476=CARTESIAN_POINT('Ctrl Pts',(-2.80660977100006,5.2,3.14888439299998));
#305477=CARTESIAN_POINT('Ctrl Pts',(-2.80660977100006,2.2,3.14888439299998));
#305478=CARTESIAN_POINT('Ctrl Pts',(-2.80599620400006,12.2,3.14743680399998));
#305479=CARTESIAN_POINT('Ctrl Pts',(-2.80599620400006,5.2,3.14743680399998));
#305480=CARTESIAN_POINT('Ctrl Pts',(-2.80599620400006,2.2,3.14743680399998));
#305481=CARTESIAN_POINT('Ctrl Pts',(-2.80538276500006,12.2,3.14599417899998));
#305482=CARTESIAN_POINT('Ctrl Pts',(-2.80538276500006,5.2,3.14599417899998));
#305483=CARTESIAN_POINT('Ctrl Pts',(-2.80538276500006,2.2,3.14599417899998));
#305484=CARTESIAN_POINT('Ctrl Pts',(-2.80476946700006,12.2,3.14455652199998));
#305485=CARTESIAN_POINT('Ctrl Pts',(-2.80476946700006,5.2,3.14455652199998));
#305486=CARTESIAN_POINT('Ctrl Pts',(-2.80476946700006,2.2,3.14455652199998));
#305487=CARTESIAN_POINT('Ctrl Pts',(-2.80415632300006,12.2,3.14312383699999));
#305488=CARTESIAN_POINT('Ctrl Pts',(-2.80415632300006,5.2,3.14312383699999));
#305489=CARTESIAN_POINT('Ctrl Pts',(-2.80415632300006,2.2,3.14312383699999));
#305490=CARTESIAN_POINT('Ctrl Pts',(-2.80354334400006,12.2,3.14169612899998));
#305491=CARTESIAN_POINT('Ctrl Pts',(-2.80354334400006,5.2,3.14169612899998));
#305492=CARTESIAN_POINT('Ctrl Pts',(-2.80354334400006,2.2,3.14169612899998));
#305493=CARTESIAN_POINT('Ctrl Pts',(-2.80293054400006,12.2,3.14027340099998));
#305494=CARTESIAN_POINT('Ctrl Pts',(-2.80293054400006,5.2,3.14027340099998));
#305495=CARTESIAN_POINT('Ctrl Pts',(-2.80293054400006,2.2,3.14027340099998));
#305496=CARTESIAN_POINT('Ctrl Pts',(-2.80231793300006,12.2,3.13885565799998));
#305497=CARTESIAN_POINT('Ctrl Pts',(-2.80231793300006,5.2,3.13885565799998));
#305498=CARTESIAN_POINT('Ctrl Pts',(-2.80231793300006,2.2,3.13885565799998));
#305499=CARTESIAN_POINT('Ctrl Pts',(-2.80170552700006,12.2,3.13744290199998));
#305500=CARTESIAN_POINT('Ctrl Pts',(-2.80170552700006,5.2,3.13744290199998));
#305501=CARTESIAN_POINT('Ctrl Pts',(-2.80170552700006,2.2,3.13744290199998));
#305502=CARTESIAN_POINT('Ctrl Pts',(-2.80109333500006,12.2,3.13603513699999));
#305503=CARTESIAN_POINT('Ctrl Pts',(-2.80109333500006,5.2,3.13603513699999));
#305504=CARTESIAN_POINT('Ctrl Pts',(-2.80109333500006,2.2,3.13603513699999));
#305505=CARTESIAN_POINT('Ctrl Pts',(-2.80048137300006,12.2,3.13463236799999));
#305506=CARTESIAN_POINT('Ctrl Pts',(-2.80048137300006,5.2,3.13463236799999));
#305507=CARTESIAN_POINT('Ctrl Pts',(-2.80048137300006,2.2,3.13463236799999));
#305508=CARTESIAN_POINT('Ctrl Pts',(-2.79986965000006,12.2,3.13323459799999));
#305509=CARTESIAN_POINT('Ctrl Pts',(-2.79986965000006,5.2,3.13323459799999));
#305510=CARTESIAN_POINT('Ctrl Pts',(-2.79986965000006,2.2,3.13323459799999));
#305511=CARTESIAN_POINT('Ctrl Pts',(-2.79925818200006,12.2,3.13184183299998));
#305512=CARTESIAN_POINT('Ctrl Pts',(-2.79925818200006,5.2,3.13184183299998));
#305513=CARTESIAN_POINT('Ctrl Pts',(-2.79925818200006,2.2,3.13184183299998));
#305514=CARTESIAN_POINT('Ctrl Pts',(-2.79864698000006,12.2,3.13045407399999));
#305515=CARTESIAN_POINT('Ctrl Pts',(-2.79864698000006,5.2,3.13045407399999));
#305516=CARTESIAN_POINT('Ctrl Pts',(-2.79864698000006,2.2,3.13045407399999));
#305517=CARTESIAN_POINT('Ctrl Pts',(-2.79803605600006,12.2,3.12907132599998));
#305518=CARTESIAN_POINT('Ctrl Pts',(-2.79803605600006,5.2,3.12907132599998));
#305519=CARTESIAN_POINT('Ctrl Pts',(-2.79803605600006,2.2,3.12907132599998));
#305520=CARTESIAN_POINT('Ctrl Pts',(-2.79742542500005,12.2,3.12769359199999));
#305521=CARTESIAN_POINT('Ctrl Pts',(-2.79742542500005,5.2,3.12769359199999));
#305522=CARTESIAN_POINT('Ctrl Pts',(-2.79742542500005,2.2,3.12769359199999));
#305523=CARTESIAN_POINT('Ctrl Pts',(-2.79681509700006,12.2,3.12632087799999));
#305524=CARTESIAN_POINT('Ctrl Pts',(-2.79681509700006,5.2,3.12632087799999));
#305525=CARTESIAN_POINT('Ctrl Pts',(-2.79681509700006,2.2,3.12632087799999));
#305526=CARTESIAN_POINT('Ctrl Pts',(-2.79620508700006,12.2,3.12495318599999));
#305527=CARTESIAN_POINT('Ctrl Pts',(-2.79620508700006,5.2,3.12495318599999));
#305528=CARTESIAN_POINT('Ctrl Pts',(-2.79620508700006,2.2,3.12495318599999));
#305529=CARTESIAN_POINT('Ctrl Pts',(-2.79559540700005,12.2,3.12359051999999));
#305530=CARTESIAN_POINT('Ctrl Pts',(-2.79559540700005,5.2,3.12359051999999));
#305531=CARTESIAN_POINT('Ctrl Pts',(-2.79559540700005,2.2,3.12359051999999));
#305532=CARTESIAN_POINT('Ctrl Pts',(-2.79498607000006,12.2,3.12223288299998));
#305533=CARTESIAN_POINT('Ctrl Pts',(-2.79498607000006,5.2,3.12223288299998));
#305534=CARTESIAN_POINT('Ctrl Pts',(-2.79498607000006,2.2,3.12223288299998));
#305535=CARTESIAN_POINT('Ctrl Pts',(-2.79437708900006,12.2,3.12088028099998));
#305536=CARTESIAN_POINT('Ctrl Pts',(-2.79437708900006,5.2,3.12088028099998));
#305537=CARTESIAN_POINT('Ctrl Pts',(-2.79437708900006,2.2,3.12088028099998));
#305538=CARTESIAN_POINT('Ctrl Pts',(-2.79376847500005,12.2,3.11953271599998));
#305539=CARTESIAN_POINT('Ctrl Pts',(-2.79376847500005,5.2,3.11953271599998));
#305540=CARTESIAN_POINT('Ctrl Pts',(-2.79376847500005,2.2,3.11953271599998));
#305541=CARTESIAN_POINT('Ctrl Pts',(-2.79316024400006,12.2,3.11819019099998));
#305542=CARTESIAN_POINT('Ctrl Pts',(-2.79316024400006,5.2,3.11819019099998));
#305543=CARTESIAN_POINT('Ctrl Pts',(-2.79316024400006,2.2,3.11819019099998));
#305544=CARTESIAN_POINT('Ctrl Pts',(-2.79255240800006,12.2,3.11685271099999));
#305545=CARTESIAN_POINT('Ctrl Pts',(-2.79255240800006,5.2,3.11685271099999));
#305546=CARTESIAN_POINT('Ctrl Pts',(-2.79255240800006,2.2,3.11685271099999));
#305547=CARTESIAN_POINT('Ctrl Pts',(-2.79194497900006,12.2,3.11552028099998));
#305548=CARTESIAN_POINT('Ctrl Pts',(-2.79194497900006,5.2,3.11552028099998));
#305549=CARTESIAN_POINT('Ctrl Pts',(-2.79194497900006,2.2,3.11552028099998));
#305550=CARTESIAN_POINT('Ctrl Pts',(-2.79133797000005,12.2,3.11419290199999));
#305551=CARTESIAN_POINT('Ctrl Pts',(-2.79133797000005,5.2,3.11419290199999));
#305552=CARTESIAN_POINT('Ctrl Pts',(-2.79133797000005,2.2,3.11419290199999));
#305553=CARTESIAN_POINT('Ctrl Pts',(-2.79073139700006,12.2,3.11287057999999));
#305554=CARTESIAN_POINT('Ctrl Pts',(-2.79073139700006,5.2,3.11287057999999));
#305555=CARTESIAN_POINT('Ctrl Pts',(-2.79073139700006,2.2,3.11287057999999));
#305556=CARTESIAN_POINT('Ctrl Pts',(-2.79012526800006,12.2,3.11155331599998));
#305557=CARTESIAN_POINT('Ctrl Pts',(-2.79012526800006,5.2,3.11155331599998));
#305558=CARTESIAN_POINT('Ctrl Pts',(-2.79012526800006,2.2,3.11155331599998));
#305559=CARTESIAN_POINT('Ctrl Pts',(-2.78951960100006,12.2,3.11024111699999));
#305560=CARTESIAN_POINT('Ctrl Pts',(-2.78951960100006,5.2,3.11024111699999));
#305561=CARTESIAN_POINT('Ctrl Pts',(-2.78951960100006,2.2,3.11024111699999));
#305562=CARTESIAN_POINT('Ctrl Pts',(-2.78891440600006,12.2,3.10893398399998));
#305563=CARTESIAN_POINT('Ctrl Pts',(-2.78891440600006,5.2,3.10893398399998));
#305564=CARTESIAN_POINT('Ctrl Pts',(-2.78891440600006,2.2,3.10893398399998));
#305565=CARTESIAN_POINT('Ctrl Pts',(-2.78830969800006,12.2,3.10763192299999));
#305566=CARTESIAN_POINT('Ctrl Pts',(-2.78830969800006,5.2,3.10763192299999));
#305567=CARTESIAN_POINT('Ctrl Pts',(-2.78830969800006,2.2,3.10763192299999));
#305568=CARTESIAN_POINT('Ctrl Pts',(-2.78770549000006,12.2,3.10633493499999));
#305569=CARTESIAN_POINT('Ctrl Pts',(-2.78770549000006,5.2,3.10633493499999));
#305570=CARTESIAN_POINT('Ctrl Pts',(-2.78770549000006,2.2,3.10633493499999));
#305571=CARTESIAN_POINT('Ctrl Pts',(-2.78710179400006,12.2,3.10504302599998));
#305572=CARTESIAN_POINT('Ctrl Pts',(-2.78710179400006,5.2,3.10504302599998));
#305573=CARTESIAN_POINT('Ctrl Pts',(-2.78710179400006,2.2,3.10504302599998));
#305574=CARTESIAN_POINT('Ctrl Pts',(-2.78649862400006,12.2,3.10375619799999));
#305575=CARTESIAN_POINT('Ctrl Pts',(-2.78649862400006,5.2,3.10375619799999));
#305576=CARTESIAN_POINT('Ctrl Pts',(-2.78649862400006,2.2,3.10375619799999));
#305577=CARTESIAN_POINT('Ctrl Pts',(-2.78589599400005,12.2,3.10247445499999));
#305578=CARTESIAN_POINT('Ctrl Pts',(-2.78589599400005,5.2,3.10247445499999));
#305579=CARTESIAN_POINT('Ctrl Pts',(-2.78589599400005,2.2,3.10247445499999));
#305580=CARTESIAN_POINT('Ctrl Pts',(-2.78529391700005,12.2,3.10119780099999));
#305581=CARTESIAN_POINT('Ctrl Pts',(-2.78529391700005,5.2,3.10119780099999));
#305582=CARTESIAN_POINT('Ctrl Pts',(-2.78529391700005,2.2,3.10119780099999));
#305583=CARTESIAN_POINT('Ctrl Pts',(-2.78469240600006,12.2,3.09992623899999));
#305584=CARTESIAN_POINT('Ctrl Pts',(-2.78469240600006,5.2,3.09992623899999));
#305585=CARTESIAN_POINT('Ctrl Pts',(-2.78469240600006,2.2,3.09992623899999));
#305586=CARTESIAN_POINT('Ctrl Pts',(-2.78409147500006,12.2,3.09865977399999));
#305587=CARTESIAN_POINT('Ctrl Pts',(-2.78409147500006,5.2,3.09865977399999));
#305588=CARTESIAN_POINT('Ctrl Pts',(-2.78409147500006,2.2,3.09865977399999));
#305589=CARTESIAN_POINT('Ctrl Pts',(-2.78349113700005,12.2,3.09739840799999));
#305590=CARTESIAN_POINT('Ctrl Pts',(-2.78349113700005,5.2,3.09739840799999));
#305591=CARTESIAN_POINT('Ctrl Pts',(-2.78349113700005,2.2,3.09739840799999));
#305592=CARTESIAN_POINT('Ctrl Pts',(-2.78289140600006,12.2,3.09614214499998));
#305593=CARTESIAN_POINT('Ctrl Pts',(-2.78289140600006,5.2,3.09614214499998));
#305594=CARTESIAN_POINT('Ctrl Pts',(-2.78289140600006,2.2,3.09614214499998));
#305595=CARTESIAN_POINT('Ctrl Pts',(-2.78229229400006,12.2,3.09489098899999));
#305596=CARTESIAN_POINT('Ctrl Pts',(-2.78229229400006,5.2,3.09489098899999));
#305597=CARTESIAN_POINT('Ctrl Pts',(-2.78229229400006,2.2,3.09489098899999));
#305598=CARTESIAN_POINT('Ctrl Pts',(-2.78169381700006,12.2,3.09364494299999));
#305599=CARTESIAN_POINT('Ctrl Pts',(-2.78169381700006,5.2,3.09364494299999));
#305600=CARTESIAN_POINT('Ctrl Pts',(-2.78169381700006,2.2,3.09364494299999));
#305601=CARTESIAN_POINT('Ctrl Pts',(-2.78109598700006,12.2,3.09240401199999));
#305602=CARTESIAN_POINT('Ctrl Pts',(-2.78109598700006,5.2,3.09240401199999));
#305603=CARTESIAN_POINT('Ctrl Pts',(-2.78109598700006,2.2,3.09240401199999));
#305604=CARTESIAN_POINT('Ctrl Pts',(-2.78049881700006,12.2,3.09116819699998));
#305605=CARTESIAN_POINT('Ctrl Pts',(-2.78049881700006,5.2,3.09116819699998));
#305606=CARTESIAN_POINT('Ctrl Pts',(-2.78049881700006,2.2,3.09116819699998));
#305607=CARTESIAN_POINT('Ctrl Pts',(-2.77990232300006,12.2,3.08993750299998));
#305608=CARTESIAN_POINT('Ctrl Pts',(-2.77990232300006,5.2,3.08993750299998));
#305609=CARTESIAN_POINT('Ctrl Pts',(-2.77990232300006,2.2,3.08993750299998));
#305610=CARTESIAN_POINT('Ctrl Pts',(-2.77930651700005,12.2,3.08871193399998));
#305611=CARTESIAN_POINT('Ctrl Pts',(-2.77930651700005,5.2,3.08871193399998));
#305612=CARTESIAN_POINT('Ctrl Pts',(-2.77930651700005,2.2,3.08871193399998));
#305613=CARTESIAN_POINT('Ctrl Pts',(-2.77871141300006,12.2,3.08749149299998));
#305614=CARTESIAN_POINT('Ctrl Pts',(-2.77871141300006,5.2,3.08749149299998));
#305615=CARTESIAN_POINT('Ctrl Pts',(-2.77871141300006,2.2,3.08749149299998));
#305616=CARTESIAN_POINT('Ctrl Pts',(-2.77811702500005,12.2,3.08627618199999));
#305617=CARTESIAN_POINT('Ctrl Pts',(-2.77811702500005,5.2,3.08627618199999));
#305618=CARTESIAN_POINT('Ctrl Pts',(-2.77811702500005,2.2,3.08627618199999));
#305619=CARTESIAN_POINT('Ctrl Pts',(-2.77752336600006,12.2,3.08506600699998));
#305620=CARTESIAN_POINT('Ctrl Pts',(-2.77752336600006,5.2,3.08506600699998));
#305621=CARTESIAN_POINT('Ctrl Pts',(-2.77752336600006,2.2,3.08506600699998));
#305622=CARTESIAN_POINT('Ctrl Pts',(-2.77693045100006,12.2,3.08386097099999));
#305623=CARTESIAN_POINT('Ctrl Pts',(-2.77693045100006,5.2,3.08386097099999));
#305624=CARTESIAN_POINT('Ctrl Pts',(-2.77693045100006,2.2,3.08386097099999));
#305625=CARTESIAN_POINT('Ctrl Pts',(-2.77633829400005,12.2,3.08266107499998));
#305626=CARTESIAN_POINT('Ctrl Pts',(-2.77633829400005,5.2,3.08266107499998));
#305627=CARTESIAN_POINT('Ctrl Pts',(-2.77633829400005,2.2,3.08266107499998));
#305628=CARTESIAN_POINT('Ctrl Pts',(-2.77574690700006,12.2,3.08146632499999));
#305629=CARTESIAN_POINT('Ctrl Pts',(-2.77574690700006,5.2,3.08146632499999));
#305630=CARTESIAN_POINT('Ctrl Pts',(-2.77574690700006,2.2,3.08146632499999));
#305631=CARTESIAN_POINT('Ctrl Pts',(-2.77515630600006,12.2,3.08027672299998));
#305632=CARTESIAN_POINT('Ctrl Pts',(-2.77515630600006,5.2,3.08027672299998));
#305633=CARTESIAN_POINT('Ctrl Pts',(-2.77515630600006,2.2,3.08027672299998));
#305634=CARTESIAN_POINT('Ctrl Pts',(-2.77456650400006,12.2,3.07909227399998));
#305635=CARTESIAN_POINT('Ctrl Pts',(-2.77456650400006,5.2,3.07909227399998));
#305636=CARTESIAN_POINT('Ctrl Pts',(-2.77456650400006,2.2,3.07909227399998));
#305637=CARTESIAN_POINT('Ctrl Pts',(-2.77397751500006,12.2,3.07791298099998));
#305638=CARTESIAN_POINT('Ctrl Pts',(-2.77397751500006,5.2,3.07791298099998));
#305639=CARTESIAN_POINT('Ctrl Pts',(-2.77397751500006,2.2,3.07791298099998));
#305640=CARTESIAN_POINT('Ctrl Pts',(-2.77338935300006,12.2,3.07673884499999));
#305641=CARTESIAN_POINT('Ctrl Pts',(-2.77338935300006,5.2,3.07673884499999));
#305642=CARTESIAN_POINT('Ctrl Pts',(-2.77338935300006,2.2,3.07673884499999));
#305643=CARTESIAN_POINT('Ctrl Pts',(-2.77280203300006,12.2,3.07556987199998));
#305644=CARTESIAN_POINT('Ctrl Pts',(-2.77280203300006,5.2,3.07556987199998));
#305645=CARTESIAN_POINT('Ctrl Pts',(-2.77280203300006,2.2,3.07556987199998));
#305646=CARTESIAN_POINT('Ctrl Pts',(-2.77221556900006,12.2,3.07440606499998));
#305647=CARTESIAN_POINT('Ctrl Pts',(-2.77221556900006,5.2,3.07440606499998));
#305648=CARTESIAN_POINT('Ctrl Pts',(-2.77221556900006,2.2,3.07440606499998));
#305649=CARTESIAN_POINT('Ctrl Pts',(-2.77162997300006,12.2,3.07324742699999));
#305650=CARTESIAN_POINT('Ctrl Pts',(-2.77162997300006,5.2,3.07324742699999));
#305651=CARTESIAN_POINT('Ctrl Pts',(-2.77162997300006,2.2,3.07324742699999));
#305652=CARTESIAN_POINT('Ctrl Pts',(-2.77104526100006,12.2,3.07209396099999));
#305653=CARTESIAN_POINT('Ctrl Pts',(-2.77104526100006,5.2,3.07209396099999));
#305654=CARTESIAN_POINT('Ctrl Pts',(-2.77104526100006,2.2,3.07209396099999));
#305655=CARTESIAN_POINT('Ctrl Pts',(-2.77046144700006,12.2,3.07094566999999));
#305656=CARTESIAN_POINT('Ctrl Pts',(-2.77046144700006,5.2,3.07094566999999));
#305657=CARTESIAN_POINT('Ctrl Pts',(-2.77046144700006,2.2,3.07094566999999));
#305658=CARTESIAN_POINT('Ctrl Pts',(-2.76987854600006,12.2,3.06980255899998));
#305659=CARTESIAN_POINT('Ctrl Pts',(-2.76987854600006,5.2,3.06980255899998));
#305660=CARTESIAN_POINT('Ctrl Pts',(-2.76987854600006,2.2,3.06980255899998));
#305661=CARTESIAN_POINT('Ctrl Pts',(-2.76929657200006,12.2,3.06866462899999));
#305662=CARTESIAN_POINT('Ctrl Pts',(-2.76929657200006,5.2,3.06866462899999));
#305663=CARTESIAN_POINT('Ctrl Pts',(-2.76929657200006,2.2,3.06866462899999));
#305664=CARTESIAN_POINT('Ctrl Pts',(-2.76871553700006,12.2,3.06753188599998));
#305665=CARTESIAN_POINT('Ctrl Pts',(-2.76871553700006,5.2,3.06753188599998));
#305666=CARTESIAN_POINT('Ctrl Pts',(-2.76871553700006,2.2,3.06753188599998));
#305667=CARTESIAN_POINT('Ctrl Pts',(-2.76813545900006,12.2,3.06640433199998));
#305668=CARTESIAN_POINT('Ctrl Pts',(-2.76813545900006,5.2,3.06640433199998));
#305669=CARTESIAN_POINT('Ctrl Pts',(-2.76813545900006,2.2,3.06640433199998));
#305670=CARTESIAN_POINT('Ctrl Pts',(-2.76755635000006,12.2,3.06528196999999));
#305671=CARTESIAN_POINT('Ctrl Pts',(-2.76755635000006,5.2,3.06528196999999));
#305672=CARTESIAN_POINT('Ctrl Pts',(-2.76755635000006,2.2,3.06528196999999));
#305673=CARTESIAN_POINT('Ctrl Pts',(-2.76697822500005,12.2,3.06416480299998));
#305674=CARTESIAN_POINT('Ctrl Pts',(-2.76697822500005,5.2,3.06416480299998));
#305675=CARTESIAN_POINT('Ctrl Pts',(-2.76697822500005,2.2,3.06416480299998));
#305676=CARTESIAN_POINT('Ctrl Pts',(-2.76640109900006,12.2,3.06305283499999));
#305677=CARTESIAN_POINT('Ctrl Pts',(-2.76640109900006,5.2,3.06305283499999));
#305678=CARTESIAN_POINT('Ctrl Pts',(-2.76640109900006,2.2,3.06305283499999));
#305679=CARTESIAN_POINT('Ctrl Pts',(-2.76582498600006,12.2,3.06194606899999));
#305680=CARTESIAN_POINT('Ctrl Pts',(-2.76582498600006,5.2,3.06194606899999));
#305681=CARTESIAN_POINT('Ctrl Pts',(-2.76582498600006,2.2,3.06194606899999));
#305682=CARTESIAN_POINT('Ctrl Pts',(-2.76524990000006,12.2,3.06084450799998));
#305683=CARTESIAN_POINT('Ctrl Pts',(-2.76524990000006,5.2,3.06084450799998));
#305684=CARTESIAN_POINT('Ctrl Pts',(-2.76524990000006,2.2,3.06084450799998));
#305685=CARTESIAN_POINT('Ctrl Pts',(-2.76467585600006,12.2,3.05974815599999));
#305686=CARTESIAN_POINT('Ctrl Pts',(-2.76467585600006,5.2,3.05974815599999));
#305687=CARTESIAN_POINT('Ctrl Pts',(-2.76467585600006,2.2,3.05974815599999));
#305688=CARTESIAN_POINT('Ctrl Pts',(-2.76410287000005,12.2,3.05865701499999));
#305689=CARTESIAN_POINT('Ctrl Pts',(-2.76410287000005,5.2,3.05865701499999));
#305690=CARTESIAN_POINT('Ctrl Pts',(-2.76410287000005,2.2,3.05865701499999));
#305691=CARTESIAN_POINT('Ctrl Pts',(-2.76353095500005,12.2,3.05757108899999));
#305692=CARTESIAN_POINT('Ctrl Pts',(-2.76353095500005,5.2,3.05757108899999));
#305693=CARTESIAN_POINT('Ctrl Pts',(-2.76353095500005,2.2,3.05757108899999));
#305694=CARTESIAN_POINT('Ctrl Pts',(-2.76296012600006,12.2,3.05649038199999));
#305695=CARTESIAN_POINT('Ctrl Pts',(-2.76296012600006,5.2,3.05649038199999));
#305696=CARTESIAN_POINT('Ctrl Pts',(-2.76296012600006,2.2,3.05649038199999));
#305697=CARTESIAN_POINT('Ctrl Pts',(-2.76239039700005,12.2,3.05541489599998));
#305698=CARTESIAN_POINT('Ctrl Pts',(-2.76239039700005,5.2,3.05541489599998));
#305699=CARTESIAN_POINT('Ctrl Pts',(-2.76239039700005,2.2,3.05541489599998));
#305700=CARTESIAN_POINT('Ctrl Pts',(-2.76182178500005,12.2,3.05434463399998));
#305701=CARTESIAN_POINT('Ctrl Pts',(-2.76182178500005,5.2,3.05434463399998));
#305702=CARTESIAN_POINT('Ctrl Pts',(-2.76182178500005,2.2,3.05434463399998));
#305703=CARTESIAN_POINT('Ctrl Pts',(-2.76125430200006,12.2,3.05327959899999));
#305704=CARTESIAN_POINT('Ctrl Pts',(-2.76125430200006,5.2,3.05327959899999));
#305705=CARTESIAN_POINT('Ctrl Pts',(-2.76125430200006,2.2,3.05327959899999));
#305706=CARTESIAN_POINT('Ctrl Pts',(-2.76068796600006,12.2,3.05221979499999));
#305707=CARTESIAN_POINT('Ctrl Pts',(-2.76068796600006,5.2,3.05221979499999));
#305708=CARTESIAN_POINT('Ctrl Pts',(-2.76068796600006,2.2,3.05221979499999));
#305709=CARTESIAN_POINT('Ctrl Pts',(-2.76012279100006,12.2,3.05116522499999));
#305710=CARTESIAN_POINT('Ctrl Pts',(-2.76012279100006,5.2,3.05116522499999));
#305711=CARTESIAN_POINT('Ctrl Pts',(-2.76012279100006,2.2,3.05116522499999));
#305712=CARTESIAN_POINT('Ctrl Pts',(-2.75955878900006,12.2,3.05011589299998));
#305713=CARTESIAN_POINT('Ctrl Pts',(-2.75955878900006,5.2,3.05011589299998));
#305714=CARTESIAN_POINT('Ctrl Pts',(-2.75955878900006,2.2,3.05011589299998));
#305715=CARTESIAN_POINT('Ctrl Pts',(-2.75899597900006,12.2,3.04907179999999));
#305716=CARTESIAN_POINT('Ctrl Pts',(-2.75899597900006,5.2,3.04907179999999));
#305717=CARTESIAN_POINT('Ctrl Pts',(-2.75899597900006,2.2,3.04907179999999));
#305718=CARTESIAN_POINT('Ctrl Pts',(-2.75843437300006,12.2,3.04803295099998));
#305719=CARTESIAN_POINT('Ctrl Pts',(-2.75843437300006,5.2,3.04803295099998));
#305720=CARTESIAN_POINT('Ctrl Pts',(-2.75843437300006,2.2,3.04803295099998));
#305721=CARTESIAN_POINT('Ctrl Pts',(-2.75787398700006,12.2,3.04699934699999));
#305722=CARTESIAN_POINT('Ctrl Pts',(-2.75787398700006,5.2,3.04699934699999));
#305723=CARTESIAN_POINT('Ctrl Pts',(-2.75787398700006,2.2,3.04699934699999));
#305724=CARTESIAN_POINT('Ctrl Pts',(-2.75731483700006,12.2,3.04597099299999));
#305725=CARTESIAN_POINT('Ctrl Pts',(-2.75731483700006,5.2,3.04597099299999));
#305726=CARTESIAN_POINT('Ctrl Pts',(-2.75731483700006,2.2,3.04597099299999));
#305727=CARTESIAN_POINT('Ctrl Pts',(-2.75675693700005,12.2,3.04494789199998));
#305728=CARTESIAN_POINT('Ctrl Pts',(-2.75675693700005,5.2,3.04494789199998));
#305729=CARTESIAN_POINT('Ctrl Pts',(-2.75675693700005,2.2,3.04494789199998));
#305730=CARTESIAN_POINT('Ctrl Pts',(-2.75620030300006,12.2,3.04393004499998));
#305731=CARTESIAN_POINT('Ctrl Pts',(-2.75620030300006,5.2,3.04393004499998));
#305732=CARTESIAN_POINT('Ctrl Pts',(-2.75620030300006,2.2,3.04393004499998));
#305733=CARTESIAN_POINT('Ctrl Pts',(-2.75564495000005,12.2,3.04291745799999));
#305734=CARTESIAN_POINT('Ctrl Pts',(-2.75564495000005,5.2,3.04291745799999));
#305735=CARTESIAN_POINT('Ctrl Pts',(-2.75564495000005,2.2,3.04291745799999));
#305736=CARTESIAN_POINT('Ctrl Pts',(-2.75509089200006,12.2,3.04191013099998));
#305737=CARTESIAN_POINT('Ctrl Pts',(-2.75509089200006,5.2,3.04191013099998));
#305738=CARTESIAN_POINT('Ctrl Pts',(-2.75509089200006,2.2,3.04191013099998));
#305739=CARTESIAN_POINT('Ctrl Pts',(-2.75453814700006,12.2,3.04090806999999));
#305740=CARTESIAN_POINT('Ctrl Pts',(-2.75453814700006,5.2,3.04090806999999));
#305741=CARTESIAN_POINT('Ctrl Pts',(-2.75453814700006,2.2,3.04090806999999));
#305742=CARTESIAN_POINT('Ctrl Pts',(-2.75398672700006,12.2,3.03991127599998));
#305743=CARTESIAN_POINT('Ctrl Pts',(-2.75398672700006,5.2,3.03991127599998));
#305744=CARTESIAN_POINT('Ctrl Pts',(-2.75398672700006,2.2,3.03991127599998));
#305745=CARTESIAN_POINT('Ctrl Pts',(-2.75343665000006,12.2,3.03891975299998));
#305746=CARTESIAN_POINT('Ctrl Pts',(-2.75343665000006,5.2,3.03891975299998));
#305747=CARTESIAN_POINT('Ctrl Pts',(-2.75343665000006,2.2,3.03891975299998));
#305748=CARTESIAN_POINT('Ctrl Pts',(-2.75288792900006,12.2,3.03793350199999));
#305749=CARTESIAN_POINT('Ctrl Pts',(-2.75288792900006,5.2,3.03793350199999));
#305750=CARTESIAN_POINT('Ctrl Pts',(-2.75288792900006,2.2,3.03793350199999));
#305751=CARTESIAN_POINT('Ctrl Pts',(-2.75234058200006,12.2,3.03695252899999));
#305752=CARTESIAN_POINT('Ctrl Pts',(-2.75234058200006,5.2,3.03695252899999));
#305753=CARTESIAN_POINT('Ctrl Pts',(-2.75234058200006,2.2,3.03695252899999));
#305754=CARTESIAN_POINT('Ctrl Pts',(-2.75179462400006,12.2,3.03597683399998));
#305755=CARTESIAN_POINT('Ctrl Pts',(-2.75179462400006,5.2,3.03597683399998));
#305756=CARTESIAN_POINT('Ctrl Pts',(-2.75179462400006,2.2,3.03597683399998));
#305757=CARTESIAN_POINT('Ctrl Pts',(-2.75125006900006,12.2,3.03500642199998));
#305758=CARTESIAN_POINT('Ctrl Pts',(-2.75125006900006,5.2,3.03500642199998));
#305759=CARTESIAN_POINT('Ctrl Pts',(-2.75125006900006,2.2,3.03500642199998));
#305760=CARTESIAN_POINT('Ctrl Pts',(-2.75070693300006,12.2,3.03404129499998));
#305761=CARTESIAN_POINT('Ctrl Pts',(-2.75070693300006,5.2,3.03404129499998));
#305762=CARTESIAN_POINT('Ctrl Pts',(-2.75070693300006,2.2,3.03404129499998));
#305763=CARTESIAN_POINT('Ctrl Pts',(-2.75016523200006,12.2,3.03308145599999));
#305764=CARTESIAN_POINT('Ctrl Pts',(-2.75016523200006,5.2,3.03308145599999));
#305765=CARTESIAN_POINT('Ctrl Pts',(-2.75016523200006,2.2,3.03308145599999));
#305766=CARTESIAN_POINT('Ctrl Pts',(-2.74962498200006,12.2,3.03212690799998));
#305767=CARTESIAN_POINT('Ctrl Pts',(-2.74962498200006,5.2,3.03212690799998));
#305768=CARTESIAN_POINT('Ctrl Pts',(-2.74962498200006,2.2,3.03212690799998));
#305769=CARTESIAN_POINT('Ctrl Pts',(-2.74908619900006,12.2,3.03117765399998));
#305770=CARTESIAN_POINT('Ctrl Pts',(-2.74908619900006,5.2,3.03117765399998));
#305771=CARTESIAN_POINT('Ctrl Pts',(-2.74908619900006,2.2,3.03117765399998));
#305772=CARTESIAN_POINT('Ctrl Pts',(-2.74854889700006,12.2,3.03023369599998));
#305773=CARTESIAN_POINT('Ctrl Pts',(-2.74854889700006,5.2,3.03023369599998));
#305774=CARTESIAN_POINT('Ctrl Pts',(-2.74854889700006,2.2,3.03023369599998));
#305775=CARTESIAN_POINT('Ctrl Pts',(-2.74801309400006,12.2,3.02929503899998));
#305776=CARTESIAN_POINT('Ctrl Pts',(-2.74801309400006,5.2,3.02929503899998));
#305777=CARTESIAN_POINT('Ctrl Pts',(-2.74801309400006,2.2,3.02929503899998));
#305778=CARTESIAN_POINT('Ctrl Pts',(-2.74747880300006,12.2,3.02836168399998));
#305779=CARTESIAN_POINT('Ctrl Pts',(-2.74747880300006,5.2,3.02836168399998));
#305780=CARTESIAN_POINT('Ctrl Pts',(-2.74747880300006,2.2,3.02836168399998));
#305781=CARTESIAN_POINT('Ctrl Pts',(-2.74694604300006,12.2,3.02743363399999));
#305782=CARTESIAN_POINT('Ctrl Pts',(-2.74694604300006,5.2,3.02743363399999));
#305783=CARTESIAN_POINT('Ctrl Pts',(-2.74694604300006,2.2,3.02743363399999));
#305784=CARTESIAN_POINT('Ctrl Pts',(-2.74641482900006,12.2,3.02651089199999));
#305785=CARTESIAN_POINT('Ctrl Pts',(-2.74641482900006,5.2,3.02651089199999));
#305786=CARTESIAN_POINT('Ctrl Pts',(-2.74641482900006,2.2,3.02651089199999));
#305787=CARTESIAN_POINT('Ctrl Pts',(-2.74588517500006,12.2,3.02559346099999));
#305788=CARTESIAN_POINT('Ctrl Pts',(-2.74588517500006,5.2,3.02559346099999));
#305789=CARTESIAN_POINT('Ctrl Pts',(-2.74588517500006,2.2,3.02559346099999));
#305790=CARTESIAN_POINT('Ctrl Pts',(-2.74535709800006,12.2,3.02468134399999));
#305791=CARTESIAN_POINT('Ctrl Pts',(-2.74535709800006,5.2,3.02468134399999));
#305792=CARTESIAN_POINT('Ctrl Pts',(-2.74535709800006,2.2,3.02468134399999));
#305793=CARTESIAN_POINT('Ctrl Pts',(-2.74483061500006,12.2,3.02377454299998));
#305794=CARTESIAN_POINT('Ctrl Pts',(-2.74483061500006,5.2,3.02377454299998));
#305795=CARTESIAN_POINT('Ctrl Pts',(-2.74483061500006,2.2,3.02377454299998));
#305796=CARTESIAN_POINT('Ctrl Pts',(-2.74430574200006,12.2,3.02287306099998));
#305797=CARTESIAN_POINT('Ctrl Pts',(-2.74430574200006,5.2,3.02287306099998));
#305798=CARTESIAN_POINT('Ctrl Pts',(-2.74430574200006,2.2,3.02287306099998));
#305799=CARTESIAN_POINT('Ctrl Pts',(-2.74378249400006,12.2,3.02197690099998));
#305800=CARTESIAN_POINT('Ctrl Pts',(-2.74378249400006,5.2,3.02197690099998));
#305801=CARTESIAN_POINT('Ctrl Pts',(-2.74378249400006,2.2,3.02197690099998));
#305802=CARTESIAN_POINT('Ctrl Pts',(-2.74326088800006,12.2,3.02108606599998));
#305803=CARTESIAN_POINT('Ctrl Pts',(-2.74326088800006,5.2,3.02108606599998));
#305804=CARTESIAN_POINT('Ctrl Pts',(-2.74326088800006,2.2,3.02108606599998));
#305805=CARTESIAN_POINT('Ctrl Pts',(-2.74274094000006,12.2,3.02020055799999));
#305806=CARTESIAN_POINT('Ctrl Pts',(-2.74274094000006,5.2,3.02020055799999));
#305807=CARTESIAN_POINT('Ctrl Pts',(-2.74274094000006,2.2,3.02020055799999));
#305808=CARTESIAN_POINT('Ctrl Pts',(-2.74222266600006,12.2,3.01932038099999));
#305809=CARTESIAN_POINT('Ctrl Pts',(-2.74222266600006,5.2,3.01932038099999));
#305810=CARTESIAN_POINT('Ctrl Pts',(-2.74222266600006,2.2,3.01932038099999));
#305811=CARTESIAN_POINT('Ctrl Pts',(-2.74170608200006,12.2,3.01844553599998));
#305812=CARTESIAN_POINT('Ctrl Pts',(-2.74170608200006,5.2,3.01844553599998));
#305813=CARTESIAN_POINT('Ctrl Pts',(-2.74170608200006,2.2,3.01844553599998));
#305814=CARTESIAN_POINT('Ctrl Pts',(-2.74119120600006,12.2,3.01757602599999));
#305815=CARTESIAN_POINT('Ctrl Pts',(-2.74119120600006,5.2,3.01757602599999));
#305816=CARTESIAN_POINT('Ctrl Pts',(-2.74119120600006,2.2,3.01757602599999));
#305817=CARTESIAN_POINT('Ctrl Pts',(-2.74067805200006,12.2,3.01671185499998));
#305818=CARTESIAN_POINT('Ctrl Pts',(-2.74067805200006,5.2,3.01671185499998));
#305819=CARTESIAN_POINT('Ctrl Pts',(-2.74067805200006,2.2,3.01671185499998));
#305820=CARTESIAN_POINT('Ctrl Pts',(-2.74016663800006,12.2,3.01585302399998));
#305821=CARTESIAN_POINT('Ctrl Pts',(-2.74016663800006,5.2,3.01585302399998));
#305822=CARTESIAN_POINT('Ctrl Pts',(-2.74016663800006,2.2,3.01585302399998));
#305823=CARTESIAN_POINT('Ctrl Pts',(-2.73965698000006,12.2,3.01499953699999));
#305824=CARTESIAN_POINT('Ctrl Pts',(-2.73965698000006,5.2,3.01499953699999));
#305825=CARTESIAN_POINT('Ctrl Pts',(-2.73965698000006,2.2,3.01499953699999));
#305826=CARTESIAN_POINT('Ctrl Pts',(-2.73914909500005,12.2,3.01415139599998));
#305827=CARTESIAN_POINT('Ctrl Pts',(-2.73914909500005,5.2,3.01415139599998));
#305828=CARTESIAN_POINT('Ctrl Pts',(-2.73914909500005,2.2,3.01415139599998));
#305829=CARTESIAN_POINT('Ctrl Pts',(-2.73864299800006,12.2,3.01330860299998));
#305830=CARTESIAN_POINT('Ctrl Pts',(-2.73864299800006,5.2,3.01330860299998));
#305831=CARTESIAN_POINT('Ctrl Pts',(-2.73864299800006,2.2,3.01330860299998));
#305832=CARTESIAN_POINT('Ctrl Pts',(-2.73813870800006,12.2,3.01247116199999));
#305833=CARTESIAN_POINT('Ctrl Pts',(-2.73813870800006,5.2,3.01247116199999));
#305834=CARTESIAN_POINT('Ctrl Pts',(-2.73813870800006,2.2,3.01247116199999));
#305835=CARTESIAN_POINT('Ctrl Pts',(-2.73763624000006,12.2,3.01163907399999));
#305836=CARTESIAN_POINT('Ctrl Pts',(-2.73763624000006,5.2,3.01163907399999));
#305837=CARTESIAN_POINT('Ctrl Pts',(-2.73763624000006,2.2,3.01163907399999));
#305838=CARTESIAN_POINT('Ctrl Pts',(-2.73713561000006,12.2,3.01081234199999));
#305839=CARTESIAN_POINT('Ctrl Pts',(-2.73713561000006,5.2,3.01081234199999));
#305840=CARTESIAN_POINT('Ctrl Pts',(-2.73713561000006,2.2,3.01081234199999));
#305841=CARTESIAN_POINT('Ctrl Pts',(-2.73663683700006,12.2,3.00999096999998));
#305842=CARTESIAN_POINT('Ctrl Pts',(-2.73663683700006,5.2,3.00999096999998));
#305843=CARTESIAN_POINT('Ctrl Pts',(-2.73663683700006,2.2,3.00999096999998));
#305844=CARTESIAN_POINT('Ctrl Pts',(-2.73613993700006,12.2,3.00917495999999));
#305845=CARTESIAN_POINT('Ctrl Pts',(-2.73613993700006,5.2,3.00917495999999));
#305846=CARTESIAN_POINT('Ctrl Pts',(-2.73613993700006,2.2,3.00917495999999));
#305847=CARTESIAN_POINT('Ctrl Pts',(-2.73564492500005,12.2,3.00836431199999));
#305848=CARTESIAN_POINT('Ctrl Pts',(-2.73564492500005,5.2,3.00836431199999));
#305849=CARTESIAN_POINT('Ctrl Pts',(-2.73564492500005,2.2,3.00836431199999));
#305850=CARTESIAN_POINT('Ctrl Pts',(-2.73515182000006,12.2,3.00755903099999));
#305851=CARTESIAN_POINT('Ctrl Pts',(-2.73515182000006,5.2,3.00755903099999));
#305852=CARTESIAN_POINT('Ctrl Pts',(-2.73515182000006,2.2,3.00755903099999));
#305853=CARTESIAN_POINT('Ctrl Pts',(-2.73466063800006,12.2,3.00675911899998));
#305854=CARTESIAN_POINT('Ctrl Pts',(-2.73466063800006,5.2,3.00675911899998));
#305855=CARTESIAN_POINT('Ctrl Pts',(-2.73466063800006,2.2,3.00675911899998));
#305856=CARTESIAN_POINT('Ctrl Pts',(-2.73417139700005,12.2,3.00596457899999));
#305857=CARTESIAN_POINT('Ctrl Pts',(-2.73417139700005,5.2,3.00596457899999));
#305858=CARTESIAN_POINT('Ctrl Pts',(-2.73417139700005,2.2,3.00596457899999));
#305859=CARTESIAN_POINT('Ctrl Pts',(-2.73368411300006,12.2,3.00517541299998));
#305860=CARTESIAN_POINT('Ctrl Pts',(-2.73368411300006,5.2,3.00517541299998));
#305861=CARTESIAN_POINT('Ctrl Pts',(-2.73368411300006,2.2,3.00517541299998));
#305862=CARTESIAN_POINT('Ctrl Pts',(-2.73319880200006,12.2,3.00439162199999));
#305863=CARTESIAN_POINT('Ctrl Pts',(-2.73319880200006,5.2,3.00439162199999));
#305864=CARTESIAN_POINT('Ctrl Pts',(-2.73319880200006,2.2,3.00439162199999));
#305865=CARTESIAN_POINT('Ctrl Pts',(-2.73271548400006,12.2,3.00361320999999));
#305866=CARTESIAN_POINT('Ctrl Pts',(-2.73271548400006,5.2,3.00361320999999));
#305867=CARTESIAN_POINT('Ctrl Pts',(-2.73271548400006,2.2,3.00361320999999));
#305868=CARTESIAN_POINT('Ctrl Pts',(-2.73223417300006,12.2,3.00284017899998));
#305869=CARTESIAN_POINT('Ctrl Pts',(-2.73223417300006,5.2,3.00284017899998));
#305870=CARTESIAN_POINT('Ctrl Pts',(-2.73223417300006,2.2,3.00284017899998));
#305871=CARTESIAN_POINT('Ctrl Pts',(-2.73175488900006,12.2,3.00207253199999));
#305872=CARTESIAN_POINT('Ctrl Pts',(-2.73175488900006,5.2,3.00207253199999));
#305873=CARTESIAN_POINT('Ctrl Pts',(-2.73175488900006,2.2,3.00207253199999));
#305874=CARTESIAN_POINT('Ctrl Pts',(-2.73127764700006,12.2,3.00131027199999));
#305875=CARTESIAN_POINT('Ctrl Pts',(-2.73127764700006,5.2,3.00131027199999));
#305876=CARTESIAN_POINT('Ctrl Pts',(-2.73127764700006,2.2,3.00131027199999));
#305877=CARTESIAN_POINT('Ctrl Pts',(-2.73080246700005,12.2,3.00055339899998));
#305878=CARTESIAN_POINT('Ctrl Pts',(-2.73080246700005,5.2,3.00055339899998));
#305879=CARTESIAN_POINT('Ctrl Pts',(-2.73080246700005,2.2,3.00055339899998));
#305880=CARTESIAN_POINT('Ctrl Pts',(-2.73032936400006,12.2,2.99980191599998));
#305881=CARTESIAN_POINT('Ctrl Pts',(-2.73032936400006,5.2,2.99980191599998));
#305882=CARTESIAN_POINT('Ctrl Pts',(-2.73032936400006,2.2,2.99980191599998));
#305883=CARTESIAN_POINT('Ctrl Pts',(-2.72985835500006,12.2,2.99905582699999));
#305884=CARTESIAN_POINT('Ctrl Pts',(-2.72985835500006,5.2,2.99905582699999));
#305885=CARTESIAN_POINT('Ctrl Pts',(-2.72985835500006,2.2,2.99905582699999));
#305886=CARTESIAN_POINT('Ctrl Pts',(-2.72938946000005,12.2,2.99831513299999));
#305887=CARTESIAN_POINT('Ctrl Pts',(-2.72938946000005,5.2,2.99831513299999));
#305888=CARTESIAN_POINT('Ctrl Pts',(-2.72938946000005,2.2,2.99831513299999));
#305889=CARTESIAN_POINT('Ctrl Pts',(-2.72892269400006,12.2,2.99757983599999));
#305890=CARTESIAN_POINT('Ctrl Pts',(-2.72892269400006,5.2,2.99757983599999));
#305891=CARTESIAN_POINT('Ctrl Pts',(-2.72892269400006,2.2,2.99757983599999));
#305892=CARTESIAN_POINT('Ctrl Pts',(-2.72845807600006,12.2,2.99684993899999));
#305893=CARTESIAN_POINT('Ctrl Pts',(-2.72845807600006,5.2,2.99684993899999));
#305894=CARTESIAN_POINT('Ctrl Pts',(-2.72845807600006,2.2,2.99684993899999));
#305895=CARTESIAN_POINT('Ctrl Pts',(-2.72799562300006,12.2,2.99612544499999));
#305896=CARTESIAN_POINT('Ctrl Pts',(-2.72799562300006,5.2,2.99612544499999));
#305897=CARTESIAN_POINT('Ctrl Pts',(-2.72799562300006,2.2,2.99612544499999));
#305898=CARTESIAN_POINT('Ctrl Pts',(-2.72753535200006,12.2,2.99540635399998));
#305899=CARTESIAN_POINT('Ctrl Pts',(-2.72753535200006,5.2,2.99540635399998));
#305900=CARTESIAN_POINT('Ctrl Pts',(-2.72753535200006,2.2,2.99540635399998));
#305901=CARTESIAN_POINT('Ctrl Pts',(-2.72707728300006,12.2,2.99469267099998));
#305902=CARTESIAN_POINT('Ctrl Pts',(-2.72707728300006,5.2,2.99469267099998));
#305903=CARTESIAN_POINT('Ctrl Pts',(-2.72707728300006,2.2,2.99469267099998));
#305904=CARTESIAN_POINT('Ctrl Pts',(-2.72662143200006,12.2,2.99398439599998));
#305905=CARTESIAN_POINT('Ctrl Pts',(-2.72662143200006,5.2,2.99398439599998));
#305906=CARTESIAN_POINT('Ctrl Pts',(-2.72662143200006,2.2,2.99398439599998));
#305907=CARTESIAN_POINT('Ctrl Pts',(-2.72616781700005,12.2,2.99328153199999));
#305908=CARTESIAN_POINT('Ctrl Pts',(-2.72616781700005,5.2,2.99328153199999));
#305909=CARTESIAN_POINT('Ctrl Pts',(-2.72616781700005,2.2,2.99328153199999));
#305910=CARTESIAN_POINT('Ctrl Pts',(-2.72571645600005,12.2,2.99258408199999));
#305911=CARTESIAN_POINT('Ctrl Pts',(-2.72571645600005,5.2,2.99258408199999));
#305912=CARTESIAN_POINT('Ctrl Pts',(-2.72571645600005,2.2,2.99258408199999));
#305913=CARTESIAN_POINT('Ctrl Pts',(-2.72526736600006,12.2,2.99189204699999));
#305914=CARTESIAN_POINT('Ctrl Pts',(-2.72526736600006,5.2,2.99189204699999));
#305915=CARTESIAN_POINT('Ctrl Pts',(-2.72526736600006,2.2,2.99189204699999));
#305916=CARTESIAN_POINT('Ctrl Pts',(-2.72482056700006,12.2,2.99120542899999));
#305917=CARTESIAN_POINT('Ctrl Pts',(-2.72482056700006,5.2,2.99120542899999));
#305918=CARTESIAN_POINT('Ctrl Pts',(-2.72482056700006,2.2,2.99120542899999));
#305919=CARTESIAN_POINT('Ctrl Pts',(-2.72437607500006,12.2,2.99052423099998));
#305920=CARTESIAN_POINT('Ctrl Pts',(-2.72437607500006,5.2,2.99052423099998));
#305921=CARTESIAN_POINT('Ctrl Pts',(-2.72437607500006,2.2,2.99052423099998));
#305922=CARTESIAN_POINT('Ctrl Pts',(-2.72393390900006,12.2,2.98984845499999));
#305923=CARTESIAN_POINT('Ctrl Pts',(-2.72393390900006,5.2,2.98984845499999));
#305924=CARTESIAN_POINT('Ctrl Pts',(-2.72393390900006,2.2,2.98984845499999));
#305925=CARTESIAN_POINT('Ctrl Pts',(-2.72349408800005,12.2,2.98917810299999));
#305926=CARTESIAN_POINT('Ctrl Pts',(-2.72349408800005,5.2,2.98917810299999));
#305927=CARTESIAN_POINT('Ctrl Pts',(-2.72349408800005,2.2,2.98917810299999));
#305928=CARTESIAN_POINT('Ctrl Pts',(-2.72305662800005,12.2,2.98851317699998));
#305929=CARTESIAN_POINT('Ctrl Pts',(-2.72305662800005,5.2,2.98851317699998));
#305930=CARTESIAN_POINT('Ctrl Pts',(-2.72305662800005,2.2,2.98851317699998));
#305931=CARTESIAN_POINT('Ctrl Pts',(-2.72262154800006,12.2,2.98785367799999));
#305932=CARTESIAN_POINT('Ctrl Pts',(-2.72262154800006,5.2,2.98785367799999));
#305933=CARTESIAN_POINT('Ctrl Pts',(-2.72262154800006,2.2,2.98785367799999));
#305934=CARTESIAN_POINT('Ctrl Pts',(-2.72218886800006,12.2,2.98719960999998));
#305935=CARTESIAN_POINT('Ctrl Pts',(-2.72218886800006,5.2,2.98719960999998));
#305936=CARTESIAN_POINT('Ctrl Pts',(-2.72218886800006,2.2,2.98719960999998));
#305937=CARTESIAN_POINT('Ctrl Pts',(-2.72175860500006,12.2,2.98655097499999));
#305938=CARTESIAN_POINT('Ctrl Pts',(-2.72175860500006,5.2,2.98655097499999));
#305939=CARTESIAN_POINT('Ctrl Pts',(-2.72175860500006,2.2,2.98655097499999));
#305940=CARTESIAN_POINT('Ctrl Pts',(-2.72133077600006,12.2,2.98590777299999));
#305941=CARTESIAN_POINT('Ctrl Pts',(-2.72133077600006,5.2,2.98590777299999));
#305942=CARTESIAN_POINT('Ctrl Pts',(-2.72133077600006,2.2,2.98590777299999));
#305943=CARTESIAN_POINT('Ctrl Pts',(-2.72090540100006,12.2,2.98527000799999));
#305944=CARTESIAN_POINT('Ctrl Pts',(-2.72090540100006,5.2,2.98527000799999));
#305945=CARTESIAN_POINT('Ctrl Pts',(-2.72090540100006,2.2,2.98527000799999));
#305946=CARTESIAN_POINT('Ctrl Pts',(-2.72048249900006,12.2,2.98463768099998));
#305947=CARTESIAN_POINT('Ctrl Pts',(-2.72048249900006,5.2,2.98463768099998));
#305948=CARTESIAN_POINT('Ctrl Pts',(-2.72048249900006,2.2,2.98463768099998));
#305949=CARTESIAN_POINT('Ctrl Pts',(-2.72006208700006,12.2,2.98401079399999));
#305950=CARTESIAN_POINT('Ctrl Pts',(-2.72006208700006,5.2,2.98401079399999));
#305951=CARTESIAN_POINT('Ctrl Pts',(-2.72006208700006,2.2,2.98401079399999));
#305952=CARTESIAN_POINT('Ctrl Pts',(-2.71964418500006,12.2,2.98338934899999));
#305953=CARTESIAN_POINT('Ctrl Pts',(-2.71964418500006,5.2,2.98338934899999));
#305954=CARTESIAN_POINT('Ctrl Pts',(-2.71964418500006,2.2,2.98338934899999));
#305955=CARTESIAN_POINT('Ctrl Pts',(-2.71922881200005,12.2,2.98277334899999));
#305956=CARTESIAN_POINT('Ctrl Pts',(-2.71922881200005,5.2,2.98277334899999));
#305957=CARTESIAN_POINT('Ctrl Pts',(-2.71922881200005,2.2,2.98277334899999));
#305958=CARTESIAN_POINT('Ctrl Pts',(-2.71881598400005,12.2,2.98216279399998));
#305959=CARTESIAN_POINT('Ctrl Pts',(-2.71881598400005,5.2,2.98216279399998));
#305960=CARTESIAN_POINT('Ctrl Pts',(-2.71881598400005,2.2,2.98216279399998));
#305961=CARTESIAN_POINT('Ctrl Pts',(-2.71840572200006,12.2,2.98155768799998));
#305962=CARTESIAN_POINT('Ctrl Pts',(-2.71840572200006,5.2,2.98155768799998));
#305963=CARTESIAN_POINT('Ctrl Pts',(-2.71840572200006,2.2,2.98155768799998));
#305964=CARTESIAN_POINT('Ctrl Pts',(-2.71799804400006,12.2,2.98095803099999));
#305965=CARTESIAN_POINT('Ctrl Pts',(-2.71799804400006,5.2,2.98095803099999));
#305966=CARTESIAN_POINT('Ctrl Pts',(-2.71799804400006,2.2,2.98095803099999));
#305967=CARTESIAN_POINT('Ctrl Pts',(-2.71759297000005,12.2,2.98036382599999));
#305968=CARTESIAN_POINT('Ctrl Pts',(-2.71759297000005,5.2,2.98036382599999));
#305969=CARTESIAN_POINT('Ctrl Pts',(-2.71759297000005,2.2,2.98036382599999));
#305970=CARTESIAN_POINT('Ctrl Pts',(-2.71719051700006,12.2,2.97977507499999));
#305971=CARTESIAN_POINT('Ctrl Pts',(-2.71719051700006,5.2,2.97977507499999));
#305972=CARTESIAN_POINT('Ctrl Pts',(-2.71719051700006,2.2,2.97977507499999));
#305973=CARTESIAN_POINT('Ctrl Pts',(-2.71679070600006,12.2,2.97919177799999));
#305974=CARTESIAN_POINT('Ctrl Pts',(-2.71679070600006,5.2,2.97919177799999));
#305975=CARTESIAN_POINT('Ctrl Pts',(-2.71679070600006,2.2,2.97919177799999));
#305976=CARTESIAN_POINT('Ctrl Pts',(-2.71639355500006,12.2,2.97861393899999));
#305977=CARTESIAN_POINT('Ctrl Pts',(-2.71639355500006,5.2,2.97861393899999));
#305978=CARTESIAN_POINT('Ctrl Pts',(-2.71639355500006,2.2,2.97861393899999));
#305979=CARTESIAN_POINT('Ctrl Pts',(-2.71599908200006,12.2,2.97804155899998));
#305980=CARTESIAN_POINT('Ctrl Pts',(-2.71599908200006,5.2,2.97804155899998));
#305981=CARTESIAN_POINT('Ctrl Pts',(-2.71599908200006,2.2,2.97804155899998));
#305982=CARTESIAN_POINT('Ctrl Pts',(-2.71560730900006,12.2,2.97747463999999));
#305983=CARTESIAN_POINT('Ctrl Pts',(-2.71560730900006,5.2,2.97747463999999));
#305984=CARTESIAN_POINT('Ctrl Pts',(-2.71560730900006,2.2,2.97747463999999));
#305985=CARTESIAN_POINT('Ctrl Pts',(-2.71521825300006,12.2,2.97691318299999));
#305986=CARTESIAN_POINT('Ctrl Pts',(-2.71521825300006,5.2,2.97691318299999));
#305987=CARTESIAN_POINT('Ctrl Pts',(-2.71521825300006,2.2,2.97691318299999));
#305988=CARTESIAN_POINT('Ctrl Pts',(-2.71483193400006,12.2,2.97635718999998));
#305989=CARTESIAN_POINT('Ctrl Pts',(-2.71483193400006,5.2,2.97635718999998));
#305990=CARTESIAN_POINT('Ctrl Pts',(-2.71483193400006,2.2,2.97635718999998));
#305991=CARTESIAN_POINT('Ctrl Pts',(-2.71444837100006,12.2,2.97580666399998));
#305992=CARTESIAN_POINT('Ctrl Pts',(-2.71444837100006,5.2,2.97580666399998));
#305993=CARTESIAN_POINT('Ctrl Pts',(-2.71444837100006,2.2,2.97580666399998));
#305994=CARTESIAN_POINT('Ctrl Pts',(-2.71406758200006,12.2,2.97526160499999));
#305995=CARTESIAN_POINT('Ctrl Pts',(-2.71406758200006,5.2,2.97526160499999));
#305996=CARTESIAN_POINT('Ctrl Pts',(-2.71406758200006,2.2,2.97526160499999));
#305997=CARTESIAN_POINT('Ctrl Pts',(-2.71368959000006,12.2,2.97472201499998));
#305998=CARTESIAN_POINT('Ctrl Pts',(-2.71368959000006,5.2,2.97472201499998));
#305999=CARTESIAN_POINT('Ctrl Pts',(-2.71368959000006,2.2,2.97472201499998));
#306000=CARTESIAN_POINT('Ctrl Pts',(-2.71331441200005,12.2,2.97418789699999));
#306001=CARTESIAN_POINT('Ctrl Pts',(-2.71331441200005,5.2,2.97418789699999));
#306002=CARTESIAN_POINT('Ctrl Pts',(-2.71331441200005,2.2,2.97418789699999));
#306003=CARTESIAN_POINT('Ctrl Pts',(-2.71294206700006,12.2,2.97365925099999));
#306004=CARTESIAN_POINT('Ctrl Pts',(-2.71294206700006,5.2,2.97365925099999));
#306005=CARTESIAN_POINT('Ctrl Pts',(-2.71294206700006,2.2,2.97365925099999));
#306006=CARTESIAN_POINT('Ctrl Pts',(-2.71257257700006,12.2,2.97313607899999));
#306007=CARTESIAN_POINT('Ctrl Pts',(-2.71257257700006,5.2,2.97313607899999));
#306008=CARTESIAN_POINT('Ctrl Pts',(-2.71257257700006,2.2,2.97313607899999));
#306009=CARTESIAN_POINT('Ctrl Pts',(-2.71220595900005,12.2,2.97261838399999));
#306010=CARTESIAN_POINT('Ctrl Pts',(-2.71220595900005,5.2,2.97261838399999));
#306011=CARTESIAN_POINT('Ctrl Pts',(-2.71220595900005,2.2,2.97261838399999));
#306012=CARTESIAN_POINT('Ctrl Pts',(-2.71184223500006,12.2,2.97210616599998));
#306013=CARTESIAN_POINT('Ctrl Pts',(-2.71184223500006,5.2,2.97210616599998));
#306014=CARTESIAN_POINT('Ctrl Pts',(-2.71184223500006,2.2,2.97210616599998));
#306015=CARTESIAN_POINT('Ctrl Pts',(-2.71148142300006,12.2,2.97159942699999));
#306016=CARTESIAN_POINT('Ctrl Pts',(-2.71148142300006,5.2,2.97159942699999));
#306017=CARTESIAN_POINT('Ctrl Pts',(-2.71148142300006,2.2,2.97159942699999));
#306018=CARTESIAN_POINT('Ctrl Pts',(-2.71112354500006,12.2,2.97109816899999));
#306019=CARTESIAN_POINT('Ctrl Pts',(-2.71112354500006,5.2,2.97109816899999));
#306020=CARTESIAN_POINT('Ctrl Pts',(-2.71112354500006,2.2,2.97109816899999));
#306021=CARTESIAN_POINT('Ctrl Pts',(-2.71076861900006,12.2,2.97060239299999));
#306022=CARTESIAN_POINT('Ctrl Pts',(-2.71076861900006,5.2,2.97060239299999));
#306023=CARTESIAN_POINT('Ctrl Pts',(-2.71076861900006,2.2,2.97060239299999));
#306024=CARTESIAN_POINT('Ctrl Pts',(-2.71041666500006,12.2,2.97011210099999));
#306025=CARTESIAN_POINT('Ctrl Pts',(-2.71041666500006,5.2,2.97011210099999));
#306026=CARTESIAN_POINT('Ctrl Pts',(-2.71041666500006,2.2,2.97011210099999));
#306027=CARTESIAN_POINT('Ctrl Pts',(-2.71006770400006,12.2,2.96962729299998));
#306028=CARTESIAN_POINT('Ctrl Pts',(-2.71006770400006,5.2,2.96962729299998));
#306029=CARTESIAN_POINT('Ctrl Pts',(-2.71006770400006,2.2,2.96962729299998));
#306030=CARTESIAN_POINT('Ctrl Pts',(-2.70972175600006,12.2,2.96914797299999));
#306031=CARTESIAN_POINT('Ctrl Pts',(-2.70972175600006,5.2,2.96914797299999));
#306032=CARTESIAN_POINT('Ctrl Pts',(-2.70972175600006,2.2,2.96914797299999));
#306033=CARTESIAN_POINT('Ctrl Pts',(-2.70937884100006,12.2,2.96867414099999));
#306034=CARTESIAN_POINT('Ctrl Pts',(-2.70937884100006,5.2,2.96867414099999));
#306035=CARTESIAN_POINT('Ctrl Pts',(-2.70937884100006,2.2,2.96867414099999));
#306036=CARTESIAN_POINT('Ctrl Pts',(-2.70903897900005,12.2,2.96820579799999));
#306037=CARTESIAN_POINT('Ctrl Pts',(-2.70903897900005,5.2,2.96820579799999));
#306038=CARTESIAN_POINT('Ctrl Pts',(-2.70903897900005,2.2,2.96820579799999));
#306039=CARTESIAN_POINT('Ctrl Pts',(-2.70870219000006,12.2,2.96774294599999));
#306040=CARTESIAN_POINT('Ctrl Pts',(-2.70870219000006,5.2,2.96774294599999));
#306041=CARTESIAN_POINT('Ctrl Pts',(-2.70870219000006,2.2,2.96774294599999));
#306042=CARTESIAN_POINT('Ctrl Pts',(-2.70836849500005,12.2,2.96728558799998));
#306043=CARTESIAN_POINT('Ctrl Pts',(-2.70836849500005,5.2,2.96728558799998));
#306044=CARTESIAN_POINT('Ctrl Pts',(-2.70836849500005,2.2,2.96728558799998));
#306045=CARTESIAN_POINT('Ctrl Pts',(-2.70803791400006,12.2,2.96683372199999));
#306046=CARTESIAN_POINT('Ctrl Pts',(-2.70803791400006,5.2,2.96683372199999));
#306047=CARTESIAN_POINT('Ctrl Pts',(-2.70803791400006,2.2,2.96683372199999));
#306048=CARTESIAN_POINT('Ctrl Pts',(-2.70771046800005,12.2,2.96638735199998));
#306049=CARTESIAN_POINT('Ctrl Pts',(-2.70771046800005,5.2,2.96638735199998));
#306050=CARTESIAN_POINT('Ctrl Pts',(-2.70771046800005,2.2,2.96638735199998));
#306051=CARTESIAN_POINT('Ctrl Pts',(-2.70738617800005,12.2,2.96594647899998));
#306052=CARTESIAN_POINT('Ctrl Pts',(-2.70738617800005,5.2,2.96594647899998));
#306053=CARTESIAN_POINT('Ctrl Pts',(-2.70738617800005,2.2,2.96594647899998));
#306054=CARTESIAN_POINT('Ctrl Pts',(-2.70706506300006,12.2,2.96551110199999));
#306055=CARTESIAN_POINT('Ctrl Pts',(-2.70706506300006,5.2,2.96551110199999));
#306056=CARTESIAN_POINT('Ctrl Pts',(-2.70706506300006,2.2,2.96551110199999));
#306057=CARTESIAN_POINT('Ctrl Pts',(-2.70674714400006,12.2,2.96508122599998));
#306058=CARTESIAN_POINT('Ctrl Pts',(-2.70674714400006,5.2,2.96508122599998));
#306059=CARTESIAN_POINT('Ctrl Pts',(-2.70674714400006,2.2,2.96508122599998));
#306060=CARTESIAN_POINT('Ctrl Pts',(-2.70643244300006,12.2,2.96465684899999));
#306061=CARTESIAN_POINT('Ctrl Pts',(-2.70643244300006,5.2,2.96465684899999));
#306062=CARTESIAN_POINT('Ctrl Pts',(-2.70643244300006,2.2,2.96465684899999));
#306063=CARTESIAN_POINT('Ctrl Pts',(-2.70612098000006,12.2,2.96423797499998));
#306064=CARTESIAN_POINT('Ctrl Pts',(-2.70612098000006,5.2,2.96423797499998));
#306065=CARTESIAN_POINT('Ctrl Pts',(-2.70612098000006,2.2,2.96423797499998));
#306066=CARTESIAN_POINT('Ctrl Pts',(-2.70581277600006,12.2,2.96382460299998));
#306067=CARTESIAN_POINT('Ctrl Pts',(-2.70581277600006,5.2,2.96382460299998));
#306068=CARTESIAN_POINT('Ctrl Pts',(-2.70581277600006,2.2,2.96382460299998));
#306069=CARTESIAN_POINT('Ctrl Pts',(-2.70550785200005,12.2,2.96341673499998));
#306070=CARTESIAN_POINT('Ctrl Pts',(-2.70550785200005,5.2,2.96341673499998));
#306071=CARTESIAN_POINT('Ctrl Pts',(-2.70550785200005,2.2,2.96341673499998));
#306072=CARTESIAN_POINT('Ctrl Pts',(-2.70520622700006,12.2,2.96301437299999));
#306073=CARTESIAN_POINT('Ctrl Pts',(-2.70520622700006,5.2,2.96301437299999));
#306074=CARTESIAN_POINT('Ctrl Pts',(-2.70520622700006,2.2,2.96301437299999));
#306075=CARTESIAN_POINT('Ctrl Pts',(-2.70490792600006,12.2,2.96261751699999));
#306076=CARTESIAN_POINT('Ctrl Pts',(-2.70490792600006,5.2,2.96261751699999));
#306077=CARTESIAN_POINT('Ctrl Pts',(-2.70490792600006,2.2,2.96261751699999));
#306078=CARTESIAN_POINT('Ctrl Pts',(-2.70461296800006,12.2,2.96222616899998));
#306079=CARTESIAN_POINT('Ctrl Pts',(-2.70461296800006,5.2,2.96222616899998));
#306080=CARTESIAN_POINT('Ctrl Pts',(-2.70461296800006,2.2,2.96222616899998));
#306081=CARTESIAN_POINT('Ctrl Pts',(-2.70432137400006,12.2,2.96184032999999));
#306082=CARTESIAN_POINT('Ctrl Pts',(-2.70432137400006,5.2,2.96184032999999));
#306083=CARTESIAN_POINT('Ctrl Pts',(-2.70432137400006,2.2,2.96184032999999));
#306084=CARTESIAN_POINT('Ctrl Pts',(-2.70403316500006,12.2,2.96145999999998));
#306085=CARTESIAN_POINT('Ctrl Pts',(-2.70403316500006,5.2,2.96145999999998));
#306086=CARTESIAN_POINT('Ctrl Pts',(-2.70403316500006,2.2,2.96145999999998));
#306087=CARTESIAN_POINT('Ctrl Pts',(-2.70374836300005,12.2,2.96108518199999));
#306088=CARTESIAN_POINT('Ctrl Pts',(-2.70374836300005,5.2,2.96108518199999));
#306089=CARTESIAN_POINT('Ctrl Pts',(-2.70374836300005,2.2,2.96108518199999));
#306090=CARTESIAN_POINT('Ctrl Pts',(-2.70346699000005,12.2,2.96071587499998));
#306091=CARTESIAN_POINT('Ctrl Pts',(-2.70346699000005,5.2,2.96071587499998));
#306092=CARTESIAN_POINT('Ctrl Pts',(-2.70346699000005,2.2,2.96071587499998));
#306093=CARTESIAN_POINT('Ctrl Pts',(-2.70318906600005,12.2,2.96035208099998));
#306094=CARTESIAN_POINT('Ctrl Pts',(-2.70318906600005,5.2,2.96035208099998));
#306095=CARTESIAN_POINT('Ctrl Pts',(-2.70318906600005,2.2,2.96035208099998));
#306096=CARTESIAN_POINT('Ctrl Pts',(-2.70291461400006,12.2,2.95999380199999));
#306097=CARTESIAN_POINT('Ctrl Pts',(-2.70291461400006,5.2,2.95999380199999));
#306098=CARTESIAN_POINT('Ctrl Pts',(-2.70291461400006,2.2,2.95999380199999));
#306099=CARTESIAN_POINT('Ctrl Pts',(-2.70264365500006,12.2,2.95964103799999));
#306100=CARTESIAN_POINT('Ctrl Pts',(-2.70264365500006,5.2,2.95964103799999));
#306101=CARTESIAN_POINT('Ctrl Pts',(-2.70264365500006,2.2,2.95964103799999));
#306102=CARTESIAN_POINT('Ctrl Pts',(-2.70237621000006,12.2,2.95929378999999));
#306103=CARTESIAN_POINT('Ctrl Pts',(-2.70237621000006,5.2,2.95929378999999));
#306104=CARTESIAN_POINT('Ctrl Pts',(-2.70237621000006,2.2,2.95929378999999));
#306105=CARTESIAN_POINT('Ctrl Pts',(-2.70211230200006,12.2,2.95895205899999));
#306106=CARTESIAN_POINT('Ctrl Pts',(-2.70211230200006,5.2,2.95895205899999));
#306107=CARTESIAN_POINT('Ctrl Pts',(-2.70211230200006,2.2,2.95895205899999));
#306108=CARTESIAN_POINT('Ctrl Pts',(-2.70185195200006,12.2,2.95861584499999));
#306109=CARTESIAN_POINT('Ctrl Pts',(-2.70185195200006,5.2,2.95861584499999));
#306110=CARTESIAN_POINT('Ctrl Pts',(-2.70185195200006,2.2,2.95861584499999));
#306111=CARTESIAN_POINT('Ctrl Pts',(-2.70159518200006,12.2,2.95828515199998));
#306112=CARTESIAN_POINT('Ctrl Pts',(-2.70159518200006,5.2,2.95828515199998));
#306113=CARTESIAN_POINT('Ctrl Pts',(-2.70159518200006,2.2,2.95828515199998));
#306114=CARTESIAN_POINT('Ctrl Pts',(-2.70134201400006,12.2,2.95795997799999));
#306115=CARTESIAN_POINT('Ctrl Pts',(-2.70134201400006,5.2,2.95795997799999));
#306116=CARTESIAN_POINT('Ctrl Pts',(-2.70134201400006,2.2,2.95795997799999));
#306117=CARTESIAN_POINT('Ctrl Pts',(-2.70109247100006,12.2,2.95764032399998));
#306118=CARTESIAN_POINT('Ctrl Pts',(-2.70109247100006,5.2,2.95764032399998));
#306119=CARTESIAN_POINT('Ctrl Pts',(-2.70109247100006,2.2,2.95764032399998));
#306120=CARTESIAN_POINT('Ctrl Pts',(-2.70084657300006,12.2,2.95732619099999));
#306121=CARTESIAN_POINT('Ctrl Pts',(-2.70084657300006,5.2,2.95732619099999));
#306122=CARTESIAN_POINT('Ctrl Pts',(-2.70084657300006,2.2,2.95732619099999));
#306123=CARTESIAN_POINT('Ctrl Pts',(-2.70060434500006,12.2,2.95701758199999));
#306124=CARTESIAN_POINT('Ctrl Pts',(-2.70060434500006,5.2,2.95701758199999));
#306125=CARTESIAN_POINT('Ctrl Pts',(-2.70060434500006,2.2,2.95701758199999));
#306126=CARTESIAN_POINT('Ctrl Pts',(-2.70036580700005,12.2,2.95671449499999));
#306127=CARTESIAN_POINT('Ctrl Pts',(-2.70036580700005,5.2,2.95671449499999));
#306128=CARTESIAN_POINT('Ctrl Pts',(-2.70036580700005,2.2,2.95671449499999));
#306129=CARTESIAN_POINT('Ctrl Pts',(-2.70013098200006,12.2,2.95641693199999));
#306130=CARTESIAN_POINT('Ctrl Pts',(-2.70013098200006,5.2,2.95641693199999));
#306131=CARTESIAN_POINT('Ctrl Pts',(-2.70013098200006,2.2,2.95641693199999));
#306132=CARTESIAN_POINT('Ctrl Pts',(-2.69989989300006,12.2,2.95612489399999));
#306133=CARTESIAN_POINT('Ctrl Pts',(-2.69989989300006,5.2,2.95612489399999));
#306134=CARTESIAN_POINT('Ctrl Pts',(-2.69989989300006,2.2,2.95612489399999));
#306135=CARTESIAN_POINT('Ctrl Pts',(-2.69967256100006,12.2,2.95583838199998));
#306136=CARTESIAN_POINT('Ctrl Pts',(-2.69967256100006,5.2,2.95583838199998));
#306137=CARTESIAN_POINT('Ctrl Pts',(-2.69967256100006,2.2,2.95583838199998));
#306138=CARTESIAN_POINT('Ctrl Pts',(-2.69944901000006,12.2,2.95555739599998));
#306139=CARTESIAN_POINT('Ctrl Pts',(-2.69944901000006,5.2,2.95555739599998));
#306140=CARTESIAN_POINT('Ctrl Pts',(-2.69944901000006,2.2,2.95555739599998));
#306141=CARTESIAN_POINT('Ctrl Pts',(-2.69922926300006,12.2,2.95528193599999));
#306142=CARTESIAN_POINT('Ctrl Pts',(-2.69922926300006,5.2,2.95528193599999));
#306143=CARTESIAN_POINT('Ctrl Pts',(-2.69922926300006,2.2,2.95528193599999));
#306144=CARTESIAN_POINT('Ctrl Pts',(-2.69901334100005,12.2,2.95501200399999));
#306145=CARTESIAN_POINT('Ctrl Pts',(-2.69901334100005,5.2,2.95501200399999));
#306146=CARTESIAN_POINT('Ctrl Pts',(-2.69901334100005,2.2,2.95501200399999));
#306147=CARTESIAN_POINT('Ctrl Pts',(-2.69880126900006,12.2,2.95474759999999));
#306148=CARTESIAN_POINT('Ctrl Pts',(-2.69880126900006,5.2,2.95474759999999));
#306149=CARTESIAN_POINT('Ctrl Pts',(-2.69880126900006,2.2,2.95474759999999));
#306150=CARTESIAN_POINT('Ctrl Pts',(-2.69859306800006,12.2,2.95448872499998));
#306151=CARTESIAN_POINT('Ctrl Pts',(-2.69859306800006,5.2,2.95448872499998));
#306152=CARTESIAN_POINT('Ctrl Pts',(-2.69859306800006,2.2,2.95448872499998));
#306153=CARTESIAN_POINT('Ctrl Pts',(-2.69838876100006,12.2,2.95423537899998));
#306154=CARTESIAN_POINT('Ctrl Pts',(-2.69838876100006,5.2,2.95423537899998));
#306155=CARTESIAN_POINT('Ctrl Pts',(-2.69838876100006,2.2,2.95423537899998));
#306156=CARTESIAN_POINT('Ctrl Pts',(-2.69818837200006,12.2,2.95398756299999));
#306157=CARTESIAN_POINT('Ctrl Pts',(-2.69818837200006,5.2,2.95398756299999));
#306158=CARTESIAN_POINT('Ctrl Pts',(-2.69818837200006,2.2,2.95398756299999));
#306159=CARTESIAN_POINT('Ctrl Pts',(-2.69799192300006,12.2,2.95374527799999));
#306160=CARTESIAN_POINT('Ctrl Pts',(-2.69799192300006,5.2,2.95374527799999));
#306161=CARTESIAN_POINT('Ctrl Pts',(-2.69799192300006,2.2,2.95374527799999));
#306162=CARTESIAN_POINT('Ctrl Pts',(-2.69779943900006,12.2,2.95350852299999));
#306163=CARTESIAN_POINT('Ctrl Pts',(-2.69779943900006,5.2,2.95350852299999));
#306164=CARTESIAN_POINT('Ctrl Pts',(-2.69779943900006,2.2,2.95350852299999));
#306165=CARTESIAN_POINT('Ctrl Pts',(-2.69761094200006,12.2,2.95327730099999));
#306166=CARTESIAN_POINT('Ctrl Pts',(-2.69761094200006,5.2,2.95327730099999));
#306167=CARTESIAN_POINT('Ctrl Pts',(-2.69761094200006,2.2,2.95327730099999));
#306168=CARTESIAN_POINT('Ctrl Pts',(-2.69742645500005,12.2,2.95305160899999));
#306169=CARTESIAN_POINT('Ctrl Pts',(-2.69742645500005,5.2,2.95305160899999));
#306170=CARTESIAN_POINT('Ctrl Pts',(-2.69742645500005,2.2,2.95305160899999));
#306171=CARTESIAN_POINT('Ctrl Pts',(-2.69724600200006,12.2,2.95283144999999));
#306172=CARTESIAN_POINT('Ctrl Pts',(-2.69724600200006,5.2,2.95283144999999));
#306173=CARTESIAN_POINT('Ctrl Pts',(-2.69724600200006,2.2,2.95283144999999));
#306174=CARTESIAN_POINT('Ctrl Pts',(-2.69706960600006,12.2,2.95261682499999));
#306175=CARTESIAN_POINT('Ctrl Pts',(-2.69706960600006,5.2,2.95261682499999));
#306176=CARTESIAN_POINT('Ctrl Pts',(-2.69706960600006,2.2,2.95261682499999));
#306177=CARTESIAN_POINT('Ctrl Pts',(-2.69689729100006,12.2,2.95240773199998));
#306178=CARTESIAN_POINT('Ctrl Pts',(-2.69689729100006,5.2,2.95240773199998));
#306179=CARTESIAN_POINT('Ctrl Pts',(-2.69689729100006,2.2,2.95240773199998));
#306180=CARTESIAN_POINT('Ctrl Pts',(-2.69672908200006,12.2,2.95220417299999));
#306181=CARTESIAN_POINT('Ctrl Pts',(-2.69672908200006,5.2,2.95220417299999));
#306182=CARTESIAN_POINT('Ctrl Pts',(-2.69672908200006,2.2,2.95220417299999));
#306183=CARTESIAN_POINT('Ctrl Pts',(-2.69656500100006,12.2,2.95200614799998));
#306184=CARTESIAN_POINT('Ctrl Pts',(-2.69656500100006,5.2,2.95200614799998));
#306185=CARTESIAN_POINT('Ctrl Pts',(-2.69656500100006,2.2,2.95200614799998));
#306186=CARTESIAN_POINT('Ctrl Pts',(-2.69640507100006,12.2,2.95181365599999));
#306187=CARTESIAN_POINT('Ctrl Pts',(-2.69640507100006,5.2,2.95181365599999));
#306188=CARTESIAN_POINT('Ctrl Pts',(-2.69640507100006,2.2,2.95181365599999));
#306189=CARTESIAN_POINT('Ctrl Pts',(-2.69624931800006,12.2,2.95162669999999));
#306190=CARTESIAN_POINT('Ctrl Pts',(-2.69624931800006,5.2,2.95162669999999));
#306191=CARTESIAN_POINT('Ctrl Pts',(-2.69624931800006,2.2,2.95162669999999));
#306192=CARTESIAN_POINT('Ctrl Pts',(-2.69609776600006,12.2,2.95144527899998));
#306193=CARTESIAN_POINT('Ctrl Pts',(-2.69609776600006,5.2,2.95144527899998));
#306194=CARTESIAN_POINT('Ctrl Pts',(-2.69609776600006,2.2,2.95144527899998));
#306195=CARTESIAN_POINT('Ctrl Pts',(-2.69595043700006,12.2,2.95126939199999));
#306196=CARTESIAN_POINT('Ctrl Pts',(-2.69595043700006,5.2,2.95126939199999));
#306197=CARTESIAN_POINT('Ctrl Pts',(-2.69595043700006,2.2,2.95126939199999));
#306198=CARTESIAN_POINT('Ctrl Pts',(-2.69580735700006,12.2,2.95109904099998));
#306199=CARTESIAN_POINT('Ctrl Pts',(-2.69580735700006,5.2,2.95109904099998));
#306200=CARTESIAN_POINT('Ctrl Pts',(-2.69580735700006,2.2,2.95109904099998));
#306201=CARTESIAN_POINT('Ctrl Pts',(-2.69566854800006,12.2,2.95093422599999));
#306202=CARTESIAN_POINT('Ctrl Pts',(-2.69566854800006,5.2,2.95093422599999));
#306203=CARTESIAN_POINT('Ctrl Pts',(-2.69566854800006,2.2,2.95093422599999));
#306204=CARTESIAN_POINT('Ctrl Pts',(-2.69553403700006,12.2,2.95077494499999));
#306205=CARTESIAN_POINT('Ctrl Pts',(-2.69553403700006,5.2,2.95077494499999));
#306206=CARTESIAN_POINT('Ctrl Pts',(-2.69553403700006,2.2,2.95077494499999));
#306207=CARTESIAN_POINT('Ctrl Pts',(-2.69540384800006,12.2,2.95062120099999));
#306208=CARTESIAN_POINT('Ctrl Pts',(-2.69540384800006,5.2,2.95062120099999));
#306209=CARTESIAN_POINT('Ctrl Pts',(-2.69540384800006,2.2,2.95062120099999));
#306210=CARTESIAN_POINT('Ctrl Pts',(-2.69527800600006,12.2,2.95047299199998));
#306211=CARTESIAN_POINT('Ctrl Pts',(-2.69527800600006,5.2,2.95047299199998));
#306212=CARTESIAN_POINT('Ctrl Pts',(-2.69527800600006,2.2,2.95047299199998));
#306213=CARTESIAN_POINT('Ctrl Pts',(-2.69515653400005,12.2,2.95033031999999));
#306214=CARTESIAN_POINT('Ctrl Pts',(-2.69515653400005,5.2,2.95033031999999));
#306215=CARTESIAN_POINT('Ctrl Pts',(-2.69515653400005,2.2,2.95033031999999));
#306216=CARTESIAN_POINT('Ctrl Pts',(-2.69503945700006,12.2,2.95019318299998));
#306217=CARTESIAN_POINT('Ctrl Pts',(-2.69503945700006,5.2,2.95019318299998));
#306218=CARTESIAN_POINT('Ctrl Pts',(-2.69503945700006,2.2,2.95019318299998));
#306219=CARTESIAN_POINT('Ctrl Pts',(-2.69492680000006,12.2,2.95006158399998));
#306220=CARTESIAN_POINT('Ctrl Pts',(-2.69492680000006,5.2,2.95006158399998));
#306221=CARTESIAN_POINT('Ctrl Pts',(-2.69492680000006,2.2,2.95006158399998));
#306222=CARTESIAN_POINT('Ctrl Pts',(-2.69481858700006,12.2,2.94993551899999));
#306223=CARTESIAN_POINT('Ctrl Pts',(-2.69481858700006,5.2,2.94993551899999));
#306224=CARTESIAN_POINT('Ctrl Pts',(-2.69481858700006,2.2,2.94993551899999));
#306225=CARTESIAN_POINT('Ctrl Pts',(-2.69471484200006,12.2,2.94981499099999));
#306226=CARTESIAN_POINT('Ctrl Pts',(-2.69471484200006,5.2,2.94981499099999));
#306227=CARTESIAN_POINT('Ctrl Pts',(-2.69471484200006,2.2,2.94981499099999));
#306228=CARTESIAN_POINT('Ctrl Pts',(-2.69461559200006,12.2,2.94969999899998));
#306229=CARTESIAN_POINT('Ctrl Pts',(-2.69461559200006,5.2,2.94969999899998));
#306230=CARTESIAN_POINT('Ctrl Pts',(-2.69461559200006,2.2,2.94969999899998));
#306231=CARTESIAN_POINT('Ctrl Pts',(-2.69452086300006,12.2,2.94959054299999));
#306232=CARTESIAN_POINT('Ctrl Pts',(-2.69452086300006,5.2,2.94959054299999));
#306233=CARTESIAN_POINT('Ctrl Pts',(-2.69452086300006,2.2,2.94959054299999));
#306234=CARTESIAN_POINT('Ctrl Pts',(-2.69443068000006,12.2,2.94948662199998));
#306235=CARTESIAN_POINT('Ctrl Pts',(-2.69443068000006,5.2,2.94948662199998));
#306236=CARTESIAN_POINT('Ctrl Pts',(-2.69443068000006,2.2,2.94948662199998));
#306237=CARTESIAN_POINT('Ctrl Pts',(-2.69434507100006,12.2,2.94938823799999));
#306238=CARTESIAN_POINT('Ctrl Pts',(-2.69434507100006,5.2,2.94938823799999));
#306239=CARTESIAN_POINT('Ctrl Pts',(-2.69434507100006,2.2,2.94938823799999));
#306240=CARTESIAN_POINT('Ctrl Pts',(-2.69426406000006,12.2,2.94929538899999));
#306241=CARTESIAN_POINT('Ctrl Pts',(-2.69426406000006,5.2,2.94929538899999));
#306242=CARTESIAN_POINT('Ctrl Pts',(-2.69426406000006,2.2,2.94929538899999));
#306243=CARTESIAN_POINT('Ctrl Pts',(-2.69418766900006,12.2,2.94920807499999));
#306244=CARTESIAN_POINT('Ctrl Pts',(-2.69418766900006,5.2,2.94920807499999));
#306245=CARTESIAN_POINT('Ctrl Pts',(-2.69418766900006,2.2,2.94920807499999));
#306246=CARTESIAN_POINT('Ctrl Pts',(-2.69411592200006,12.2,2.94912629699999));
#306247=CARTESIAN_POINT('Ctrl Pts',(-2.69411592200006,5.2,2.94912629699999));
#306248=CARTESIAN_POINT('Ctrl Pts',(-2.69411592200006,2.2,2.94912629699999));
#306249=CARTESIAN_POINT('Ctrl Pts',(-2.69404884200006,12.2,2.94905005299999));
#306250=CARTESIAN_POINT('Ctrl Pts',(-2.69404884200006,5.2,2.94905005299999));
#306251=CARTESIAN_POINT('Ctrl Pts',(-2.69404884200006,2.2,2.94905005299999));
#306252=CARTESIAN_POINT('Ctrl Pts',(-2.69398645600006,12.2,2.94897934399999));
#306253=CARTESIAN_POINT('Ctrl Pts',(-2.69398645600006,5.2,2.94897934399999));
#306254=CARTESIAN_POINT('Ctrl Pts',(-2.69398645600006,2.2,2.94897934399999));
#306255=CARTESIAN_POINT('Ctrl Pts',(-2.69392879100006,12.2,2.94891416999998));
#306256=CARTESIAN_POINT('Ctrl Pts',(-2.69392879100006,5.2,2.94891416999998));
#306257=CARTESIAN_POINT('Ctrl Pts',(-2.69392879100006,2.2,2.94891416999998));
#306258=CARTESIAN_POINT('Ctrl Pts',(-2.69387588400006,12.2,2.94885452999999));
#306259=CARTESIAN_POINT('Ctrl Pts',(-2.69387588400006,5.2,2.94885452999999));
#306260=CARTESIAN_POINT('Ctrl Pts',(-2.69387588400006,2.2,2.94885452999999));
#306261=CARTESIAN_POINT('Ctrl Pts',(-2.69382776600006,12.2,2.94880042199999));
#306262=CARTESIAN_POINT('Ctrl Pts',(-2.69382776600006,5.2,2.94880042199999));
#306263=CARTESIAN_POINT('Ctrl Pts',(-2.69382776600006,2.2,2.94880042199999));
#306264=CARTESIAN_POINT('Ctrl Pts',(-2.69378446300006,12.2,2.94875184899999));
#306265=CARTESIAN_POINT('Ctrl Pts',(-2.69378446300006,5.2,2.94875184899999));
#306266=CARTESIAN_POINT('Ctrl Pts',(-2.69378446300006,2.2,2.94875184899999));
#306267=CARTESIAN_POINT('Ctrl Pts',(-2.69374600100006,12.2,2.94870880699998));
#306268=CARTESIAN_POINT('Ctrl Pts',(-2.69374600100006,5.2,2.94870880699998));
#306269=CARTESIAN_POINT('Ctrl Pts',(-2.69374600100006,2.2,2.94870880699998));
#306270=CARTESIAN_POINT('Ctrl Pts',(-2.69370879074423,12.2,2.94866728366678));
#306271=CARTESIAN_POINT('Ctrl Pts',(-2.69370879074423,5.2,2.94866728366678));
#306272=CARTESIAN_POINT('Ctrl Pts',(-2.69370879074423,2.2,2.94866728366678));
#306273=CARTESIAN_POINT('Ctrl Pts',(-2.69368329797707,12.2,2.94863895095595));
#306274=CARTESIAN_POINT('Ctrl Pts',(-2.69368329797707,5.2,2.94863895095595));
#306275=CARTESIAN_POINT('Ctrl Pts',(-2.69368329797707,2.2,2.94863895095595));
#306276=CARTESIAN_POINT('Ctrl Pts',(-2.69366646359,12.2,2.94862032138212));
#306277=CARTESIAN_POINT('Ctrl Pts',(-2.69366646359,5.2,2.94862032138212));
#306278=CARTESIAN_POINT('Ctrl Pts',(-2.69366646359,2.2,2.94862032138212));
#306279=CARTESIAN_POINT('Ctrl Pts',(-2.69365595548621,12.2,2.9486087420261));
#306280=CARTESIAN_POINT('Ctrl Pts',(-2.69365595548621,5.2,2.9486087420261));
#306281=CARTESIAN_POINT('Ctrl Pts',(-2.69365595548621,2.2,2.9486087420261));
#306282=CARTESIAN_POINT('Ctrl Pts',(-2.69364946500006,12.2,2.94860158799998));
#306283=CARTESIAN_POINT('Ctrl Pts',(-2.69364946500006,5.2,2.94860158799998));
#306284=CARTESIAN_POINT('Ctrl Pts',(-2.69364946500006,2.2,2.94860158799998));
#306285=CARTESIAN_POINT('',(-2.69364961400006,2.7,2.94860145299998));
#306286=CARTESIAN_POINT('',(-2.69364961400006,12.2,2.94860145299998));
#306287=CARTESIAN_POINT('Ctrl Pts',(-2.94378355400006,2.7,3.72781952199999));
#306288=CARTESIAN_POINT('Ctrl Pts',(-2.919025134039,2.7,3.47165304727227));
#306289=CARTESIAN_POINT('Ctrl Pts',(-2.86296672116152,2.7,3.28773125003828));
#306290=CARTESIAN_POINT('Ctrl Pts',(-2.75669794542552,2.7,3.02504202830561));
#306291=CARTESIAN_POINT('Ctrl Pts',(-2.70202149940583,2.7,2.95807419909088));
#306292=CARTESIAN_POINT('Ctrl Pts',(-2.69387506136249,2.7,2.94885330493632));
#306293=CARTESIAN_POINT('Ctrl Pts',(-2.69376302502467,2.7,2.94872675757333));
#306294=CARTESIAN_POINT('Ctrl Pts',(-2.69364946500006,2.7,2.94860158799998));
#306295=CARTESIAN_POINT('Origin',(-2.69361500300006,15.2,2.94856356499999));
#306296=CARTESIAN_POINT('',(-2.44494327000006,2.7,2.67635524699998));
#306297=CARTESIAN_POINT('',(-2.44494327000006,2.2,2.67635524699998));
#306298=CARTESIAN_POINT('',(-1.34680750196728,2.7,1.47428178207316));
#306299=CARTESIAN_POINT('Origin',(-5.66300478732629E-14,15.2,-1.77635683940025E-14));
#306300=CARTESIAN_POINT('',(-2.82878727700006,2.7,2.26684528399998));
#306301=CARTESIAN_POINT('',(-2.82878727700006,12.2,2.26684528399999));
#306302=CARTESIAN_POINT('Origin',(-5.66300478732629E-14,2.7,-1.92943768261394E-14));
#306303=CARTESIAN_POINT('Origin',(-5.66300478732629E-14,15.2,-1.77635683940025E-14));
#306304=CARTESIAN_POINT('',(-3.11652594000006,2.7,2.49742431399999));
#306305=CARTESIAN_POINT('',(-3.11652594000006,12.2,2.49742431399999));
#306306=CARTESIAN_POINT('',(-5.70184935903678E-14,2.7,-1.89830963177552E-14));
#306307=CARTESIAN_POINT('Ctrl Pts',(-3.11652602400006,12.2,2.49742420799999));
#306308=CARTESIAN_POINT('Ctrl Pts',(-3.11652602400006,5.2,2.49742420799999));
#306309=CARTESIAN_POINT('Ctrl Pts',(-3.11652602400006,2.2,2.49742420799999));
#306310=CARTESIAN_POINT('Ctrl Pts',(-3.11653137956376,12.2,2.49742846665313));
#306311=CARTESIAN_POINT('Ctrl Pts',(-3.11653137956376,5.2,2.49742846665313));
#306312=CARTESIAN_POINT('Ctrl Pts',(-3.11653137956376,2.2,2.49742846665313));
#306313=CARTESIAN_POINT('Ctrl Pts',(-3.11654173911751,12.2,2.49743670245955));
#306314=CARTESIAN_POINT('Ctrl Pts',(-3.11654173911751,5.2,2.49743670245955));
#306315=CARTESIAN_POINT('Ctrl Pts',(-3.11654173911751,2.2,2.49743670245955));
#306316=CARTESIAN_POINT('Ctrl Pts',(-3.1165571021189,12.2,2.49744892153641));
#306317=CARTESIAN_POINT('Ctrl Pts',(-3.1165571021189,5.19999999999999,2.49744892153641));
#306318=CARTESIAN_POINT('Ctrl Pts',(-3.1165571021189,2.2,2.49744892153641));
#306319=CARTESIAN_POINT('Ctrl Pts',(-3.1165774474675,12.2,2.49746508885391));
#306320=CARTESIAN_POINT('Ctrl Pts',(-3.1165774474675,5.2,2.49746508885391));
#306321=CARTESIAN_POINT('Ctrl Pts',(-3.1165774474675,2.2,2.49746508885391));
#306322=CARTESIAN_POINT('Ctrl Pts',(-3.11661304600006,12.2,2.49749314099999));
#306323=CARTESIAN_POINT('Ctrl Pts',(-3.11661304600006,5.2,2.49749314099999));
#306324=CARTESIAN_POINT('Ctrl Pts',(-3.11661304600006,2.2,2.49749314099999));
#306325=CARTESIAN_POINT('Ctrl Pts',(-3.11665264900005,12.2,2.49752425699998));
#306326=CARTESIAN_POINT('Ctrl Pts',(-3.11665264900005,5.2,2.49752425699998));
#306327=CARTESIAN_POINT('Ctrl Pts',(-3.11665264900005,2.2,2.49752425699998));
#306328=CARTESIAN_POINT('Ctrl Pts',(-3.11669808600006,12.2,2.49755985799998));
#306329=CARTESIAN_POINT('Ctrl Pts',(-3.11669808600006,5.2,2.49755985799998));
#306330=CARTESIAN_POINT('Ctrl Pts',(-3.11669808600006,2.2,2.49755985799998));
#306331=CARTESIAN_POINT('Ctrl Pts',(-3.11674935600006,12.2,2.49759992999999));
#306332=CARTESIAN_POINT('Ctrl Pts',(-3.11674935600006,5.2,2.49759992999999));
#306333=CARTESIAN_POINT('Ctrl Pts',(-3.11674935600006,2.2,2.49759992999999));
#306334=CARTESIAN_POINT('Ctrl Pts',(-3.11680646000006,12.2,2.49764445099999));
#306335=CARTESIAN_POINT('Ctrl Pts',(-3.11680646000006,5.2,2.49764445099999));
#306336=CARTESIAN_POINT('Ctrl Pts',(-3.11680646000006,2.2,2.49764445099999));
#306337=CARTESIAN_POINT('Ctrl Pts',(-3.11686939600006,12.2,2.49769339299998));
#306338=CARTESIAN_POINT('Ctrl Pts',(-3.11686939600006,5.2,2.49769339299998));
#306339=CARTESIAN_POINT('Ctrl Pts',(-3.11686939600006,2.2,2.49769339299998));
#306340=CARTESIAN_POINT('Ctrl Pts',(-3.11693816100005,12.2,2.49774672399998));
#306341=CARTESIAN_POINT('Ctrl Pts',(-3.11693816100005,5.2,2.49774672399998));
#306342=CARTESIAN_POINT('Ctrl Pts',(-3.11693816100005,2.2,2.49774672399998));
#306343=CARTESIAN_POINT('Ctrl Pts',(-3.11701275400006,12.2,2.49780440899999));
#306344=CARTESIAN_POINT('Ctrl Pts',(-3.11701275400006,5.2,2.49780440899999));
#306345=CARTESIAN_POINT('Ctrl Pts',(-3.11701275400006,2.2,2.49780440899999));
#306346=CARTESIAN_POINT('Ctrl Pts',(-3.11709317400005,12.2,2.49786642099998));
#306347=CARTESIAN_POINT('Ctrl Pts',(-3.11709317400005,5.2,2.49786642099998));
#306348=CARTESIAN_POINT('Ctrl Pts',(-3.11709317400005,2.2,2.49786642099998));
#306349=CARTESIAN_POINT('Ctrl Pts',(-3.11717941900006,12.2,2.49793273199998));
#306350=CARTESIAN_POINT('Ctrl Pts',(-3.11717941900006,5.2,2.49793273199998));
#306351=CARTESIAN_POINT('Ctrl Pts',(-3.11717941900006,2.2,2.49793273199998));
#306352=CARTESIAN_POINT('Ctrl Pts',(-3.11727148800006,12.2,2.49800331999998));
#306353=CARTESIAN_POINT('Ctrl Pts',(-3.11727148800006,5.2,2.49800331999998));
#306354=CARTESIAN_POINT('Ctrl Pts',(-3.11727148800006,2.2,2.49800331999998));
#306355=CARTESIAN_POINT('Ctrl Pts',(-3.11736937900006,12.2,2.49807816099998));
#306356=CARTESIAN_POINT('Ctrl Pts',(-3.11736937900006,5.2,2.49807816099998));
#306357=CARTESIAN_POINT('Ctrl Pts',(-3.11736937900006,2.2,2.49807816099998));
#306358=CARTESIAN_POINT('Ctrl Pts',(-3.11747309100005,12.2,2.49815723099999));
#306359=CARTESIAN_POINT('Ctrl Pts',(-3.11747309100005,5.2,2.49815723099999));
#306360=CARTESIAN_POINT('Ctrl Pts',(-3.11747309100005,2.2,2.49815723099999));
#306361=CARTESIAN_POINT('Ctrl Pts',(-3.11758262300006,12.2,2.49824050899999));
#306362=CARTESIAN_POINT('Ctrl Pts',(-3.11758262300006,5.2,2.49824050899999));
#306363=CARTESIAN_POINT('Ctrl Pts',(-3.11758262300006,2.2,2.49824050899999));
#306364=CARTESIAN_POINT('Ctrl Pts',(-3.11769797300005,12.2,2.49832796499999));
#306365=CARTESIAN_POINT('Ctrl Pts',(-3.11769797300005,5.2,2.49832796499999));
#306366=CARTESIAN_POINT('Ctrl Pts',(-3.11769797300005,2.2,2.49832796499999));
#306367=CARTESIAN_POINT('Ctrl Pts',(-3.11781913900006,12.2,2.49841957499999));
#306368=CARTESIAN_POINT('Ctrl Pts',(-3.11781913900006,5.2,2.49841957499999));
#306369=CARTESIAN_POINT('Ctrl Pts',(-3.11781913900006,2.2,2.49841957499999));
#306370=CARTESIAN_POINT('Ctrl Pts',(-3.11794612100006,12.2,2.49851531299999));
#306371=CARTESIAN_POINT('Ctrl Pts',(-3.11794612100006,5.2,2.49851531299999));
#306372=CARTESIAN_POINT('Ctrl Pts',(-3.11794612100006,2.2,2.49851531299999));
#306373=CARTESIAN_POINT('Ctrl Pts',(-3.11807891600006,12.2,2.49861515099998));
#306374=CARTESIAN_POINT('Ctrl Pts',(-3.11807891600006,5.2,2.49861515099998));
#306375=CARTESIAN_POINT('Ctrl Pts',(-3.11807891600006,2.2,2.49861515099998));
#306376=CARTESIAN_POINT('Ctrl Pts',(-3.11821752300005,12.2,2.49871906699998));
#306377=CARTESIAN_POINT('Ctrl Pts',(-3.11821752300005,5.2,2.49871906699998));
#306378=CARTESIAN_POINT('Ctrl Pts',(-3.11821752300005,2.2,2.49871906699998));
#306379=CARTESIAN_POINT('Ctrl Pts',(-3.11836194000006,12.2,2.49882703499999));
#306380=CARTESIAN_POINT('Ctrl Pts',(-3.11836194000006,5.2,2.49882703499999));
#306381=CARTESIAN_POINT('Ctrl Pts',(-3.11836194000006,2.2,2.49882703499999));
#306382=CARTESIAN_POINT('Ctrl Pts',(-3.11851216600005,12.2,2.49893903099998));
#306383=CARTESIAN_POINT('Ctrl Pts',(-3.11851216600005,5.2,2.49893903099998));
#306384=CARTESIAN_POINT('Ctrl Pts',(-3.11851216600005,2.2,2.49893903099998));
#306385=CARTESIAN_POINT('Ctrl Pts',(-3.11866819800006,12.2,2.49905503099999));
#306386=CARTESIAN_POINT('Ctrl Pts',(-3.11866819800006,5.2,2.49905503099999));
#306387=CARTESIAN_POINT('Ctrl Pts',(-3.11866819800006,2.2,2.49905503099999));
#306388=CARTESIAN_POINT('Ctrl Pts',(-3.11883003500005,12.2,2.49917501099999));
#306389=CARTESIAN_POINT('Ctrl Pts',(-3.11883003500005,5.2,2.49917501099999));
#306390=CARTESIAN_POINT('Ctrl Pts',(-3.11883003500005,2.2,2.49917501099999));
#306391=CARTESIAN_POINT('Ctrl Pts',(-3.11899767600006,12.2,2.49929894499999));
#306392=CARTESIAN_POINT('Ctrl Pts',(-3.11899767600006,5.2,2.49929894499999));
#306393=CARTESIAN_POINT('Ctrl Pts',(-3.11899767600006,2.2,2.49929894499999));
#306394=CARTESIAN_POINT('Ctrl Pts',(-3.11917111900006,12.2,2.49942681099999));
#306395=CARTESIAN_POINT('Ctrl Pts',(-3.11917111900006,5.2,2.49942681099999));
#306396=CARTESIAN_POINT('Ctrl Pts',(-3.11917111900006,2.2,2.49942681099999));
#306397=CARTESIAN_POINT('Ctrl Pts',(-3.11935036300006,12.2,2.49955858199999));
#306398=CARTESIAN_POINT('Ctrl Pts',(-3.11935036300006,5.2,2.49955858199999));
#306399=CARTESIAN_POINT('Ctrl Pts',(-3.11935036300006,2.2,2.49955858199999));
#306400=CARTESIAN_POINT('Ctrl Pts',(-3.11953540400005,12.2,2.49969423399998));
#306401=CARTESIAN_POINT('Ctrl Pts',(-3.11953540400005,5.2,2.49969423399998));
#306402=CARTESIAN_POINT('Ctrl Pts',(-3.11953540400005,2.2,2.49969423399998));
#306403=CARTESIAN_POINT('Ctrl Pts',(-3.11972624100005,12.2,2.49983374399999));
#306404=CARTESIAN_POINT('Ctrl Pts',(-3.11972624100005,5.2,2.49983374399999));
#306405=CARTESIAN_POINT('Ctrl Pts',(-3.11972624100005,2.2,2.49983374399999));
#306406=CARTESIAN_POINT('Ctrl Pts',(-3.11992287400006,12.2,2.49997708699999));
#306407=CARTESIAN_POINT('Ctrl Pts',(-3.11992287400006,5.2,2.49997708699999));
#306408=CARTESIAN_POINT('Ctrl Pts',(-3.11992287400006,2.2,2.49997708699999));
#306409=CARTESIAN_POINT('Ctrl Pts',(-3.12012529900006,12.2,2.50012423999999));
#306410=CARTESIAN_POINT('Ctrl Pts',(-3.12012529900006,5.2,2.50012423999999));
#306411=CARTESIAN_POINT('Ctrl Pts',(-3.12012529900006,2.2,2.50012423999999));
#306412=CARTESIAN_POINT('Ctrl Pts',(-3.12033351600005,12.2,2.50027517899999));
#306413=CARTESIAN_POINT('Ctrl Pts',(-3.12033351600005,5.2,2.50027517899999));
#306414=CARTESIAN_POINT('Ctrl Pts',(-3.12033351600005,2.2,2.50027517899999));
#306415=CARTESIAN_POINT('Ctrl Pts',(-3.12054752100006,12.2,2.50042987999999));
#306416=CARTESIAN_POINT('Ctrl Pts',(-3.12054752100006,5.2,2.50042987999999));
#306417=CARTESIAN_POINT('Ctrl Pts',(-3.12054752100006,2.2,2.50042987999999));
#306418=CARTESIAN_POINT('Ctrl Pts',(-3.12076731400006,12.2,2.50058831899998));
#306419=CARTESIAN_POINT('Ctrl Pts',(-3.12076731400006,5.2,2.50058831899998));
#306420=CARTESIAN_POINT('Ctrl Pts',(-3.12076731400006,2.2,2.50058831899998));
#306421=CARTESIAN_POINT('Ctrl Pts',(-3.12099289300006,12.2,2.50075047399999));
#306422=CARTESIAN_POINT('Ctrl Pts',(-3.12099289300006,5.2,2.50075047399999));
#306423=CARTESIAN_POINT('Ctrl Pts',(-3.12099289300006,2.2,2.50075047399999));
#306424=CARTESIAN_POINT('Ctrl Pts',(-3.12122425400006,12.2,2.50091631999998));
#306425=CARTESIAN_POINT('Ctrl Pts',(-3.12122425400006,5.2,2.50091631999998));
#306426=CARTESIAN_POINT('Ctrl Pts',(-3.12122425400006,2.2,2.50091631999998));
#306427=CARTESIAN_POINT('Ctrl Pts',(-3.12146139800006,12.2,2.50108583399999));
#306428=CARTESIAN_POINT('Ctrl Pts',(-3.12146139800006,5.2,2.50108583399999));
#306429=CARTESIAN_POINT('Ctrl Pts',(-3.12146139800006,2.2,2.50108583399999));
#306430=CARTESIAN_POINT('Ctrl Pts',(-3.12170432100006,12.2,2.50125899199999));
#306431=CARTESIAN_POINT('Ctrl Pts',(-3.12170432100006,5.2,2.50125899199999));
#306432=CARTESIAN_POINT('Ctrl Pts',(-3.12170432100006,2.2,2.50125899199999));
#306433=CARTESIAN_POINT('Ctrl Pts',(-3.12195302200006,12.2,2.50143577099998));
#306434=CARTESIAN_POINT('Ctrl Pts',(-3.12195302200006,5.2,2.50143577099998));
#306435=CARTESIAN_POINT('Ctrl Pts',(-3.12195302200006,2.2,2.50143577099998));
#306436=CARTESIAN_POINT('Ctrl Pts',(-3.12220749700006,12.2,2.50161614799998));
#306437=CARTESIAN_POINT('Ctrl Pts',(-3.12220749700006,5.2,2.50161614799998));
#306438=CARTESIAN_POINT('Ctrl Pts',(-3.12220749700006,2.2,2.50161614799998));
#306439=CARTESIAN_POINT('Ctrl Pts',(-3.12246774800006,12.2,2.50180010099999));
#306440=CARTESIAN_POINT('Ctrl Pts',(-3.12246774800006,5.2,2.50180010099999));
#306441=CARTESIAN_POINT('Ctrl Pts',(-3.12246774800006,2.2,2.50180010099999));
#306442=CARTESIAN_POINT('Ctrl Pts',(-3.12273376900006,12.2,2.50198760499998));
#306443=CARTESIAN_POINT('Ctrl Pts',(-3.12273376900006,5.2,2.50198760499998));
#306444=CARTESIAN_POINT('Ctrl Pts',(-3.12273376900006,2.2,2.50198760499998));
#306445=CARTESIAN_POINT('Ctrl Pts',(-3.12300556000006,12.2,2.50217863899999));
#306446=CARTESIAN_POINT('Ctrl Pts',(-3.12300556000006,5.2,2.50217863899999));
#306447=CARTESIAN_POINT('Ctrl Pts',(-3.12300556000006,2.2,2.50217863899999));
#306448=CARTESIAN_POINT('Ctrl Pts',(-3.12328311900006,12.2,2.50237317899998));
#306449=CARTESIAN_POINT('Ctrl Pts',(-3.12328311900006,5.2,2.50237317899998));
#306450=CARTESIAN_POINT('Ctrl Pts',(-3.12328311900006,2.2,2.50237317899998));
#306451=CARTESIAN_POINT('Ctrl Pts',(-3.12356644200006,12.2,2.50257120199999));
#306452=CARTESIAN_POINT('Ctrl Pts',(-3.12356644200006,5.2,2.50257120199999));
#306453=CARTESIAN_POINT('Ctrl Pts',(-3.12356644200006,2.2,2.50257120199999));
#306454=CARTESIAN_POINT('Ctrl Pts',(-3.12385552900006,12.2,2.50277268499998));
#306455=CARTESIAN_POINT('Ctrl Pts',(-3.12385552900006,5.2,2.50277268499998));
#306456=CARTESIAN_POINT('Ctrl Pts',(-3.12385552900006,2.2,2.50277268499998));
#306457=CARTESIAN_POINT('Ctrl Pts',(-3.12415037700006,12.2,2.50297760799998));
#306458=CARTESIAN_POINT('Ctrl Pts',(-3.12415037700006,5.2,2.50297760799998));
#306459=CARTESIAN_POINT('Ctrl Pts',(-3.12415037700006,2.2,2.50297760799998));
#306460=CARTESIAN_POINT('Ctrl Pts',(-3.12445098400006,12.2,2.50318594399998));
#306461=CARTESIAN_POINT('Ctrl Pts',(-3.12445098400006,5.2,2.50318594399998));
#306462=CARTESIAN_POINT('Ctrl Pts',(-3.12445098400006,2.2,2.50318594399998));
#306463=CARTESIAN_POINT('Ctrl Pts',(-3.12475734800006,12.2,2.50339767399999));
#306464=CARTESIAN_POINT('Ctrl Pts',(-3.12475734800006,5.2,2.50339767399999));
#306465=CARTESIAN_POINT('Ctrl Pts',(-3.12475734800006,2.2,2.50339767399999));
#306466=CARTESIAN_POINT('Ctrl Pts',(-3.12506946600006,12.2,2.50361277599998));
#306467=CARTESIAN_POINT('Ctrl Pts',(-3.12506946600006,5.2,2.50361277599998));
#306468=CARTESIAN_POINT('Ctrl Pts',(-3.12506946600006,2.2,2.50361277599998));
#306469=CARTESIAN_POINT('Ctrl Pts',(-3.12538733700006,12.2,2.50383122499999));
#306470=CARTESIAN_POINT('Ctrl Pts',(-3.12538733700006,5.2,2.50383122499999));
#306471=CARTESIAN_POINT('Ctrl Pts',(-3.12538733700006,2.2,2.50383122499999));
#306472=CARTESIAN_POINT('Ctrl Pts',(-3.12571095700005,12.2,2.50405299999999));
#306473=CARTESIAN_POINT('Ctrl Pts',(-3.12571095700005,5.2,2.50405299999999));
#306474=CARTESIAN_POINT('Ctrl Pts',(-3.12571095700005,2.2,2.50405299999999));
#306475=CARTESIAN_POINT('Ctrl Pts',(-3.12604032600006,12.2,2.50427807899998));
#306476=CARTESIAN_POINT('Ctrl Pts',(-3.12604032600006,5.2,2.50427807899998));
#306477=CARTESIAN_POINT('Ctrl Pts',(-3.12604032600006,2.2,2.50427807899998));
#306478=CARTESIAN_POINT('Ctrl Pts',(-3.12637544100005,12.2,2.50450643999999));
#306479=CARTESIAN_POINT('Ctrl Pts',(-3.12637544100005,5.2,2.50450643999999));
#306480=CARTESIAN_POINT('Ctrl Pts',(-3.12637544100005,2.2,2.50450643999999));
#306481=CARTESIAN_POINT('Ctrl Pts',(-3.12671629800006,12.2,2.50473806099999));
#306482=CARTESIAN_POINT('Ctrl Pts',(-3.12671629800006,5.2,2.50473806099999));
#306483=CARTESIAN_POINT('Ctrl Pts',(-3.12671629800006,2.2,2.50473806099999));
#306484=CARTESIAN_POINT('Ctrl Pts',(-3.12706289700006,12.2,2.50497291999999));
#306485=CARTESIAN_POINT('Ctrl Pts',(-3.12706289700006,5.2,2.50497291999999));
#306486=CARTESIAN_POINT('Ctrl Pts',(-3.12706289700006,2.2,2.50497291999999));
#306487=CARTESIAN_POINT('Ctrl Pts',(-3.12741523500006,12.2,2.50521099399998));
#306488=CARTESIAN_POINT('Ctrl Pts',(-3.12741523500006,5.2,2.50521099399998));
#306489=CARTESIAN_POINT('Ctrl Pts',(-3.12741523500006,2.2,2.50521099399998));
#306490=CARTESIAN_POINT('Ctrl Pts',(-3.12777330900006,12.2,2.50545226299998));
#306491=CARTESIAN_POINT('Ctrl Pts',(-3.12777330900006,5.2,2.50545226299998));
#306492=CARTESIAN_POINT('Ctrl Pts',(-3.12777330900006,2.2,2.50545226299998));
#306493=CARTESIAN_POINT('Ctrl Pts',(-3.12813711700006,12.2,2.50569670399998));
#306494=CARTESIAN_POINT('Ctrl Pts',(-3.12813711700006,5.2,2.50569670399998));
#306495=CARTESIAN_POINT('Ctrl Pts',(-3.12813711700006,2.2,2.50569670399998));
#306496=CARTESIAN_POINT('Ctrl Pts',(-3.12850665800006,12.2,2.50594429599998));
#306497=CARTESIAN_POINT('Ctrl Pts',(-3.12850665800006,5.2,2.50594429599998));
#306498=CARTESIAN_POINT('Ctrl Pts',(-3.12850665800006,2.2,2.50594429599998));
#306499=CARTESIAN_POINT('Ctrl Pts',(-3.12888192700005,12.2,2.50619501699998));
#306500=CARTESIAN_POINT('Ctrl Pts',(-3.12888192700005,5.2,2.50619501699998));
#306501=CARTESIAN_POINT('Ctrl Pts',(-3.12888192700005,2.2,2.50619501699998));
#306502=CARTESIAN_POINT('Ctrl Pts',(-3.12926292300005,12.2,2.50644884599998));
#306503=CARTESIAN_POINT('Ctrl Pts',(-3.12926292300005,5.2,2.50644884599998));
#306504=CARTESIAN_POINT('Ctrl Pts',(-3.12926292300005,2.2,2.50644884599998));
#306505=CARTESIAN_POINT('Ctrl Pts',(-3.12964964300006,12.2,2.50670576099999));
#306506=CARTESIAN_POINT('Ctrl Pts',(-3.12964964300006,5.2,2.50670576099999));
#306507=CARTESIAN_POINT('Ctrl Pts',(-3.12964964300006,2.2,2.50670576099999));
#306508=CARTESIAN_POINT('Ctrl Pts',(-3.13004208700006,12.2,2.50696574099998));
#306509=CARTESIAN_POINT('Ctrl Pts',(-3.13004208700006,5.2,2.50696574099998));
#306510=CARTESIAN_POINT('Ctrl Pts',(-3.13004208700006,2.2,2.50696574099998));
#306511=CARTESIAN_POINT('Ctrl Pts',(-3.13044025000006,12.2,2.50722876399998));
#306512=CARTESIAN_POINT('Ctrl Pts',(-3.13044025000006,5.2,2.50722876399998));
#306513=CARTESIAN_POINT('Ctrl Pts',(-3.13044025000006,2.2,2.50722876399998));
#306514=CARTESIAN_POINT('Ctrl Pts',(-3.13084413000006,12.2,2.50749480999998));
#306515=CARTESIAN_POINT('Ctrl Pts',(-3.13084413000006,5.2,2.50749480999998));
#306516=CARTESIAN_POINT('Ctrl Pts',(-3.13084413000006,2.2,2.50749480999998));
#306517=CARTESIAN_POINT('Ctrl Pts',(-3.13125372400005,12.2,2.50776385699999));
#306518=CARTESIAN_POINT('Ctrl Pts',(-3.13125372400005,5.2,2.50776385699999));
#306519=CARTESIAN_POINT('Ctrl Pts',(-3.13125372400005,2.2,2.50776385699999));
#306520=CARTESIAN_POINT('Ctrl Pts',(-3.13166903000006,12.2,2.50803588399998));
#306521=CARTESIAN_POINT('Ctrl Pts',(-3.13166903000006,5.2,2.50803588399998));
#306522=CARTESIAN_POINT('Ctrl Pts',(-3.13166903000006,2.2,2.50803588399998));
#306523=CARTESIAN_POINT('Ctrl Pts',(-3.13209004700005,12.2,2.50831087099999));
#306524=CARTESIAN_POINT('Ctrl Pts',(-3.13209004700005,5.2,2.50831087099999));
#306525=CARTESIAN_POINT('Ctrl Pts',(-3.13209004700005,2.2,2.50831087099999));
#306526=CARTESIAN_POINT('Ctrl Pts',(-3.13251677000005,12.2,2.50858879499999));
#306527=CARTESIAN_POINT('Ctrl Pts',(-3.13251677000005,5.2,2.50858879499999));
#306528=CARTESIAN_POINT('Ctrl Pts',(-3.13251677000005,2.2,2.50858879499999));
#306529=CARTESIAN_POINT('Ctrl Pts',(-3.13294919800006,12.2,2.50886963599999));
#306530=CARTESIAN_POINT('Ctrl Pts',(-3.13294919800006,5.2,2.50886963599999));
#306531=CARTESIAN_POINT('Ctrl Pts',(-3.13294919800006,2.2,2.50886963599999));
#306532=CARTESIAN_POINT('Ctrl Pts',(-3.13338732900006,12.2,2.50915337399999));
#306533=CARTESIAN_POINT('Ctrl Pts',(-3.13338732900006,5.2,2.50915337399999));
#306534=CARTESIAN_POINT('Ctrl Pts',(-3.13338732900006,2.2,2.50915337399999));
#306535=CARTESIAN_POINT('Ctrl Pts',(-3.13383115700006,12.2,2.50943998799999));
#306536=CARTESIAN_POINT('Ctrl Pts',(-3.13383115700006,5.2,2.50943998799999));
#306537=CARTESIAN_POINT('Ctrl Pts',(-3.13383115700006,2.2,2.50943998799999));
#306538=CARTESIAN_POINT('Ctrl Pts',(-3.13428068400006,12.2,2.50972945699999));
#306539=CARTESIAN_POINT('Ctrl Pts',(-3.13428068400006,5.2,2.50972945699999));
#306540=CARTESIAN_POINT('Ctrl Pts',(-3.13428068400006,2.2,2.50972945699999));
#306541=CARTESIAN_POINT('Ctrl Pts',(-3.13473590500006,12.2,2.51002175999999));
#306542=CARTESIAN_POINT('Ctrl Pts',(-3.13473590500006,5.2,2.51002175999999));
#306543=CARTESIAN_POINT('Ctrl Pts',(-3.13473590500006,2.2,2.51002175999999));
#306544=CARTESIAN_POINT('Ctrl Pts',(-3.13519681700006,12.2,2.51031687599998));
#306545=CARTESIAN_POINT('Ctrl Pts',(-3.13519681700006,5.2,2.51031687599998));
#306546=CARTESIAN_POINT('Ctrl Pts',(-3.13519681700006,2.2,2.51031687599998));
#306547=CARTESIAN_POINT('Ctrl Pts',(-3.13566341800006,12.2,2.51061478699998));
#306548=CARTESIAN_POINT('Ctrl Pts',(-3.13566341800006,5.2,2.51061478699998));
#306549=CARTESIAN_POINT('Ctrl Pts',(-3.13566341800006,2.2,2.51061478699998));
#306550=CARTESIAN_POINT('Ctrl Pts',(-3.13613570600006,12.2,2.51091546999999));
#306551=CARTESIAN_POINT('Ctrl Pts',(-3.13613570600006,5.2,2.51091546999999));
#306552=CARTESIAN_POINT('Ctrl Pts',(-3.13613570600006,2.2,2.51091546999999));
#306553=CARTESIAN_POINT('Ctrl Pts',(-3.13661367700006,12.2,2.51121890599999));
#306554=CARTESIAN_POINT('Ctrl Pts',(-3.13661367700006,5.2,2.51121890599999));
#306555=CARTESIAN_POINT('Ctrl Pts',(-3.13661367700006,2.2,2.51121890599999));
#306556=CARTESIAN_POINT('Ctrl Pts',(-3.13709732900006,12.2,2.51152507399999));
#306557=CARTESIAN_POINT('Ctrl Pts',(-3.13709732900006,5.2,2.51152507399999));
#306558=CARTESIAN_POINT('Ctrl Pts',(-3.13709732900006,2.2,2.51152507399999));
#306559=CARTESIAN_POINT('Ctrl Pts',(-3.13758665900005,12.2,2.51183395499999));
#306560=CARTESIAN_POINT('Ctrl Pts',(-3.13758665900005,5.2,2.51183395499999));
#306561=CARTESIAN_POINT('Ctrl Pts',(-3.13758665900005,2.2,2.51183395499999));
#306562=CARTESIAN_POINT('Ctrl Pts',(-3.13808166500006,12.2,2.51214552699999));
#306563=CARTESIAN_POINT('Ctrl Pts',(-3.13808166500006,5.2,2.51214552699999));
#306564=CARTESIAN_POINT('Ctrl Pts',(-3.13808166500006,2.2,2.51214552699999));
#306565=CARTESIAN_POINT('Ctrl Pts',(-3.13858234300006,12.2,2.51245977099998));
#306566=CARTESIAN_POINT('Ctrl Pts',(-3.13858234300006,5.2,2.51245977099998));
#306567=CARTESIAN_POINT('Ctrl Pts',(-3.13858234300006,2.2,2.51245977099998));
#306568=CARTESIAN_POINT('Ctrl Pts',(-3.13908869200006,12.2,2.51277666599999));
#306569=CARTESIAN_POINT('Ctrl Pts',(-3.13908869200006,5.2,2.51277666599999));
#306570=CARTESIAN_POINT('Ctrl Pts',(-3.13908869200006,2.2,2.51277666599999));
#306571=CARTESIAN_POINT('Ctrl Pts',(-3.13960070700006,12.2,2.51309619499998));
#306572=CARTESIAN_POINT('Ctrl Pts',(-3.13960070700006,5.2,2.51309619499998));
#306573=CARTESIAN_POINT('Ctrl Pts',(-3.13960070700006,2.2,2.51309619499998));
#306574=CARTESIAN_POINT('Ctrl Pts',(-3.14011838700006,12.2,2.51341833399999));
#306575=CARTESIAN_POINT('Ctrl Pts',(-3.14011838700006,5.2,2.51341833399999));
#306576=CARTESIAN_POINT('Ctrl Pts',(-3.14011838700006,2.2,2.51341833399999));
#306577=CARTESIAN_POINT('Ctrl Pts',(-3.14064172800005,12.2,2.51374306599998));
#306578=CARTESIAN_POINT('Ctrl Pts',(-3.14064172800005,5.2,2.51374306599998));
#306579=CARTESIAN_POINT('Ctrl Pts',(-3.14064172800005,2.2,2.51374306599998));
#306580=CARTESIAN_POINT('Ctrl Pts',(-3.14117072900005,12.2,2.51407036999999));
#306581=CARTESIAN_POINT('Ctrl Pts',(-3.14117072900005,5.2,2.51407036999999));
#306582=CARTESIAN_POINT('Ctrl Pts',(-3.14117072900005,2.2,2.51407036999999));
#306583=CARTESIAN_POINT('Ctrl Pts',(-3.14170538500006,12.2,2.51440022599999));
#306584=CARTESIAN_POINT('Ctrl Pts',(-3.14170538500006,5.2,2.51440022599999));
#306585=CARTESIAN_POINT('Ctrl Pts',(-3.14170538500006,2.2,2.51440022599999));
#306586=CARTESIAN_POINT('Ctrl Pts',(-3.14224569400006,12.2,2.51473261599998));
#306587=CARTESIAN_POINT('Ctrl Pts',(-3.14224569400006,5.2,2.51473261599998));
#306588=CARTESIAN_POINT('Ctrl Pts',(-3.14224569400006,2.2,2.51473261599998));
#306589=CARTESIAN_POINT('Ctrl Pts',(-3.14279165400006,12.2,2.51506751899999));
#306590=CARTESIAN_POINT('Ctrl Pts',(-3.14279165400006,5.2,2.51506751899999));
#306591=CARTESIAN_POINT('Ctrl Pts',(-3.14279165400006,2.2,2.51506751899999));
#306592=CARTESIAN_POINT('Ctrl Pts',(-3.14334326000006,12.2,2.51540491499998));
#306593=CARTESIAN_POINT('Ctrl Pts',(-3.14334326000006,5.2,2.51540491499998));
#306594=CARTESIAN_POINT('Ctrl Pts',(-3.14334326000006,2.2,2.51540491499998));
#306595=CARTESIAN_POINT('Ctrl Pts',(-3.14390051100006,12.2,2.51574478699998));
#306596=CARTESIAN_POINT('Ctrl Pts',(-3.14390051100006,5.2,2.51574478699998));
#306597=CARTESIAN_POINT('Ctrl Pts',(-3.14390051100006,2.2,2.51574478699998));
#306598=CARTESIAN_POINT('Ctrl Pts',(-3.14446340400006,12.2,2.51608711299999));
#306599=CARTESIAN_POINT('Ctrl Pts',(-3.14446340400006,5.2,2.51608711299999));
#306600=CARTESIAN_POINT('Ctrl Pts',(-3.14446340400006,2.2,2.51608711299999));
#306601=CARTESIAN_POINT('Ctrl Pts',(-3.14503193500005,12.2,2.51643187499998));
#306602=CARTESIAN_POINT('Ctrl Pts',(-3.14503193500005,5.2,2.51643187499998));
#306603=CARTESIAN_POINT('Ctrl Pts',(-3.14503193500005,2.2,2.51643187499998));
#306604=CARTESIAN_POINT('Ctrl Pts',(-3.14560610200005,12.2,2.51677905199998));
#306605=CARTESIAN_POINT('Ctrl Pts',(-3.14560610200005,5.2,2.51677905199998));
#306606=CARTESIAN_POINT('Ctrl Pts',(-3.14560610200005,2.2,2.51677905199998));
#306607=CARTESIAN_POINT('Ctrl Pts',(-3.14618590100006,12.2,2.51712862799998));
#306608=CARTESIAN_POINT('Ctrl Pts',(-3.14618590100006,5.2,2.51712862799998));
#306609=CARTESIAN_POINT('Ctrl Pts',(-3.14618590100006,2.2,2.51712862799998));
#306610=CARTESIAN_POINT('Ctrl Pts',(-3.14677133100006,12.2,2.51748058099999));
#306611=CARTESIAN_POINT('Ctrl Pts',(-3.14677133100006,5.2,2.51748058099999));
#306612=CARTESIAN_POINT('Ctrl Pts',(-3.14677133100006,2.2,2.51748058099999));
#306613=CARTESIAN_POINT('Ctrl Pts',(-3.14736238700006,12.2,2.51783489199998));
#306614=CARTESIAN_POINT('Ctrl Pts',(-3.14736238700006,5.2,2.51783489199998));
#306615=CARTESIAN_POINT('Ctrl Pts',(-3.14736238700006,2.2,2.51783489199998));
#306616=CARTESIAN_POINT('Ctrl Pts',(-3.14795906700006,12.2,2.51819154399998));
#306617=CARTESIAN_POINT('Ctrl Pts',(-3.14795906700006,5.2,2.51819154399998));
#306618=CARTESIAN_POINT('Ctrl Pts',(-3.14795906700006,2.2,2.51819154399998));
#306619=CARTESIAN_POINT('Ctrl Pts',(-3.14856136800006,12.2,2.51855051599998));
#306620=CARTESIAN_POINT('Ctrl Pts',(-3.14856136800006,5.2,2.51855051599998));
#306621=CARTESIAN_POINT('Ctrl Pts',(-3.14856136800006,2.2,2.51855051599998));
#306622=CARTESIAN_POINT('Ctrl Pts',(-3.14916928600006,12.2,2.51891178999998));
#306623=CARTESIAN_POINT('Ctrl Pts',(-3.14916928600006,5.2,2.51891178999998));
#306624=CARTESIAN_POINT('Ctrl Pts',(-3.14916928600006,2.2,2.51891178999998));
#306625=CARTESIAN_POINT('Ctrl Pts',(-3.14978281900005,12.2,2.51927534799999));
#306626=CARTESIAN_POINT('Ctrl Pts',(-3.14978281900005,5.2,2.51927534799999));
#306627=CARTESIAN_POINT('Ctrl Pts',(-3.14978281900005,2.2,2.51927534799999));
#306628=CARTESIAN_POINT('Ctrl Pts',(-3.15040196400005,12.2,2.51964116899998));
#306629=CARTESIAN_POINT('Ctrl Pts',(-3.15040196400005,5.2,2.51964116899998));
#306630=CARTESIAN_POINT('Ctrl Pts',(-3.15040196400005,2.2,2.51964116899998));
#306631=CARTESIAN_POINT('Ctrl Pts',(-3.15102671700005,12.2,2.52000923599999));
#306632=CARTESIAN_POINT('Ctrl Pts',(-3.15102671700005,5.2,2.52000923599999));
#306633=CARTESIAN_POINT('Ctrl Pts',(-3.15102671700005,2.2,2.52000923599999));
#306634=CARTESIAN_POINT('Ctrl Pts',(-3.15165707500006,12.2,2.52037952899999));
#306635=CARTESIAN_POINT('Ctrl Pts',(-3.15165707500006,5.2,2.52037952899999));
#306636=CARTESIAN_POINT('Ctrl Pts',(-3.15165707500006,2.2,2.52037952899999));
#306637=CARTESIAN_POINT('Ctrl Pts',(-3.15229303600006,12.2,2.52075202999999));
#306638=CARTESIAN_POINT('Ctrl Pts',(-3.15229303600006,5.2,2.52075202999999));
#306639=CARTESIAN_POINT('Ctrl Pts',(-3.15229303600006,2.2,2.52075202999999));
#306640=CARTESIAN_POINT('Ctrl Pts',(-3.15293459600006,12.2,2.52112671999999));
#306641=CARTESIAN_POINT('Ctrl Pts',(-3.15293459600006,5.2,2.52112671999999));
#306642=CARTESIAN_POINT('Ctrl Pts',(-3.15293459600006,2.2,2.52112671999999));
#306643=CARTESIAN_POINT('Ctrl Pts',(-3.15358175200006,12.2,2.52150358099998));
#306644=CARTESIAN_POINT('Ctrl Pts',(-3.15358175200006,5.2,2.52150358099998));
#306645=CARTESIAN_POINT('Ctrl Pts',(-3.15358175200006,2.2,2.52150358099998));
#306646=CARTESIAN_POINT('Ctrl Pts',(-3.15423450100006,12.2,2.52188259499999));
#306647=CARTESIAN_POINT('Ctrl Pts',(-3.15423450100006,5.2,2.52188259499999));
#306648=CARTESIAN_POINT('Ctrl Pts',(-3.15423450100006,2.2,2.52188259499999));
#306649=CARTESIAN_POINT('Ctrl Pts',(-3.15489284100006,12.2,2.52226374299998));
#306650=CARTESIAN_POINT('Ctrl Pts',(-3.15489284100006,5.2,2.52226374299998));
#306651=CARTESIAN_POINT('Ctrl Pts',(-3.15489284100006,2.2,2.52226374299998));
#306652=CARTESIAN_POINT('Ctrl Pts',(-3.15555676600006,12.2,2.52264700699998));
#306653=CARTESIAN_POINT('Ctrl Pts',(-3.15555676600006,5.2,2.52264700699998));
#306654=CARTESIAN_POINT('Ctrl Pts',(-3.15555676600006,2.2,2.52264700699998));
#306655=CARTESIAN_POINT('Ctrl Pts',(-3.15622627500006,12.2,2.52303236699999));
#306656=CARTESIAN_POINT('Ctrl Pts',(-3.15622627500006,5.2,2.52303236699999));
#306657=CARTESIAN_POINT('Ctrl Pts',(-3.15622627500006,2.2,2.52303236699999));
#306658=CARTESIAN_POINT('Ctrl Pts',(-3.15690136500006,12.2,2.52341980599999));
#306659=CARTESIAN_POINT('Ctrl Pts',(-3.15690136500006,5.2,2.52341980599999));
#306660=CARTESIAN_POINT('Ctrl Pts',(-3.15690136500006,2.2,2.52341980599999));
#306661=CARTESIAN_POINT('Ctrl Pts',(-3.15758203100006,12.2,2.52380930699999));
#306662=CARTESIAN_POINT('Ctrl Pts',(-3.15758203100006,5.2,2.52380930699999));
#306663=CARTESIAN_POINT('Ctrl Pts',(-3.15758203100006,2.2,2.52380930699999));
#306664=CARTESIAN_POINT('Ctrl Pts',(-3.15826827100006,12.2,2.52420084999999));
#306665=CARTESIAN_POINT('Ctrl Pts',(-3.15826827100006,5.2,2.52420084999999));
#306666=CARTESIAN_POINT('Ctrl Pts',(-3.15826827100006,2.2,2.52420084999999));
#306667=CARTESIAN_POINT('Ctrl Pts',(-3.15896008200005,12.2,2.52459441699998));
#306668=CARTESIAN_POINT('Ctrl Pts',(-3.15896008200005,5.2,2.52459441699998));
#306669=CARTESIAN_POINT('Ctrl Pts',(-3.15896008200005,2.2,2.52459441699998));
#306670=CARTESIAN_POINT('Ctrl Pts',(-3.15965746100006,12.2,2.52498999199998));
#306671=CARTESIAN_POINT('Ctrl Pts',(-3.15965746100006,5.2,2.52498999199998));
#306672=CARTESIAN_POINT('Ctrl Pts',(-3.15965746100006,2.2,2.52498999199998));
#306673=CARTESIAN_POINT('Ctrl Pts',(-3.16036040300005,12.2,2.52538755399998));
#306674=CARTESIAN_POINT('Ctrl Pts',(-3.16036040300005,5.2,2.52538755399998));
#306675=CARTESIAN_POINT('Ctrl Pts',(-3.16036040300005,2.2,2.52538755399998));
#306676=CARTESIAN_POINT('Ctrl Pts',(-3.16106890600006,12.2,2.52578708699998));
#306677=CARTESIAN_POINT('Ctrl Pts',(-3.16106890600006,5.2,2.52578708699998));
#306678=CARTESIAN_POINT('Ctrl Pts',(-3.16106890600006,2.2,2.52578708699998));
#306679=CARTESIAN_POINT('Ctrl Pts',(-3.16178296600006,12.2,2.52618857299999));
#306680=CARTESIAN_POINT('Ctrl Pts',(-3.16178296600006,5.2,2.52618857299999));
#306681=CARTESIAN_POINT('Ctrl Pts',(-3.16178296600006,2.2,2.52618857299999));
#306682=CARTESIAN_POINT('Ctrl Pts',(-3.16250258100006,12.2,2.52659199399999));
#306683=CARTESIAN_POINT('Ctrl Pts',(-3.16250258100006,5.2,2.52659199399999));
#306684=CARTESIAN_POINT('Ctrl Pts',(-3.16250258100006,2.2,2.52659199399999));
#306685=CARTESIAN_POINT('Ctrl Pts',(-3.16322774700006,12.2,2.52699733099998));
#306686=CARTESIAN_POINT('Ctrl Pts',(-3.16322774700006,5.2,2.52699733099998));
#306687=CARTESIAN_POINT('Ctrl Pts',(-3.16322774700006,2.2,2.52699733099998));
#306688=CARTESIAN_POINT('Ctrl Pts',(-3.16395846100006,12.2,2.52740456899998));
#306689=CARTESIAN_POINT('Ctrl Pts',(-3.16395846100006,5.2,2.52740456899998));
#306690=CARTESIAN_POINT('Ctrl Pts',(-3.16395846100006,2.2,2.52740456899998));
#306691=CARTESIAN_POINT('Ctrl Pts',(-3.16469471800006,12.2,2.52781368799998));
#306692=CARTESIAN_POINT('Ctrl Pts',(-3.16469471800006,5.2,2.52781368799998));
#306693=CARTESIAN_POINT('Ctrl Pts',(-3.16469471800006,2.2,2.52781368799998));
#306694=CARTESIAN_POINT('Ctrl Pts',(-3.16543651700006,12.2,2.52822466999999));
#306695=CARTESIAN_POINT('Ctrl Pts',(-3.16543651700006,5.2,2.52822466999999));
#306696=CARTESIAN_POINT('Ctrl Pts',(-3.16543651700006,2.2,2.52822466999999));
#306697=CARTESIAN_POINT('Ctrl Pts',(-3.16618385300006,12.2,2.52863749999998));
#306698=CARTESIAN_POINT('Ctrl Pts',(-3.16618385300006,5.2,2.52863749999998));
#306699=CARTESIAN_POINT('Ctrl Pts',(-3.16618385300006,2.2,2.52863749999998));
#306700=CARTESIAN_POINT('Ctrl Pts',(-3.16693672400006,12.2,2.52905215799998));
#306701=CARTESIAN_POINT('Ctrl Pts',(-3.16693672400006,5.2,2.52905215799998));
#306702=CARTESIAN_POINT('Ctrl Pts',(-3.16693672400006,2.2,2.52905215799998));
#306703=CARTESIAN_POINT('Ctrl Pts',(-3.16769512400006,12.2,2.52946862799998));
#306704=CARTESIAN_POINT('Ctrl Pts',(-3.16769512400006,5.2,2.52946862799998));
#306705=CARTESIAN_POINT('Ctrl Pts',(-3.16769512400006,2.2,2.52946862799998));
#306706=CARTESIAN_POINT('Ctrl Pts',(-3.16845905300006,12.2,2.52988689199999));
#306707=CARTESIAN_POINT('Ctrl Pts',(-3.16845905300006,5.2,2.52988689199999));
#306708=CARTESIAN_POINT('Ctrl Pts',(-3.16845905300006,2.2,2.52988689199999));
#306709=CARTESIAN_POINT('Ctrl Pts',(-3.16922850500006,12.2,2.53030693299999));
#306710=CARTESIAN_POINT('Ctrl Pts',(-3.16922850500006,5.2,2.53030693299999));
#306711=CARTESIAN_POINT('Ctrl Pts',(-3.16922850500006,2.2,2.53030693299999));
#306712=CARTESIAN_POINT('Ctrl Pts',(-3.17000347800006,12.2,2.53072873299999));
#306713=CARTESIAN_POINT('Ctrl Pts',(-3.17000347800006,5.2,2.53072873299999));
#306714=CARTESIAN_POINT('Ctrl Pts',(-3.17000347800006,2.2,2.53072873299999));
#306715=CARTESIAN_POINT('Ctrl Pts',(-3.17078396800006,12.2,2.53115227499999));
#306716=CARTESIAN_POINT('Ctrl Pts',(-3.17078396800006,5.2,2.53115227499999));
#306717=CARTESIAN_POINT('Ctrl Pts',(-3.17078396800006,2.2,2.53115227499999));
#306718=CARTESIAN_POINT('Ctrl Pts',(-3.17156997100006,12.2,2.53157754199999));
#306719=CARTESIAN_POINT('Ctrl Pts',(-3.17156997100006,5.2,2.53157754199999));
#306720=CARTESIAN_POINT('Ctrl Pts',(-3.17156997100006,2.2,2.53157754199999));
#306721=CARTESIAN_POINT('Ctrl Pts',(-3.17236148500006,12.2,2.53200451699998));
#306722=CARTESIAN_POINT('Ctrl Pts',(-3.17236148500006,5.2,2.53200451699998));
#306723=CARTESIAN_POINT('Ctrl Pts',(-3.17236148500006,2.2,2.53200451699998));
#306724=CARTESIAN_POINT('Ctrl Pts',(-3.17315850600006,12.2,2.53243318299998));
#306725=CARTESIAN_POINT('Ctrl Pts',(-3.17315850600006,5.2,2.53243318299998));
#306726=CARTESIAN_POINT('Ctrl Pts',(-3.17315850600006,2.2,2.53243318299998));
#306727=CARTESIAN_POINT('Ctrl Pts',(-3.17396102900006,12.2,2.53286352099998));
#306728=CARTESIAN_POINT('Ctrl Pts',(-3.17396102900006,5.2,2.53286352099998));
#306729=CARTESIAN_POINT('Ctrl Pts',(-3.17396102900006,2.2,2.53286352099998));
#306730=CARTESIAN_POINT('Ctrl Pts',(-3.17476905200006,12.2,2.53329551799998));
#306731=CARTESIAN_POINT('Ctrl Pts',(-3.17476905200006,5.2,2.53329551799998));
#306732=CARTESIAN_POINT('Ctrl Pts',(-3.17476905200006,2.2,2.53329551799998));
#306733=CARTESIAN_POINT('Ctrl Pts',(-3.17558257100006,12.2,2.53372915199999));
#306734=CARTESIAN_POINT('Ctrl Pts',(-3.17558257100006,5.2,2.53372915199999));
#306735=CARTESIAN_POINT('Ctrl Pts',(-3.17558257100006,2.2,2.53372915199999));
#306736=CARTESIAN_POINT('Ctrl Pts',(-3.17640158400006,12.2,2.53416441099999));
#306737=CARTESIAN_POINT('Ctrl Pts',(-3.17640158400006,5.2,2.53416441099999));
#306738=CARTESIAN_POINT('Ctrl Pts',(-3.17640158400006,2.2,2.53416441099999));
#306739=CARTESIAN_POINT('Ctrl Pts',(-3.17722608400006,12.2,2.53460127399999));
#306740=CARTESIAN_POINT('Ctrl Pts',(-3.17722608400006,5.2,2.53460127399999));
#306741=CARTESIAN_POINT('Ctrl Pts',(-3.17722608400006,2.2,2.53460127399999));
#306742=CARTESIAN_POINT('Ctrl Pts',(-3.17805607100006,12.2,2.53503972699999));
#306743=CARTESIAN_POINT('Ctrl Pts',(-3.17805607100006,5.2,2.53503972699999));
#306744=CARTESIAN_POINT('Ctrl Pts',(-3.17805607100006,2.2,2.53503972699999));
#306745=CARTESIAN_POINT('Ctrl Pts',(-3.17889154000006,12.2,2.53547975099998));
#306746=CARTESIAN_POINT('Ctrl Pts',(-3.17889154000006,5.2,2.53547975099998));
#306747=CARTESIAN_POINT('Ctrl Pts',(-3.17889154000006,2.2,2.53547975099998));
#306748=CARTESIAN_POINT('Ctrl Pts',(-3.17973248600006,12.2,2.53592133199999));
#306749=CARTESIAN_POINT('Ctrl Pts',(-3.17973248600006,5.2,2.53592133199999));
#306750=CARTESIAN_POINT('Ctrl Pts',(-3.17973248600006,2.2,2.53592133199999));
#306751=CARTESIAN_POINT('Ctrl Pts',(-3.18057890900006,12.2,2.53636445099998));
#306752=CARTESIAN_POINT('Ctrl Pts',(-3.18057890900006,5.2,2.53636445099998));
#306753=CARTESIAN_POINT('Ctrl Pts',(-3.18057890900006,2.2,2.53636445099998));
#306754=CARTESIAN_POINT('Ctrl Pts',(-3.18143080200006,12.2,2.53680909099998));
#306755=CARTESIAN_POINT('Ctrl Pts',(-3.18143080200006,5.2,2.53680909099998));
#306756=CARTESIAN_POINT('Ctrl Pts',(-3.18143080200006,2.2,2.53680909099998));
#306757=CARTESIAN_POINT('Ctrl Pts',(-3.18228816200006,12.2,2.53725523899998));
#306758=CARTESIAN_POINT('Ctrl Pts',(-3.18228816200006,5.2,2.53725523899998));
#306759=CARTESIAN_POINT('Ctrl Pts',(-3.18228816200006,2.2,2.53725523899998));
#306760=CARTESIAN_POINT('Ctrl Pts',(-3.18315098700006,12.2,2.53770287399998));
#306761=CARTESIAN_POINT('Ctrl Pts',(-3.18315098700006,5.2,2.53770287399998));
#306762=CARTESIAN_POINT('Ctrl Pts',(-3.18315098700006,2.2,2.53770287399998));
#306763=CARTESIAN_POINT('Ctrl Pts',(-3.18401927200005,12.2,2.53815198299999));
#306764=CARTESIAN_POINT('Ctrl Pts',(-3.18401927200005,5.2,2.53815198299999));
#306765=CARTESIAN_POINT('Ctrl Pts',(-3.18401927200005,2.2,2.53815198299999));
#306766=CARTESIAN_POINT('Ctrl Pts',(-3.18489301400006,12.2,2.53860254699998));
#306767=CARTESIAN_POINT('Ctrl Pts',(-3.18489301400006,5.2,2.53860254699998));
#306768=CARTESIAN_POINT('Ctrl Pts',(-3.18489301400006,2.2,2.53860254699998));
#306769=CARTESIAN_POINT('Ctrl Pts',(-3.18577220800006,12.2,2.53905455099999));
#306770=CARTESIAN_POINT('Ctrl Pts',(-3.18577220800006,5.2,2.53905455099999));
#306771=CARTESIAN_POINT('Ctrl Pts',(-3.18577220800006,2.2,2.53905455099999));
#306772=CARTESIAN_POINT('Ctrl Pts',(-3.18665685300005,12.2,2.53950797899999));
#306773=CARTESIAN_POINT('Ctrl Pts',(-3.18665685300005,5.2,2.53950797899999));
#306774=CARTESIAN_POINT('Ctrl Pts',(-3.18665685300005,2.2,2.53950797899999));
#306775=CARTESIAN_POINT('Ctrl Pts',(-3.18754694300006,12.2,2.53996281299998));
#306776=CARTESIAN_POINT('Ctrl Pts',(-3.18754694300006,5.2,2.53996281299998));
#306777=CARTESIAN_POINT('Ctrl Pts',(-3.18754694300006,2.2,2.53996281299998));
#306778=CARTESIAN_POINT('Ctrl Pts',(-3.18844247500006,12.2,2.54041903699999));
#306779=CARTESIAN_POINT('Ctrl Pts',(-3.18844247500006,5.2,2.54041903699999));
#306780=CARTESIAN_POINT('Ctrl Pts',(-3.18844247500006,2.2,2.54041903699999));
#306781=CARTESIAN_POINT('Ctrl Pts',(-3.18934344500006,12.2,2.54087663699998));
#306782=CARTESIAN_POINT('Ctrl Pts',(-3.18934344500006,5.2,2.54087663699998));
#306783=CARTESIAN_POINT('Ctrl Pts',(-3.18934344500006,2.2,2.54087663699998));
#306784=CARTESIAN_POINT('Ctrl Pts',(-3.19024985000006,12.2,2.54133559499999));
#306785=CARTESIAN_POINT('Ctrl Pts',(-3.19024985000006,5.2,2.54133559499999));
#306786=CARTESIAN_POINT('Ctrl Pts',(-3.19024985000006,2.2,2.54133559499999));
#306787=CARTESIAN_POINT('Ctrl Pts',(-3.19116168500006,12.2,2.54179589499999));
#306788=CARTESIAN_POINT('Ctrl Pts',(-3.19116168500006,5.2,2.54179589499999));
#306789=CARTESIAN_POINT('Ctrl Pts',(-3.19116168500006,2.2,2.54179589499999));
#306790=CARTESIAN_POINT('Ctrl Pts',(-3.19207894900006,12.2,2.54225752099998));
#306791=CARTESIAN_POINT('Ctrl Pts',(-3.19207894900006,5.2,2.54225752099998));
#306792=CARTESIAN_POINT('Ctrl Pts',(-3.19207894900006,2.2,2.54225752099998));
#306793=CARTESIAN_POINT('Ctrl Pts',(-3.19300163400006,12.2,2.54272045899998));
#306794=CARTESIAN_POINT('Ctrl Pts',(-3.19300163400006,5.2,2.54272045899998));
#306795=CARTESIAN_POINT('Ctrl Pts',(-3.19300163400006,2.2,2.54272045899998));
#306796=CARTESIAN_POINT('Ctrl Pts',(-3.19392974100006,12.2,2.54318468899999));
#306797=CARTESIAN_POINT('Ctrl Pts',(-3.19392974100006,5.2,2.54318468899999));
#306798=CARTESIAN_POINT('Ctrl Pts',(-3.19392974100006,2.2,2.54318468899999));
#306799=CARTESIAN_POINT('Ctrl Pts',(-3.19486326300006,12.2,2.54365019799998));
#306800=CARTESIAN_POINT('Ctrl Pts',(-3.19486326300006,5.2,2.54365019799998));
#306801=CARTESIAN_POINT('Ctrl Pts',(-3.19486326300006,2.2,2.54365019799998));
#306802=CARTESIAN_POINT('Ctrl Pts',(-3.19580219600006,12.2,2.54411696899999));
#306803=CARTESIAN_POINT('Ctrl Pts',(-3.19580219600006,5.2,2.54411696899999));
#306804=CARTESIAN_POINT('Ctrl Pts',(-3.19580219600006,2.2,2.54411696899999));
#306805=CARTESIAN_POINT('Ctrl Pts',(-3.19674653900006,12.2,2.54458498699999));
#306806=CARTESIAN_POINT('Ctrl Pts',(-3.19674653900006,5.2,2.54458498699999));
#306807=CARTESIAN_POINT('Ctrl Pts',(-3.19674653900006,2.2,2.54458498699999));
#306808=CARTESIAN_POINT('Ctrl Pts',(-3.19769628500006,12.2,2.54505423499998));
#306809=CARTESIAN_POINT('Ctrl Pts',(-3.19769628500006,5.2,2.54505423499998));
#306810=CARTESIAN_POINT('Ctrl Pts',(-3.19769628500006,2.2,2.54505423499998));
#306811=CARTESIAN_POINT('Ctrl Pts',(-3.19865143200006,12.2,2.54552469799999));
#306812=CARTESIAN_POINT('Ctrl Pts',(-3.19865143200006,5.2,2.54552469799999));
#306813=CARTESIAN_POINT('Ctrl Pts',(-3.19865143200006,2.2,2.54552469799999));
#306814=CARTESIAN_POINT('Ctrl Pts',(-3.19961197700006,12.2,2.54599635999998));
#306815=CARTESIAN_POINT('Ctrl Pts',(-3.19961197700006,5.2,2.54599635999998));
#306816=CARTESIAN_POINT('Ctrl Pts',(-3.19961197700006,2.2,2.54599635999998));
#306817=CARTESIAN_POINT('Ctrl Pts',(-3.20057791400005,12.2,2.54646920599999));
#306818=CARTESIAN_POINT('Ctrl Pts',(-3.20057791400005,5.2,2.54646920599999));
#306819=CARTESIAN_POINT('Ctrl Pts',(-3.20057791400005,2.2,2.54646920599999));
#306820=CARTESIAN_POINT('Ctrl Pts',(-3.20154924000006,12.2,2.54694321899999));
#306821=CARTESIAN_POINT('Ctrl Pts',(-3.20154924000006,5.2,2.54694321899999));
#306822=CARTESIAN_POINT('Ctrl Pts',(-3.20154924000006,2.2,2.54694321899999));
#306823=CARTESIAN_POINT('Ctrl Pts',(-3.20252595200006,12.2,2.54741838499999));
#306824=CARTESIAN_POINT('Ctrl Pts',(-3.20252595200006,5.2,2.54741838499999));
#306825=CARTESIAN_POINT('Ctrl Pts',(-3.20252595200006,2.2,2.54741838499999));
#306826=CARTESIAN_POINT('Ctrl Pts',(-3.20350804500006,12.2,2.54789468699999));
#306827=CARTESIAN_POINT('Ctrl Pts',(-3.20350804500006,5.2,2.54789468699999));
#306828=CARTESIAN_POINT('Ctrl Pts',(-3.20350804500006,2.2,2.54789468699999));
#306829=CARTESIAN_POINT('Ctrl Pts',(-3.20449551600006,12.2,2.54837210999998));
#306830=CARTESIAN_POINT('Ctrl Pts',(-3.20449551600006,5.2,2.54837210999998));
#306831=CARTESIAN_POINT('Ctrl Pts',(-3.20449551600006,2.2,2.54837210999998));
#306832=CARTESIAN_POINT('Ctrl Pts',(-3.20548836100006,12.2,2.54885063899999));
#306833=CARTESIAN_POINT('Ctrl Pts',(-3.20548836100006,5.2,2.54885063899999));
#306834=CARTESIAN_POINT('Ctrl Pts',(-3.20548836100006,2.2,2.54885063899999));
#306835=CARTESIAN_POINT('Ctrl Pts',(-3.20648657500006,12.2,2.54933025799998));
#306836=CARTESIAN_POINT('Ctrl Pts',(-3.20648657500006,5.2,2.54933025799998));
#306837=CARTESIAN_POINT('Ctrl Pts',(-3.20648657500006,2.2,2.54933025799998));
#306838=CARTESIAN_POINT('Ctrl Pts',(-3.20749015500006,12.2,2.54981095199999));
#306839=CARTESIAN_POINT('Ctrl Pts',(-3.20749015500006,5.2,2.54981095199999));
#306840=CARTESIAN_POINT('Ctrl Pts',(-3.20749015500006,2.2,2.54981095199999));
#306841=CARTESIAN_POINT('Ctrl Pts',(-3.20849909800006,12.2,2.55029270599999));
#306842=CARTESIAN_POINT('Ctrl Pts',(-3.20849909800006,5.2,2.55029270599999));
#306843=CARTESIAN_POINT('Ctrl Pts',(-3.20849909800006,2.2,2.55029270599999));
#306844=CARTESIAN_POINT('Ctrl Pts',(-3.20951339800006,12.2,2.55077550299998));
#306845=CARTESIAN_POINT('Ctrl Pts',(-3.20951339800006,5.2,2.55077550299998));
#306846=CARTESIAN_POINT('Ctrl Pts',(-3.20951339800006,2.2,2.55077550299998));
#306847=CARTESIAN_POINT('Ctrl Pts',(-3.21053305200006,12.2,2.55125932999999));
#306848=CARTESIAN_POINT('Ctrl Pts',(-3.21053305200006,5.2,2.55125932999999));
#306849=CARTESIAN_POINT('Ctrl Pts',(-3.21053305200006,2.2,2.55125932999999));
#306850=CARTESIAN_POINT('Ctrl Pts',(-3.21155805600006,12.2,2.55174416999999));
#306851=CARTESIAN_POINT('Ctrl Pts',(-3.21155805600006,5.2,2.55174416999999));
#306852=CARTESIAN_POINT('Ctrl Pts',(-3.21155805600006,2.2,2.55174416999999));
#306853=CARTESIAN_POINT('Ctrl Pts',(-3.21258840700006,12.2,2.55223000899999));
#306854=CARTESIAN_POINT('Ctrl Pts',(-3.21258840700006,5.2,2.55223000899999));
#306855=CARTESIAN_POINT('Ctrl Pts',(-3.21258840700006,2.2,2.55223000899999));
#306856=CARTESIAN_POINT('Ctrl Pts',(-3.21362410000006,12.2,2.55271683099998));
#306857=CARTESIAN_POINT('Ctrl Pts',(-3.21362410000006,5.2,2.55271683099998));
#306858=CARTESIAN_POINT('Ctrl Pts',(-3.21362410000006,2.2,2.55271683099998));
#306859=CARTESIAN_POINT('Ctrl Pts',(-3.21466513100006,12.2,2.55320462199998));
#306860=CARTESIAN_POINT('Ctrl Pts',(-3.21466513100006,5.2,2.55320462199998));
#306861=CARTESIAN_POINT('Ctrl Pts',(-3.21466513100006,2.2,2.55320462199998));
#306862=CARTESIAN_POINT('Ctrl Pts',(-3.21571149700006,12.2,2.55369336599998));
#306863=CARTESIAN_POINT('Ctrl Pts',(-3.21571149700006,5.2,2.55369336599998));
#306864=CARTESIAN_POINT('Ctrl Pts',(-3.21571149700006,2.2,2.55369336599998));
#306865=CARTESIAN_POINT('Ctrl Pts',(-3.21676319300006,12.2,2.55418304699998));
#306866=CARTESIAN_POINT('Ctrl Pts',(-3.21676319300006,5.2,2.55418304699998));
#306867=CARTESIAN_POINT('Ctrl Pts',(-3.21676319300006,2.2,2.55418304699998));
#306868=CARTESIAN_POINT('Ctrl Pts',(-3.21782021500006,12.2,2.55467365199999));
#306869=CARTESIAN_POINT('Ctrl Pts',(-3.21782021500006,5.2,2.55467365199999));
#306870=CARTESIAN_POINT('Ctrl Pts',(-3.21782021500006,2.2,2.55467365199999));
#306871=CARTESIAN_POINT('Ctrl Pts',(-3.21888255800005,12.2,2.55516516599998));
#306872=CARTESIAN_POINT('Ctrl Pts',(-3.21888255800005,5.2,2.55516516599998));
#306873=CARTESIAN_POINT('Ctrl Pts',(-3.21888255800005,2.2,2.55516516599998));
#306874=CARTESIAN_POINT('Ctrl Pts',(-3.21995022000006,12.2,2.55565757299999));
#306875=CARTESIAN_POINT('Ctrl Pts',(-3.21995022000006,5.2,2.55565757299999));
#306876=CARTESIAN_POINT('Ctrl Pts',(-3.21995022000006,2.2,2.55565757299999));
#306877=CARTESIAN_POINT('Ctrl Pts',(-3.22102319800006,12.2,2.55615085899999));
#306878=CARTESIAN_POINT('Ctrl Pts',(-3.22102319800006,5.2,2.55615085899999));
#306879=CARTESIAN_POINT('Ctrl Pts',(-3.22102319800006,2.2,2.55615085899999));
#306880=CARTESIAN_POINT('Ctrl Pts',(-3.22210148400006,12.2,2.55664500799998));
#306881=CARTESIAN_POINT('Ctrl Pts',(-3.22210148400006,5.2,2.55664500799998));
#306882=CARTESIAN_POINT('Ctrl Pts',(-3.22210148400006,2.2,2.55664500799998));
#306883=CARTESIAN_POINT('Ctrl Pts',(-3.22318507700006,12.2,2.55714000599998));
#306884=CARTESIAN_POINT('Ctrl Pts',(-3.22318507700006,5.2,2.55714000599998));
#306885=CARTESIAN_POINT('Ctrl Pts',(-3.22318507700006,2.2,2.55714000599998));
#306886=CARTESIAN_POINT('Ctrl Pts',(-3.22427397100005,12.2,2.55763583899999));
#306887=CARTESIAN_POINT('Ctrl Pts',(-3.22427397100005,5.2,2.55763583899999));
#306888=CARTESIAN_POINT('Ctrl Pts',(-3.22427397100005,2.2,2.55763583899999));
#306889=CARTESIAN_POINT('Ctrl Pts',(-3.22536816400006,12.2,2.55813249099998));
#306890=CARTESIAN_POINT('Ctrl Pts',(-3.22536816400006,5.2,2.55813249099998));
#306891=CARTESIAN_POINT('Ctrl Pts',(-3.22536816400006,2.2,2.55813249099998));
#306892=CARTESIAN_POINT('Ctrl Pts',(-3.22646765100005,12.2,2.55862994799998));
#306893=CARTESIAN_POINT('Ctrl Pts',(-3.22646765100005,5.2,2.55862994799998));
#306894=CARTESIAN_POINT('Ctrl Pts',(-3.22646765100005,2.2,2.55862994799998));
#306895=CARTESIAN_POINT('Ctrl Pts',(-3.22757242600006,12.2,2.55912819499999));
#306896=CARTESIAN_POINT('Ctrl Pts',(-3.22757242600006,5.2,2.55912819499999));
#306897=CARTESIAN_POINT('Ctrl Pts',(-3.22757242600006,2.2,2.55912819499999));
#306898=CARTESIAN_POINT('Ctrl Pts',(-3.22868248800006,12.2,2.55962721799998));
#306899=CARTESIAN_POINT('Ctrl Pts',(-3.22868248800006,5.2,2.55962721799998));
#306900=CARTESIAN_POINT('Ctrl Pts',(-3.22868248800006,2.2,2.55962721799998));
#306901=CARTESIAN_POINT('Ctrl Pts',(-3.22979783200006,12.2,2.56012700199998));
#306902=CARTESIAN_POINT('Ctrl Pts',(-3.22979783200006,5.2,2.56012700199998));
#306903=CARTESIAN_POINT('Ctrl Pts',(-3.22979783200006,2.2,2.56012700199998));
#306904=CARTESIAN_POINT('Ctrl Pts',(-3.23091845200006,12.2,2.56062753299998));
#306905=CARTESIAN_POINT('Ctrl Pts',(-3.23091845200006,5.2,2.56062753299998));
#306906=CARTESIAN_POINT('Ctrl Pts',(-3.23091845200006,2.2,2.56062753299998));
#306907=CARTESIAN_POINT('Ctrl Pts',(-3.23204434700005,12.2,2.56112879599999));
#306908=CARTESIAN_POINT('Ctrl Pts',(-3.23204434700005,5.2,2.56112879599999));
#306909=CARTESIAN_POINT('Ctrl Pts',(-3.23204434700005,2.2,2.56112879599999));
#306910=CARTESIAN_POINT('Ctrl Pts',(-3.23317551000006,12.2,2.56163077699998));
#306911=CARTESIAN_POINT('Ctrl Pts',(-3.23317551000006,5.2,2.56163077699998));
#306912=CARTESIAN_POINT('Ctrl Pts',(-3.23317551000006,2.2,2.56163077699998));
#306913=CARTESIAN_POINT('Ctrl Pts',(-3.23431193700006,12.2,2.56213345999999));
#306914=CARTESIAN_POINT('Ctrl Pts',(-3.23431193700006,5.2,2.56213345999999));
#306915=CARTESIAN_POINT('Ctrl Pts',(-3.23431193700006,2.2,2.56213345999999));
#306916=CARTESIAN_POINT('Ctrl Pts',(-3.23545362600006,12.2,2.56263683399998));
#306917=CARTESIAN_POINT('Ctrl Pts',(-3.23545362600006,5.2,2.56263683399998));
#306918=CARTESIAN_POINT('Ctrl Pts',(-3.23545362600006,2.2,2.56263683399998));
#306919=CARTESIAN_POINT('Ctrl Pts',(-3.23660057200006,12.2,2.56314088099998));
#306920=CARTESIAN_POINT('Ctrl Pts',(-3.23660057200006,5.2,2.56314088099998));
#306921=CARTESIAN_POINT('Ctrl Pts',(-3.23660057200006,2.2,2.56314088099998));
#306922=CARTESIAN_POINT('Ctrl Pts',(-3.23775276900006,12.2,2.56364558999999));
#306923=CARTESIAN_POINT('Ctrl Pts',(-3.23775276900006,5.2,2.56364558999999));
#306924=CARTESIAN_POINT('Ctrl Pts',(-3.23775276900006,2.2,2.56364558999999));
#306925=CARTESIAN_POINT('Ctrl Pts',(-3.23891021500006,12.2,2.56415094499998));
#306926=CARTESIAN_POINT('Ctrl Pts',(-3.23891021500006,5.2,2.56415094499998));
#306927=CARTESIAN_POINT('Ctrl Pts',(-3.23891021500006,2.2,2.56415094499998));
#306928=CARTESIAN_POINT('Ctrl Pts',(-3.24007290600006,12.2,2.56465693099998));
#306929=CARTESIAN_POINT('Ctrl Pts',(-3.24007290600006,5.2,2.56465693099998));
#306930=CARTESIAN_POINT('Ctrl Pts',(-3.24007290600006,2.2,2.56465693099998));
#306931=CARTESIAN_POINT('Ctrl Pts',(-3.24124083500006,12.2,2.56516353499999));
#306932=CARTESIAN_POINT('Ctrl Pts',(-3.24124083500006,5.2,2.56516353499999));
#306933=CARTESIAN_POINT('Ctrl Pts',(-3.24124083500006,2.2,2.56516353499999));
#306934=CARTESIAN_POINT('Ctrl Pts',(-3.24241400000005,12.2,2.56567074399998));
#306935=CARTESIAN_POINT('Ctrl Pts',(-3.24241400000005,5.2,2.56567074399998));
#306936=CARTESIAN_POINT('Ctrl Pts',(-3.24241400000005,2.2,2.56567074399998));
#306937=CARTESIAN_POINT('Ctrl Pts',(-3.24359239700006,12.2,2.56617854099999));
#306938=CARTESIAN_POINT('Ctrl Pts',(-3.24359239700006,5.2,2.56617854099999));
#306939=CARTESIAN_POINT('Ctrl Pts',(-3.24359239700006,2.2,2.56617854099999));
#306940=CARTESIAN_POINT('Ctrl Pts',(-3.24477602100006,12.2,2.56668691499998));
#306941=CARTESIAN_POINT('Ctrl Pts',(-3.24477602100006,5.2,2.56668691499998));
#306942=CARTESIAN_POINT('Ctrl Pts',(-3.24477602100006,2.2,2.56668691499998));
#306943=CARTESIAN_POINT('Ctrl Pts',(-3.24596486800006,12.2,2.56719584999999));
#306944=CARTESIAN_POINT('Ctrl Pts',(-3.24596486800006,5.2,2.56719584999999));
#306945=CARTESIAN_POINT('Ctrl Pts',(-3.24596486800006,2.2,2.56719584999999));
#306946=CARTESIAN_POINT('Ctrl Pts',(-3.24715893300006,12.2,2.56770533199998));
#306947=CARTESIAN_POINT('Ctrl Pts',(-3.24715893300006,5.2,2.56770533199998));
#306948=CARTESIAN_POINT('Ctrl Pts',(-3.24715893300006,2.2,2.56770533199998));
#306949=CARTESIAN_POINT('Ctrl Pts',(-3.24835821300006,12.2,2.56821534799998));
#306950=CARTESIAN_POINT('Ctrl Pts',(-3.24835821300006,5.2,2.56821534799998));
#306951=CARTESIAN_POINT('Ctrl Pts',(-3.24835821300006,2.2,2.56821534799998));
#306952=CARTESIAN_POINT('Ctrl Pts',(-3.24956270200006,12.2,2.56872588399998));
#306953=CARTESIAN_POINT('Ctrl Pts',(-3.24956270200006,5.2,2.56872588399998));
#306954=CARTESIAN_POINT('Ctrl Pts',(-3.24956270200006,2.2,2.56872588399998));
#306955=CARTESIAN_POINT('Ctrl Pts',(-3.25077239900006,12.2,2.56923692599998));
#306956=CARTESIAN_POINT('Ctrl Pts',(-3.25077239900006,5.2,2.56923692599998));
#306957=CARTESIAN_POINT('Ctrl Pts',(-3.25077239900006,2.2,2.56923692599998));
#306958=CARTESIAN_POINT('Ctrl Pts',(-3.25198729600006,12.2,2.56974845999999));
#306959=CARTESIAN_POINT('Ctrl Pts',(-3.25198729600006,5.2,2.56974845999999));
#306960=CARTESIAN_POINT('Ctrl Pts',(-3.25198729600006,2.2,2.56974845999999));
#306961=CARTESIAN_POINT('Ctrl Pts',(-3.25320739000006,12.2,2.57026047199999));
#306962=CARTESIAN_POINT('Ctrl Pts',(-3.25320739000006,5.2,2.57026047199999));
#306963=CARTESIAN_POINT('Ctrl Pts',(-3.25320739000006,2.2,2.57026047199999));
#306964=CARTESIAN_POINT('Ctrl Pts',(-3.25443267700006,12.2,2.57077294899998));
#306965=CARTESIAN_POINT('Ctrl Pts',(-3.25443267700006,5.2,2.57077294899998));
#306966=CARTESIAN_POINT('Ctrl Pts',(-3.25443267700006,2.2,2.57077294899998));
#306967=CARTESIAN_POINT('Ctrl Pts',(-3.25566315300006,12.2,2.57128587699999));
#306968=CARTESIAN_POINT('Ctrl Pts',(-3.25566315300006,5.2,2.57128587699999));
#306969=CARTESIAN_POINT('Ctrl Pts',(-3.25566315300006,2.2,2.57128587699999));
#306970=CARTESIAN_POINT('Ctrl Pts',(-3.25689881400006,12.2,2.57179923999999));
#306971=CARTESIAN_POINT('Ctrl Pts',(-3.25689881400006,5.2,2.57179923999999));
#306972=CARTESIAN_POINT('Ctrl Pts',(-3.25689881400006,2.2,2.57179923999999));
#306973=CARTESIAN_POINT('Ctrl Pts',(-3.25813965300005,12.2,2.57231302899999));
#306974=CARTESIAN_POINT('Ctrl Pts',(-3.25813965300005,5.2,2.57231302899999));
#306975=CARTESIAN_POINT('Ctrl Pts',(-3.25813965300005,2.2,2.57231302899999));
#306976=CARTESIAN_POINT('Ctrl Pts',(-3.25938567000006,12.2,2.57282722699999));
#306977=CARTESIAN_POINT('Ctrl Pts',(-3.25938567000006,5.2,2.57282722699999));
#306978=CARTESIAN_POINT('Ctrl Pts',(-3.25938567000006,2.2,2.57282722699999));
#306979=CARTESIAN_POINT('Ctrl Pts',(-3.26063685700006,12.2,2.57334181999998));
#306980=CARTESIAN_POINT('Ctrl Pts',(-3.26063685700006,5.2,2.57334181999998));
#306981=CARTESIAN_POINT('Ctrl Pts',(-3.26063685700006,2.2,2.57334181999998));
#306982=CARTESIAN_POINT('Ctrl Pts',(-3.26189321000005,12.2,2.57385679699999));
#306983=CARTESIAN_POINT('Ctrl Pts',(-3.26189321000005,5.2,2.57385679699999));
#306984=CARTESIAN_POINT('Ctrl Pts',(-3.26189321000005,2.2,2.57385679699999));
#306985=CARTESIAN_POINT('Ctrl Pts',(-3.26315472700006,12.2,2.57437214299999));
#306986=CARTESIAN_POINT('Ctrl Pts',(-3.26315472700006,5.2,2.57437214299999));
#306987=CARTESIAN_POINT('Ctrl Pts',(-3.26315472700006,2.2,2.57437214299999));
#306988=CARTESIAN_POINT('Ctrl Pts',(-3.26442140100006,12.2,2.57488784499999));
#306989=CARTESIAN_POINT('Ctrl Pts',(-3.26442140100006,5.2,2.57488784499999));
#306990=CARTESIAN_POINT('Ctrl Pts',(-3.26442140100006,2.2,2.57488784499999));
#306991=CARTESIAN_POINT('Ctrl Pts',(-3.26569322900006,12.2,2.57540388899999));
#306992=CARTESIAN_POINT('Ctrl Pts',(-3.26569322900006,5.2,2.57540388899999));
#306993=CARTESIAN_POINT('Ctrl Pts',(-3.26569322900006,2.2,2.57540388899999));
#306994=CARTESIAN_POINT('Ctrl Pts',(-3.26697020700006,12.2,2.57592026099999));
#306995=CARTESIAN_POINT('Ctrl Pts',(-3.26697020700006,5.2,2.57592026099999));
#306996=CARTESIAN_POINT('Ctrl Pts',(-3.26697020700006,2.2,2.57592026099999));
#306997=CARTESIAN_POINT('Ctrl Pts',(-3.26825232900006,12.2,2.57643694899999));
#306998=CARTESIAN_POINT('Ctrl Pts',(-3.26825232900006,5.2,2.57643694899999));
#306999=CARTESIAN_POINT('Ctrl Pts',(-3.26825232900006,2.2,2.57643694899999));
#307000=CARTESIAN_POINT('Ctrl Pts',(-3.26953959300006,12.2,2.57695393999998));
#307001=CARTESIAN_POINT('Ctrl Pts',(-3.26953959300006,5.2,2.57695393999998));
#307002=CARTESIAN_POINT('Ctrl Pts',(-3.26953959300006,2.2,2.57695393999998));
#307003=CARTESIAN_POINT('Ctrl Pts',(-3.27083199200006,12.2,2.57747121899998));
#307004=CARTESIAN_POINT('Ctrl Pts',(-3.27083199200006,5.2,2.57747121899998));
#307005=CARTESIAN_POINT('Ctrl Pts',(-3.27083199200006,2.2,2.57747121899998));
#307006=CARTESIAN_POINT('Ctrl Pts',(-3.27212952400005,12.2,2.57798877299999));
#307007=CARTESIAN_POINT('Ctrl Pts',(-3.27212952400005,5.2,2.57798877299999));
#307008=CARTESIAN_POINT('Ctrl Pts',(-3.27212952400005,2.2,2.57798877299999));
#307009=CARTESIAN_POINT('Ctrl Pts',(-3.27343218200005,12.2,2.57850658999998));
#307010=CARTESIAN_POINT('Ctrl Pts',(-3.27343218200005,5.2,2.57850658999998));
#307011=CARTESIAN_POINT('Ctrl Pts',(-3.27343218200005,2.2,2.57850658999998));
#307012=CARTESIAN_POINT('Ctrl Pts',(-3.27473996200006,12.2,2.57902465599999));
#307013=CARTESIAN_POINT('Ctrl Pts',(-3.27473996200006,5.2,2.57902465599999));
#307014=CARTESIAN_POINT('Ctrl Pts',(-3.27473996200006,2.2,2.57902465599999));
#307015=CARTESIAN_POINT('Ctrl Pts',(-3.27605286300006,12.2,2.57954295799999));
#307016=CARTESIAN_POINT('Ctrl Pts',(-3.27605286300006,5.2,2.57954295799999));
#307017=CARTESIAN_POINT('Ctrl Pts',(-3.27605286300006,2.2,2.57954295799999));
#307018=CARTESIAN_POINT('Ctrl Pts',(-3.27737087600006,12.2,2.58006148299998));
#307019=CARTESIAN_POINT('Ctrl Pts',(-3.27737087600006,5.2,2.58006148299998));
#307020=CARTESIAN_POINT('Ctrl Pts',(-3.27737087600006,2.2,2.58006148299998));
#307021=CARTESIAN_POINT('Ctrl Pts',(-3.27869399900006,12.2,2.58058021799998));
#307022=CARTESIAN_POINT('Ctrl Pts',(-3.27869399900006,5.2,2.58058021799998));
#307023=CARTESIAN_POINT('Ctrl Pts',(-3.27869399900006,2.2,2.58058021799998));
#307024=CARTESIAN_POINT('Ctrl Pts',(-3.28002222700006,12.2,2.58109914799999));
#307025=CARTESIAN_POINT('Ctrl Pts',(-3.28002222700006,5.2,2.58109914799999));
#307026=CARTESIAN_POINT('Ctrl Pts',(-3.28002222700006,2.2,2.58109914799999));
#307027=CARTESIAN_POINT('Ctrl Pts',(-3.28135555500006,12.2,2.58161826399999));
#307028=CARTESIAN_POINT('Ctrl Pts',(-3.28135555500006,5.2,2.58161826399999));
#307029=CARTESIAN_POINT('Ctrl Pts',(-3.28135555500006,2.2,2.58161826399999));
#307030=CARTESIAN_POINT('Ctrl Pts',(-3.28269397900006,12.2,2.58213754899998));
#307031=CARTESIAN_POINT('Ctrl Pts',(-3.28269397900006,5.2,2.58213754899998));
#307032=CARTESIAN_POINT('Ctrl Pts',(-3.28269397900006,2.2,2.58213754899998));
#307033=CARTESIAN_POINT('Ctrl Pts',(-3.28403749500006,12.2,2.58265699099999));
#307034=CARTESIAN_POINT('Ctrl Pts',(-3.28403749500006,5.2,2.58265699099999));
#307035=CARTESIAN_POINT('Ctrl Pts',(-3.28403749500006,2.2,2.58265699099999));
#307036=CARTESIAN_POINT('Ctrl Pts',(-3.28538609800006,12.2,2.58317657899998));
#307037=CARTESIAN_POINT('Ctrl Pts',(-3.28538609800006,5.2,2.58317657899998));
#307038=CARTESIAN_POINT('Ctrl Pts',(-3.28538609800006,2.2,2.58317657899998));
#307039=CARTESIAN_POINT('Ctrl Pts',(-3.28673978400006,12.2,2.58369629799999));
#307040=CARTESIAN_POINT('Ctrl Pts',(-3.28673978400006,5.2,2.58369629799999));
#307041=CARTESIAN_POINT('Ctrl Pts',(-3.28673978400006,2.2,2.58369629799999));
#307042=CARTESIAN_POINT('Ctrl Pts',(-3.28809854700005,12.2,2.58421613699999));
#307043=CARTESIAN_POINT('Ctrl Pts',(-3.28809854700005,5.2,2.58421613699999));
#307044=CARTESIAN_POINT('Ctrl Pts',(-3.28809854700005,2.2,2.58421613699999));
#307045=CARTESIAN_POINT('Ctrl Pts',(-3.28946238400006,12.2,2.58473607999999));
#307046=CARTESIAN_POINT('Ctrl Pts',(-3.28946238400006,5.2,2.58473607999999));
#307047=CARTESIAN_POINT('Ctrl Pts',(-3.28946238400006,2.2,2.58473607999999));
#307048=CARTESIAN_POINT('Ctrl Pts',(-3.29083129000006,12.2,2.58525611799998));
#307049=CARTESIAN_POINT('Ctrl Pts',(-3.29083129000006,5.2,2.58525611799998));
#307050=CARTESIAN_POINT('Ctrl Pts',(-3.29083129000006,2.2,2.58525611799998));
#307051=CARTESIAN_POINT('Ctrl Pts',(-3.29220526000006,12.2,2.58577623599999));
#307052=CARTESIAN_POINT('Ctrl Pts',(-3.29220526000006,5.2,2.58577623599999));
#307053=CARTESIAN_POINT('Ctrl Pts',(-3.29220526000006,2.2,2.58577623599999));
#307054=CARTESIAN_POINT('Ctrl Pts',(-3.29358429000006,12.2,2.58629642199999));
#307055=CARTESIAN_POINT('Ctrl Pts',(-3.29358429000006,5.2,2.58629642199999));
#307056=CARTESIAN_POINT('Ctrl Pts',(-3.29358429000006,2.2,2.58629642199999));
#307057=CARTESIAN_POINT('Ctrl Pts',(-3.29496837500006,12.2,2.58681666199998));
#307058=CARTESIAN_POINT('Ctrl Pts',(-3.29496837500006,5.2,2.58681666199998));
#307059=CARTESIAN_POINT('Ctrl Pts',(-3.29496837500006,2.2,2.58681666199998));
#307060=CARTESIAN_POINT('Ctrl Pts',(-3.29635751000006,12.2,2.58733694599999));
#307061=CARTESIAN_POINT('Ctrl Pts',(-3.29635751000006,5.2,2.58733694599999));
#307062=CARTESIAN_POINT('Ctrl Pts',(-3.29635751000006,2.2,2.58733694599999));
#307063=CARTESIAN_POINT('Ctrl Pts',(-3.29775169200006,12.2,2.58785725799999));
#307064=CARTESIAN_POINT('Ctrl Pts',(-3.29775169200006,5.2,2.58785725799999));
#307065=CARTESIAN_POINT('Ctrl Pts',(-3.29775169200006,2.2,2.58785725799999));
#307066=CARTESIAN_POINT('Ctrl Pts',(-3.29915091600005,12.2,2.58837758699999));
#307067=CARTESIAN_POINT('Ctrl Pts',(-3.29915091600005,5.2,2.58837758699999));
#307068=CARTESIAN_POINT('Ctrl Pts',(-3.29915091600005,2.2,2.58837758699999));
#307069=CARTESIAN_POINT('Ctrl Pts',(-3.30055517600006,12.2,2.58889792199999));
#307070=CARTESIAN_POINT('Ctrl Pts',(-3.30055517600006,5.2,2.58889792199999));
#307071=CARTESIAN_POINT('Ctrl Pts',(-3.30055517600006,2.2,2.58889792199999));
#307072=CARTESIAN_POINT('Ctrl Pts',(-3.30196446900006,12.2,2.58941824799999));
#307073=CARTESIAN_POINT('Ctrl Pts',(-3.30196446900006,5.2,2.58941824799999));
#307074=CARTESIAN_POINT('Ctrl Pts',(-3.30196446900006,2.2,2.58941824799999));
#307075=CARTESIAN_POINT('Ctrl Pts',(-3.30337878900006,12.2,2.58993855299998));
#307076=CARTESIAN_POINT('Ctrl Pts',(-3.30337878900006,5.2,2.58993855299998));
#307077=CARTESIAN_POINT('Ctrl Pts',(-3.30337878900006,2.2,2.58993855299998));
#307078=CARTESIAN_POINT('Ctrl Pts',(-3.30479813300005,12.2,2.59045882499999));
#307079=CARTESIAN_POINT('Ctrl Pts',(-3.30479813300005,5.2,2.59045882499999));
#307080=CARTESIAN_POINT('Ctrl Pts',(-3.30479813300005,2.2,2.59045882499999));
#307081=CARTESIAN_POINT('Ctrl Pts',(-3.30622249500006,12.2,2.59097905199998));
#307082=CARTESIAN_POINT('Ctrl Pts',(-3.30622249500006,5.2,2.59097905199998));
#307083=CARTESIAN_POINT('Ctrl Pts',(-3.30622249500006,2.2,2.59097905199998));
#307084=CARTESIAN_POINT('Ctrl Pts',(-3.30765187100006,12.2,2.59149922099999));
#307085=CARTESIAN_POINT('Ctrl Pts',(-3.30765187100006,5.2,2.59149922099999));
#307086=CARTESIAN_POINT('Ctrl Pts',(-3.30765187100006,2.2,2.59149922099999));
#307087=CARTESIAN_POINT('Ctrl Pts',(-3.30908625600005,12.2,2.59201931899998));
#307088=CARTESIAN_POINT('Ctrl Pts',(-3.30908625600005,5.2,2.59201931899998));
#307089=CARTESIAN_POINT('Ctrl Pts',(-3.30908625600005,2.2,2.59201931899998));
#307090=CARTESIAN_POINT('Ctrl Pts',(-3.31052564600005,12.2,2.59253933499998));
#307091=CARTESIAN_POINT('Ctrl Pts',(-3.31052564600005,5.2,2.59253933499998));
#307092=CARTESIAN_POINT('Ctrl Pts',(-3.31052564600005,2.2,2.59253933499998));
#307093=CARTESIAN_POINT('Ctrl Pts',(-3.31197003500006,12.2,2.59305925499999));
#307094=CARTESIAN_POINT('Ctrl Pts',(-3.31197003500006,5.2,2.59305925499999));
#307095=CARTESIAN_POINT('Ctrl Pts',(-3.31197003500006,2.2,2.59305925499999));
#307096=CARTESIAN_POINT('Ctrl Pts',(-3.31341941900006,12.2,2.59357906899999));
#307097=CARTESIAN_POINT('Ctrl Pts',(-3.31341941900006,5.2,2.59357906899999));
#307098=CARTESIAN_POINT('Ctrl Pts',(-3.31341941900006,2.2,2.59357906899999));
#307099=CARTESIAN_POINT('Ctrl Pts',(-3.31487379500006,12.2,2.59409876299999));
#307100=CARTESIAN_POINT('Ctrl Pts',(-3.31487379500006,5.2,2.59409876299999));
#307101=CARTESIAN_POINT('Ctrl Pts',(-3.31487379500006,2.2,2.59409876299999));
#307102=CARTESIAN_POINT('Ctrl Pts',(-3.31633315600006,12.2,2.59461832399998));
#307103=CARTESIAN_POINT('Ctrl Pts',(-3.31633315600006,5.2,2.59461832399998));
#307104=CARTESIAN_POINT('Ctrl Pts',(-3.31633315600006,2.2,2.59461832399998));
#307105=CARTESIAN_POINT('Ctrl Pts',(-3.31779749900006,12.2,2.59513774099998));
#307106=CARTESIAN_POINT('Ctrl Pts',(-3.31779749900006,5.2,2.59513774099998));
#307107=CARTESIAN_POINT('Ctrl Pts',(-3.31779749900006,2.2,2.59513774099998));
#307108=CARTESIAN_POINT('Ctrl Pts',(-3.31926681800006,12.2,2.59565700299999));
#307109=CARTESIAN_POINT('Ctrl Pts',(-3.31926681800006,5.2,2.59565700299999));
#307110=CARTESIAN_POINT('Ctrl Pts',(-3.31926681800006,2.2,2.59565700299999));
#307111=CARTESIAN_POINT('Ctrl Pts',(-3.32074110900006,12.2,2.59617609599999));
#307112=CARTESIAN_POINT('Ctrl Pts',(-3.32074110900006,5.2,2.59617609599999));
#307113=CARTESIAN_POINT('Ctrl Pts',(-3.32074110900006,2.2,2.59617609599999));
#307114=CARTESIAN_POINT('Ctrl Pts',(-3.32222036700006,12.2,2.59669500799999));
#307115=CARTESIAN_POINT('Ctrl Pts',(-3.32222036700006,5.2,2.59669500799999));
#307116=CARTESIAN_POINT('Ctrl Pts',(-3.32222036700006,2.2,2.59669500799999));
#307117=CARTESIAN_POINT('Ctrl Pts',(-3.32370458800006,12.2,2.59721372699998));
#307118=CARTESIAN_POINT('Ctrl Pts',(-3.32370458800006,5.2,2.59721372699998));
#307119=CARTESIAN_POINT('Ctrl Pts',(-3.32370458800006,2.2,2.59721372699998));
#307120=CARTESIAN_POINT('Ctrl Pts',(-3.32519376600006,12.2,2.59773224199999));
#307121=CARTESIAN_POINT('Ctrl Pts',(-3.32519376600006,5.2,2.59773224199999));
#307122=CARTESIAN_POINT('Ctrl Pts',(-3.32519376600006,2.2,2.59773224199999));
#307123=CARTESIAN_POINT('Ctrl Pts',(-3.32668789800006,12.2,2.59825053999998));
#307124=CARTESIAN_POINT('Ctrl Pts',(-3.32668789800006,5.2,2.59825053999998));
#307125=CARTESIAN_POINT('Ctrl Pts',(-3.32668789800006,2.2,2.59825053999998));
#307126=CARTESIAN_POINT('Ctrl Pts',(-3.32818697700006,12.2,2.59876860899999));
#307127=CARTESIAN_POINT('Ctrl Pts',(-3.32818697700006,5.2,2.59876860899999));
#307128=CARTESIAN_POINT('Ctrl Pts',(-3.32818697700006,2.2,2.59876860899999));
#307129=CARTESIAN_POINT('Ctrl Pts',(-3.32969100100006,12.2,2.59928643799999));
#307130=CARTESIAN_POINT('Ctrl Pts',(-3.32969100100006,5.2,2.59928643799999));
#307131=CARTESIAN_POINT('Ctrl Pts',(-3.32969100100006,2.2,2.59928643799999));
#307132=CARTESIAN_POINT('Ctrl Pts',(-3.33119996300006,12.2,2.59980401299998));
#307133=CARTESIAN_POINT('Ctrl Pts',(-3.33119996300006,5.2,2.59980401299998));
#307134=CARTESIAN_POINT('Ctrl Pts',(-3.33119996300006,2.2,2.59980401299998));
#307135=CARTESIAN_POINT('Ctrl Pts',(-3.33271385900006,12.2,2.60032132499998));
#307136=CARTESIAN_POINT('Ctrl Pts',(-3.33271385900006,5.2,2.60032132499998));
#307137=CARTESIAN_POINT('Ctrl Pts',(-3.33271385900006,2.2,2.60032132499998));
#307138=CARTESIAN_POINT('Ctrl Pts',(-3.33423268400006,12.2,2.60083835899999));
#307139=CARTESIAN_POINT('Ctrl Pts',(-3.33423268400006,5.2,2.60083835899999));
#307140=CARTESIAN_POINT('Ctrl Pts',(-3.33423268400006,2.2,2.60083835899999));
#307141=CARTESIAN_POINT('Ctrl Pts',(-3.33575643400006,12.2,2.60135510599999));
#307142=CARTESIAN_POINT('Ctrl Pts',(-3.33575643400006,5.2,2.60135510599999));
#307143=CARTESIAN_POINT('Ctrl Pts',(-3.33575643400006,2.2,2.60135510599999));
#307144=CARTESIAN_POINT('Ctrl Pts',(-3.33728510500006,12.2,2.60187155199999));
#307145=CARTESIAN_POINT('Ctrl Pts',(-3.33728510500006,5.2,2.60187155199999));
#307146=CARTESIAN_POINT('Ctrl Pts',(-3.33728510500006,2.2,2.60187155199999));
#307147=CARTESIAN_POINT('Ctrl Pts',(-3.33881868900006,12.2,2.60238768599999));
#307148=CARTESIAN_POINT('Ctrl Pts',(-3.33881868900006,5.2,2.60238768599999));
#307149=CARTESIAN_POINT('Ctrl Pts',(-3.33881868900006,2.2,2.60238768599999));
#307150=CARTESIAN_POINT('Ctrl Pts',(-3.34035718400005,12.2,2.60290349699999));
#307151=CARTESIAN_POINT('Ctrl Pts',(-3.34035718400005,5.2,2.60290349699999));
#307152=CARTESIAN_POINT('Ctrl Pts',(-3.34035718400005,2.2,2.60290349699999));
#307153=CARTESIAN_POINT('Ctrl Pts',(-3.34190058500006,12.2,2.60341897199999));
#307154=CARTESIAN_POINT('Ctrl Pts',(-3.34190058500006,5.2,2.60341897199999));
#307155=CARTESIAN_POINT('Ctrl Pts',(-3.34190058500006,2.2,2.60341897199999));
#307156=CARTESIAN_POINT('Ctrl Pts',(-3.34344888600006,12.2,2.60393409999998));
#307157=CARTESIAN_POINT('Ctrl Pts',(-3.34344888600006,5.2,2.60393409999998));
#307158=CARTESIAN_POINT('Ctrl Pts',(-3.34344888600006,2.2,2.60393409999998));
#307159=CARTESIAN_POINT('Ctrl Pts',(-3.34500208300006,12.2,2.60444886799998));
#307160=CARTESIAN_POINT('Ctrl Pts',(-3.34500208300006,5.2,2.60444886799998));
#307161=CARTESIAN_POINT('Ctrl Pts',(-3.34500208300006,2.2,2.60444886799998));
#307162=CARTESIAN_POINT('Ctrl Pts',(-3.34656017100006,12.2,2.60496326699998));
#307163=CARTESIAN_POINT('Ctrl Pts',(-3.34656017100006,5.2,2.60496326699998));
#307164=CARTESIAN_POINT('Ctrl Pts',(-3.34656017100006,2.2,2.60496326699998));
#307165=CARTESIAN_POINT('Ctrl Pts',(-3.34812314600006,12.2,2.60547728199998));
#307166=CARTESIAN_POINT('Ctrl Pts',(-3.34812314600006,5.2,2.60547728199998));
#307167=CARTESIAN_POINT('Ctrl Pts',(-3.34812314600006,2.2,2.60547728199998));
#307168=CARTESIAN_POINT('Ctrl Pts',(-3.34969100100006,12.2,2.60599090499999));
#307169=CARTESIAN_POINT('Ctrl Pts',(-3.34969100100006,5.2,2.60599090499999));
#307170=CARTESIAN_POINT('Ctrl Pts',(-3.34969100100006,2.2,2.60599090499999));
#307171=CARTESIAN_POINT('Ctrl Pts',(-3.35126373300006,12.2,2.60650412199999));
#307172=CARTESIAN_POINT('Ctrl Pts',(-3.35126373300006,5.2,2.60650412199999));
#307173=CARTESIAN_POINT('Ctrl Pts',(-3.35126373300006,2.2,2.60650412199999));
#307174=CARTESIAN_POINT('Ctrl Pts',(-3.35284133700006,12.2,2.60701692199999));
#307175=CARTESIAN_POINT('Ctrl Pts',(-3.35284133700006,5.2,2.60701692199999));
#307176=CARTESIAN_POINT('Ctrl Pts',(-3.35284133700006,2.2,2.60701692199999));
#307177=CARTESIAN_POINT('Ctrl Pts',(-3.35442380800006,12.2,2.60752929399998));
#307178=CARTESIAN_POINT('Ctrl Pts',(-3.35442380800006,5.2,2.60752929399998));
#307179=CARTESIAN_POINT('Ctrl Pts',(-3.35442380800006,2.2,2.60752929399998));
#307180=CARTESIAN_POINT('Ctrl Pts',(-3.35601114000006,12.2,2.60804122499999));
#307181=CARTESIAN_POINT('Ctrl Pts',(-3.35601114000006,5.2,2.60804122499999));
#307182=CARTESIAN_POINT('Ctrl Pts',(-3.35601114000006,2.2,2.60804122499999));
#307183=CARTESIAN_POINT('Ctrl Pts',(-3.35760333100006,12.2,2.60855270599999));
#307184=CARTESIAN_POINT('Ctrl Pts',(-3.35760333100006,5.2,2.60855270599999));
#307185=CARTESIAN_POINT('Ctrl Pts',(-3.35760333100006,2.2,2.60855270599999));
#307186=CARTESIAN_POINT('Ctrl Pts',(-3.35920037300005,12.2,2.60906372399998));
#307187=CARTESIAN_POINT('Ctrl Pts',(-3.35920037300005,5.2,2.60906372399998));
#307188=CARTESIAN_POINT('Ctrl Pts',(-3.35920037300005,2.2,2.60906372399998));
#307189=CARTESIAN_POINT('Ctrl Pts',(-3.36080226300006,12.2,2.60957426799998));
#307190=CARTESIAN_POINT('Ctrl Pts',(-3.36080226300006,5.2,2.60957426799998));
#307191=CARTESIAN_POINT('Ctrl Pts',(-3.36080226300006,2.2,2.60957426799998));
#307192=CARTESIAN_POINT('Ctrl Pts',(-3.36240899500006,12.2,2.61008432499998));
#307193=CARTESIAN_POINT('Ctrl Pts',(-3.36240899500006,5.2,2.61008432499998));
#307194=CARTESIAN_POINT('Ctrl Pts',(-3.36240899500006,2.2,2.61008432499998));
#307195=CARTESIAN_POINT('Ctrl Pts',(-3.36402056500006,12.2,2.61059388699999));
#307196=CARTESIAN_POINT('Ctrl Pts',(-3.36402056500006,5.2,2.61059388699999));
#307197=CARTESIAN_POINT('Ctrl Pts',(-3.36402056500006,2.2,2.61059388699999));
#307198=CARTESIAN_POINT('Ctrl Pts',(-3.36563696800006,12.2,2.61110293999998));
#307199=CARTESIAN_POINT('Ctrl Pts',(-3.36563696800006,5.2,2.61110293999998));
#307200=CARTESIAN_POINT('Ctrl Pts',(-3.36563696800006,2.2,2.61110293999998));
#307201=CARTESIAN_POINT('Ctrl Pts',(-3.36725819900006,12.2,2.61161147299998));
#307202=CARTESIAN_POINT('Ctrl Pts',(-3.36725819900006,5.2,2.61161147299998));
#307203=CARTESIAN_POINT('Ctrl Pts',(-3.36725819900006,2.2,2.61161147299998));
#307204=CARTESIAN_POINT('Ctrl Pts',(-3.36888425300006,12.2,2.61211947599998));
#307205=CARTESIAN_POINT('Ctrl Pts',(-3.36888425300006,5.2,2.61211947599998));
#307206=CARTESIAN_POINT('Ctrl Pts',(-3.36888425300006,2.2,2.61211947599998));
#307207=CARTESIAN_POINT('Ctrl Pts',(-3.37051512400006,12.2,2.61262693699998));
#307208=CARTESIAN_POINT('Ctrl Pts',(-3.37051512400006,5.2,2.61262693699998));
#307209=CARTESIAN_POINT('Ctrl Pts',(-3.37051512400006,2.2,2.61262693699998));
#307210=CARTESIAN_POINT('Ctrl Pts',(-3.37215081000006,12.2,2.61313384499999));
#307211=CARTESIAN_POINT('Ctrl Pts',(-3.37215081000006,5.2,2.61313384499999));
#307212=CARTESIAN_POINT('Ctrl Pts',(-3.37215081000006,2.2,2.61313384499999));
#307213=CARTESIAN_POINT('Ctrl Pts',(-3.37379130200006,12.2,2.61364018799998));
#307214=CARTESIAN_POINT('Ctrl Pts',(-3.37379130200006,5.2,2.61364018799998));
#307215=CARTESIAN_POINT('Ctrl Pts',(-3.37379130200006,2.2,2.61364018799998));
#307216=CARTESIAN_POINT('Ctrl Pts',(-3.37543659900006,12.2,2.61414595499998));
#307217=CARTESIAN_POINT('Ctrl Pts',(-3.37543659900006,5.2,2.61414595499998));
#307218=CARTESIAN_POINT('Ctrl Pts',(-3.37543659900006,2.2,2.61414595499998));
#307219=CARTESIAN_POINT('Ctrl Pts',(-3.37708669500006,12.2,2.61465113699998));
#307220=CARTESIAN_POINT('Ctrl Pts',(-3.37708669500006,5.2,2.61465113699998));
#307221=CARTESIAN_POINT('Ctrl Pts',(-3.37708669500006,2.2,2.61465113699998));
#307222=CARTESIAN_POINT('Ctrl Pts',(-3.37874158300006,12.2,2.61515571999999));
#307223=CARTESIAN_POINT('Ctrl Pts',(-3.37874158300006,5.2,2.61515571999999));
#307224=CARTESIAN_POINT('Ctrl Pts',(-3.37874158300006,2.2,2.61515571999999));
#307225=CARTESIAN_POINT('Ctrl Pts',(-3.38040126000006,12.2,2.61565969399999));
#307226=CARTESIAN_POINT('Ctrl Pts',(-3.38040126000006,5.2,2.61565969399999));
#307227=CARTESIAN_POINT('Ctrl Pts',(-3.38040126000006,2.2,2.61565969399999));
#307228=CARTESIAN_POINT('Ctrl Pts',(-3.38206572100006,12.2,2.61616304899999));
#307229=CARTESIAN_POINT('Ctrl Pts',(-3.38206572100006,5.2,2.61616304899999));
#307230=CARTESIAN_POINT('Ctrl Pts',(-3.38206572100006,2.2,2.61616304899999));
#307231=CARTESIAN_POINT('Ctrl Pts',(-3.38373496000006,12.2,2.61666577199998));
#307232=CARTESIAN_POINT('Ctrl Pts',(-3.38373496000006,5.2,2.61666577199998));
#307233=CARTESIAN_POINT('Ctrl Pts',(-3.38373496000006,2.2,2.61666577199998));
#307234=CARTESIAN_POINT('Ctrl Pts',(-3.38540897300006,12.2,2.61716785299999));
#307235=CARTESIAN_POINT('Ctrl Pts',(-3.38540897300006,5.2,2.61716785299999));
#307236=CARTESIAN_POINT('Ctrl Pts',(-3.38540897300006,2.2,2.61716785299999));
#307237=CARTESIAN_POINT('Ctrl Pts',(-3.38708775500006,12.2,2.61766928299998));
#307238=CARTESIAN_POINT('Ctrl Pts',(-3.38708775500006,5.2,2.61766928299998));
#307239=CARTESIAN_POINT('Ctrl Pts',(-3.38708775500006,2.2,2.61766928299998));
#307240=CARTESIAN_POINT('Ctrl Pts',(-3.38877130000005,12.2,2.61817004799998));
#307241=CARTESIAN_POINT('Ctrl Pts',(-3.38877130000005,5.2,2.61817004799998));
#307242=CARTESIAN_POINT('Ctrl Pts',(-3.38877130000005,2.2,2.61817004799998));
#307243=CARTESIAN_POINT('Ctrl Pts',(-3.39045960500005,12.2,2.61867013699998));
#307244=CARTESIAN_POINT('Ctrl Pts',(-3.39045960500005,5.2,2.61867013699998));
#307245=CARTESIAN_POINT('Ctrl Pts',(-3.39045960500005,2.2,2.61867013699998));
#307246=CARTESIAN_POINT('Ctrl Pts',(-3.39215266200006,12.2,2.61916954299998));
#307247=CARTESIAN_POINT('Ctrl Pts',(-3.39215266200006,5.2,2.61916954299998));
#307248=CARTESIAN_POINT('Ctrl Pts',(-3.39215266200006,2.2,2.61916954299998));
#307249=CARTESIAN_POINT('Ctrl Pts',(-3.39385047000006,12.2,2.61966825099999));
#307250=CARTESIAN_POINT('Ctrl Pts',(-3.39385047000006,5.2,2.61966825099999));
#307251=CARTESIAN_POINT('Ctrl Pts',(-3.39385047000006,2.2,2.61966825099999));
#307252=CARTESIAN_POINT('Ctrl Pts',(-3.39555302000006,12.2,2.62016625199998));
#307253=CARTESIAN_POINT('Ctrl Pts',(-3.39555302000006,5.2,2.62016625199998));
#307254=CARTESIAN_POINT('Ctrl Pts',(-3.39555302000006,2.2,2.62016625199998));
#307255=CARTESIAN_POINT('Ctrl Pts',(-3.39726030900006,12.2,2.62066353399998));
#307256=CARTESIAN_POINT('Ctrl Pts',(-3.39726030900006,5.2,2.62066353399998));
#307257=CARTESIAN_POINT('Ctrl Pts',(-3.39726030900006,2.2,2.62066353399998));
#307258=CARTESIAN_POINT('Ctrl Pts',(-3.39897233300006,12.2,2.62116008899999));
#307259=CARTESIAN_POINT('Ctrl Pts',(-3.39897233300006,5.2,2.62116008899999));
#307260=CARTESIAN_POINT('Ctrl Pts',(-3.39897233300006,2.2,2.62116008899999));
#307261=CARTESIAN_POINT('Ctrl Pts',(-3.40068908500006,12.2,2.62165590199999));
#307262=CARTESIAN_POINT('Ctrl Pts',(-3.40068908500006,5.2,2.62165590199999));
#307263=CARTESIAN_POINT('Ctrl Pts',(-3.40068908500006,2.2,2.62165590199999));
#307264=CARTESIAN_POINT('Ctrl Pts',(-3.40241056000006,12.2,2.62215096699999));
#307265=CARTESIAN_POINT('Ctrl Pts',(-3.40241056000006,5.2,2.62215096699999));
#307266=CARTESIAN_POINT('Ctrl Pts',(-3.40241056000006,2.2,2.62215096699999));
#307267=CARTESIAN_POINT('Ctrl Pts',(-3.40413675500006,12.2,2.62264526799999));
#307268=CARTESIAN_POINT('Ctrl Pts',(-3.40413675500006,5.2,2.62264526799999));
#307269=CARTESIAN_POINT('Ctrl Pts',(-3.40413675500006,2.2,2.62264526799999));
#307270=CARTESIAN_POINT('Ctrl Pts',(-3.40586766300006,12.2,2.62313879999999));
#307271=CARTESIAN_POINT('Ctrl Pts',(-3.40586766300006,5.2,2.62313879999999));
#307272=CARTESIAN_POINT('Ctrl Pts',(-3.40586766300006,2.2,2.62313879999999));
#307273=CARTESIAN_POINT('Ctrl Pts',(-3.40760327900006,12.2,2.62363154799999));
#307274=CARTESIAN_POINT('Ctrl Pts',(-3.40760327900006,5.2,2.62363154799999));
#307275=CARTESIAN_POINT('Ctrl Pts',(-3.40760327900006,2.2,2.62363154799999));
#307276=CARTESIAN_POINT('Ctrl Pts',(-3.40934360000006,12.2,2.62412350299999));
#307277=CARTESIAN_POINT('Ctrl Pts',(-3.40934360000006,5.2,2.62412350299999));
#307278=CARTESIAN_POINT('Ctrl Pts',(-3.40934360000006,2.2,2.62412350299999));
#307279=CARTESIAN_POINT('Ctrl Pts',(-3.41108862000006,12.2,2.62461465499998));
#307280=CARTESIAN_POINT('Ctrl Pts',(-3.41108862000006,5.2,2.62461465499998));
#307281=CARTESIAN_POINT('Ctrl Pts',(-3.41108862000006,2.2,2.62461465499998));
#307282=CARTESIAN_POINT('Ctrl Pts',(-3.41283833100006,12.2,2.62510499299999));
#307283=CARTESIAN_POINT('Ctrl Pts',(-3.41283833100006,5.2,2.62510499299999));
#307284=CARTESIAN_POINT('Ctrl Pts',(-3.41283833100006,2.2,2.62510499299999));
#307285=CARTESIAN_POINT('Ctrl Pts',(-3.41459273300006,12.2,2.62559450499998));
#307286=CARTESIAN_POINT('Ctrl Pts',(-3.41459273300006,5.2,2.62559450499998));
#307287=CARTESIAN_POINT('Ctrl Pts',(-3.41459273300006,2.2,2.62559450499998));
#307288=CARTESIAN_POINT('Ctrl Pts',(-3.41635181700005,12.2,2.62608318199998));
#307289=CARTESIAN_POINT('Ctrl Pts',(-3.41635181700005,5.2,2.62608318199998));
#307290=CARTESIAN_POINT('Ctrl Pts',(-3.41635181700005,2.2,2.62608318199998));
#307291=CARTESIAN_POINT('Ctrl Pts',(-3.41811558000006,12.2,2.62657101299999));
#307292=CARTESIAN_POINT('Ctrl Pts',(-3.41811558000006,5.2,2.62657101299999));
#307293=CARTESIAN_POINT('Ctrl Pts',(-3.41811558000006,2.2,2.62657101299999));
#307294=CARTESIAN_POINT('Ctrl Pts',(-3.41988401600006,12.2,2.62705798799999));
#307295=CARTESIAN_POINT('Ctrl Pts',(-3.41988401600006,5.2,2.62705798799999));
#307296=CARTESIAN_POINT('Ctrl Pts',(-3.41988401600006,2.2,2.62705798799999));
#307297=CARTESIAN_POINT('Ctrl Pts',(-3.42165712000006,12.2,2.62754409599999));
#307298=CARTESIAN_POINT('Ctrl Pts',(-3.42165712000006,5.2,2.62754409599999));
#307299=CARTESIAN_POINT('Ctrl Pts',(-3.42165712000006,2.2,2.62754409599999));
#307300=CARTESIAN_POINT('Ctrl Pts',(-3.42343488700006,12.2,2.62802932799998));
#307301=CARTESIAN_POINT('Ctrl Pts',(-3.42343488700006,5.2,2.62802932799998));
#307302=CARTESIAN_POINT('Ctrl Pts',(-3.42343488700006,2.2,2.62802932799998));
#307303=CARTESIAN_POINT('Ctrl Pts',(-3.42521731200006,12.2,2.62851367099999));
#307304=CARTESIAN_POINT('Ctrl Pts',(-3.42521731200006,5.2,2.62851367099999));
#307305=CARTESIAN_POINT('Ctrl Pts',(-3.42521731200006,2.2,2.62851367099999));
#307306=CARTESIAN_POINT('Ctrl Pts',(-3.42700439000006,12.2,2.62899711699998));
#307307=CARTESIAN_POINT('Ctrl Pts',(-3.42700439000006,5.2,2.62899711699998));
#307308=CARTESIAN_POINT('Ctrl Pts',(-3.42700439000006,2.2,2.62899711699998));
#307309=CARTESIAN_POINT('Ctrl Pts',(-3.42879611600006,12.2,2.62947965299999));
#307310=CARTESIAN_POINT('Ctrl Pts',(-3.42879611600006,5.2,2.62947965299999));
#307311=CARTESIAN_POINT('Ctrl Pts',(-3.42879611600006,2.2,2.62947965299999));
#307312=CARTESIAN_POINT('Ctrl Pts',(-3.43059248500006,12.2,2.62996127199998));
#307313=CARTESIAN_POINT('Ctrl Pts',(-3.43059248500006,5.2,2.62996127199998));
#307314=CARTESIAN_POINT('Ctrl Pts',(-3.43059248500006,2.2,2.62996127199998));
#307315=CARTESIAN_POINT('Ctrl Pts',(-3.43239349100006,12.2,2.63044195999999));
#307316=CARTESIAN_POINT('Ctrl Pts',(-3.43239349100006,5.2,2.63044195999999));
#307317=CARTESIAN_POINT('Ctrl Pts',(-3.43239349100006,2.2,2.63044195999999));
#307318=CARTESIAN_POINT('Ctrl Pts',(-3.43419913000006,12.2,2.63092171099998));
#307319=CARTESIAN_POINT('Ctrl Pts',(-3.43419913000006,5.2,2.63092171099998));
#307320=CARTESIAN_POINT('Ctrl Pts',(-3.43419913000006,2.2,2.63092171099998));
#307321=CARTESIAN_POINT('Ctrl Pts',(-3.43600939600006,12.2,2.63140051199999));
#307322=CARTESIAN_POINT('Ctrl Pts',(-3.43600939600006,5.2,2.63140051199999));
#307323=CARTESIAN_POINT('Ctrl Pts',(-3.43600939600006,2.2,2.63140051199999));
#307324=CARTESIAN_POINT('Ctrl Pts',(-3.43782428400006,12.2,2.63187835199999));
#307325=CARTESIAN_POINT('Ctrl Pts',(-3.43782428400006,5.2,2.63187835199999));
#307326=CARTESIAN_POINT('Ctrl Pts',(-3.43782428400006,2.2,2.63187835199999));
#307327=CARTESIAN_POINT('Ctrl Pts',(-3.43964378900006,12.2,2.63235522299999));
#307328=CARTESIAN_POINT('Ctrl Pts',(-3.43964378900006,5.2,2.63235522299999));
#307329=CARTESIAN_POINT('Ctrl Pts',(-3.43964378900006,2.2,2.63235522299999));
#307330=CARTESIAN_POINT('Ctrl Pts',(-3.44146790600006,12.2,2.63283111299998));
#307331=CARTESIAN_POINT('Ctrl Pts',(-3.44146790600006,5.2,2.63283111299998));
#307332=CARTESIAN_POINT('Ctrl Pts',(-3.44146790600006,2.2,2.63283111299998));
#307333=CARTESIAN_POINT('Ctrl Pts',(-3.44329663000006,12.2,2.63330601399999));
#307334=CARTESIAN_POINT('Ctrl Pts',(-3.44329663000006,5.2,2.63330601399999));
#307335=CARTESIAN_POINT('Ctrl Pts',(-3.44329663000006,2.2,2.63330601399999));
#307336=CARTESIAN_POINT('Ctrl Pts',(-3.44512995600006,12.2,2.63377991399998));
#307337=CARTESIAN_POINT('Ctrl Pts',(-3.44512995600006,5.2,2.63377991399998));
#307338=CARTESIAN_POINT('Ctrl Pts',(-3.44512995600006,2.2,2.63377991399998));
#307339=CARTESIAN_POINT('Ctrl Pts',(-3.44696787800005,12.2,2.63425280299998));
#307340=CARTESIAN_POINT('Ctrl Pts',(-3.44696787800005,5.2,2.63425280299998));
#307341=CARTESIAN_POINT('Ctrl Pts',(-3.44696787800005,2.2,2.63425280299998));
#307342=CARTESIAN_POINT('Ctrl Pts',(-3.44881039100006,12.2,2.63472467199998));
#307343=CARTESIAN_POINT('Ctrl Pts',(-3.44881039100006,5.2,2.63472467199998));
#307344=CARTESIAN_POINT('Ctrl Pts',(-3.44881039100006,2.2,2.63472467199998));
#307345=CARTESIAN_POINT('Ctrl Pts',(-3.45065749100006,12.2,2.63519550999998));
#307346=CARTESIAN_POINT('Ctrl Pts',(-3.45065749100006,5.2,2.63519550999998));
#307347=CARTESIAN_POINT('Ctrl Pts',(-3.45065749100006,2.2,2.63519550999998));
#307348=CARTESIAN_POINT('Ctrl Pts',(-3.45250917200006,12.2,2.63566530699999));
#307349=CARTESIAN_POINT('Ctrl Pts',(-3.45250917200006,5.2,2.63566530699999));
#307350=CARTESIAN_POINT('Ctrl Pts',(-3.45250917200006,2.2,2.63566530699999));
#307351=CARTESIAN_POINT('Ctrl Pts',(-3.45436542900006,12.2,2.63613405299999));
#307352=CARTESIAN_POINT('Ctrl Pts',(-3.45436542900006,5.2,2.63613405299999));
#307353=CARTESIAN_POINT('Ctrl Pts',(-3.45436542900006,2.2,2.63613405299999));
#307354=CARTESIAN_POINT('Ctrl Pts',(-3.45622625500006,12.2,2.63660173899999));
#307355=CARTESIAN_POINT('Ctrl Pts',(-3.45622625500006,5.2,2.63660173899999));
#307356=CARTESIAN_POINT('Ctrl Pts',(-3.45622625500006,2.2,2.63660173899999));
#307357=CARTESIAN_POINT('Ctrl Pts',(-3.45809164800006,12.2,2.63706835399999));
#307358=CARTESIAN_POINT('Ctrl Pts',(-3.45809164800006,5.2,2.63706835399999));
#307359=CARTESIAN_POINT('Ctrl Pts',(-3.45809164800006,2.2,2.63706835399999));
#307360=CARTESIAN_POINT('Ctrl Pts',(-3.45996160100006,12.2,2.63753388799999));
#307361=CARTESIAN_POINT('Ctrl Pts',(-3.45996160100006,5.2,2.63753388799999));
#307362=CARTESIAN_POINT('Ctrl Pts',(-3.45996160100006,2.2,2.63753388799999));
#307363=CARTESIAN_POINT('Ctrl Pts',(-3.46183610800006,12.2,2.63799833099998));
#307364=CARTESIAN_POINT('Ctrl Pts',(-3.46183610800006,5.2,2.63799833099998));
#307365=CARTESIAN_POINT('Ctrl Pts',(-3.46183610800006,2.2,2.63799833099998));
#307366=CARTESIAN_POINT('Ctrl Pts',(-3.46371516600006,12.2,2.63846167499998));
#307367=CARTESIAN_POINT('Ctrl Pts',(-3.46371516600006,5.2,2.63846167499998));
#307368=CARTESIAN_POINT('Ctrl Pts',(-3.46371516600006,2.2,2.63846167499998));
#307369=CARTESIAN_POINT('Ctrl Pts',(-3.46559876800006,12.2,2.63892390799998));
#307370=CARTESIAN_POINT('Ctrl Pts',(-3.46559876800006,5.2,2.63892390799998));
#307371=CARTESIAN_POINT('Ctrl Pts',(-3.46559876800006,2.2,2.63892390799998));
#307372=CARTESIAN_POINT('Ctrl Pts',(-3.46748691000006,12.2,2.63938501999998));
#307373=CARTESIAN_POINT('Ctrl Pts',(-3.46748691000006,5.2,2.63938501999998));
#307374=CARTESIAN_POINT('Ctrl Pts',(-3.46748691000006,2.2,2.63938501999998));
#307375=CARTESIAN_POINT('Ctrl Pts',(-3.46937958700006,12.2,2.63984500299999));
#307376=CARTESIAN_POINT('Ctrl Pts',(-3.46937958700006,5.2,2.63984500299999));
#307377=CARTESIAN_POINT('Ctrl Pts',(-3.46937958700006,2.2,2.63984500299999));
#307378=CARTESIAN_POINT('Ctrl Pts',(-3.47127679100006,12.2,2.64030384499998));
#307379=CARTESIAN_POINT('Ctrl Pts',(-3.47127679100006,5.2,2.64030384499998));
#307380=CARTESIAN_POINT('Ctrl Pts',(-3.47127679100006,2.2,2.64030384499998));
#307381=CARTESIAN_POINT('Ctrl Pts',(-3.47317852100006,12.2,2.64076153799999));
#307382=CARTESIAN_POINT('Ctrl Pts',(-3.47317852100006,5.2,2.64076153799999));
#307383=CARTESIAN_POINT('Ctrl Pts',(-3.47317852100006,2.2,2.64076153799999));
#307384=CARTESIAN_POINT('Ctrl Pts',(-3.47508476800006,12.2,2.64121807199999));
#307385=CARTESIAN_POINT('Ctrl Pts',(-3.47508476800006,5.2,2.64121807199999));
#307386=CARTESIAN_POINT('Ctrl Pts',(-3.47508476800006,2.2,2.64121807199999));
#307387=CARTESIAN_POINT('Ctrl Pts',(-3.47699552900006,12.2,2.64167343599999));
#307388=CARTESIAN_POINT('Ctrl Pts',(-3.47699552900006,5.2,2.64167343599999));
#307389=CARTESIAN_POINT('Ctrl Pts',(-3.47699552900006,2.2,2.64167343599999));
#307390=CARTESIAN_POINT('Ctrl Pts',(-3.47891079800006,12.2,2.64212762199998));
#307391=CARTESIAN_POINT('Ctrl Pts',(-3.47891079800006,5.2,2.64212762199998));
#307392=CARTESIAN_POINT('Ctrl Pts',(-3.47891079800006,2.2,2.64212762199998));
#307393=CARTESIAN_POINT('Ctrl Pts',(-3.48083056900006,12.2,2.64258061899999));
#307394=CARTESIAN_POINT('Ctrl Pts',(-3.48083056900006,5.2,2.64258061899999));
#307395=CARTESIAN_POINT('Ctrl Pts',(-3.48083056900006,2.2,2.64258061899999));
#307396=CARTESIAN_POINT('Ctrl Pts',(-3.48275483900006,12.2,2.64303241699999));
#307397=CARTESIAN_POINT('Ctrl Pts',(-3.48275483900006,5.2,2.64303241699999));
#307398=CARTESIAN_POINT('Ctrl Pts',(-3.48275483900006,2.2,2.64303241699999));
#307399=CARTESIAN_POINT('Ctrl Pts',(-3.48468360100005,12.2,2.64348300799998));
#307400=CARTESIAN_POINT('Ctrl Pts',(-3.48468360100005,5.2,2.64348300799998));
#307401=CARTESIAN_POINT('Ctrl Pts',(-3.48468360100005,2.2,2.64348300799998));
#307402=CARTESIAN_POINT('Ctrl Pts',(-3.48661684900006,12.2,2.64393238199998));
#307403=CARTESIAN_POINT('Ctrl Pts',(-3.48661684900006,5.2,2.64393238199998));
#307404=CARTESIAN_POINT('Ctrl Pts',(-3.48661684900006,2.2,2.64393238199998));
#307405=CARTESIAN_POINT('Ctrl Pts',(-3.48855458000005,12.2,2.64438052799999));
#307406=CARTESIAN_POINT('Ctrl Pts',(-3.48855458000005,5.2,2.64438052799999));
#307407=CARTESIAN_POINT('Ctrl Pts',(-3.48855458000005,2.2,2.64438052799999));
#307408=CARTESIAN_POINT('Ctrl Pts',(-3.49049678700006,12.2,2.64482743799999));
#307409=CARTESIAN_POINT('Ctrl Pts',(-3.49049678700006,5.2,2.64482743799999));
#307410=CARTESIAN_POINT('Ctrl Pts',(-3.49049678700006,2.2,2.64482743799999));
#307411=CARTESIAN_POINT('Ctrl Pts',(-3.49244346600006,12.2,2.64527310199998));
#307412=CARTESIAN_POINT('Ctrl Pts',(-3.49244346600006,5.2,2.64527310199998));
#307413=CARTESIAN_POINT('Ctrl Pts',(-3.49244346600006,2.2,2.64527310199998));
#307414=CARTESIAN_POINT('Ctrl Pts',(-3.49439461000005,12.2,2.64571750999998));
#307415=CARTESIAN_POINT('Ctrl Pts',(-3.49439461000005,5.2,2.64571750999998));
#307416=CARTESIAN_POINT('Ctrl Pts',(-3.49439461000005,2.2,2.64571750999998));
#307417=CARTESIAN_POINT('Ctrl Pts',(-3.49635021500006,12.2,2.64616065299998));
#307418=CARTESIAN_POINT('Ctrl Pts',(-3.49635021500006,5.2,2.64616065299998));
#307419=CARTESIAN_POINT('Ctrl Pts',(-3.49635021500006,2.2,2.64616065299998));
#307420=CARTESIAN_POINT('Ctrl Pts',(-3.49831027600006,12.2,2.64660251999998));
#307421=CARTESIAN_POINT('Ctrl Pts',(-3.49831027600006,5.2,2.64660251999998));
#307422=CARTESIAN_POINT('Ctrl Pts',(-3.49831027600006,2.2,2.64660251999998));
#307423=CARTESIAN_POINT('Ctrl Pts',(-3.50027478700006,12.2,2.64704310399999));
#307424=CARTESIAN_POINT('Ctrl Pts',(-3.50027478700006,5.2,2.64704310399999));
#307425=CARTESIAN_POINT('Ctrl Pts',(-3.50027478700006,2.2,2.64704310399999));
#307426=CARTESIAN_POINT('Ctrl Pts',(-3.50224374300006,12.2,2.64748239399999));
#307427=CARTESIAN_POINT('Ctrl Pts',(-3.50224374300006,5.2,2.64748239399999));
#307428=CARTESIAN_POINT('Ctrl Pts',(-3.50224374300006,2.2,2.64748239399999));
#307429=CARTESIAN_POINT('Ctrl Pts',(-3.50421713800006,12.2,2.64792038099999));
#307430=CARTESIAN_POINT('Ctrl Pts',(-3.50421713800006,5.2,2.64792038099999));
#307431=CARTESIAN_POINT('Ctrl Pts',(-3.50421713800006,2.2,2.64792038099999));
#307432=CARTESIAN_POINT('Ctrl Pts',(-3.50619496700006,12.2,2.64835705499999));
#307433=CARTESIAN_POINT('Ctrl Pts',(-3.50619496700006,5.2,2.64835705499999));
#307434=CARTESIAN_POINT('Ctrl Pts',(-3.50619496700006,2.2,2.64835705499999));
#307435=CARTESIAN_POINT('Ctrl Pts',(-3.50817722600006,12.2,2.64879240799999));
#307436=CARTESIAN_POINT('Ctrl Pts',(-3.50817722600006,5.2,2.64879240799999));
#307437=CARTESIAN_POINT('Ctrl Pts',(-3.50817722600006,2.2,2.64879240799999));
#307438=CARTESIAN_POINT('Ctrl Pts',(-3.51016390800006,12.2,2.64922642899998));
#307439=CARTESIAN_POINT('Ctrl Pts',(-3.51016390800006,5.2,2.64922642899998));
#307440=CARTESIAN_POINT('Ctrl Pts',(-3.51016390800006,2.2,2.64922642899998));
#307441=CARTESIAN_POINT('Ctrl Pts',(-3.51215500900006,12.2,2.64965911099999));
#307442=CARTESIAN_POINT('Ctrl Pts',(-3.51215500900006,5.2,2.64965911099999));
#307443=CARTESIAN_POINT('Ctrl Pts',(-3.51215500900006,2.2,2.64965911099999));
#307444=CARTESIAN_POINT('Ctrl Pts',(-3.51415052200006,12.2,2.65009044199999));
#307445=CARTESIAN_POINT('Ctrl Pts',(-3.51415052200006,5.2,2.65009044199999));
#307446=CARTESIAN_POINT('Ctrl Pts',(-3.51415052200006,2.2,2.65009044199999));
#307447=CARTESIAN_POINT('Ctrl Pts',(-3.51615044300006,12.2,2.65052041399999));
#307448=CARTESIAN_POINT('Ctrl Pts',(-3.51615044300006,5.2,2.65052041399999));
#307449=CARTESIAN_POINT('Ctrl Pts',(-3.51615044300006,2.2,2.65052041399999));
#307450=CARTESIAN_POINT('Ctrl Pts',(-3.51815476700006,12.2,2.65094901799999));
#307451=CARTESIAN_POINT('Ctrl Pts',(-3.51815476700006,5.2,2.65094901799999));
#307452=CARTESIAN_POINT('Ctrl Pts',(-3.51815476700006,2.2,2.65094901799999));
#307453=CARTESIAN_POINT('Ctrl Pts',(-3.52016348700006,12.2,2.65137624399999));
#307454=CARTESIAN_POINT('Ctrl Pts',(-3.52016348700006,5.2,2.65137624399999));
#307455=CARTESIAN_POINT('Ctrl Pts',(-3.52016348700006,2.2,2.65137624399999));
#307456=CARTESIAN_POINT('Ctrl Pts',(-3.52217659900006,12.2,2.65180208299999));
#307457=CARTESIAN_POINT('Ctrl Pts',(-3.52217659900006,5.2,2.65180208299999));
#307458=CARTESIAN_POINT('Ctrl Pts',(-3.52217659900006,2.2,2.65180208299999));
#307459=CARTESIAN_POINT('Ctrl Pts',(-3.52419409800006,12.2,2.65222652599999));
#307460=CARTESIAN_POINT('Ctrl Pts',(-3.52419409800006,5.2,2.65222652599999));
#307461=CARTESIAN_POINT('Ctrl Pts',(-3.52419409800006,2.2,2.65222652599999));
#307462=CARTESIAN_POINT('Ctrl Pts',(-3.52621597700006,12.2,2.65264956399999));
#307463=CARTESIAN_POINT('Ctrl Pts',(-3.52621597700006,5.2,2.65264956399999));
#307464=CARTESIAN_POINT('Ctrl Pts',(-3.52621597700006,2.2,2.65264956399999));
#307465=CARTESIAN_POINT('Ctrl Pts',(-3.52824223300006,12.2,2.65307118699998));
#307466=CARTESIAN_POINT('Ctrl Pts',(-3.52824223300006,5.2,2.65307118699998));
#307467=CARTESIAN_POINT('Ctrl Pts',(-3.52824223300006,2.2,2.65307118699998));
#307468=CARTESIAN_POINT('Ctrl Pts',(-3.53027285800006,12.2,2.65349138699998));
#307469=CARTESIAN_POINT('Ctrl Pts',(-3.53027285800006,5.2,2.65349138699998));
#307470=CARTESIAN_POINT('Ctrl Pts',(-3.53027285800006,2.2,2.65349138699998));
#307471=CARTESIAN_POINT('Ctrl Pts',(-3.53230784800005,12.2,2.65391015399998));
#307472=CARTESIAN_POINT('Ctrl Pts',(-3.53230784800005,5.2,2.65391015399998));
#307473=CARTESIAN_POINT('Ctrl Pts',(-3.53230784800005,2.2,2.65391015399998));
#307474=CARTESIAN_POINT('Ctrl Pts',(-3.53434719800005,12.2,2.65432747999998));
#307475=CARTESIAN_POINT('Ctrl Pts',(-3.53434719800005,5.2,2.65432747999998));
#307476=CARTESIAN_POINT('Ctrl Pts',(-3.53434719800005,2.2,2.65432747999998));
#307477=CARTESIAN_POINT('Ctrl Pts',(-3.53639090200006,12.2,2.65474335499999));
#307478=CARTESIAN_POINT('Ctrl Pts',(-3.53639090200006,5.2,2.65474335499999));
#307479=CARTESIAN_POINT('Ctrl Pts',(-3.53639090200006,2.2,2.65474335499999));
#307480=CARTESIAN_POINT('Ctrl Pts',(-3.53843895500006,12.2,2.65515776899999));
#307481=CARTESIAN_POINT('Ctrl Pts',(-3.53843895500006,5.2,2.65515776899999));
#307482=CARTESIAN_POINT('Ctrl Pts',(-3.53843895500006,2.2,2.65515776899999));
#307483=CARTESIAN_POINT('Ctrl Pts',(-3.54049135100006,12.2,2.65557071499998));
#307484=CARTESIAN_POINT('Ctrl Pts',(-3.54049135100006,5.2,2.65557071499998));
#307485=CARTESIAN_POINT('Ctrl Pts',(-3.54049135100006,2.2,2.65557071499998));
#307486=CARTESIAN_POINT('Ctrl Pts',(-3.54254808600006,12.2,2.65598218399998));
#307487=CARTESIAN_POINT('Ctrl Pts',(-3.54254808600006,5.2,2.65598218399998));
#307488=CARTESIAN_POINT('Ctrl Pts',(-3.54254808600006,2.2,2.65598218399998));
#307489=CARTESIAN_POINT('Ctrl Pts',(-3.54460915300006,12.2,2.65639216399999));
#307490=CARTESIAN_POINT('Ctrl Pts',(-3.54460915300006,5.2,2.65639216399999));
#307491=CARTESIAN_POINT('Ctrl Pts',(-3.54460915300006,2.2,2.65639216399999));
#307492=CARTESIAN_POINT('Ctrl Pts',(-3.54667454700006,12.2,2.65680064999999));
#307493=CARTESIAN_POINT('Ctrl Pts',(-3.54667454700006,5.2,2.65680064999999));
#307494=CARTESIAN_POINT('Ctrl Pts',(-3.54667454700006,2.2,2.65680064999999));
#307495=CARTESIAN_POINT('Ctrl Pts',(-3.54874426400006,12.2,2.65720763099999));
#307496=CARTESIAN_POINT('Ctrl Pts',(-3.54874426400006,5.2,2.65720763099999));
#307497=CARTESIAN_POINT('Ctrl Pts',(-3.54874426400006,2.2,2.65720763099999));
#307498=CARTESIAN_POINT('Ctrl Pts',(-3.55081829600006,12.2,2.65761309799998));
#307499=CARTESIAN_POINT('Ctrl Pts',(-3.55081829600006,5.2,2.65761309799998));
#307500=CARTESIAN_POINT('Ctrl Pts',(-3.55081829600006,2.2,2.65761309799998));
#307501=CARTESIAN_POINT('Ctrl Pts',(-3.55289663900006,12.2,2.65801704099999));
#307502=CARTESIAN_POINT('Ctrl Pts',(-3.55289663900006,5.2,2.65801704099999));
#307503=CARTESIAN_POINT('Ctrl Pts',(-3.55289663900006,2.2,2.65801704099999));
#307504=CARTESIAN_POINT('Ctrl Pts',(-3.55497929000006,12.2,2.65841945399998));
#307505=CARTESIAN_POINT('Ctrl Pts',(-3.55497929000006,5.2,2.65841945399998));
#307506=CARTESIAN_POINT('Ctrl Pts',(-3.55497929000006,2.2,2.65841945399998));
#307507=CARTESIAN_POINT('Ctrl Pts',(-3.55706623900006,12.2,2.65882032599999));
#307508=CARTESIAN_POINT('Ctrl Pts',(-3.55706623900006,5.2,2.65882032599999));
#307509=CARTESIAN_POINT('Ctrl Pts',(-3.55706623900006,2.2,2.65882032599999));
#307510=CARTESIAN_POINT('Ctrl Pts',(-3.55915748400006,12.2,2.65921964999999));
#307511=CARTESIAN_POINT('Ctrl Pts',(-3.55915748400006,5.2,2.65921964999999));
#307512=CARTESIAN_POINT('Ctrl Pts',(-3.55915748400006,2.2,2.65921964999999));
#307513=CARTESIAN_POINT('Ctrl Pts',(-3.56125301800006,12.2,2.65961741499999));
#307514=CARTESIAN_POINT('Ctrl Pts',(-3.56125301800006,5.2,2.65961741499999));
#307515=CARTESIAN_POINT('Ctrl Pts',(-3.56125301800006,2.2,2.65961741499999));
#307516=CARTESIAN_POINT('Ctrl Pts',(-3.56335283600006,12.2,2.66001361199999));
#307517=CARTESIAN_POINT('Ctrl Pts',(-3.56335283600006,5.2,2.66001361199999));
#307518=CARTESIAN_POINT('Ctrl Pts',(-3.56335283600006,2.2,2.66001361199999));
#307519=CARTESIAN_POINT('Ctrl Pts',(-3.56545693200006,12.2,2.66040823499999));
#307520=CARTESIAN_POINT('Ctrl Pts',(-3.56545693200006,5.2,2.66040823499999));
#307521=CARTESIAN_POINT('Ctrl Pts',(-3.56545693200006,2.2,2.66040823499999));
#307522=CARTESIAN_POINT('Ctrl Pts',(-3.56756530200006,12.2,2.66080127299999));
#307523=CARTESIAN_POINT('Ctrl Pts',(-3.56756530200006,5.2,2.66080127299999));
#307524=CARTESIAN_POINT('Ctrl Pts',(-3.56756530200006,2.2,2.66080127299999));
#307525=CARTESIAN_POINT('Ctrl Pts',(-3.56967794000006,12.2,2.66119271799998));
#307526=CARTESIAN_POINT('Ctrl Pts',(-3.56967794000006,5.2,2.66119271799998));
#307527=CARTESIAN_POINT('Ctrl Pts',(-3.56967794000006,2.2,2.66119271799998));
#307528=CARTESIAN_POINT('Ctrl Pts',(-3.57179484000006,12.2,2.66158256099998));
#307529=CARTESIAN_POINT('Ctrl Pts',(-3.57179484000006,5.2,2.66158256099998));
#307530=CARTESIAN_POINT('Ctrl Pts',(-3.57179484000006,2.2,2.66158256099998));
#307531=CARTESIAN_POINT('Ctrl Pts',(-3.57391599700006,12.2,2.66197079399999));
#307532=CARTESIAN_POINT('Ctrl Pts',(-3.57391599700006,5.2,2.66197079399999));
#307533=CARTESIAN_POINT('Ctrl Pts',(-3.57391599700006,2.2,2.66197079399999));
#307534=CARTESIAN_POINT('Ctrl Pts',(-3.57604140400006,12.2,2.66235740799999));
#307535=CARTESIAN_POINT('Ctrl Pts',(-3.57604140400006,5.2,2.66235740799999));
#307536=CARTESIAN_POINT('Ctrl Pts',(-3.57604140400006,2.2,2.66235740799999));
#307537=CARTESIAN_POINT('Ctrl Pts',(-3.57817105900006,12.2,2.66274239199999));
#307538=CARTESIAN_POINT('Ctrl Pts',(-3.57817105900006,5.2,2.66274239199999));
#307539=CARTESIAN_POINT('Ctrl Pts',(-3.57817105900006,2.2,2.66274239199999));
#307540=CARTESIAN_POINT('Ctrl Pts',(-3.58030495300006,12.2,2.66312574099998));
#307541=CARTESIAN_POINT('Ctrl Pts',(-3.58030495300006,5.2,2.66312574099998));
#307542=CARTESIAN_POINT('Ctrl Pts',(-3.58030495300006,2.2,2.66312574099998));
#307543=CARTESIAN_POINT('Ctrl Pts',(-3.58244308300006,12.2,2.66350744499999));
#307544=CARTESIAN_POINT('Ctrl Pts',(-3.58244308300006,5.2,2.66350744499999));
#307545=CARTESIAN_POINT('Ctrl Pts',(-3.58244308300006,2.2,2.66350744499999));
#307546=CARTESIAN_POINT('Ctrl Pts',(-3.58458544200006,12.2,2.66388749499999));
#307547=CARTESIAN_POINT('Ctrl Pts',(-3.58458544200006,5.2,2.66388749499999));
#307548=CARTESIAN_POINT('Ctrl Pts',(-3.58458544200006,2.2,2.66388749499999));
#307549=CARTESIAN_POINT('Ctrl Pts',(-3.58673202600006,12.2,2.66426588299999));
#307550=CARTESIAN_POINT('Ctrl Pts',(-3.58673202600006,5.2,2.66426588299999));
#307551=CARTESIAN_POINT('Ctrl Pts',(-3.58673202600006,2.2,2.66426588299999));
#307552=CARTESIAN_POINT('Ctrl Pts',(-3.58888282800006,12.2,2.66464259999999));
#307553=CARTESIAN_POINT('Ctrl Pts',(-3.58888282800006,5.2,2.66464259999999));
#307554=CARTESIAN_POINT('Ctrl Pts',(-3.58888282800006,2.2,2.66464259999999));
#307555=CARTESIAN_POINT('Ctrl Pts',(-3.59103784200006,12.2,2.66501763699999));
#307556=CARTESIAN_POINT('Ctrl Pts',(-3.59103784200006,5.2,2.66501763699999));
#307557=CARTESIAN_POINT('Ctrl Pts',(-3.59103784200006,2.2,2.66501763699999));
#307558=CARTESIAN_POINT('Ctrl Pts',(-3.59319706600005,12.2,2.66539098699998));
#307559=CARTESIAN_POINT('Ctrl Pts',(-3.59319706600005,5.2,2.66539098699998));
#307560=CARTESIAN_POINT('Ctrl Pts',(-3.59319706600005,2.2,2.66539098699998));
#307561=CARTESIAN_POINT('Ctrl Pts',(-3.59536049100006,12.2,2.66576263999998));
#307562=CARTESIAN_POINT('Ctrl Pts',(-3.59536049100006,5.2,2.66576263999998));
#307563=CARTESIAN_POINT('Ctrl Pts',(-3.59536049100006,2.2,2.66576263999998));
#307564=CARTESIAN_POINT('Ctrl Pts',(-3.59752811200006,12.2,2.66613258799998));
#307565=CARTESIAN_POINT('Ctrl Pts',(-3.59752811200006,5.2,2.66613258799998));
#307566=CARTESIAN_POINT('Ctrl Pts',(-3.59752811200006,2.2,2.66613258799998));
#307567=CARTESIAN_POINT('Ctrl Pts',(-3.59969992500006,12.2,2.66650082299999));
#307568=CARTESIAN_POINT('Ctrl Pts',(-3.59969992500006,5.2,2.66650082299999));
#307569=CARTESIAN_POINT('Ctrl Pts',(-3.59969992500006,2.2,2.66650082299999));
#307570=CARTESIAN_POINT('Ctrl Pts',(-3.60187592400006,12.2,2.66686733599999));
#307571=CARTESIAN_POINT('Ctrl Pts',(-3.60187592400006,5.2,2.66686733599999));
#307572=CARTESIAN_POINT('Ctrl Pts',(-3.60187592400006,2.2,2.66686733599999));
#307573=CARTESIAN_POINT('Ctrl Pts',(-3.60405610400006,12.2,2.66723211899999));
#307574=CARTESIAN_POINT('Ctrl Pts',(-3.60405610400006,5.2,2.66723211899999));
#307575=CARTESIAN_POINT('Ctrl Pts',(-3.60405610400006,2.2,2.66723211899999));
#307576=CARTESIAN_POINT('Ctrl Pts',(-3.60624045800006,12.2,2.66759516299999));
#307577=CARTESIAN_POINT('Ctrl Pts',(-3.60624045800006,5.2,2.66759516299999));
#307578=CARTESIAN_POINT('Ctrl Pts',(-3.60624045800006,2.2,2.66759516299999));
#307579=CARTESIAN_POINT('Ctrl Pts',(-3.60842898100006,12.2,2.66795645999998));
#307580=CARTESIAN_POINT('Ctrl Pts',(-3.60842898100006,5.2,2.66795645999998));
#307581=CARTESIAN_POINT('Ctrl Pts',(-3.60842898100006,2.2,2.66795645999998));
#307582=CARTESIAN_POINT('Ctrl Pts',(-3.61062166800005,12.2,2.66831600199998));
#307583=CARTESIAN_POINT('Ctrl Pts',(-3.61062166800005,5.2,2.66831600199998));
#307584=CARTESIAN_POINT('Ctrl Pts',(-3.61062166800005,2.2,2.66831600199998));
#307585=CARTESIAN_POINT('Ctrl Pts',(-3.61281851300006,12.2,2.66867377999999));
#307586=CARTESIAN_POINT('Ctrl Pts',(-3.61281851300006,5.2,2.66867377999999));
#307587=CARTESIAN_POINT('Ctrl Pts',(-3.61281851300006,2.2,2.66867377999999));
#307588=CARTESIAN_POINT('Ctrl Pts',(-3.61501951100006,12.2,2.66902978699999));
#307589=CARTESIAN_POINT('Ctrl Pts',(-3.61501951100006,5.2,2.66902978699999));
#307590=CARTESIAN_POINT('Ctrl Pts',(-3.61501951100006,2.2,2.66902978699999));
#307591=CARTESIAN_POINT('Ctrl Pts',(-3.61722465600006,12.2,2.66938401199998));
#307592=CARTESIAN_POINT('Ctrl Pts',(-3.61722465600006,5.2,2.66938401199998));
#307593=CARTESIAN_POINT('Ctrl Pts',(-3.61722465600006,2.2,2.66938401199998));
#307594=CARTESIAN_POINT('Ctrl Pts',(-3.61943394400006,12.2,2.66973644999998));
#307595=CARTESIAN_POINT('Ctrl Pts',(-3.61943394400006,5.2,2.66973644999998));
#307596=CARTESIAN_POINT('Ctrl Pts',(-3.61943394400006,2.2,2.66973644999998));
#307597=CARTESIAN_POINT('Ctrl Pts',(-3.62164736600006,12.2,2.67008708999998));
#307598=CARTESIAN_POINT('Ctrl Pts',(-3.62164736600006,5.2,2.67008708999998));
#307599=CARTESIAN_POINT('Ctrl Pts',(-3.62164736600006,2.2,2.67008708999998));
#307600=CARTESIAN_POINT('Ctrl Pts',(-3.62386492100006,12.2,2.67043592499999));
#307601=CARTESIAN_POINT('Ctrl Pts',(-3.62386492100006,5.2,2.67043592499999));
#307602=CARTESIAN_POINT('Ctrl Pts',(-3.62386492100006,2.2,2.67043592499999));
#307603=CARTESIAN_POINT('Ctrl Pts',(-3.62608660000006,12.2,2.67078294699999));
#307604=CARTESIAN_POINT('Ctrl Pts',(-3.62608660000006,5.2,2.67078294699999));
#307605=CARTESIAN_POINT('Ctrl Pts',(-3.62608660000006,2.2,2.67078294699999));
#307606=CARTESIAN_POINT('Ctrl Pts',(-3.62831239800006,12.2,2.67112814699999));
#307607=CARTESIAN_POINT('Ctrl Pts',(-3.62831239800006,5.2,2.67112814699999));
#307608=CARTESIAN_POINT('Ctrl Pts',(-3.62831239800006,2.2,2.67112814699999));
#307609=CARTESIAN_POINT('Ctrl Pts',(-3.63054231100006,12.2,2.67147151799998));
#307610=CARTESIAN_POINT('Ctrl Pts',(-3.63054231100006,5.2,2.67147151799998));
#307611=CARTESIAN_POINT('Ctrl Pts',(-3.63054231100006,2.2,2.67147151799998));
#307612=CARTESIAN_POINT('Ctrl Pts',(-3.63277633200005,12.2,2.67181304999998));
#307613=CARTESIAN_POINT('Ctrl Pts',(-3.63277633200005,5.2,2.67181304999998));
#307614=CARTESIAN_POINT('Ctrl Pts',(-3.63277633200005,2.2,2.67181304999998));
#307615=CARTESIAN_POINT('Ctrl Pts',(-3.63501445700006,12.2,2.67215273699998));
#307616=CARTESIAN_POINT('Ctrl Pts',(-3.63501445700006,5.2,2.67215273699998));
#307617=CARTESIAN_POINT('Ctrl Pts',(-3.63501445700006,2.2,2.67215273699998));
#307618=CARTESIAN_POINT('Ctrl Pts',(-3.63725667900006,12.2,2.67249056999999));
#307619=CARTESIAN_POINT('Ctrl Pts',(-3.63725667900006,5.2,2.67249056999999));
#307620=CARTESIAN_POINT('Ctrl Pts',(-3.63725667900006,2.2,2.67249056999999));
#307621=CARTESIAN_POINT('Ctrl Pts',(-3.63950299200006,12.2,2.67282653999998));
#307622=CARTESIAN_POINT('Ctrl Pts',(-3.63950299200006,5.2,2.67282653999998));
#307623=CARTESIAN_POINT('Ctrl Pts',(-3.63950299200006,2.2,2.67282653999998));
#307624=CARTESIAN_POINT('Ctrl Pts',(-3.64175339200006,12.2,2.67316064099998));
#307625=CARTESIAN_POINT('Ctrl Pts',(-3.64175339200006,5.2,2.67316064099998));
#307626=CARTESIAN_POINT('Ctrl Pts',(-3.64175339200006,2.2,2.67316064099998));
#307627=CARTESIAN_POINT('Ctrl Pts',(-3.64400787400006,12.2,2.67349286199998));
#307628=CARTESIAN_POINT('Ctrl Pts',(-3.64400787400006,5.2,2.67349286199998));
#307629=CARTESIAN_POINT('Ctrl Pts',(-3.64400787400006,2.2,2.67349286199998));
#307630=CARTESIAN_POINT('Ctrl Pts',(-3.64626642900006,12.2,2.67382319699998));
#307631=CARTESIAN_POINT('Ctrl Pts',(-3.64626642900006,5.2,2.67382319699998));
#307632=CARTESIAN_POINT('Ctrl Pts',(-3.64626642900006,2.2,2.67382319699998));
#307633=CARTESIAN_POINT('Ctrl Pts',(-3.64852905500006,12.2,2.67415163699999));
#307634=CARTESIAN_POINT('Ctrl Pts',(-3.64852905500006,5.2,2.67415163699999));
#307635=CARTESIAN_POINT('Ctrl Pts',(-3.64852905500006,2.2,2.67415163699999));
#307636=CARTESIAN_POINT('Ctrl Pts',(-3.65079574500006,12.2,2.67447817499999));
#307637=CARTESIAN_POINT('Ctrl Pts',(-3.65079574500006,5.2,2.67447817499999));
#307638=CARTESIAN_POINT('Ctrl Pts',(-3.65079574500006,2.2,2.67447817499999));
#307639=CARTESIAN_POINT('Ctrl Pts',(-3.65306649300006,12.2,2.67480280299999));
#307640=CARTESIAN_POINT('Ctrl Pts',(-3.65306649300006,5.2,2.67480280299999));
#307641=CARTESIAN_POINT('Ctrl Pts',(-3.65306649300006,2.2,2.67480280299999));
#307642=CARTESIAN_POINT('Ctrl Pts',(-3.65534129500006,12.2,2.67512551199999));
#307643=CARTESIAN_POINT('Ctrl Pts',(-3.65534129500006,5.2,2.67512551199999));
#307644=CARTESIAN_POINT('Ctrl Pts',(-3.65534129500006,2.2,2.67512551199999));
#307645=CARTESIAN_POINT('Ctrl Pts',(-3.65762014400006,12.2,2.67544629399998));
#307646=CARTESIAN_POINT('Ctrl Pts',(-3.65762014400006,5.2,2.67544629399998));
#307647=CARTESIAN_POINT('Ctrl Pts',(-3.65762014400006,2.2,2.67544629399998));
#307648=CARTESIAN_POINT('Ctrl Pts',(-3.65990303400006,12.2,2.67576514099999));
#307649=CARTESIAN_POINT('Ctrl Pts',(-3.65990303400006,5.2,2.67576514099999));
#307650=CARTESIAN_POINT('Ctrl Pts',(-3.65990303400006,2.2,2.67576514099999));
#307651=CARTESIAN_POINT('Ctrl Pts',(-3.66218996100006,12.2,2.67608204699999));
#307652=CARTESIAN_POINT('Ctrl Pts',(-3.66218996100006,5.2,2.67608204699999));
#307653=CARTESIAN_POINT('Ctrl Pts',(-3.66218996100006,2.2,2.67608204699999));
#307654=CARTESIAN_POINT('Ctrl Pts',(-3.66448091900006,12.2,2.67639700199998));
#307655=CARTESIAN_POINT('Ctrl Pts',(-3.66448091900006,5.2,2.67639700199998));
#307656=CARTESIAN_POINT('Ctrl Pts',(-3.66448091900006,2.2,2.67639700199998));
#307657=CARTESIAN_POINT('Ctrl Pts',(-3.66677590100006,12.2,2.67670999999999));
#307658=CARTESIAN_POINT('Ctrl Pts',(-3.66677590100006,5.2,2.67670999999999));
#307659=CARTESIAN_POINT('Ctrl Pts',(-3.66677590100006,2.2,2.67670999999999));
#307660=CARTESIAN_POINT('Ctrl Pts',(-3.66907490300005,12.2,2.67702103099998));
#307661=CARTESIAN_POINT('Ctrl Pts',(-3.66907490300005,5.2,2.67702103099998));
#307662=CARTESIAN_POINT('Ctrl Pts',(-3.66907490300005,2.2,2.67702103099998));
#307663=CARTESIAN_POINT('Ctrl Pts',(-3.67137791900006,12.2,2.67733008799999));
#307664=CARTESIAN_POINT('Ctrl Pts',(-3.67137791900006,5.2,2.67733008799999));
#307665=CARTESIAN_POINT('Ctrl Pts',(-3.67137791900006,2.2,2.67733008799999));
#307666=CARTESIAN_POINT('Ctrl Pts',(-3.67368494300006,12.2,2.67763716499999));
#307667=CARTESIAN_POINT('Ctrl Pts',(-3.67368494300006,5.2,2.67763716499999));
#307668=CARTESIAN_POINT('Ctrl Pts',(-3.67368494300006,2.2,2.67763716499999));
#307669=CARTESIAN_POINT('Ctrl Pts',(-3.67599597000006,12.2,2.67794225099999));
#307670=CARTESIAN_POINT('Ctrl Pts',(-3.67599597000006,5.2,2.67794225099999));
#307671=CARTESIAN_POINT('Ctrl Pts',(-3.67599597000006,2.2,2.67794225099999));
#307672=CARTESIAN_POINT('Ctrl Pts',(-3.67831099400005,12.2,2.67824533899999));
#307673=CARTESIAN_POINT('Ctrl Pts',(-3.67831099400005,5.2,2.67824533899999));
#307674=CARTESIAN_POINT('Ctrl Pts',(-3.67831099400005,2.2,2.67824533899999));
#307675=CARTESIAN_POINT('Ctrl Pts',(-3.68063001000006,12.2,2.67854642399998));
#307676=CARTESIAN_POINT('Ctrl Pts',(-3.68063001000006,5.2,2.67854642399998));
#307677=CARTESIAN_POINT('Ctrl Pts',(-3.68063001000006,2.2,2.67854642399998));
#307678=CARTESIAN_POINT('Ctrl Pts',(-3.68295301100006,12.2,2.67884549499998));
#307679=CARTESIAN_POINT('Ctrl Pts',(-3.68295301100006,5.2,2.67884549499998));
#307680=CARTESIAN_POINT('Ctrl Pts',(-3.68295301100006,2.2,2.67884549499998));
#307681=CARTESIAN_POINT('Ctrl Pts',(-3.68527999200006,12.2,2.67914254499999));
#307682=CARTESIAN_POINT('Ctrl Pts',(-3.68527999200006,5.2,2.67914254499999));
#307683=CARTESIAN_POINT('Ctrl Pts',(-3.68527999200006,2.2,2.67914254499999));
#307684=CARTESIAN_POINT('Ctrl Pts',(-3.68761094800006,12.2,2.67943756799998));
#307685=CARTESIAN_POINT('Ctrl Pts',(-3.68761094800006,5.2,2.67943756799998));
#307686=CARTESIAN_POINT('Ctrl Pts',(-3.68761094800006,2.2,2.67943756799998));
#307687=CARTESIAN_POINT('Ctrl Pts',(-3.68994587300006,12.2,2.67973055399998));
#307688=CARTESIAN_POINT('Ctrl Pts',(-3.68994587300006,5.2,2.67973055399998));
#307689=CARTESIAN_POINT('Ctrl Pts',(-3.68994587300006,2.2,2.67973055399998));
#307690=CARTESIAN_POINT('Ctrl Pts',(-3.69228476200006,12.2,2.68002149699999));
#307691=CARTESIAN_POINT('Ctrl Pts',(-3.69228476200006,5.2,2.68002149699999));
#307692=CARTESIAN_POINT('Ctrl Pts',(-3.69228476200006,2.2,2.68002149699999));
#307693=CARTESIAN_POINT('Ctrl Pts',(-3.69462760800006,12.2,2.68031038799998));
#307694=CARTESIAN_POINT('Ctrl Pts',(-3.69462760800006,5.2,2.68031038799998));
#307695=CARTESIAN_POINT('Ctrl Pts',(-3.69462760800006,2.2,2.68031038799998));
#307696=CARTESIAN_POINT('Ctrl Pts',(-3.69697440600006,12.2,2.68059721999999));
#307697=CARTESIAN_POINT('Ctrl Pts',(-3.69697440600006,5.2,2.68059721999999));
#307698=CARTESIAN_POINT('Ctrl Pts',(-3.69697440600006,2.2,2.68059721999999));
#307699=CARTESIAN_POINT('Ctrl Pts',(-3.69932515100006,12.2,2.68088198699999));
#307700=CARTESIAN_POINT('Ctrl Pts',(-3.69932515100006,5.2,2.68088198699999));
#307701=CARTESIAN_POINT('Ctrl Pts',(-3.69932515100006,2.2,2.68088198699999));
#307702=CARTESIAN_POINT('Ctrl Pts',(-3.70167983700005,12.2,2.68116467799998));
#307703=CARTESIAN_POINT('Ctrl Pts',(-3.70167983700005,5.2,2.68116467799998));
#307704=CARTESIAN_POINT('Ctrl Pts',(-3.70167983700005,2.2,2.68116467799998));
#307705=CARTESIAN_POINT('Ctrl Pts',(-3.70403845800006,12.2,2.68144528699998));
#307706=CARTESIAN_POINT('Ctrl Pts',(-3.70403845800006,5.2,2.68144528699998));
#307707=CARTESIAN_POINT('Ctrl Pts',(-3.70403845800006,2.2,2.68144528699998));
#307708=CARTESIAN_POINT('Ctrl Pts',(-3.70640100800006,12.2,2.68172380799999));
#307709=CARTESIAN_POINT('Ctrl Pts',(-3.70640100800006,5.2,2.68172380799999));
#307710=CARTESIAN_POINT('Ctrl Pts',(-3.70640100800006,2.2,2.68172380799999));
#307711=CARTESIAN_POINT('Ctrl Pts',(-3.70876748400006,12.2,2.68200023099999));
#307712=CARTESIAN_POINT('Ctrl Pts',(-3.70876748400006,5.2,2.68200023099999));
#307713=CARTESIAN_POINT('Ctrl Pts',(-3.70876748400006,2.2,2.68200023099999));
#307714=CARTESIAN_POINT('Ctrl Pts',(-3.71113787600006,12.2,2.68227454999998));
#307715=CARTESIAN_POINT('Ctrl Pts',(-3.71113787600006,5.2,2.68227454999998));
#307716=CARTESIAN_POINT('Ctrl Pts',(-3.71113787600006,2.2,2.68227454999998));
#307717=CARTESIAN_POINT('Ctrl Pts',(-3.71351218200005,12.2,2.68254675699998));
#307718=CARTESIAN_POINT('Ctrl Pts',(-3.71351218200005,5.2,2.68254675699998));
#307719=CARTESIAN_POINT('Ctrl Pts',(-3.71351218200005,2.2,2.68254675699998));
#307720=CARTESIAN_POINT('Ctrl Pts',(-3.71589039400006,12.2,2.68281684399999));
#307721=CARTESIAN_POINT('Ctrl Pts',(-3.71589039400006,5.2,2.68281684399999));
#307722=CARTESIAN_POINT('Ctrl Pts',(-3.71589039400006,2.2,2.68281684399999));
#307723=CARTESIAN_POINT('Ctrl Pts',(-3.71827250800006,12.2,2.68308480499999));
#307724=CARTESIAN_POINT('Ctrl Pts',(-3.71827250800006,5.2,2.68308480499999));
#307725=CARTESIAN_POINT('Ctrl Pts',(-3.71827250800006,2.2,2.68308480499999));
#307726=CARTESIAN_POINT('Ctrl Pts',(-3.72065851800006,12.2,2.68335063099999));
#307727=CARTESIAN_POINT('Ctrl Pts',(-3.72065851800006,5.2,2.68335063099999));
#307728=CARTESIAN_POINT('Ctrl Pts',(-3.72065851800006,2.2,2.68335063099999));
#307729=CARTESIAN_POINT('Ctrl Pts',(-3.72304841700006,12.2,2.68361431399998));
#307730=CARTESIAN_POINT('Ctrl Pts',(-3.72304841700006,5.2,2.68361431399998));
#307731=CARTESIAN_POINT('Ctrl Pts',(-3.72304841700006,2.2,2.68361431399998));
#307732=CARTESIAN_POINT('Ctrl Pts',(-3.72544220100006,12.2,2.68387584899998));
#307733=CARTESIAN_POINT('Ctrl Pts',(-3.72544220100006,5.2,2.68387584899998));
#307734=CARTESIAN_POINT('Ctrl Pts',(-3.72544220100006,2.2,2.68387584899998));
#307735=CARTESIAN_POINT('Ctrl Pts',(-3.72783986300006,12.2,2.68413522699999));
#307736=CARTESIAN_POINT('Ctrl Pts',(-3.72783986300006,5.2,2.68413522699999));
#307737=CARTESIAN_POINT('Ctrl Pts',(-3.72783986300006,2.2,2.68413522699999));
#307738=CARTESIAN_POINT('Ctrl Pts',(-3.73024140000005,12.2,2.68439243999998));
#307739=CARTESIAN_POINT('Ctrl Pts',(-3.73024140000005,5.2,2.68439243999998));
#307740=CARTESIAN_POINT('Ctrl Pts',(-3.73024140000005,2.2,2.68439243999998));
#307741=CARTESIAN_POINT('Ctrl Pts',(-3.73264680300006,12.2,2.68464748299999));
#307742=CARTESIAN_POINT('Ctrl Pts',(-3.73264680300006,5.2,2.68464748299999));
#307743=CARTESIAN_POINT('Ctrl Pts',(-3.73264680300006,2.2,2.68464748299999));
#307744=CARTESIAN_POINT('Ctrl Pts',(-3.73505606800006,12.2,2.68490034499998));
#307745=CARTESIAN_POINT('Ctrl Pts',(-3.73505606800006,5.2,2.68490034499998));
#307746=CARTESIAN_POINT('Ctrl Pts',(-3.73505606800006,2.2,2.68490034499998));
#307747=CARTESIAN_POINT('Ctrl Pts',(-3.73746918800006,12.2,2.68515102199999));
#307748=CARTESIAN_POINT('Ctrl Pts',(-3.73746918800006,5.2,2.68515102199999));
#307749=CARTESIAN_POINT('Ctrl Pts',(-3.73746918800006,2.2,2.68515102199999));
#307750=CARTESIAN_POINT('Ctrl Pts',(-3.73988616000006,12.2,2.68539950499999));
#307751=CARTESIAN_POINT('Ctrl Pts',(-3.73988616000006,5.2,2.68539950499999));
#307752=CARTESIAN_POINT('Ctrl Pts',(-3.73988616000006,2.2,2.68539950499999));
#307753=CARTESIAN_POINT('Ctrl Pts',(-3.74230697500006,12.2,2.68564578699999));
#307754=CARTESIAN_POINT('Ctrl Pts',(-3.74230697500006,5.2,2.68564578699999));
#307755=CARTESIAN_POINT('Ctrl Pts',(-3.74230697500006,2.2,2.68564578699999));
#307756=CARTESIAN_POINT('Ctrl Pts',(-3.74473163000006,12.2,2.68588986199998));
#307757=CARTESIAN_POINT('Ctrl Pts',(-3.74473163000006,5.2,2.68588986199998));
#307758=CARTESIAN_POINT('Ctrl Pts',(-3.74473163000006,2.2,2.68588986199998));
#307759=CARTESIAN_POINT('Ctrl Pts',(-3.74716011800006,12.2,2.68613171999998));
#307760=CARTESIAN_POINT('Ctrl Pts',(-3.74716011800006,5.2,2.68613171999998));
#307761=CARTESIAN_POINT('Ctrl Pts',(-3.74716011800006,2.2,2.68613171999998));
#307762=CARTESIAN_POINT('Ctrl Pts',(-3.74959243400006,12.2,2.68637135599998));
#307763=CARTESIAN_POINT('Ctrl Pts',(-3.74959243400006,5.2,2.68637135599998));
#307764=CARTESIAN_POINT('Ctrl Pts',(-3.74959243400006,2.2,2.68637135599998));
#307765=CARTESIAN_POINT('Ctrl Pts',(-3.75202857100006,12.2,2.68660876099998));
#307766=CARTESIAN_POINT('Ctrl Pts',(-3.75202857100006,5.2,2.68660876099998));
#307767=CARTESIAN_POINT('Ctrl Pts',(-3.75202857100006,2.2,2.68660876099998));
#307768=CARTESIAN_POINT('Ctrl Pts',(-3.75446852500006,12.2,2.68684392999998));
#307769=CARTESIAN_POINT('Ctrl Pts',(-3.75446852500006,5.2,2.68684392999998));
#307770=CARTESIAN_POINT('Ctrl Pts',(-3.75446852500006,2.2,2.68684392999998));
#307771=CARTESIAN_POINT('Ctrl Pts',(-3.75691229000005,12.2,2.68707685299999));
#307772=CARTESIAN_POINT('Ctrl Pts',(-3.75691229000005,5.2,2.68707685299999));
#307773=CARTESIAN_POINT('Ctrl Pts',(-3.75691229000005,2.2,2.68707685299999));
#307774=CARTESIAN_POINT('Ctrl Pts',(-3.75935985900006,12.2,2.68730752599998));
#307775=CARTESIAN_POINT('Ctrl Pts',(-3.75935985900006,5.2,2.68730752599998));
#307776=CARTESIAN_POINT('Ctrl Pts',(-3.75935985900006,2.2,2.68730752599998));
#307777=CARTESIAN_POINT('Ctrl Pts',(-3.76181122700006,12.2,2.68753593899999));
#307778=CARTESIAN_POINT('Ctrl Pts',(-3.76181122700006,5.2,2.68753593899999));
#307779=CARTESIAN_POINT('Ctrl Pts',(-3.76181122700006,2.2,2.68753593899999));
#307780=CARTESIAN_POINT('Ctrl Pts',(-3.76426638900006,12.2,2.68776208699999));
#307781=CARTESIAN_POINT('Ctrl Pts',(-3.76426638900006,5.2,2.68776208699999));
#307782=CARTESIAN_POINT('Ctrl Pts',(-3.76426638900006,2.2,2.68776208699999));
#307783=CARTESIAN_POINT('Ctrl Pts',(-3.76672533800006,12.2,2.68798596099998));
#307784=CARTESIAN_POINT('Ctrl Pts',(-3.76672533800006,5.2,2.68798596099998));
#307785=CARTESIAN_POINT('Ctrl Pts',(-3.76672533800006,2.2,2.68798596099998));
#307786=CARTESIAN_POINT('Ctrl Pts',(-3.76918807000005,12.2,2.68820755499998));
#307787=CARTESIAN_POINT('Ctrl Pts',(-3.76918807000005,5.2,2.68820755499998));
#307788=CARTESIAN_POINT('Ctrl Pts',(-3.76918807000005,2.2,2.68820755499998));
#307789=CARTESIAN_POINT('Ctrl Pts',(-3.77165457700006,12.2,2.68842686199999));
#307790=CARTESIAN_POINT('Ctrl Pts',(-3.77165457700006,5.2,2.68842686199999));
#307791=CARTESIAN_POINT('Ctrl Pts',(-3.77165457700006,2.2,2.68842686199999));
#307792=CARTESIAN_POINT('Ctrl Pts',(-3.77412485600006,12.2,2.68864387299999));
#307793=CARTESIAN_POINT('Ctrl Pts',(-3.77412485600006,5.2,2.68864387299999));
#307794=CARTESIAN_POINT('Ctrl Pts',(-3.77412485600006,2.2,2.68864387299999));
#307795=CARTESIAN_POINT('Ctrl Pts',(-3.77659889800006,12.2,2.68885858399998));
#307796=CARTESIAN_POINT('Ctrl Pts',(-3.77659889800006,5.2,2.68885858399998));
#307797=CARTESIAN_POINT('Ctrl Pts',(-3.77659889800006,2.2,2.68885858399998));
#307798=CARTESIAN_POINT('Ctrl Pts',(-3.77907670100006,12.2,2.68907098599998));
#307799=CARTESIAN_POINT('Ctrl Pts',(-3.77907670100006,5.2,2.68907098599998));
#307800=CARTESIAN_POINT('Ctrl Pts',(-3.77907670100006,2.2,2.68907098599998));
#307801=CARTESIAN_POINT('Ctrl Pts',(-3.78155825700006,12.2,2.68928107199999));
#307802=CARTESIAN_POINT('Ctrl Pts',(-3.78155825700006,5.2,2.68928107199999));
#307803=CARTESIAN_POINT('Ctrl Pts',(-3.78155825700006,2.2,2.68928107199999));
#307804=CARTESIAN_POINT('Ctrl Pts',(-3.78404356000006,12.2,2.68948883599998));
#307805=CARTESIAN_POINT('Ctrl Pts',(-3.78404356000006,5.2,2.68948883599998));
#307806=CARTESIAN_POINT('Ctrl Pts',(-3.78404356000006,2.2,2.68948883599998));
#307807=CARTESIAN_POINT('Ctrl Pts',(-3.78653260400006,12.2,2.68969426999998));
#307808=CARTESIAN_POINT('Ctrl Pts',(-3.78653260400006,5.2,2.68969426999998));
#307809=CARTESIAN_POINT('Ctrl Pts',(-3.78653260400006,2.2,2.68969426999998));
#307810=CARTESIAN_POINT('Ctrl Pts',(-3.78902538700006,12.2,2.68989736599998));
#307811=CARTESIAN_POINT('Ctrl Pts',(-3.78902538700006,5.2,2.68989736599998));
#307812=CARTESIAN_POINT('Ctrl Pts',(-3.78902538700006,2.2,2.68989736599998));
#307813=CARTESIAN_POINT('Ctrl Pts',(-3.79152189800006,12.2,2.69009811999998));
#307814=CARTESIAN_POINT('Ctrl Pts',(-3.79152189800006,5.2,2.69009811999998));
#307815=CARTESIAN_POINT('Ctrl Pts',(-3.79152189800006,2.2,2.69009811999998));
#307816=CARTESIAN_POINT('Ctrl Pts',(-3.79402213500006,12.2,2.69029652299999));
#307817=CARTESIAN_POINT('Ctrl Pts',(-3.79402213500006,5.2,2.69029652299999));
#307818=CARTESIAN_POINT('Ctrl Pts',(-3.79402213500006,2.2,2.69029652299999));
#307819=CARTESIAN_POINT('Ctrl Pts',(-3.79652609100006,12.2,2.69049256799998));
#307820=CARTESIAN_POINT('Ctrl Pts',(-3.79652609100006,5.2,2.69049256799998));
#307821=CARTESIAN_POINT('Ctrl Pts',(-3.79652609100006,2.2,2.69049256799998));
#307822=CARTESIAN_POINT('Ctrl Pts',(-3.79903376000006,12.2,2.69068624799999));
#307823=CARTESIAN_POINT('Ctrl Pts',(-3.79903376000006,5.2,2.69068624799999));
#307824=CARTESIAN_POINT('Ctrl Pts',(-3.79903376000006,2.2,2.69068624799999));
#307825=CARTESIAN_POINT('Ctrl Pts',(-3.80154513600006,12.2,2.69087755799998));
#307826=CARTESIAN_POINT('Ctrl Pts',(-3.80154513600006,5.2,2.69087755799998));
#307827=CARTESIAN_POINT('Ctrl Pts',(-3.80154513600006,2.2,2.69087755799998));
#307828=CARTESIAN_POINT('Ctrl Pts',(-3.80406021400006,12.2,2.69106648899999));
#307829=CARTESIAN_POINT('Ctrl Pts',(-3.80406021400006,5.2,2.69106648899999));
#307830=CARTESIAN_POINT('Ctrl Pts',(-3.80406021400006,2.2,2.69106648899999));
#307831=CARTESIAN_POINT('Ctrl Pts',(-3.80657898900005,12.2,2.69125303399999));
#307832=CARTESIAN_POINT('Ctrl Pts',(-3.80657898900005,5.2,2.69125303399999));
#307833=CARTESIAN_POINT('Ctrl Pts',(-3.80657898900005,2.2,2.69125303399999));
#307834=CARTESIAN_POINT('Ctrl Pts',(-3.80910145400006,12.2,2.69143718799998));
#307835=CARTESIAN_POINT('Ctrl Pts',(-3.80910145400006,5.2,2.69143718799998));
#307836=CARTESIAN_POINT('Ctrl Pts',(-3.80910145400006,2.2,2.69143718799998));
#307837=CARTESIAN_POINT('Ctrl Pts',(-3.81162760300006,12.2,2.69161894299998));
#307838=CARTESIAN_POINT('Ctrl Pts',(-3.81162760300006,5.2,2.69161894299998));
#307839=CARTESIAN_POINT('Ctrl Pts',(-3.81162760300006,2.2,2.69161894299998));
#307840=CARTESIAN_POINT('Ctrl Pts',(-3.81415743000006,12.2,2.69179829199999));
#307841=CARTESIAN_POINT('Ctrl Pts',(-3.81415743000006,5.2,2.69179829199999));
#307842=CARTESIAN_POINT('Ctrl Pts',(-3.81415743000006,2.2,2.69179829199999));
#307843=CARTESIAN_POINT('Ctrl Pts',(-3.81669093200006,12.2,2.69197522899999));
#307844=CARTESIAN_POINT('Ctrl Pts',(-3.81669093200006,5.2,2.69197522899999));
#307845=CARTESIAN_POINT('Ctrl Pts',(-3.81669093200006,2.2,2.69197522899999));
#307846=CARTESIAN_POINT('Ctrl Pts',(-3.81922810000006,12.2,2.69214974599999));
#307847=CARTESIAN_POINT('Ctrl Pts',(-3.81922810000006,5.2,2.69214974599999));
#307848=CARTESIAN_POINT('Ctrl Pts',(-3.81922810000006,2.2,2.69214974599999));
#307849=CARTESIAN_POINT('Ctrl Pts',(-3.82176893000006,12.2,2.69232183699998));
#307850=CARTESIAN_POINT('Ctrl Pts',(-3.82176893000006,5.2,2.69232183699998));
#307851=CARTESIAN_POINT('Ctrl Pts',(-3.82176893000006,2.2,2.69232183699998));
#307852=CARTESIAN_POINT('Ctrl Pts',(-3.82431341600006,12.2,2.69249149599998));
#307853=CARTESIAN_POINT('Ctrl Pts',(-3.82431341600006,5.2,2.69249149599998));
#307854=CARTESIAN_POINT('Ctrl Pts',(-3.82431341600006,2.2,2.69249149599998));
#307855=CARTESIAN_POINT('Ctrl Pts',(-3.82686155200005,12.2,2.69265871399998));
#307856=CARTESIAN_POINT('Ctrl Pts',(-3.82686155200005,5.2,2.69265871399998));
#307857=CARTESIAN_POINT('Ctrl Pts',(-3.82686155200005,2.2,2.69265871399998));
#307858=CARTESIAN_POINT('Ctrl Pts',(-3.82941333200006,12.2,2.69282348599998));
#307859=CARTESIAN_POINT('Ctrl Pts',(-3.82941333200006,5.2,2.69282348599998));
#307860=CARTESIAN_POINT('Ctrl Pts',(-3.82941333200006,2.2,2.69282348599998));
#307861=CARTESIAN_POINT('Ctrl Pts',(-3.83196874900006,12.2,2.69298580499999));
#307862=CARTESIAN_POINT('Ctrl Pts',(-3.83196874900006,5.2,2.69298580499999));
#307863=CARTESIAN_POINT('Ctrl Pts',(-3.83196874900006,2.2,2.69298580499999));
#307864=CARTESIAN_POINT('Ctrl Pts',(-3.83452780100006,12.2,2.69314566399999));
#307865=CARTESIAN_POINT('Ctrl Pts',(-3.83452780100006,5.2,2.69314566399999));
#307866=CARTESIAN_POINT('Ctrl Pts',(-3.83452780100006,2.2,2.69314566399999));
#307867=CARTESIAN_POINT('Ctrl Pts',(-3.83709047900005,12.2,2.69330305699999));
#307868=CARTESIAN_POINT('Ctrl Pts',(-3.83709047900005,5.2,2.69330305699999));
#307869=CARTESIAN_POINT('Ctrl Pts',(-3.83709047900005,2.2,2.69330305699999));
#307870=CARTESIAN_POINT('Ctrl Pts',(-3.83965677700006,12.2,2.69345797599998));
#307871=CARTESIAN_POINT('Ctrl Pts',(-3.83965677700006,5.2,2.69345797599998));
#307872=CARTESIAN_POINT('Ctrl Pts',(-3.83965677700006,2.2,2.69345797599998));
#307873=CARTESIAN_POINT('Ctrl Pts',(-3.84222669200006,12.2,2.69361041599999));
#307874=CARTESIAN_POINT('Ctrl Pts',(-3.84222669200006,5.2,2.69361041599999));
#307875=CARTESIAN_POINT('Ctrl Pts',(-3.84222669200006,2.2,2.69361041599999));
#307876=CARTESIAN_POINT('Ctrl Pts',(-3.84480021600006,12.2,2.69376036799999));
#307877=CARTESIAN_POINT('Ctrl Pts',(-3.84480021600006,5.2,2.69376036799999));
#307878=CARTESIAN_POINT('Ctrl Pts',(-3.84480021600006,2.2,2.69376036799999));
#307879=CARTESIAN_POINT('Ctrl Pts',(-3.84737734300006,12.2,2.69390782799999));
#307880=CARTESIAN_POINT('Ctrl Pts',(-3.84737734300006,5.2,2.69390782799999));
#307881=CARTESIAN_POINT('Ctrl Pts',(-3.84737734300006,2.2,2.69390782799999));
#307882=CARTESIAN_POINT('Ctrl Pts',(-3.84995807000006,12.2,2.69405278999999));
#307883=CARTESIAN_POINT('Ctrl Pts',(-3.84995807000006,5.2,2.69405278999999));
#307884=CARTESIAN_POINT('Ctrl Pts',(-3.84995807000006,2.2,2.69405278999999));
#307885=CARTESIAN_POINT('Ctrl Pts',(-3.85254238800006,12.2,2.69419524399999));
#307886=CARTESIAN_POINT('Ctrl Pts',(-3.85254238800006,5.2,2.69419524399999));
#307887=CARTESIAN_POINT('Ctrl Pts',(-3.85254238800006,2.2,2.69419524399999));
#307888=CARTESIAN_POINT('Ctrl Pts',(-3.85513029300006,12.2,2.69433518699999));
#307889=CARTESIAN_POINT('Ctrl Pts',(-3.85513029300006,5.2,2.69433518699999));
#307890=CARTESIAN_POINT('Ctrl Pts',(-3.85513029300006,2.2,2.69433518699999));
#307891=CARTESIAN_POINT('Ctrl Pts',(-3.85772177900006,12.2,2.69447260899998));
#307892=CARTESIAN_POINT('Ctrl Pts',(-3.85772177900006,5.2,2.69447260899998));
#307893=CARTESIAN_POINT('Ctrl Pts',(-3.85772177900006,2.2,2.69447260899998));
#307894=CARTESIAN_POINT('Ctrl Pts',(-3.86031684000006,12.2,2.69460750499999));
#307895=CARTESIAN_POINT('Ctrl Pts',(-3.86031684000006,5.2,2.69460750499999));
#307896=CARTESIAN_POINT('Ctrl Pts',(-3.86031684000006,2.2,2.69460750499999));
#307897=CARTESIAN_POINT('Ctrl Pts',(-3.86291546800006,12.2,2.69473986899998));
#307898=CARTESIAN_POINT('Ctrl Pts',(-3.86291546800006,5.2,2.69473986899998));
#307899=CARTESIAN_POINT('Ctrl Pts',(-3.86291546800006,2.2,2.69473986899998));
#307900=CARTESIAN_POINT('Ctrl Pts',(-3.86551766000006,12.2,2.69486969199999));
#307901=CARTESIAN_POINT('Ctrl Pts',(-3.86551766000006,5.2,2.69486969199999));
#307902=CARTESIAN_POINT('Ctrl Pts',(-3.86551766000006,2.2,2.69486969199999));
#307903=CARTESIAN_POINT('Ctrl Pts',(-3.86812340800006,12.2,2.69499696899998));
#307904=CARTESIAN_POINT('Ctrl Pts',(-3.86812340800006,5.2,2.69499696899998));
#307905=CARTESIAN_POINT('Ctrl Pts',(-3.86812340800006,2.2,2.69499696899998));
#307906=CARTESIAN_POINT('Ctrl Pts',(-3.87073270700006,12.2,2.69512169399999));
#307907=CARTESIAN_POINT('Ctrl Pts',(-3.87073270700006,5.2,2.69512169399999));
#307908=CARTESIAN_POINT('Ctrl Pts',(-3.87073270700006,2.2,2.69512169399999));
#307909=CARTESIAN_POINT('Ctrl Pts',(-3.87334555400006,12.2,2.69524386199999));
#307910=CARTESIAN_POINT('Ctrl Pts',(-3.87334555400006,5.2,2.69524386199999));
#307911=CARTESIAN_POINT('Ctrl Pts',(-3.87334555400006,2.2,2.69524386199999));
#307912=CARTESIAN_POINT('Ctrl Pts',(-3.87596194200006,12.2,2.69536346599998));
#307913=CARTESIAN_POINT('Ctrl Pts',(-3.87596194200006,5.2,2.69536346599998));
#307914=CARTESIAN_POINT('Ctrl Pts',(-3.87596194200006,2.2,2.69536346599998));
#307915=CARTESIAN_POINT('Ctrl Pts',(-3.87858186500006,12.2,2.69548049999998));
#307916=CARTESIAN_POINT('Ctrl Pts',(-3.87858186500006,5.2,2.69548049999998));
#307917=CARTESIAN_POINT('Ctrl Pts',(-3.87858186500006,2.2,2.69548049999998));
#307918=CARTESIAN_POINT('Ctrl Pts',(-3.88120531800006,12.2,2.69559495899999));
#307919=CARTESIAN_POINT('Ctrl Pts',(-3.88120531800006,5.2,2.69559495899999));
#307920=CARTESIAN_POINT('Ctrl Pts',(-3.88120531800006,2.2,2.69559495899999));
#307921=CARTESIAN_POINT('Ctrl Pts',(-3.88383229600006,12.2,2.69570683299998));
#307922=CARTESIAN_POINT('Ctrl Pts',(-3.88383229600006,5.2,2.69570683299998));
#307923=CARTESIAN_POINT('Ctrl Pts',(-3.88383229600006,2.2,2.69570683299998));
#307924=CARTESIAN_POINT('Ctrl Pts',(-3.88646278800006,12.2,2.69581611799998));
#307925=CARTESIAN_POINT('Ctrl Pts',(-3.88646278800006,5.2,2.69581611799998));
#307926=CARTESIAN_POINT('Ctrl Pts',(-3.88646278800006,2.2,2.69581611799998));
#307927=CARTESIAN_POINT('Ctrl Pts',(-3.88909679200006,12.2,2.69592280299998));
#307928=CARTESIAN_POINT('Ctrl Pts',(-3.88909679200006,5.2,2.69592280299998));
#307929=CARTESIAN_POINT('Ctrl Pts',(-3.88909679200006,2.2,2.69592280299998));
#307930=CARTESIAN_POINT('Ctrl Pts',(-3.89173429500006,12.2,2.69602688099998));
#307931=CARTESIAN_POINT('Ctrl Pts',(-3.89173429500006,5.2,2.69602688099998));
#307932=CARTESIAN_POINT('Ctrl Pts',(-3.89173429500006,2.2,2.69602688099998));
#307933=CARTESIAN_POINT('Ctrl Pts',(-3.89437529600006,12.2,2.69612834599998));
#307934=CARTESIAN_POINT('Ctrl Pts',(-3.89437529600006,5.2,2.69612834599998));
#307935=CARTESIAN_POINT('Ctrl Pts',(-3.89437529600006,2.2,2.69612834599998));
#307936=CARTESIAN_POINT('Ctrl Pts',(-3.89701978600006,12.2,2.69622718999998));
#307937=CARTESIAN_POINT('Ctrl Pts',(-3.89701978600006,5.2,2.69622718999998));
#307938=CARTESIAN_POINT('Ctrl Pts',(-3.89701978600006,2.2,2.69622718999998));
#307939=CARTESIAN_POINT('Ctrl Pts',(-3.89966776200006,12.2,2.69632340999999));
#307940=CARTESIAN_POINT('Ctrl Pts',(-3.89966776200006,5.2,2.69632340999999));
#307941=CARTESIAN_POINT('Ctrl Pts',(-3.89966776200006,2.2,2.69632340999999));
#307942=CARTESIAN_POINT('Ctrl Pts',(-3.90231922000006,12.2,2.69641700299999));
#307943=CARTESIAN_POINT('Ctrl Pts',(-3.90231922000006,5.2,2.69641700299999));
#307944=CARTESIAN_POINT('Ctrl Pts',(-3.90231922000006,2.2,2.69641700299999));
#307945=CARTESIAN_POINT('Ctrl Pts',(-3.90497416000006,12.2,2.69650796599999));
#307946=CARTESIAN_POINT('Ctrl Pts',(-3.90497416000006,5.2,2.69650796599999));
#307947=CARTESIAN_POINT('Ctrl Pts',(-3.90497416000006,2.2,2.69650796599999));
#307948=CARTESIAN_POINT('Ctrl Pts',(-3.90710089600006,12.2,2.69657863299999));
#307949=CARTESIAN_POINT('Ctrl Pts',(-3.90710089600006,5.2,2.69657863299999));
#307950=CARTESIAN_POINT('Ctrl Pts',(-3.90710089600006,2.2,2.69657863299999));
#307951=CARTESIAN_POINT('Ctrl Pts',(-3.90869751400006,12.2,2.69663044999999));
#307952=CARTESIAN_POINT('Ctrl Pts',(-3.90869751400006,5.2,2.69663044999999));
#307953=CARTESIAN_POINT('Ctrl Pts',(-3.90869751400006,2.2,2.69663044999999));
#307954=CARTESIAN_POINT('Ctrl Pts',(-3.90976262200006,12.2,2.69666446799998));
#307955=CARTESIAN_POINT('Ctrl Pts',(-3.90976262200006,5.2,2.69666446799998));
#307956=CARTESIAN_POINT('Ctrl Pts',(-3.90976262200006,2.2,2.69666446799998));
#307957=CARTESIAN_POINT('Ctrl Pts',(-3.91029535000006,12.2,2.69668134599998));
#307958=CARTESIAN_POINT('Ctrl Pts',(-3.91029535000006,5.2,2.69668134599998));
#307959=CARTESIAN_POINT('Ctrl Pts',(-3.91029535000006,2.2,2.69668134599998));
#307960=CARTESIAN_POINT('',(-3.91029535000006,2.7,2.69668134599998));
#307961=CARTESIAN_POINT('',(-3.91029535000006,12.2,2.69668134599998));
#307962=CARTESIAN_POINT('Ctrl Pts',(-3.11652602400006,2.7,2.49742420799999));
#307963=CARTESIAN_POINT('Ctrl Pts',(-3.1168936600151,2.7,2.49771654590457));
#307964=CARTESIAN_POINT('Ctrl Pts',(-3.11816799097087,2.7,2.49871239564421));
#307965=CARTESIAN_POINT('Ctrl Pts',(-3.12398442812182,2.7,2.502910285736));
#307966=CARTESIAN_POINT('Ctrl Pts',(-3.12772253913452,2.7,2.50544873038177));
#307967=CARTESIAN_POINT('Ctrl Pts',(-3.14431490947368,2.7,2.51632623854521));
#307968=CARTESIAN_POINT('Ctrl Pts',(-3.15872784906809,2.7,2.52467057788753));
#307969=CARTESIAN_POINT('Ctrl Pts',(-3.21189785985966,2.7,2.55327156940896));
#307970=CARTESIAN_POINT('Ctrl Pts',(-3.26446474401564,2.7,2.57695346780209));
#307971=CARTESIAN_POINT('Ctrl Pts',(-3.45446370493968,2.7,2.64200888222062));
#307972=CARTESIAN_POINT('Ctrl Pts',(-3.64593588656003,2.7,2.68830585414583));
#307973=CARTESIAN_POINT('Ctrl Pts',(-3.91029535000006,2.7,2.69668134599998));
#307974=CARTESIAN_POINT('Origin',(-5.66300478732629E-14,15.2,-1.77635683940025E-14));
#307975=CARTESIAN_POINT('',(-4.09164014900006,2.7,2.41267090399998));
#307976=CARTESIAN_POINT('',(-4.09164014900006,12.2,2.41267090399998));
#307977=CARTESIAN_POINT('Origin',(-5.66300478732629E-14,2.7,-1.92943768261394E-14));
#307978=CARTESIAN_POINT('Ctrl Pts',(-4.09164015000006,12.2,2.41267090399998));
#307979=CARTESIAN_POINT('Ctrl Pts',(-4.09164015000006,5.2,2.41267090399998));
#307980=CARTESIAN_POINT('Ctrl Pts',(-4.09164015000006,2.2,2.41267090399998));
#307981=CARTESIAN_POINT('Ctrl Pts',(-4.09140069000006,12.2,2.41219472799998));
#307982=CARTESIAN_POINT('Ctrl Pts',(-4.09140069000006,5.2,2.41219472799998));
#307983=CARTESIAN_POINT('Ctrl Pts',(-4.09140069000006,2.2,2.41219472799998));
#307984=CARTESIAN_POINT('Ctrl Pts',(-4.09092167800006,12.2,2.41124280399998));
#307985=CARTESIAN_POINT('Ctrl Pts',(-4.09092167800006,5.2,2.41124280399998));
#307986=CARTESIAN_POINT('Ctrl Pts',(-4.09092167800006,2.2,2.41124280399998));
#307987=CARTESIAN_POINT('Ctrl Pts',(-4.09020288500006,12.2,2.40981619699999));
#307988=CARTESIAN_POINT('Ctrl Pts',(-4.09020288500006,5.2,2.40981619699999));
#307989=CARTESIAN_POINT('Ctrl Pts',(-4.09020288500006,2.2,2.40981619699999));
#307990=CARTESIAN_POINT('Ctrl Pts',(-4.08924394000006,12.2,2.40791661099998));
#307991=CARTESIAN_POINT('Ctrl Pts',(-4.08924394000006,5.2,2.40791661099998));
#307992=CARTESIAN_POINT('Ctrl Pts',(-4.08924394000006,2.2,2.40791661099998));
#307993=CARTESIAN_POINT('Ctrl Pts',(-4.08804433600006,12.2,2.40554639299998));
#307994=CARTESIAN_POINT('Ctrl Pts',(-4.08804433600006,5.2,2.40554639299998));
#307995=CARTESIAN_POINT('Ctrl Pts',(-4.08804433600006,2.2,2.40554639299998));
#307996=CARTESIAN_POINT('Ctrl Pts',(-4.08684381400006,12.2,2.40318043899999));
#307997=CARTESIAN_POINT('Ctrl Pts',(-4.08684381400006,5.2,2.40318043899999));
#307998=CARTESIAN_POINT('Ctrl Pts',(-4.08684381400006,2.2,2.40318043899999));
#307999=CARTESIAN_POINT('Ctrl Pts',(-4.08564237300006,12.2,2.40081874999999));
#308000=CARTESIAN_POINT('Ctrl Pts',(-4.08564237300006,5.2,2.40081874999999));
#308001=CARTESIAN_POINT('Ctrl Pts',(-4.08564237300006,2.2,2.40081874999999));
#308002=CARTESIAN_POINT('Ctrl Pts',(-4.08444001800006,12.2,2.39846132899999));
#308003=CARTESIAN_POINT('Ctrl Pts',(-4.08444001800006,5.2,2.39846132899999));
#308004=CARTESIAN_POINT('Ctrl Pts',(-4.08444001800006,2.2,2.39846132899999));
#308005=CARTESIAN_POINT('Ctrl Pts',(-4.08323675400006,12.2,2.39610817499998));
#308006=CARTESIAN_POINT('Ctrl Pts',(-4.08323675400006,5.2,2.39610817499998));
#308007=CARTESIAN_POINT('Ctrl Pts',(-4.08323675400006,2.2,2.39610817499998));
#308008=CARTESIAN_POINT('Ctrl Pts',(-4.08203258900006,12.2,2.39375929199999));
#308009=CARTESIAN_POINT('Ctrl Pts',(-4.08203258900006,5.2,2.39375929199999));
#308010=CARTESIAN_POINT('Ctrl Pts',(-4.08203258900006,2.2,2.39375929199999));
#308011=CARTESIAN_POINT('Ctrl Pts',(-4.08082753400006,12.2,2.39141468199998));
#308012=CARTESIAN_POINT('Ctrl Pts',(-4.08082753400006,5.2,2.39141468199998));
#308013=CARTESIAN_POINT('Ctrl Pts',(-4.08082753400006,2.2,2.39141468199998));
#308014=CARTESIAN_POINT('Ctrl Pts',(-4.07962159800006,12.2,2.38907435099998));
#308015=CARTESIAN_POINT('Ctrl Pts',(-4.07962159800006,5.2,2.38907435099998));
#308016=CARTESIAN_POINT('Ctrl Pts',(-4.07962159800006,2.2,2.38907435099998));
#308017=CARTESIAN_POINT('Ctrl Pts',(-4.07841479000006,12.2,2.38673829799998));
#308018=CARTESIAN_POINT('Ctrl Pts',(-4.07841479000006,5.2,2.38673829799998));
#308019=CARTESIAN_POINT('Ctrl Pts',(-4.07841479000006,2.2,2.38673829799998));
#308020=CARTESIAN_POINT('Ctrl Pts',(-4.07720712200006,12.2,2.38440652899998));
#308021=CARTESIAN_POINT('Ctrl Pts',(-4.07720712200006,5.2,2.38440652899998));
#308022=CARTESIAN_POINT('Ctrl Pts',(-4.07720712200006,2.2,2.38440652899998));
#308023=CARTESIAN_POINT('Ctrl Pts',(-4.07599860100006,12.2,2.38207904699999));
#308024=CARTESIAN_POINT('Ctrl Pts',(-4.07599860100006,5.2,2.38207904699999));
#308025=CARTESIAN_POINT('Ctrl Pts',(-4.07599860100006,2.2,2.38207904699999));
#308026=CARTESIAN_POINT('Ctrl Pts',(-4.07478923800006,12.2,2.37975585299999));
#308027=CARTESIAN_POINT('Ctrl Pts',(-4.07478923800006,5.2,2.37975585299999));
#308028=CARTESIAN_POINT('Ctrl Pts',(-4.07478923800006,2.2,2.37975585299999));
#308029=CARTESIAN_POINT('Ctrl Pts',(-4.07357903900006,12.2,2.37743694999998));
#308030=CARTESIAN_POINT('Ctrl Pts',(-4.07357903900006,5.2,2.37743694999998));
#308031=CARTESIAN_POINT('Ctrl Pts',(-4.07357903900006,2.2,2.37743694999998));
#308032=CARTESIAN_POINT('Ctrl Pts',(-4.07236801200006,12.2,2.37512234199999));
#308033=CARTESIAN_POINT('Ctrl Pts',(-4.07236801200006,5.2,2.37512234199999));
#308034=CARTESIAN_POINT('Ctrl Pts',(-4.07236801200006,2.2,2.37512234199999));
#308035=CARTESIAN_POINT('Ctrl Pts',(-4.07115616400006,12.2,2.37281202899998));
#308036=CARTESIAN_POINT('Ctrl Pts',(-4.07115616400006,5.2,2.37281202899998));
#308037=CARTESIAN_POINT('Ctrl Pts',(-4.07115616400006,2.2,2.37281202899998));
#308038=CARTESIAN_POINT('Ctrl Pts',(-4.06994350400006,12.2,2.37050601299998));
#308039=CARTESIAN_POINT('Ctrl Pts',(-4.06994350400006,5.2,2.37050601299998));
#308040=CARTESIAN_POINT('Ctrl Pts',(-4.06994350400006,2.2,2.37050601299998));
#308041=CARTESIAN_POINT('Ctrl Pts',(-4.06873003700006,12.2,2.36820429799998));
#308042=CARTESIAN_POINT('Ctrl Pts',(-4.06873003700006,5.2,2.36820429799998));
#308043=CARTESIAN_POINT('Ctrl Pts',(-4.06873003700006,2.2,2.36820429799998));
#308044=CARTESIAN_POINT('Ctrl Pts',(-4.06751577500006,12.2,2.36590688599998));
#308045=CARTESIAN_POINT('Ctrl Pts',(-4.06751577500006,5.2,2.36590688599998));
#308046=CARTESIAN_POINT('Ctrl Pts',(-4.06751577500006,2.2,2.36590688599998));
#308047=CARTESIAN_POINT('Ctrl Pts',(-4.06630072400006,12.2,2.36361377999999));
#308048=CARTESIAN_POINT('Ctrl Pts',(-4.06630072400006,5.2,2.36361377999999));
#308049=CARTESIAN_POINT('Ctrl Pts',(-4.06630072400006,2.2,2.36361377999999));
#308050=CARTESIAN_POINT('Ctrl Pts',(-4.06508489400006,12.2,2.36132498199999));
#308051=CARTESIAN_POINT('Ctrl Pts',(-4.06508489400006,5.2,2.36132498199999));
#308052=CARTESIAN_POINT('Ctrl Pts',(-4.06508489400006,2.2,2.36132498199999));
#308053=CARTESIAN_POINT('Ctrl Pts',(-4.06386829400006,12.2,2.35904049499998));
#308054=CARTESIAN_POINT('Ctrl Pts',(-4.06386829400006,5.2,2.35904049499998));
#308055=CARTESIAN_POINT('Ctrl Pts',(-4.06386829400006,2.2,2.35904049499998));
#308056=CARTESIAN_POINT('Ctrl Pts',(-4.06265093200005,12.2,2.35676032199999));
#308057=CARTESIAN_POINT('Ctrl Pts',(-4.06265093200005,5.2,2.35676032199999));
#308058=CARTESIAN_POINT('Ctrl Pts',(-4.06265093200005,2.2,2.35676032199999));
#308059=CARTESIAN_POINT('Ctrl Pts',(-4.06143281700006,12.2,2.35448446399998));
#308060=CARTESIAN_POINT('Ctrl Pts',(-4.06143281700006,5.2,2.35448446399998));
#308061=CARTESIAN_POINT('Ctrl Pts',(-4.06143281700006,2.2,2.35448446399998));
#308062=CARTESIAN_POINT('Ctrl Pts',(-4.06021395700006,12.2,2.35221292499999));
#308063=CARTESIAN_POINT('Ctrl Pts',(-4.06021395700006,5.2,2.35221292499999));
#308064=CARTESIAN_POINT('Ctrl Pts',(-4.06021395700006,2.2,2.35221292499999));
#308065=CARTESIAN_POINT('Ctrl Pts',(-4.05899436000006,12.2,2.34994570499998));
#308066=CARTESIAN_POINT('Ctrl Pts',(-4.05899436000006,5.2,2.34994570499998));
#308067=CARTESIAN_POINT('Ctrl Pts',(-4.05899436000006,2.2,2.34994570499998));
#308068=CARTESIAN_POINT('Ctrl Pts',(-4.05777403500006,12.2,2.34768281099999));
#308069=CARTESIAN_POINT('Ctrl Pts',(-4.05777403500006,5.2,2.34768281099999));
#308070=CARTESIAN_POINT('Ctrl Pts',(-4.05777403500006,2.2,2.34768281099999));
#308071=CARTESIAN_POINT('Ctrl Pts',(-4.05655298900006,12.2,2.34542424099998));
#308072=CARTESIAN_POINT('Ctrl Pts',(-4.05655298900006,5.2,2.34542424099998));
#308073=CARTESIAN_POINT('Ctrl Pts',(-4.05655298900006,2.2,2.34542424099998));
#308074=CARTESIAN_POINT('Ctrl Pts',(-4.05533123200006,12.2,2.34316999899999));
#308075=CARTESIAN_POINT('Ctrl Pts',(-4.05533123200006,5.2,2.34316999899999));
#308076=CARTESIAN_POINT('Ctrl Pts',(-4.05533123200006,2.2,2.34316999899999));
#308077=CARTESIAN_POINT('Ctrl Pts',(-4.05410877200006,12.2,2.34092008799998));
#308078=CARTESIAN_POINT('Ctrl Pts',(-4.05410877200006,5.2,2.34092008799998));
#308079=CARTESIAN_POINT('Ctrl Pts',(-4.05410877200006,2.2,2.34092008799998));
#308080=CARTESIAN_POINT('Ctrl Pts',(-4.05288561800006,12.2,2.33867450899998));
#308081=CARTESIAN_POINT('Ctrl Pts',(-4.05288561800006,5.2,2.33867450899998));
#308082=CARTESIAN_POINT('Ctrl Pts',(-4.05288561800006,2.2,2.33867450899998));
#308083=CARTESIAN_POINT('Ctrl Pts',(-4.05166177700006,12.2,2.33643326599998));
#308084=CARTESIAN_POINT('Ctrl Pts',(-4.05166177700006,5.2,2.33643326599998));
#308085=CARTESIAN_POINT('Ctrl Pts',(-4.05166177700006,2.2,2.33643326599998));
#308086=CARTESIAN_POINT('Ctrl Pts',(-4.05043725800006,12.2,2.33419635999998));
#308087=CARTESIAN_POINT('Ctrl Pts',(-4.05043725800006,5.2,2.33419635999998));
#308088=CARTESIAN_POINT('Ctrl Pts',(-4.05043725800006,2.2,2.33419635999998));
#308089=CARTESIAN_POINT('Ctrl Pts',(-4.04921207100006,12.2,2.33196379399998));
#308090=CARTESIAN_POINT('Ctrl Pts',(-4.04921207100006,5.2,2.33196379399998));
#308091=CARTESIAN_POINT('Ctrl Pts',(-4.04921207100006,2.2,2.33196379399998));
#308092=CARTESIAN_POINT('Ctrl Pts',(-4.04798622300006,12.2,2.32973557199998));
#308093=CARTESIAN_POINT('Ctrl Pts',(-4.04798622300006,5.2,2.32973557199998));
#308094=CARTESIAN_POINT('Ctrl Pts',(-4.04798622300006,2.2,2.32973557199998));
#308095=CARTESIAN_POINT('Ctrl Pts',(-4.04675972500006,12.2,2.32751169299998));
#308096=CARTESIAN_POINT('Ctrl Pts',(-4.04675972500006,5.2,2.32751169299998));
#308097=CARTESIAN_POINT('Ctrl Pts',(-4.04675972500006,2.2,2.32751169299998));
#308098=CARTESIAN_POINT('Ctrl Pts',(-4.04553258300006,12.2,2.32529216199998));
#308099=CARTESIAN_POINT('Ctrl Pts',(-4.04553258300006,5.2,2.32529216199998));
#308100=CARTESIAN_POINT('Ctrl Pts',(-4.04553258300006,2.2,2.32529216199998));
#308101=CARTESIAN_POINT('Ctrl Pts',(-4.04430480600006,12.2,2.32307697999998));
#308102=CARTESIAN_POINT('Ctrl Pts',(-4.04430480600006,5.2,2.32307697999998));
#308103=CARTESIAN_POINT('Ctrl Pts',(-4.04430480600006,2.2,2.32307697999998));
#308104=CARTESIAN_POINT('Ctrl Pts',(-4.04307640300006,12.2,2.32086615099998));
#308105=CARTESIAN_POINT('Ctrl Pts',(-4.04307640300006,5.2,2.32086615099998));
#308106=CARTESIAN_POINT('Ctrl Pts',(-4.04307640300006,2.2,2.32086615099998));
#308107=CARTESIAN_POINT('Ctrl Pts',(-4.04184738300006,12.2,2.31865967499999));
#308108=CARTESIAN_POINT('Ctrl Pts',(-4.04184738300006,5.2,2.31865967499999));
#308109=CARTESIAN_POINT('Ctrl Pts',(-4.04184738300006,2.2,2.31865967499999));
#308110=CARTESIAN_POINT('Ctrl Pts',(-4.04061775500006,12.2,2.31645755699999));
#308111=CARTESIAN_POINT('Ctrl Pts',(-4.04061775500006,5.2,2.31645755699999));
#308112=CARTESIAN_POINT('Ctrl Pts',(-4.04061775500006,2.2,2.31645755699999));
#308113=CARTESIAN_POINT('Ctrl Pts',(-4.03938752700006,12.2,2.31425979699999));
#308114=CARTESIAN_POINT('Ctrl Pts',(-4.03938752700006,5.2,2.31425979699999));
#308115=CARTESIAN_POINT('Ctrl Pts',(-4.03938752700006,2.2,2.31425979699999));
#308116=CARTESIAN_POINT('Ctrl Pts',(-4.03815670700006,12.2,2.31206639799999));
#308117=CARTESIAN_POINT('Ctrl Pts',(-4.03815670700006,5.2,2.31206639799999));
#308118=CARTESIAN_POINT('Ctrl Pts',(-4.03815670700006,2.2,2.31206639799999));
#308119=CARTESIAN_POINT('Ctrl Pts',(-4.03692530400006,12.2,2.30987736199999));
#308120=CARTESIAN_POINT('Ctrl Pts',(-4.03692530400006,5.2,2.30987736199999));
#308121=CARTESIAN_POINT('Ctrl Pts',(-4.03692530400006,2.2,2.30987736199999));
#308122=CARTESIAN_POINT('Ctrl Pts',(-4.03569332700005,12.2,2.30769269299998));
#308123=CARTESIAN_POINT('Ctrl Pts',(-4.03569332700005,5.2,2.30769269299998));
#308124=CARTESIAN_POINT('Ctrl Pts',(-4.03569332700005,2.2,2.30769269299998));
#308125=CARTESIAN_POINT('Ctrl Pts',(-4.03446078600005,12.2,2.30551239099999));
#308126=CARTESIAN_POINT('Ctrl Pts',(-4.03446078600005,5.2,2.30551239099999));
#308127=CARTESIAN_POINT('Ctrl Pts',(-4.03446078600005,2.2,2.30551239099999));
#308128=CARTESIAN_POINT('Ctrl Pts',(-4.03322768800006,12.2,2.30333645999998));
#308129=CARTESIAN_POINT('Ctrl Pts',(-4.03322768800006,5.2,2.30333645999998));
#308130=CARTESIAN_POINT('Ctrl Pts',(-4.03322768800006,2.2,2.30333645999998));
#308131=CARTESIAN_POINT('Ctrl Pts',(-4.03199404200006,12.2,2.30116490199999));
#308132=CARTESIAN_POINT('Ctrl Pts',(-4.03199404200006,5.2,2.30116490199999));
#308133=CARTESIAN_POINT('Ctrl Pts',(-4.03199404200006,2.2,2.30116490199999));
#308134=CARTESIAN_POINT('Ctrl Pts',(-4.03075985700006,12.2,2.29899771799999));
#308135=CARTESIAN_POINT('Ctrl Pts',(-4.03075985700006,5.2,2.29899771799999));
#308136=CARTESIAN_POINT('Ctrl Pts',(-4.03075985700006,2.2,2.29899771799999));
#308137=CARTESIAN_POINT('Ctrl Pts',(-4.02952514200006,12.2,2.29683491099999));
#308138=CARTESIAN_POINT('Ctrl Pts',(-4.02952514200006,5.2,2.29683491099999));
#308139=CARTESIAN_POINT('Ctrl Pts',(-4.02952514200006,2.2,2.29683491099999));
#308140=CARTESIAN_POINT('Ctrl Pts',(-4.02828990600006,12.2,2.29467648299998));
#308141=CARTESIAN_POINT('Ctrl Pts',(-4.02828990600006,5.2,2.29467648299998));
#308142=CARTESIAN_POINT('Ctrl Pts',(-4.02828990600006,2.2,2.29467648299998));
#308143=CARTESIAN_POINT('Ctrl Pts',(-4.02705415600006,12.2,2.29252243799999));
#308144=CARTESIAN_POINT('Ctrl Pts',(-4.02705415600006,5.2,2.29252243799999));
#308145=CARTESIAN_POINT('Ctrl Pts',(-4.02705415600006,2.2,2.29252243799999));
#308146=CARTESIAN_POINT('Ctrl Pts',(-4.02581790300006,12.2,2.29037277599998));
#308147=CARTESIAN_POINT('Ctrl Pts',(-4.02581790300006,5.2,2.29037277599998));
#308148=CARTESIAN_POINT('Ctrl Pts',(-4.02581790300006,2.2,2.29037277599998));
#308149=CARTESIAN_POINT('Ctrl Pts',(-4.02458115500006,12.2,2.28822749899999));
#308150=CARTESIAN_POINT('Ctrl Pts',(-4.02458115500006,5.2,2.28822749899999));
#308151=CARTESIAN_POINT('Ctrl Pts',(-4.02458115500006,2.2,2.28822749899999));
#308152=CARTESIAN_POINT('Ctrl Pts',(-4.02334392100006,12.2,2.28608661099999));
#308153=CARTESIAN_POINT('Ctrl Pts',(-4.02334392100006,5.2,2.28608661099999));
#308154=CARTESIAN_POINT('Ctrl Pts',(-4.02334392100006,2.2,2.28608661099999));
#308155=CARTESIAN_POINT('Ctrl Pts',(-4.02210620900005,12.2,2.28395011399999));
#308156=CARTESIAN_POINT('Ctrl Pts',(-4.02210620900005,5.2,2.28395011399999));
#308157=CARTESIAN_POINT('Ctrl Pts',(-4.02210620900005,2.2,2.28395011399999));
#308158=CARTESIAN_POINT('Ctrl Pts',(-4.02086802900006,12.2,2.28181800899999));
#308159=CARTESIAN_POINT('Ctrl Pts',(-4.02086802900006,5.2,2.28181800899999));
#308160=CARTESIAN_POINT('Ctrl Pts',(-4.02086802900006,2.2,2.28181800899999));
#308161=CARTESIAN_POINT('Ctrl Pts',(-4.01962939000006,12.2,2.27969029899999));
#308162=CARTESIAN_POINT('Ctrl Pts',(-4.01962939000006,5.2,2.27969029899999));
#308163=CARTESIAN_POINT('Ctrl Pts',(-4.01962939000006,2.2,2.27969029899999));
#308164=CARTESIAN_POINT('Ctrl Pts',(-4.01839029900006,12.2,2.27756698499999));
#308165=CARTESIAN_POINT('Ctrl Pts',(-4.01839029900006,5.2,2.27756698499999));
#308166=CARTESIAN_POINT('Ctrl Pts',(-4.01839029900006,2.2,2.27756698499999));
#308167=CARTESIAN_POINT('Ctrl Pts',(-4.01715076700006,12.2,2.27544807099999));
#308168=CARTESIAN_POINT('Ctrl Pts',(-4.01715076700006,5.2,2.27544807099999));
#308169=CARTESIAN_POINT('Ctrl Pts',(-4.01715076700006,2.2,2.27544807099999));
#308170=CARTESIAN_POINT('Ctrl Pts',(-4.01591080300006,12.2,2.27333355699999));
#308171=CARTESIAN_POINT('Ctrl Pts',(-4.01591080300006,5.2,2.27333355699999));
#308172=CARTESIAN_POINT('Ctrl Pts',(-4.01591080300006,2.2,2.27333355699999));
#308173=CARTESIAN_POINT('Ctrl Pts',(-4.01467041400006,12.2,2.27122344799998));
#308174=CARTESIAN_POINT('Ctrl Pts',(-4.01467041400006,5.2,2.27122344799998));
#308175=CARTESIAN_POINT('Ctrl Pts',(-4.01467041400006,2.2,2.27122344799998));
#308176=CARTESIAN_POINT('Ctrl Pts',(-4.01342961000006,12.2,2.26911774299999));
#308177=CARTESIAN_POINT('Ctrl Pts',(-4.01342961000006,5.2,2.26911774299999));
#308178=CARTESIAN_POINT('Ctrl Pts',(-4.01342961000006,2.2,2.26911774299999));
#308179=CARTESIAN_POINT('Ctrl Pts',(-4.01218840000006,12.2,2.26701644599999));
#308180=CARTESIAN_POINT('Ctrl Pts',(-4.01218840000006,5.2,2.26701644599999));
#308181=CARTESIAN_POINT('Ctrl Pts',(-4.01218840000006,2.2,2.26701644599999));
#308182=CARTESIAN_POINT('Ctrl Pts',(-4.01094679400006,12.2,2.26491955899998));
#308183=CARTESIAN_POINT('Ctrl Pts',(-4.01094679400006,5.2,2.26491955899998));
#308184=CARTESIAN_POINT('Ctrl Pts',(-4.01094679400006,2.2,2.26491955899998));
#308185=CARTESIAN_POINT('Ctrl Pts',(-4.00970479900006,12.2,2.26282708299999));
#308186=CARTESIAN_POINT('Ctrl Pts',(-4.00970479900006,5.2,2.26282708299999));
#308187=CARTESIAN_POINT('Ctrl Pts',(-4.00970479900006,2.2,2.26282708299999));
#308188=CARTESIAN_POINT('Ctrl Pts',(-4.00846242600006,12.2,2.26073902199999));
#308189=CARTESIAN_POINT('Ctrl Pts',(-4.00846242600006,5.2,2.26073902199999));
#308190=CARTESIAN_POINT('Ctrl Pts',(-4.00846242600006,2.2,2.26073902199999));
#308191=CARTESIAN_POINT('Ctrl Pts',(-4.00721968300005,12.2,2.25865537699999));
#308192=CARTESIAN_POINT('Ctrl Pts',(-4.00721968300005,5.2,2.25865537699999));
#308193=CARTESIAN_POINT('Ctrl Pts',(-4.00721968300005,2.2,2.25865537699999));
#308194=CARTESIAN_POINT('Ctrl Pts',(-4.00597657800006,12.2,2.25657614799998));
#308195=CARTESIAN_POINT('Ctrl Pts',(-4.00597657800006,5.2,2.25657614799998));
#308196=CARTESIAN_POINT('Ctrl Pts',(-4.00597657800006,2.2,2.25657614799998));
#308197=CARTESIAN_POINT('Ctrl Pts',(-4.00473312200006,12.2,2.25450133999999));
#308198=CARTESIAN_POINT('Ctrl Pts',(-4.00473312200006,5.2,2.25450133999999));
#308199=CARTESIAN_POINT('Ctrl Pts',(-4.00473312200006,2.2,2.25450133999999));
#308200=CARTESIAN_POINT('Ctrl Pts',(-4.00348932300005,12.2,2.25243095499998));
#308201=CARTESIAN_POINT('Ctrl Pts',(-4.00348932300005,5.2,2.25243095499998));
#308202=CARTESIAN_POINT('Ctrl Pts',(-4.00348932300005,2.2,2.25243095499998));
#308203=CARTESIAN_POINT('Ctrl Pts',(-4.00224519000006,12.2,2.25036499399998));
#308204=CARTESIAN_POINT('Ctrl Pts',(-4.00224519000006,5.2,2.25036499399998));
#308205=CARTESIAN_POINT('Ctrl Pts',(-4.00224519000006,2.2,2.25036499399998));
#308206=CARTESIAN_POINT('Ctrl Pts',(-4.00100073300006,12.2,2.24830345699999));
#308207=CARTESIAN_POINT('Ctrl Pts',(-4.00100073300006,5.2,2.24830345699999));
#308208=CARTESIAN_POINT('Ctrl Pts',(-4.00100073300006,2.2,2.24830345699999));
#308209=CARTESIAN_POINT('Ctrl Pts',(-3.99975596000006,12.2,2.24624635099998));
#308210=CARTESIAN_POINT('Ctrl Pts',(-3.99975596000006,5.2,2.24624635099998));
#308211=CARTESIAN_POINT('Ctrl Pts',(-3.99975596000006,2.2,2.24624635099998));
#308212=CARTESIAN_POINT('Ctrl Pts',(-3.99851088100006,12.2,2.24419367399999));
#308213=CARTESIAN_POINT('Ctrl Pts',(-3.99851088100006,5.2,2.24419367399999));
#308214=CARTESIAN_POINT('Ctrl Pts',(-3.99851088100006,2.2,2.24419367399999));
#308215=CARTESIAN_POINT('Ctrl Pts',(-3.99726550600006,12.2,2.24214542899999));
#308216=CARTESIAN_POINT('Ctrl Pts',(-3.99726550600006,5.2,2.24214542899999));
#308217=CARTESIAN_POINT('Ctrl Pts',(-3.99726550600006,2.2,2.24214542899999));
#308218=CARTESIAN_POINT('Ctrl Pts',(-3.99601984000006,12.2,2.24010161799999));
#308219=CARTESIAN_POINT('Ctrl Pts',(-3.99601984000006,5.2,2.24010161799999));
#308220=CARTESIAN_POINT('Ctrl Pts',(-3.99601984000006,2.2,2.24010161799999));
#308221=CARTESIAN_POINT('Ctrl Pts',(-3.99477389700006,12.2,2.23806224299999));
#308222=CARTESIAN_POINT('Ctrl Pts',(-3.99477389700006,5.2,2.23806224299999));
#308223=CARTESIAN_POINT('Ctrl Pts',(-3.99477389700006,2.2,2.23806224299999));
#308224=CARTESIAN_POINT('Ctrl Pts',(-3.99352768500005,12.2,2.23602730699998));
#308225=CARTESIAN_POINT('Ctrl Pts',(-3.99352768500005,5.2,2.23602730699998));
#308226=CARTESIAN_POINT('Ctrl Pts',(-3.99352768500005,2.2,2.23602730699998));
#308227=CARTESIAN_POINT('Ctrl Pts',(-3.99228121100006,12.2,2.23399680999998));
#308228=CARTESIAN_POINT('Ctrl Pts',(-3.99228121100006,5.2,2.23399680999998));
#308229=CARTESIAN_POINT('Ctrl Pts',(-3.99228121100006,2.2,2.23399680999998));
#308230=CARTESIAN_POINT('Ctrl Pts',(-3.99103448600005,12.2,2.23197075599999));
#308231=CARTESIAN_POINT('Ctrl Pts',(-3.99103448600005,5.2,2.23197075599999));
#308232=CARTESIAN_POINT('Ctrl Pts',(-3.99103448600005,2.2,2.23197075599999));
#308233=CARTESIAN_POINT('Ctrl Pts',(-3.98978751900006,12.2,2.22994914599999));
#308234=CARTESIAN_POINT('Ctrl Pts',(-3.98978751900006,5.2,2.22994914599999));
#308235=CARTESIAN_POINT('Ctrl Pts',(-3.98978751900006,2.2,2.22994914599999));
#308236=CARTESIAN_POINT('Ctrl Pts',(-3.98854032000005,12.2,2.22793198099998));
#308237=CARTESIAN_POINT('Ctrl Pts',(-3.98854032000005,5.2,2.22793198099998));
#308238=CARTESIAN_POINT('Ctrl Pts',(-3.98854032000005,2.2,2.22793198099998));
#308239=CARTESIAN_POINT('Ctrl Pts',(-3.98729289800006,12.2,2.22591926399998));
#308240=CARTESIAN_POINT('Ctrl Pts',(-3.98729289800006,5.2,2.22591926399998));
#308241=CARTESIAN_POINT('Ctrl Pts',(-3.98729289800006,2.2,2.22591926399998));
#308242=CARTESIAN_POINT('Ctrl Pts',(-3.98604526000006,12.2,2.22391099699998));
#308243=CARTESIAN_POINT('Ctrl Pts',(-3.98604526000006,5.2,2.22391099699998));
#308244=CARTESIAN_POINT('Ctrl Pts',(-3.98604526000006,2.2,2.22391099699998));
#308245=CARTESIAN_POINT('Ctrl Pts',(-3.98479741800006,12.2,2.22190718199998));
#308246=CARTESIAN_POINT('Ctrl Pts',(-3.98479741800006,5.2,2.22190718199998));
#308247=CARTESIAN_POINT('Ctrl Pts',(-3.98479741800006,2.2,2.22190718199998));
#308248=CARTESIAN_POINT('Ctrl Pts',(-3.98354938000006,12.2,2.21990781899999));
#308249=CARTESIAN_POINT('Ctrl Pts',(-3.98354938000006,5.2,2.21990781899999));
#308250=CARTESIAN_POINT('Ctrl Pts',(-3.98354938000006,2.2,2.21990781899999));
#308251=CARTESIAN_POINT('Ctrl Pts',(-3.98230115500006,12.2,2.21791291299999));
#308252=CARTESIAN_POINT('Ctrl Pts',(-3.98230115500006,5.2,2.21791291299999));
#308253=CARTESIAN_POINT('Ctrl Pts',(-3.98230115500006,2.2,2.21791291299999));
#308254=CARTESIAN_POINT('Ctrl Pts',(-3.98105275500006,12.2,2.21592246299998));
#308255=CARTESIAN_POINT('Ctrl Pts',(-3.98105275500006,5.2,2.21592246299998));
#308256=CARTESIAN_POINT('Ctrl Pts',(-3.98105275500006,2.2,2.21592246299998));
#308257=CARTESIAN_POINT('Ctrl Pts',(-3.97980418500006,12.2,2.21393647299998));
#308258=CARTESIAN_POINT('Ctrl Pts',(-3.97980418500006,5.2,2.21393647299998));
#308259=CARTESIAN_POINT('Ctrl Pts',(-3.97980418500006,2.2,2.21393647299998));
#308260=CARTESIAN_POINT('Ctrl Pts',(-3.97855545900006,12.2,2.21195494399999));
#308261=CARTESIAN_POINT('Ctrl Pts',(-3.97855545900006,5.2,2.21195494399999));
#308262=CARTESIAN_POINT('Ctrl Pts',(-3.97855545900006,2.2,2.21195494399999));
#308263=CARTESIAN_POINT('Ctrl Pts',(-3.97730658300006,12.2,2.20997787699998));
#308264=CARTESIAN_POINT('Ctrl Pts',(-3.97730658300006,5.2,2.20997787699998));
#308265=CARTESIAN_POINT('Ctrl Pts',(-3.97730658300006,2.2,2.20997787699998));
#308266=CARTESIAN_POINT('Ctrl Pts',(-3.97605756700006,12.2,2.20800527499998));
#308267=CARTESIAN_POINT('Ctrl Pts',(-3.97605756700006,5.2,2.20800527499998));
#308268=CARTESIAN_POINT('Ctrl Pts',(-3.97605756700006,2.2,2.20800527499998));
#308269=CARTESIAN_POINT('Ctrl Pts',(-3.97480842100006,12.2,2.20603713899999));
#308270=CARTESIAN_POINT('Ctrl Pts',(-3.97480842100006,5.2,2.20603713899999));
#308271=CARTESIAN_POINT('Ctrl Pts',(-3.97480842100006,2.2,2.20603713899999));
#308272=CARTESIAN_POINT('Ctrl Pts',(-3.97355915400006,12.2,2.20407347199998));
#308273=CARTESIAN_POINT('Ctrl Pts',(-3.97355915400006,5.2,2.20407347199998));
#308274=CARTESIAN_POINT('Ctrl Pts',(-3.97355915400006,2.2,2.20407347199998));
#308275=CARTESIAN_POINT('Ctrl Pts',(-3.97230977800006,12.2,2.20211427399999));
#308276=CARTESIAN_POINT('Ctrl Pts',(-3.97230977800006,5.2,2.20211427399999));
#308277=CARTESIAN_POINT('Ctrl Pts',(-3.97230977800006,2.2,2.20211427399999));
#308278=CARTESIAN_POINT('Ctrl Pts',(-3.97106029800006,12.2,2.20015954799999));
#308279=CARTESIAN_POINT('Ctrl Pts',(-3.97106029800006,5.2,2.20015954799999));
#308280=CARTESIAN_POINT('Ctrl Pts',(-3.97106029800006,2.2,2.20015954799999));
#308281=CARTESIAN_POINT('Ctrl Pts',(-3.96981072700005,12.2,2.19820929599999));
#308282=CARTESIAN_POINT('Ctrl Pts',(-3.96981072700005,5.2,2.19820929599999));
#308283=CARTESIAN_POINT('Ctrl Pts',(-3.96981072700005,2.2,2.19820929599999));
#308284=CARTESIAN_POINT('Ctrl Pts',(-3.96856107200006,12.2,2.19626351999999));
#308285=CARTESIAN_POINT('Ctrl Pts',(-3.96856107200006,5.2,2.19626351999999));
#308286=CARTESIAN_POINT('Ctrl Pts',(-3.96856107200006,2.2,2.19626351999999));
#308287=CARTESIAN_POINT('Ctrl Pts',(-3.96731134500006,12.2,2.19432221999998));
#308288=CARTESIAN_POINT('Ctrl Pts',(-3.96731134500006,5.2,2.19432221999998));
#308289=CARTESIAN_POINT('Ctrl Pts',(-3.96731134500006,2.2,2.19432221999998));
#308290=CARTESIAN_POINT('Ctrl Pts',(-3.96606155400006,12.2,2.19238539899999));
#308291=CARTESIAN_POINT('Ctrl Pts',(-3.96606155400006,5.2,2.19238539899999));
#308292=CARTESIAN_POINT('Ctrl Pts',(-3.96606155400006,2.2,2.19238539899999));
#308293=CARTESIAN_POINT('Ctrl Pts',(-3.96481170800006,12.2,2.19045305899999));
#308294=CARTESIAN_POINT('Ctrl Pts',(-3.96481170800006,5.2,2.19045305899999));
#308295=CARTESIAN_POINT('Ctrl Pts',(-3.96481170800006,2.2,2.19045305899999));
#308296=CARTESIAN_POINT('Ctrl Pts',(-3.96356181700006,12.2,2.18852520099999));
#308297=CARTESIAN_POINT('Ctrl Pts',(-3.96356181700006,5.2,2.18852520099999));
#308298=CARTESIAN_POINT('Ctrl Pts',(-3.96356181700006,2.2,2.18852520099999));
#308299=CARTESIAN_POINT('Ctrl Pts',(-3.96231189200006,12.2,2.18660182699999));
#308300=CARTESIAN_POINT('Ctrl Pts',(-3.96231189200006,5.2,2.18660182699999));
#308301=CARTESIAN_POINT('Ctrl Pts',(-3.96231189200006,2.2,2.18660182699999));
#308302=CARTESIAN_POINT('Ctrl Pts',(-3.96106194100006,12.2,2.18468293799999));
#308303=CARTESIAN_POINT('Ctrl Pts',(-3.96106194100006,5.2,2.18468293799999));
#308304=CARTESIAN_POINT('Ctrl Pts',(-3.96106194100006,2.2,2.18468293799999));
#308305=CARTESIAN_POINT('Ctrl Pts',(-3.95981197400006,12.2,2.18276853699999));
#308306=CARTESIAN_POINT('Ctrl Pts',(-3.95981197400006,5.2,2.18276853699999));
#308307=CARTESIAN_POINT('Ctrl Pts',(-3.95981197400006,2.2,2.18276853699999));
#308308=CARTESIAN_POINT('Ctrl Pts',(-3.95856200100006,12.2,2.18085862499999));
#308309=CARTESIAN_POINT('Ctrl Pts',(-3.95856200100006,5.2,2.18085862499999));
#308310=CARTESIAN_POINT('Ctrl Pts',(-3.95856200100006,2.2,2.18085862499999));
#308311=CARTESIAN_POINT('Ctrl Pts',(-3.95731203200006,12.2,2.17895320399998));
#308312=CARTESIAN_POINT('Ctrl Pts',(-3.95731203200006,5.2,2.17895320399998));
#308313=CARTESIAN_POINT('Ctrl Pts',(-3.95731203200006,2.2,2.17895320399998));
#308314=CARTESIAN_POINT('Ctrl Pts',(-3.95606207500006,12.2,2.17705227499998));
#308315=CARTESIAN_POINT('Ctrl Pts',(-3.95606207500006,5.2,2.17705227499998));
#308316=CARTESIAN_POINT('Ctrl Pts',(-3.95606207500006,2.2,2.17705227499998));
#308317=CARTESIAN_POINT('Ctrl Pts',(-3.95481214000006,12.2,2.17515584099999));
#308318=CARTESIAN_POINT('Ctrl Pts',(-3.95481214000006,5.2,2.17515584099999));
#308319=CARTESIAN_POINT('Ctrl Pts',(-3.95481214000006,2.2,2.17515584099999));
#308320=CARTESIAN_POINT('Ctrl Pts',(-3.95356223800006,12.2,2.17326390099998));
#308321=CARTESIAN_POINT('Ctrl Pts',(-3.95356223800006,5.2,2.17326390099998));
#308322=CARTESIAN_POINT('Ctrl Pts',(-3.95356223800006,2.2,2.17326390099998));
#308323=CARTESIAN_POINT('Ctrl Pts',(-3.95231237800005,12.2,2.17137645899999));
#308324=CARTESIAN_POINT('Ctrl Pts',(-3.95231237800005,5.2,2.17137645899999));
#308325=CARTESIAN_POINT('Ctrl Pts',(-3.95231237800005,2.2,2.17137645899999));
#308326=CARTESIAN_POINT('Ctrl Pts',(-3.95106257000006,12.2,2.16949351599999));
#308327=CARTESIAN_POINT('Ctrl Pts',(-3.95106257000006,5.2,2.16949351599999));
#308328=CARTESIAN_POINT('Ctrl Pts',(-3.95106257000006,2.2,2.16949351599999));
#308329=CARTESIAN_POINT('Ctrl Pts',(-3.94981282300006,12.2,2.16761507299998));
#308330=CARTESIAN_POINT('Ctrl Pts',(-3.94981282300006,5.2,2.16761507299998));
#308331=CARTESIAN_POINT('Ctrl Pts',(-3.94981282300006,2.2,2.16761507299998));
#308332=CARTESIAN_POINT('Ctrl Pts',(-3.94856314700006,12.2,2.16574113299998));
#308333=CARTESIAN_POINT('Ctrl Pts',(-3.94856314700006,5.2,2.16574113299998));
#308334=CARTESIAN_POINT('Ctrl Pts',(-3.94856314700006,2.2,2.16574113299998));
#308335=CARTESIAN_POINT('Ctrl Pts',(-3.94731355300006,12.2,2.16387169499999));
#308336=CARTESIAN_POINT('Ctrl Pts',(-3.94731355300006,5.2,2.16387169499999));
#308337=CARTESIAN_POINT('Ctrl Pts',(-3.94731355300006,2.2,2.16387169499999));
#308338=CARTESIAN_POINT('Ctrl Pts',(-3.94606404800006,12.2,2.16200676399998));
#308339=CARTESIAN_POINT('Ctrl Pts',(-3.94606404800006,5.2,2.16200676399998));
#308340=CARTESIAN_POINT('Ctrl Pts',(-3.94606404800006,2.2,2.16200676399998));
#308341=CARTESIAN_POINT('Ctrl Pts',(-3.94481464400006,12.2,2.16014633899999));
#308342=CARTESIAN_POINT('Ctrl Pts',(-3.94481464400006,5.2,2.16014633899999));
#308343=CARTESIAN_POINT('Ctrl Pts',(-3.94481464400006,2.2,2.16014633899999));
#308344=CARTESIAN_POINT('Ctrl Pts',(-3.94356535100005,12.2,2.15829042199998));
#308345=CARTESIAN_POINT('Ctrl Pts',(-3.94356535100005,5.2,2.15829042199998));
#308346=CARTESIAN_POINT('Ctrl Pts',(-3.94356535100005,2.2,2.15829042199998));
#308347=CARTESIAN_POINT('Ctrl Pts',(-3.94231617800005,12.2,2.15643901499998));
#308348=CARTESIAN_POINT('Ctrl Pts',(-3.94231617800005,5.2,2.15643901499998));
#308349=CARTESIAN_POINT('Ctrl Pts',(-3.94231617800005,2.2,2.15643901499998));
#308350=CARTESIAN_POINT('Ctrl Pts',(-3.94106713400006,12.2,2.15459211999999));
#308351=CARTESIAN_POINT('Ctrl Pts',(-3.94106713400006,5.2,2.15459211999999));
#308352=CARTESIAN_POINT('Ctrl Pts',(-3.94106713400006,2.2,2.15459211999999));
#308353=CARTESIAN_POINT('Ctrl Pts',(-3.93981823000006,12.2,2.15274973599998));
#308354=CARTESIAN_POINT('Ctrl Pts',(-3.93981823000006,5.2,2.15274973599998));
#308355=CARTESIAN_POINT('Ctrl Pts',(-3.93981823000006,2.2,2.15274973599998));
#308356=CARTESIAN_POINT('Ctrl Pts',(-3.93856947700006,12.2,2.15091186799999));
#308357=CARTESIAN_POINT('Ctrl Pts',(-3.93856947700006,5.2,2.15091186799999));
#308358=CARTESIAN_POINT('Ctrl Pts',(-3.93856947700006,2.2,2.15091186799999));
#308359=CARTESIAN_POINT('Ctrl Pts',(-3.93732088100006,12.2,2.14907851499999));
#308360=CARTESIAN_POINT('Ctrl Pts',(-3.93732088100006,5.2,2.14907851499999));
#308361=CARTESIAN_POINT('Ctrl Pts',(-3.93732088100006,2.2,2.14907851499999));
#308362=CARTESIAN_POINT('Ctrl Pts',(-3.93607245700006,12.2,2.14724967999999));
#308363=CARTESIAN_POINT('Ctrl Pts',(-3.93607245700006,5.2,2.14724967999999));
#308364=CARTESIAN_POINT('Ctrl Pts',(-3.93607245700006,2.2,2.14724967999999));
#308365=CARTESIAN_POINT('Ctrl Pts',(-3.93482421000006,12.2,2.14542536399998));
#308366=CARTESIAN_POINT('Ctrl Pts',(-3.93482421000006,5.2,2.14542536399998));
#308367=CARTESIAN_POINT('Ctrl Pts',(-3.93482421000006,2.2,2.14542536399998));
#308368=CARTESIAN_POINT('Ctrl Pts',(-3.93357615500006,12.2,2.14360556799999));
#308369=CARTESIAN_POINT('Ctrl Pts',(-3.93357615500006,5.2,2.14360556799999));
#308370=CARTESIAN_POINT('Ctrl Pts',(-3.93357615500006,2.2,2.14360556799999));
#308371=CARTESIAN_POINT('Ctrl Pts',(-3.93232829700006,12.2,2.14179029299999));
#308372=CARTESIAN_POINT('Ctrl Pts',(-3.93232829700006,5.2,2.14179029299999));
#308373=CARTESIAN_POINT('Ctrl Pts',(-3.93232829700006,2.2,2.14179029299999));
#308374=CARTESIAN_POINT('Ctrl Pts',(-3.93108064900006,12.2,2.13997954199999));
#308375=CARTESIAN_POINT('Ctrl Pts',(-3.93108064900006,5.2,2.13997954199999));
#308376=CARTESIAN_POINT('Ctrl Pts',(-3.93108064900006,2.2,2.13997954199999));
#308377=CARTESIAN_POINT('Ctrl Pts',(-3.92983322000005,12.2,2.13817331499999));
#308378=CARTESIAN_POINT('Ctrl Pts',(-3.92983322000005,5.2,2.13817331499999));
#308379=CARTESIAN_POINT('Ctrl Pts',(-3.92983322000005,2.2,2.13817331499999));
#308380=CARTESIAN_POINT('Ctrl Pts',(-3.92858602100006,12.2,2.13637161499999));
#308381=CARTESIAN_POINT('Ctrl Pts',(-3.92858602100006,5.2,2.13637161499999));
#308382=CARTESIAN_POINT('Ctrl Pts',(-3.92858602100006,2.2,2.13637161499999));
#308383=CARTESIAN_POINT('Ctrl Pts',(-3.92733906000006,12.2,2.13457443999999));
#308384=CARTESIAN_POINT('Ctrl Pts',(-3.92733906000006,5.2,2.13457443999999));
#308385=CARTESIAN_POINT('Ctrl Pts',(-3.92733906000006,2.2,2.13457443999999));
#308386=CARTESIAN_POINT('Ctrl Pts',(-3.92609234900006,12.2,2.13278179599998));
#308387=CARTESIAN_POINT('Ctrl Pts',(-3.92609234900006,5.2,2.13278179599998));
#308388=CARTESIAN_POINT('Ctrl Pts',(-3.92609234900006,2.2,2.13278179599998));
#308389=CARTESIAN_POINT('Ctrl Pts',(-3.92484589600006,12.2,2.13099368199998));
#308390=CARTESIAN_POINT('Ctrl Pts',(-3.92484589600006,5.2,2.13099368199998));
#308391=CARTESIAN_POINT('Ctrl Pts',(-3.92484589600006,2.2,2.13099368199998));
#308392=CARTESIAN_POINT('Ctrl Pts',(-3.92359971400006,12.2,2.12921009799999));
#308393=CARTESIAN_POINT('Ctrl Pts',(-3.92359971400006,5.2,2.12921009799999));
#308394=CARTESIAN_POINT('Ctrl Pts',(-3.92359971400006,2.2,2.12921009799999));
#308395=CARTESIAN_POINT('Ctrl Pts',(-3.92235381000006,12.2,2.12743104699999));
#308396=CARTESIAN_POINT('Ctrl Pts',(-3.92235381000006,5.2,2.12743104699999));
#308397=CARTESIAN_POINT('Ctrl Pts',(-3.92235381000006,2.2,2.12743104699999));
#308398=CARTESIAN_POINT('Ctrl Pts',(-3.92110819600005,12.2,2.12565653099999));
#308399=CARTESIAN_POINT('Ctrl Pts',(-3.92110819600005,5.2,2.12565653099999));
#308400=CARTESIAN_POINT('Ctrl Pts',(-3.92110819600005,2.2,2.12565653099999));
#308401=CARTESIAN_POINT('Ctrl Pts',(-3.91986288200005,12.2,2.12388654999998));
#308402=CARTESIAN_POINT('Ctrl Pts',(-3.91986288200005,5.2,2.12388654999998));
#308403=CARTESIAN_POINT('Ctrl Pts',(-3.91986288200005,2.2,2.12388654999998));
#308404=CARTESIAN_POINT('Ctrl Pts',(-3.91861787700006,12.2,2.12212110599999));
#308405=CARTESIAN_POINT('Ctrl Pts',(-3.91861787700006,5.2,2.12212110599999));
#308406=CARTESIAN_POINT('Ctrl Pts',(-3.91861787700006,2.2,2.12212110599999));
#308407=CARTESIAN_POINT('Ctrl Pts',(-3.91737319300006,12.2,2.12036019899998));
#308408=CARTESIAN_POINT('Ctrl Pts',(-3.91737319300006,5.2,2.12036019899998));
#308409=CARTESIAN_POINT('Ctrl Pts',(-3.91737319300006,2.2,2.12036019899998));
#308410=CARTESIAN_POINT('Ctrl Pts',(-3.91612883800006,12.2,2.11860383299999));
#308411=CARTESIAN_POINT('Ctrl Pts',(-3.91612883800006,5.2,2.11860383299999));
#308412=CARTESIAN_POINT('Ctrl Pts',(-3.91612883800006,2.2,2.11860383299999));
#308413=CARTESIAN_POINT('Ctrl Pts',(-3.91488482300006,12.2,2.11685200699999));
#308414=CARTESIAN_POINT('Ctrl Pts',(-3.91488482300006,5.2,2.11685200699999));
#308415=CARTESIAN_POINT('Ctrl Pts',(-3.91488482300006,2.2,2.11685200699999));
#308416=CARTESIAN_POINT('Ctrl Pts',(-3.91364116000006,12.2,2.11510472299999));
#308417=CARTESIAN_POINT('Ctrl Pts',(-3.91364116000006,5.2,2.11510472299999));
#308418=CARTESIAN_POINT('Ctrl Pts',(-3.91364116000006,2.2,2.11510472299999));
#308419=CARTESIAN_POINT('Ctrl Pts',(-3.91239785600006,12.2,2.11336198099998));
#308420=CARTESIAN_POINT('Ctrl Pts',(-3.91239785600006,5.2,2.11336198099998));
#308421=CARTESIAN_POINT('Ctrl Pts',(-3.91239785600006,2.2,2.11336198099998));
#308422=CARTESIAN_POINT('Ctrl Pts',(-3.91115492400006,12.2,2.11162378499999));
#308423=CARTESIAN_POINT('Ctrl Pts',(-3.91115492400006,5.2,2.11162378499999));
#308424=CARTESIAN_POINT('Ctrl Pts',(-3.91115492400006,2.2,2.11162378499999));
#308425=CARTESIAN_POINT('Ctrl Pts',(-3.90991237300006,12.2,2.10989013399999));
#308426=CARTESIAN_POINT('Ctrl Pts',(-3.90991237300006,5.2,2.10989013399999));
#308427=CARTESIAN_POINT('Ctrl Pts',(-3.90991237300006,2.2,2.10989013399999));
#308428=CARTESIAN_POINT('Ctrl Pts',(-3.90867021300005,12.2,2.10816102999999));
#308429=CARTESIAN_POINT('Ctrl Pts',(-3.90867021300005,5.2,2.10816102999999));
#308430=CARTESIAN_POINT('Ctrl Pts',(-3.90867021300005,2.2,2.10816102999999));
#308431=CARTESIAN_POINT('Ctrl Pts',(-3.90742845400006,12.2,2.10643647399999));
#308432=CARTESIAN_POINT('Ctrl Pts',(-3.90742845400006,5.2,2.10643647399999));
#308433=CARTESIAN_POINT('Ctrl Pts',(-3.90742845400006,2.2,2.10643647399999));
#308434=CARTESIAN_POINT('Ctrl Pts',(-3.90618710900006,12.2,2.10471646599999));
#308435=CARTESIAN_POINT('Ctrl Pts',(-3.90618710900006,5.2,2.10471646599999));
#308436=CARTESIAN_POINT('Ctrl Pts',(-3.90618710900006,2.2,2.10471646599999));
#308437=CARTESIAN_POINT('Ctrl Pts',(-3.90494618400006,12.2,2.10300100899998));
#308438=CARTESIAN_POINT('Ctrl Pts',(-3.90494618400006,5.2,2.10300100899998));
#308439=CARTESIAN_POINT('Ctrl Pts',(-3.90494618400006,2.2,2.10300100899998));
#308440=CARTESIAN_POINT('Ctrl Pts',(-3.90370569300006,12.2,2.10129010399998));
#308441=CARTESIAN_POINT('Ctrl Pts',(-3.90370569300006,5.2,2.10129010399998));
#308442=CARTESIAN_POINT('Ctrl Pts',(-3.90370569300006,2.2,2.10129010399998));
#308443=CARTESIAN_POINT('Ctrl Pts',(-3.90246564400006,12.2,2.09958375199998));
#308444=CARTESIAN_POINT('Ctrl Pts',(-3.90246564400006,5.2,2.09958375199998));
#308445=CARTESIAN_POINT('Ctrl Pts',(-3.90246564400006,2.2,2.09958375199998));
#308446=CARTESIAN_POINT('Ctrl Pts',(-3.90122604900006,12.2,2.09788195299998));
#308447=CARTESIAN_POINT('Ctrl Pts',(-3.90122604900006,5.2,2.09788195299998));
#308448=CARTESIAN_POINT('Ctrl Pts',(-3.90122604900006,2.2,2.09788195299998));
#308449=CARTESIAN_POINT('Ctrl Pts',(-3.89998691800006,12.2,2.09618470999999));
#308450=CARTESIAN_POINT('Ctrl Pts',(-3.89998691800006,5.2,2.09618470999999));
#308451=CARTESIAN_POINT('Ctrl Pts',(-3.89998691800006,2.2,2.09618470999999));
#308452=CARTESIAN_POINT('Ctrl Pts',(-3.89874826100006,12.2,2.09449202299998));
#308453=CARTESIAN_POINT('Ctrl Pts',(-3.89874826100006,5.2,2.09449202299998));
#308454=CARTESIAN_POINT('Ctrl Pts',(-3.89874826100006,2.2,2.09449202299998));
#308455=CARTESIAN_POINT('Ctrl Pts',(-3.89751008800006,12.2,2.09280389199999));
#308456=CARTESIAN_POINT('Ctrl Pts',(-3.89751008800006,5.2,2.09280389199999));
#308457=CARTESIAN_POINT('Ctrl Pts',(-3.89751008800006,2.2,2.09280389199999));
#308458=CARTESIAN_POINT('Ctrl Pts',(-3.89627241100006,12.2,2.09112031999998));
#308459=CARTESIAN_POINT('Ctrl Pts',(-3.89627241100006,5.2,2.09112031999998));
#308460=CARTESIAN_POINT('Ctrl Pts',(-3.89627241100006,2.2,2.09112031999998));
#308461=CARTESIAN_POINT('Ctrl Pts',(-3.89503523800006,12.2,2.08944130799999));
#308462=CARTESIAN_POINT('Ctrl Pts',(-3.89503523800006,5.2,2.08944130799999));
#308463=CARTESIAN_POINT('Ctrl Pts',(-3.89503523800006,2.2,2.08944130799999));
#308464=CARTESIAN_POINT('Ctrl Pts',(-3.89379858200006,12.2,2.08776685599998));
#308465=CARTESIAN_POINT('Ctrl Pts',(-3.89379858200006,5.2,2.08776685599998));
#308466=CARTESIAN_POINT('Ctrl Pts',(-3.89379858200006,2.2,2.08776685599998));
#308467=CARTESIAN_POINT('Ctrl Pts',(-3.89256245200006,12.2,2.08609696499999));
#308468=CARTESIAN_POINT('Ctrl Pts',(-3.89256245200006,5.2,2.08609696499999));
#308469=CARTESIAN_POINT('Ctrl Pts',(-3.89256245200006,2.2,2.08609696499999));
#308470=CARTESIAN_POINT('Ctrl Pts',(-3.89132685900006,12.2,2.08443163799998));
#308471=CARTESIAN_POINT('Ctrl Pts',(-3.89132685900006,5.2,2.08443163799998));
#308472=CARTESIAN_POINT('Ctrl Pts',(-3.89132685900006,2.2,2.08443163799998));
#308473=CARTESIAN_POINT('Ctrl Pts',(-3.89009181400006,12.2,2.08277087299999));
#308474=CARTESIAN_POINT('Ctrl Pts',(-3.89009181400006,5.2,2.08277087299999));
#308475=CARTESIAN_POINT('Ctrl Pts',(-3.89009181400006,2.2,2.08277087299999));
#308476=CARTESIAN_POINT('Ctrl Pts',(-3.88885732600006,12.2,2.08111467299998));
#308477=CARTESIAN_POINT('Ctrl Pts',(-3.88885732600006,5.2,2.08111467299998));
#308478=CARTESIAN_POINT('Ctrl Pts',(-3.88885732600006,2.2,2.08111467299998));
#308479=CARTESIAN_POINT('Ctrl Pts',(-3.88762340700006,12.2,2.07946303899998));
#308480=CARTESIAN_POINT('Ctrl Pts',(-3.88762340700006,5.2,2.07946303899998));
#308481=CARTESIAN_POINT('Ctrl Pts',(-3.88762340700006,2.2,2.07946303899998));
#308482=CARTESIAN_POINT('Ctrl Pts',(-3.88639006700005,12.2,2.07781597099999));
#308483=CARTESIAN_POINT('Ctrl Pts',(-3.88639006700005,5.2,2.07781597099999));
#308484=CARTESIAN_POINT('Ctrl Pts',(-3.88639006700005,2.2,2.07781597099999));
#308485=CARTESIAN_POINT('Ctrl Pts',(-3.88515731700006,12.2,2.07617347099998));
#308486=CARTESIAN_POINT('Ctrl Pts',(-3.88515731700006,5.2,2.07617347099998));
#308487=CARTESIAN_POINT('Ctrl Pts',(-3.88515731700006,2.2,2.07617347099998));
#308488=CARTESIAN_POINT('Ctrl Pts',(-3.88392516600006,12.2,2.07453553899999));
#308489=CARTESIAN_POINT('Ctrl Pts',(-3.88392516600006,5.2,2.07453553899999));
#308490=CARTESIAN_POINT('Ctrl Pts',(-3.88392516600006,2.2,2.07453553899999));
#308491=CARTESIAN_POINT('Ctrl Pts',(-3.88269362800005,12.2,2.07290217699999));
#308492=CARTESIAN_POINT('Ctrl Pts',(-3.88269362800005,5.2,2.07290217699999));
#308493=CARTESIAN_POINT('Ctrl Pts',(-3.88269362800005,2.2,2.07290217699999));
#308494=CARTESIAN_POINT('Ctrl Pts',(-3.88146271000006,12.2,2.07127338399999));
#308495=CARTESIAN_POINT('Ctrl Pts',(-3.88146271000006,5.2,2.07127338399999));
#308496=CARTESIAN_POINT('Ctrl Pts',(-3.88146271000006,2.2,2.07127338399999));
#308497=CARTESIAN_POINT('Ctrl Pts',(-3.88023242500006,12.2,2.06964916399999));
#308498=CARTESIAN_POINT('Ctrl Pts',(-3.88023242500006,5.2,2.06964916399999));
#308499=CARTESIAN_POINT('Ctrl Pts',(-3.88023242500006,2.2,2.06964916399999));
#308500=CARTESIAN_POINT('Ctrl Pts',(-3.87900278300005,12.2,2.06802951599999));
#308501=CARTESIAN_POINT('Ctrl Pts',(-3.87900278300005,5.2,2.06802951599999));
#308502=CARTESIAN_POINT('Ctrl Pts',(-3.87900278300005,2.2,2.06802951599999));
#308503=CARTESIAN_POINT('Ctrl Pts',(-3.87777379500006,12.2,2.06641444099999));
#308504=CARTESIAN_POINT('Ctrl Pts',(-3.87777379500006,5.2,2.06641444099999));
#308505=CARTESIAN_POINT('Ctrl Pts',(-3.87777379500006,2.2,2.06641444099999));
#308506=CARTESIAN_POINT('Ctrl Pts',(-3.87654547000006,12.2,2.06480393899998));
#308507=CARTESIAN_POINT('Ctrl Pts',(-3.87654547000006,5.2,2.06480393899998));
#308508=CARTESIAN_POINT('Ctrl Pts',(-3.87654547000006,2.2,2.06480393899998));
#308509=CARTESIAN_POINT('Ctrl Pts',(-3.87531782100006,12.2,2.06319801299998));
#308510=CARTESIAN_POINT('Ctrl Pts',(-3.87531782100006,5.2,2.06319801299998));
#308511=CARTESIAN_POINT('Ctrl Pts',(-3.87531782100006,2.2,2.06319801299998));
#308512=CARTESIAN_POINT('Ctrl Pts',(-3.87409085900006,12.2,2.06159666199999));
#308513=CARTESIAN_POINT('Ctrl Pts',(-3.87409085900006,5.2,2.06159666199999));
#308514=CARTESIAN_POINT('Ctrl Pts',(-3.87409085900006,2.2,2.06159666199999));
#308515=CARTESIAN_POINT('Ctrl Pts',(-3.87286459200006,12.2,2.05999988799999));
#308516=CARTESIAN_POINT('Ctrl Pts',(-3.87286459200006,5.2,2.05999988799999));
#308517=CARTESIAN_POINT('Ctrl Pts',(-3.87286459200006,2.2,2.05999988799999));
#308518=CARTESIAN_POINT('Ctrl Pts',(-3.87163903300006,12.2,2.05840769199999));
#308519=CARTESIAN_POINT('Ctrl Pts',(-3.87163903300006,5.2,2.05840769199999));
#308520=CARTESIAN_POINT('Ctrl Pts',(-3.87163903300006,2.2,2.05840769199999));
#308521=CARTESIAN_POINT('Ctrl Pts',(-3.87041419300005,12.2,2.05682007299998));
#308522=CARTESIAN_POINT('Ctrl Pts',(-3.87041419300005,5.2,2.05682007299998));
#308523=CARTESIAN_POINT('Ctrl Pts',(-3.87041419300005,2.2,2.05682007299998));
#308524=CARTESIAN_POINT('Ctrl Pts',(-3.86919008000006,12.2,2.05523703399999));
#308525=CARTESIAN_POINT('Ctrl Pts',(-3.86919008000006,5.2,2.05523703399999));
#308526=CARTESIAN_POINT('Ctrl Pts',(-3.86919008000006,2.2,2.05523703399999));
#308527=CARTESIAN_POINT('Ctrl Pts',(-3.86796670900006,12.2,2.05365857399999));
#308528=CARTESIAN_POINT('Ctrl Pts',(-3.86796670900006,5.2,2.05365857399999));
#308529=CARTESIAN_POINT('Ctrl Pts',(-3.86796670900006,2.2,2.05365857399999));
#308530=CARTESIAN_POINT('Ctrl Pts',(-3.86674408800006,12.2,2.05208469499999));
#308531=CARTESIAN_POINT('Ctrl Pts',(-3.86674408800006,5.2,2.05208469499999));
#308532=CARTESIAN_POINT('Ctrl Pts',(-3.86674408800006,2.2,2.05208469499999));
#308533=CARTESIAN_POINT('Ctrl Pts',(-3.86552222900006,12.2,2.05051539699999));
#308534=CARTESIAN_POINT('Ctrl Pts',(-3.86552222900006,5.2,2.05051539699999));
#308535=CARTESIAN_POINT('Ctrl Pts',(-3.86552222900006,2.2,2.05051539699999));
#308536=CARTESIAN_POINT('Ctrl Pts',(-3.86430114200006,12.2,2.04895068199999));
#308537=CARTESIAN_POINT('Ctrl Pts',(-3.86430114200006,5.2,2.04895068199999));
#308538=CARTESIAN_POINT('Ctrl Pts',(-3.86430114200006,2.2,2.04895068199999));
#308539=CARTESIAN_POINT('Ctrl Pts',(-3.86308083900006,12.2,2.04739054899999));
#308540=CARTESIAN_POINT('Ctrl Pts',(-3.86308083900006,5.2,2.04739054899999));
#308541=CARTESIAN_POINT('Ctrl Pts',(-3.86308083900006,2.2,2.04739054899999));
#308542=CARTESIAN_POINT('Ctrl Pts',(-3.86186133000006,12.2,2.04583499999998));
#308543=CARTESIAN_POINT('Ctrl Pts',(-3.86186133000006,5.2,2.04583499999998));
#308544=CARTESIAN_POINT('Ctrl Pts',(-3.86186133000006,2.2,2.04583499999998));
#308545=CARTESIAN_POINT('Ctrl Pts',(-3.86064262700006,12.2,2.04428403499998));
#308546=CARTESIAN_POINT('Ctrl Pts',(-3.86064262700006,5.2,2.04428403499998));
#308547=CARTESIAN_POINT('Ctrl Pts',(-3.86064262700006,2.2,2.04428403499998));
#308548=CARTESIAN_POINT('Ctrl Pts',(-3.85942474000006,12.2,2.04273765499998));
#308549=CARTESIAN_POINT('Ctrl Pts',(-3.85942474000006,5.2,2.04273765499998));
#308550=CARTESIAN_POINT('Ctrl Pts',(-3.85942474000006,2.2,2.04273765499998));
#308551=CARTESIAN_POINT('Ctrl Pts',(-3.85820768000006,12.2,2.04119585999999));
#308552=CARTESIAN_POINT('Ctrl Pts',(-3.85820768000006,5.2,2.04119585999999));
#308553=CARTESIAN_POINT('Ctrl Pts',(-3.85820768000006,2.2,2.04119585999999));
#308554=CARTESIAN_POINT('Ctrl Pts',(-3.85699145900006,12.2,2.03965865299998));
#308555=CARTESIAN_POINT('Ctrl Pts',(-3.85699145900006,5.2,2.03965865299998));
#308556=CARTESIAN_POINT('Ctrl Pts',(-3.85699145900006,2.2,2.03965865299998));
#308557=CARTESIAN_POINT('Ctrl Pts',(-3.85577608800006,12.2,2.03812603199998));
#308558=CARTESIAN_POINT('Ctrl Pts',(-3.85577608800006,5.2,2.03812603199998));
#308559=CARTESIAN_POINT('Ctrl Pts',(-3.85577608800006,2.2,2.03812603199998));
#308560=CARTESIAN_POINT('Ctrl Pts',(-3.85456157700006,12.2,2.03659799799999));
#308561=CARTESIAN_POINT('Ctrl Pts',(-3.85456157700006,5.2,2.03659799799999));
#308562=CARTESIAN_POINT('Ctrl Pts',(-3.85456157700006,2.2,2.03659799799999));
#308563=CARTESIAN_POINT('Ctrl Pts',(-3.85334793700006,12.2,2.03507455299999));
#308564=CARTESIAN_POINT('Ctrl Pts',(-3.85334793700006,5.2,2.03507455299999));
#308565=CARTESIAN_POINT('Ctrl Pts',(-3.85334793700006,2.2,2.03507455299999));
#308566=CARTESIAN_POINT('Ctrl Pts',(-3.85213518000006,12.2,2.03355569699998));
#308567=CARTESIAN_POINT('Ctrl Pts',(-3.85213518000006,5.2,2.03355569699998));
#308568=CARTESIAN_POINT('Ctrl Pts',(-3.85213518000006,2.2,2.03355569699998));
#308569=CARTESIAN_POINT('Ctrl Pts',(-3.85092331700006,12.2,2.03204142899999));
#308570=CARTESIAN_POINT('Ctrl Pts',(-3.85092331700006,5.2,2.03204142899999));
#308571=CARTESIAN_POINT('Ctrl Pts',(-3.85092331700006,2.2,2.03204142899999));
#308572=CARTESIAN_POINT('Ctrl Pts',(-3.84971235800006,12.2,2.03053175199999));
#308573=CARTESIAN_POINT('Ctrl Pts',(-3.84971235800006,5.2,2.03053175199999));
#308574=CARTESIAN_POINT('Ctrl Pts',(-3.84971235800006,2.2,2.03053175199999));
#308575=CARTESIAN_POINT('Ctrl Pts',(-3.84850231600006,12.2,2.02902666499998));
#308576=CARTESIAN_POINT('Ctrl Pts',(-3.84850231600006,5.2,2.02902666499998));
#308577=CARTESIAN_POINT('Ctrl Pts',(-3.84850231600006,2.2,2.02902666499998));
#308578=CARTESIAN_POINT('Ctrl Pts',(-3.84729320100006,12.2,2.02752616999998));
#308579=CARTESIAN_POINT('Ctrl Pts',(-3.84729320100006,5.2,2.02752616999998));
#308580=CARTESIAN_POINT('Ctrl Pts',(-3.84729320100006,2.2,2.02752616999998));
#308581=CARTESIAN_POINT('Ctrl Pts',(-3.84608502400006,12.2,2.02603026699999));
#308582=CARTESIAN_POINT('Ctrl Pts',(-3.84608502400006,5.2,2.02603026699999));
#308583=CARTESIAN_POINT('Ctrl Pts',(-3.84608502400006,2.2,2.02603026699999));
#308584=CARTESIAN_POINT('Ctrl Pts',(-3.84487779800006,12.2,2.02453895399998));
#308585=CARTESIAN_POINT('Ctrl Pts',(-3.84487779800006,5.2,2.02453895399998));
#308586=CARTESIAN_POINT('Ctrl Pts',(-3.84487779800006,2.2,2.02453895399998));
#308587=CARTESIAN_POINT('Ctrl Pts',(-3.84367153100006,12.2,2.02305223599998));
#308588=CARTESIAN_POINT('Ctrl Pts',(-3.84367153100006,5.2,2.02305223599998));
#308589=CARTESIAN_POINT('Ctrl Pts',(-3.84367153100006,2.2,2.02305223599998));
#308590=CARTESIAN_POINT('Ctrl Pts',(-3.84246623700006,12.2,2.02157010999999));
#308591=CARTESIAN_POINT('Ctrl Pts',(-3.84246623700006,5.2,2.02157010999999));
#308592=CARTESIAN_POINT('Ctrl Pts',(-3.84246623700006,2.2,2.02157010999999));
#308593=CARTESIAN_POINT('Ctrl Pts',(-3.84126192700006,12.2,2.02009257799999));
#308594=CARTESIAN_POINT('Ctrl Pts',(-3.84126192700006,5.2,2.02009257799999));
#308595=CARTESIAN_POINT('Ctrl Pts',(-3.84126192700006,2.2,2.02009257799999));
#308596=CARTESIAN_POINT('Ctrl Pts',(-3.84005861100006,12.2,2.01861963999999));
#308597=CARTESIAN_POINT('Ctrl Pts',(-3.84005861100006,5.2,2.01861963999999));
#308598=CARTESIAN_POINT('Ctrl Pts',(-3.84005861100006,2.2,2.01861963999999));
#308599=CARTESIAN_POINT('Ctrl Pts',(-3.83885630100006,12.2,2.01715129799998));
#308600=CARTESIAN_POINT('Ctrl Pts',(-3.83885630100006,5.2,2.01715129799998));
#308601=CARTESIAN_POINT('Ctrl Pts',(-3.83885630100006,2.2,2.01715129799998));
#308602=CARTESIAN_POINT('Ctrl Pts',(-3.83765500700005,12.2,2.01568754899998));
#308603=CARTESIAN_POINT('Ctrl Pts',(-3.83765500700005,5.2,2.01568754899998));
#308604=CARTESIAN_POINT('Ctrl Pts',(-3.83765500700005,2.2,2.01568754899998));
#308605=CARTESIAN_POINT('Ctrl Pts',(-3.83645474300006,12.2,2.01422839599998));
#308606=CARTESIAN_POINT('Ctrl Pts',(-3.83645474300006,5.2,2.01422839599998));
#308607=CARTESIAN_POINT('Ctrl Pts',(-3.83645474300006,2.2,2.01422839599998));
#308608=CARTESIAN_POINT('Ctrl Pts',(-3.83525551800005,12.2,2.01277383899999));
#308609=CARTESIAN_POINT('Ctrl Pts',(-3.83525551800005,5.2,2.01277383899999));
#308610=CARTESIAN_POINT('Ctrl Pts',(-3.83525551800005,2.2,2.01277383899999));
#308611=CARTESIAN_POINT('Ctrl Pts',(-3.83405734600006,12.2,2.01132387799999));
#308612=CARTESIAN_POINT('Ctrl Pts',(-3.83405734600006,5.2,2.01132387799999));
#308613=CARTESIAN_POINT('Ctrl Pts',(-3.83405734600006,2.2,2.01132387799999));
#308614=CARTESIAN_POINT('Ctrl Pts',(-3.83286023400006,12.2,2.00987851499999));
#308615=CARTESIAN_POINT('Ctrl Pts',(-3.83286023400006,5.2,2.00987851499999));
#308616=CARTESIAN_POINT('Ctrl Pts',(-3.83286023400006,2.2,2.00987851499999));
#308617=CARTESIAN_POINT('Ctrl Pts',(-3.83166419800006,12.2,2.00843774699999));
#308618=CARTESIAN_POINT('Ctrl Pts',(-3.83166419800006,5.2,2.00843774699999));
#308619=CARTESIAN_POINT('Ctrl Pts',(-3.83166419800006,2.2,2.00843774699999));
#308620=CARTESIAN_POINT('Ctrl Pts',(-3.83046924700006,12.2,2.00700157699998));
#308621=CARTESIAN_POINT('Ctrl Pts',(-3.83046924700006,5.2,2.00700157699998));
#308622=CARTESIAN_POINT('Ctrl Pts',(-3.83046924700006,2.2,2.00700157699998));
#308623=CARTESIAN_POINT('Ctrl Pts',(-3.82927539400006,12.2,2.00557000499999));
#308624=CARTESIAN_POINT('Ctrl Pts',(-3.82927539400006,5.2,2.00557000499999));
#308625=CARTESIAN_POINT('Ctrl Pts',(-3.82927539400006,2.2,2.00557000499999));
#308626=CARTESIAN_POINT('Ctrl Pts',(-3.82808264900006,12.2,2.00414303099999));
#308627=CARTESIAN_POINT('Ctrl Pts',(-3.82808264900006,5.2,2.00414303099999));
#308628=CARTESIAN_POINT('Ctrl Pts',(-3.82808264900006,2.2,2.00414303099999));
#308629=CARTESIAN_POINT('Ctrl Pts',(-3.82689102400006,12.2,2.00272065499998));
#308630=CARTESIAN_POINT('Ctrl Pts',(-3.82689102400006,5.2,2.00272065499998));
#308631=CARTESIAN_POINT('Ctrl Pts',(-3.82689102400006,2.2,2.00272065499998));
#308632=CARTESIAN_POINT('Ctrl Pts',(-3.82570053100006,12.2,2.00130287699999));
#308633=CARTESIAN_POINT('Ctrl Pts',(-3.82570053100006,5.2,2.00130287699999));
#308634=CARTESIAN_POINT('Ctrl Pts',(-3.82570053100006,2.2,2.00130287699999));
#308635=CARTESIAN_POINT('Ctrl Pts',(-3.82451118100006,12.2,1.99988969899998));
#308636=CARTESIAN_POINT('Ctrl Pts',(-3.82451118100006,5.2,1.99988969899998));
#308637=CARTESIAN_POINT('Ctrl Pts',(-3.82451118100006,2.2,1.99988969899998));
#308638=CARTESIAN_POINT('Ctrl Pts',(-3.82332298400006,12.2,1.99848111899998));
#308639=CARTESIAN_POINT('Ctrl Pts',(-3.82332298400006,5.2,1.99848111899998));
#308640=CARTESIAN_POINT('Ctrl Pts',(-3.82332298400006,2.2,1.99848111899998));
#308641=CARTESIAN_POINT('Ctrl Pts',(-3.82213595500006,12.2,1.99707713899999));
#308642=CARTESIAN_POINT('Ctrl Pts',(-3.82213595500006,5.2,1.99707713899999));
#308643=CARTESIAN_POINT('Ctrl Pts',(-3.82213595500006,2.2,1.99707713899999));
#308644=CARTESIAN_POINT('Ctrl Pts',(-3.82095010300006,12.2,1.99567775799999));
#308645=CARTESIAN_POINT('Ctrl Pts',(-3.82095010300006,5.2,1.99567775799999));
#308646=CARTESIAN_POINT('Ctrl Pts',(-3.82095010300006,2.2,1.99567775799999));
#308647=CARTESIAN_POINT('Ctrl Pts',(-3.81976544100006,12.2,1.99428297799999));
#308648=CARTESIAN_POINT('Ctrl Pts',(-3.81976544100006,5.2,1.99428297799999));
#308649=CARTESIAN_POINT('Ctrl Pts',(-3.81976544100006,2.2,1.99428297799999));
#308650=CARTESIAN_POINT('Ctrl Pts',(-3.81858197900006,12.2,1.99289279599999));
#308651=CARTESIAN_POINT('Ctrl Pts',(-3.81858197900006,5.2,1.99289279599999));
#308652=CARTESIAN_POINT('Ctrl Pts',(-3.81858197900006,2.2,1.99289279599999));
#308653=CARTESIAN_POINT('Ctrl Pts',(-3.81739973200006,12.2,1.99150721599999));
#308654=CARTESIAN_POINT('Ctrl Pts',(-3.81739973200006,5.2,1.99150721599999));
#308655=CARTESIAN_POINT('Ctrl Pts',(-3.81739973200006,2.2,1.99150721599999));
#308656=CARTESIAN_POINT('Ctrl Pts',(-3.81621870800006,12.2,1.99012623499998));
#308657=CARTESIAN_POINT('Ctrl Pts',(-3.81621870800006,5.2,1.99012623499998));
#308658=CARTESIAN_POINT('Ctrl Pts',(-3.81621870800006,2.2,1.99012623499998));
#308659=CARTESIAN_POINT('Ctrl Pts',(-3.81503891900006,12.2,1.98874985499998));
#308660=CARTESIAN_POINT('Ctrl Pts',(-3.81503891900006,5.2,1.98874985499998));
#308661=CARTESIAN_POINT('Ctrl Pts',(-3.81503891900006,2.2,1.98874985499998));
#308662=CARTESIAN_POINT('Ctrl Pts',(-3.81386038000006,12.2,1.98737807599999));
#308663=CARTESIAN_POINT('Ctrl Pts',(-3.81386038000006,5.2,1.98737807599999));
#308664=CARTESIAN_POINT('Ctrl Pts',(-3.81386038000006,2.2,1.98737807599999));
#308665=CARTESIAN_POINT('Ctrl Pts',(-3.81268309900006,12.2,1.98601089699999));
#308666=CARTESIAN_POINT('Ctrl Pts',(-3.81268309900006,5.2,1.98601089699999));
#308667=CARTESIAN_POINT('Ctrl Pts',(-3.81268309900006,2.2,1.98601089699999));
#308668=CARTESIAN_POINT('Ctrl Pts',(-3.81150709100006,12.2,1.98464831899999));
#308669=CARTESIAN_POINT('Ctrl Pts',(-3.81150709100006,5.2,1.98464831899999));
#308670=CARTESIAN_POINT('Ctrl Pts',(-3.81150709100006,2.2,1.98464831899999));
#308671=CARTESIAN_POINT('Ctrl Pts',(-3.81033236500006,12.2,1.98329034199999));
#308672=CARTESIAN_POINT('Ctrl Pts',(-3.81033236500006,5.2,1.98329034199999));
#308673=CARTESIAN_POINT('Ctrl Pts',(-3.81033236500006,2.2,1.98329034199999));
#308674=CARTESIAN_POINT('Ctrl Pts',(-3.80915893500006,12.2,1.98193696599999));
#308675=CARTESIAN_POINT('Ctrl Pts',(-3.80915893500006,5.2,1.98193696599999));
#308676=CARTESIAN_POINT('Ctrl Pts',(-3.80915893500006,2.2,1.98193696599999));
#308677=CARTESIAN_POINT('Ctrl Pts',(-3.80798681000006,12.2,1.98058818999999));
#308678=CARTESIAN_POINT('Ctrl Pts',(-3.80798681000006,5.2,1.98058818999999));
#308679=CARTESIAN_POINT('Ctrl Pts',(-3.80798681000006,2.2,1.98058818999999));
#308680=CARTESIAN_POINT('Ctrl Pts',(-3.80681600500006,12.2,1.97924401599999));
#308681=CARTESIAN_POINT('Ctrl Pts',(-3.80681600500006,5.2,1.97924401599999));
#308682=CARTESIAN_POINT('Ctrl Pts',(-3.80681600500006,2.2,1.97924401599999));
#308683=CARTESIAN_POINT('Ctrl Pts',(-3.80564653100006,12.2,1.97790444299998));
#308684=CARTESIAN_POINT('Ctrl Pts',(-3.80564653100006,5.2,1.97790444299998));
#308685=CARTESIAN_POINT('Ctrl Pts',(-3.80564653100006,2.2,1.97790444299998));
#308686=CARTESIAN_POINT('Ctrl Pts',(-3.80447839700006,12.2,1.97656947099999));
#308687=CARTESIAN_POINT('Ctrl Pts',(-3.80447839700006,5.2,1.97656947099999));
#308688=CARTESIAN_POINT('Ctrl Pts',(-3.80447839700006,2.2,1.97656947099999));
#308689=CARTESIAN_POINT('Ctrl Pts',(-3.80331162000005,12.2,1.97523910099999));
#308690=CARTESIAN_POINT('Ctrl Pts',(-3.80331162000005,5.2,1.97523910099999));
#308691=CARTESIAN_POINT('Ctrl Pts',(-3.80331162000005,2.2,1.97523910099999));
#308692=CARTESIAN_POINT('Ctrl Pts',(-3.80214620800006,12.2,1.97391332999999));
#308693=CARTESIAN_POINT('Ctrl Pts',(-3.80214620800006,5.2,1.97391332999999));
#308694=CARTESIAN_POINT('Ctrl Pts',(-3.80214620800006,2.2,1.97391332999999));
#308695=CARTESIAN_POINT('Ctrl Pts',(-3.80098217400006,12.2,1.97259216199999));
#308696=CARTESIAN_POINT('Ctrl Pts',(-3.80098217400006,5.2,1.97259216199999));
#308697=CARTESIAN_POINT('Ctrl Pts',(-3.80098217400006,2.2,1.97259216199999));
#308698=CARTESIAN_POINT('Ctrl Pts',(-3.79981953100006,12.2,1.97127559299998));
#308699=CARTESIAN_POINT('Ctrl Pts',(-3.79981953100006,5.2,1.97127559299998));
#308700=CARTESIAN_POINT('Ctrl Pts',(-3.79981953100006,2.2,1.97127559299998));
#308701=CARTESIAN_POINT('Ctrl Pts',(-3.79865829000006,12.2,1.96996362599998));
#308702=CARTESIAN_POINT('Ctrl Pts',(-3.79865829000006,5.2,1.96996362599998));
#308703=CARTESIAN_POINT('Ctrl Pts',(-3.79865829000006,2.2,1.96996362599998));
#308704=CARTESIAN_POINT('Ctrl Pts',(-3.79749846300006,12.2,1.96865625899999));
#308705=CARTESIAN_POINT('Ctrl Pts',(-3.79749846300006,5.2,1.96865625899999));
#308706=CARTESIAN_POINT('Ctrl Pts',(-3.79749846300006,2.2,1.96865625899999));
#308707=CARTESIAN_POINT('Ctrl Pts',(-3.79634006200006,12.2,1.96735349499999));
#308708=CARTESIAN_POINT('Ctrl Pts',(-3.79634006200006,5.2,1.96735349499999));
#308709=CARTESIAN_POINT('Ctrl Pts',(-3.79634006200006,2.2,1.96735349499999));
#308710=CARTESIAN_POINT('Ctrl Pts',(-3.79518310000006,12.2,1.96605532899999));
#308711=CARTESIAN_POINT('Ctrl Pts',(-3.79518310000006,5.2,1.96605532899999));
#308712=CARTESIAN_POINT('Ctrl Pts',(-3.79518310000006,2.2,1.96605532899999));
#308713=CARTESIAN_POINT('Ctrl Pts',(-3.79402758800006,12.2,1.96476176399999));
#308714=CARTESIAN_POINT('Ctrl Pts',(-3.79402758800006,5.2,1.96476176399999));
#308715=CARTESIAN_POINT('Ctrl Pts',(-3.79402758800006,2.2,1.96476176399999));
#308716=CARTESIAN_POINT('Ctrl Pts',(-3.79287353800006,12.2,1.96347279899999));
#308717=CARTESIAN_POINT('Ctrl Pts',(-3.79287353800006,5.2,1.96347279899999));
#308718=CARTESIAN_POINT('Ctrl Pts',(-3.79287353800006,2.2,1.96347279899999));
#308719=CARTESIAN_POINT('Ctrl Pts',(-3.79172096300006,12.2,1.96218843399999));
#308720=CARTESIAN_POINT('Ctrl Pts',(-3.79172096300006,5.2,1.96218843399999));
#308721=CARTESIAN_POINT('Ctrl Pts',(-3.79172096300006,2.2,1.96218843399999));
#308722=CARTESIAN_POINT('Ctrl Pts',(-3.79056987400006,12.2,1.96090866999999));
#308723=CARTESIAN_POINT('Ctrl Pts',(-3.79056987400006,5.2,1.96090866999999));
#308724=CARTESIAN_POINT('Ctrl Pts',(-3.79056987400006,2.2,1.96090866999999));
#308725=CARTESIAN_POINT('Ctrl Pts',(-3.78942028500005,12.2,1.95963350399999));
#308726=CARTESIAN_POINT('Ctrl Pts',(-3.78942028500005,5.2,1.95963350399999));
#308727=CARTESIAN_POINT('Ctrl Pts',(-3.78942028500005,2.2,1.95963350399999));
#308728=CARTESIAN_POINT('Ctrl Pts',(-3.78827220700006,12.2,1.95836293899998));
#308729=CARTESIAN_POINT('Ctrl Pts',(-3.78827220700006,5.2,1.95836293899998));
#308730=CARTESIAN_POINT('Ctrl Pts',(-3.78827220700006,2.2,1.95836293899998));
#308731=CARTESIAN_POINT('Ctrl Pts',(-3.78712565200006,12.2,1.95709697199999));
#308732=CARTESIAN_POINT('Ctrl Pts',(-3.78712565200006,5.2,1.95709697199999));
#308733=CARTESIAN_POINT('Ctrl Pts',(-3.78712565200006,2.2,1.95709697199999));
#308734=CARTESIAN_POINT('Ctrl Pts',(-3.78598063200006,12.2,1.95583560399998));
#308735=CARTESIAN_POINT('Ctrl Pts',(-3.78598063200006,5.2,1.95583560399998));
#308736=CARTESIAN_POINT('Ctrl Pts',(-3.78598063200006,2.2,1.95583560399998));
#308737=CARTESIAN_POINT('Ctrl Pts',(-3.78483716200006,12.2,1.95457883599999));
#308738=CARTESIAN_POINT('Ctrl Pts',(-3.78483716200006,5.2,1.95457883599999));
#308739=CARTESIAN_POINT('Ctrl Pts',(-3.78483716200006,2.2,1.95457883599999));
#308740=CARTESIAN_POINT('Ctrl Pts',(-3.78369525000006,12.2,1.95332666499999));
#308741=CARTESIAN_POINT('Ctrl Pts',(-3.78369525000006,5.2,1.95332666499999));
#308742=CARTESIAN_POINT('Ctrl Pts',(-3.78369525000006,2.2,1.95332666499999));
#308743=CARTESIAN_POINT('Ctrl Pts',(-3.78255491200005,12.2,1.95207909299999));
#308744=CARTESIAN_POINT('Ctrl Pts',(-3.78255491200005,5.2,1.95207909299999));
#308745=CARTESIAN_POINT('Ctrl Pts',(-3.78255491200005,2.2,1.95207909299999));
#308746=CARTESIAN_POINT('Ctrl Pts',(-3.78141615700006,12.2,1.95083611699999));
#308747=CARTESIAN_POINT('Ctrl Pts',(-3.78141615700006,5.2,1.95083611699999));
#308748=CARTESIAN_POINT('Ctrl Pts',(-3.78141615700006,2.2,1.95083611699999));
#308749=CARTESIAN_POINT('Ctrl Pts',(-3.78027899900006,12.2,1.94959773899999));
#308750=CARTESIAN_POINT('Ctrl Pts',(-3.78027899900006,5.2,1.94959773899999));
#308751=CARTESIAN_POINT('Ctrl Pts',(-3.78027899900006,2.2,1.94959773899999));
#308752=CARTESIAN_POINT('Ctrl Pts',(-3.77914345200006,12.2,1.94836395899999));
#308753=CARTESIAN_POINT('Ctrl Pts',(-3.77914345200006,5.2,1.94836395899999));
#308754=CARTESIAN_POINT('Ctrl Pts',(-3.77914345200006,2.2,1.94836395899999));
#308755=CARTESIAN_POINT('Ctrl Pts',(-3.77800952600006,12.2,1.94713477499999));
#308756=CARTESIAN_POINT('Ctrl Pts',(-3.77800952600006,5.2,1.94713477499999));
#308757=CARTESIAN_POINT('Ctrl Pts',(-3.77800952600006,2.2,1.94713477499999));
#308758=CARTESIAN_POINT('Ctrl Pts',(-3.77687723500006,12.2,1.94591018699999));
#308759=CARTESIAN_POINT('Ctrl Pts',(-3.77687723500006,5.2,1.94591018699999));
#308760=CARTESIAN_POINT('Ctrl Pts',(-3.77687723500006,2.2,1.94591018699999));
#308761=CARTESIAN_POINT('Ctrl Pts',(-3.77574659000006,12.2,1.94469019499998));
#308762=CARTESIAN_POINT('Ctrl Pts',(-3.77574659000006,5.2,1.94469019499998));
#308763=CARTESIAN_POINT('Ctrl Pts',(-3.77574659000006,2.2,1.94469019499998));
#308764=CARTESIAN_POINT('Ctrl Pts',(-3.77461760400006,12.2,1.94347479799998));
#308765=CARTESIAN_POINT('Ctrl Pts',(-3.77461760400006,5.2,1.94347479799998));
#308766=CARTESIAN_POINT('Ctrl Pts',(-3.77461760400006,2.2,1.94347479799998));
#308767=CARTESIAN_POINT('Ctrl Pts',(-3.77349028900006,12.2,1.94226399599998));
#308768=CARTESIAN_POINT('Ctrl Pts',(-3.77349028900006,5.2,1.94226399599998));
#308769=CARTESIAN_POINT('Ctrl Pts',(-3.77349028900006,2.2,1.94226399599998));
#308770=CARTESIAN_POINT('Ctrl Pts',(-3.77236465900006,12.2,1.94105778899999));
#308771=CARTESIAN_POINT('Ctrl Pts',(-3.77236465900006,5.2,1.94105778899999));
#308772=CARTESIAN_POINT('Ctrl Pts',(-3.77236465900006,2.2,1.94105778899999));
#308773=CARTESIAN_POINT('Ctrl Pts',(-3.77124072700005,12.2,1.93985617599999));
#308774=CARTESIAN_POINT('Ctrl Pts',(-3.77124072700005,5.2,1.93985617599999));
#308775=CARTESIAN_POINT('Ctrl Pts',(-3.77124072700005,2.2,1.93985617599999));
#308776=CARTESIAN_POINT('Ctrl Pts',(-3.77011850300006,12.2,1.93865915599998));
#308777=CARTESIAN_POINT('Ctrl Pts',(-3.77011850300006,5.2,1.93865915599998));
#308778=CARTESIAN_POINT('Ctrl Pts',(-3.77011850300006,2.2,1.93865915599998));
#308779=CARTESIAN_POINT('Ctrl Pts',(-3.76899800000006,12.2,1.93746672799998));
#308780=CARTESIAN_POINT('Ctrl Pts',(-3.76899800000006,5.2,1.93746672799998));
#308781=CARTESIAN_POINT('Ctrl Pts',(-3.76899800000006,2.2,1.93746672799998));
#308782=CARTESIAN_POINT('Ctrl Pts',(-3.76787923300006,12.2,1.93627889399998));
#308783=CARTESIAN_POINT('Ctrl Pts',(-3.76787923300006,5.2,1.93627889399998));
#308784=CARTESIAN_POINT('Ctrl Pts',(-3.76787923300006,2.2,1.93627889399998));
#308785=CARTESIAN_POINT('Ctrl Pts',(-3.76676221100006,12.2,1.93509564999998));
#308786=CARTESIAN_POINT('Ctrl Pts',(-3.76676221100006,5.2,1.93509564999998));
#308787=CARTESIAN_POINT('Ctrl Pts',(-3.76676221100006,2.2,1.93509564999998));
#308788=CARTESIAN_POINT('Ctrl Pts',(-3.76564695000006,12.2,1.93391699899998));
#308789=CARTESIAN_POINT('Ctrl Pts',(-3.76564695000006,5.2,1.93391699899998));
#308790=CARTESIAN_POINT('Ctrl Pts',(-3.76564695000006,2.2,1.93391699899998));
#308791=CARTESIAN_POINT('Ctrl Pts',(-3.76453346100006,12.2,1.93274293799998));
#308792=CARTESIAN_POINT('Ctrl Pts',(-3.76453346100006,5.2,1.93274293799998));
#308793=CARTESIAN_POINT('Ctrl Pts',(-3.76453346100006,2.2,1.93274293799998));
#308794=CARTESIAN_POINT('Ctrl Pts',(-3.76342175700006,12.2,1.93157346699998));
#308795=CARTESIAN_POINT('Ctrl Pts',(-3.76342175700006,5.2,1.93157346699998));
#308796=CARTESIAN_POINT('Ctrl Pts',(-3.76342175700006,2.2,1.93157346699998));
#308797=CARTESIAN_POINT('Ctrl Pts',(-3.76231185100006,12.2,1.93040858599999));
#308798=CARTESIAN_POINT('Ctrl Pts',(-3.76231185100006,5.2,1.93040858599999));
#308799=CARTESIAN_POINT('Ctrl Pts',(-3.76231185100006,2.2,1.93040858599999));
#308800=CARTESIAN_POINT('Ctrl Pts',(-3.76120375500006,12.2,1.92924829299999));
#308801=CARTESIAN_POINT('Ctrl Pts',(-3.76120375500006,5.2,1.92924829299999));
#308802=CARTESIAN_POINT('Ctrl Pts',(-3.76120375500006,2.2,1.92924829299999));
#308803=CARTESIAN_POINT('Ctrl Pts',(-3.76009748200006,12.2,1.92809258799999));
#308804=CARTESIAN_POINT('Ctrl Pts',(-3.76009748200006,5.2,1.92809258799999));
#308805=CARTESIAN_POINT('Ctrl Pts',(-3.76009748200006,2.2,1.92809258799999));
#308806=CARTESIAN_POINT('Ctrl Pts',(-3.75899304500006,12.2,1.92694146999999));
#308807=CARTESIAN_POINT('Ctrl Pts',(-3.75899304500006,5.2,1.92694146999999));
#308808=CARTESIAN_POINT('Ctrl Pts',(-3.75899304500006,2.2,1.92694146999999));
#308809=CARTESIAN_POINT('Ctrl Pts',(-3.75789045700006,12.2,1.92579493999999));
#308810=CARTESIAN_POINT('Ctrl Pts',(-3.75789045700006,5.2,1.92579493999999));
#308811=CARTESIAN_POINT('Ctrl Pts',(-3.75789045700006,2.2,1.92579493999999));
#308812=CARTESIAN_POINT('Ctrl Pts',(-3.75678973100006,12.2,1.92465299499998));
#308813=CARTESIAN_POINT('Ctrl Pts',(-3.75678973100006,5.2,1.92465299499998));
#308814=CARTESIAN_POINT('Ctrl Pts',(-3.75678973100006,2.2,1.92465299499998));
#308815=CARTESIAN_POINT('Ctrl Pts',(-3.75569087900006,12.2,1.92351563499999));
#308816=CARTESIAN_POINT('Ctrl Pts',(-3.75569087900006,5.2,1.92351563499999));
#308817=CARTESIAN_POINT('Ctrl Pts',(-3.75569087900006,2.2,1.92351563499999));
#308818=CARTESIAN_POINT('Ctrl Pts',(-3.75459391600006,12.2,1.92238285999998));
#308819=CARTESIAN_POINT('Ctrl Pts',(-3.75459391600006,5.2,1.92238285999998));
#308820=CARTESIAN_POINT('Ctrl Pts',(-3.75459391600006,2.2,1.92238285999998));
#308821=CARTESIAN_POINT('Ctrl Pts',(-3.75349885100006,12.2,1.92125466899999));
#308822=CARTESIAN_POINT('Ctrl Pts',(-3.75349885100006,5.2,1.92125466899999));
#308823=CARTESIAN_POINT('Ctrl Pts',(-3.75349885100006,2.2,1.92125466899999));
#308824=CARTESIAN_POINT('Ctrl Pts',(-3.75240570000006,12.2,1.92013106099999));
#308825=CARTESIAN_POINT('Ctrl Pts',(-3.75240570000006,5.2,1.92013106099999));
#308826=CARTESIAN_POINT('Ctrl Pts',(-3.75240570000006,2.2,1.92013106099999));
#308827=CARTESIAN_POINT('Ctrl Pts',(-3.75131447600006,12.2,1.91901203499999));
#308828=CARTESIAN_POINT('Ctrl Pts',(-3.75131447600006,5.2,1.91901203499999));
#308829=CARTESIAN_POINT('Ctrl Pts',(-3.75131447600006,2.2,1.91901203499999));
#308830=CARTESIAN_POINT('Ctrl Pts',(-3.75022519000006,12.2,1.91789758999999));
#308831=CARTESIAN_POINT('Ctrl Pts',(-3.75022519000006,5.2,1.91789758999999));
#308832=CARTESIAN_POINT('Ctrl Pts',(-3.75022519000006,2.2,1.91789758999999));
#308833=CARTESIAN_POINT('Ctrl Pts',(-3.74913785700006,12.2,1.91678772499999));
#308834=CARTESIAN_POINT('Ctrl Pts',(-3.74913785700006,5.2,1.91678772499999));
#308835=CARTESIAN_POINT('Ctrl Pts',(-3.74913785700006,2.2,1.91678772499999));
#308836=CARTESIAN_POINT('Ctrl Pts',(-3.74805248800006,12.2,1.91568243999999));
#308837=CARTESIAN_POINT('Ctrl Pts',(-3.74805248800006,5.2,1.91568243999999));
#308838=CARTESIAN_POINT('Ctrl Pts',(-3.74805248800006,2.2,1.91568243999999));
#308839=CARTESIAN_POINT('Ctrl Pts',(-3.74696909800006,12.2,1.91458173299999));
#308840=CARTESIAN_POINT('Ctrl Pts',(-3.74696909800006,5.2,1.91458173299999));
#308841=CARTESIAN_POINT('Ctrl Pts',(-3.74696909800006,2.2,1.91458173299999));
#308842=CARTESIAN_POINT('Ctrl Pts',(-3.74588770000006,12.2,1.91348560399998));
#308843=CARTESIAN_POINT('Ctrl Pts',(-3.74588770000006,5.2,1.91348560399998));
#308844=CARTESIAN_POINT('Ctrl Pts',(-3.74588770000006,2.2,1.91348560399998));
#308845=CARTESIAN_POINT('Ctrl Pts',(-3.74480830500006,12.2,1.91239405099998));
#308846=CARTESIAN_POINT('Ctrl Pts',(-3.74480830500006,5.2,1.91239405099998));
#308847=CARTESIAN_POINT('Ctrl Pts',(-3.74480830500006,2.2,1.91239405099998));
#308848=CARTESIAN_POINT('Ctrl Pts',(-3.74373092900006,12.2,1.91130707499998));
#308849=CARTESIAN_POINT('Ctrl Pts',(-3.74373092900006,5.2,1.91130707499998));
#308850=CARTESIAN_POINT('Ctrl Pts',(-3.74373092900006,2.2,1.91130707499998));
#308851=CARTESIAN_POINT('Ctrl Pts',(-3.74265558200006,12.2,1.91022467399999));
#308852=CARTESIAN_POINT('Ctrl Pts',(-3.74265558200006,5.2,1.91022467399999));
#308853=CARTESIAN_POINT('Ctrl Pts',(-3.74265558200006,2.2,1.91022467399999));
#308854=CARTESIAN_POINT('Ctrl Pts',(-3.74158227900006,12.2,1.90914684599999));
#308855=CARTESIAN_POINT('Ctrl Pts',(-3.74158227900006,5.2,1.90914684599999));
#308856=CARTESIAN_POINT('Ctrl Pts',(-3.74158227900006,2.2,1.90914684599999));
#308857=CARTESIAN_POINT('Ctrl Pts',(-3.74051103400006,12.2,1.90807359099999));
#308858=CARTESIAN_POINT('Ctrl Pts',(-3.74051103400006,5.2,1.90807359099999));
#308859=CARTESIAN_POINT('Ctrl Pts',(-3.74051103400006,2.2,1.90807359099999));
#308860=CARTESIAN_POINT('Ctrl Pts',(-3.73944185800006,12.2,1.90700490799999));
#308861=CARTESIAN_POINT('Ctrl Pts',(-3.73944185800006,5.2,1.90700490799999));
#308862=CARTESIAN_POINT('Ctrl Pts',(-3.73944185800006,2.2,1.90700490799999));
#308863=CARTESIAN_POINT('Ctrl Pts',(-3.73837476700006,12.2,1.90594079599999));
#308864=CARTESIAN_POINT('Ctrl Pts',(-3.73837476700006,5.2,1.90594079599999));
#308865=CARTESIAN_POINT('Ctrl Pts',(-3.73837476700006,2.2,1.90594079599999));
#308866=CARTESIAN_POINT('Ctrl Pts',(-3.73730977200006,12.2,1.90488125399999));
#308867=CARTESIAN_POINT('Ctrl Pts',(-3.73730977200006,5.2,1.90488125399999));
#308868=CARTESIAN_POINT('Ctrl Pts',(-3.73730977200006,2.2,1.90488125399999));
#308869=CARTESIAN_POINT('Ctrl Pts',(-3.73624688700006,12.2,1.90382627899998));
#308870=CARTESIAN_POINT('Ctrl Pts',(-3.73624688700006,5.2,1.90382627899998));
#308871=CARTESIAN_POINT('Ctrl Pts',(-3.73624688700006,2.2,1.90382627899998));
#308872=CARTESIAN_POINT('Ctrl Pts',(-3.73518612500006,12.2,1.90277587299999));
#308873=CARTESIAN_POINT('Ctrl Pts',(-3.73518612500006,5.2,1.90277587299999));
#308874=CARTESIAN_POINT('Ctrl Pts',(-3.73518612500006,2.2,1.90277587299999));
#308875=CARTESIAN_POINT('Ctrl Pts',(-3.73412750100006,12.2,1.90173003299998));
#308876=CARTESIAN_POINT('Ctrl Pts',(-3.73412750100006,5.2,1.90173003299998));
#308877=CARTESIAN_POINT('Ctrl Pts',(-3.73412750100006,2.2,1.90173003299998));
#308878=CARTESIAN_POINT('Ctrl Pts',(-3.73307102500006,12.2,1.90068875799998));
#308879=CARTESIAN_POINT('Ctrl Pts',(-3.73307102500006,5.2,1.90068875799998));
#308880=CARTESIAN_POINT('Ctrl Pts',(-3.73307102500006,2.2,1.90068875799998));
#308881=CARTESIAN_POINT('Ctrl Pts',(-3.73201671400006,12.2,1.89965204599998));
#308882=CARTESIAN_POINT('Ctrl Pts',(-3.73201671400006,5.2,1.89965204599998));
#308883=CARTESIAN_POINT('Ctrl Pts',(-3.73201671400006,2.2,1.89965204599998));
#308884=CARTESIAN_POINT('Ctrl Pts',(-3.73096458000005,12.2,1.89861989799998));
#308885=CARTESIAN_POINT('Ctrl Pts',(-3.73096458000005,5.2,1.89861989799998));
#308886=CARTESIAN_POINT('Ctrl Pts',(-3.73096458000005,2.2,1.89861989799998));
#308887=CARTESIAN_POINT('Ctrl Pts',(-3.72991463600005,12.2,1.89759231199998));
#308888=CARTESIAN_POINT('Ctrl Pts',(-3.72991463600005,5.2,1.89759231199998));
#308889=CARTESIAN_POINT('Ctrl Pts',(-3.72991463600005,2.2,1.89759231199998));
#308890=CARTESIAN_POINT('Ctrl Pts',(-3.72886689600006,12.2,1.89656928499998));
#308891=CARTESIAN_POINT('Ctrl Pts',(-3.72886689600006,5.2,1.89656928499998));
#308892=CARTESIAN_POINT('Ctrl Pts',(-3.72886689600006,2.2,1.89656928499998));
#308893=CARTESIAN_POINT('Ctrl Pts',(-3.72782137300006,12.2,1.89555081899998));
#308894=CARTESIAN_POINT('Ctrl Pts',(-3.72782137300006,5.2,1.89555081899998));
#308895=CARTESIAN_POINT('Ctrl Pts',(-3.72782137300006,2.2,1.89555081899998));
#308896=CARTESIAN_POINT('Ctrl Pts',(-3.72677808100006,12.2,1.89453690999999));
#308897=CARTESIAN_POINT('Ctrl Pts',(-3.72677808100006,5.2,1.89453690999999));
#308898=CARTESIAN_POINT('Ctrl Pts',(-3.72677808100006,2.2,1.89453690999999));
#308899=CARTESIAN_POINT('Ctrl Pts',(-3.72573703400006,12.2,1.89352755799999));
#308900=CARTESIAN_POINT('Ctrl Pts',(-3.72573703400006,5.2,1.89352755799999));
#308901=CARTESIAN_POINT('Ctrl Pts',(-3.72573703400006,2.2,1.89352755799999));
#308902=CARTESIAN_POINT('Ctrl Pts',(-3.72469824400006,12.2,1.89252275999999));
#308903=CARTESIAN_POINT('Ctrl Pts',(-3.72469824400006,5.2,1.89252275999999));
#308904=CARTESIAN_POINT('Ctrl Pts',(-3.72469824400006,2.2,1.89252275999999));
#308905=CARTESIAN_POINT('Ctrl Pts',(-3.72366172600006,12.2,1.89152251699999));
#308906=CARTESIAN_POINT('Ctrl Pts',(-3.72366172600006,5.2,1.89152251699999));
#308907=CARTESIAN_POINT('Ctrl Pts',(-3.72366172600006,2.2,1.89152251699999));
#308908=CARTESIAN_POINT('Ctrl Pts',(-3.72262749400006,12.2,1.89052682599999));
#308909=CARTESIAN_POINT('Ctrl Pts',(-3.72262749400006,5.2,1.89052682599999));
#308910=CARTESIAN_POINT('Ctrl Pts',(-3.72262749400006,2.2,1.89052682599999));
#308911=CARTESIAN_POINT('Ctrl Pts',(-3.72159556000006,12.2,1.88953568699999));
#308912=CARTESIAN_POINT('Ctrl Pts',(-3.72159556000006,5.2,1.88953568699999));
#308913=CARTESIAN_POINT('Ctrl Pts',(-3.72159556000006,2.2,1.88953568699999));
#308914=CARTESIAN_POINT('Ctrl Pts',(-3.72056593900006,12.2,1.88854909599999));
#308915=CARTESIAN_POINT('Ctrl Pts',(-3.72056593900006,5.2,1.88854909599999));
#308916=CARTESIAN_POINT('Ctrl Pts',(-3.72056593900006,2.2,1.88854909599999));
#308917=CARTESIAN_POINT('Ctrl Pts',(-3.71953864400006,12.2,1.88756705499999));
#308918=CARTESIAN_POINT('Ctrl Pts',(-3.71953864400006,5.2,1.88756705499999));
#308919=CARTESIAN_POINT('Ctrl Pts',(-3.71953864400006,2.2,1.88756705499999));
#308920=CARTESIAN_POINT('Ctrl Pts',(-3.71851369000006,12.2,1.88658955999998));
#308921=CARTESIAN_POINT('Ctrl Pts',(-3.71851369000006,5.2,1.88658955999998));
#308922=CARTESIAN_POINT('Ctrl Pts',(-3.71851369000006,2.2,1.88658955999998));
#308923=CARTESIAN_POINT('Ctrl Pts',(-3.71749108900006,12.2,1.88561661199998));
#308924=CARTESIAN_POINT('Ctrl Pts',(-3.71749108900006,5.2,1.88561661199998));
#308925=CARTESIAN_POINT('Ctrl Pts',(-3.71749108900006,2.2,1.88561661199998));
#308926=CARTESIAN_POINT('Ctrl Pts',(-3.71647085600006,12.2,1.88464820699998));
#308927=CARTESIAN_POINT('Ctrl Pts',(-3.71647085600006,5.2,1.88464820699998));
#308928=CARTESIAN_POINT('Ctrl Pts',(-3.71647085600006,2.2,1.88464820699998));
#308929=CARTESIAN_POINT('Ctrl Pts',(-3.71545300400006,12.2,1.88368434499999));
#308930=CARTESIAN_POINT('Ctrl Pts',(-3.71545300400006,5.2,1.88368434499999));
#308931=CARTESIAN_POINT('Ctrl Pts',(-3.71545300400006,2.2,1.88368434499999));
#308932=CARTESIAN_POINT('Ctrl Pts',(-3.71443754800006,12.2,1.88272502299998));
#308933=CARTESIAN_POINT('Ctrl Pts',(-3.71443754800006,5.2,1.88272502299998));
#308934=CARTESIAN_POINT('Ctrl Pts',(-3.71443754800006,2.2,1.88272502299998));
#308935=CARTESIAN_POINT('Ctrl Pts',(-3.71342450000006,12.2,1.88177023999998));
#308936=CARTESIAN_POINT('Ctrl Pts',(-3.71342450000006,5.2,1.88177023999998));
#308937=CARTESIAN_POINT('Ctrl Pts',(-3.71342450000006,2.2,1.88177023999998));
#308938=CARTESIAN_POINT('Ctrl Pts',(-3.71241387600006,12.2,1.88081999599999));
#308939=CARTESIAN_POINT('Ctrl Pts',(-3.71241387600006,5.2,1.88081999599999));
#308940=CARTESIAN_POINT('Ctrl Pts',(-3.71241387600006,2.2,1.88081999599999));
#308941=CARTESIAN_POINT('Ctrl Pts',(-3.71140568900006,12.2,1.87987428799998));
#308942=CARTESIAN_POINT('Ctrl Pts',(-3.71140568900006,5.2,1.87987428799998));
#308943=CARTESIAN_POINT('Ctrl Pts',(-3.71140568900006,2.2,1.87987428799998));
#308944=CARTESIAN_POINT('Ctrl Pts',(-3.71039995200006,12.2,1.87893311499999));
#308945=CARTESIAN_POINT('Ctrl Pts',(-3.71039995200006,5.2,1.87893311499999));
#308946=CARTESIAN_POINT('Ctrl Pts',(-3.71039995200006,2.2,1.87893311499999));
#308947=CARTESIAN_POINT('Ctrl Pts',(-3.70939668200006,12.2,1.87799647399999));
#308948=CARTESIAN_POINT('Ctrl Pts',(-3.70939668200006,5.2,1.87799647399999));
#308949=CARTESIAN_POINT('Ctrl Pts',(-3.70939668200006,2.2,1.87799647399999));
#308950=CARTESIAN_POINT('Ctrl Pts',(-3.70839588900005,12.2,1.87706436599999));
#308951=CARTESIAN_POINT('Ctrl Pts',(-3.70839588900005,5.2,1.87706436599999));
#308952=CARTESIAN_POINT('Ctrl Pts',(-3.70839588900005,2.2,1.87706436599999));
#308953=CARTESIAN_POINT('Ctrl Pts',(-3.70739759000006,12.2,1.87613678599998));
#308954=CARTESIAN_POINT('Ctrl Pts',(-3.70739759000006,5.2,1.87613678599998));
#308955=CARTESIAN_POINT('Ctrl Pts',(-3.70739759000006,2.2,1.87613678599998));
#308956=CARTESIAN_POINT('Ctrl Pts',(-3.70640179700006,12.2,1.87521373399999));
#308957=CARTESIAN_POINT('Ctrl Pts',(-3.70640179700006,5.2,1.87521373399999));
#308958=CARTESIAN_POINT('Ctrl Pts',(-3.70640179700006,2.2,1.87521373399999));
#308959=CARTESIAN_POINT('Ctrl Pts',(-3.70540852600006,12.2,1.87429520899999));
#308960=CARTESIAN_POINT('Ctrl Pts',(-3.70540852600006,5.2,1.87429520899999));
#308961=CARTESIAN_POINT('Ctrl Pts',(-3.70540852600006,2.2,1.87429520899999));
#308962=CARTESIAN_POINT('Ctrl Pts',(-3.70441779000005,12.2,1.87338120899998));
#308963=CARTESIAN_POINT('Ctrl Pts',(-3.70441779000005,5.2,1.87338120899998));
#308964=CARTESIAN_POINT('Ctrl Pts',(-3.70441779000005,2.2,1.87338120899998));
#308965=CARTESIAN_POINT('Ctrl Pts',(-3.70342960400006,12.2,1.87247173099998));
#308966=CARTESIAN_POINT('Ctrl Pts',(-3.70342960400006,5.2,1.87247173099998));
#308967=CARTESIAN_POINT('Ctrl Pts',(-3.70342960400006,2.2,1.87247173099998));
#308968=CARTESIAN_POINT('Ctrl Pts',(-3.70244398200006,12.2,1.87156677399999));
#308969=CARTESIAN_POINT('Ctrl Pts',(-3.70244398200006,5.2,1.87156677399999));
#308970=CARTESIAN_POINT('Ctrl Pts',(-3.70244398200006,2.2,1.87156677399999));
#308971=CARTESIAN_POINT('Ctrl Pts',(-3.70146093700006,12.2,1.87066633599999));
#308972=CARTESIAN_POINT('Ctrl Pts',(-3.70146093700006,5.2,1.87066633599999));
#308973=CARTESIAN_POINT('Ctrl Pts',(-3.70146093700006,2.2,1.87066633599999));
#308974=CARTESIAN_POINT('Ctrl Pts',(-3.70048048300006,12.2,1.86977041599999));
#308975=CARTESIAN_POINT('Ctrl Pts',(-3.70048048300006,5.2,1.86977041599999));
#308976=CARTESIAN_POINT('Ctrl Pts',(-3.70048048300006,2.2,1.86977041599999));
#308977=CARTESIAN_POINT('Ctrl Pts',(-3.69950263700006,12.2,1.86887901099999));
#308978=CARTESIAN_POINT('Ctrl Pts',(-3.69950263700006,5.2,1.86887901099999));
#308979=CARTESIAN_POINT('Ctrl Pts',(-3.69950263700006,2.2,1.86887901099999));
#308980=CARTESIAN_POINT('Ctrl Pts',(-3.69852741200006,12.2,1.86799211899999));
#308981=CARTESIAN_POINT('Ctrl Pts',(-3.69852741200006,5.2,1.86799211899999));
#308982=CARTESIAN_POINT('Ctrl Pts',(-3.69852741200006,2.2,1.86799211899999));
#308983=CARTESIAN_POINT('Ctrl Pts',(-3.69755482000006,12.2,1.86710973899999));
#308984=CARTESIAN_POINT('Ctrl Pts',(-3.69755482000006,5.2,1.86710973899999));
#308985=CARTESIAN_POINT('Ctrl Pts',(-3.69755482000006,2.2,1.86710973899999));
#308986=CARTESIAN_POINT('Ctrl Pts',(-3.69658487900006,12.2,1.86623186999999));
#308987=CARTESIAN_POINT('Ctrl Pts',(-3.69658487900006,5.2,1.86623186999999));
#308988=CARTESIAN_POINT('Ctrl Pts',(-3.69658487900006,2.2,1.86623186999999));
#308989=CARTESIAN_POINT('Ctrl Pts',(-3.69561760100006,12.2,1.86535850699999));
#308990=CARTESIAN_POINT('Ctrl Pts',(-3.69561760100006,5.2,1.86535850699999));
#308991=CARTESIAN_POINT('Ctrl Pts',(-3.69561760100006,2.2,1.86535850699999));
#308992=CARTESIAN_POINT('Ctrl Pts',(-3.69465300100006,12.2,1.86448964999999));
#308993=CARTESIAN_POINT('Ctrl Pts',(-3.69465300100006,5.2,1.86448964999999));
#308994=CARTESIAN_POINT('Ctrl Pts',(-3.69465300100006,2.2,1.86448964999999));
#308995=CARTESIAN_POINT('Ctrl Pts',(-3.69369109400006,12.2,1.86362529699998));
#308996=CARTESIAN_POINT('Ctrl Pts',(-3.69369109400006,5.2,1.86362529699998));
#308997=CARTESIAN_POINT('Ctrl Pts',(-3.69369109400006,2.2,1.86362529699998));
#308998=CARTESIAN_POINT('Ctrl Pts',(-3.69273189400006,12.2,1.86276544599998));
#308999=CARTESIAN_POINT('Ctrl Pts',(-3.69273189400006,5.2,1.86276544599998));
#309000=CARTESIAN_POINT('Ctrl Pts',(-3.69273189400006,2.2,1.86276544599998));
#309001=CARTESIAN_POINT('Ctrl Pts',(-3.69177541500005,12.2,1.86191009499999));
#309002=CARTESIAN_POINT('Ctrl Pts',(-3.69177541500005,5.2,1.86191009499999));
#309003=CARTESIAN_POINT('Ctrl Pts',(-3.69177541500005,2.2,1.86191009499999));
#309004=CARTESIAN_POINT('Ctrl Pts',(-3.69082167100006,12.2,1.86105924099999));
#309005=CARTESIAN_POINT('Ctrl Pts',(-3.69082167100006,5.2,1.86105924099999));
#309006=CARTESIAN_POINT('Ctrl Pts',(-3.69082167100006,2.2,1.86105924099999));
#309007=CARTESIAN_POINT('Ctrl Pts',(-3.68987068000005,12.2,1.86021288299999));
#309008=CARTESIAN_POINT('Ctrl Pts',(-3.68987068000005,5.2,1.86021288299999));
#309009=CARTESIAN_POINT('Ctrl Pts',(-3.68987068000005,2.2,1.86021288299999));
#309010=CARTESIAN_POINT('Ctrl Pts',(-3.68892245300006,12.2,1.85937101899999));
#309011=CARTESIAN_POINT('Ctrl Pts',(-3.68892245300006,5.2,1.85937101899999));
#309012=CARTESIAN_POINT('Ctrl Pts',(-3.68892245300006,2.2,1.85937101899999));
#309013=CARTESIAN_POINT('Ctrl Pts',(-3.68797700500005,12.2,1.85853364499998));
#309014=CARTESIAN_POINT('Ctrl Pts',(-3.68797700500005,5.2,1.85853364499998));
#309015=CARTESIAN_POINT('Ctrl Pts',(-3.68797700500005,2.2,1.85853364499998));
#309016=CARTESIAN_POINT('Ctrl Pts',(-3.68703435300006,12.2,1.85770076099999));
#309017=CARTESIAN_POINT('Ctrl Pts',(-3.68703435300006,5.2,1.85770076099999));
#309018=CARTESIAN_POINT('Ctrl Pts',(-3.68703435300006,2.2,1.85770076099999));
#309019=CARTESIAN_POINT('Ctrl Pts',(-3.68609450900006,12.2,1.85687236399998));
#309020=CARTESIAN_POINT('Ctrl Pts',(-3.68609450900006,5.2,1.85687236399998));
#309021=CARTESIAN_POINT('Ctrl Pts',(-3.68609450900006,2.2,1.85687236399998));
#309022=CARTESIAN_POINT('Ctrl Pts',(-3.68515749000006,12.2,1.85604845099999));
#309023=CARTESIAN_POINT('Ctrl Pts',(-3.68515749000006,5.2,1.85604845099999));
#309024=CARTESIAN_POINT('Ctrl Pts',(-3.68515749000006,2.2,1.85604845099999));
#309025=CARTESIAN_POINT('Ctrl Pts',(-3.68422330900006,12.2,1.85522902099999));
#309026=CARTESIAN_POINT('Ctrl Pts',(-3.68422330900006,5.2,1.85522902099999));
#309027=CARTESIAN_POINT('Ctrl Pts',(-3.68422330900006,2.2,1.85522902099999));
#309028=CARTESIAN_POINT('Ctrl Pts',(-3.68329198100006,12.2,1.85441407199999));
#309029=CARTESIAN_POINT('Ctrl Pts',(-3.68329198100006,5.2,1.85441407199999));
#309030=CARTESIAN_POINT('Ctrl Pts',(-3.68329198100006,2.2,1.85441407199999));
#309031=CARTESIAN_POINT('Ctrl Pts',(-3.68236352100006,12.2,1.85360359999999));
#309032=CARTESIAN_POINT('Ctrl Pts',(-3.68236352100006,5.2,1.85360359999999));
#309033=CARTESIAN_POINT('Ctrl Pts',(-3.68236352100006,2.2,1.85360359999999));
#309034=CARTESIAN_POINT('Ctrl Pts',(-3.68143794400006,12.2,1.85279760399998));
#309035=CARTESIAN_POINT('Ctrl Pts',(-3.68143794400006,5.2,1.85279760399998));
#309036=CARTESIAN_POINT('Ctrl Pts',(-3.68143794400006,2.2,1.85279760399998));
#309037=CARTESIAN_POINT('Ctrl Pts',(-3.68051526600006,12.2,1.85199608199999));
#309038=CARTESIAN_POINT('Ctrl Pts',(-3.68051526600006,5.2,1.85199608199999));
#309039=CARTESIAN_POINT('Ctrl Pts',(-3.68051526600006,2.2,1.85199608199999));
#309040=CARTESIAN_POINT('Ctrl Pts',(-3.67959550000006,12.2,1.85119902999999));
#309041=CARTESIAN_POINT('Ctrl Pts',(-3.67959550000006,5.2,1.85119902999999));
#309042=CARTESIAN_POINT('Ctrl Pts',(-3.67959550000006,2.2,1.85119902999999));
#309043=CARTESIAN_POINT('Ctrl Pts',(-3.67867866100006,12.2,1.85040644699999));
#309044=CARTESIAN_POINT('Ctrl Pts',(-3.67867866100006,5.2,1.85040644699999));
#309045=CARTESIAN_POINT('Ctrl Pts',(-3.67867866100006,2.2,1.85040644699999));
#309046=CARTESIAN_POINT('Ctrl Pts',(-3.67776476600006,12.2,1.84961832999999));
#309047=CARTESIAN_POINT('Ctrl Pts',(-3.67776476600006,5.2,1.84961832999999));
#309048=CARTESIAN_POINT('Ctrl Pts',(-3.67776476600006,2.2,1.84961832999999));
#309049=CARTESIAN_POINT('Ctrl Pts',(-3.67685382700006,12.2,1.84883467599999));
#309050=CARTESIAN_POINT('Ctrl Pts',(-3.67685382700006,5.2,1.84883467599999));
#309051=CARTESIAN_POINT('Ctrl Pts',(-3.67685382700006,2.2,1.84883467599999));
#309052=CARTESIAN_POINT('Ctrl Pts',(-3.67594586200005,12.2,1.84805548499998));
#309053=CARTESIAN_POINT('Ctrl Pts',(-3.67594586200005,5.2,1.84805548499998));
#309054=CARTESIAN_POINT('Ctrl Pts',(-3.67594586200005,2.2,1.84805548499998));
#309055=CARTESIAN_POINT('Ctrl Pts',(-3.67504088400006,12.2,1.84728075099999));
#309056=CARTESIAN_POINT('Ctrl Pts',(-3.67504088400006,5.2,1.84728075099999));
#309057=CARTESIAN_POINT('Ctrl Pts',(-3.67504088400006,2.2,1.84728075099999));
#309058=CARTESIAN_POINT('Ctrl Pts',(-3.67413890800006,12.2,1.84651047499999));
#309059=CARTESIAN_POINT('Ctrl Pts',(-3.67413890800006,5.2,1.84651047499999));
#309060=CARTESIAN_POINT('Ctrl Pts',(-3.67413890800006,2.2,1.84651047499999));
#309061=CARTESIAN_POINT('Ctrl Pts',(-3.67323995100006,12.2,1.84574465199999));
#309062=CARTESIAN_POINT('Ctrl Pts',(-3.67323995100006,5.2,1.84574465199999));
#309063=CARTESIAN_POINT('Ctrl Pts',(-3.67323995100006,2.2,1.84574465199999));
#309064=CARTESIAN_POINT('Ctrl Pts',(-3.67234402700006,12.2,1.84498327999998));
#309065=CARTESIAN_POINT('Ctrl Pts',(-3.67234402700006,5.2,1.84498327999998));
#309066=CARTESIAN_POINT('Ctrl Pts',(-3.67234402700006,2.2,1.84498327999998));
#309067=CARTESIAN_POINT('Ctrl Pts',(-3.67145115000006,12.2,1.84422635699999));
#309068=CARTESIAN_POINT('Ctrl Pts',(-3.67145115000006,5.2,1.84422635699999));
#309069=CARTESIAN_POINT('Ctrl Pts',(-3.67145115000006,2.2,1.84422635699999));
#309070=CARTESIAN_POINT('Ctrl Pts',(-3.67056133700006,12.2,1.84347387999999));
#309071=CARTESIAN_POINT('Ctrl Pts',(-3.67056133700006,5.2,1.84347387999999));
#309072=CARTESIAN_POINT('Ctrl Pts',(-3.67056133700006,2.2,1.84347387999999));
#309073=CARTESIAN_POINT('Ctrl Pts',(-3.66967460300006,12.2,1.84272584599999));
#309074=CARTESIAN_POINT('Ctrl Pts',(-3.66967460300006,5.2,1.84272584599999));
#309075=CARTESIAN_POINT('Ctrl Pts',(-3.66967460300006,2.2,1.84272584599999));
#309076=CARTESIAN_POINT('Ctrl Pts',(-3.66879096200006,12.2,1.84198225299999));
#309077=CARTESIAN_POINT('Ctrl Pts',(-3.66879096200006,5.2,1.84198225299999));
#309078=CARTESIAN_POINT('Ctrl Pts',(-3.66879096200006,2.2,1.84198225299999));
#309079=CARTESIAN_POINT('Ctrl Pts',(-3.66791043200006,12.2,1.84124309799999));
#309080=CARTESIAN_POINT('Ctrl Pts',(-3.66791043200006,5.2,1.84124309799999));
#309081=CARTESIAN_POINT('Ctrl Pts',(-3.66791043200006,2.2,1.84124309799999));
#309082=CARTESIAN_POINT('Ctrl Pts',(-3.66703302500006,12.2,1.84050837899999));
#309083=CARTESIAN_POINT('Ctrl Pts',(-3.66703302500006,5.2,1.84050837899999));
#309084=CARTESIAN_POINT('Ctrl Pts',(-3.66703302500006,2.2,1.84050837899999));
#309085=CARTESIAN_POINT('Ctrl Pts',(-3.66615875800006,12.2,1.83977809099999));
#309086=CARTESIAN_POINT('Ctrl Pts',(-3.66615875800006,5.2,1.83977809099999));
#309087=CARTESIAN_POINT('Ctrl Pts',(-3.66615875800006,2.2,1.83977809099999));
#309088=CARTESIAN_POINT('Ctrl Pts',(-3.66528764600006,12.2,1.83905223399998));
#309089=CARTESIAN_POINT('Ctrl Pts',(-3.66528764600006,5.2,1.83905223399998));
#309090=CARTESIAN_POINT('Ctrl Pts',(-3.66528764600006,2.2,1.83905223399998));
#309091=CARTESIAN_POINT('Ctrl Pts',(-3.66441970600006,12.2,1.83833080299999));
#309092=CARTESIAN_POINT('Ctrl Pts',(-3.66441970600006,5.2,1.83833080299999));
#309093=CARTESIAN_POINT('Ctrl Pts',(-3.66441970600006,2.2,1.83833080299999));
#309094=CARTESIAN_POINT('Ctrl Pts',(-3.66355495100006,12.2,1.83761379699999));
#309095=CARTESIAN_POINT('Ctrl Pts',(-3.66355495100006,5.2,1.83761379699999));
#309096=CARTESIAN_POINT('Ctrl Pts',(-3.66355495100006,2.2,1.83761379699999));
#309097=CARTESIAN_POINT('Ctrl Pts',(-3.66269339700006,12.2,1.83690121199998));
#309098=CARTESIAN_POINT('Ctrl Pts',(-3.66269339700006,5.2,1.83690121199998));
#309099=CARTESIAN_POINT('Ctrl Pts',(-3.66269339700006,2.2,1.83690121199998));
#309100=CARTESIAN_POINT('Ctrl Pts',(-3.66183506100006,12.2,1.83619304499999));
#309101=CARTESIAN_POINT('Ctrl Pts',(-3.66183506100006,5.2,1.83619304499999));
#309102=CARTESIAN_POINT('Ctrl Pts',(-3.66183506100006,2.2,1.83619304499999));
#309103=CARTESIAN_POINT('Ctrl Pts',(-3.66097995800006,12.2,1.83548929399999));
#309104=CARTESIAN_POINT('Ctrl Pts',(-3.66097995800006,5.2,1.83548929399999));
#309105=CARTESIAN_POINT('Ctrl Pts',(-3.66097995800006,2.2,1.83548929399999));
#309106=CARTESIAN_POINT('Ctrl Pts',(-3.66012810400006,12.2,1.83478995599998));
#309107=CARTESIAN_POINT('Ctrl Pts',(-3.66012810400006,5.2,1.83478995599998));
#309108=CARTESIAN_POINT('Ctrl Pts',(-3.66012810400006,2.2,1.83478995599998));
#309109=CARTESIAN_POINT('Ctrl Pts',(-3.65927951400006,12.2,1.83409502799998));
#309110=CARTESIAN_POINT('Ctrl Pts',(-3.65927951400006,5.2,1.83409502799998));
#309111=CARTESIAN_POINT('Ctrl Pts',(-3.65927951400006,2.2,1.83409502799998));
#309112=CARTESIAN_POINT('Ctrl Pts',(-3.65843420300005,12.2,1.83340450599998));
#309113=CARTESIAN_POINT('Ctrl Pts',(-3.65843420300005,5.2,1.83340450599998));
#309114=CARTESIAN_POINT('Ctrl Pts',(-3.65843420300005,2.2,1.83340450599998));
#309115=CARTESIAN_POINT('Ctrl Pts',(-3.65759218800005,12.2,1.83271838799998));
#309116=CARTESIAN_POINT('Ctrl Pts',(-3.65759218800005,5.2,1.83271838799998));
#309117=CARTESIAN_POINT('Ctrl Pts',(-3.65759218800005,2.2,1.83271838799998));
#309118=CARTESIAN_POINT('Ctrl Pts',(-3.65675348400006,12.2,1.83203666999999));
#309119=CARTESIAN_POINT('Ctrl Pts',(-3.65675348400006,5.2,1.83203666999999));
#309120=CARTESIAN_POINT('Ctrl Pts',(-3.65675348400006,2.2,1.83203666999999));
#309121=CARTESIAN_POINT('Ctrl Pts',(-3.65591810600006,12.2,1.83135934999999));
#309122=CARTESIAN_POINT('Ctrl Pts',(-3.65591810600006,5.2,1.83135934999999));
#309123=CARTESIAN_POINT('Ctrl Pts',(-3.65591810600006,2.2,1.83135934999999));
#309124=CARTESIAN_POINT('Ctrl Pts',(-3.65508607100006,12.2,1.83068642499999));
#309125=CARTESIAN_POINT('Ctrl Pts',(-3.65508607100006,5.2,1.83068642499999));
#309126=CARTESIAN_POINT('Ctrl Pts',(-3.65508607100006,2.2,1.83068642499999));
#309127=CARTESIAN_POINT('Ctrl Pts',(-3.65425739600005,12.2,1.83001788999999));
#309128=CARTESIAN_POINT('Ctrl Pts',(-3.65425739600005,5.2,1.83001788999999));
#309129=CARTESIAN_POINT('Ctrl Pts',(-3.65425739600005,2.2,1.83001788999999));
#309130=CARTESIAN_POINT('Ctrl Pts',(-3.65343209400006,12.2,1.82935374399999));
#309131=CARTESIAN_POINT('Ctrl Pts',(-3.65343209400006,5.2,1.82935374399999));
#309132=CARTESIAN_POINT('Ctrl Pts',(-3.65343209400006,2.2,1.82935374399999));
#309133=CARTESIAN_POINT('Ctrl Pts',(-3.65261018300005,12.2,1.82869398399998));
#309134=CARTESIAN_POINT('Ctrl Pts',(-3.65261018300005,5.2,1.82869398399998));
#309135=CARTESIAN_POINT('Ctrl Pts',(-3.65261018300005,2.2,1.82869398399998));
#309136=CARTESIAN_POINT('Ctrl Pts',(-3.65179167700005,12.2,1.82803860399999));
#309137=CARTESIAN_POINT('Ctrl Pts',(-3.65179167700005,5.2,1.82803860399999));
#309138=CARTESIAN_POINT('Ctrl Pts',(-3.65179167700005,2.2,1.82803860399999));
#309139=CARTESIAN_POINT('Ctrl Pts',(-3.65097659500006,12.2,1.82738760299999));
#309140=CARTESIAN_POINT('Ctrl Pts',(-3.65097659500006,5.2,1.82738760299999));
#309141=CARTESIAN_POINT('Ctrl Pts',(-3.65097659500006,2.2,1.82738760299999));
#309142=CARTESIAN_POINT('Ctrl Pts',(-3.65016495000006,12.2,1.82674097899998));
#309143=CARTESIAN_POINT('Ctrl Pts',(-3.65016495000006,5.2,1.82674097899998));
#309144=CARTESIAN_POINT('Ctrl Pts',(-3.65016495000006,2.2,1.82674097899998));
#309145=CARTESIAN_POINT('Ctrl Pts',(-3.64935676100006,12.2,1.82609872499999));
#309146=CARTESIAN_POINT('Ctrl Pts',(-3.64935676100006,5.2,1.82609872499999));
#309147=CARTESIAN_POINT('Ctrl Pts',(-3.64935676100006,2.2,1.82609872499999));
#309148=CARTESIAN_POINT('Ctrl Pts',(-3.64855204100006,12.2,1.82546084099998));
#309149=CARTESIAN_POINT('Ctrl Pts',(-3.64855204100006,5.2,1.82546084099998));
#309150=CARTESIAN_POINT('Ctrl Pts',(-3.64855204100006,2.2,1.82546084099998));
#309151=CARTESIAN_POINT('Ctrl Pts',(-3.64775080700006,12.2,1.82482732199999));
#309152=CARTESIAN_POINT('Ctrl Pts',(-3.64775080700006,5.2,1.82482732199999));
#309153=CARTESIAN_POINT('Ctrl Pts',(-3.64775080700006,2.2,1.82482732199999));
#309154=CARTESIAN_POINT('Ctrl Pts',(-3.64695307800006,12.2,1.82419816399999));
#309155=CARTESIAN_POINT('Ctrl Pts',(-3.64695307800006,5.2,1.82419816399999));
#309156=CARTESIAN_POINT('Ctrl Pts',(-3.64695307800006,2.2,1.82419816399999));
#309157=CARTESIAN_POINT('Ctrl Pts',(-3.64615886600006,12.2,1.82357336599999));
#309158=CARTESIAN_POINT('Ctrl Pts',(-3.64615886600006,5.2,1.82357336599999));
#309159=CARTESIAN_POINT('Ctrl Pts',(-3.64615886600006,2.2,1.82357336599999));
#309160=CARTESIAN_POINT('Ctrl Pts',(-3.64536819000006,12.2,1.82295292299999));
#309161=CARTESIAN_POINT('Ctrl Pts',(-3.64536819000006,5.2,1.82295292299999));
#309162=CARTESIAN_POINT('Ctrl Pts',(-3.64536819000006,2.2,1.82295292299999));
#309163=CARTESIAN_POINT('Ctrl Pts',(-3.64458106600006,12.2,1.82233683099998));
#309164=CARTESIAN_POINT('Ctrl Pts',(-3.64458106600006,5.2,1.82233683099998));
#309165=CARTESIAN_POINT('Ctrl Pts',(-3.64458106600006,2.2,1.82233683099998));
#309166=CARTESIAN_POINT('Ctrl Pts',(-3.64379750800006,12.2,1.82172508799999));
#309167=CARTESIAN_POINT('Ctrl Pts',(-3.64379750800006,5.2,1.82172508799999));
#309168=CARTESIAN_POINT('Ctrl Pts',(-3.64379750800006,2.2,1.82172508799999));
#309169=CARTESIAN_POINT('Ctrl Pts',(-3.64301753500006,12.2,1.82111768899999));
#309170=CARTESIAN_POINT('Ctrl Pts',(-3.64301753500006,5.2,1.82111768899999));
#309171=CARTESIAN_POINT('Ctrl Pts',(-3.64301753500006,2.2,1.82111768899999));
#309172=CARTESIAN_POINT('Ctrl Pts',(-3.64224116200006,12.2,1.82051463099999));
#309173=CARTESIAN_POINT('Ctrl Pts',(-3.64224116200006,5.2,1.82051463099999));
#309174=CARTESIAN_POINT('Ctrl Pts',(-3.64224116200006,2.2,1.82051463099999));
#309175=CARTESIAN_POINT('Ctrl Pts',(-3.64146840700006,12.2,1.81991591099999));
#309176=CARTESIAN_POINT('Ctrl Pts',(-3.64146840700006,5.2,1.81991591099999));
#309177=CARTESIAN_POINT('Ctrl Pts',(-3.64146840700006,2.2,1.81991591099999));
#309178=CARTESIAN_POINT('Ctrl Pts',(-3.64069928400006,12.2,1.81932152599999));
#309179=CARTESIAN_POINT('Ctrl Pts',(-3.64069928400006,5.2,1.81932152599999));
#309180=CARTESIAN_POINT('Ctrl Pts',(-3.64069928400006,2.2,1.81932152599999));
#309181=CARTESIAN_POINT('Ctrl Pts',(-3.63993381200006,12.2,1.81873146999999));
#309182=CARTESIAN_POINT('Ctrl Pts',(-3.63993381200006,5.2,1.81873146999999));
#309183=CARTESIAN_POINT('Ctrl Pts',(-3.63993381200006,2.2,1.81873146999999));
#309184=CARTESIAN_POINT('Ctrl Pts',(-3.63917200600006,12.2,1.81814573999999));
#309185=CARTESIAN_POINT('Ctrl Pts',(-3.63917200600006,5.2,1.81814573999999));
#309186=CARTESIAN_POINT('Ctrl Pts',(-3.63917200600006,2.2,1.81814573999999));
#309187=CARTESIAN_POINT('Ctrl Pts',(-3.63841388300005,12.2,1.81756433299999));
#309188=CARTESIAN_POINT('Ctrl Pts',(-3.63841388300005,5.2,1.81756433299999));
#309189=CARTESIAN_POINT('Ctrl Pts',(-3.63841388300005,2.2,1.81756433299999));
#309190=CARTESIAN_POINT('Ctrl Pts',(-3.63765945900006,12.2,1.81698724599999));
#309191=CARTESIAN_POINT('Ctrl Pts',(-3.63765945900006,5.2,1.81698724599999));
#309192=CARTESIAN_POINT('Ctrl Pts',(-3.63765945900006,2.2,1.81698724599999));
#309193=CARTESIAN_POINT('Ctrl Pts',(-3.63690875100006,12.2,1.81641447499999));
#309194=CARTESIAN_POINT('Ctrl Pts',(-3.63690875100006,5.2,1.81641447499999));
#309195=CARTESIAN_POINT('Ctrl Pts',(-3.63690875100006,2.2,1.81641447499999));
#309196=CARTESIAN_POINT('Ctrl Pts',(-3.63616177600006,12.2,1.81584601399999));
#309197=CARTESIAN_POINT('Ctrl Pts',(-3.63616177600006,5.2,1.81584601399999));
#309198=CARTESIAN_POINT('Ctrl Pts',(-3.63616177600006,2.2,1.81584601399999));
#309199=CARTESIAN_POINT('Ctrl Pts',(-3.63541855100006,12.2,1.81528186099999));
#309200=CARTESIAN_POINT('Ctrl Pts',(-3.63541855100006,5.2,1.81528186099999));
#309201=CARTESIAN_POINT('Ctrl Pts',(-3.63541855100006,2.2,1.81528186099999));
#309202=CARTESIAN_POINT('Ctrl Pts',(-3.63467909100006,12.2,1.81472201299998));
#309203=CARTESIAN_POINT('Ctrl Pts',(-3.63467909100006,5.2,1.81472201299998));
#309204=CARTESIAN_POINT('Ctrl Pts',(-3.63467909100006,2.2,1.81472201299998));
#309205=CARTESIAN_POINT('Ctrl Pts',(-3.63394341600006,12.2,1.81416646399999));
#309206=CARTESIAN_POINT('Ctrl Pts',(-3.63394341600006,5.2,1.81416646399999));
#309207=CARTESIAN_POINT('Ctrl Pts',(-3.63394341600006,2.2,1.81416646399999));
#309208=CARTESIAN_POINT('Ctrl Pts',(-3.63321154000006,12.2,1.81361521199999));
#309209=CARTESIAN_POINT('Ctrl Pts',(-3.63321154000006,5.2,1.81361521199999));
#309210=CARTESIAN_POINT('Ctrl Pts',(-3.63321154000006,2.2,1.81361521199999));
#309211=CARTESIAN_POINT('Ctrl Pts',(-3.63248348000006,12.2,1.81306825299998));
#309212=CARTESIAN_POINT('Ctrl Pts',(-3.63248348000006,5.2,1.81306825299998));
#309213=CARTESIAN_POINT('Ctrl Pts',(-3.63248348000006,2.2,1.81306825299998));
#309214=CARTESIAN_POINT('Ctrl Pts',(-3.63175925500006,12.2,1.81252557999999));
#309215=CARTESIAN_POINT('Ctrl Pts',(-3.63175925500006,5.2,1.81252557999999));
#309216=CARTESIAN_POINT('Ctrl Pts',(-3.63175925500006,2.2,1.81252557999999));
#309217=CARTESIAN_POINT('Ctrl Pts',(-3.63103888100006,12.2,1.81198719199998));
#309218=CARTESIAN_POINT('Ctrl Pts',(-3.63103888100006,5.2,1.81198719199998));
#309219=CARTESIAN_POINT('Ctrl Pts',(-3.63103888100006,2.2,1.81198719199998));
#309220=CARTESIAN_POINT('Ctrl Pts',(-3.63032237400006,12.2,1.81145308399998));
#309221=CARTESIAN_POINT('Ctrl Pts',(-3.63032237400006,5.2,1.81145308399998));
#309222=CARTESIAN_POINT('Ctrl Pts',(-3.63032237400006,2.2,1.81145308399998));
#309223=CARTESIAN_POINT('Ctrl Pts',(-3.62960975100005,12.2,1.81092325199999));
#309224=CARTESIAN_POINT('Ctrl Pts',(-3.62960975100005,5.2,1.81092325199999));
#309225=CARTESIAN_POINT('Ctrl Pts',(-3.62960975100005,2.2,1.81092325199999));
#309226=CARTESIAN_POINT('Ctrl Pts',(-3.62890103000006,12.2,1.81039769199999));
#309227=CARTESIAN_POINT('Ctrl Pts',(-3.62890103000006,5.2,1.81039769199999));
#309228=CARTESIAN_POINT('Ctrl Pts',(-3.62890103000006,2.2,1.81039769199999));
#309229=CARTESIAN_POINT('Ctrl Pts',(-3.62819622900005,12.2,1.80987640099998));
#309230=CARTESIAN_POINT('Ctrl Pts',(-3.62819622900005,5.2,1.80987640099998));
#309231=CARTESIAN_POINT('Ctrl Pts',(-3.62819622900005,2.2,1.80987640099998));
#309232=CARTESIAN_POINT('Ctrl Pts',(-3.62749536200006,12.2,1.80935937299999));
#309233=CARTESIAN_POINT('Ctrl Pts',(-3.62749536200006,5.2,1.80935937299999));
#309234=CARTESIAN_POINT('Ctrl Pts',(-3.62749536200006,2.2,1.80935937299999));
#309235=CARTESIAN_POINT('Ctrl Pts',(-3.62679845000006,12.2,1.80884660299999));
#309236=CARTESIAN_POINT('Ctrl Pts',(-3.62679845000006,5.2,1.80884660299999));
#309237=CARTESIAN_POINT('Ctrl Pts',(-3.62679845000006,2.2,1.80884660299999));
#309238=CARTESIAN_POINT('Ctrl Pts',(-3.62610550700006,12.2,1.80833808899999));
#309239=CARTESIAN_POINT('Ctrl Pts',(-3.62610550700006,5.2,1.80833808899999));
#309240=CARTESIAN_POINT('Ctrl Pts',(-3.62610550700006,2.2,1.80833808899999));
#309241=CARTESIAN_POINT('Ctrl Pts',(-3.62541655300006,12.2,1.80783382599999));
#309242=CARTESIAN_POINT('Ctrl Pts',(-3.62541655300006,5.2,1.80783382599999));
#309243=CARTESIAN_POINT('Ctrl Pts',(-3.62541655300006,2.2,1.80783382599999));
#309244=CARTESIAN_POINT('Ctrl Pts',(-3.62473160400006,12.2,1.80733380999999));
#309245=CARTESIAN_POINT('Ctrl Pts',(-3.62473160400006,5.2,1.80733380999999));
#309246=CARTESIAN_POINT('Ctrl Pts',(-3.62473160400006,2.2,1.80733380999999));
#309247=CARTESIAN_POINT('Ctrl Pts',(-3.62405067700006,12.2,1.80683803499999));
#309248=CARTESIAN_POINT('Ctrl Pts',(-3.62405067700006,5.2,1.80683803499999));
#309249=CARTESIAN_POINT('Ctrl Pts',(-3.62405067700006,2.2,1.80683803499999));
#309250=CARTESIAN_POINT('Ctrl Pts',(-3.62337379000006,12.2,1.80634649899998));
#309251=CARTESIAN_POINT('Ctrl Pts',(-3.62337379000006,5.2,1.80634649899998));
#309252=CARTESIAN_POINT('Ctrl Pts',(-3.62337379000006,2.2,1.80634649899998));
#309253=CARTESIAN_POINT('Ctrl Pts',(-3.62270096000006,12.2,1.80585919599999));
#309254=CARTESIAN_POINT('Ctrl Pts',(-3.62270096000006,5.2,1.80585919599999));
#309255=CARTESIAN_POINT('Ctrl Pts',(-3.62270096000006,2.2,1.80585919599999));
#309256=CARTESIAN_POINT('Ctrl Pts',(-3.62203220500006,12.2,1.80537612199998));
#309257=CARTESIAN_POINT('Ctrl Pts',(-3.62203220500006,5.2,1.80537612199998));
#309258=CARTESIAN_POINT('Ctrl Pts',(-3.62203220500006,2.2,1.80537612199998));
#309259=CARTESIAN_POINT('Ctrl Pts',(-3.62136754200006,12.2,1.80489727299999));
#309260=CARTESIAN_POINT('Ctrl Pts',(-3.62136754200006,5.2,1.80489727299999));
#309261=CARTESIAN_POINT('Ctrl Pts',(-3.62136754200006,2.2,1.80489727299999));
#309262=CARTESIAN_POINT('Ctrl Pts',(-3.62070698900006,12.2,1.80442264399999));
#309263=CARTESIAN_POINT('Ctrl Pts',(-3.62070698900006,5.2,1.80442264399999));
#309264=CARTESIAN_POINT('Ctrl Pts',(-3.62070698900006,2.2,1.80442264399999));
#309265=CARTESIAN_POINT('Ctrl Pts',(-3.62005056300006,12.2,1.80395222999998));
#309266=CARTESIAN_POINT('Ctrl Pts',(-3.62005056300006,5.2,1.80395222999998));
#309267=CARTESIAN_POINT('Ctrl Pts',(-3.62005056300006,2.2,1.80395222999998));
#309268=CARTESIAN_POINT('Ctrl Pts',(-3.61939828100006,12.2,1.80348602699999));
#309269=CARTESIAN_POINT('Ctrl Pts',(-3.61939828100006,5.2,1.80348602699999));
#309270=CARTESIAN_POINT('Ctrl Pts',(-3.61939828100006,2.2,1.80348602699999));
#309271=CARTESIAN_POINT('Ctrl Pts',(-3.61875016400006,12.2,1.80302403099999));
#309272=CARTESIAN_POINT('Ctrl Pts',(-3.61875016400006,5.2,1.80302403099999));
#309273=CARTESIAN_POINT('Ctrl Pts',(-3.61875016400006,2.2,1.80302403099999));
#309274=CARTESIAN_POINT('Ctrl Pts',(-3.61810622700006,12.2,1.80256623599998));
#309275=CARTESIAN_POINT('Ctrl Pts',(-3.61810622700006,5.2,1.80256623599998));
#309276=CARTESIAN_POINT('Ctrl Pts',(-3.61810622700006,2.2,1.80256623599998));
#309277=CARTESIAN_POINT('Ctrl Pts',(-3.61746648700006,12.2,1.80211263799999));
#309278=CARTESIAN_POINT('Ctrl Pts',(-3.61746648700006,5.2,1.80211263799999));
#309279=CARTESIAN_POINT('Ctrl Pts',(-3.61746648700006,2.2,1.80211263799999));
#309280=CARTESIAN_POINT('Ctrl Pts',(-3.61683096400006,12.2,1.80166323299999));
#309281=CARTESIAN_POINT('Ctrl Pts',(-3.61683096400006,5.2,1.80166323299999));
#309282=CARTESIAN_POINT('Ctrl Pts',(-3.61683096400006,2.2,1.80166323299999));
#309283=CARTESIAN_POINT('Ctrl Pts',(-3.61619967500006,12.2,1.80121801399999));
#309284=CARTESIAN_POINT('Ctrl Pts',(-3.61619967500006,5.2,1.80121801399999));
#309285=CARTESIAN_POINT('Ctrl Pts',(-3.61619967500006,2.2,1.80121801399999));
#309286=CARTESIAN_POINT('Ctrl Pts',(-3.61557263800006,12.2,1.80077697899999));
#309287=CARTESIAN_POINT('Ctrl Pts',(-3.61557263800006,5.2,1.80077697899999));
#309288=CARTESIAN_POINT('Ctrl Pts',(-3.61557263800006,2.2,1.80077697899999));
#309289=CARTESIAN_POINT('Ctrl Pts',(-3.61494987000006,12.2,1.80034012099998));
#309290=CARTESIAN_POINT('Ctrl Pts',(-3.61494987000006,5.2,1.80034012099998));
#309291=CARTESIAN_POINT('Ctrl Pts',(-3.61494987000006,2.2,1.80034012099998));
#309292=CARTESIAN_POINT('Ctrl Pts',(-3.61433139100006,12.2,1.79990743799999));
#309293=CARTESIAN_POINT('Ctrl Pts',(-3.61433139100006,5.2,1.79990743799999));
#309294=CARTESIAN_POINT('Ctrl Pts',(-3.61433139100006,2.2,1.79990743799999));
#309295=CARTESIAN_POINT('Ctrl Pts',(-3.61371721600006,12.2,1.79947892099999));
#309296=CARTESIAN_POINT('Ctrl Pts',(-3.61371721600006,5.2,1.79947892099999));
#309297=CARTESIAN_POINT('Ctrl Pts',(-3.61371721600006,2.2,1.79947892099999));
#309298=CARTESIAN_POINT('Ctrl Pts',(-3.61310736600006,12.2,1.79905456799998));
#309299=CARTESIAN_POINT('Ctrl Pts',(-3.61310736600006,5.2,1.79905456799998));
#309300=CARTESIAN_POINT('Ctrl Pts',(-3.61310736600006,2.2,1.79905456799998));
#309301=CARTESIAN_POINT('Ctrl Pts',(-3.61250185900006,12.2,1.79863437299999));
#309302=CARTESIAN_POINT('Ctrl Pts',(-3.61250185900006,5.2,1.79863437299999));
#309303=CARTESIAN_POINT('Ctrl Pts',(-3.61250185900006,2.2,1.79863437299999));
#309304=CARTESIAN_POINT('Ctrl Pts',(-3.61190071000006,12.2,1.79821833199998));
#309305=CARTESIAN_POINT('Ctrl Pts',(-3.61190071000006,5.2,1.79821833199998));
#309306=CARTESIAN_POINT('Ctrl Pts',(-3.61190071000006,2.2,1.79821833199998));
#309307=CARTESIAN_POINT('Ctrl Pts',(-3.61130394200006,12.2,1.79780643799999));
#309308=CARTESIAN_POINT('Ctrl Pts',(-3.61130394200006,5.2,1.79780643799999));
#309309=CARTESIAN_POINT('Ctrl Pts',(-3.61130394200006,2.2,1.79780643799999));
#309310=CARTESIAN_POINT('Ctrl Pts',(-3.61071156900006,12.2,1.79739868899999));
#309311=CARTESIAN_POINT('Ctrl Pts',(-3.61071156900006,5.2,1.79739868899999));
#309312=CARTESIAN_POINT('Ctrl Pts',(-3.61071156900006,2.2,1.79739868899999));
#309313=CARTESIAN_POINT('Ctrl Pts',(-3.61012361200006,12.2,1.79699507699999));
#309314=CARTESIAN_POINT('Ctrl Pts',(-3.61012361200006,5.2,1.79699507699999));
#309315=CARTESIAN_POINT('Ctrl Pts',(-3.61012361200006,2.2,1.79699507699999));
#309316=CARTESIAN_POINT('Ctrl Pts',(-3.60954008800006,12.2,1.79659559799999));
#309317=CARTESIAN_POINT('Ctrl Pts',(-3.60954008800006,5.2,1.79659559799999));
#309318=CARTESIAN_POINT('Ctrl Pts',(-3.60954008800006,2.2,1.79659559799999));
#309319=CARTESIAN_POINT('Ctrl Pts',(-3.60896101600006,12.2,1.79620024699998));
#309320=CARTESIAN_POINT('Ctrl Pts',(-3.60896101600006,5.2,1.79620024699998));
#309321=CARTESIAN_POINT('Ctrl Pts',(-3.60896101600006,2.2,1.79620024699998));
#309322=CARTESIAN_POINT('Ctrl Pts',(-3.60838641400006,12.2,1.79580901699998));
#309323=CARTESIAN_POINT('Ctrl Pts',(-3.60838641400006,5.2,1.79580901699998));
#309324=CARTESIAN_POINT('Ctrl Pts',(-3.60838641400006,2.2,1.79580901699998));
#309325=CARTESIAN_POINT('Ctrl Pts',(-3.60781630100006,12.2,1.79542190599999));
#309326=CARTESIAN_POINT('Ctrl Pts',(-3.60781630100006,5.2,1.79542190599999));
#309327=CARTESIAN_POINT('Ctrl Pts',(-3.60781630100006,2.2,1.79542190599999));
#309328=CARTESIAN_POINT('Ctrl Pts',(-3.60725069600006,12.2,1.79503890699999));
#309329=CARTESIAN_POINT('Ctrl Pts',(-3.60725069600006,5.2,1.79503890699999));
#309330=CARTESIAN_POINT('Ctrl Pts',(-3.60725069600006,2.2,1.79503890699999));
#309331=CARTESIAN_POINT('Ctrl Pts',(-3.60668961600005,12.2,1.79466001299998));
#309332=CARTESIAN_POINT('Ctrl Pts',(-3.60668961600005,5.2,1.79466001299998));
#309333=CARTESIAN_POINT('Ctrl Pts',(-3.60668961600005,2.2,1.79466001299998));
#309334=CARTESIAN_POINT('Ctrl Pts',(-3.60613308100006,12.2,1.79428522199998));
#309335=CARTESIAN_POINT('Ctrl Pts',(-3.60613308100006,5.2,1.79428522199998));
#309336=CARTESIAN_POINT('Ctrl Pts',(-3.60613308100006,2.2,1.79428522199998));
#309337=CARTESIAN_POINT('Ctrl Pts',(-3.60558110800006,12.2,1.79391452599999));
#309338=CARTESIAN_POINT('Ctrl Pts',(-3.60558110800006,5.2,1.79391452599999));
#309339=CARTESIAN_POINT('Ctrl Pts',(-3.60558110800006,2.2,1.79391452599999));
#309340=CARTESIAN_POINT('Ctrl Pts',(-3.60503372000006,12.2,1.79354792099998));
#309341=CARTESIAN_POINT('Ctrl Pts',(-3.60503372000006,5.2,1.79354792099998));
#309342=CARTESIAN_POINT('Ctrl Pts',(-3.60503372000006,2.2,1.79354792099998));
#309343=CARTESIAN_POINT('Ctrl Pts',(-3.60449093000006,12.2,1.79318539999999));
#309344=CARTESIAN_POINT('Ctrl Pts',(-3.60449093000006,5.2,1.79318539999999));
#309345=CARTESIAN_POINT('Ctrl Pts',(-3.60449093000006,2.2,1.79318539999999));
#309346=CARTESIAN_POINT('Ctrl Pts',(-3.60395276000006,12.2,1.79282695799999));
#309347=CARTESIAN_POINT('Ctrl Pts',(-3.60395276000006,5.2,1.79282695799999));
#309348=CARTESIAN_POINT('Ctrl Pts',(-3.60395276000006,2.2,1.79282695799999));
#309349=CARTESIAN_POINT('Ctrl Pts',(-3.60341923000006,12.2,1.79247259099999));
#309350=CARTESIAN_POINT('Ctrl Pts',(-3.60341923000006,5.2,1.79247259099999));
#309351=CARTESIAN_POINT('Ctrl Pts',(-3.60341923000006,2.2,1.79247259099999));
#309352=CARTESIAN_POINT('Ctrl Pts',(-3.60289035500006,12.2,1.79212229099999));
#309353=CARTESIAN_POINT('Ctrl Pts',(-3.60289035500006,5.2,1.79212229099999));
#309354=CARTESIAN_POINT('Ctrl Pts',(-3.60289035500006,2.2,1.79212229099999));
#309355=CARTESIAN_POINT('Ctrl Pts',(-3.60236615800006,12.2,1.79177605499998));
#309356=CARTESIAN_POINT('Ctrl Pts',(-3.60236615800006,5.2,1.79177605499998));
#309357=CARTESIAN_POINT('Ctrl Pts',(-3.60236615800006,2.2,1.79177605499998));
#309358=CARTESIAN_POINT('Ctrl Pts',(-3.60184665600006,12.2,1.79143387499999));
#309359=CARTESIAN_POINT('Ctrl Pts',(-3.60184665600006,5.2,1.79143387499999));
#309360=CARTESIAN_POINT('Ctrl Pts',(-3.60184665600006,2.2,1.79143387499999));
#309361=CARTESIAN_POINT('Ctrl Pts',(-3.60133186900006,12.2,1.79109574699998));
#309362=CARTESIAN_POINT('Ctrl Pts',(-3.60133186900006,5.2,1.79109574699998));
#309363=CARTESIAN_POINT('Ctrl Pts',(-3.60133186900006,2.2,1.79109574699998));
#309364=CARTESIAN_POINT('Ctrl Pts',(-3.60082181600006,12.2,1.79076166399998));
#309365=CARTESIAN_POINT('Ctrl Pts',(-3.60082181600006,5.2,1.79076166399998));
#309366=CARTESIAN_POINT('Ctrl Pts',(-3.60082181600006,2.2,1.79076166399998));
#309367=CARTESIAN_POINT('Ctrl Pts',(-3.60031651500006,12.2,1.79043161999999));
#309368=CARTESIAN_POINT('Ctrl Pts',(-3.60031651500006,5.2,1.79043161999999));
#309369=CARTESIAN_POINT('Ctrl Pts',(-3.60031651500006,2.2,1.79043161999999));
#309370=CARTESIAN_POINT('Ctrl Pts',(-3.59981598500006,12.2,1.79010560999998));
#309371=CARTESIAN_POINT('Ctrl Pts',(-3.59981598500006,5.2,1.79010560999998));
#309372=CARTESIAN_POINT('Ctrl Pts',(-3.59981598500006,2.2,1.79010560999998));
#309373=CARTESIAN_POINT('Ctrl Pts',(-3.59932024800006,12.2,1.78978362799999));
#309374=CARTESIAN_POINT('Ctrl Pts',(-3.59932024800006,5.2,1.78978362799999));
#309375=CARTESIAN_POINT('Ctrl Pts',(-3.59932024800006,2.2,1.78978362799999));
#309376=CARTESIAN_POINT('Ctrl Pts',(-3.59882932100006,12.2,1.78946566799999));
#309377=CARTESIAN_POINT('Ctrl Pts',(-3.59882932100006,5.2,1.78946566799999));
#309378=CARTESIAN_POINT('Ctrl Pts',(-3.59882932100006,2.2,1.78946566799999));
#309379=CARTESIAN_POINT('Ctrl Pts',(-3.59834322400006,12.2,1.78915172399998));
#309380=CARTESIAN_POINT('Ctrl Pts',(-3.59834322400006,5.2,1.78915172399998));
#309381=CARTESIAN_POINT('Ctrl Pts',(-3.59834322400006,2.2,1.78915172399998));
#309382=CARTESIAN_POINT('Ctrl Pts',(-3.59786197700006,12.2,1.78884178999999));
#309383=CARTESIAN_POINT('Ctrl Pts',(-3.59786197700006,5.2,1.78884178999999));
#309384=CARTESIAN_POINT('Ctrl Pts',(-3.59786197700006,2.2,1.78884178999999));
#309385=CARTESIAN_POINT('Ctrl Pts',(-3.59738559900006,12.2,1.78853585999999));
#309386=CARTESIAN_POINT('Ctrl Pts',(-3.59738559900006,5.2,1.78853585999999));
#309387=CARTESIAN_POINT('Ctrl Pts',(-3.59738559900006,2.2,1.78853585999999));
#309388=CARTESIAN_POINT('Ctrl Pts',(-3.59691410800006,12.2,1.78823392699998));
#309389=CARTESIAN_POINT('Ctrl Pts',(-3.59691410800006,5.2,1.78823392699998));
#309390=CARTESIAN_POINT('Ctrl Pts',(-3.59691410800006,2.2,1.78823392699998));
#309391=CARTESIAN_POINT('Ctrl Pts',(-3.59644752700006,12.2,1.78793598599999));
#309392=CARTESIAN_POINT('Ctrl Pts',(-3.59644752700006,5.2,1.78793598599999));
#309393=CARTESIAN_POINT('Ctrl Pts',(-3.59644752700006,2.2,1.78793598599999));
#309394=CARTESIAN_POINT('Ctrl Pts',(-3.59598587300006,12.2,1.78764203199998));
#309395=CARTESIAN_POINT('Ctrl Pts',(-3.59598587300006,5.2,1.78764203199998));
#309396=CARTESIAN_POINT('Ctrl Pts',(-3.59598587300006,2.2,1.78764203199998));
#309397=CARTESIAN_POINT('Ctrl Pts',(-3.59552916600006,12.2,1.78735205599999));
#309398=CARTESIAN_POINT('Ctrl Pts',(-3.59552916600006,5.2,1.78735205599999));
#309399=CARTESIAN_POINT('Ctrl Pts',(-3.59552916600006,2.2,1.78735205599999));
#309400=CARTESIAN_POINT('Ctrl Pts',(-3.59507742600006,12.2,1.78706605299999));
#309401=CARTESIAN_POINT('Ctrl Pts',(-3.59507742600006,5.2,1.78706605299999));
#309402=CARTESIAN_POINT('Ctrl Pts',(-3.59507742600006,2.2,1.78706605299999));
#309403=CARTESIAN_POINT('Ctrl Pts',(-3.59463067400006,12.2,1.78678401699999));
#309404=CARTESIAN_POINT('Ctrl Pts',(-3.59463067400006,5.2,1.78678401699999));
#309405=CARTESIAN_POINT('Ctrl Pts',(-3.59463067400006,2.2,1.78678401699999));
#309406=CARTESIAN_POINT('Ctrl Pts',(-3.59418892800006,12.2,1.78650594099999));
#309407=CARTESIAN_POINT('Ctrl Pts',(-3.59418892800006,5.2,1.78650594099999));
#309408=CARTESIAN_POINT('Ctrl Pts',(-3.59418892800006,2.2,1.78650594099999));
#309409=CARTESIAN_POINT('Ctrl Pts',(-3.59375221000006,12.2,1.78623181999999));
#309410=CARTESIAN_POINT('Ctrl Pts',(-3.59375221000006,5.2,1.78623181999999));
#309411=CARTESIAN_POINT('Ctrl Pts',(-3.59375221000006,2.2,1.78623181999999));
#309412=CARTESIAN_POINT('Ctrl Pts',(-3.59332053700006,12.2,1.78596164699998));
#309413=CARTESIAN_POINT('Ctrl Pts',(-3.59332053700006,5.2,1.78596164699998));
#309414=CARTESIAN_POINT('Ctrl Pts',(-3.59332053700006,2.2,1.78596164699998));
#309415=CARTESIAN_POINT('Ctrl Pts',(-3.59289393100005,12.2,1.78569541399999));
#309416=CARTESIAN_POINT('Ctrl Pts',(-3.59289393100005,5.2,1.78569541399999));
#309417=CARTESIAN_POINT('Ctrl Pts',(-3.59289393100005,2.2,1.78569541399999));
#309418=CARTESIAN_POINT('Ctrl Pts',(-3.59247241200006,12.2,1.78543311499999));
#309419=CARTESIAN_POINT('Ctrl Pts',(-3.59247241200006,5.2,1.78543311499999));
#309420=CARTESIAN_POINT('Ctrl Pts',(-3.59247241200006,2.2,1.78543311499999));
#309421=CARTESIAN_POINT('Ctrl Pts',(-3.59205600100006,12.2,1.78517474599999));
#309422=CARTESIAN_POINT('Ctrl Pts',(-3.59205600100006,5.2,1.78517474599999));
#309423=CARTESIAN_POINT('Ctrl Pts',(-3.59205600100006,2.2,1.78517474599999));
#309424=CARTESIAN_POINT('Ctrl Pts',(-3.59164471600006,12.2,1.78492029699999));
#309425=CARTESIAN_POINT('Ctrl Pts',(-3.59164471600006,5.2,1.78492029699999));
#309426=CARTESIAN_POINT('Ctrl Pts',(-3.59164471600006,2.2,1.78492029699999));
#309427=CARTESIAN_POINT('Ctrl Pts',(-3.59123857800006,12.2,1.78466976299998));
#309428=CARTESIAN_POINT('Ctrl Pts',(-3.59123857800006,5.2,1.78466976299998));
#309429=CARTESIAN_POINT('Ctrl Pts',(-3.59123857800006,2.2,1.78466976299998));
#309430=CARTESIAN_POINT('Ctrl Pts',(-3.59083760900006,12.2,1.78442313799998));
#309431=CARTESIAN_POINT('Ctrl Pts',(-3.59083760900006,5.2,1.78442313799998));
#309432=CARTESIAN_POINT('Ctrl Pts',(-3.59083760900006,2.2,1.78442313799998));
#309433=CARTESIAN_POINT('Ctrl Pts',(-3.59044182600006,12.2,1.78418041299999));
#309434=CARTESIAN_POINT('Ctrl Pts',(-3.59044182600006,5.2,1.78418041299999));
#309435=CARTESIAN_POINT('Ctrl Pts',(-3.59044182600006,2.2,1.78418041299999));
#309436=CARTESIAN_POINT('Ctrl Pts',(-3.59005125300006,12.2,1.78394158299998));
#309437=CARTESIAN_POINT('Ctrl Pts',(-3.59005125300006,5.2,1.78394158299998));
#309438=CARTESIAN_POINT('Ctrl Pts',(-3.59005125300006,2.2,1.78394158299998));
#309439=CARTESIAN_POINT('Ctrl Pts',(-3.58966590900006,12.2,1.78370664199999));
#309440=CARTESIAN_POINT('Ctrl Pts',(-3.58966590900006,5.2,1.78370664199999));
#309441=CARTESIAN_POINT('Ctrl Pts',(-3.58966590900006,2.2,1.78370664199999));
#309442=CARTESIAN_POINT('Ctrl Pts',(-3.58928581300006,12.2,1.78347557999999));
#309443=CARTESIAN_POINT('Ctrl Pts',(-3.58928581300006,5.2,1.78347557999999));
#309444=CARTESIAN_POINT('Ctrl Pts',(-3.58928581300006,2.2,1.78347557999999));
#309445=CARTESIAN_POINT('Ctrl Pts',(-3.58891098800005,12.2,1.78324839299998));
#309446=CARTESIAN_POINT('Ctrl Pts',(-3.58891098800005,5.2,1.78324839299998));
#309447=CARTESIAN_POINT('Ctrl Pts',(-3.58891098800005,2.2,1.78324839299998));
#309448=CARTESIAN_POINT('Ctrl Pts',(-3.58854145300006,12.2,1.78302507299998));
#309449=CARTESIAN_POINT('Ctrl Pts',(-3.58854145300006,5.2,1.78302507299998));
#309450=CARTESIAN_POINT('Ctrl Pts',(-3.58854145300006,2.2,1.78302507299998));
#309451=CARTESIAN_POINT('Ctrl Pts',(-3.58817723000006,12.2,1.78280561299998));
#309452=CARTESIAN_POINT('Ctrl Pts',(-3.58817723000006,5.2,1.78280561299998));
#309453=CARTESIAN_POINT('Ctrl Pts',(-3.58817723000006,2.2,1.78280561299998));
#309454=CARTESIAN_POINT('Ctrl Pts',(-3.58781834000006,12.2,1.78259000599999));
#309455=CARTESIAN_POINT('Ctrl Pts',(-3.58781834000006,5.2,1.78259000599999));
#309456=CARTESIAN_POINT('Ctrl Pts',(-3.58781834000006,2.2,1.78259000599999));
#309457=CARTESIAN_POINT('Ctrl Pts',(-3.58746480100006,12.2,1.78237824499998));
#309458=CARTESIAN_POINT('Ctrl Pts',(-3.58746480100006,5.2,1.78237824499998));
#309459=CARTESIAN_POINT('Ctrl Pts',(-3.58746480100006,2.2,1.78237824499998));
#309460=CARTESIAN_POINT('Ctrl Pts',(-3.58711663600006,12.2,1.78217032199999));
#309461=CARTESIAN_POINT('Ctrl Pts',(-3.58711663600006,5.2,1.78217032199999));
#309462=CARTESIAN_POINT('Ctrl Pts',(-3.58711663600006,2.2,1.78217032199999));
#309463=CARTESIAN_POINT('Ctrl Pts',(-3.58677386600006,12.2,1.78196623099999));
#309464=CARTESIAN_POINT('Ctrl Pts',(-3.58677386600006,5.2,1.78196623099999));
#309465=CARTESIAN_POINT('Ctrl Pts',(-3.58677386600006,2.2,1.78196623099999));
#309466=CARTESIAN_POINT('Ctrl Pts',(-3.58643651200006,12.2,1.78176596399998));
#309467=CARTESIAN_POINT('Ctrl Pts',(-3.58643651200006,5.2,1.78176596399998));
#309468=CARTESIAN_POINT('Ctrl Pts',(-3.58643651200006,2.2,1.78176596399998));
#309469=CARTESIAN_POINT('Ctrl Pts',(-3.58610459400006,12.2,1.78156951399998));
#309470=CARTESIAN_POINT('Ctrl Pts',(-3.58610459400006,5.2,1.78156951399998));
#309471=CARTESIAN_POINT('Ctrl Pts',(-3.58610459400006,2.2,1.78156951399998));
#309472=CARTESIAN_POINT('Ctrl Pts',(-3.58577813500006,12.2,1.78137687299999));
#309473=CARTESIAN_POINT('Ctrl Pts',(-3.58577813500006,5.2,1.78137687299999));
#309474=CARTESIAN_POINT('Ctrl Pts',(-3.58577813500006,2.2,1.78137687299999));
#309475=CARTESIAN_POINT('Ctrl Pts',(-3.58545715400005,12.2,1.78118803499999));
#309476=CARTESIAN_POINT('Ctrl Pts',(-3.58545715400005,5.2,1.78118803499999));
#309477=CARTESIAN_POINT('Ctrl Pts',(-3.58545715400005,2.2,1.78118803499999));
#309478=CARTESIAN_POINT('Ctrl Pts',(-3.58514167400006,12.2,1.78100299199999));
#309479=CARTESIAN_POINT('Ctrl Pts',(-3.58514167400006,5.2,1.78100299199999));
#309480=CARTESIAN_POINT('Ctrl Pts',(-3.58514167400006,2.2,1.78100299199999));
#309481=CARTESIAN_POINT('Ctrl Pts',(-3.58483171500006,12.2,1.78082173499998));
#309482=CARTESIAN_POINT('Ctrl Pts',(-3.58483171500006,5.2,1.78082173499998));
#309483=CARTESIAN_POINT('Ctrl Pts',(-3.58483171500006,2.2,1.78082173499998));
#309484=CARTESIAN_POINT('Ctrl Pts',(-3.58452729900006,12.2,1.78064425899999));
#309485=CARTESIAN_POINT('Ctrl Pts',(-3.58452729900006,5.2,1.78064425899999));
#309486=CARTESIAN_POINT('Ctrl Pts',(-3.58452729900006,2.2,1.78064425899999));
#309487=CARTESIAN_POINT('Ctrl Pts',(-3.58422844800006,12.2,1.78047055499999));
#309488=CARTESIAN_POINT('Ctrl Pts',(-3.58422844800006,5.2,1.78047055499999));
#309489=CARTESIAN_POINT('Ctrl Pts',(-3.58422844800006,2.2,1.78047055499999));
#309490=CARTESIAN_POINT('Ctrl Pts',(-3.58393518200006,12.2,1.78030061499999));
#309491=CARTESIAN_POINT('Ctrl Pts',(-3.58393518200006,5.2,1.78030061499999));
#309492=CARTESIAN_POINT('Ctrl Pts',(-3.58393518200006,2.2,1.78030061499999));
#309493=CARTESIAN_POINT('Ctrl Pts',(-3.58364752400006,12.2,1.78013443199998));
#309494=CARTESIAN_POINT('Ctrl Pts',(-3.58364752400006,5.2,1.78013443199998));
#309495=CARTESIAN_POINT('Ctrl Pts',(-3.58364752400006,2.2,1.78013443199998));
#309496=CARTESIAN_POINT('Ctrl Pts',(-3.58336549500006,12.2,1.77997199799998));
#309497=CARTESIAN_POINT('Ctrl Pts',(-3.58336549500006,5.2,1.77997199799998));
#309498=CARTESIAN_POINT('Ctrl Pts',(-3.58336549500006,2.2,1.77997199799998));
#309499=CARTESIAN_POINT('Ctrl Pts',(-3.58308911600006,12.2,1.77981330499998));
#309500=CARTESIAN_POINT('Ctrl Pts',(-3.58308911600006,5.2,1.77981330499998));
#309501=CARTESIAN_POINT('Ctrl Pts',(-3.58308911600006,2.2,1.77981330499998));
#309502=CARTESIAN_POINT('Ctrl Pts',(-3.58281840900006,12.2,1.77965834599998));
#309503=CARTESIAN_POINT('Ctrl Pts',(-3.58281840900006,5.2,1.77965834599998));
#309504=CARTESIAN_POINT('Ctrl Pts',(-3.58281840900006,2.2,1.77965834599998));
#309505=CARTESIAN_POINT('Ctrl Pts',(-3.58255339700006,12.2,1.77950711299999));
#309506=CARTESIAN_POINT('Ctrl Pts',(-3.58255339700006,5.2,1.77950711299999));
#309507=CARTESIAN_POINT('Ctrl Pts',(-3.58255339700006,2.2,1.77950711299999));
#309508=CARTESIAN_POINT('Ctrl Pts',(-3.58229410100006,12.2,1.77935959699999));
#309509=CARTESIAN_POINT('Ctrl Pts',(-3.58229410100006,5.2,1.77935959699999));
#309510=CARTESIAN_POINT('Ctrl Pts',(-3.58229410100006,2.2,1.77935959699999));
#309511=CARTESIAN_POINT('Ctrl Pts',(-3.58204054400006,12.2,1.77921579099999));
#309512=CARTESIAN_POINT('Ctrl Pts',(-3.58204054400006,5.2,1.77921579099999));
#309513=CARTESIAN_POINT('Ctrl Pts',(-3.58204054400006,2.2,1.77921579099999));
#309514=CARTESIAN_POINT('Ctrl Pts',(-3.58179274500006,12.2,1.77907568499998));
#309515=CARTESIAN_POINT('Ctrl Pts',(-3.58179274500006,5.2,1.77907568499998));
#309516=CARTESIAN_POINT('Ctrl Pts',(-3.58179274500006,2.2,1.77907568499998));
#309517=CARTESIAN_POINT('Ctrl Pts',(-3.58155073000006,12.2,1.77893927499999));
#309518=CARTESIAN_POINT('Ctrl Pts',(-3.58155073000006,5.2,1.77893927499999));
#309519=CARTESIAN_POINT('Ctrl Pts',(-3.58155073000006,2.2,1.77893927499999));
#309520=CARTESIAN_POINT('Ctrl Pts',(-3.58131451900006,12.2,1.77880654899999));
#309521=CARTESIAN_POINT('Ctrl Pts',(-3.58131451900006,5.2,1.77880654899999));
#309522=CARTESIAN_POINT('Ctrl Pts',(-3.58131451900006,2.2,1.77880654899999));
#309523=CARTESIAN_POINT('Ctrl Pts',(-3.58108413300006,12.2,1.77867749899999));
#309524=CARTESIAN_POINT('Ctrl Pts',(-3.58108413300006,5.2,1.77867749899999));
#309525=CARTESIAN_POINT('Ctrl Pts',(-3.58108413300006,2.2,1.77867749899999));
#309526=CARTESIAN_POINT('Ctrl Pts',(-3.58085959700006,12.2,1.77855211999999));
#309527=CARTESIAN_POINT('Ctrl Pts',(-3.58085959700006,5.2,1.77855211999999));
#309528=CARTESIAN_POINT('Ctrl Pts',(-3.58085959700006,2.2,1.77855211999999));
#309529=CARTESIAN_POINT('Ctrl Pts',(-3.58064093200006,12.2,1.77843039999999));
#309530=CARTESIAN_POINT('Ctrl Pts',(-3.58064093200006,5.2,1.77843039999999));
#309531=CARTESIAN_POINT('Ctrl Pts',(-3.58064093200006,2.2,1.77843039999999));
#309532=CARTESIAN_POINT('Ctrl Pts',(-3.58042816000006,12.2,1.77831233299999));
#309533=CARTESIAN_POINT('Ctrl Pts',(-3.58042816000006,5.2,1.77831233299999));
#309534=CARTESIAN_POINT('Ctrl Pts',(-3.58042816000006,2.2,1.77831233299999));
#309535=CARTESIAN_POINT('Ctrl Pts',(-3.58022130400006,12.2,1.77819790999999));
#309536=CARTESIAN_POINT('Ctrl Pts',(-3.58022130400006,5.2,1.77819790999999));
#309537=CARTESIAN_POINT('Ctrl Pts',(-3.58022130400006,2.2,1.77819790999999));
#309538=CARTESIAN_POINT('Ctrl Pts',(-3.58002038700006,12.2,1.77808712199999));
#309539=CARTESIAN_POINT('Ctrl Pts',(-3.58002038700006,5.2,1.77808712199999));
#309540=CARTESIAN_POINT('Ctrl Pts',(-3.58002038700006,2.2,1.77808712199999));
#309541=CARTESIAN_POINT('Ctrl Pts',(-3.57982543100006,12.2,1.77797995999999));
#309542=CARTESIAN_POINT('Ctrl Pts',(-3.57982543100006,5.2,1.77797995999999));
#309543=CARTESIAN_POINT('Ctrl Pts',(-3.57982543100006,2.2,1.77797995999999));
#309544=CARTESIAN_POINT('Ctrl Pts',(-3.57963645700006,12.2,1.77787641799998));
#309545=CARTESIAN_POINT('Ctrl Pts',(-3.57963645700006,5.2,1.77787641799998));
#309546=CARTESIAN_POINT('Ctrl Pts',(-3.57963645700006,2.2,1.77787641799998));
#309547=CARTESIAN_POINT('Ctrl Pts',(-3.57945349100006,12.2,1.77777648499998));
#309548=CARTESIAN_POINT('Ctrl Pts',(-3.57945349100006,5.2,1.77777648499998));
#309549=CARTESIAN_POINT('Ctrl Pts',(-3.57945349100006,2.2,1.77777648499998));
#309550=CARTESIAN_POINT('Ctrl Pts',(-3.57927655500006,12.2,1.77768015199999));
#309551=CARTESIAN_POINT('Ctrl Pts',(-3.57927655500006,5.2,1.77768015199999));
#309552=CARTESIAN_POINT('Ctrl Pts',(-3.57927655500006,2.2,1.77768015199999));
#309553=CARTESIAN_POINT('Ctrl Pts',(-3.57910567000006,12.2,1.77758741099999));
#309554=CARTESIAN_POINT('Ctrl Pts',(-3.57910567000006,5.2,1.77758741099999));
#309555=CARTESIAN_POINT('Ctrl Pts',(-3.57910567000006,2.2,1.77758741099999));
#309556=CARTESIAN_POINT('Ctrl Pts',(-3.57894086200006,12.2,1.77749825399999));
#309557=CARTESIAN_POINT('Ctrl Pts',(-3.57894086200006,5.2,1.77749825399999));
#309558=CARTESIAN_POINT('Ctrl Pts',(-3.57894086200006,2.2,1.77749825399999));
#309559=CARTESIAN_POINT('Ctrl Pts',(-3.57878215200006,12.2,1.77741267099998));
#309560=CARTESIAN_POINT('Ctrl Pts',(-3.57878215200006,5.2,1.77741267099998));
#309561=CARTESIAN_POINT('Ctrl Pts',(-3.57878215200006,2.2,1.77741267099998));
#309562=CARTESIAN_POINT('Ctrl Pts',(-3.57862956300006,12.2,1.77733065399998));
#309563=CARTESIAN_POINT('Ctrl Pts',(-3.57862956300006,5.2,1.77733065399998));
#309564=CARTESIAN_POINT('Ctrl Pts',(-3.57862956300006,2.2,1.77733065399998));
#309565=CARTESIAN_POINT('Ctrl Pts',(-3.57848311700006,12.2,1.77725219399999));
#309566=CARTESIAN_POINT('Ctrl Pts',(-3.57848311700006,5.2,1.77725219399999));
#309567=CARTESIAN_POINT('Ctrl Pts',(-3.57848311700006,2.2,1.77725219399999));
#309568=CARTESIAN_POINT('Ctrl Pts',(-3.57834283900006,12.2,1.77717728099998));
#309569=CARTESIAN_POINT('Ctrl Pts',(-3.57834283900006,5.2,1.77717728099998));
#309570=CARTESIAN_POINT('Ctrl Pts',(-3.57834283900006,2.2,1.77717728099998));
#309571=CARTESIAN_POINT('Ctrl Pts',(-3.57820875100006,12.2,1.77710590699999));
#309572=CARTESIAN_POINT('Ctrl Pts',(-3.57820875100006,5.2,1.77710590699999));
#309573=CARTESIAN_POINT('Ctrl Pts',(-3.57820875100006,2.2,1.77710590699999));
#309574=CARTESIAN_POINT('Ctrl Pts',(-3.57808087800006,12.2,1.77703806299998));
#309575=CARTESIAN_POINT('Ctrl Pts',(-3.57808087800006,5.2,1.77703806299998));
#309576=CARTESIAN_POINT('Ctrl Pts',(-3.57808087800006,2.2,1.77703806299998));
#309577=CARTESIAN_POINT('Ctrl Pts',(-3.57795924500006,12.2,1.77697373799999));
#309578=CARTESIAN_POINT('Ctrl Pts',(-3.57795924500006,5.2,1.77697373799999));
#309579=CARTESIAN_POINT('Ctrl Pts',(-3.57795924500006,2.2,1.77697373799999));
#309580=CARTESIAN_POINT('Ctrl Pts',(-3.57784387600006,12.2,1.77691292299999));
#309581=CARTESIAN_POINT('Ctrl Pts',(-3.57784387600006,5.2,1.77691292299999));
#309582=CARTESIAN_POINT('Ctrl Pts',(-3.57784387600006,2.2,1.77691292299999));
#309583=CARTESIAN_POINT('Ctrl Pts',(-3.57773479500006,12.2,1.77685560799999));
#309584=CARTESIAN_POINT('Ctrl Pts',(-3.57773479500006,5.2,1.77685560799999));
#309585=CARTESIAN_POINT('Ctrl Pts',(-3.57773479500006,2.2,1.77685560799999));
#309586=CARTESIAN_POINT('Ctrl Pts',(-3.57763202200006,12.2,1.77680178599998));
#309587=CARTESIAN_POINT('Ctrl Pts',(-3.57763202200006,5.2,1.77680178599998));
#309588=CARTESIAN_POINT('Ctrl Pts',(-3.57763202200006,2.2,1.77680178599998));
#309589=CARTESIAN_POINT('Ctrl Pts',(-3.57753557800006,12.2,1.77675144799998));
#309590=CARTESIAN_POINT('Ctrl Pts',(-3.57753557800006,5.2,1.77675144799998));
#309591=CARTESIAN_POINT('Ctrl Pts',(-3.57753557800006,2.2,1.77675144799998));
#309592=CARTESIAN_POINT('Ctrl Pts',(-3.57744548500006,12.2,1.77670458499998));
#309593=CARTESIAN_POINT('Ctrl Pts',(-3.57744548500006,5.2,1.77670458499998));
#309594=CARTESIAN_POINT('Ctrl Pts',(-3.57744548500006,2.2,1.77670458499998));
#309595=CARTESIAN_POINT('Ctrl Pts',(-3.57736176800006,12.2,1.77666118799999));
#309596=CARTESIAN_POINT('Ctrl Pts',(-3.57736176800006,5.2,1.77666118799999));
#309597=CARTESIAN_POINT('Ctrl Pts',(-3.57736176800006,2.2,1.77666118799999));
#309598=CARTESIAN_POINT('Ctrl Pts',(-3.57728445400006,12.2,1.77662124499999));
#309599=CARTESIAN_POINT('Ctrl Pts',(-3.57728445400006,5.2,1.77662124499999));
#309600=CARTESIAN_POINT('Ctrl Pts',(-3.57728445400006,2.2,1.77662124499999));
#309601=CARTESIAN_POINT('Ctrl Pts',(-3.57721357500006,12.2,1.77658474499998));
#309602=CARTESIAN_POINT('Ctrl Pts',(-3.57721357500006,5.2,1.77658474499998));
#309603=CARTESIAN_POINT('Ctrl Pts',(-3.57721357500006,2.2,1.77658474499998));
#309604=CARTESIAN_POINT('Ctrl Pts',(-3.57714916000006,12.2,1.77655167399998));
#309605=CARTESIAN_POINT('Ctrl Pts',(-3.57714916000006,5.2,1.77655167399998));
#309606=CARTESIAN_POINT('Ctrl Pts',(-3.57714916000006,2.2,1.77655167399998));
#309607=CARTESIAN_POINT('Ctrl Pts',(-3.57709123600006,12.2,1.77652202299999));
#309608=CARTESIAN_POINT('Ctrl Pts',(-3.57709123600006,5.2,1.77652202299999));
#309609=CARTESIAN_POINT('Ctrl Pts',(-3.57709123600006,2.2,1.77652202299999));
#309610=CARTESIAN_POINT('Ctrl Pts',(-3.57703982100006,12.2,1.77649578199999));
#309611=CARTESIAN_POINT('Ctrl Pts',(-3.57703982100006,5.2,1.77649578199999));
#309612=CARTESIAN_POINT('Ctrl Pts',(-3.57703982100006,2.2,1.77649578199999));
#309613=CARTESIAN_POINT('Ctrl Pts',(-3.57699012332173,12.2,1.77647050473256));
#309614=CARTESIAN_POINT('Ctrl Pts',(-3.57699012332173,5.2,1.77647050473256));
#309615=CARTESIAN_POINT('Ctrl Pts',(-3.57699012332173,2.2,1.77647050473256));
#309616=CARTESIAN_POINT('Ctrl Pts',(-3.5769561191391,12.2,1.77645329379262));
#309617=CARTESIAN_POINT('Ctrl Pts',(-3.5769561191391,5.2,1.77645329379262));
#309618=CARTESIAN_POINT('Ctrl Pts',(-3.5769561191391,2.2,1.77645329379262));
#309619=CARTESIAN_POINT('Ctrl Pts',(-3.57693369172082,12.2,1.77644200373862));
#309620=CARTESIAN_POINT('Ctrl Pts',(-3.57693369172082,5.2,1.77644200373862));
#309621=CARTESIAN_POINT('Ctrl Pts',(-3.57693369172082,2.2,1.77644200373862));
#309622=CARTESIAN_POINT('Ctrl Pts',(-3.57691970642208,12.2,1.77643500294693));
#309623=CARTESIAN_POINT('Ctrl Pts',(-3.57691970642208,5.2,1.77643500294693));
#309624=CARTESIAN_POINT('Ctrl Pts',(-3.57691970642208,2.2,1.77643500294693));
#309625=CARTESIAN_POINT('Ctrl Pts',(-3.57691107200006,12.2,1.77643067499998));
#309626=CARTESIAN_POINT('Ctrl Pts',(-3.57691107200006,5.2,1.77643067499998));
#309627=CARTESIAN_POINT('Ctrl Pts',(-3.57691107200006,2.2,1.77643067499998));
#309628=CARTESIAN_POINT('',(-3.57691116300006,2.7,1.77643049499998));
#309629=CARTESIAN_POINT('',(-3.57691116300006,12.2,1.77643049499999));
#309630=CARTESIAN_POINT('Ctrl Pts',(-4.09164015000006,2.7,2.41267090399998));
#309631=CARTESIAN_POINT('Ctrl Pts',(-3.98263969989265,2.7,2.19591905262488));
#309632=CARTESIAN_POINT('Ctrl Pts',(-3.86694481153583,2.6999999999955,2.0417626137312));
#309633=CARTESIAN_POINT('Ctrl Pts',(-3.66335261251423,2.6999999999955,1.82497302201057));
#309634=CARTESIAN_POINT('Ctrl Pts',(-3.58821589879921,2.7,1.78227875956844));
#309635=CARTESIAN_POINT('Ctrl Pts',(-3.57721236596159,2.7,1.77658390024682));
#309636=CARTESIAN_POINT('Ctrl Pts',(-3.57706216165585,2.7,1.77650640769084));
#309637=CARTESIAN_POINT('Ctrl Pts',(-3.57691107226376,2.7,1.77643067513216));
#309638=CARTESIAN_POINT('Origin',(-3.57686520200006,15.2,1.77640766899998));
#309639=CARTESIAN_POINT('',(-3.24665273100006,2.7,1.61241156299999));
#309640=CARTESIAN_POINT('',(-3.24665273100006,2.2,1.61241156299999));
#309641=CARTESIAN_POINT('',(-1.78843260106674,2.7,0.888203834365703));
#309642=CARTESIAN_POINT('Origin',(-5.66300478732629E-14,15.2,-1.77635683940025E-14));
#309643=CARTESIAN_POINT('',(-3.45664454600006,2.7,1.09189444699998));
#309644=CARTESIAN_POINT('',(-3.45664454600006,12.2,1.09189444699998));
#309645=CARTESIAN_POINT('Origin',(-5.66300478732629E-14,2.7,-1.92943768261394E-14));
#309646=CARTESIAN_POINT('Origin',(-5.66300478732629E-14,15.2,-1.77635683940025E-14));
#309647=CARTESIAN_POINT('',(-3.80824761100006,2.7,1.20295979699998));
#309648=CARTESIAN_POINT('',(-3.80824761100006,12.2,1.20295979699999));
#309649=CARTESIAN_POINT('',(-5.68586833118453E-14,2.7,-1.92221548309966E-14));
#309650=CARTESIAN_POINT('Ctrl Pts',(-3.80828031400006,12.2,1.20296984599999));
#309651=CARTESIAN_POINT('Ctrl Pts',(-3.80828031400006,5.2,1.20296984599999));
#309652=CARTESIAN_POINT('Ctrl Pts',(-3.80828031400006,2.2,1.20296984599999));
#309653=CARTESIAN_POINT('Ctrl Pts',(-3.80828641700006,12.2,1.20297174799999));
#309654=CARTESIAN_POINT('Ctrl Pts',(-3.80828641700006,5.2,1.20297174799999));
#309655=CARTESIAN_POINT('Ctrl Pts',(-3.80828641700006,2.2,1.20297174799999));
#309656=CARTESIAN_POINT('Ctrl Pts',(-3.80829932800006,12.2,1.20297575999999));
#309657=CARTESIAN_POINT('Ctrl Pts',(-3.80829932800006,5.2,1.20297575999999));
#309658=CARTESIAN_POINT('Ctrl Pts',(-3.80829932800006,2.2,1.20297575999999));
#309659=CARTESIAN_POINT('Ctrl Pts',(-3.80832081300006,12.2,1.20298240199999));
#309660=CARTESIAN_POINT('Ctrl Pts',(-3.80832081300006,5.2,1.20298240199999));
#309661=CARTESIAN_POINT('Ctrl Pts',(-3.80832081300006,2.2,1.20298240199999));
#309662=CARTESIAN_POINT('Ctrl Pts',(-3.80835369800006,12.2,1.20299250699999));
#309663=CARTESIAN_POINT('Ctrl Pts',(-3.80835369800006,5.2,1.20299250699999));
#309664=CARTESIAN_POINT('Ctrl Pts',(-3.80835369800006,2.2,1.20299250699999));
#309665=CARTESIAN_POINT('Ctrl Pts',(-3.80840186700006,12.2,1.20300721599999));
#309666=CARTESIAN_POINT('Ctrl Pts',(-3.80840186700006,5.2,1.20300721599999));
#309667=CARTESIAN_POINT('Ctrl Pts',(-3.80840186700006,2.2,1.20300721599999));
#309668=CARTESIAN_POINT('Ctrl Pts',(-3.80845709700006,12.2,1.20302399999999));
#309669=CARTESIAN_POINT('Ctrl Pts',(-3.80845709700006,5.2,1.20302399999999));
#309670=CARTESIAN_POINT('Ctrl Pts',(-3.80845709700006,2.2,1.20302399999999));
#309671=CARTESIAN_POINT('Ctrl Pts',(-3.80851938100006,12.2,1.20304284399999));
#309672=CARTESIAN_POINT('Ctrl Pts',(-3.80851938100006,5.2,1.20304284399999));
#309673=CARTESIAN_POINT('Ctrl Pts',(-3.80851938100006,2.2,1.20304284399999));
#309674=CARTESIAN_POINT('Ctrl Pts',(-3.80858871200005,12.2,1.20306372999998));
#309675=CARTESIAN_POINT('Ctrl Pts',(-3.80858871200005,5.2,1.20306372999998));
#309676=CARTESIAN_POINT('Ctrl Pts',(-3.80858871200005,2.2,1.20306372999998));
#309677=CARTESIAN_POINT('Ctrl Pts',(-3.80866507800006,12.2,1.20308663199999));
#309678=CARTESIAN_POINT('Ctrl Pts',(-3.80866507800006,5.2,1.20308663199999));
#309679=CARTESIAN_POINT('Ctrl Pts',(-3.80866507800006,2.2,1.20308663199999));
#309680=CARTESIAN_POINT('Ctrl Pts',(-3.80874846400006,12.2,1.20311152099998));
#309681=CARTESIAN_POINT('Ctrl Pts',(-3.80874846400006,5.2,1.20311152099998));
#309682=CARTESIAN_POINT('Ctrl Pts',(-3.80874846400006,2.2,1.20311152099998));
#309683=CARTESIAN_POINT('Ctrl Pts',(-3.80883885900006,12.2,1.20313836599999));
#309684=CARTESIAN_POINT('Ctrl Pts',(-3.80883885900006,5.2,1.20313836599999));
#309685=CARTESIAN_POINT('Ctrl Pts',(-3.80883885900006,2.2,1.20313836599999));
#309686=CARTESIAN_POINT('Ctrl Pts',(-3.80893624900006,12.2,1.20316713899999));
#309687=CARTESIAN_POINT('Ctrl Pts',(-3.80893624900006,5.2,1.20316713899999));
#309688=CARTESIAN_POINT('Ctrl Pts',(-3.80893624900006,2.2,1.20316713899999));
#309689=CARTESIAN_POINT('Ctrl Pts',(-3.80904062400006,12.2,1.20319781699999));
#309690=CARTESIAN_POINT('Ctrl Pts',(-3.80904062400006,5.2,1.20319781699999));
#309691=CARTESIAN_POINT('Ctrl Pts',(-3.80904062400006,2.2,1.20319781699999));
#309692=CARTESIAN_POINT('Ctrl Pts',(-3.80915197500006,12.2,1.20323037899999));
#309693=CARTESIAN_POINT('Ctrl Pts',(-3.80915197500006,5.2,1.20323037899999));
#309694=CARTESIAN_POINT('Ctrl Pts',(-3.80915197500006,2.2,1.20323037899999));
#309695=CARTESIAN_POINT('Ctrl Pts',(-3.80927029100006,12.2,1.20326480299998));
#309696=CARTESIAN_POINT('Ctrl Pts',(-3.80927029100006,5.2,1.20326480299998));
#309697=CARTESIAN_POINT('Ctrl Pts',(-3.80927029100006,2.2,1.20326480299998));
#309698=CARTESIAN_POINT('Ctrl Pts',(-3.80939556400006,12.2,1.20330106999999));
#309699=CARTESIAN_POINT('Ctrl Pts',(-3.80939556400006,5.2,1.20330106999999));
#309700=CARTESIAN_POINT('Ctrl Pts',(-3.80939556400006,2.2,1.20330106999999));
#309701=CARTESIAN_POINT('Ctrl Pts',(-3.80952778300006,12.2,1.20333915499999));
#309702=CARTESIAN_POINT('Ctrl Pts',(-3.80952778300006,5.2,1.20333915499999));
#309703=CARTESIAN_POINT('Ctrl Pts',(-3.80952778300006,2.2,1.20333915499999));
#309704=CARTESIAN_POINT('Ctrl Pts',(-3.80966693600006,12.2,1.20337903699999));
#309705=CARTESIAN_POINT('Ctrl Pts',(-3.80966693600006,5.2,1.20337903699999));
#309706=CARTESIAN_POINT('Ctrl Pts',(-3.80966693600006,2.2,1.20337903699999));
#309707=CARTESIAN_POINT('Ctrl Pts',(-3.80981301400006,12.2,1.20342068999999));
#309708=CARTESIAN_POINT('Ctrl Pts',(-3.80981301400006,5.2,1.20342068999999));
#309709=CARTESIAN_POINT('Ctrl Pts',(-3.80981301400006,2.2,1.20342068999999));
#309710=CARTESIAN_POINT('Ctrl Pts',(-3.80996600500006,12.2,1.20346409199998));
#309711=CARTESIAN_POINT('Ctrl Pts',(-3.80996600500006,5.2,1.20346409199998));
#309712=CARTESIAN_POINT('Ctrl Pts',(-3.80996600500006,2.2,1.20346409199998));
#309713=CARTESIAN_POINT('Ctrl Pts',(-3.81012589900006,12.2,1.20350921799998));
#309714=CARTESIAN_POINT('Ctrl Pts',(-3.81012589900006,5.2,1.20350921799998));
#309715=CARTESIAN_POINT('Ctrl Pts',(-3.81012589900006,2.2,1.20350921799998));
#309716=CARTESIAN_POINT('Ctrl Pts',(-3.81029268400006,12.2,1.20355604499998));
#309717=CARTESIAN_POINT('Ctrl Pts',(-3.81029268400006,5.2,1.20355604499998));
#309718=CARTESIAN_POINT('Ctrl Pts',(-3.81029268400006,2.2,1.20355604499998));
#309719=CARTESIAN_POINT('Ctrl Pts',(-3.81046635100006,12.2,1.20360455299998));
#309720=CARTESIAN_POINT('Ctrl Pts',(-3.81046635100006,5.2,1.20360455299998));
#309721=CARTESIAN_POINT('Ctrl Pts',(-3.81046635100006,2.2,1.20360455299998));
#309722=CARTESIAN_POINT('Ctrl Pts',(-3.81064689100006,12.2,1.20365471899999));
#309723=CARTESIAN_POINT('Ctrl Pts',(-3.81064689100006,5.2,1.20365471899999));
#309724=CARTESIAN_POINT('Ctrl Pts',(-3.81064689100006,2.2,1.20365471899999));
#309725=CARTESIAN_POINT('Ctrl Pts',(-3.81083429100006,12.2,1.20370652099998));
#309726=CARTESIAN_POINT('Ctrl Pts',(-3.81083429100006,5.2,1.20370652099998));
#309727=CARTESIAN_POINT('Ctrl Pts',(-3.81083429100006,2.2,1.20370652099998));
#309728=CARTESIAN_POINT('Ctrl Pts',(-3.81102854100006,12.2,1.20375993599998));
#309729=CARTESIAN_POINT('Ctrl Pts',(-3.81102854100006,5.2,1.20375993599998));
#309730=CARTESIAN_POINT('Ctrl Pts',(-3.81102854100006,2.2,1.20375993599998));
#309731=CARTESIAN_POINT('Ctrl Pts',(-3.81122963200006,12.2,1.20381494299998));
#309732=CARTESIAN_POINT('Ctrl Pts',(-3.81122963200006,5.2,1.20381494299998));
#309733=CARTESIAN_POINT('Ctrl Pts',(-3.81122963200006,2.2,1.20381494299998));
#309734=CARTESIAN_POINT('Ctrl Pts',(-3.81143755300006,12.2,1.20387151799998));
#309735=CARTESIAN_POINT('Ctrl Pts',(-3.81143755300006,5.2,1.20387151799998));
#309736=CARTESIAN_POINT('Ctrl Pts',(-3.81143755300006,2.2,1.20387151799998));
#309737=CARTESIAN_POINT('Ctrl Pts',(-3.81165229300006,12.2,1.20392964099999));
#309738=CARTESIAN_POINT('Ctrl Pts',(-3.81165229300006,5.2,1.20392964099999));
#309739=CARTESIAN_POINT('Ctrl Pts',(-3.81165229300006,2.2,1.20392964099999));
#309740=CARTESIAN_POINT('Ctrl Pts',(-3.81187384200006,12.2,1.20398928799998));
#309741=CARTESIAN_POINT('Ctrl Pts',(-3.81187384200006,5.2,1.20398928799998));
#309742=CARTESIAN_POINT('Ctrl Pts',(-3.81187384200006,2.2,1.20398928799998));
#309743=CARTESIAN_POINT('Ctrl Pts',(-3.81210219000006,12.2,1.20405043799999));
#309744=CARTESIAN_POINT('Ctrl Pts',(-3.81210219000006,5.2,1.20405043799999));
#309745=CARTESIAN_POINT('Ctrl Pts',(-3.81210219000006,2.2,1.20405043799999));
#309746=CARTESIAN_POINT('Ctrl Pts',(-3.81233732600006,12.2,1.20411306999999));
#309747=CARTESIAN_POINT('Ctrl Pts',(-3.81233732600006,5.2,1.20411306999999));
#309748=CARTESIAN_POINT('Ctrl Pts',(-3.81233732600006,2.2,1.20411306999999));
#309749=CARTESIAN_POINT('Ctrl Pts',(-3.81257924000006,12.2,1.20417716199999));
#309750=CARTESIAN_POINT('Ctrl Pts',(-3.81257924000006,5.2,1.20417716199999));
#309751=CARTESIAN_POINT('Ctrl Pts',(-3.81257924000006,2.2,1.20417716199999));
#309752=CARTESIAN_POINT('Ctrl Pts',(-3.81282792200006,12.2,1.20424269199999));
#309753=CARTESIAN_POINT('Ctrl Pts',(-3.81282792200006,5.2,1.20424269199999));
#309754=CARTESIAN_POINT('Ctrl Pts',(-3.81282792200006,2.2,1.20424269199999));
#309755=CARTESIAN_POINT('Ctrl Pts',(-3.81308336100005,12.2,1.20430963899999));
#309756=CARTESIAN_POINT('Ctrl Pts',(-3.81308336100005,5.2,1.20430963899999));
#309757=CARTESIAN_POINT('Ctrl Pts',(-3.81308336100005,2.2,1.20430963899999));
#309758=CARTESIAN_POINT('Ctrl Pts',(-3.81334554600006,12.2,1.20437798099998));
#309759=CARTESIAN_POINT('Ctrl Pts',(-3.81334554600006,5.2,1.20437798099998));
#309760=CARTESIAN_POINT('Ctrl Pts',(-3.81334554600006,2.2,1.20437798099998));
#309761=CARTESIAN_POINT('Ctrl Pts',(-3.81361446800006,12.2,1.20444769799999));
#309762=CARTESIAN_POINT('Ctrl Pts',(-3.81361446800006,5.2,1.20444769799999));
#309763=CARTESIAN_POINT('Ctrl Pts',(-3.81361446800006,2.2,1.20444769799999));
#309764=CARTESIAN_POINT('Ctrl Pts',(-3.81389011800006,12.2,1.20451876599999));
#309765=CARTESIAN_POINT('Ctrl Pts',(-3.81389011800006,5.2,1.20451876599999));
#309766=CARTESIAN_POINT('Ctrl Pts',(-3.81389011800006,2.2,1.20451876599999));
#309767=CARTESIAN_POINT('Ctrl Pts',(-3.81417248200006,12.2,1.20459116699998));
#309768=CARTESIAN_POINT('Ctrl Pts',(-3.81417248200006,5.2,1.20459116699998));
#309769=CARTESIAN_POINT('Ctrl Pts',(-3.81417248200006,2.2,1.20459116699998));
#309770=CARTESIAN_POINT('Ctrl Pts',(-3.81446155400006,12.2,1.20466487799999));
#309771=CARTESIAN_POINT('Ctrl Pts',(-3.81446155400006,5.2,1.20466487799999));
#309772=CARTESIAN_POINT('Ctrl Pts',(-3.81446155400006,2.2,1.20466487799999));
#309773=CARTESIAN_POINT('Ctrl Pts',(-3.81475731900006,12.2,1.20473987899999));
#309774=CARTESIAN_POINT('Ctrl Pts',(-3.81475731900006,5.2,1.20473987899999));
#309775=CARTESIAN_POINT('Ctrl Pts',(-3.81475731900006,2.2,1.20473987899999));
#309776=CARTESIAN_POINT('Ctrl Pts',(-3.81505977100006,12.2,1.20481614899999));
#309777=CARTESIAN_POINT('Ctrl Pts',(-3.81505977100006,5.2,1.20481614899999));
#309778=CARTESIAN_POINT('Ctrl Pts',(-3.81505977100006,2.2,1.20481614899999));
#309779=CARTESIAN_POINT('Ctrl Pts',(-3.81536889800006,12.2,1.20489366599998));
#309780=CARTESIAN_POINT('Ctrl Pts',(-3.81536889800006,5.2,1.20489366599998));
#309781=CARTESIAN_POINT('Ctrl Pts',(-3.81536889800006,2.2,1.20489366599998));
#309782=CARTESIAN_POINT('Ctrl Pts',(-3.81568469000006,12.2,1.20497241099998));
#309783=CARTESIAN_POINT('Ctrl Pts',(-3.81568469000006,5.2,1.20497241099998));
#309784=CARTESIAN_POINT('Ctrl Pts',(-3.81568469000006,2.2,1.20497241099998));
#309785=CARTESIAN_POINT('Ctrl Pts',(-3.81600713700006,12.2,1.20505236199998));
#309786=CARTESIAN_POINT('Ctrl Pts',(-3.81600713700006,5.2,1.20505236199998));
#309787=CARTESIAN_POINT('Ctrl Pts',(-3.81600713700006,2.2,1.20505236199998));
#309788=CARTESIAN_POINT('Ctrl Pts',(-3.81633622800006,12.2,1.20513349999999));
#309789=CARTESIAN_POINT('Ctrl Pts',(-3.81633622800006,5.2,1.20513349999999));
#309790=CARTESIAN_POINT('Ctrl Pts',(-3.81633622800006,2.2,1.20513349999999));
#309791=CARTESIAN_POINT('Ctrl Pts',(-3.81667195400006,12.2,1.20521580199998));
#309792=CARTESIAN_POINT('Ctrl Pts',(-3.81667195400006,5.2,1.20521580199998));
#309793=CARTESIAN_POINT('Ctrl Pts',(-3.81667195400006,2.2,1.20521580199998));
#309794=CARTESIAN_POINT('Ctrl Pts',(-3.81701430400006,12.2,1.20529924999999));
#309795=CARTESIAN_POINT('Ctrl Pts',(-3.81701430400006,5.2,1.20529924999999));
#309796=CARTESIAN_POINT('Ctrl Pts',(-3.81701430400006,2.2,1.20529924999999));
#309797=CARTESIAN_POINT('Ctrl Pts',(-3.81736326800006,12.2,1.20538382199999));
#309798=CARTESIAN_POINT('Ctrl Pts',(-3.81736326800006,5.2,1.20538382199999));
#309799=CARTESIAN_POINT('Ctrl Pts',(-3.81736326800006,2.2,1.20538382199999));
#309800=CARTESIAN_POINT('Ctrl Pts',(-3.81771883600006,12.2,1.20546949899999));
#309801=CARTESIAN_POINT('Ctrl Pts',(-3.81771883600006,5.2,1.20546949899999));
#309802=CARTESIAN_POINT('Ctrl Pts',(-3.81771883600006,2.2,1.20546949899999));
#309803=CARTESIAN_POINT('Ctrl Pts',(-3.81808099700006,12.2,1.20555625999998));
#309804=CARTESIAN_POINT('Ctrl Pts',(-3.81808099700006,5.2,1.20555625999998));
#309805=CARTESIAN_POINT('Ctrl Pts',(-3.81808099700006,2.2,1.20555625999998));
#309806=CARTESIAN_POINT('Ctrl Pts',(-3.81844974300006,12.2,1.20564408499999));
#309807=CARTESIAN_POINT('Ctrl Pts',(-3.81844974300006,5.2,1.20564408499999));
#309808=CARTESIAN_POINT('Ctrl Pts',(-3.81844974300006,2.2,1.20564408499999));
#309809=CARTESIAN_POINT('Ctrl Pts',(-3.81882506000006,12.2,1.20573295599999));
#309810=CARTESIAN_POINT('Ctrl Pts',(-3.81882506000006,5.2,1.20573295599999));
#309811=CARTESIAN_POINT('Ctrl Pts',(-3.81882506000006,2.2,1.20573295599999));
#309812=CARTESIAN_POINT('Ctrl Pts',(-3.81920694300006,12.2,1.20582284899998));
#309813=CARTESIAN_POINT('Ctrl Pts',(-3.81920694300006,5.2,1.20582284899998));
#309814=CARTESIAN_POINT('Ctrl Pts',(-3.81920694300006,2.2,1.20582284899998));
#309815=CARTESIAN_POINT('Ctrl Pts',(-3.81959537800006,12.2,1.20591374799998));
#309816=CARTESIAN_POINT('Ctrl Pts',(-3.81959537800006,5.2,1.20591374799998));
#309817=CARTESIAN_POINT('Ctrl Pts',(-3.81959537800006,2.2,1.20591374799998));
#309818=CARTESIAN_POINT('Ctrl Pts',(-3.81999035700006,12.2,1.20600563099998));
#309819=CARTESIAN_POINT('Ctrl Pts',(-3.81999035700006,5.2,1.20600563099998));
#309820=CARTESIAN_POINT('Ctrl Pts',(-3.81999035700006,2.2,1.20600563099998));
#309821=CARTESIAN_POINT('Ctrl Pts',(-3.82039186800006,12.2,1.20609847899999));
#309822=CARTESIAN_POINT('Ctrl Pts',(-3.82039186800006,5.2,1.20609847899999));
#309823=CARTESIAN_POINT('Ctrl Pts',(-3.82039186800006,2.2,1.20609847899999));
#309824=CARTESIAN_POINT('Ctrl Pts',(-3.82079990200006,12.2,1.20619227199999));
#309825=CARTESIAN_POINT('Ctrl Pts',(-3.82079990200006,5.2,1.20619227199999));
#309826=CARTESIAN_POINT('Ctrl Pts',(-3.82079990200006,2.2,1.20619227199999));
#309827=CARTESIAN_POINT('Ctrl Pts',(-3.82121445000006,12.2,1.20628698999999));
#309828=CARTESIAN_POINT('Ctrl Pts',(-3.82121445000006,5.2,1.20628698999999));
#309829=CARTESIAN_POINT('Ctrl Pts',(-3.82121445000006,2.2,1.20628698999999));
#309830=CARTESIAN_POINT('Ctrl Pts',(-3.82163550100006,12.2,1.20638261599999));
#309831=CARTESIAN_POINT('Ctrl Pts',(-3.82163550100006,5.2,1.20638261599999));
#309832=CARTESIAN_POINT('Ctrl Pts',(-3.82163550100006,2.2,1.20638261599999));
#309833=CARTESIAN_POINT('Ctrl Pts',(-3.82206304400006,12.2,1.20647912799999));
#309834=CARTESIAN_POINT('Ctrl Pts',(-3.82206304400006,5.2,1.20647912799999));
#309835=CARTESIAN_POINT('Ctrl Pts',(-3.82206304400006,2.2,1.20647912799999));
#309836=CARTESIAN_POINT('Ctrl Pts',(-3.82249707000006,12.2,1.20657650699998));
#309837=CARTESIAN_POINT('Ctrl Pts',(-3.82249707000006,5.2,1.20657650699998));
#309838=CARTESIAN_POINT('Ctrl Pts',(-3.82249707000006,2.2,1.20657650699998));
#309839=CARTESIAN_POINT('Ctrl Pts',(-3.82293757000006,12.2,1.20667473499998));
#309840=CARTESIAN_POINT('Ctrl Pts',(-3.82293757000006,5.2,1.20667473499998));
#309841=CARTESIAN_POINT('Ctrl Pts',(-3.82293757000006,2.2,1.20667473499998));
#309842=CARTESIAN_POINT('Ctrl Pts',(-3.82338453200005,12.2,1.20677379099998));
#309843=CARTESIAN_POINT('Ctrl Pts',(-3.82338453200005,5.2,1.20677379099998));
#309844=CARTESIAN_POINT('Ctrl Pts',(-3.82338453200005,2.2,1.20677379099998));
#309845=CARTESIAN_POINT('Ctrl Pts',(-3.82383794600006,12.2,1.20687365699998));
#309846=CARTESIAN_POINT('Ctrl Pts',(-3.82383794600006,5.2,1.20687365699998));
#309847=CARTESIAN_POINT('Ctrl Pts',(-3.82383794600006,2.2,1.20687365699998));
#309848=CARTESIAN_POINT('Ctrl Pts',(-3.82429780400006,12.2,1.20697431499998));
#309849=CARTESIAN_POINT('Ctrl Pts',(-3.82429780400006,5.2,1.20697431499998));
#309850=CARTESIAN_POINT('Ctrl Pts',(-3.82429780400006,2.2,1.20697431499998));
#309851=CARTESIAN_POINT('Ctrl Pts',(-3.82476409500006,12.2,1.20707574399999));
#309852=CARTESIAN_POINT('Ctrl Pts',(-3.82476409500006,5.2,1.20707574399999));
#309853=CARTESIAN_POINT('Ctrl Pts',(-3.82476409500006,2.2,1.20707574399999));
#309854=CARTESIAN_POINT('Ctrl Pts',(-3.82523680800006,12.2,1.20717792599998));
#309855=CARTESIAN_POINT('Ctrl Pts',(-3.82523680800006,5.2,1.20717792599998));
#309856=CARTESIAN_POINT('Ctrl Pts',(-3.82523680800006,2.2,1.20717792599998));
#309857=CARTESIAN_POINT('Ctrl Pts',(-3.82571593500006,12.2,1.20728084299999));
#309858=CARTESIAN_POINT('Ctrl Pts',(-3.82571593500006,5.2,1.20728084299999));
#309859=CARTESIAN_POINT('Ctrl Pts',(-3.82571593500006,2.2,1.20728084299999));
#309860=CARTESIAN_POINT('Ctrl Pts',(-3.82620146300006,12.2,1.20738447399999));
#309861=CARTESIAN_POINT('Ctrl Pts',(-3.82620146300006,5.2,1.20738447399999));
#309862=CARTESIAN_POINT('Ctrl Pts',(-3.82620146300006,2.2,1.20738447399999));
#309863=CARTESIAN_POINT('Ctrl Pts',(-3.82669338600006,12.2,1.20748880199999));
#309864=CARTESIAN_POINT('Ctrl Pts',(-3.82669338600006,5.2,1.20748880199999));
#309865=CARTESIAN_POINT('Ctrl Pts',(-3.82669338600006,2.2,1.20748880199999));
#309866=CARTESIAN_POINT('Ctrl Pts',(-3.82719169200006,12.2,1.20759380899999));
#309867=CARTESIAN_POINT('Ctrl Pts',(-3.82719169200006,5.2,1.20759380899999));
#309868=CARTESIAN_POINT('Ctrl Pts',(-3.82719169200006,2.2,1.20759380899999));
#309869=CARTESIAN_POINT('Ctrl Pts',(-3.82769637100006,12.2,1.20769947499999));
#309870=CARTESIAN_POINT('Ctrl Pts',(-3.82769637100006,5.2,1.20769947499999));
#309871=CARTESIAN_POINT('Ctrl Pts',(-3.82769637100006,2.2,1.20769947499999));
#309872=CARTESIAN_POINT('Ctrl Pts',(-3.82820741400006,12.2,1.20780578099998));
#309873=CARTESIAN_POINT('Ctrl Pts',(-3.82820741400006,5.2,1.20780578099998));
#309874=CARTESIAN_POINT('Ctrl Pts',(-3.82820741400006,2.2,1.20780578099998));
#309875=CARTESIAN_POINT('Ctrl Pts',(-3.82872480900006,12.2,1.20791271199999));
#309876=CARTESIAN_POINT('Ctrl Pts',(-3.82872480900006,5.2,1.20791271199999));
#309877=CARTESIAN_POINT('Ctrl Pts',(-3.82872480900006,2.2,1.20791271199999));
#309878=CARTESIAN_POINT('Ctrl Pts',(-3.82924854800006,12.2,1.20802024499998));
#309879=CARTESIAN_POINT('Ctrl Pts',(-3.82924854800006,5.2,1.20802024499998));
#309880=CARTESIAN_POINT('Ctrl Pts',(-3.82924854800006,2.2,1.20802024499998));
#309881=CARTESIAN_POINT('Ctrl Pts',(-3.82977862000006,12.2,1.20812836499999));
#309882=CARTESIAN_POINT('Ctrl Pts',(-3.82977862000006,5.2,1.20812836499999));
#309883=CARTESIAN_POINT('Ctrl Pts',(-3.82977862000006,2.2,1.20812836499999));
#309884=CARTESIAN_POINT('Ctrl Pts',(-3.83031501700006,12.2,1.20823705199999));
#309885=CARTESIAN_POINT('Ctrl Pts',(-3.83031501700006,5.2,1.20823705199999));
#309886=CARTESIAN_POINT('Ctrl Pts',(-3.83031501700006,2.2,1.20823705199999));
#309887=CARTESIAN_POINT('Ctrl Pts',(-3.83085772700006,12.2,1.20834629099999));
#309888=CARTESIAN_POINT('Ctrl Pts',(-3.83085772700006,5.2,1.20834629099999));
#309889=CARTESIAN_POINT('Ctrl Pts',(-3.83085772700006,2.2,1.20834629099999));
#309890=CARTESIAN_POINT('Ctrl Pts',(-3.83140674200006,12.2,1.20845605799999));
#309891=CARTESIAN_POINT('Ctrl Pts',(-3.83140674200006,5.2,1.20845605799999));
#309892=CARTESIAN_POINT('Ctrl Pts',(-3.83140674200006,2.2,1.20845605799999));
#309893=CARTESIAN_POINT('Ctrl Pts',(-3.83196205000006,12.2,1.20856634199999));
#309894=CARTESIAN_POINT('Ctrl Pts',(-3.83196205000006,5.2,1.20856634199999));
#309895=CARTESIAN_POINT('Ctrl Pts',(-3.83196205000006,2.2,1.20856634199999));
#309896=CARTESIAN_POINT('Ctrl Pts',(-3.83252364200006,12.2,1.20867711899999));
#309897=CARTESIAN_POINT('Ctrl Pts',(-3.83252364200006,5.2,1.20867711899999));
#309898=CARTESIAN_POINT('Ctrl Pts',(-3.83252364200006,2.2,1.20867711899999));
#309899=CARTESIAN_POINT('Ctrl Pts',(-3.83309151000006,12.2,1.20878837499999));
#309900=CARTESIAN_POINT('Ctrl Pts',(-3.83309151000006,5.2,1.20878837499999));
#309901=CARTESIAN_POINT('Ctrl Pts',(-3.83309151000006,2.2,1.20878837499999));
#309902=CARTESIAN_POINT('Ctrl Pts',(-3.83366564200006,12.2,1.20890009099998));
#309903=CARTESIAN_POINT('Ctrl Pts',(-3.83366564200006,5.2,1.20890009099998));
#309904=CARTESIAN_POINT('Ctrl Pts',(-3.83366564200006,2.2,1.20890009099998));
#309905=CARTESIAN_POINT('Ctrl Pts',(-3.83424602900006,12.2,1.20901224799999));
#309906=CARTESIAN_POINT('Ctrl Pts',(-3.83424602900006,5.2,1.20901224799999));
#309907=CARTESIAN_POINT('Ctrl Pts',(-3.83424602900006,2.2,1.20901224799999));
#309908=CARTESIAN_POINT('Ctrl Pts',(-3.83483266100006,12.2,1.20912483099998));
#309909=CARTESIAN_POINT('Ctrl Pts',(-3.83483266100006,5.2,1.20912483099998));
#309910=CARTESIAN_POINT('Ctrl Pts',(-3.83483266100006,2.2,1.20912483099998));
#309911=CARTESIAN_POINT('Ctrl Pts',(-3.83542552800006,12.2,1.20923782099998));
#309912=CARTESIAN_POINT('Ctrl Pts',(-3.83542552800006,5.2,1.20923782099998));
#309913=CARTESIAN_POINT('Ctrl Pts',(-3.83542552800006,2.2,1.20923782099998));
#309914=CARTESIAN_POINT('Ctrl Pts',(-3.83602461900006,12.2,1.20935119999999));
#309915=CARTESIAN_POINT('Ctrl Pts',(-3.83602461900006,5.2,1.20935119999999));
#309916=CARTESIAN_POINT('Ctrl Pts',(-3.83602461900006,2.2,1.20935119999999));
#309917=CARTESIAN_POINT('Ctrl Pts',(-3.83662992800006,12.2,1.20946494999998));
#309918=CARTESIAN_POINT('Ctrl Pts',(-3.83662992800006,5.2,1.20946494999998));
#309919=CARTESIAN_POINT('Ctrl Pts',(-3.83662992800006,2.2,1.20946494999998));
#309920=CARTESIAN_POINT('Ctrl Pts',(-3.83724144100006,12.2,1.20957905399999));
#309921=CARTESIAN_POINT('Ctrl Pts',(-3.83724144100006,5.2,1.20957905399999));
#309922=CARTESIAN_POINT('Ctrl Pts',(-3.83724144100006,2.2,1.20957905399999));
#309923=CARTESIAN_POINT('Ctrl Pts',(-3.83785915100006,12.2,1.20969349699998));
#309924=CARTESIAN_POINT('Ctrl Pts',(-3.83785915100006,5.2,1.20969349699998));
#309925=CARTESIAN_POINT('Ctrl Pts',(-3.83785915100006,2.2,1.20969349699998));
#309926=CARTESIAN_POINT('Ctrl Pts',(-3.83848304800006,12.2,1.20980825899998));
#309927=CARTESIAN_POINT('Ctrl Pts',(-3.83848304800006,5.2,1.20980825899998));
#309928=CARTESIAN_POINT('Ctrl Pts',(-3.83848304800006,2.2,1.20980825899998));
#309929=CARTESIAN_POINT('Ctrl Pts',(-3.83911312000006,12.2,1.20992332299998));
#309930=CARTESIAN_POINT('Ctrl Pts',(-3.83911312000006,5.2,1.20992332299998));
#309931=CARTESIAN_POINT('Ctrl Pts',(-3.83911312000006,2.2,1.20992332299998));
#309932=CARTESIAN_POINT('Ctrl Pts',(-3.83974936000006,12.2,1.21003867299999));
#309933=CARTESIAN_POINT('Ctrl Pts',(-3.83974936000006,5.2,1.21003867299999));
#309934=CARTESIAN_POINT('Ctrl Pts',(-3.83974936000006,2.2,1.21003867299999));
#309935=CARTESIAN_POINT('Ctrl Pts',(-3.84039175700006,12.2,1.21015429099999));
#309936=CARTESIAN_POINT('Ctrl Pts',(-3.84039175700006,5.2,1.21015429099999));
#309937=CARTESIAN_POINT('Ctrl Pts',(-3.84039175700006,2.2,1.21015429099999));
#309938=CARTESIAN_POINT('Ctrl Pts',(-3.84104030200006,12.2,1.21027015999998));
#309939=CARTESIAN_POINT('Ctrl Pts',(-3.84104030200006,5.2,1.21027015999998));
#309940=CARTESIAN_POINT('Ctrl Pts',(-3.84104030200006,2.2,1.21027015999998));
#309941=CARTESIAN_POINT('Ctrl Pts',(-3.84169498400006,12.2,1.21038626399999));
#309942=CARTESIAN_POINT('Ctrl Pts',(-3.84169498400006,5.2,1.21038626399999));
#309943=CARTESIAN_POINT('Ctrl Pts',(-3.84169498400006,2.2,1.21038626399999));
#309944=CARTESIAN_POINT('Ctrl Pts',(-3.84235579300006,12.2,1.21050258499999));
#309945=CARTESIAN_POINT('Ctrl Pts',(-3.84235579300006,5.2,1.21050258499999));
#309946=CARTESIAN_POINT('Ctrl Pts',(-3.84235579300006,2.2,1.21050258499999));
#309947=CARTESIAN_POINT('Ctrl Pts',(-3.84302272200006,12.2,1.21061910599999));
#309948=CARTESIAN_POINT('Ctrl Pts',(-3.84302272200006,5.2,1.21061910599999));
#309949=CARTESIAN_POINT('Ctrl Pts',(-3.84302272200006,2.2,1.21061910599999));
#309950=CARTESIAN_POINT('Ctrl Pts',(-3.84369575800006,12.2,1.21073581099999));
#309951=CARTESIAN_POINT('Ctrl Pts',(-3.84369575800006,5.2,1.21073581099999));
#309952=CARTESIAN_POINT('Ctrl Pts',(-3.84369575800006,2.2,1.21073581099999));
#309953=CARTESIAN_POINT('Ctrl Pts',(-3.84437489400006,12.2,1.21085268299999));
#309954=CARTESIAN_POINT('Ctrl Pts',(-3.84437489400006,5.2,1.21085268299999));
#309955=CARTESIAN_POINT('Ctrl Pts',(-3.84437489400006,2.2,1.21085268299999));
#309956=CARTESIAN_POINT('Ctrl Pts',(-3.84506011900006,12.2,1.21096970499998));
#309957=CARTESIAN_POINT('Ctrl Pts',(-3.84506011900006,5.2,1.21096970499998));
#309958=CARTESIAN_POINT('Ctrl Pts',(-3.84506011900006,2.2,1.21096970499998));
#309959=CARTESIAN_POINT('Ctrl Pts',(-3.84575142300006,12.2,1.21108685999999));
#309960=CARTESIAN_POINT('Ctrl Pts',(-3.84575142300006,5.2,1.21108685999999));
#309961=CARTESIAN_POINT('Ctrl Pts',(-3.84575142300006,2.2,1.21108685999999));
#309962=CARTESIAN_POINT('Ctrl Pts',(-3.84644879800006,12.2,1.21120413299999));
#309963=CARTESIAN_POINT('Ctrl Pts',(-3.84644879800006,5.2,1.21120413299999));
#309964=CARTESIAN_POINT('Ctrl Pts',(-3.84644879800006,2.2,1.21120413299999));
#309965=CARTESIAN_POINT('Ctrl Pts',(-3.84715223200006,12.2,1.21132150599998));
#309966=CARTESIAN_POINT('Ctrl Pts',(-3.84715223200006,5.2,1.21132150599998));
#309967=CARTESIAN_POINT('Ctrl Pts',(-3.84715223200006,2.2,1.21132150599998));
#309968=CARTESIAN_POINT('Ctrl Pts',(-3.84786171700005,12.2,1.21143896399999));
#309969=CARTESIAN_POINT('Ctrl Pts',(-3.84786171700005,5.2,1.21143896399999));
#309970=CARTESIAN_POINT('Ctrl Pts',(-3.84786171700005,2.2,1.21143896399999));
#309971=CARTESIAN_POINT('Ctrl Pts',(-3.84857724200006,12.2,1.21155648899999));
#309972=CARTESIAN_POINT('Ctrl Pts',(-3.84857724200006,5.2,1.21155648899999));
#309973=CARTESIAN_POINT('Ctrl Pts',(-3.84857724200006,2.2,1.21155648899999));
#309974=CARTESIAN_POINT('Ctrl Pts',(-3.84929880000006,12.2,1.21167406499998));
#309975=CARTESIAN_POINT('Ctrl Pts',(-3.84929880000006,5.2,1.21167406499998));
#309976=CARTESIAN_POINT('Ctrl Pts',(-3.84929880000006,2.2,1.21167406499998));
#309977=CARTESIAN_POINT('Ctrl Pts',(-3.85002637800006,12.2,1.21179167599998));
#309978=CARTESIAN_POINT('Ctrl Pts',(-3.85002637800006,5.2,1.21179167599998));
#309979=CARTESIAN_POINT('Ctrl Pts',(-3.85002637800006,2.2,1.21179167599998));
#309980=CARTESIAN_POINT('Ctrl Pts',(-3.85075996900006,12.2,1.21190930699999));
#309981=CARTESIAN_POINT('Ctrl Pts',(-3.85075996900006,5.2,1.21190930699999));
#309982=CARTESIAN_POINT('Ctrl Pts',(-3.85075996900006,2.2,1.21190930699999));
#309983=CARTESIAN_POINT('Ctrl Pts',(-3.85149956200006,12.2,1.21202693899999));
#309984=CARTESIAN_POINT('Ctrl Pts',(-3.85149956200006,5.2,1.21202693899999));
#309985=CARTESIAN_POINT('Ctrl Pts',(-3.85149956200006,2.2,1.21202693899999));
#309986=CARTESIAN_POINT('Ctrl Pts',(-3.85224514800006,12.2,1.21214455899999));
#309987=CARTESIAN_POINT('Ctrl Pts',(-3.85224514800006,5.2,1.21214455899999));
#309988=CARTESIAN_POINT('Ctrl Pts',(-3.85224514800006,2.2,1.21214455899999));
#309989=CARTESIAN_POINT('Ctrl Pts',(-3.85299671700006,12.2,1.21226214899998));
#309990=CARTESIAN_POINT('Ctrl Pts',(-3.85299671700006,5.2,1.21226214899998));
#309991=CARTESIAN_POINT('Ctrl Pts',(-3.85299671700006,2.2,1.21226214899998));
#309992=CARTESIAN_POINT('Ctrl Pts',(-3.85375426000006,12.2,1.21237969399999));
#309993=CARTESIAN_POINT('Ctrl Pts',(-3.85375426000006,5.2,1.21237969399999));
#309994=CARTESIAN_POINT('Ctrl Pts',(-3.85375426000006,2.2,1.21237969399999));
#309995=CARTESIAN_POINT('Ctrl Pts',(-3.85451776700005,12.2,1.21249717699999));
#309996=CARTESIAN_POINT('Ctrl Pts',(-3.85451776700005,5.2,1.21249717699999));
#309997=CARTESIAN_POINT('Ctrl Pts',(-3.85451776700005,2.2,1.21249717699999));
#309998=CARTESIAN_POINT('Ctrl Pts',(-3.85528722900006,12.2,1.21261458399998));
#309999=CARTESIAN_POINT('Ctrl Pts',(-3.85528722900006,5.2,1.21261458399998));
#310000=CARTESIAN_POINT('Ctrl Pts',(-3.85528722900006,2.2,1.21261458399998));
#310001=CARTESIAN_POINT('Ctrl Pts',(-3.85606263500006,12.2,1.21273189699998));
#310002=CARTESIAN_POINT('Ctrl Pts',(-3.85606263500006,5.2,1.21273189699998));
#310003=CARTESIAN_POINT('Ctrl Pts',(-3.85606263500006,2.2,1.21273189699998));
#310004=CARTESIAN_POINT('Ctrl Pts',(-3.85684397700006,12.2,1.21284910099998));
#310005=CARTESIAN_POINT('Ctrl Pts',(-3.85684397700006,5.2,1.21284910099998));
#310006=CARTESIAN_POINT('Ctrl Pts',(-3.85684397700006,2.2,1.21284910099998));
#310007=CARTESIAN_POINT('Ctrl Pts',(-3.85763124500006,12.2,1.21296618199999));
#310008=CARTESIAN_POINT('Ctrl Pts',(-3.85763124500006,5.2,1.21296618199999));
#310009=CARTESIAN_POINT('Ctrl Pts',(-3.85763124500006,2.2,1.21296618199999));
#310010=CARTESIAN_POINT('Ctrl Pts',(-3.85842442800006,12.2,1.21308312099998));
#310011=CARTESIAN_POINT('Ctrl Pts',(-3.85842442800006,5.2,1.21308312099998));
#310012=CARTESIAN_POINT('Ctrl Pts',(-3.85842442800006,2.2,1.21308312099998));
#310013=CARTESIAN_POINT('Ctrl Pts',(-3.85922351900006,12.2,1.21319990499998));
#310014=CARTESIAN_POINT('Ctrl Pts',(-3.85922351900006,5.2,1.21319990499998));
#310015=CARTESIAN_POINT('Ctrl Pts',(-3.85922351900006,2.2,1.21319990499998));
#310016=CARTESIAN_POINT('Ctrl Pts',(-3.86002850600006,12.2,1.21331651799998));
#310017=CARTESIAN_POINT('Ctrl Pts',(-3.86002850600006,5.2,1.21331651799998));
#310018=CARTESIAN_POINT('Ctrl Pts',(-3.86002850600006,2.2,1.21331651799998));
#310019=CARTESIAN_POINT('Ctrl Pts',(-3.86083938100006,12.2,1.21343294399999));
#310020=CARTESIAN_POINT('Ctrl Pts',(-3.86083938100006,5.2,1.21343294399999));
#310021=CARTESIAN_POINT('Ctrl Pts',(-3.86083938100006,2.2,1.21343294399999));
#310022=CARTESIAN_POINT('Ctrl Pts',(-3.86165613400006,12.2,1.21354916799998));
#310023=CARTESIAN_POINT('Ctrl Pts',(-3.86165613400006,5.2,1.21354916799998));
#310024=CARTESIAN_POINT('Ctrl Pts',(-3.86165613400006,2.2,1.21354916799998));
#310025=CARTESIAN_POINT('Ctrl Pts',(-3.86247875600006,12.2,1.21366517399998));
#310026=CARTESIAN_POINT('Ctrl Pts',(-3.86247875600006,5.2,1.21366517399998));
#310027=CARTESIAN_POINT('Ctrl Pts',(-3.86247875600006,2.2,1.21366517399998));
#310028=CARTESIAN_POINT('Ctrl Pts',(-3.86330723700006,12.2,1.21378094699998));
#310029=CARTESIAN_POINT('Ctrl Pts',(-3.86330723700006,5.2,1.21378094699998));
#310030=CARTESIAN_POINT('Ctrl Pts',(-3.86330723700006,2.2,1.21378094699998));
#310031=CARTESIAN_POINT('Ctrl Pts',(-3.86414156800006,12.2,1.21389647099999));
#310032=CARTESIAN_POINT('Ctrl Pts',(-3.86414156800006,5.2,1.21389647099999));
#310033=CARTESIAN_POINT('Ctrl Pts',(-3.86414156800006,2.2,1.21389647099999));
#310034=CARTESIAN_POINT('Ctrl Pts',(-3.86498173800006,12.2,1.21401173299999));
#310035=CARTESIAN_POINT('Ctrl Pts',(-3.86498173800006,5.2,1.21401173299999));
#310036=CARTESIAN_POINT('Ctrl Pts',(-3.86498173800006,2.2,1.21401173299999));
#310037=CARTESIAN_POINT('Ctrl Pts',(-3.86582774000006,12.2,1.21412671599999));
#310038=CARTESIAN_POINT('Ctrl Pts',(-3.86582774000006,5.2,1.21412671599999));
#310039=CARTESIAN_POINT('Ctrl Pts',(-3.86582774000006,2.2,1.21412671599999));
#310040=CARTESIAN_POINT('Ctrl Pts',(-3.86667956300006,12.2,1.21424140599999));
#310041=CARTESIAN_POINT('Ctrl Pts',(-3.86667956300006,5.2,1.21424140599999));
#310042=CARTESIAN_POINT('Ctrl Pts',(-3.86667956300006,2.2,1.21424140599999));
#310043=CARTESIAN_POINT('Ctrl Pts',(-3.86753719600006,12.2,1.21435578599999));
#310044=CARTESIAN_POINT('Ctrl Pts',(-3.86753719600006,5.2,1.21435578599999));
#310045=CARTESIAN_POINT('Ctrl Pts',(-3.86753719600006,2.2,1.21435578599999));
#310046=CARTESIAN_POINT('Ctrl Pts',(-3.86840063300006,12.2,1.21446984299999));
#310047=CARTESIAN_POINT('Ctrl Pts',(-3.86840063300006,5.2,1.21446984299999));
#310048=CARTESIAN_POINT('Ctrl Pts',(-3.86840063300006,2.2,1.21446984299999));
#310049=CARTESIAN_POINT('Ctrl Pts',(-3.86926986200006,12.2,1.21458356099998));
#310050=CARTESIAN_POINT('Ctrl Pts',(-3.86926986200006,5.2,1.21458356099998));
#310051=CARTESIAN_POINT('Ctrl Pts',(-3.86926986200006,2.2,1.21458356099998));
#310052=CARTESIAN_POINT('Ctrl Pts',(-3.87014487400006,12.2,1.21469692599999));
#310053=CARTESIAN_POINT('Ctrl Pts',(-3.87014487400006,5.2,1.21469692599999));
#310054=CARTESIAN_POINT('Ctrl Pts',(-3.87014487400006,2.2,1.21469692599999));
#310055=CARTESIAN_POINT('Ctrl Pts',(-3.87102566100006,12.2,1.21480992199999));
#310056=CARTESIAN_POINT('Ctrl Pts',(-3.87102566100006,5.2,1.21480992199999));
#310057=CARTESIAN_POINT('Ctrl Pts',(-3.87102566100006,2.2,1.21480992199999));
#310058=CARTESIAN_POINT('Ctrl Pts',(-3.87191221100006,12.2,1.21492253399999));
#310059=CARTESIAN_POINT('Ctrl Pts',(-3.87191221100006,5.2,1.21492253399999));
#310060=CARTESIAN_POINT('Ctrl Pts',(-3.87191221100006,2.2,1.21492253399999));
#310061=CARTESIAN_POINT('Ctrl Pts',(-3.87280451700006,12.2,1.21503474899999));
#310062=CARTESIAN_POINT('Ctrl Pts',(-3.87280451700006,5.2,1.21503474899999));
#310063=CARTESIAN_POINT('Ctrl Pts',(-3.87280451700006,2.2,1.21503474899999));
#310064=CARTESIAN_POINT('Ctrl Pts',(-3.87370256800006,12.2,1.21514654999999));
#310065=CARTESIAN_POINT('Ctrl Pts',(-3.87370256800006,5.2,1.21514654999999));
#310066=CARTESIAN_POINT('Ctrl Pts',(-3.87370256800006,2.2,1.21514654999999));
#310067=CARTESIAN_POINT('Ctrl Pts',(-3.87460635500006,12.2,1.21525792399999));
#310068=CARTESIAN_POINT('Ctrl Pts',(-3.87460635500006,5.2,1.21525792399999));
#310069=CARTESIAN_POINT('Ctrl Pts',(-3.87460635500006,2.2,1.21525792399999));
#310070=CARTESIAN_POINT('Ctrl Pts',(-3.87551586900006,12.2,1.21536885699999));
#310071=CARTESIAN_POINT('Ctrl Pts',(-3.87551586900006,5.2,1.21536885699999));
#310072=CARTESIAN_POINT('Ctrl Pts',(-3.87551586900006,2.2,1.21536885699999));
#310073=CARTESIAN_POINT('Ctrl Pts',(-3.87643110100006,12.2,1.21547933299999));
#310074=CARTESIAN_POINT('Ctrl Pts',(-3.87643110100006,5.2,1.21547933299999));
#310075=CARTESIAN_POINT('Ctrl Pts',(-3.87643110100006,2.2,1.21547933299999));
#310076=CARTESIAN_POINT('Ctrl Pts',(-3.87735204000006,12.2,1.21558933699998));
#310077=CARTESIAN_POINT('Ctrl Pts',(-3.87735204000006,5.2,1.21558933699998));
#310078=CARTESIAN_POINT('Ctrl Pts',(-3.87735204000006,2.2,1.21558933699998));
#310079=CARTESIAN_POINT('Ctrl Pts',(-3.87827867800006,12.2,1.21569885599999));
#310080=CARTESIAN_POINT('Ctrl Pts',(-3.87827867800006,5.2,1.21569885599999));
#310081=CARTESIAN_POINT('Ctrl Pts',(-3.87827867800006,2.2,1.21569885599999));
#310082=CARTESIAN_POINT('Ctrl Pts',(-3.87921100400006,12.2,1.21580787499999));
#310083=CARTESIAN_POINT('Ctrl Pts',(-3.87921100400006,5.2,1.21580787499999));
#310084=CARTESIAN_POINT('Ctrl Pts',(-3.87921100400006,2.2,1.21580787499999));
#310085=CARTESIAN_POINT('Ctrl Pts',(-3.88014901100005,12.2,1.21591637999999));
#310086=CARTESIAN_POINT('Ctrl Pts',(-3.88014901100005,5.2,1.21591637999999));
#310087=CARTESIAN_POINT('Ctrl Pts',(-3.88014901100005,2.2,1.21591637999999));
#310088=CARTESIAN_POINT('Ctrl Pts',(-3.88109268800005,12.2,1.21602435599999));
#310089=CARTESIAN_POINT('Ctrl Pts',(-3.88109268800005,5.2,1.21602435599999));
#310090=CARTESIAN_POINT('Ctrl Pts',(-3.88109268800005,2.2,1.21602435599999));
#310091=CARTESIAN_POINT('Ctrl Pts',(-3.88204202600006,12.2,1.21613178899999));
#310092=CARTESIAN_POINT('Ctrl Pts',(-3.88204202600006,5.2,1.21613178899999));
#310093=CARTESIAN_POINT('Ctrl Pts',(-3.88204202600006,2.2,1.21613178899999));
#310094=CARTESIAN_POINT('Ctrl Pts',(-3.88299701500006,12.2,1.21623866599998));
#310095=CARTESIAN_POINT('Ctrl Pts',(-3.88299701500006,5.2,1.21623866599998));
#310096=CARTESIAN_POINT('Ctrl Pts',(-3.88299701500006,2.2,1.21623866599998));
#310097=CARTESIAN_POINT('Ctrl Pts',(-3.88395764700006,12.2,1.21634497099999));
#310098=CARTESIAN_POINT('Ctrl Pts',(-3.88395764700006,5.2,1.21634497099999));
#310099=CARTESIAN_POINT('Ctrl Pts',(-3.88395764700006,2.2,1.21634497099999));
#310100=CARTESIAN_POINT('Ctrl Pts',(-3.88492391200006,12.2,1.21645068999999));
#310101=CARTESIAN_POINT('Ctrl Pts',(-3.88492391200006,5.2,1.21645068999999));
#310102=CARTESIAN_POINT('Ctrl Pts',(-3.88492391200006,2.2,1.21645068999999));
#310103=CARTESIAN_POINT('Ctrl Pts',(-3.88589580000006,12.2,1.21655580999999));
#310104=CARTESIAN_POINT('Ctrl Pts',(-3.88589580000006,5.2,1.21655580999999));
#310105=CARTESIAN_POINT('Ctrl Pts',(-3.88589580000006,2.2,1.21655580999999));
#310106=CARTESIAN_POINT('Ctrl Pts',(-3.88687330200006,12.2,1.21666031799998));
#310107=CARTESIAN_POINT('Ctrl Pts',(-3.88687330200006,5.2,1.21666031799998));
#310108=CARTESIAN_POINT('Ctrl Pts',(-3.88687330200006,2.2,1.21666031799998));
#310109=CARTESIAN_POINT('Ctrl Pts',(-3.88785641000006,12.2,1.21676419699998));
#310110=CARTESIAN_POINT('Ctrl Pts',(-3.88785641000006,5.2,1.21676419699998));
#310111=CARTESIAN_POINT('Ctrl Pts',(-3.88785641000006,2.2,1.21676419699998));
#310112=CARTESIAN_POINT('Ctrl Pts',(-3.88884511400006,12.2,1.21686743499998));
#310113=CARTESIAN_POINT('Ctrl Pts',(-3.88884511400006,5.2,1.21686743499998));
#310114=CARTESIAN_POINT('Ctrl Pts',(-3.88884511400006,2.2,1.21686743499998));
#310115=CARTESIAN_POINT('Ctrl Pts',(-3.88983940300006,12.2,1.21697001799999));
#310116=CARTESIAN_POINT('Ctrl Pts',(-3.88983940300006,5.2,1.21697001799999));
#310117=CARTESIAN_POINT('Ctrl Pts',(-3.88983940300006,2.2,1.21697001799999));
#310118=CARTESIAN_POINT('Ctrl Pts',(-3.89083926900006,12.2,1.21707193199999));
#310119=CARTESIAN_POINT('Ctrl Pts',(-3.89083926900006,5.2,1.21707193199999));
#310120=CARTESIAN_POINT('Ctrl Pts',(-3.89083926900006,2.2,1.21707193199999));
#310121=CARTESIAN_POINT('Ctrl Pts',(-3.89184470200005,12.2,1.21717316299998));
#310122=CARTESIAN_POINT('Ctrl Pts',(-3.89184470200005,5.2,1.21717316299998));
#310123=CARTESIAN_POINT('Ctrl Pts',(-3.89184470200005,2.2,1.21717316299998));
#310124=CARTESIAN_POINT('Ctrl Pts',(-3.89285569500006,12.2,1.21727369699999));
#310125=CARTESIAN_POINT('Ctrl Pts',(-3.89285569500006,5.2,1.21727369699999));
#310126=CARTESIAN_POINT('Ctrl Pts',(-3.89285569500006,2.2,1.21727369699999));
#310127=CARTESIAN_POINT('Ctrl Pts',(-3.89387223600006,12.2,1.21737352099998));
#310128=CARTESIAN_POINT('Ctrl Pts',(-3.89387223600006,5.2,1.21737352099998));
#310129=CARTESIAN_POINT('Ctrl Pts',(-3.89387223600006,2.2,1.21737352099998));
#310130=CARTESIAN_POINT('Ctrl Pts',(-3.89489431600006,12.2,1.21747262099999));
#310131=CARTESIAN_POINT('Ctrl Pts',(-3.89489431600006,5.2,1.21747262099999));
#310132=CARTESIAN_POINT('Ctrl Pts',(-3.89489431600006,2.2,1.21747262099999));
#310133=CARTESIAN_POINT('Ctrl Pts',(-3.89592192800006,12.2,1.21757098399998));
#310134=CARTESIAN_POINT('Ctrl Pts',(-3.89592192800006,5.2,1.21757098399998));
#310135=CARTESIAN_POINT('Ctrl Pts',(-3.89592192800006,2.2,1.21757098399998));
#310136=CARTESIAN_POINT('Ctrl Pts',(-3.89695506000006,12.2,1.21766859599999));
#310137=CARTESIAN_POINT('Ctrl Pts',(-3.89695506000006,5.2,1.21766859599999));
#310138=CARTESIAN_POINT('Ctrl Pts',(-3.89695506000006,2.2,1.21766859599999));
#310139=CARTESIAN_POINT('Ctrl Pts',(-3.89799370500006,12.2,1.21776544299999));
#310140=CARTESIAN_POINT('Ctrl Pts',(-3.89799370500006,5.2,1.21776544299999));
#310141=CARTESIAN_POINT('Ctrl Pts',(-3.89799370500006,2.2,1.21776544299999));
#310142=CARTESIAN_POINT('Ctrl Pts',(-3.89903785100006,12.2,1.21786151199998));
#310143=CARTESIAN_POINT('Ctrl Pts',(-3.89903785100006,5.2,1.21786151199998));
#310144=CARTESIAN_POINT('Ctrl Pts',(-3.89903785100006,2.2,1.21786151199998));
#310145=CARTESIAN_POINT('Ctrl Pts',(-3.90008749200006,12.2,1.21795678899999));
#310146=CARTESIAN_POINT('Ctrl Pts',(-3.90008749200006,5.2,1.21795678899999));
#310147=CARTESIAN_POINT('Ctrl Pts',(-3.90008749200006,2.2,1.21795678899999));
#310148=CARTESIAN_POINT('Ctrl Pts',(-3.90114261600006,12.2,1.21805126199999));
#310149=CARTESIAN_POINT('Ctrl Pts',(-3.90114261600006,5.2,1.21805126199999));
#310150=CARTESIAN_POINT('Ctrl Pts',(-3.90114261600006,2.2,1.21805126199999));
#310151=CARTESIAN_POINT('Ctrl Pts',(-3.90220321500006,12.2,1.21814491699999));
#310152=CARTESIAN_POINT('Ctrl Pts',(-3.90220321500006,5.2,1.21814491699999));
#310153=CARTESIAN_POINT('Ctrl Pts',(-3.90220321500006,2.2,1.21814491699999));
#310154=CARTESIAN_POINT('Ctrl Pts',(-3.90326928000006,12.2,1.21823773999999));
#310155=CARTESIAN_POINT('Ctrl Pts',(-3.90326928000006,5.2,1.21823773999999));
#310156=CARTESIAN_POINT('Ctrl Pts',(-3.90326928000006,2.2,1.21823773999999));
#310157=CARTESIAN_POINT('Ctrl Pts',(-3.90434080200006,12.2,1.21832971899998));
#310158=CARTESIAN_POINT('Ctrl Pts',(-3.90434080200006,5.2,1.21832971899998));
#310159=CARTESIAN_POINT('Ctrl Pts',(-3.90434080200006,2.2,1.21832971899998));
#310160=CARTESIAN_POINT('Ctrl Pts',(-3.90541777000006,12.2,1.21842083999999));
#310161=CARTESIAN_POINT('Ctrl Pts',(-3.90541777000006,5.2,1.21842083999999));
#310162=CARTESIAN_POINT('Ctrl Pts',(-3.90541777000006,2.2,1.21842083999999));
#310163=CARTESIAN_POINT('Ctrl Pts',(-3.90650017600006,12.2,1.21851108999998));
#310164=CARTESIAN_POINT('Ctrl Pts',(-3.90650017600006,5.2,1.21851108999998));
#310165=CARTESIAN_POINT('Ctrl Pts',(-3.90650017600006,2.2,1.21851108999998));
#310166=CARTESIAN_POINT('Ctrl Pts',(-3.90758801000006,12.2,1.21860045499998));
#310167=CARTESIAN_POINT('Ctrl Pts',(-3.90758801000006,5.2,1.21860045499998));
#310168=CARTESIAN_POINT('Ctrl Pts',(-3.90758801000006,2.2,1.21860045499998));
#310169=CARTESIAN_POINT('Ctrl Pts',(-3.90868126500005,12.2,1.21868892299998));
#310170=CARTESIAN_POINT('Ctrl Pts',(-3.90868126500005,5.2,1.21868892299998));
#310171=CARTESIAN_POINT('Ctrl Pts',(-3.90868126500005,2.2,1.21868892299998));
#310172=CARTESIAN_POINT('Ctrl Pts',(-3.90977993000006,12.2,1.21877648099999));
#310173=CARTESIAN_POINT('Ctrl Pts',(-3.90977993000006,5.2,1.21877648099999));
#310174=CARTESIAN_POINT('Ctrl Pts',(-3.90977993000006,2.2,1.21877648099999));
#310175=CARTESIAN_POINT('Ctrl Pts',(-3.91088399500005,12.2,1.21886311599999));
#310176=CARTESIAN_POINT('Ctrl Pts',(-3.91088399500005,5.2,1.21886311599999));
#310177=CARTESIAN_POINT('Ctrl Pts',(-3.91088399500005,2.2,1.21886311599999));
#310178=CARTESIAN_POINT('Ctrl Pts',(-3.91199345200006,12.2,1.21894881599999));
#310179=CARTESIAN_POINT('Ctrl Pts',(-3.91199345200006,5.2,1.21894881599999));
#310180=CARTESIAN_POINT('Ctrl Pts',(-3.91199345200006,2.2,1.21894881599999));
#310181=CARTESIAN_POINT('Ctrl Pts',(-3.91310829200005,12.2,1.21903356499999));
#310182=CARTESIAN_POINT('Ctrl Pts',(-3.91310829200005,5.2,1.21903356499999));
#310183=CARTESIAN_POINT('Ctrl Pts',(-3.91310829200005,2.2,1.21903356499999));
#310184=CARTESIAN_POINT('Ctrl Pts',(-3.91422850500006,12.2,1.21911735199999));
#310185=CARTESIAN_POINT('Ctrl Pts',(-3.91422850500006,5.2,1.21911735199999));
#310186=CARTESIAN_POINT('Ctrl Pts',(-3.91422850500006,2.2,1.21911735199999));
#310187=CARTESIAN_POINT('Ctrl Pts',(-3.91535408400006,12.2,1.21920016599999));
#310188=CARTESIAN_POINT('Ctrl Pts',(-3.91535408400006,5.2,1.21920016599999));
#310189=CARTESIAN_POINT('Ctrl Pts',(-3.91535408400006,2.2,1.21920016599999));
#310190=CARTESIAN_POINT('Ctrl Pts',(-3.91648501700006,12.2,1.21928199199999));
#310191=CARTESIAN_POINT('Ctrl Pts',(-3.91648501700006,5.2,1.21928199199999));
#310192=CARTESIAN_POINT('Ctrl Pts',(-3.91648501700006,2.2,1.21928199199999));
#310193=CARTESIAN_POINT('Ctrl Pts',(-3.91762129500006,12.2,1.21936281799998));
#310194=CARTESIAN_POINT('Ctrl Pts',(-3.91762129500006,5.2,1.21936281799998));
#310195=CARTESIAN_POINT('Ctrl Pts',(-3.91762129500006,2.2,1.21936281799998));
#310196=CARTESIAN_POINT('Ctrl Pts',(-3.91876291000006,12.2,1.21944262999999));
#310197=CARTESIAN_POINT('Ctrl Pts',(-3.91876291000006,5.2,1.21944262999999));
#310198=CARTESIAN_POINT('Ctrl Pts',(-3.91876291000006,2.2,1.21944262999999));
#310199=CARTESIAN_POINT('Ctrl Pts',(-3.91990985300006,12.2,1.21952141699999));
#310200=CARTESIAN_POINT('Ctrl Pts',(-3.91990985300006,5.2,1.21952141699999));
#310201=CARTESIAN_POINT('Ctrl Pts',(-3.91990985300006,2.2,1.21952141699999));
#310202=CARTESIAN_POINT('Ctrl Pts',(-3.92106211500006,12.2,1.21959916599998));
#310203=CARTESIAN_POINT('Ctrl Pts',(-3.92106211500006,5.2,1.21959916599998));
#310204=CARTESIAN_POINT('Ctrl Pts',(-3.92106211500006,2.2,1.21959916599998));
#310205=CARTESIAN_POINT('Ctrl Pts',(-3.92221968500006,12.2,1.21967586499999));
#310206=CARTESIAN_POINT('Ctrl Pts',(-3.92221968500006,5.2,1.21967586499999));
#310207=CARTESIAN_POINT('Ctrl Pts',(-3.92221968500006,2.2,1.21967586499999));
#310208=CARTESIAN_POINT('Ctrl Pts',(-3.92338255600006,12.2,1.21975150099999));
#310209=CARTESIAN_POINT('Ctrl Pts',(-3.92338255600006,5.2,1.21975150099999));
#310210=CARTESIAN_POINT('Ctrl Pts',(-3.92338255600006,2.2,1.21975150099999));
#310211=CARTESIAN_POINT('Ctrl Pts',(-3.92455071700006,12.2,1.21982605999999));
#310212=CARTESIAN_POINT('Ctrl Pts',(-3.92455071700006,5.2,1.21982605999999));
#310213=CARTESIAN_POINT('Ctrl Pts',(-3.92455071700006,2.2,1.21982605999999));
#310214=CARTESIAN_POINT('Ctrl Pts',(-3.92572416100006,12.2,1.21989953199999));
#310215=CARTESIAN_POINT('Ctrl Pts',(-3.92572416100006,5.2,1.21989953199999));
#310216=CARTESIAN_POINT('Ctrl Pts',(-3.92572416100006,2.2,1.21989953199999));
#310217=CARTESIAN_POINT('Ctrl Pts',(-3.92690287700006,12.2,1.21997190299998));
#310218=CARTESIAN_POINT('Ctrl Pts',(-3.92690287700006,5.2,1.21997190299998));
#310219=CARTESIAN_POINT('Ctrl Pts',(-3.92690287700006,2.2,1.21997190299998));
#310220=CARTESIAN_POINT('Ctrl Pts',(-3.92808685700006,12.2,1.22004316099999));
#310221=CARTESIAN_POINT('Ctrl Pts',(-3.92808685700006,5.2,1.22004316099999));
#310222=CARTESIAN_POINT('Ctrl Pts',(-3.92808685700006,2.2,1.22004316099999));
#310223=CARTESIAN_POINT('Ctrl Pts',(-3.92927609100005,12.2,1.22011329499998));
#310224=CARTESIAN_POINT('Ctrl Pts',(-3.92927609100005,5.2,1.22011329499998));
#310225=CARTESIAN_POINT('Ctrl Pts',(-3.92927609100005,2.2,1.22011329499998));
#310226=CARTESIAN_POINT('Ctrl Pts',(-3.93047057000006,12.2,1.22018229099998));
#310227=CARTESIAN_POINT('Ctrl Pts',(-3.93047057000006,5.2,1.22018229099998));
#310228=CARTESIAN_POINT('Ctrl Pts',(-3.93047057000006,2.2,1.22018229099998));
#310229=CARTESIAN_POINT('Ctrl Pts',(-3.93167028600006,12.2,1.22025013799998));
#310230=CARTESIAN_POINT('Ctrl Pts',(-3.93167028600006,5.2,1.22025013799998));
#310231=CARTESIAN_POINT('Ctrl Pts',(-3.93167028600006,2.2,1.22025013799998));
#310232=CARTESIAN_POINT('Ctrl Pts',(-3.93287522900006,12.2,1.22031682099998));
#310233=CARTESIAN_POINT('Ctrl Pts',(-3.93287522900006,5.2,1.22031682099998));
#310234=CARTESIAN_POINT('Ctrl Pts',(-3.93287522900006,2.2,1.22031682099998));
#310235=CARTESIAN_POINT('Ctrl Pts',(-3.93408539000006,12.2,1.22038233299998));
#310236=CARTESIAN_POINT('Ctrl Pts',(-3.93408539000006,5.2,1.22038233299998));
#310237=CARTESIAN_POINT('Ctrl Pts',(-3.93408539000006,2.2,1.22038233299998));
#310238=CARTESIAN_POINT('Ctrl Pts',(-3.93530076000006,12.2,1.22044665699999));
#310239=CARTESIAN_POINT('Ctrl Pts',(-3.93530076000006,5.2,1.22044665699999));
#310240=CARTESIAN_POINT('Ctrl Pts',(-3.93530076000006,2.2,1.22044665699999));
#310241=CARTESIAN_POINT('Ctrl Pts',(-3.93652132800006,12.2,1.22050978299999));
#310242=CARTESIAN_POINT('Ctrl Pts',(-3.93652132800006,5.2,1.22050978299999));
#310243=CARTESIAN_POINT('Ctrl Pts',(-3.93652132800006,2.2,1.22050978299999));
#310244=CARTESIAN_POINT('Ctrl Pts',(-3.93774708800006,12.2,1.22057169899998));
#310245=CARTESIAN_POINT('Ctrl Pts',(-3.93774708800006,5.2,1.22057169899998));
#310246=CARTESIAN_POINT('Ctrl Pts',(-3.93774708800006,2.2,1.22057169899998));
#310247=CARTESIAN_POINT('Ctrl Pts',(-3.93897803100006,12.2,1.22063239299999));
#310248=CARTESIAN_POINT('Ctrl Pts',(-3.93897803100006,5.2,1.22063239299999));
#310249=CARTESIAN_POINT('Ctrl Pts',(-3.93897803100006,2.2,1.22063239299999));
#310250=CARTESIAN_POINT('Ctrl Pts',(-3.94021414500005,12.2,1.22069185299999));
#310251=CARTESIAN_POINT('Ctrl Pts',(-3.94021414500005,5.2,1.22069185299999));
#310252=CARTESIAN_POINT('Ctrl Pts',(-3.94021414500005,2.2,1.22069185299999));
#310253=CARTESIAN_POINT('Ctrl Pts',(-3.94145542300006,12.2,1.22075006699998));
#310254=CARTESIAN_POINT('Ctrl Pts',(-3.94145542300006,5.2,1.22075006699998));
#310255=CARTESIAN_POINT('Ctrl Pts',(-3.94145542300006,2.2,1.22075006699998));
#310256=CARTESIAN_POINT('Ctrl Pts',(-3.94270185600006,12.2,1.22080702299999));
#310257=CARTESIAN_POINT('Ctrl Pts',(-3.94270185600006,5.2,1.22080702299999));
#310258=CARTESIAN_POINT('Ctrl Pts',(-3.94270185600006,2.2,1.22080702299999));
#310259=CARTESIAN_POINT('Ctrl Pts',(-3.94395343300006,12.2,1.22086270899999));
#310260=CARTESIAN_POINT('Ctrl Pts',(-3.94395343300006,5.2,1.22086270899999));
#310261=CARTESIAN_POINT('Ctrl Pts',(-3.94395343300006,2.2,1.22086270899999));
#310262=CARTESIAN_POINT('Ctrl Pts',(-3.94521014800006,12.2,1.22091711399999));
#310263=CARTESIAN_POINT('Ctrl Pts',(-3.94521014800006,5.2,1.22091711399999));
#310264=CARTESIAN_POINT('Ctrl Pts',(-3.94521014800006,2.2,1.22091711399999));
#310265=CARTESIAN_POINT('Ctrl Pts',(-3.94647198800006,12.2,1.22097022499998));
#310266=CARTESIAN_POINT('Ctrl Pts',(-3.94647198800006,5.2,1.22097022499998));
#310267=CARTESIAN_POINT('Ctrl Pts',(-3.94647198800006,2.2,1.22097022499998));
#310268=CARTESIAN_POINT('Ctrl Pts',(-3.94773894800006,12.2,1.22102203099999));
#310269=CARTESIAN_POINT('Ctrl Pts',(-3.94773894800006,5.2,1.22102203099999));
#310270=CARTESIAN_POINT('Ctrl Pts',(-3.94773894800006,2.2,1.22102203099999));
#310271=CARTESIAN_POINT('Ctrl Pts',(-3.94901101700006,12.2,1.22107252099998));
#310272=CARTESIAN_POINT('Ctrl Pts',(-3.94901101700006,5.2,1.22107252099998));
#310273=CARTESIAN_POINT('Ctrl Pts',(-3.94901101700006,2.2,1.22107252099998));
#310274=CARTESIAN_POINT('Ctrl Pts',(-3.95028818600006,12.2,1.22112168199998));
#310275=CARTESIAN_POINT('Ctrl Pts',(-3.95028818600006,5.2,1.22112168199998));
#310276=CARTESIAN_POINT('Ctrl Pts',(-3.95028818600006,2.2,1.22112168199998));
#310277=CARTESIAN_POINT('Ctrl Pts',(-3.95157044600006,12.2,1.22116950299999));
#310278=CARTESIAN_POINT('Ctrl Pts',(-3.95157044600006,5.2,1.22116950299999));
#310279=CARTESIAN_POINT('Ctrl Pts',(-3.95157044600006,2.2,1.22116950299999));
#310280=CARTESIAN_POINT('Ctrl Pts',(-3.95285778800006,12.2,1.22121597299999));
#310281=CARTESIAN_POINT('Ctrl Pts',(-3.95285778800006,5.2,1.22121597299999));
#310282=CARTESIAN_POINT('Ctrl Pts',(-3.95285778800006,2.2,1.22121597299999));
#310283=CARTESIAN_POINT('Ctrl Pts',(-3.95415020300006,12.2,1.22126108099998));
#310284=CARTESIAN_POINT('Ctrl Pts',(-3.95415020300006,5.2,1.22126108099998));
#310285=CARTESIAN_POINT('Ctrl Pts',(-3.95415020300006,2.2,1.22126108099998));
#310286=CARTESIAN_POINT('Ctrl Pts',(-3.95544768200006,12.2,1.22130481199999));
#310287=CARTESIAN_POINT('Ctrl Pts',(-3.95544768200006,5.2,1.22130481199999));
#310288=CARTESIAN_POINT('Ctrl Pts',(-3.95544768200006,2.2,1.22130481199999));
#310289=CARTESIAN_POINT('Ctrl Pts',(-3.95675021600006,12.2,1.22134715899998));
#310290=CARTESIAN_POINT('Ctrl Pts',(-3.95675021600006,5.2,1.22134715899998));
#310291=CARTESIAN_POINT('Ctrl Pts',(-3.95675021600006,2.2,1.22134715899998));
#310292=CARTESIAN_POINT('Ctrl Pts',(-3.95805779600006,12.2,1.22138810799999));
#310293=CARTESIAN_POINT('Ctrl Pts',(-3.95805779600006,5.2,1.22138810799999));
#310294=CARTESIAN_POINT('Ctrl Pts',(-3.95805779600006,2.2,1.22138810799999));
#310295=CARTESIAN_POINT('Ctrl Pts',(-3.95937041400006,12.2,1.22142764599999));
#310296=CARTESIAN_POINT('Ctrl Pts',(-3.95937041400006,5.2,1.22142764599999));
#310297=CARTESIAN_POINT('Ctrl Pts',(-3.95937041400006,2.2,1.22142764599999));
#310298=CARTESIAN_POINT('Ctrl Pts',(-3.96068805900006,12.2,1.22146576599999));
#310299=CARTESIAN_POINT('Ctrl Pts',(-3.96068805900006,5.2,1.22146576599999));
#310300=CARTESIAN_POINT('Ctrl Pts',(-3.96068805900006,2.2,1.22146576599999));
#310301=CARTESIAN_POINT('Ctrl Pts',(-3.96201072300006,12.2,1.22150245499999));
#310302=CARTESIAN_POINT('Ctrl Pts',(-3.96201072300006,5.2,1.22150245499999));
#310303=CARTESIAN_POINT('Ctrl Pts',(-3.96201072300006,2.2,1.22150245499999));
#310304=CARTESIAN_POINT('Ctrl Pts',(-3.96333839700006,12.2,1.22153769999999));
#310305=CARTESIAN_POINT('Ctrl Pts',(-3.96333839700006,5.2,1.22153769999999));
#310306=CARTESIAN_POINT('Ctrl Pts',(-3.96333839700006,2.2,1.22153769999999));
#310307=CARTESIAN_POINT('Ctrl Pts',(-3.96467107200006,12.2,1.22157149099999));
#310308=CARTESIAN_POINT('Ctrl Pts',(-3.96467107200006,5.2,1.22157149099999));
#310309=CARTESIAN_POINT('Ctrl Pts',(-3.96467107200006,2.2,1.22157149099999));
#310310=CARTESIAN_POINT('Ctrl Pts',(-3.96600874000006,12.2,1.22160381699999));
#310311=CARTESIAN_POINT('Ctrl Pts',(-3.96600874000006,5.2,1.22160381699999));
#310312=CARTESIAN_POINT('Ctrl Pts',(-3.96600874000006,2.2,1.22160381699999));
#310313=CARTESIAN_POINT('Ctrl Pts',(-3.96735139100006,12.2,1.22163466699998));
#310314=CARTESIAN_POINT('Ctrl Pts',(-3.96735139100006,5.2,1.22163466699998));
#310315=CARTESIAN_POINT('Ctrl Pts',(-3.96735139100006,2.2,1.22163466699998));
#310316=CARTESIAN_POINT('Ctrl Pts',(-3.96869901600006,12.2,1.22166402999999));
#310317=CARTESIAN_POINT('Ctrl Pts',(-3.96869901600006,5.2,1.22166402999999));
#310318=CARTESIAN_POINT('Ctrl Pts',(-3.96869901600006,2.2,1.22166402999999));
#310319=CARTESIAN_POINT('Ctrl Pts',(-3.97005160500006,12.2,1.22169189399999));
#310320=CARTESIAN_POINT('Ctrl Pts',(-3.97005160500006,5.2,1.22169189399999));
#310321=CARTESIAN_POINT('Ctrl Pts',(-3.97005160500006,2.2,1.22169189399999));
#310322=CARTESIAN_POINT('Ctrl Pts',(-3.97140915200006,12.2,1.22171824799999));
#310323=CARTESIAN_POINT('Ctrl Pts',(-3.97140915200006,5.2,1.22171824799999));
#310324=CARTESIAN_POINT('Ctrl Pts',(-3.97140915200006,2.2,1.22171824799999));
#310325=CARTESIAN_POINT('Ctrl Pts',(-3.97277164500006,12.2,1.22174308099999));
#310326=CARTESIAN_POINT('Ctrl Pts',(-3.97277164500006,5.2,1.22174308099999));
#310327=CARTESIAN_POINT('Ctrl Pts',(-3.97277164500006,2.2,1.22174308099999));
#310328=CARTESIAN_POINT('Ctrl Pts',(-3.97413907700006,12.2,1.22176638299999));
#310329=CARTESIAN_POINT('Ctrl Pts',(-3.97413907700006,5.2,1.22176638299999));
#310330=CARTESIAN_POINT('Ctrl Pts',(-3.97413907700006,2.2,1.22176638299999));
#310331=CARTESIAN_POINT('Ctrl Pts',(-3.97551143800006,12.2,1.22178814199998));
#310332=CARTESIAN_POINT('Ctrl Pts',(-3.97551143800006,5.2,1.22178814199998));
#310333=CARTESIAN_POINT('Ctrl Pts',(-3.97551143800006,2.2,1.22178814199998));
#310334=CARTESIAN_POINT('Ctrl Pts',(-3.97688871900006,12.2,1.22180834799998));
#310335=CARTESIAN_POINT('Ctrl Pts',(-3.97688871900006,5.2,1.22180834799998));
#310336=CARTESIAN_POINT('Ctrl Pts',(-3.97688871900006,2.2,1.22180834799998));
#310337=CARTESIAN_POINT('Ctrl Pts',(-3.97827091300006,12.2,1.22182698899998));
#310338=CARTESIAN_POINT('Ctrl Pts',(-3.97827091300006,5.2,1.22182698899998));
#310339=CARTESIAN_POINT('Ctrl Pts',(-3.97827091300006,2.2,1.22182698899998));
#310340=CARTESIAN_POINT('Ctrl Pts',(-3.97965800800006,12.2,1.22184405499999));
#310341=CARTESIAN_POINT('Ctrl Pts',(-3.97965800800006,5.2,1.22184405499999));
#310342=CARTESIAN_POINT('Ctrl Pts',(-3.97965800800006,2.2,1.22184405499999));
#310343=CARTESIAN_POINT('Ctrl Pts',(-3.98104999700006,12.2,1.22185953499999));
#310344=CARTESIAN_POINT('Ctrl Pts',(-3.98104999700006,5.2,1.22185953499999));
#310345=CARTESIAN_POINT('Ctrl Pts',(-3.98104999700006,2.2,1.22185953499999));
#310346=CARTESIAN_POINT('Ctrl Pts',(-3.98244687100005,12.2,1.22187341799998));
#310347=CARTESIAN_POINT('Ctrl Pts',(-3.98244687100005,5.2,1.22187341799998));
#310348=CARTESIAN_POINT('Ctrl Pts',(-3.98244687100005,2.2,1.22187341799998));
#310349=CARTESIAN_POINT('Ctrl Pts',(-3.98384862200006,12.2,1.22188569399999));
#310350=CARTESIAN_POINT('Ctrl Pts',(-3.98384862200006,5.2,1.22188569399999));
#310351=CARTESIAN_POINT('Ctrl Pts',(-3.98384862200006,2.2,1.22188569399999));
#310352=CARTESIAN_POINT('Ctrl Pts',(-3.98525523800005,12.2,1.22189634999998));
#310353=CARTESIAN_POINT('Ctrl Pts',(-3.98525523800005,5.2,1.22189634999998));
#310354=CARTESIAN_POINT('Ctrl Pts',(-3.98525523800005,2.2,1.22189634999998));
#310355=CARTESIAN_POINT('Ctrl Pts',(-3.98666671300006,12.2,1.22190537899999));
#310356=CARTESIAN_POINT('Ctrl Pts',(-3.98666671300006,5.2,1.22190537899999));
#310357=CARTESIAN_POINT('Ctrl Pts',(-3.98666671300006,2.2,1.22190537899999));
#310358=CARTESIAN_POINT('Ctrl Pts',(-3.98808303600005,12.2,1.22191276799999));
#310359=CARTESIAN_POINT('Ctrl Pts',(-3.98808303600005,5.2,1.22191276799999));
#310360=CARTESIAN_POINT('Ctrl Pts',(-3.98808303600005,2.2,1.22191276799999));
#310361=CARTESIAN_POINT('Ctrl Pts',(-3.98950420000006,12.2,1.22191850599998));
#310362=CARTESIAN_POINT('Ctrl Pts',(-3.98950420000006,5.2,1.22191850599998));
#310363=CARTESIAN_POINT('Ctrl Pts',(-3.98950420000006,2.2,1.22191850599998));
#310364=CARTESIAN_POINT('Ctrl Pts',(-3.99093019600006,12.2,1.22192258299998));
#310365=CARTESIAN_POINT('Ctrl Pts',(-3.99093019600006,5.2,1.22192258299998));
#310366=CARTESIAN_POINT('Ctrl Pts',(-3.99093019600006,2.2,1.22192258299998));
#310367=CARTESIAN_POINT('Ctrl Pts',(-3.99236101300006,12.2,1.22192498899999));
#310368=CARTESIAN_POINT('Ctrl Pts',(-3.99236101300006,5.2,1.22192498899999));
#310369=CARTESIAN_POINT('Ctrl Pts',(-3.99236101300006,2.2,1.22192498899999));
#310370=CARTESIAN_POINT('Ctrl Pts',(-3.99379664400006,12.2,1.22192571399999));
#310371=CARTESIAN_POINT('Ctrl Pts',(-3.99379664400006,5.2,1.22192571399999));
#310372=CARTESIAN_POINT('Ctrl Pts',(-3.99379664400006,2.2,1.22192571399999));
#310373=CARTESIAN_POINT('Ctrl Pts',(-3.99523707900006,12.2,1.22192474599998));
#310374=CARTESIAN_POINT('Ctrl Pts',(-3.99523707900006,5.2,1.22192474599998));
#310375=CARTESIAN_POINT('Ctrl Pts',(-3.99523707900006,2.2,1.22192474599998));
#310376=CARTESIAN_POINT('Ctrl Pts',(-3.99668231100006,12.2,1.22192207599999));
#310377=CARTESIAN_POINT('Ctrl Pts',(-3.99668231100006,5.2,1.22192207599999));
#310378=CARTESIAN_POINT('Ctrl Pts',(-3.99668231100006,2.2,1.22192207599999));
#310379=CARTESIAN_POINT('Ctrl Pts',(-3.99813233000006,12.2,1.22191769199999));
#310380=CARTESIAN_POINT('Ctrl Pts',(-3.99813233000006,5.2,1.22191769199999));
#310381=CARTESIAN_POINT('Ctrl Pts',(-3.99813233000006,2.2,1.22191769199999));
#310382=CARTESIAN_POINT('Ctrl Pts',(-3.99958712600006,12.2,1.22191158499998));
#310383=CARTESIAN_POINT('Ctrl Pts',(-3.99958712600006,5.2,1.22191158499998));
#310384=CARTESIAN_POINT('Ctrl Pts',(-3.99958712600006,2.2,1.22191158499998));
#310385=CARTESIAN_POINT('Ctrl Pts',(-4.00104669100006,12.2,1.22190374299999));
#310386=CARTESIAN_POINT('Ctrl Pts',(-4.00104669100006,5.2,1.22190374299999));
#310387=CARTESIAN_POINT('Ctrl Pts',(-4.00104669100006,2.2,1.22190374299999));
#310388=CARTESIAN_POINT('Ctrl Pts',(-4.00251101700006,12.2,1.22189415799999));
#310389=CARTESIAN_POINT('Ctrl Pts',(-4.00251101700006,5.2,1.22189415799999));
#310390=CARTESIAN_POINT('Ctrl Pts',(-4.00251101700006,2.2,1.22189415799999));
#310391=CARTESIAN_POINT('Ctrl Pts',(-4.00398009500006,12.2,1.22188281799998));
#310392=CARTESIAN_POINT('Ctrl Pts',(-4.00398009500006,5.2,1.22188281799998));
#310393=CARTESIAN_POINT('Ctrl Pts',(-4.00398009500006,2.2,1.22188281799998));
#310394=CARTESIAN_POINT('Ctrl Pts',(-4.00545391400006,12.2,1.22186971399998));
#310395=CARTESIAN_POINT('Ctrl Pts',(-4.00545391400006,5.2,1.22186971399998));
#310396=CARTESIAN_POINT('Ctrl Pts',(-4.00545391400006,2.2,1.22186971399998));
#310397=CARTESIAN_POINT('Ctrl Pts',(-4.00693246700006,12.2,1.22185483399999));
#310398=CARTESIAN_POINT('Ctrl Pts',(-4.00693246700006,5.2,1.22185483399999));
#310399=CARTESIAN_POINT('Ctrl Pts',(-4.00693246700006,2.2,1.22185483399999));
#310400=CARTESIAN_POINT('Ctrl Pts',(-4.00841574600006,12.2,1.22183816999998));
#310401=CARTESIAN_POINT('Ctrl Pts',(-4.00841574600006,5.2,1.22183816999998));
#310402=CARTESIAN_POINT('Ctrl Pts',(-4.00841574600006,2.2,1.22183816999998));
#310403=CARTESIAN_POINT('Ctrl Pts',(-4.00990374000005,12.2,1.22181970999999));
#310404=CARTESIAN_POINT('Ctrl Pts',(-4.00990374000005,5.2,1.22181970999999));
#310405=CARTESIAN_POINT('Ctrl Pts',(-4.00990374000005,2.2,1.22181970999999));
#310406=CARTESIAN_POINT('Ctrl Pts',(-4.01139644200006,12.2,1.22179944599999));
#310407=CARTESIAN_POINT('Ctrl Pts',(-4.01139644200006,5.2,1.22179944599999));
#310408=CARTESIAN_POINT('Ctrl Pts',(-4.01139644200006,2.2,1.22179944599999));
#310409=CARTESIAN_POINT('Ctrl Pts',(-4.01289384200005,12.2,1.22177736499999));
#310410=CARTESIAN_POINT('Ctrl Pts',(-4.01289384200005,5.2,1.22177736499999));
#310411=CARTESIAN_POINT('Ctrl Pts',(-4.01289384200005,2.2,1.22177736499999));
#310412=CARTESIAN_POINT('Ctrl Pts',(-4.01439593200006,12.2,1.22175345999999));
#310413=CARTESIAN_POINT('Ctrl Pts',(-4.01439593200006,5.2,1.22175345999999));
#310414=CARTESIAN_POINT('Ctrl Pts',(-4.01439593200006,2.2,1.22175345999999));
#310415=CARTESIAN_POINT('Ctrl Pts',(-4.01590270300006,12.2,1.22172771799999));
#310416=CARTESIAN_POINT('Ctrl Pts',(-4.01590270300006,5.2,1.22172771799999));
#310417=CARTESIAN_POINT('Ctrl Pts',(-4.01590270300006,2.2,1.22172771799999));
#310418=CARTESIAN_POINT('Ctrl Pts',(-4.01741414500006,12.2,1.22170013199999));
#310419=CARTESIAN_POINT('Ctrl Pts',(-4.01741414500006,5.2,1.22170013199999));
#310420=CARTESIAN_POINT('Ctrl Pts',(-4.01741414500006,2.2,1.22170013199999));
#310421=CARTESIAN_POINT('Ctrl Pts',(-4.01893025000006,12.2,1.22167069099998));
#310422=CARTESIAN_POINT('Ctrl Pts',(-4.01893025000006,5.2,1.22167069099998));
#310423=CARTESIAN_POINT('Ctrl Pts',(-4.01893025000006,2.2,1.22167069099998));
#310424=CARTESIAN_POINT('Ctrl Pts',(-4.02045101100006,12.2,1.22163938299999));
#310425=CARTESIAN_POINT('Ctrl Pts',(-4.02045101100006,5.2,1.22163938299999));
#310426=CARTESIAN_POINT('Ctrl Pts',(-4.02045101100006,2.2,1.22163938299999));
#310427=CARTESIAN_POINT('Ctrl Pts',(-4.02197641600006,12.2,1.22160620099999));
#310428=CARTESIAN_POINT('Ctrl Pts',(-4.02197641600006,5.2,1.22160620099999));
#310429=CARTESIAN_POINT('Ctrl Pts',(-4.02197641600006,2.2,1.22160620099999));
#310430=CARTESIAN_POINT('Ctrl Pts',(-4.02350645800006,12.2,1.22157113399998));
#310431=CARTESIAN_POINT('Ctrl Pts',(-4.02350645800006,5.2,1.22157113399998));
#310432=CARTESIAN_POINT('Ctrl Pts',(-4.02350645800006,2.2,1.22157113399998));
#310433=CARTESIAN_POINT('Ctrl Pts',(-4.02504112800006,12.2,1.22153417099998));
#310434=CARTESIAN_POINT('Ctrl Pts',(-4.02504112800006,5.2,1.22153417099998));
#310435=CARTESIAN_POINT('Ctrl Pts',(-4.02504112800006,2.2,1.22153417099998));
#310436=CARTESIAN_POINT('Ctrl Pts',(-4.02658041700006,12.2,1.22149530499998));
#310437=CARTESIAN_POINT('Ctrl Pts',(-4.02658041700006,5.2,1.22149530499998));
#310438=CARTESIAN_POINT('Ctrl Pts',(-4.02658041700006,2.2,1.22149530499998));
#310439=CARTESIAN_POINT('Ctrl Pts',(-4.02812431700006,12.2,1.22145452299999));
#310440=CARTESIAN_POINT('Ctrl Pts',(-4.02812431700006,5.2,1.22145452299999));
#310441=CARTESIAN_POINT('Ctrl Pts',(-4.02812431700006,2.2,1.22145452299999));
#310442=CARTESIAN_POINT('Ctrl Pts',(-4.02967281800006,12.2,1.22141181799998));
#310443=CARTESIAN_POINT('Ctrl Pts',(-4.02967281800006,5.2,1.22141181799998));
#310444=CARTESIAN_POINT('Ctrl Pts',(-4.02967281800006,2.2,1.22141181799998));
#310445=CARTESIAN_POINT('Ctrl Pts',(-4.03122591200006,12.2,1.22136717899998));
#310446=CARTESIAN_POINT('Ctrl Pts',(-4.03122591200006,5.2,1.22136717899998));
#310447=CARTESIAN_POINT('Ctrl Pts',(-4.03122591200006,2.2,1.22136717899998));
#310448=CARTESIAN_POINT('Ctrl Pts',(-4.03278359100006,12.2,1.22132059599998));
#310449=CARTESIAN_POINT('Ctrl Pts',(-4.03278359100006,5.2,1.22132059599998));
#310450=CARTESIAN_POINT('Ctrl Pts',(-4.03278359100006,2.2,1.22132059599998));
#310451=CARTESIAN_POINT('Ctrl Pts',(-4.03434584400006,12.2,1.22127206099998));
#310452=CARTESIAN_POINT('Ctrl Pts',(-4.03434584400006,5.2,1.22127206099998));
#310453=CARTESIAN_POINT('Ctrl Pts',(-4.03434584400006,2.2,1.22127206099998));
#310454=CARTESIAN_POINT('Ctrl Pts',(-4.03591266300006,12.2,1.22122156299998));
#310455=CARTESIAN_POINT('Ctrl Pts',(-4.03591266300006,5.2,1.22122156299998));
#310456=CARTESIAN_POINT('Ctrl Pts',(-4.03591266300006,2.2,1.22122156299998));
#310457=CARTESIAN_POINT('Ctrl Pts',(-4.03748404100006,12.2,1.22116909199999));
#310458=CARTESIAN_POINT('Ctrl Pts',(-4.03748404100006,5.2,1.22116909199999));
#310459=CARTESIAN_POINT('Ctrl Pts',(-4.03748404100006,2.2,1.22116909199999));
#310460=CARTESIAN_POINT('Ctrl Pts',(-4.03905996800006,12.2,1.22111463899999));
#310461=CARTESIAN_POINT('Ctrl Pts',(-4.03905996800006,5.2,1.22111463899999));
#310462=CARTESIAN_POINT('Ctrl Pts',(-4.03905996800006,2.2,1.22111463899999));
#310463=CARTESIAN_POINT('Ctrl Pts',(-4.04064043500005,12.2,1.22105819399998));
#310464=CARTESIAN_POINT('Ctrl Pts',(-4.04064043500005,5.2,1.22105819399998));
#310465=CARTESIAN_POINT('Ctrl Pts',(-4.04064043500005,2.2,1.22105819399998));
#310466=CARTESIAN_POINT('Ctrl Pts',(-4.04222543400006,12.2,1.22099974999998));
#310467=CARTESIAN_POINT('Ctrl Pts',(-4.04222543400006,5.2,1.22099974999998));
#310468=CARTESIAN_POINT('Ctrl Pts',(-4.04222543400006,2.2,1.22099974999998));
#310469=CARTESIAN_POINT('Ctrl Pts',(-4.04381495400005,12.2,1.22093929399998));
#310470=CARTESIAN_POINT('Ctrl Pts',(-4.04381495400005,5.2,1.22093929399998));
#310471=CARTESIAN_POINT('Ctrl Pts',(-4.04381495400005,2.2,1.22093929399998));
#310472=CARTESIAN_POINT('Ctrl Pts',(-4.04540899000006,12.2,1.22087681899998));
#310473=CARTESIAN_POINT('Ctrl Pts',(-4.04540899000006,5.2,1.22087681899998));
#310474=CARTESIAN_POINT('Ctrl Pts',(-4.04540899000006,2.2,1.22087681899998));
#310475=CARTESIAN_POINT('Ctrl Pts',(-4.04700753000006,12.2,1.22081231499998));
#310476=CARTESIAN_POINT('Ctrl Pts',(-4.04700753000006,5.2,1.22081231499998));
#310477=CARTESIAN_POINT('Ctrl Pts',(-4.04700753000006,2.2,1.22081231499998));
#310478=CARTESIAN_POINT('Ctrl Pts',(-4.04861056700006,12.2,1.22074577299998));
#310479=CARTESIAN_POINT('Ctrl Pts',(-4.04861056700006,5.2,1.22074577299998));
#310480=CARTESIAN_POINT('Ctrl Pts',(-4.04861056700006,2.2,1.22074577299998));
#310481=CARTESIAN_POINT('Ctrl Pts',(-4.05021809200006,12.2,1.22067718299999));
#310482=CARTESIAN_POINT('Ctrl Pts',(-4.05021809200006,5.2,1.22067718299999));
#310483=CARTESIAN_POINT('Ctrl Pts',(-4.05021809200006,2.2,1.22067718299999));
#310484=CARTESIAN_POINT('Ctrl Pts',(-4.05183009600006,12.2,1.22060653499998));
#310485=CARTESIAN_POINT('Ctrl Pts',(-4.05183009600006,5.2,1.22060653499998));
#310486=CARTESIAN_POINT('Ctrl Pts',(-4.05183009600006,2.2,1.22060653499998));
#310487=CARTESIAN_POINT('Ctrl Pts',(-4.05344657100006,12.2,1.22053382099998));
#310488=CARTESIAN_POINT('Ctrl Pts',(-4.05344657100006,5.2,1.22053382099998));
#310489=CARTESIAN_POINT('Ctrl Pts',(-4.05344657100006,2.2,1.22053382099998));
#310490=CARTESIAN_POINT('Ctrl Pts',(-4.05506750700006,12.2,1.22045903099998));
#310491=CARTESIAN_POINT('Ctrl Pts',(-4.05506750700006,5.2,1.22045903099998));
#310492=CARTESIAN_POINT('Ctrl Pts',(-4.05506750700006,2.2,1.22045903099998));
#310493=CARTESIAN_POINT('Ctrl Pts',(-4.05669289600006,12.2,1.22038215699999));
#310494=CARTESIAN_POINT('Ctrl Pts',(-4.05669289600006,5.2,1.22038215699999));
#310495=CARTESIAN_POINT('Ctrl Pts',(-4.05669289600006,2.2,1.22038215699999));
#310496=CARTESIAN_POINT('Ctrl Pts',(-4.05832272900006,12.2,1.22030318799998));
#310497=CARTESIAN_POINT('Ctrl Pts',(-4.05832272900006,5.2,1.22030318799998));
#310498=CARTESIAN_POINT('Ctrl Pts',(-4.05832272900006,2.2,1.22030318799998));
#310499=CARTESIAN_POINT('Ctrl Pts',(-4.05995699900005,12.2,1.22022211699999));
#310500=CARTESIAN_POINT('Ctrl Pts',(-4.05995699900005,5.2,1.22022211699999));
#310501=CARTESIAN_POINT('Ctrl Pts',(-4.05995699900005,2.2,1.22022211699999));
#310502=CARTESIAN_POINT('Ctrl Pts',(-4.06159569400006,12.2,1.22013893199998));
#310503=CARTESIAN_POINT('Ctrl Pts',(-4.06159569400006,5.2,1.22013893199998));
#310504=CARTESIAN_POINT('Ctrl Pts',(-4.06159569400006,2.2,1.22013893199998));
#310505=CARTESIAN_POINT('Ctrl Pts',(-4.06323880800006,12.2,1.22005362699999));
#310506=CARTESIAN_POINT('Ctrl Pts',(-4.06323880800006,5.2,1.22005362699999));
#310507=CARTESIAN_POINT('Ctrl Pts',(-4.06323880800006,2.2,1.22005362699999));
#310508=CARTESIAN_POINT('Ctrl Pts',(-4.06488633200006,12.2,1.21996618999999));
#310509=CARTESIAN_POINT('Ctrl Pts',(-4.06488633200006,5.2,1.21996618999999));
#310510=CARTESIAN_POINT('Ctrl Pts',(-4.06488633200006,2.2,1.21996618999999));
#310511=CARTESIAN_POINT('Ctrl Pts',(-4.06653825600006,12.2,1.21987661499999));
#310512=CARTESIAN_POINT('Ctrl Pts',(-4.06653825600006,5.2,1.21987661499999));
#310513=CARTESIAN_POINT('Ctrl Pts',(-4.06653825600006,2.2,1.21987661499999));
#310514=CARTESIAN_POINT('Ctrl Pts',(-4.06819457300006,12.2,1.21978488999999));
#310515=CARTESIAN_POINT('Ctrl Pts',(-4.06819457300006,5.2,1.21978488999999));
#310516=CARTESIAN_POINT('Ctrl Pts',(-4.06819457300006,2.2,1.21978488999999));
#310517=CARTESIAN_POINT('Ctrl Pts',(-4.06985527300006,12.2,1.21969100899999));
#310518=CARTESIAN_POINT('Ctrl Pts',(-4.06985527300006,5.2,1.21969100899999));
#310519=CARTESIAN_POINT('Ctrl Pts',(-4.06985527300006,2.2,1.21969100899999));
#310520=CARTESIAN_POINT('Ctrl Pts',(-4.07152034800006,12.2,1.21959495999999));
#310521=CARTESIAN_POINT('Ctrl Pts',(-4.07152034800006,5.2,1.21959495999999));
#310522=CARTESIAN_POINT('Ctrl Pts',(-4.07152034800006,2.2,1.21959495999999));
#310523=CARTESIAN_POINT('Ctrl Pts',(-4.07318978900006,12.2,1.21949673599998));
#310524=CARTESIAN_POINT('Ctrl Pts',(-4.07318978900006,5.2,1.21949673599998));
#310525=CARTESIAN_POINT('Ctrl Pts',(-4.07318978900006,2.2,1.21949673599998));
#310526=CARTESIAN_POINT('Ctrl Pts',(-4.07486358800006,12.2,1.21939632799998));
#310527=CARTESIAN_POINT('Ctrl Pts',(-4.07486358800006,5.2,1.21939632799998));
#310528=CARTESIAN_POINT('Ctrl Pts',(-4.07486358800006,2.2,1.21939632799998));
#310529=CARTESIAN_POINT('Ctrl Pts',(-4.07654173500006,12.2,1.21929372599999));
#310530=CARTESIAN_POINT('Ctrl Pts',(-4.07654173500006,5.2,1.21929372599999));
#310531=CARTESIAN_POINT('Ctrl Pts',(-4.07654173500006,2.2,1.21929372599999));
#310532=CARTESIAN_POINT('Ctrl Pts',(-4.07822422300006,12.2,1.21918892199998));
#310533=CARTESIAN_POINT('Ctrl Pts',(-4.07822422300006,5.2,1.21918892199998));
#310534=CARTESIAN_POINT('Ctrl Pts',(-4.07822422300006,2.2,1.21918892199998));
#310535=CARTESIAN_POINT('Ctrl Pts',(-4.07991104100006,12.2,1.21908190799998));
#310536=CARTESIAN_POINT('Ctrl Pts',(-4.07991104100006,5.2,1.21908190799998));
#310537=CARTESIAN_POINT('Ctrl Pts',(-4.07991104100006,2.2,1.21908190799998));
#310538=CARTESIAN_POINT('Ctrl Pts',(-4.08160218300006,12.2,1.21897267399998));
#310539=CARTESIAN_POINT('Ctrl Pts',(-4.08160218300006,5.2,1.21897267399998));
#310540=CARTESIAN_POINT('Ctrl Pts',(-4.08160218300006,2.2,1.21897267399998));
#310541=CARTESIAN_POINT('Ctrl Pts',(-4.08329763900006,12.2,1.21886121099998));
#310542=CARTESIAN_POINT('Ctrl Pts',(-4.08329763900006,5.2,1.21886121099998));
#310543=CARTESIAN_POINT('Ctrl Pts',(-4.08329763900006,2.2,1.21886121099998));
#310544=CARTESIAN_POINT('Ctrl Pts',(-4.08499740100006,12.2,1.21874751099998));
#310545=CARTESIAN_POINT('Ctrl Pts',(-4.08499740100006,5.2,1.21874751099998));
#310546=CARTESIAN_POINT('Ctrl Pts',(-4.08499740100006,2.2,1.21874751099998));
#310547=CARTESIAN_POINT('Ctrl Pts',(-4.08670146000006,12.2,1.21863156499999));
#310548=CARTESIAN_POINT('Ctrl Pts',(-4.08670146000006,5.2,1.21863156499999));
#310549=CARTESIAN_POINT('Ctrl Pts',(-4.08670146000006,2.2,1.21863156499999));
#310550=CARTESIAN_POINT('Ctrl Pts',(-4.08840980700006,12.2,1.21851336499998));
#310551=CARTESIAN_POINT('Ctrl Pts',(-4.08840980700006,5.2,1.21851336499998));
#310552=CARTESIAN_POINT('Ctrl Pts',(-4.08840980700006,2.2,1.21851336499998));
#310553=CARTESIAN_POINT('Ctrl Pts',(-4.09012243300006,12.2,1.21839290099999));
#310554=CARTESIAN_POINT('Ctrl Pts',(-4.09012243300006,5.2,1.21839290099999));
#310555=CARTESIAN_POINT('Ctrl Pts',(-4.09012243300006,2.2,1.21839290099999));
#310556=CARTESIAN_POINT('Ctrl Pts',(-4.09183933100006,12.2,1.21827016599998));
#310557=CARTESIAN_POINT('Ctrl Pts',(-4.09183933100006,5.2,1.21827016599998));
#310558=CARTESIAN_POINT('Ctrl Pts',(-4.09183933100006,2.2,1.21827016599998));
#310559=CARTESIAN_POINT('Ctrl Pts',(-4.09356049200006,12.2,1.21814514999999));
#310560=CARTESIAN_POINT('Ctrl Pts',(-4.09356049200006,5.2,1.21814514999999));
#310561=CARTESIAN_POINT('Ctrl Pts',(-4.09356049200006,2.2,1.21814514999999));
#310562=CARTESIAN_POINT('Ctrl Pts',(-4.09528590600006,12.2,1.21801784499999));
#310563=CARTESIAN_POINT('Ctrl Pts',(-4.09528590600006,5.2,1.21801784499999));
#310564=CARTESIAN_POINT('Ctrl Pts',(-4.09528590600006,2.2,1.21801784499999));
#310565=CARTESIAN_POINT('Ctrl Pts',(-4.09701556600006,12.2,1.21788824299998));
#310566=CARTESIAN_POINT('Ctrl Pts',(-4.09701556600006,5.2,1.21788824299998));
#310567=CARTESIAN_POINT('Ctrl Pts',(-4.09701556600006,2.2,1.21788824299998));
#310568=CARTESIAN_POINT('Ctrl Pts',(-4.09874946100006,12.2,1.21775633399999));
#310569=CARTESIAN_POINT('Ctrl Pts',(-4.09874946100006,5.2,1.21775633399999));
#310570=CARTESIAN_POINT('Ctrl Pts',(-4.09874946100006,2.2,1.21775633399999));
#310571=CARTESIAN_POINT('Ctrl Pts',(-4.10048758500006,12.2,1.21762211099998));
#310572=CARTESIAN_POINT('Ctrl Pts',(-4.10048758500006,5.2,1.21762211099998));
#310573=CARTESIAN_POINT('Ctrl Pts',(-4.10048758500006,2.2,1.21762211099998));
#310574=CARTESIAN_POINT('Ctrl Pts',(-4.10222992800006,12.2,1.21748556499998));
#310575=CARTESIAN_POINT('Ctrl Pts',(-4.10222992800006,5.2,1.21748556499998));
#310576=CARTESIAN_POINT('Ctrl Pts',(-4.10222992800006,2.2,1.21748556499998));
#310577=CARTESIAN_POINT('Ctrl Pts',(-4.10397648300005,12.2,1.21734668799999));
#310578=CARTESIAN_POINT('Ctrl Pts',(-4.10397648300005,5.2,1.21734668799999));
#310579=CARTESIAN_POINT('Ctrl Pts',(-4.10397648300005,2.2,1.21734668799999));
#310580=CARTESIAN_POINT('Ctrl Pts',(-4.10572724000006,12.2,1.21720546999999));
#310581=CARTESIAN_POINT('Ctrl Pts',(-4.10572724000006,5.2,1.21720546999999));
#310582=CARTESIAN_POINT('Ctrl Pts',(-4.10572724000006,2.2,1.21720546999999));
#310583=CARTESIAN_POINT('Ctrl Pts',(-4.10748219000006,12.2,1.21706190499999));
#310584=CARTESIAN_POINT('Ctrl Pts',(-4.10748219000006,5.2,1.21706190499999));
#310585=CARTESIAN_POINT('Ctrl Pts',(-4.10748219000006,2.2,1.21706190499999));
#310586=CARTESIAN_POINT('Ctrl Pts',(-4.10924132600006,12.2,1.21691598299998));
#310587=CARTESIAN_POINT('Ctrl Pts',(-4.10924132600006,5.2,1.21691598299998));
#310588=CARTESIAN_POINT('Ctrl Pts',(-4.10924132600006,2.2,1.21691598299998));
#310589=CARTESIAN_POINT('Ctrl Pts',(-4.11100463700006,12.2,1.21676769599999));
#310590=CARTESIAN_POINT('Ctrl Pts',(-4.11100463700006,5.2,1.21676769599999));
#310591=CARTESIAN_POINT('Ctrl Pts',(-4.11100463700006,2.2,1.21676769599999));
#310592=CARTESIAN_POINT('Ctrl Pts',(-4.11277211800006,12.2,1.21661703499999));
#310593=CARTESIAN_POINT('Ctrl Pts',(-4.11277211800006,5.2,1.21661703499999));
#310594=CARTESIAN_POINT('Ctrl Pts',(-4.11277211800006,2.2,1.21661703499999));
#310595=CARTESIAN_POINT('Ctrl Pts',(-4.11454375600006,12.2,1.21646399399999));
#310596=CARTESIAN_POINT('Ctrl Pts',(-4.11454375600006,5.2,1.21646399399999));
#310597=CARTESIAN_POINT('Ctrl Pts',(-4.11454375600006,2.2,1.21646399399999));
#310598=CARTESIAN_POINT('Ctrl Pts',(-4.11631954700006,12.2,1.21630856299999));
#310599=CARTESIAN_POINT('Ctrl Pts',(-4.11631954700006,5.2,1.21630856299999));
#310600=CARTESIAN_POINT('Ctrl Pts',(-4.11631954700006,2.2,1.21630856299999));
#310601=CARTESIAN_POINT('Ctrl Pts',(-4.11809947900006,12.2,1.21615073299999));
#310602=CARTESIAN_POINT('Ctrl Pts',(-4.11809947900006,5.2,1.21615073299999));
#310603=CARTESIAN_POINT('Ctrl Pts',(-4.11809947900006,2.2,1.21615073299999));
#310604=CARTESIAN_POINT('Ctrl Pts',(-4.11988354400005,12.2,1.21599049699999));
#310605=CARTESIAN_POINT('Ctrl Pts',(-4.11988354400005,5.2,1.21599049699999));
#310606=CARTESIAN_POINT('Ctrl Pts',(-4.11988354400005,2.2,1.21599049699999));
#310607=CARTESIAN_POINT('Ctrl Pts',(-4.12167173600006,12.2,1.21582784799998));
#310608=CARTESIAN_POINT('Ctrl Pts',(-4.12167173600006,5.2,1.21582784799998));
#310609=CARTESIAN_POINT('Ctrl Pts',(-4.12167173600006,2.2,1.21582784799998));
#310610=CARTESIAN_POINT('Ctrl Pts',(-4.12346404300005,12.2,1.21566277499999));
#310611=CARTESIAN_POINT('Ctrl Pts',(-4.12346404300005,5.2,1.21566277499999));
#310612=CARTESIAN_POINT('Ctrl Pts',(-4.12346404300005,2.2,1.21566277499999));
#310613=CARTESIAN_POINT('Ctrl Pts',(-4.12526045900006,12.2,1.21549527199999));
#310614=CARTESIAN_POINT('Ctrl Pts',(-4.12526045900006,5.2,1.21549527199999));
#310615=CARTESIAN_POINT('Ctrl Pts',(-4.12526045900006,2.2,1.21549527199999));
#310616=CARTESIAN_POINT('Ctrl Pts',(-4.12706097400006,12.2,1.21532533099999));
#310617=CARTESIAN_POINT('Ctrl Pts',(-4.12706097400006,5.2,1.21532533099999));
#310618=CARTESIAN_POINT('Ctrl Pts',(-4.12706097400006,2.2,1.21532533099999));
#310619=CARTESIAN_POINT('Ctrl Pts',(-4.12886558100006,12.2,1.21515294199999));
#310620=CARTESIAN_POINT('Ctrl Pts',(-4.12886558100006,5.2,1.21515294199999));
#310621=CARTESIAN_POINT('Ctrl Pts',(-4.12886558100006,2.2,1.21515294199999));
#310622=CARTESIAN_POINT('Ctrl Pts',(-4.13067426900006,12.2,1.21497809899999));
#310623=CARTESIAN_POINT('Ctrl Pts',(-4.13067426900006,5.2,1.21497809899999));
#310624=CARTESIAN_POINT('Ctrl Pts',(-4.13067426900006,2.2,1.21497809899999));
#310625=CARTESIAN_POINT('Ctrl Pts',(-4.13248703200006,12.2,1.21480079399999));
#310626=CARTESIAN_POINT('Ctrl Pts',(-4.13248703200006,5.2,1.21480079399999));
#310627=CARTESIAN_POINT('Ctrl Pts',(-4.13248703200006,2.2,1.21480079399999));
#310628=CARTESIAN_POINT('Ctrl Pts',(-4.13430386000006,12.2,1.21462101699999));
#310629=CARTESIAN_POINT('Ctrl Pts',(-4.13430386000006,5.2,1.21462101699999));
#310630=CARTESIAN_POINT('Ctrl Pts',(-4.13430386000006,2.2,1.21462101699999));
#310631=CARTESIAN_POINT('Ctrl Pts',(-4.13612474400006,12.2,1.21443876199999));
#310632=CARTESIAN_POINT('Ctrl Pts',(-4.13612474400006,5.2,1.21443876199999));
#310633=CARTESIAN_POINT('Ctrl Pts',(-4.13612474400006,2.2,1.21443876199999));
#310634=CARTESIAN_POINT('Ctrl Pts',(-4.13794967700006,12.2,1.21425401899999));
#310635=CARTESIAN_POINT('Ctrl Pts',(-4.13794967700006,5.2,1.21425401899999));
#310636=CARTESIAN_POINT('Ctrl Pts',(-4.13794967700006,2.2,1.21425401899999));
#310637=CARTESIAN_POINT('Ctrl Pts',(-4.13977865000006,12.2,1.21406678299998));
#310638=CARTESIAN_POINT('Ctrl Pts',(-4.13977865000006,5.2,1.21406678299998));
#310639=CARTESIAN_POINT('Ctrl Pts',(-4.13977865000006,2.2,1.21406678299998));
#310640=CARTESIAN_POINT('Ctrl Pts',(-4.14161165400006,12.2,1.21387704299998));
#310641=CARTESIAN_POINT('Ctrl Pts',(-4.14161165400006,5.2,1.21387704299998));
#310642=CARTESIAN_POINT('Ctrl Pts',(-4.14161165400006,2.2,1.21387704299998));
#310643=CARTESIAN_POINT('Ctrl Pts',(-4.14344868100006,12.2,1.21368479399999));
#310644=CARTESIAN_POINT('Ctrl Pts',(-4.14344868100006,5.2,1.21368479399999));
#310645=CARTESIAN_POINT('Ctrl Pts',(-4.14344868100006,2.2,1.21368479399999));
#310646=CARTESIAN_POINT('Ctrl Pts',(-4.14528972300006,12.2,1.21349002599999));
#310647=CARTESIAN_POINT('Ctrl Pts',(-4.14528972300006,5.2,1.21349002599999));
#310648=CARTESIAN_POINT('Ctrl Pts',(-4.14528972300006,2.2,1.21349002599999));
#310649=CARTESIAN_POINT('Ctrl Pts',(-4.14713477000006,12.2,1.21329273299999));
#310650=CARTESIAN_POINT('Ctrl Pts',(-4.14713477000006,5.2,1.21329273299999));
#310651=CARTESIAN_POINT('Ctrl Pts',(-4.14713477000006,2.2,1.21329273299999));
#310652=CARTESIAN_POINT('Ctrl Pts',(-4.14898381500006,12.2,1.21309290499998));
#310653=CARTESIAN_POINT('Ctrl Pts',(-4.14898381500006,5.2,1.21309290499998));
#310654=CARTESIAN_POINT('Ctrl Pts',(-4.14898381500006,2.2,1.21309290499998));
#310655=CARTESIAN_POINT('Ctrl Pts',(-4.15083684800006,12.2,1.21289053599998));
#310656=CARTESIAN_POINT('Ctrl Pts',(-4.15083684800006,5.2,1.21289053599998));
#310657=CARTESIAN_POINT('Ctrl Pts',(-4.15083684800006,2.2,1.21289053599998));
#310658=CARTESIAN_POINT('Ctrl Pts',(-4.15269386100006,12.2,1.21268561699999));
#310659=CARTESIAN_POINT('Ctrl Pts',(-4.15269386100006,5.2,1.21268561699999));
#310660=CARTESIAN_POINT('Ctrl Pts',(-4.15269386100006,2.2,1.21268561699999));
#310661=CARTESIAN_POINT('Ctrl Pts',(-4.15455484700006,12.2,1.21247814199998));
#310662=CARTESIAN_POINT('Ctrl Pts',(-4.15455484700006,5.2,1.21247814199998));
#310663=CARTESIAN_POINT('Ctrl Pts',(-4.15455484700006,2.2,1.21247814199998));
#310664=CARTESIAN_POINT('Ctrl Pts',(-4.15641979500006,12.2,1.21226810299999));
#310665=CARTESIAN_POINT('Ctrl Pts',(-4.15641979500006,5.2,1.21226810299999));
#310666=CARTESIAN_POINT('Ctrl Pts',(-4.15641979500006,2.2,1.21226810299999));
#310667=CARTESIAN_POINT('Ctrl Pts',(-4.15828869900006,12.2,1.21205548999999));
#310668=CARTESIAN_POINT('Ctrl Pts',(-4.15828869900006,5.2,1.21205548999999));
#310669=CARTESIAN_POINT('Ctrl Pts',(-4.15828869900006,2.2,1.21205548999999));
#310670=CARTESIAN_POINT('Ctrl Pts',(-4.16016154900006,12.2,1.21184029699998));
#310671=CARTESIAN_POINT('Ctrl Pts',(-4.16016154900006,5.2,1.21184029699998));
#310672=CARTESIAN_POINT('Ctrl Pts',(-4.16016154900006,2.2,1.21184029699998));
#310673=CARTESIAN_POINT('Ctrl Pts',(-4.16203833700005,12.2,1.21162251699999));
#310674=CARTESIAN_POINT('Ctrl Pts',(-4.16203833700005,5.2,1.21162251699999));
#310675=CARTESIAN_POINT('Ctrl Pts',(-4.16203833700005,2.2,1.21162251699999));
#310676=CARTESIAN_POINT('Ctrl Pts',(-4.16391905500006,12.2,1.21140214299999));
#310677=CARTESIAN_POINT('Ctrl Pts',(-4.16391905500006,5.2,1.21140214299999));
#310678=CARTESIAN_POINT('Ctrl Pts',(-4.16391905500006,2.2,1.21140214299999));
#310679=CARTESIAN_POINT('Ctrl Pts',(-4.16580369400006,12.2,1.21117916399998));
#310680=CARTESIAN_POINT('Ctrl Pts',(-4.16580369400006,5.2,1.21117916399998));
#310681=CARTESIAN_POINT('Ctrl Pts',(-4.16580369400006,2.2,1.21117916399998));
#310682=CARTESIAN_POINT('Ctrl Pts',(-4.16769224400006,12.2,1.21095357599998));
#310683=CARTESIAN_POINT('Ctrl Pts',(-4.16769224400006,5.2,1.21095357599998));
#310684=CARTESIAN_POINT('Ctrl Pts',(-4.16769224400006,2.2,1.21095357599998));
#310685=CARTESIAN_POINT('Ctrl Pts',(-4.16958470100006,12.2,1.21072537099999));
#310686=CARTESIAN_POINT('Ctrl Pts',(-4.16958470100006,5.2,1.21072537099999));
#310687=CARTESIAN_POINT('Ctrl Pts',(-4.16958470100006,2.2,1.21072537099999));
#310688=CARTESIAN_POINT('Ctrl Pts',(-4.17148105100006,12.2,1.21049453899999));
#310689=CARTESIAN_POINT('Ctrl Pts',(-4.17148105100006,5.2,1.21049453899999));
#310690=CARTESIAN_POINT('Ctrl Pts',(-4.17148105100006,2.2,1.21049453899999));
#310691=CARTESIAN_POINT('Ctrl Pts',(-4.17338129000006,12.2,1.21026107499999));
#310692=CARTESIAN_POINT('Ctrl Pts',(-4.17338129000006,5.2,1.21026107499999));
#310693=CARTESIAN_POINT('Ctrl Pts',(-4.17338129000006,2.2,1.21026107499999));
#310694=CARTESIAN_POINT('Ctrl Pts',(-4.17528540700006,12.2,1.21002497099999));
#310695=CARTESIAN_POINT('Ctrl Pts',(-4.17528540700006,5.2,1.21002497099999));
#310696=CARTESIAN_POINT('Ctrl Pts',(-4.17528540700006,2.2,1.21002497099999));
#310697=CARTESIAN_POINT('Ctrl Pts',(-4.17719339400006,12.2,1.20978621799999));
#310698=CARTESIAN_POINT('Ctrl Pts',(-4.17719339400006,5.2,1.20978621799999));
#310699=CARTESIAN_POINT('Ctrl Pts',(-4.17719339400006,2.2,1.20978621799999));
#310700=CARTESIAN_POINT('Ctrl Pts',(-4.17910524400006,12.2,1.20954481199998));
#310701=CARTESIAN_POINT('Ctrl Pts',(-4.17910524400006,5.2,1.20954481199998));
#310702=CARTESIAN_POINT('Ctrl Pts',(-4.17910524400006,2.2,1.20954481199998));
#310703=CARTESIAN_POINT('Ctrl Pts',(-4.18102094700005,12.2,1.20930074099999));
#310704=CARTESIAN_POINT('Ctrl Pts',(-4.18102094700005,5.2,1.20930074099999));
#310705=CARTESIAN_POINT('Ctrl Pts',(-4.18102094700005,2.2,1.20930074099999));
#310706=CARTESIAN_POINT('Ctrl Pts',(-4.18294049500005,12.2,1.20905400199999));
#310707=CARTESIAN_POINT('Ctrl Pts',(-4.18294049500005,5.2,1.20905400199999));
#310708=CARTESIAN_POINT('Ctrl Pts',(-4.18294049500005,2.2,1.20905400199999));
#310709=CARTESIAN_POINT('Ctrl Pts',(-4.18486388000006,12.2,1.20880458599999));
#310710=CARTESIAN_POINT('Ctrl Pts',(-4.18486388000006,5.2,1.20880458599999));
#310711=CARTESIAN_POINT('Ctrl Pts',(-4.18486388000006,2.2,1.20880458599999));
#310712=CARTESIAN_POINT('Ctrl Pts',(-4.18679109200006,12.2,1.20855248499999));
#310713=CARTESIAN_POINT('Ctrl Pts',(-4.18679109200006,5.2,1.20855248499999));
#310714=CARTESIAN_POINT('Ctrl Pts',(-4.18679109200006,2.2,1.20855248499999));
#310715=CARTESIAN_POINT('Ctrl Pts',(-4.18872212500006,12.2,1.20829769199998));
#310716=CARTESIAN_POINT('Ctrl Pts',(-4.18872212500006,5.2,1.20829769199998));
#310717=CARTESIAN_POINT('Ctrl Pts',(-4.18872212500006,2.2,1.20829769199998));
#310718=CARTESIAN_POINT('Ctrl Pts',(-4.19065696900006,12.2,1.20804020099999));
#310719=CARTESIAN_POINT('Ctrl Pts',(-4.19065696900006,5.2,1.20804020099999));
#310720=CARTESIAN_POINT('Ctrl Pts',(-4.19065696900006,2.2,1.20804020099999));
#310721=CARTESIAN_POINT('Ctrl Pts',(-4.19259561700006,12.2,1.20778000299998));
#310722=CARTESIAN_POINT('Ctrl Pts',(-4.19259561700006,5.2,1.20778000299998));
#310723=CARTESIAN_POINT('Ctrl Pts',(-4.19259561700006,2.2,1.20778000299998));
#310724=CARTESIAN_POINT('Ctrl Pts',(-4.19453805800006,12.2,1.20751709199999));
#310725=CARTESIAN_POINT('Ctrl Pts',(-4.19453805800006,5.2,1.20751709199999));
#310726=CARTESIAN_POINT('Ctrl Pts',(-4.19453805800006,2.2,1.20751709199999));
#310727=CARTESIAN_POINT('Ctrl Pts',(-4.19648428600006,12.2,1.20725145999999));
#310728=CARTESIAN_POINT('Ctrl Pts',(-4.19648428600006,5.2,1.20725145999999));
#310729=CARTESIAN_POINT('Ctrl Pts',(-4.19648428600006,2.2,1.20725145999999));
#310730=CARTESIAN_POINT('Ctrl Pts',(-4.19843429200006,12.2,1.20698310099999));
#310731=CARTESIAN_POINT('Ctrl Pts',(-4.19843429200006,5.2,1.20698310099999));
#310732=CARTESIAN_POINT('Ctrl Pts',(-4.19843429200006,2.2,1.20698310099999));
#310733=CARTESIAN_POINT('Ctrl Pts',(-4.20038806700005,12.2,1.20671200599999));
#310734=CARTESIAN_POINT('Ctrl Pts',(-4.20038806700005,5.2,1.20671200599999));
#310735=CARTESIAN_POINT('Ctrl Pts',(-4.20038806700005,2.2,1.20671200599999));
#310736=CARTESIAN_POINT('Ctrl Pts',(-4.20234560400006,12.2,1.20643816999999));
#310737=CARTESIAN_POINT('Ctrl Pts',(-4.20234560400006,5.2,1.20643816999999));
#310738=CARTESIAN_POINT('Ctrl Pts',(-4.20234560400006,2.2,1.20643816999999));
#310739=CARTESIAN_POINT('Ctrl Pts',(-4.20430689200006,12.2,1.20616158499999));
#310740=CARTESIAN_POINT('Ctrl Pts',(-4.20430689200006,5.2,1.20616158499999));
#310741=CARTESIAN_POINT('Ctrl Pts',(-4.20430689200006,2.2,1.20616158499999));
#310742=CARTESIAN_POINT('Ctrl Pts',(-4.20627192600006,12.2,1.20588224299999));
#310743=CARTESIAN_POINT('Ctrl Pts',(-4.20627192600006,5.2,1.20588224299999));
#310744=CARTESIAN_POINT('Ctrl Pts',(-4.20627192600006,2.2,1.20588224299999));
#310745=CARTESIAN_POINT('Ctrl Pts',(-4.20824069400005,12.2,1.20560013799999));
#310746=CARTESIAN_POINT('Ctrl Pts',(-4.20824069400005,5.2,1.20560013799999));
#310747=CARTESIAN_POINT('Ctrl Pts',(-4.20824069400005,2.2,1.20560013799999));
#310748=CARTESIAN_POINT('Ctrl Pts',(-4.21021319200006,12.2,1.20531526299999));
#310749=CARTESIAN_POINT('Ctrl Pts',(-4.21021319200006,5.2,1.20531526299999));
#310750=CARTESIAN_POINT('Ctrl Pts',(-4.21021319200006,2.2,1.20531526299999));
#310751=CARTESIAN_POINT('Ctrl Pts',(-4.21218940700006,12.2,1.20502761099999));
#310752=CARTESIAN_POINT('Ctrl Pts',(-4.21218940700006,5.2,1.20502761099999));
#310753=CARTESIAN_POINT('Ctrl Pts',(-4.21218940700006,2.2,1.20502761099999));
#310754=CARTESIAN_POINT('Ctrl Pts',(-4.21416933400006,12.2,1.20473717299999));
#310755=CARTESIAN_POINT('Ctrl Pts',(-4.21416933400006,5.2,1.20473717299999));
#310756=CARTESIAN_POINT('Ctrl Pts',(-4.21416933400006,2.2,1.20473717299999));
#310757=CARTESIAN_POINT('Ctrl Pts',(-4.21615296300006,12.2,1.20444394499998));
#310758=CARTESIAN_POINT('Ctrl Pts',(-4.21615296300006,5.2,1.20444394499998));
#310759=CARTESIAN_POINT('Ctrl Pts',(-4.21615296300006,2.2,1.20444394499998));
#310760=CARTESIAN_POINT('Ctrl Pts',(-4.21814028600005,12.2,1.20414791999998));
#310761=CARTESIAN_POINT('Ctrl Pts',(-4.21814028600005,5.2,1.20414791999998));
#310762=CARTESIAN_POINT('Ctrl Pts',(-4.21814028600005,2.2,1.20414791999998));
#310763=CARTESIAN_POINT('Ctrl Pts',(-4.22013129500006,12.2,1.20384908899998));
#310764=CARTESIAN_POINT('Ctrl Pts',(-4.22013129500006,5.2,1.20384908899998));
#310765=CARTESIAN_POINT('Ctrl Pts',(-4.22013129500006,2.2,1.20384908899998));
#310766=CARTESIAN_POINT('Ctrl Pts',(-4.22212598100006,12.2,1.20354744499998));
#310767=CARTESIAN_POINT('Ctrl Pts',(-4.22212598100006,5.2,1.20354744499998));
#310768=CARTESIAN_POINT('Ctrl Pts',(-4.22212598100006,2.2,1.20354744499998));
#310769=CARTESIAN_POINT('Ctrl Pts',(-4.22412433700006,12.2,1.20324298299999));
#310770=CARTESIAN_POINT('Ctrl Pts',(-4.22412433700006,5.2,1.20324298299999));
#310771=CARTESIAN_POINT('Ctrl Pts',(-4.22412433700006,2.2,1.20324298299999));
#310772=CARTESIAN_POINT('Ctrl Pts',(-4.22612635400006,12.2,1.20293569499998));
#310773=CARTESIAN_POINT('Ctrl Pts',(-4.22612635400006,5.2,1.20293569499998));
#310774=CARTESIAN_POINT('Ctrl Pts',(-4.22612635400006,2.2,1.20293569499998));
#310775=CARTESIAN_POINT('Ctrl Pts',(-4.22813202200006,12.2,1.20262557599998));
#310776=CARTESIAN_POINT('Ctrl Pts',(-4.22813202200006,5.2,1.20262557599998));
#310777=CARTESIAN_POINT('Ctrl Pts',(-4.22813202200006,2.2,1.20262557599998));
#310778=CARTESIAN_POINT('Ctrl Pts',(-4.23014133400006,12.2,1.20231261699999));
#310779=CARTESIAN_POINT('Ctrl Pts',(-4.23014133400006,5.2,1.20231261699999));
#310780=CARTESIAN_POINT('Ctrl Pts',(-4.23014133400006,2.2,1.20231261699999));
#310781=CARTESIAN_POINT('Ctrl Pts',(-4.23215428300006,12.2,1.20199681099999));
#310782=CARTESIAN_POINT('Ctrl Pts',(-4.23215428300006,5.2,1.20199681099999));
#310783=CARTESIAN_POINT('Ctrl Pts',(-4.23215428300006,2.2,1.20199681099999));
#310784=CARTESIAN_POINT('Ctrl Pts',(-4.23417085900006,12.2,1.20167815299999));
#310785=CARTESIAN_POINT('Ctrl Pts',(-4.23417085900006,5.2,1.20167815299999));
#310786=CARTESIAN_POINT('Ctrl Pts',(-4.23417085900006,2.2,1.20167815299999));
#310787=CARTESIAN_POINT('Ctrl Pts',(-4.23619105300006,12.2,1.20135663499998));
#310788=CARTESIAN_POINT('Ctrl Pts',(-4.23619105300006,5.2,1.20135663499998));
#310789=CARTESIAN_POINT('Ctrl Pts',(-4.23619105300006,2.2,1.20135663499998));
#310790=CARTESIAN_POINT('Ctrl Pts',(-4.23821485900006,12.2,1.20103224999998));
#310791=CARTESIAN_POINT('Ctrl Pts',(-4.23821485900006,5.2,1.20103224999998));
#310792=CARTESIAN_POINT('Ctrl Pts',(-4.23821485900006,2.2,1.20103224999998));
#310793=CARTESIAN_POINT('Ctrl Pts',(-4.24024226600006,12.2,1.20070499299999));
#310794=CARTESIAN_POINT('Ctrl Pts',(-4.24024226600006,5.2,1.20070499299999));
#310795=CARTESIAN_POINT('Ctrl Pts',(-4.24024226600006,2.2,1.20070499299999));
#310796=CARTESIAN_POINT('Ctrl Pts',(-4.24227326800006,12.2,1.20037485699998));
#310797=CARTESIAN_POINT('Ctrl Pts',(-4.24227326800006,5.2,1.20037485699998));
#310798=CARTESIAN_POINT('Ctrl Pts',(-4.24227326800006,2.2,1.20037485699998));
#310799=CARTESIAN_POINT('Ctrl Pts',(-4.24430785700006,12.2,1.20004183399999));
#310800=CARTESIAN_POINT('Ctrl Pts',(-4.24430785700006,5.2,1.20004183399999));
#310801=CARTESIAN_POINT('Ctrl Pts',(-4.24430785700006,2.2,1.20004183399999));
#310802=CARTESIAN_POINT('Ctrl Pts',(-4.24634602200006,12.2,1.19970591699999));
#310803=CARTESIAN_POINT('Ctrl Pts',(-4.24634602200006,5.2,1.19970591699999));
#310804=CARTESIAN_POINT('Ctrl Pts',(-4.24634602200006,2.2,1.19970591699999));
#310805=CARTESIAN_POINT('Ctrl Pts',(-4.24838775700006,12.2,1.19936710199998));
#310806=CARTESIAN_POINT('Ctrl Pts',(-4.24838775700006,5.2,1.19936710199998));
#310807=CARTESIAN_POINT('Ctrl Pts',(-4.24838775700006,2.2,1.19936710199998));
#310808=CARTESIAN_POINT('Ctrl Pts',(-4.25043305200006,12.2,1.19902537999999));
#310809=CARTESIAN_POINT('Ctrl Pts',(-4.25043305200006,5.2,1.19902537999999));
#310810=CARTESIAN_POINT('Ctrl Pts',(-4.25043305200006,2.2,1.19902537999999));
#310811=CARTESIAN_POINT('Ctrl Pts',(-4.25248190000006,12.2,1.19868074599998));
#310812=CARTESIAN_POINT('Ctrl Pts',(-4.25248190000006,5.2,1.19868074599998));
#310813=CARTESIAN_POINT('Ctrl Pts',(-4.25248190000006,2.2,1.19868074599998));
#310814=CARTESIAN_POINT('Ctrl Pts',(-4.25453429300005,12.2,1.19833319199998));
#310815=CARTESIAN_POINT('Ctrl Pts',(-4.25453429300005,5.2,1.19833319199998));
#310816=CARTESIAN_POINT('Ctrl Pts',(-4.25453429300005,2.2,1.19833319199998));
#310817=CARTESIAN_POINT('Ctrl Pts',(-4.25659022200006,12.2,1.19798271199999));
#310818=CARTESIAN_POINT('Ctrl Pts',(-4.25659022200006,5.2,1.19798271199999));
#310819=CARTESIAN_POINT('Ctrl Pts',(-4.25659022200006,2.2,1.19798271199999));
#310820=CARTESIAN_POINT('Ctrl Pts',(-4.25864967800006,12.2,1.19762930099998));
#310821=CARTESIAN_POINT('Ctrl Pts',(-4.25864967800006,5.2,1.19762930099998));
#310822=CARTESIAN_POINT('Ctrl Pts',(-4.25864967800006,2.2,1.19762930099998));
#310823=CARTESIAN_POINT('Ctrl Pts',(-4.26071265400005,12.2,1.19727295099999));
#310824=CARTESIAN_POINT('Ctrl Pts',(-4.26071265400005,5.2,1.19727295099999));
#310825=CARTESIAN_POINT('Ctrl Pts',(-4.26071265400005,2.2,1.19727295099999));
#310826=CARTESIAN_POINT('Ctrl Pts',(-4.26277914100006,12.2,1.19691365499999));
#310827=CARTESIAN_POINT('Ctrl Pts',(-4.26277914100006,5.2,1.19691365499999));
#310828=CARTESIAN_POINT('Ctrl Pts',(-4.26277914100006,2.2,1.19691365499999));
#310829=CARTESIAN_POINT('Ctrl Pts',(-4.26484913100006,12.2,1.19655140799999));
#310830=CARTESIAN_POINT('Ctrl Pts',(-4.26484913100006,5.2,1.19655140799999));
#310831=CARTESIAN_POINT('Ctrl Pts',(-4.26484913100006,2.2,1.19655140799999));
#310832=CARTESIAN_POINT('Ctrl Pts',(-4.26692261600006,12.2,1.19618620299998));
#310833=CARTESIAN_POINT('Ctrl Pts',(-4.26692261600006,5.2,1.19618620299998));
#310834=CARTESIAN_POINT('Ctrl Pts',(-4.26692261600006,2.2,1.19618620299998));
#310835=CARTESIAN_POINT('Ctrl Pts',(-4.26899958700006,12.2,1.19581803199999));
#310836=CARTESIAN_POINT('Ctrl Pts',(-4.26899958700006,5.2,1.19581803199999));
#310837=CARTESIAN_POINT('Ctrl Pts',(-4.26899958700006,2.2,1.19581803199999));
#310838=CARTESIAN_POINT('Ctrl Pts',(-4.27108003600006,12.2,1.19544689199999));
#310839=CARTESIAN_POINT('Ctrl Pts',(-4.27108003600006,5.2,1.19544689199999));
#310840=CARTESIAN_POINT('Ctrl Pts',(-4.27108003600006,2.2,1.19544689199999));
#310841=CARTESIAN_POINT('Ctrl Pts',(-4.27316395600006,12.2,1.19507277499999));
#310842=CARTESIAN_POINT('Ctrl Pts',(-4.27316395600006,5.2,1.19507277499999));
#310843=CARTESIAN_POINT('Ctrl Pts',(-4.27316395600006,2.2,1.19507277499999));
#310844=CARTESIAN_POINT('Ctrl Pts',(-4.27525133600006,12.2,1.19469567399999));
#310845=CARTESIAN_POINT('Ctrl Pts',(-4.27525133600006,5.2,1.19469567399999));
#310846=CARTESIAN_POINT('Ctrl Pts',(-4.27525133600006,2.2,1.19469567399999));
#310847=CARTESIAN_POINT('Ctrl Pts',(-4.27734217100006,12.2,1.19431558299999));
#310848=CARTESIAN_POINT('Ctrl Pts',(-4.27734217100006,5.2,1.19431558299999));
#310849=CARTESIAN_POINT('Ctrl Pts',(-4.27734217100006,2.2,1.19431558299999));
#310850=CARTESIAN_POINT('Ctrl Pts',(-4.27943645000005,12.2,1.19393249499999));
#310851=CARTESIAN_POINT('Ctrl Pts',(-4.27943645000005,5.2,1.19393249499999));
#310852=CARTESIAN_POINT('Ctrl Pts',(-4.27943645000005,2.2,1.19393249499999));
#310853=CARTESIAN_POINT('Ctrl Pts',(-4.28153416700006,12.2,1.19354640599999));
#310854=CARTESIAN_POINT('Ctrl Pts',(-4.28153416700006,5.2,1.19354640599999));
#310855=CARTESIAN_POINT('Ctrl Pts',(-4.28153416700006,2.2,1.19354640599999));
#310856=CARTESIAN_POINT('Ctrl Pts',(-4.28363531300006,12.2,1.19315730799999));
#310857=CARTESIAN_POINT('Ctrl Pts',(-4.28363531300006,5.2,1.19315730799999));
#310858=CARTESIAN_POINT('Ctrl Pts',(-4.28363531300006,2.2,1.19315730799999));
#310859=CARTESIAN_POINT('Ctrl Pts',(-4.28573987800006,12.2,1.19276519499998));
#310860=CARTESIAN_POINT('Ctrl Pts',(-4.28573987800006,5.2,1.19276519499998));
#310861=CARTESIAN_POINT('Ctrl Pts',(-4.28573987800006,2.2,1.19276519499998));
#310862=CARTESIAN_POINT('Ctrl Pts',(-4.28784785600006,12.2,1.19237006199999));
#310863=CARTESIAN_POINT('Ctrl Pts',(-4.28784785600006,5.2,1.19237006199999));
#310864=CARTESIAN_POINT('Ctrl Pts',(-4.28784785600006,2.2,1.19237006199999));
#310865=CARTESIAN_POINT('Ctrl Pts',(-4.28995923900006,12.2,1.19197189999999));
#310866=CARTESIAN_POINT('Ctrl Pts',(-4.28995923900006,5.2,1.19197189999999));
#310867=CARTESIAN_POINT('Ctrl Pts',(-4.28995923900006,2.2,1.19197189999999));
#310868=CARTESIAN_POINT('Ctrl Pts',(-4.29207401600006,12.2,1.19157070599998));
#310869=CARTESIAN_POINT('Ctrl Pts',(-4.29207401600006,5.2,1.19157070599998));
#310870=CARTESIAN_POINT('Ctrl Pts',(-4.29207401600006,2.2,1.19157070599998));
#310871=CARTESIAN_POINT('Ctrl Pts',(-4.29419218200006,12.2,1.19116647099998));
#310872=CARTESIAN_POINT('Ctrl Pts',(-4.29419218200006,5.2,1.19116647099998));
#310873=CARTESIAN_POINT('Ctrl Pts',(-4.29419218200006,2.2,1.19116647099998));
#310874=CARTESIAN_POINT('Ctrl Pts',(-4.29631372700006,12.2,1.19075919199998));
#310875=CARTESIAN_POINT('Ctrl Pts',(-4.29631372700006,5.2,1.19075919199998));
#310876=CARTESIAN_POINT('Ctrl Pts',(-4.29631372700006,2.2,1.19075919199998));
#310877=CARTESIAN_POINT('Ctrl Pts',(-4.29843864300006,12.2,1.19034885999998));
#310878=CARTESIAN_POINT('Ctrl Pts',(-4.29843864300006,5.2,1.19034885999998));
#310879=CARTESIAN_POINT('Ctrl Pts',(-4.29843864300006,2.2,1.19034885999998));
#310880=CARTESIAN_POINT('Ctrl Pts',(-4.30056692200006,12.2,1.18993547099999));
#310881=CARTESIAN_POINT('Ctrl Pts',(-4.30056692200006,5.2,1.18993547099999));
#310882=CARTESIAN_POINT('Ctrl Pts',(-4.30056692200006,2.2,1.18993547099999));
#310883=CARTESIAN_POINT('Ctrl Pts',(-4.30269855500006,12.2,1.18951901699999));
#310884=CARTESIAN_POINT('Ctrl Pts',(-4.30269855500006,5.2,1.18951901699999));
#310885=CARTESIAN_POINT('Ctrl Pts',(-4.30269855500006,2.2,1.18951901699999));
#310886=CARTESIAN_POINT('Ctrl Pts',(-4.30483353600006,12.2,1.18909949499999));
#310887=CARTESIAN_POINT('Ctrl Pts',(-4.30483353600006,5.2,1.18909949499999));
#310888=CARTESIAN_POINT('Ctrl Pts',(-4.30483353600006,2.2,1.18909949499999));
#310889=CARTESIAN_POINT('Ctrl Pts',(-4.30697185500006,12.2,1.18867689499998));
#310890=CARTESIAN_POINT('Ctrl Pts',(-4.30697185500006,5.2,1.18867689499998));
#310891=CARTESIAN_POINT('Ctrl Pts',(-4.30697185500006,2.2,1.18867689499998));
#310892=CARTESIAN_POINT('Ctrl Pts',(-4.30911350400006,12.2,1.18825121399999));
#310893=CARTESIAN_POINT('Ctrl Pts',(-4.30911350400006,5.2,1.18825121399999));
#310894=CARTESIAN_POINT('Ctrl Pts',(-4.30911350400006,2.2,1.18825121399999));
#310895=CARTESIAN_POINT('Ctrl Pts',(-4.31125847500006,12.2,1.18782244499998));
#310896=CARTESIAN_POINT('Ctrl Pts',(-4.31125847500006,5.2,1.18782244499998));
#310897=CARTESIAN_POINT('Ctrl Pts',(-4.31125847500006,2.2,1.18782244499998));
#310898=CARTESIAN_POINT('Ctrl Pts',(-4.31340675900006,12.2,1.18739058199999));
#310899=CARTESIAN_POINT('Ctrl Pts',(-4.31340675900006,5.2,1.18739058199999));
#310900=CARTESIAN_POINT('Ctrl Pts',(-4.31340675900006,2.2,1.18739058199999));
#310901=CARTESIAN_POINT('Ctrl Pts',(-4.31555834900006,12.2,1.18695561799999));
#310902=CARTESIAN_POINT('Ctrl Pts',(-4.31555834900006,5.2,1.18695561799999));
#310903=CARTESIAN_POINT('Ctrl Pts',(-4.31555834900006,2.2,1.18695561799999));
#310904=CARTESIAN_POINT('Ctrl Pts',(-4.31771323800006,12.2,1.18651754899998));
#310905=CARTESIAN_POINT('Ctrl Pts',(-4.31771323800006,5.2,1.18651754899998));
#310906=CARTESIAN_POINT('Ctrl Pts',(-4.31771323800006,2.2,1.18651754899998));
#310907=CARTESIAN_POINT('Ctrl Pts',(-4.31987141500006,12.2,1.18607636799998));
#310908=CARTESIAN_POINT('Ctrl Pts',(-4.31987141500006,5.2,1.18607636799998));
#310909=CARTESIAN_POINT('Ctrl Pts',(-4.31987141500006,2.2,1.18607636799998));
#310910=CARTESIAN_POINT('Ctrl Pts',(-4.32203287300006,12.2,1.18563207099998));
#310911=CARTESIAN_POINT('Ctrl Pts',(-4.32203287300006,5.2,1.18563207099998));
#310912=CARTESIAN_POINT('Ctrl Pts',(-4.32203287300006,2.2,1.18563207099998));
#310913=CARTESIAN_POINT('Ctrl Pts',(-4.32419760400006,12.2,1.18518464899998));
#310914=CARTESIAN_POINT('Ctrl Pts',(-4.32419760400006,5.2,1.18518464899998));
#310915=CARTESIAN_POINT('Ctrl Pts',(-4.32419760400006,2.2,1.18518464899998));
#310916=CARTESIAN_POINT('Ctrl Pts',(-4.32636560100006,12.2,1.18473409699998));
#310917=CARTESIAN_POINT('Ctrl Pts',(-4.32636560100006,5.2,1.18473409699998));
#310918=CARTESIAN_POINT('Ctrl Pts',(-4.32636560100006,2.2,1.18473409699998));
#310919=CARTESIAN_POINT('Ctrl Pts',(-4.32853685400006,12.2,1.18428041099999));
#310920=CARTESIAN_POINT('Ctrl Pts',(-4.32853685400006,5.2,1.18428041099999));
#310921=CARTESIAN_POINT('Ctrl Pts',(-4.32853685400006,2.2,1.18428041099999));
#310922=CARTESIAN_POINT('Ctrl Pts',(-4.33071135500006,12.2,1.18382358399999));
#310923=CARTESIAN_POINT('Ctrl Pts',(-4.33071135500006,5.2,1.18382358399999));
#310924=CARTESIAN_POINT('Ctrl Pts',(-4.33071135500006,2.2,1.18382358399999));
#310925=CARTESIAN_POINT('Ctrl Pts',(-4.33288909700006,12.2,1.18336361099999));
#310926=CARTESIAN_POINT('Ctrl Pts',(-4.33288909700006,5.2,1.18336361099999));
#310927=CARTESIAN_POINT('Ctrl Pts',(-4.33288909700006,2.2,1.18336361099999));
#310928=CARTESIAN_POINT('Ctrl Pts',(-4.33507007000006,12.2,1.18290048399999));
#310929=CARTESIAN_POINT('Ctrl Pts',(-4.33507007000006,5.2,1.18290048399999));
#310930=CARTESIAN_POINT('Ctrl Pts',(-4.33507007000006,2.2,1.18290048399999));
#310931=CARTESIAN_POINT('Ctrl Pts',(-4.33725426800006,12.2,1.18243419999999));
#310932=CARTESIAN_POINT('Ctrl Pts',(-4.33725426800006,5.2,1.18243419999999));
#310933=CARTESIAN_POINT('Ctrl Pts',(-4.33725426800006,2.2,1.18243419999999));
#310934=CARTESIAN_POINT('Ctrl Pts',(-4.33944168200005,12.2,1.18196475099999));
#310935=CARTESIAN_POINT('Ctrl Pts',(-4.33944168200005,5.2,1.18196475099999));
#310936=CARTESIAN_POINT('Ctrl Pts',(-4.33944168200005,2.2,1.18196475099999));
#310937=CARTESIAN_POINT('Ctrl Pts',(-4.34163230300006,12.2,1.18149213299999));
#310938=CARTESIAN_POINT('Ctrl Pts',(-4.34163230300006,5.2,1.18149213299999));
#310939=CARTESIAN_POINT('Ctrl Pts',(-4.34163230300006,2.2,1.18149213299999));
#310940=CARTESIAN_POINT('Ctrl Pts',(-4.34382612500006,12.2,1.18101633899999));
#310941=CARTESIAN_POINT('Ctrl Pts',(-4.34382612500006,5.2,1.18101633899999));
#310942=CARTESIAN_POINT('Ctrl Pts',(-4.34382612500006,2.2,1.18101633899999));
#310943=CARTESIAN_POINT('Ctrl Pts',(-4.34602313800006,12.2,1.18053736299998));
#310944=CARTESIAN_POINT('Ctrl Pts',(-4.34602313800006,5.2,1.18053736299998));
#310945=CARTESIAN_POINT('Ctrl Pts',(-4.34602313800006,2.2,1.18053736299998));
#310946=CARTESIAN_POINT('Ctrl Pts',(-4.34822333400006,12.2,1.18005520199999));
#310947=CARTESIAN_POINT('Ctrl Pts',(-4.34822333400006,5.2,1.18005520199999));
#310948=CARTESIAN_POINT('Ctrl Pts',(-4.34822333400006,2.2,1.18005520199999));
#310949=CARTESIAN_POINT('Ctrl Pts',(-4.35042670500006,12.2,1.17956984899998));
#310950=CARTESIAN_POINT('Ctrl Pts',(-4.35042670500006,5.2,1.17956984899998));
#310951=CARTESIAN_POINT('Ctrl Pts',(-4.35042670500006,2.2,1.17956984899998));
#310952=CARTESIAN_POINT('Ctrl Pts',(-4.35263324400006,12.2,1.17908129599999));
#310953=CARTESIAN_POINT('Ctrl Pts',(-4.35263324400006,5.2,1.17908129599999));
#310954=CARTESIAN_POINT('Ctrl Pts',(-4.35263324400006,2.2,1.17908129599999));
#310955=CARTESIAN_POINT('Ctrl Pts',(-4.35484294200006,12.2,1.17858954199999));
#310956=CARTESIAN_POINT('Ctrl Pts',(-4.35484294200006,5.2,1.17858954199999));
#310957=CARTESIAN_POINT('Ctrl Pts',(-4.35484294200006,2.2,1.17858954199999));
#310958=CARTESIAN_POINT('Ctrl Pts',(-4.35705579000006,12.2,1.17809457699999));
#310959=CARTESIAN_POINT('Ctrl Pts',(-4.35705579000006,5.2,1.17809457699999));
#310960=CARTESIAN_POINT('Ctrl Pts',(-4.35705579000006,2.2,1.17809457699999));
#310961=CARTESIAN_POINT('Ctrl Pts',(-4.35927178200005,12.2,1.17759639799999));
#310962=CARTESIAN_POINT('Ctrl Pts',(-4.35927178200005,5.2,1.17759639799999));
#310963=CARTESIAN_POINT('Ctrl Pts',(-4.35927178200005,2.2,1.17759639799999));
#310964=CARTESIAN_POINT('Ctrl Pts',(-4.36149090800006,12.2,1.17709499799998));
#310965=CARTESIAN_POINT('Ctrl Pts',(-4.36149090800006,5.2,1.17709499799998));
#310966=CARTESIAN_POINT('Ctrl Pts',(-4.36149090800006,2.2,1.17709499799998));
#310967=CARTESIAN_POINT('Ctrl Pts',(-4.36371316200006,12.2,1.17659037299998));
#310968=CARTESIAN_POINT('Ctrl Pts',(-4.36371316200006,5.2,1.17659037299998));
#310969=CARTESIAN_POINT('Ctrl Pts',(-4.36371316200006,2.2,1.17659037299998));
#310970=CARTESIAN_POINT('Ctrl Pts',(-4.36593853300006,12.2,1.17608251699998));
#310971=CARTESIAN_POINT('Ctrl Pts',(-4.36593853300006,5.2,1.17608251699998));
#310972=CARTESIAN_POINT('Ctrl Pts',(-4.36593853300006,2.2,1.17608251699998));
#310973=CARTESIAN_POINT('Ctrl Pts',(-4.36816701500006,12.2,1.17557142399999));
#310974=CARTESIAN_POINT('Ctrl Pts',(-4.36816701500006,5.2,1.17557142399999));
#310975=CARTESIAN_POINT('Ctrl Pts',(-4.36816701500006,2.2,1.17557142399999));
#310976=CARTESIAN_POINT('Ctrl Pts',(-4.37039860000006,12.2,1.17505708799999));
#310977=CARTESIAN_POINT('Ctrl Pts',(-4.37039860000006,5.2,1.17505708799999));
#310978=CARTESIAN_POINT('Ctrl Pts',(-4.37039860000006,2.2,1.17505708799999));
#310979=CARTESIAN_POINT('Ctrl Pts',(-4.37263327900006,12.2,1.17453950599999));
#310980=CARTESIAN_POINT('Ctrl Pts',(-4.37263327900006,5.2,1.17453950599999));
#310981=CARTESIAN_POINT('Ctrl Pts',(-4.37263327900006,2.2,1.17453950599999));
#310982=CARTESIAN_POINT('Ctrl Pts',(-4.37487104400006,12.2,1.17401866899999));
#310983=CARTESIAN_POINT('Ctrl Pts',(-4.37487104400006,5.2,1.17401866899999));
#310984=CARTESIAN_POINT('Ctrl Pts',(-4.37487104400006,2.2,1.17401866899999));
#310985=CARTESIAN_POINT('Ctrl Pts',(-4.37711188600006,12.2,1.17349457499999));
#310986=CARTESIAN_POINT('Ctrl Pts',(-4.37711188600006,5.2,1.17349457499999));
#310987=CARTESIAN_POINT('Ctrl Pts',(-4.37711188600006,2.2,1.17349457499999));
#310988=CARTESIAN_POINT('Ctrl Pts',(-4.37935580000006,12.2,1.17296721699998));
#310989=CARTESIAN_POINT('Ctrl Pts',(-4.37935580000006,5.2,1.17296721699998));
#310990=CARTESIAN_POINT('Ctrl Pts',(-4.37935580000006,2.2,1.17296721699998));
#310991=CARTESIAN_POINT('Ctrl Pts',(-4.38160277500006,12.2,1.17243658999998));
#310992=CARTESIAN_POINT('Ctrl Pts',(-4.38160277500006,5.2,1.17243658999998));
#310993=CARTESIAN_POINT('Ctrl Pts',(-4.38160277500006,2.2,1.17243658999998));
#310994=CARTESIAN_POINT('Ctrl Pts',(-4.38385280500006,12.2,1.17190268799999));
#310995=CARTESIAN_POINT('Ctrl Pts',(-4.38385280500006,5.2,1.17190268799999));
#310996=CARTESIAN_POINT('Ctrl Pts',(-4.38385280500006,2.2,1.17190268799999));
#310997=CARTESIAN_POINT('Ctrl Pts',(-4.38610588000006,12.2,1.17136550599998));
#310998=CARTESIAN_POINT('Ctrl Pts',(-4.38610588000006,5.2,1.17136550599998));
#310999=CARTESIAN_POINT('Ctrl Pts',(-4.38610588000006,2.2,1.17136550599998));
#311000=CARTESIAN_POINT('Ctrl Pts',(-4.38836199200006,12.2,1.17082503799999));
#311001=CARTESIAN_POINT('Ctrl Pts',(-4.38836199200006,5.2,1.17082503799999));
#311002=CARTESIAN_POINT('Ctrl Pts',(-4.38836199200006,2.2,1.17082503799999));
#311003=CARTESIAN_POINT('Ctrl Pts',(-4.39062113500006,12.2,1.17028128099999));
#311004=CARTESIAN_POINT('Ctrl Pts',(-4.39062113500006,5.2,1.17028128099999));
#311005=CARTESIAN_POINT('Ctrl Pts',(-4.39062113500006,2.2,1.17028128099999));
#311006=CARTESIAN_POINT('Ctrl Pts',(-4.39288330000006,12.2,1.16973422599999));
#311007=CARTESIAN_POINT('Ctrl Pts',(-4.39288330000006,5.2,1.16973422599999));
#311008=CARTESIAN_POINT('Ctrl Pts',(-4.39288330000006,2.2,1.16973422599999));
#311009=CARTESIAN_POINT('Ctrl Pts',(-4.39514847900006,12.2,1.16918387199998));
#311010=CARTESIAN_POINT('Ctrl Pts',(-4.39514847900006,5.2,1.16918387199998));
#311011=CARTESIAN_POINT('Ctrl Pts',(-4.39514847900006,2.2,1.16918387199998));
#311012=CARTESIAN_POINT('Ctrl Pts',(-4.39741666100006,12.2,1.16863021099999));
#311013=CARTESIAN_POINT('Ctrl Pts',(-4.39741666100006,5.2,1.16863021099999));
#311014=CARTESIAN_POINT('Ctrl Pts',(-4.39741666100006,2.2,1.16863021099999));
#311015=CARTESIAN_POINT('Ctrl Pts',(-4.39968784400006,12.2,1.16807323799998));
#311016=CARTESIAN_POINT('Ctrl Pts',(-4.39968784400006,5.2,1.16807323799998));
#311017=CARTESIAN_POINT('Ctrl Pts',(-4.39968784400006,2.2,1.16807323799998));
#311018=CARTESIAN_POINT('Ctrl Pts',(-4.40196201500005,12.2,1.16751294799998));
#311019=CARTESIAN_POINT('Ctrl Pts',(-4.40196201500005,5.2,1.16751294799998));
#311020=CARTESIAN_POINT('Ctrl Pts',(-4.40196201500005,2.2,1.16751294799998));
#311021=CARTESIAN_POINT('Ctrl Pts',(-4.40423916700006,12.2,1.16694933699999));
#311022=CARTESIAN_POINT('Ctrl Pts',(-4.40423916700006,5.2,1.16694933699999));
#311023=CARTESIAN_POINT('Ctrl Pts',(-4.40423916700006,2.2,1.16694933699999));
#311024=CARTESIAN_POINT('Ctrl Pts',(-4.40651929300006,12.2,1.16638239899999));
#311025=CARTESIAN_POINT('Ctrl Pts',(-4.40651929300006,5.2,1.16638239899999));
#311026=CARTESIAN_POINT('Ctrl Pts',(-4.40651929300006,2.2,1.16638239899999));
#311027=CARTESIAN_POINT('Ctrl Pts',(-4.40880238500006,12.2,1.16581212899999));
#311028=CARTESIAN_POINT('Ctrl Pts',(-4.40880238500006,5.2,1.16581212899999));
#311029=CARTESIAN_POINT('Ctrl Pts',(-4.40880238500006,2.2,1.16581212899999));
#311030=CARTESIAN_POINT('Ctrl Pts',(-4.41108843400006,12.2,1.16523851999998));
#311031=CARTESIAN_POINT('Ctrl Pts',(-4.41108843400006,5.2,1.16523851999998));
#311032=CARTESIAN_POINT('Ctrl Pts',(-4.41108843400006,2.2,1.16523851999998));
#311033=CARTESIAN_POINT('Ctrl Pts',(-4.41337743300006,12.2,1.16466156999998));
#311034=CARTESIAN_POINT('Ctrl Pts',(-4.41337743300006,5.2,1.16466156999998));
#311035=CARTESIAN_POINT('Ctrl Pts',(-4.41337743300006,2.2,1.16466156999998));
#311036=CARTESIAN_POINT('Ctrl Pts',(-4.41566937300006,12.2,1.16408127199998));
#311037=CARTESIAN_POINT('Ctrl Pts',(-4.41566937300006,5.2,1.16408127199998));
#311038=CARTESIAN_POINT('Ctrl Pts',(-4.41566937300006,2.2,1.16408127199998));
#311039=CARTESIAN_POINT('Ctrl Pts',(-4.41796424600006,12.2,1.16349762099999));
#311040=CARTESIAN_POINT('Ctrl Pts',(-4.41796424600006,5.2,1.16349762099999));
#311041=CARTESIAN_POINT('Ctrl Pts',(-4.41796424600006,2.2,1.16349762099999));
#311042=CARTESIAN_POINT('Ctrl Pts',(-4.42026204600006,12.2,1.16291061199998));
#311043=CARTESIAN_POINT('Ctrl Pts',(-4.42026204600006,5.2,1.16291061199998));
#311044=CARTESIAN_POINT('Ctrl Pts',(-4.42026204600006,2.2,1.16291061199998));
#311045=CARTESIAN_POINT('Ctrl Pts',(-4.42256276200006,12.2,1.16232024099999));
#311046=CARTESIAN_POINT('Ctrl Pts',(-4.42256276200006,5.2,1.16232024099999));
#311047=CARTESIAN_POINT('Ctrl Pts',(-4.42256276200006,2.2,1.16232024099999));
#311048=CARTESIAN_POINT('Ctrl Pts',(-4.42486638800006,12.2,1.16172650199998));
#311049=CARTESIAN_POINT('Ctrl Pts',(-4.42486638800006,5.2,1.16172650199998));
#311050=CARTESIAN_POINT('Ctrl Pts',(-4.42486638800006,2.2,1.16172650199998));
#311051=CARTESIAN_POINT('Ctrl Pts',(-4.42717291500006,12.2,1.16112938999999));
#311052=CARTESIAN_POINT('Ctrl Pts',(-4.42717291500006,5.2,1.16112938999999));
#311053=CARTESIAN_POINT('Ctrl Pts',(-4.42717291500006,2.2,1.16112938999999));
#311054=CARTESIAN_POINT('Ctrl Pts',(-4.42948233700006,12.2,1.16052889999999));
#311055=CARTESIAN_POINT('Ctrl Pts',(-4.42948233700006,5.2,1.16052889999999));
#311056=CARTESIAN_POINT('Ctrl Pts',(-4.42948233700006,2.2,1.16052889999999));
#311057=CARTESIAN_POINT('Ctrl Pts',(-4.43179464300006,12.2,1.15992502699998));
#311058=CARTESIAN_POINT('Ctrl Pts',(-4.43179464300006,5.2,1.15992502699998));
#311059=CARTESIAN_POINT('Ctrl Pts',(-4.43179464300006,2.2,1.15992502699998));
#311060=CARTESIAN_POINT('Ctrl Pts',(-4.43410982700006,12.2,1.15931776699998));
#311061=CARTESIAN_POINT('Ctrl Pts',(-4.43410982700006,5.2,1.15931776699998));
#311062=CARTESIAN_POINT('Ctrl Pts',(-4.43410982700006,2.2,1.15931776699998));
#311063=CARTESIAN_POINT('Ctrl Pts',(-4.43642788100005,12.2,1.15870711299999));
#311064=CARTESIAN_POINT('Ctrl Pts',(-4.43642788100005,5.2,1.15870711299999));
#311065=CARTESIAN_POINT('Ctrl Pts',(-4.43642788100005,2.2,1.15870711299999));
#311066=CARTESIAN_POINT('Ctrl Pts',(-4.43874879500005,12.2,1.15809306299999));
#311067=CARTESIAN_POINT('Ctrl Pts',(-4.43874879500005,5.2,1.15809306299999));
#311068=CARTESIAN_POINT('Ctrl Pts',(-4.43874879500005,2.2,1.15809306299999));
#311069=CARTESIAN_POINT('Ctrl Pts',(-4.44107256400006,12.2,1.15747560899999));
#311070=CARTESIAN_POINT('Ctrl Pts',(-4.44107256400006,5.2,1.15747560899999));
#311071=CARTESIAN_POINT('Ctrl Pts',(-4.44107256400006,2.2,1.15747560899999));
#311072=CARTESIAN_POINT('Ctrl Pts',(-4.44339917800006,12.2,1.15685474899998));
#311073=CARTESIAN_POINT('Ctrl Pts',(-4.44339917800006,5.2,1.15685474899998));
#311074=CARTESIAN_POINT('Ctrl Pts',(-4.44339917800006,2.2,1.15685474899998));
#311075=CARTESIAN_POINT('Ctrl Pts',(-4.44572863100006,12.2,1.15623047599998));
#311076=CARTESIAN_POINT('Ctrl Pts',(-4.44572863100006,5.2,1.15623047599998));
#311077=CARTESIAN_POINT('Ctrl Pts',(-4.44572863100006,2.2,1.15623047599998));
#311078=CARTESIAN_POINT('Ctrl Pts',(-4.44806091200006,12.2,1.15560278499999));
#311079=CARTESIAN_POINT('Ctrl Pts',(-4.44806091200006,5.2,1.15560278499999));
#311080=CARTESIAN_POINT('Ctrl Pts',(-4.44806091200006,2.2,1.15560278499999));
#311081=CARTESIAN_POINT('Ctrl Pts',(-4.45039601500006,12.2,1.15497167299999));
#311082=CARTESIAN_POINT('Ctrl Pts',(-4.45039601500006,5.2,1.15497167299999));
#311083=CARTESIAN_POINT('Ctrl Pts',(-4.45039601500006,2.2,1.15497167299999));
#311084=CARTESIAN_POINT('Ctrl Pts',(-4.45273393300006,12.2,1.15433713399999));
#311085=CARTESIAN_POINT('Ctrl Pts',(-4.45273393300006,5.2,1.15433713399999));
#311086=CARTESIAN_POINT('Ctrl Pts',(-4.45273393300006,2.2,1.15433713399999));
#311087=CARTESIAN_POINT('Ctrl Pts',(-4.45507465600006,12.2,1.15369916299999));
#311088=CARTESIAN_POINT('Ctrl Pts',(-4.45507465600006,5.2,1.15369916299999));
#311089=CARTESIAN_POINT('Ctrl Pts',(-4.45507465600006,2.2,1.15369916299999));
#311090=CARTESIAN_POINT('Ctrl Pts',(-4.45741817600006,12.2,1.15305775599999));
#311091=CARTESIAN_POINT('Ctrl Pts',(-4.45741817600006,5.2,1.15305775599999));
#311092=CARTESIAN_POINT('Ctrl Pts',(-4.45741817600006,2.2,1.15305775599999));
#311093=CARTESIAN_POINT('Ctrl Pts',(-4.45976448700006,12.2,1.15241290799998));
#311094=CARTESIAN_POINT('Ctrl Pts',(-4.45976448700006,5.2,1.15241290799998));
#311095=CARTESIAN_POINT('Ctrl Pts',(-4.45976448700006,2.2,1.15241290799998));
#311096=CARTESIAN_POINT('Ctrl Pts',(-4.46211358000006,12.2,1.15176461399999));
#311097=CARTESIAN_POINT('Ctrl Pts',(-4.46211358000006,5.2,1.15176461399999));
#311098=CARTESIAN_POINT('Ctrl Pts',(-4.46211358000006,2.2,1.15176461399999));
#311099=CARTESIAN_POINT('Ctrl Pts',(-4.46446544700006,12.2,1.15111286899999));
#311100=CARTESIAN_POINT('Ctrl Pts',(-4.46446544700006,5.2,1.15111286899999));
#311101=CARTESIAN_POINT('Ctrl Pts',(-4.46446544700006,2.2,1.15111286899999));
#311102=CARTESIAN_POINT('Ctrl Pts',(-4.46682008000006,12.2,1.15045766899998));
#311103=CARTESIAN_POINT('Ctrl Pts',(-4.46682008000006,5.2,1.15045766899998));
#311104=CARTESIAN_POINT('Ctrl Pts',(-4.46682008000006,2.2,1.15045766899998));
#311105=CARTESIAN_POINT('Ctrl Pts',(-4.46917747200006,12.2,1.14979900899999));
#311106=CARTESIAN_POINT('Ctrl Pts',(-4.46917747200006,5.2,1.14979900899999));
#311107=CARTESIAN_POINT('Ctrl Pts',(-4.46917747200006,2.2,1.14979900899999));
#311108=CARTESIAN_POINT('Ctrl Pts',(-4.47153761400005,12.2,1.14913688399998));
#311109=CARTESIAN_POINT('Ctrl Pts',(-4.47153761400005,5.2,1.14913688399998));
#311110=CARTESIAN_POINT('Ctrl Pts',(-4.47153761400005,2.2,1.14913688399998));
#311111=CARTESIAN_POINT('Ctrl Pts',(-4.47390049800005,12.2,1.14847128899998));
#311112=CARTESIAN_POINT('Ctrl Pts',(-4.47390049800005,5.2,1.14847128899998));
#311113=CARTESIAN_POINT('Ctrl Pts',(-4.47390049800005,2.2,1.14847128899998));
#311114=CARTESIAN_POINT('Ctrl Pts',(-4.47626611700006,12.2,1.14780221999998));
#311115=CARTESIAN_POINT('Ctrl Pts',(-4.47626611700006,5.2,1.14780221999998));
#311116=CARTESIAN_POINT('Ctrl Pts',(-4.47626611700006,2.2,1.14780221999998));
#311117=CARTESIAN_POINT('Ctrl Pts',(-4.47863446200006,12.2,1.14712967299999));
#311118=CARTESIAN_POINT('Ctrl Pts',(-4.47863446200006,5.2,1.14712967299999));
#311119=CARTESIAN_POINT('Ctrl Pts',(-4.47863446200006,2.2,1.14712967299999));
#311120=CARTESIAN_POINT('Ctrl Pts',(-4.48100552600006,12.2,1.14645364299998));
#311121=CARTESIAN_POINT('Ctrl Pts',(-4.48100552600006,5.2,1.14645364299998));
#311122=CARTESIAN_POINT('Ctrl Pts',(-4.48100552600006,2.2,1.14645364299998));
#311123=CARTESIAN_POINT('Ctrl Pts',(-4.48337930100006,12.2,1.14577412399999));
#311124=CARTESIAN_POINT('Ctrl Pts',(-4.48337930100006,5.2,1.14577412399999));
#311125=CARTESIAN_POINT('Ctrl Pts',(-4.48337930100006,2.2,1.14577412399999));
#311126=CARTESIAN_POINT('Ctrl Pts',(-4.48575577900006,12.2,1.14509111299999));
#311127=CARTESIAN_POINT('Ctrl Pts',(-4.48575577900006,5.2,1.14509111299999));
#311128=CARTESIAN_POINT('Ctrl Pts',(-4.48575577900006,2.2,1.14509111299999));
#311129=CARTESIAN_POINT('Ctrl Pts',(-4.48813495100006,12.2,1.14440460599999));
#311130=CARTESIAN_POINT('Ctrl Pts',(-4.48813495100006,5.2,1.14440460599999));
#311131=CARTESIAN_POINT('Ctrl Pts',(-4.48813495100006,2.2,1.14440460599999));
#311132=CARTESIAN_POINT('Ctrl Pts',(-4.49051681000006,12.2,1.14371459599999));
#311133=CARTESIAN_POINT('Ctrl Pts',(-4.49051681000006,5.2,1.14371459599999));
#311134=CARTESIAN_POINT('Ctrl Pts',(-4.49051681000006,2.2,1.14371459599999));
#311135=CARTESIAN_POINT('Ctrl Pts',(-4.49290134900005,12.2,1.14302107999999));
#311136=CARTESIAN_POINT('Ctrl Pts',(-4.49290134900005,5.2,1.14302107999999));
#311137=CARTESIAN_POINT('Ctrl Pts',(-4.49290134900005,2.2,1.14302107999999));
#311138=CARTESIAN_POINT('Ctrl Pts',(-4.49528855900006,12.2,1.14232405299999));
#311139=CARTESIAN_POINT('Ctrl Pts',(-4.49528855900006,5.2,1.14232405299999));
#311140=CARTESIAN_POINT('Ctrl Pts',(-4.49528855900006,2.2,1.14232405299999));
#311141=CARTESIAN_POINT('Ctrl Pts',(-4.49767843300005,12.2,1.14162351099999));
#311142=CARTESIAN_POINT('Ctrl Pts',(-4.49767843300005,5.2,1.14162351099999));
#311143=CARTESIAN_POINT('Ctrl Pts',(-4.49767843300005,2.2,1.14162351099999));
#311144=CARTESIAN_POINT('Ctrl Pts',(-4.50007096200006,12.2,1.14091944999998));
#311145=CARTESIAN_POINT('Ctrl Pts',(-4.50007096200006,5.2,1.14091944999998));
#311146=CARTESIAN_POINT('Ctrl Pts',(-4.50007096200006,2.2,1.14091944999998));
#311147=CARTESIAN_POINT('Ctrl Pts',(-4.50246613900006,12.2,1.14021186399999));
#311148=CARTESIAN_POINT('Ctrl Pts',(-4.50246613900006,5.2,1.14021186399999));
#311149=CARTESIAN_POINT('Ctrl Pts',(-4.50246613900006,2.2,1.14021186399999));
#311150=CARTESIAN_POINT('Ctrl Pts',(-4.50486395600006,12.2,1.13950074999998));
#311151=CARTESIAN_POINT('Ctrl Pts',(-4.50486395600006,5.2,1.13950074999998));
#311152=CARTESIAN_POINT('Ctrl Pts',(-4.50486395600006,2.2,1.13950074999998));
#311153=CARTESIAN_POINT('Ctrl Pts',(-4.50726440400006,12.2,1.13878610299999));
#311154=CARTESIAN_POINT('Ctrl Pts',(-4.50726440400006,5.2,1.13878610299999));
#311155=CARTESIAN_POINT('Ctrl Pts',(-4.50726440400006,2.2,1.13878610299999));
#311156=CARTESIAN_POINT('Ctrl Pts',(-4.50966747700006,12.2,1.13806791899998));
#311157=CARTESIAN_POINT('Ctrl Pts',(-4.50966747700006,5.2,1.13806791899998));
#311158=CARTESIAN_POINT('Ctrl Pts',(-4.50966747700006,2.2,1.13806791899998));
#311159=CARTESIAN_POINT('Ctrl Pts',(-4.51207316600006,12.2,1.13734619299999));
#311160=CARTESIAN_POINT('Ctrl Pts',(-4.51207316600006,5.2,1.13734619299999));
#311161=CARTESIAN_POINT('Ctrl Pts',(-4.51207316600006,2.2,1.13734619299999));
#311162=CARTESIAN_POINT('Ctrl Pts',(-4.51448146400006,12.2,1.13662091999998));
#311163=CARTESIAN_POINT('Ctrl Pts',(-4.51448146400006,5.2,1.13662091999998));
#311164=CARTESIAN_POINT('Ctrl Pts',(-4.51448146400006,2.2,1.13662091999998));
#311165=CARTESIAN_POINT('Ctrl Pts',(-4.51689236100006,12.2,1.13589209599999));
#311166=CARTESIAN_POINT('Ctrl Pts',(-4.51689236100006,5.2,1.13589209599999));
#311167=CARTESIAN_POINT('Ctrl Pts',(-4.51689236100006,2.2,1.13589209599999));
#311168=CARTESIAN_POINT('Ctrl Pts',(-4.51930585100006,12.2,1.13515971799998));
#311169=CARTESIAN_POINT('Ctrl Pts',(-4.51930585100006,5.2,1.13515971799998));
#311170=CARTESIAN_POINT('Ctrl Pts',(-4.51930585100006,2.2,1.13515971799998));
#311171=CARTESIAN_POINT('Ctrl Pts',(-4.52172192700006,12.2,1.13442378099998));
#311172=CARTESIAN_POINT('Ctrl Pts',(-4.52172192700006,5.2,1.13442378099998));
#311173=CARTESIAN_POINT('Ctrl Pts',(-4.52172192700006,2.2,1.13442378099998));
#311174=CARTESIAN_POINT('Ctrl Pts',(-4.52414057900006,12.2,1.13368427999998));
#311175=CARTESIAN_POINT('Ctrl Pts',(-4.52414057900006,5.2,1.13368427999998));
#311176=CARTESIAN_POINT('Ctrl Pts',(-4.52414057900006,2.2,1.13368427999998));
#311177=CARTESIAN_POINT('Ctrl Pts',(-4.52656180000006,12.2,1.13294121099999));
#311178=CARTESIAN_POINT('Ctrl Pts',(-4.52656180000006,5.2,1.13294121099999));
#311179=CARTESIAN_POINT('Ctrl Pts',(-4.52656180000006,2.2,1.13294121099999));
#311180=CARTESIAN_POINT('Ctrl Pts',(-4.52898558300006,12.2,1.13219456899999));
#311181=CARTESIAN_POINT('Ctrl Pts',(-4.52898558300006,5.2,1.13219456899999));
#311182=CARTESIAN_POINT('Ctrl Pts',(-4.52898558300006,2.2,1.13219456899999));
#311183=CARTESIAN_POINT('Ctrl Pts',(-4.53141191900006,12.2,1.13144435199999));
#311184=CARTESIAN_POINT('Ctrl Pts',(-4.53141191900006,5.2,1.13144435199999));
#311185=CARTESIAN_POINT('Ctrl Pts',(-4.53141191900006,2.2,1.13144435199999));
#311186=CARTESIAN_POINT('Ctrl Pts',(-4.53384080100006,12.2,1.13069055299999));
#311187=CARTESIAN_POINT('Ctrl Pts',(-4.53384080100006,5.2,1.13069055299999));
#311188=CARTESIAN_POINT('Ctrl Pts',(-4.53384080100006,2.2,1.13069055299999));
#311189=CARTESIAN_POINT('Ctrl Pts',(-4.53627222100006,12.2,1.12993316999999));
#311190=CARTESIAN_POINT('Ctrl Pts',(-4.53627222100006,5.2,1.12993316999999));
#311191=CARTESIAN_POINT('Ctrl Pts',(-4.53627222100006,2.2,1.12993316999999));
#311192=CARTESIAN_POINT('Ctrl Pts',(-4.53870617100006,12.2,1.12917219699999));
#311193=CARTESIAN_POINT('Ctrl Pts',(-4.53870617100006,5.2,1.12917219699999));
#311194=CARTESIAN_POINT('Ctrl Pts',(-4.53870617100006,2.2,1.12917219699999));
#311195=CARTESIAN_POINT('Ctrl Pts',(-4.54114264300006,12.2,1.12840763099999));
#311196=CARTESIAN_POINT('Ctrl Pts',(-4.54114264300006,5.2,1.12840763099999));
#311197=CARTESIAN_POINT('Ctrl Pts',(-4.54114264300006,2.2,1.12840763099999));
#311198=CARTESIAN_POINT('Ctrl Pts',(-4.54358163000006,12.2,1.12763946699999));
#311199=CARTESIAN_POINT('Ctrl Pts',(-4.54358163000006,5.2,1.12763946699999));
#311200=CARTESIAN_POINT('Ctrl Pts',(-4.54358163000006,2.2,1.12763946699999));
#311201=CARTESIAN_POINT('Ctrl Pts',(-4.54602312200006,12.2,1.12686770099999));
#311202=CARTESIAN_POINT('Ctrl Pts',(-4.54602312200006,5.2,1.12686770099999));
#311203=CARTESIAN_POINT('Ctrl Pts',(-4.54602312200006,2.2,1.12686770099999));
#311204=CARTESIAN_POINT('Ctrl Pts',(-4.54846711400006,12.2,1.12609232899999));
#311205=CARTESIAN_POINT('Ctrl Pts',(-4.54846711400006,5.2,1.12609232899999));
#311206=CARTESIAN_POINT('Ctrl Pts',(-4.54846711400006,2.2,1.12609232899999));
#311207=CARTESIAN_POINT('Ctrl Pts',(-4.55091359700006,12.2,1.12531334799999));
#311208=CARTESIAN_POINT('Ctrl Pts',(-4.55091359700006,5.2,1.12531334799999));
#311209=CARTESIAN_POINT('Ctrl Pts',(-4.55091359700006,2.2,1.12531334799999));
#311210=CARTESIAN_POINT('Ctrl Pts',(-4.55336256300006,12.2,1.12453075199999));
#311211=CARTESIAN_POINT('Ctrl Pts',(-4.55336256300006,5.2,1.12453075199999));
#311212=CARTESIAN_POINT('Ctrl Pts',(-4.55336256300006,2.2,1.12453075199999));
#311213=CARTESIAN_POINT('Ctrl Pts',(-4.55581400300006,12.2,1.12374453699998));
#311214=CARTESIAN_POINT('Ctrl Pts',(-4.55581400300006,5.2,1.12374453699998));
#311215=CARTESIAN_POINT('Ctrl Pts',(-4.55581400300006,2.2,1.12374453699998));
#311216=CARTESIAN_POINT('Ctrl Pts',(-4.55826791200006,12.2,1.12295469999999));
#311217=CARTESIAN_POINT('Ctrl Pts',(-4.55826791200006,5.2,1.12295469999999));
#311218=CARTESIAN_POINT('Ctrl Pts',(-4.55826791200006,2.2,1.12295469999999));
#311219=CARTESIAN_POINT('Ctrl Pts',(-4.56072428100006,12.2,1.12216123699998));
#311220=CARTESIAN_POINT('Ctrl Pts',(-4.56072428100006,5.2,1.12216123699998));
#311221=CARTESIAN_POINT('Ctrl Pts',(-4.56072428100006,2.2,1.12216123699998));
#311222=CARTESIAN_POINT('Ctrl Pts',(-4.56318310300006,12.2,1.12136414299998));
#311223=CARTESIAN_POINT('Ctrl Pts',(-4.56318310300006,5.2,1.12136414299998));
#311224=CARTESIAN_POINT('Ctrl Pts',(-4.56318310300006,2.2,1.12136414299998));
#311225=CARTESIAN_POINT('Ctrl Pts',(-4.56564436900006,12.2,1.12056341499999));
#311226=CARTESIAN_POINT('Ctrl Pts',(-4.56564436900006,5.2,1.12056341499999));
#311227=CARTESIAN_POINT('Ctrl Pts',(-4.56564436900006,2.2,1.12056341499999));
#311228=CARTESIAN_POINT('Ctrl Pts',(-4.56810807200006,12.2,1.11975904799999));
#311229=CARTESIAN_POINT('Ctrl Pts',(-4.56810807200006,5.2,1.11975904799999));
#311230=CARTESIAN_POINT('Ctrl Pts',(-4.56810807200006,2.2,1.11975904799999));
#311231=CARTESIAN_POINT('Ctrl Pts',(-4.57057420300006,12.2,1.11895103799998));
#311232=CARTESIAN_POINT('Ctrl Pts',(-4.57057420300006,5.2,1.11895103799998));
#311233=CARTESIAN_POINT('Ctrl Pts',(-4.57057420300006,2.2,1.11895103799998));
#311234=CARTESIAN_POINT('Ctrl Pts',(-4.57304275500006,12.2,1.11813938099999));
#311235=CARTESIAN_POINT('Ctrl Pts',(-4.57304275500006,5.2,1.11813938099999));
#311236=CARTESIAN_POINT('Ctrl Pts',(-4.57304275500006,2.2,1.11813938099999));
#311237=CARTESIAN_POINT('Ctrl Pts',(-4.57551371900006,12.2,1.11732407299999));
#311238=CARTESIAN_POINT('Ctrl Pts',(-4.57551371900006,5.2,1.11732407299999));
#311239=CARTESIAN_POINT('Ctrl Pts',(-4.57551371900006,2.2,1.11732407299999));
#311240=CARTESIAN_POINT('Ctrl Pts',(-4.57798708800006,12.2,1.11650510999999));
#311241=CARTESIAN_POINT('Ctrl Pts',(-4.57798708800006,5.2,1.11650510999999));
#311242=CARTESIAN_POINT('Ctrl Pts',(-4.57798708800006,2.2,1.11650510999999));
#311243=CARTESIAN_POINT('Ctrl Pts',(-4.58046285400005,12.2,1.11568248799998));
#311244=CARTESIAN_POINT('Ctrl Pts',(-4.58046285400005,5.2,1.11568248799998));
#311245=CARTESIAN_POINT('Ctrl Pts',(-4.58046285400005,2.2,1.11568248799998));
#311246=CARTESIAN_POINT('Ctrl Pts',(-4.58294100900006,12.2,1.11485620299999));
#311247=CARTESIAN_POINT('Ctrl Pts',(-4.58294100900006,5.2,1.11485620299999));
#311248=CARTESIAN_POINT('Ctrl Pts',(-4.58294100900006,2.2,1.11485620299999));
#311249=CARTESIAN_POINT('Ctrl Pts',(-4.58542154700006,12.2,1.11402625099998));
#311250=CARTESIAN_POINT('Ctrl Pts',(-4.58542154700006,5.2,1.11402625099998));
#311251=CARTESIAN_POINT('Ctrl Pts',(-4.58542154700006,2.2,1.11402625099998));
#311252=CARTESIAN_POINT('Ctrl Pts',(-4.58790446200006,12.2,1.11319262999999));
#311253=CARTESIAN_POINT('Ctrl Pts',(-4.58790446200006,5.2,1.11319262999999));
#311254=CARTESIAN_POINT('Ctrl Pts',(-4.58790446200006,2.2,1.11319262999999));
#311255=CARTESIAN_POINT('Ctrl Pts',(-4.59038974600006,12.2,1.11235533599999));
#311256=CARTESIAN_POINT('Ctrl Pts',(-4.59038974600006,5.2,1.11235533599999));
#311257=CARTESIAN_POINT('Ctrl Pts',(-4.59038974600006,2.2,1.11235533599999));
#311258=CARTESIAN_POINT('Ctrl Pts',(-4.59287739000006,12.2,1.11151436499998));
#311259=CARTESIAN_POINT('Ctrl Pts',(-4.59287739000006,5.2,1.11151436499998));
#311260=CARTESIAN_POINT('Ctrl Pts',(-4.59287739000006,2.2,1.11151436499998));
#311261=CARTESIAN_POINT('Ctrl Pts',(-4.59536738800006,12.2,1.11066971099998));
#311262=CARTESIAN_POINT('Ctrl Pts',(-4.59536738800006,5.2,1.11066971099998));
#311263=CARTESIAN_POINT('Ctrl Pts',(-4.59536738800006,2.2,1.11066971099998));
#311264=CARTESIAN_POINT('Ctrl Pts',(-4.59785972700006,12.2,1.10982137199999));
#311265=CARTESIAN_POINT('Ctrl Pts',(-4.59785972700006,5.2,1.10982137199999));
#311266=CARTESIAN_POINT('Ctrl Pts',(-4.59785972700006,2.2,1.10982137199999));
#311267=CARTESIAN_POINT('Ctrl Pts',(-4.60035440100006,12.2,1.10896934199999));
#311268=CARTESIAN_POINT('Ctrl Pts',(-4.60035440100006,5.2,1.10896934199999));
#311269=CARTESIAN_POINT('Ctrl Pts',(-4.60035440100006,2.2,1.10896934199999));
#311270=CARTESIAN_POINT('Ctrl Pts',(-4.60285139700006,12.2,1.10811361599998));
#311271=CARTESIAN_POINT('Ctrl Pts',(-4.60285139700006,5.2,1.10811361599998));
#311272=CARTESIAN_POINT('Ctrl Pts',(-4.60285139700006,2.2,1.10811361599998));
#311273=CARTESIAN_POINT('Ctrl Pts',(-4.60535071000006,12.2,1.10725418899999));
#311274=CARTESIAN_POINT('Ctrl Pts',(-4.60535071000006,5.2,1.10725418899999));
#311275=CARTESIAN_POINT('Ctrl Pts',(-4.60535071000006,2.2,1.10725418899999));
#311276=CARTESIAN_POINT('Ctrl Pts',(-4.60785233100006,12.2,1.10639105899998));
#311277=CARTESIAN_POINT('Ctrl Pts',(-4.60785233100006,5.2,1.10639105899998));
#311278=CARTESIAN_POINT('Ctrl Pts',(-4.60785233100006,2.2,1.10639105899998));
#311279=CARTESIAN_POINT('Ctrl Pts',(-4.61035625300006,12.2,1.10552422199999));
#311280=CARTESIAN_POINT('Ctrl Pts',(-4.61035625300006,5.2,1.10552422199999));
#311281=CARTESIAN_POINT('Ctrl Pts',(-4.61035625300006,2.2,1.10552422199999));
#311282=CARTESIAN_POINT('Ctrl Pts',(-4.61286247400006,12.2,1.10465367699998));
#311283=CARTESIAN_POINT('Ctrl Pts',(-4.61286247400006,5.2,1.10465367699998));
#311284=CARTESIAN_POINT('Ctrl Pts',(-4.61286247400006,2.2,1.10465367699998));
#311285=CARTESIAN_POINT('Ctrl Pts',(-4.61537099100005,12.2,1.10377942299999));
#311286=CARTESIAN_POINT('Ctrl Pts',(-4.61537099100005,5.2,1.10377942299999));
#311287=CARTESIAN_POINT('Ctrl Pts',(-4.61537099100005,2.2,1.10377942299999));
#311288=CARTESIAN_POINT('Ctrl Pts',(-4.61737964100006,12.2,1.10307705199999));
#311289=CARTESIAN_POINT('Ctrl Pts',(-4.61737964100006,5.2,1.10307705199999));
#311290=CARTESIAN_POINT('Ctrl Pts',(-4.61737964100006,2.2,1.10307705199999));
#311291=CARTESIAN_POINT('Ctrl Pts',(-4.61888716100006,12.2,1.10254860399999));
#311292=CARTESIAN_POINT('Ctrl Pts',(-4.61888716100006,5.2,1.10254860399999));
#311293=CARTESIAN_POINT('Ctrl Pts',(-4.61888716100006,2.2,1.10254860399999));
#311294=CARTESIAN_POINT('Ctrl Pts',(-4.61989263400006,12.2,1.10219556399999));
#311295=CARTESIAN_POINT('Ctrl Pts',(-4.61989263400006,5.2,1.10219556399999));
#311296=CARTESIAN_POINT('Ctrl Pts',(-4.61989263400006,2.2,1.10219556399999));
#311297=CARTESIAN_POINT('Ctrl Pts',(-4.62039548500006,12.2,1.10201885899999));
#311298=CARTESIAN_POINT('Ctrl Pts',(-4.62039548500006,5.2,1.10201885899999));
#311299=CARTESIAN_POINT('Ctrl Pts',(-4.62039548500006,2.2,1.10201885899999));
#311300=CARTESIAN_POINT('',(-4.62039548500006,2.7,1.10201885899999));
#311301=CARTESIAN_POINT('',(-4.62039548500006,12.2,1.10201885899999));
#311302=CARTESIAN_POINT('Ctrl Pts',(-3.80828031400006,2.7,1.20296984599999));
#311303=CARTESIAN_POINT('Ctrl Pts',(-3.80845769136914,2.7,1.20302512565856));
#311304=CARTESIAN_POINT('Ctrl Pts',(-3.81014983883408,2.7,1.20354748054386));
#311305=CARTESIAN_POINT('Ctrl Pts',(-3.81751691756265,2.7,1.20546182228747));
#311306=CARTESIAN_POINT('Ctrl Pts',(-3.82198099636819,2.7,1.20648710942369));
#311307=CARTESIAN_POINT('Ctrl Pts',(-3.84154121060164,2.7,1.21064530016897));
#311308=CARTESIAN_POINT('Ctrl Pts',(-3.85807057032119,2.7,1.21321507966715));
#311309=CARTESIAN_POINT('Ctrl Pts',(-3.91840592137738,2.7,1.22066908254686));
#311310=CARTESIAN_POINT('Ctrl Pts',(-3.97606115021901,2.7,1.22367498425562));
#311311=CARTESIAN_POINT('Ctrl Pts',(-4.17888715549711,2.7,1.21549033946434));
#311312=CARTESIAN_POINT('Ctrl Pts',(-4.3738307801898,2.7,1.1886632450385));
#311313=CARTESIAN_POINT('Ctrl Pts',(-4.62039548500006,2.7,1.10201885899999));
#311314=CARTESIAN_POINT('Origin',(-5.66300478732629E-14,15.2,-1.77635683940025E-14));
#311315=CARTESIAN_POINT('',(-4.68689806900006,2.7,0.771677711999986));
#311316=CARTESIAN_POINT('',(-4.68689806900006,12.2,0.771677711999987));
#311317=CARTESIAN_POINT('Origin',(-5.66300478732629E-14,2.7,-1.92943768261394E-14));
#311318=CARTESIAN_POINT('Ctrl Pts',(-4.68689806900006,12.2,0.771677711999987));
#311319=CARTESIAN_POINT('Ctrl Pts',(-4.68689806900006,5.2,0.771677711999987));
#311320=CARTESIAN_POINT('Ctrl Pts',(-4.68689806900006,2.2,0.771677711999987));
#311321=CARTESIAN_POINT('Ctrl Pts',(-4.68650276500005,12.2,0.771320194999987));
#311322=CARTESIAN_POINT('Ctrl Pts',(-4.68650276500005,5.2,0.771320194999987));
#311323=CARTESIAN_POINT('Ctrl Pts',(-4.68650276500005,2.2,0.771320194999987));
#311324=CARTESIAN_POINT('Ctrl Pts',(-4.68571222500006,12.2,0.770605589999986));
#311325=CARTESIAN_POINT('Ctrl Pts',(-4.68571222500006,5.2,0.770605589999986));
#311326=CARTESIAN_POINT('Ctrl Pts',(-4.68571222500006,2.2,0.770605589999986));
#311327=CARTESIAN_POINT('Ctrl Pts',(-4.68452662000006,12.2,0.769534975999986));
#311328=CARTESIAN_POINT('Ctrl Pts',(-4.68452662000006,5.2,0.769534975999986));
#311329=CARTESIAN_POINT('Ctrl Pts',(-4.68452662000006,2.2,0.769534975999986));
#311330=CARTESIAN_POINT('Ctrl Pts',(-4.68294622100006,12.2,0.768110075999986));
#311331=CARTESIAN_POINT('Ctrl Pts',(-4.68294622100006,5.2,0.768110075999986));
#311332=CARTESIAN_POINT('Ctrl Pts',(-4.68294622100006,2.2,0.768110075999986));
#311333=CARTESIAN_POINT('Ctrl Pts',(-4.68097140300006,12.2,0.766333260999983));
#311334=CARTESIAN_POINT('Ctrl Pts',(-4.68097140300006,5.2,0.766333260999983));
#311335=CARTESIAN_POINT('Ctrl Pts',(-4.68097140300006,2.2,0.766333260999983));
#311336=CARTESIAN_POINT('Ctrl Pts',(-4.67899726800006,12.2,0.764560752999985));
#311337=CARTESIAN_POINT('Ctrl Pts',(-4.67899726800006,5.2,0.764560752999985));
#311338=CARTESIAN_POINT('Ctrl Pts',(-4.67899726800006,2.2,0.764560752999985));
#311339=CARTESIAN_POINT('Ctrl Pts',(-4.67702381800006,12.2,0.762792554999985));
#311340=CARTESIAN_POINT('Ctrl Pts',(-4.67702381800006,5.2,0.762792554999985));
#311341=CARTESIAN_POINT('Ctrl Pts',(-4.67702381800006,2.2,0.762792554999985));
#311342=CARTESIAN_POINT('Ctrl Pts',(-4.67505105600006,12.2,0.761028664999985));
#311343=CARTESIAN_POINT('Ctrl Pts',(-4.67505105600006,5.2,0.761028664999985));
#311344=CARTESIAN_POINT('Ctrl Pts',(-4.67505105600006,2.2,0.761028664999985));
#311345=CARTESIAN_POINT('Ctrl Pts',(-4.67307898900006,12.2,0.759269083999987));
#311346=CARTESIAN_POINT('Ctrl Pts',(-4.67307898900006,5.2,0.759269083999987));
#311347=CARTESIAN_POINT('Ctrl Pts',(-4.67307898900006,2.2,0.759269083999987));
#311348=CARTESIAN_POINT('Ctrl Pts',(-4.67110762500006,12.2,0.757513809999986));
#311349=CARTESIAN_POINT('Ctrl Pts',(-4.67110762500006,5.2,0.757513809999986));
#311350=CARTESIAN_POINT('Ctrl Pts',(-4.67110762500006,2.2,0.757513809999986));
#311351=CARTESIAN_POINT('Ctrl Pts',(-4.66913697300006,12.2,0.755762842999985));
#311352=CARTESIAN_POINT('Ctrl Pts',(-4.66913697300006,5.2,0.755762842999985));
#311353=CARTESIAN_POINT('Ctrl Pts',(-4.66913697300006,2.2,0.755762842999985));
#311354=CARTESIAN_POINT('Ctrl Pts',(-4.66716704600006,12.2,0.754016181999986));
#311355=CARTESIAN_POINT('Ctrl Pts',(-4.66716704600006,5.2,0.754016181999986));
#311356=CARTESIAN_POINT('Ctrl Pts',(-4.66716704600006,2.2,0.754016181999986));
#311357=CARTESIAN_POINT('Ctrl Pts',(-4.66519785100005,12.2,0.752273827999983));
#311358=CARTESIAN_POINT('Ctrl Pts',(-4.66519785100005,5.2,0.752273827999983));
#311359=CARTESIAN_POINT('Ctrl Pts',(-4.66519785100005,2.2,0.752273827999983));
#311360=CARTESIAN_POINT('Ctrl Pts',(-4.66322940300006,12.2,0.750535778999986));
#311361=CARTESIAN_POINT('Ctrl Pts',(-4.66322940300006,5.2,0.750535778999986));
#311362=CARTESIAN_POINT('Ctrl Pts',(-4.66322940300006,2.2,0.750535778999986));
#311363=CARTESIAN_POINT('Ctrl Pts',(-4.66126170700006,12.2,0.748802032999984));
#311364=CARTESIAN_POINT('Ctrl Pts',(-4.66126170700006,5.2,0.748802032999984));
#311365=CARTESIAN_POINT('Ctrl Pts',(-4.66126170700006,2.2,0.748802032999984));
#311366=CARTESIAN_POINT('Ctrl Pts',(-4.65929477500006,12.2,0.747072591999984));
#311367=CARTESIAN_POINT('Ctrl Pts',(-4.65929477500006,5.2,0.747072591999984));
#311368=CARTESIAN_POINT('Ctrl Pts',(-4.65929477500006,2.2,0.747072591999984));
#311369=CARTESIAN_POINT('Ctrl Pts',(-4.65732861400006,12.2,0.745347453999985));
#311370=CARTESIAN_POINT('Ctrl Pts',(-4.65732861400006,5.2,0.745347453999985));
#311371=CARTESIAN_POINT('Ctrl Pts',(-4.65732861400006,2.2,0.745347453999985));
#311372=CARTESIAN_POINT('Ctrl Pts',(-4.65536323200006,12.2,0.743626618999986));
#311373=CARTESIAN_POINT('Ctrl Pts',(-4.65536323200006,5.2,0.743626618999986));
#311374=CARTESIAN_POINT('Ctrl Pts',(-4.65536323200006,2.2,0.743626618999986));
#311375=CARTESIAN_POINT('Ctrl Pts',(-4.65339863500006,12.2,0.741910085999984));
#311376=CARTESIAN_POINT('Ctrl Pts',(-4.65339863500006,5.2,0.741910085999984));
#311377=CARTESIAN_POINT('Ctrl Pts',(-4.65339863500006,2.2,0.741910085999984));
#311378=CARTESIAN_POINT('Ctrl Pts',(-4.65143483400006,12.2,0.740197854999987));
#311379=CARTESIAN_POINT('Ctrl Pts',(-4.65143483400006,5.2,0.740197854999987));
#311380=CARTESIAN_POINT('Ctrl Pts',(-4.65143483400006,2.2,0.740197854999987));
#311381=CARTESIAN_POINT('Ctrl Pts',(-4.64947183500006,12.2,0.738489923999985));
#311382=CARTESIAN_POINT('Ctrl Pts',(-4.64947183500006,5.2,0.738489923999985));
#311383=CARTESIAN_POINT('Ctrl Pts',(-4.64947183500006,2.2,0.738489923999985));
#311384=CARTESIAN_POINT('Ctrl Pts',(-4.64750964800006,12.2,0.736786292999985));
#311385=CARTESIAN_POINT('Ctrl Pts',(-4.64750964800006,5.2,0.736786292999985));
#311386=CARTESIAN_POINT('Ctrl Pts',(-4.64750964800006,2.2,0.736786292999985));
#311387=CARTESIAN_POINT('Ctrl Pts',(-4.64554828100006,12.2,0.735086962999985));
#311388=CARTESIAN_POINT('Ctrl Pts',(-4.64554828100006,5.2,0.735086962999985));
#311389=CARTESIAN_POINT('Ctrl Pts',(-4.64554828100006,2.2,0.735086962999985));
#311390=CARTESIAN_POINT('Ctrl Pts',(-4.64358774500006,12.2,0.733391930999985));
#311391=CARTESIAN_POINT('Ctrl Pts',(-4.64358774500006,5.2,0.733391930999985));
#311392=CARTESIAN_POINT('Ctrl Pts',(-4.64358774500006,2.2,0.733391930999985));
#311393=CARTESIAN_POINT('Ctrl Pts',(-4.64162804700006,12.2,0.731701195999985));
#311394=CARTESIAN_POINT('Ctrl Pts',(-4.64162804700006,5.2,0.731701195999985));
#311395=CARTESIAN_POINT('Ctrl Pts',(-4.64162804700006,2.2,0.731701195999985));
#311396=CARTESIAN_POINT('Ctrl Pts',(-4.63966919700006,12.2,0.730014758999986));
#311397=CARTESIAN_POINT('Ctrl Pts',(-4.63966919700006,5.2,0.730014758999986));
#311398=CARTESIAN_POINT('Ctrl Pts',(-4.63966919700006,2.2,0.730014758999986));
#311399=CARTESIAN_POINT('Ctrl Pts',(-4.63771120400006,12.2,0.728332618999987));
#311400=CARTESIAN_POINT('Ctrl Pts',(-4.63771120400006,5.2,0.728332618999987));
#311401=CARTESIAN_POINT('Ctrl Pts',(-4.63771120400006,2.2,0.728332618999987));
#311402=CARTESIAN_POINT('Ctrl Pts',(-4.63575407600006,12.2,0.726654774999984));
#311403=CARTESIAN_POINT('Ctrl Pts',(-4.63575407600006,5.2,0.726654774999984));
#311404=CARTESIAN_POINT('Ctrl Pts',(-4.63575407600006,2.2,0.726654774999984));
#311405=CARTESIAN_POINT('Ctrl Pts',(-4.63379782200006,12.2,0.724981225999985));
#311406=CARTESIAN_POINT('Ctrl Pts',(-4.63379782200006,5.2,0.724981225999985));
#311407=CARTESIAN_POINT('Ctrl Pts',(-4.63379782200006,2.2,0.724981225999985));
#311408=CARTESIAN_POINT('Ctrl Pts',(-4.63184245000006,12.2,0.723311970999987));
#311409=CARTESIAN_POINT('Ctrl Pts',(-4.63184245000006,5.2,0.723311970999987));
#311410=CARTESIAN_POINT('Ctrl Pts',(-4.63184245000006,2.2,0.723311970999987));
#311411=CARTESIAN_POINT('Ctrl Pts',(-4.62988797000006,12.2,0.721647009999984));
#311412=CARTESIAN_POINT('Ctrl Pts',(-4.62988797000006,5.2,0.721647009999984));
#311413=CARTESIAN_POINT('Ctrl Pts',(-4.62988797000006,2.2,0.721647009999984));
#311414=CARTESIAN_POINT('Ctrl Pts',(-4.62793439000006,12.2,0.719986340999985));
#311415=CARTESIAN_POINT('Ctrl Pts',(-4.62793439000006,5.2,0.719986340999985));
#311416=CARTESIAN_POINT('Ctrl Pts',(-4.62793439000006,2.2,0.719986340999985));
#311417=CARTESIAN_POINT('Ctrl Pts',(-4.62598171700006,12.2,0.718329964999986));
#311418=CARTESIAN_POINT('Ctrl Pts',(-4.62598171700006,5.2,0.718329964999986));
#311419=CARTESIAN_POINT('Ctrl Pts',(-4.62598171700006,2.2,0.718329964999986));
#311420=CARTESIAN_POINT('Ctrl Pts',(-4.62402996300006,12.2,0.716677880999987));
#311421=CARTESIAN_POINT('Ctrl Pts',(-4.62402996300006,5.2,0.716677880999987));
#311422=CARTESIAN_POINT('Ctrl Pts',(-4.62402996300006,2.2,0.716677880999987));
#311423=CARTESIAN_POINT('Ctrl Pts',(-4.62207913600006,12.2,0.715030085999988));
#311424=CARTESIAN_POINT('Ctrl Pts',(-4.62207913600006,5.2,0.715030085999988));
#311425=CARTESIAN_POINT('Ctrl Pts',(-4.62207913600006,2.2,0.715030085999988));
#311426=CARTESIAN_POINT('Ctrl Pts',(-4.62012924300006,12.2,0.713386579999984));
#311427=CARTESIAN_POINT('Ctrl Pts',(-4.62012924300006,5.2,0.713386579999984));
#311428=CARTESIAN_POINT('Ctrl Pts',(-4.62012924300006,2.2,0.713386579999984));
#311429=CARTESIAN_POINT('Ctrl Pts',(-4.61818029300006,12.2,0.711747362999984));
#311430=CARTESIAN_POINT('Ctrl Pts',(-4.61818029300006,5.2,0.711747362999984));
#311431=CARTESIAN_POINT('Ctrl Pts',(-4.61818029300006,2.2,0.711747362999984));
#311432=CARTESIAN_POINT('Ctrl Pts',(-4.61623229800006,12.2,0.710112433999988));
#311433=CARTESIAN_POINT('Ctrl Pts',(-4.61623229800006,5.2,0.710112433999988));
#311434=CARTESIAN_POINT('Ctrl Pts',(-4.61623229800006,2.2,0.710112433999988));
#311435=CARTESIAN_POINT('Ctrl Pts',(-4.61428526400006,12.2,0.708481791999986));
#311436=CARTESIAN_POINT('Ctrl Pts',(-4.61428526400006,5.2,0.708481791999986));
#311437=CARTESIAN_POINT('Ctrl Pts',(-4.61428526400006,2.2,0.708481791999986));
#311438=CARTESIAN_POINT('Ctrl Pts',(-4.61233920200006,12.2,0.706855434999984));
#311439=CARTESIAN_POINT('Ctrl Pts',(-4.61233920200006,5.2,0.706855434999984));
#311440=CARTESIAN_POINT('Ctrl Pts',(-4.61233920200006,2.2,0.706855434999984));
#311441=CARTESIAN_POINT('Ctrl Pts',(-4.61039411800006,12.2,0.705233363999986));
#311442=CARTESIAN_POINT('Ctrl Pts',(-4.61039411800006,5.2,0.705233363999986));
#311443=CARTESIAN_POINT('Ctrl Pts',(-4.61039411800006,2.2,0.705233363999986));
#311444=CARTESIAN_POINT('Ctrl Pts',(-4.60845002300006,12.2,0.703615577999983));
#311445=CARTESIAN_POINT('Ctrl Pts',(-4.60845002300006,5.2,0.703615577999983));
#311446=CARTESIAN_POINT('Ctrl Pts',(-4.60845002300006,2.2,0.703615577999983));
#311447=CARTESIAN_POINT('Ctrl Pts',(-4.60650692500006,12.2,0.702002073999988));
#311448=CARTESIAN_POINT('Ctrl Pts',(-4.60650692500006,5.2,0.702002073999988));
#311449=CARTESIAN_POINT('Ctrl Pts',(-4.60650692500006,2.2,0.702002073999988));
#311450=CARTESIAN_POINT('Ctrl Pts',(-4.60456483400006,12.2,0.700392851999982));
#311451=CARTESIAN_POINT('Ctrl Pts',(-4.60456483400006,5.2,0.700392851999982));
#311452=CARTESIAN_POINT('Ctrl Pts',(-4.60456483400006,2.2,0.700392851999982));
#311453=CARTESIAN_POINT('Ctrl Pts',(-4.60262375700006,12.2,0.698787911999985));
#311454=CARTESIAN_POINT('Ctrl Pts',(-4.60262375700006,5.2,0.698787911999985));
#311455=CARTESIAN_POINT('Ctrl Pts',(-4.60262375700006,2.2,0.698787911999985));
#311456=CARTESIAN_POINT('Ctrl Pts',(-4.60068370500006,12.2,0.697187250999987));
#311457=CARTESIAN_POINT('Ctrl Pts',(-4.60068370500006,5.2,0.697187250999987));
#311458=CARTESIAN_POINT('Ctrl Pts',(-4.60068370500006,2.2,0.697187250999987));
#311459=CARTESIAN_POINT('Ctrl Pts',(-4.59874468500006,12.2,0.695590870999983));
#311460=CARTESIAN_POINT('Ctrl Pts',(-4.59874468500006,5.2,0.695590870999983));
#311461=CARTESIAN_POINT('Ctrl Pts',(-4.59874468500006,2.2,0.695590870999983));
#311462=CARTESIAN_POINT('Ctrl Pts',(-4.59680670800005,12.2,0.693998767999986));
#311463=CARTESIAN_POINT('Ctrl Pts',(-4.59680670800005,5.2,0.693998767999986));
#311464=CARTESIAN_POINT('Ctrl Pts',(-4.59680670800005,2.2,0.693998767999986));
#311465=CARTESIAN_POINT('Ctrl Pts',(-4.59486978100006,12.2,0.692410942999988));
#311466=CARTESIAN_POINT('Ctrl Pts',(-4.59486978100006,5.2,0.692410942999988));
#311467=CARTESIAN_POINT('Ctrl Pts',(-4.59486978100006,2.2,0.692410942999988));
#311468=CARTESIAN_POINT('Ctrl Pts',(-4.59293391500006,12.2,0.690827393999989));
#311469=CARTESIAN_POINT('Ctrl Pts',(-4.59293391500006,5.2,0.690827393999989));
#311470=CARTESIAN_POINT('Ctrl Pts',(-4.59293391500006,2.2,0.690827393999989));
#311471=CARTESIAN_POINT('Ctrl Pts',(-4.59099911700006,12.2,0.689248119999988));
#311472=CARTESIAN_POINT('Ctrl Pts',(-4.59099911700006,5.2,0.689248119999988));
#311473=CARTESIAN_POINT('Ctrl Pts',(-4.59099911700006,2.2,0.689248119999988));
#311474=CARTESIAN_POINT('Ctrl Pts',(-4.58906539600005,12.2,0.687673120999985));
#311475=CARTESIAN_POINT('Ctrl Pts',(-4.58906539600005,5.2,0.687673120999985));
#311476=CARTESIAN_POINT('Ctrl Pts',(-4.58906539600005,2.2,0.687673120999985));
#311477=CARTESIAN_POINT('Ctrl Pts',(-4.58713276200006,12.2,0.686102393999986));
#311478=CARTESIAN_POINT('Ctrl Pts',(-4.58713276200006,5.2,0.686102393999986));
#311479=CARTESIAN_POINT('Ctrl Pts',(-4.58713276200006,2.2,0.686102393999986));
#311480=CARTESIAN_POINT('Ctrl Pts',(-4.58520122500006,12.2,0.684535938999984));
#311481=CARTESIAN_POINT('Ctrl Pts',(-4.58520122500006,5.2,0.684535938999984));
#311482=CARTESIAN_POINT('Ctrl Pts',(-4.58520122500006,2.2,0.684535938999984));
#311483=CARTESIAN_POINT('Ctrl Pts',(-4.58327079200005,12.2,0.682973754999985));
#311484=CARTESIAN_POINT('Ctrl Pts',(-4.58327079200005,5.2,0.682973754999985));
#311485=CARTESIAN_POINT('Ctrl Pts',(-4.58327079200005,2.2,0.682973754999985));
#311486=CARTESIAN_POINT('Ctrl Pts',(-4.58134147300005,12.2,0.681415840999984));
#311487=CARTESIAN_POINT('Ctrl Pts',(-4.58134147300005,5.2,0.681415840999984));
#311488=CARTESIAN_POINT('Ctrl Pts',(-4.58134147300005,2.2,0.681415840999984));
#311489=CARTESIAN_POINT('Ctrl Pts',(-4.57941327700006,12.2,0.679862194999985));
#311490=CARTESIAN_POINT('Ctrl Pts',(-4.57941327700006,5.2,0.679862194999985));
#311491=CARTESIAN_POINT('Ctrl Pts',(-4.57941327700006,2.2,0.679862194999985));
#311492=CARTESIAN_POINT('Ctrl Pts',(-4.57748621200006,12.2,0.678312816999984));
#311493=CARTESIAN_POINT('Ctrl Pts',(-4.57748621200006,5.2,0.678312816999984));
#311494=CARTESIAN_POINT('Ctrl Pts',(-4.57748621200006,2.2,0.678312816999984));
#311495=CARTESIAN_POINT('Ctrl Pts',(-4.57556028800005,12.2,0.676767706999986));
#311496=CARTESIAN_POINT('Ctrl Pts',(-4.57556028800005,5.2,0.676767706999986));
#311497=CARTESIAN_POINT('Ctrl Pts',(-4.57556028800005,2.2,0.676767706999986));
#311498=CARTESIAN_POINT('Ctrl Pts',(-4.57363551500006,12.2,0.675226858999984));
#311499=CARTESIAN_POINT('Ctrl Pts',(-4.57363551500006,5.2,0.675226858999984));
#311500=CARTESIAN_POINT('Ctrl Pts',(-4.57363551500006,2.2,0.675226858999984));
#311501=CARTESIAN_POINT('Ctrl Pts',(-4.57171190000006,12.2,0.673690276999985));
#311502=CARTESIAN_POINT('Ctrl Pts',(-4.57171190000006,5.2,0.673690276999985));
#311503=CARTESIAN_POINT('Ctrl Pts',(-4.57171190000006,2.2,0.673690276999985));
#311504=CARTESIAN_POINT('Ctrl Pts',(-4.56978945400006,12.2,0.672157956999988));
#311505=CARTESIAN_POINT('Ctrl Pts',(-4.56978945400006,5.2,0.672157956999988));
#311506=CARTESIAN_POINT('Ctrl Pts',(-4.56978945400006,2.2,0.672157956999988));
#311507=CARTESIAN_POINT('Ctrl Pts',(-4.56786818400006,12.2,0.670629898999984));
#311508=CARTESIAN_POINT('Ctrl Pts',(-4.56786818400006,5.2,0.670629898999984));
#311509=CARTESIAN_POINT('Ctrl Pts',(-4.56786818400006,2.2,0.670629898999984));
#311510=CARTESIAN_POINT('Ctrl Pts',(-4.56594810100006,12.2,0.669106100999985));
#311511=CARTESIAN_POINT('Ctrl Pts',(-4.56594810100006,5.2,0.669106100999985));
#311512=CARTESIAN_POINT('Ctrl Pts',(-4.56594810100006,2.2,0.669106100999985));
#311513=CARTESIAN_POINT('Ctrl Pts',(-4.56402921300006,12.2,0.667586562999984));
#311514=CARTESIAN_POINT('Ctrl Pts',(-4.56402921300006,5.2,0.667586562999984));
#311515=CARTESIAN_POINT('Ctrl Pts',(-4.56402921300006,2.2,0.667586562999984));
#311516=CARTESIAN_POINT('Ctrl Pts',(-4.56211153000006,12.2,0.666071280999985));
#311517=CARTESIAN_POINT('Ctrl Pts',(-4.56211153000006,5.2,0.666071280999985));
#311518=CARTESIAN_POINT('Ctrl Pts',(-4.56211153000006,2.2,0.666071280999985));
#311519=CARTESIAN_POINT('Ctrl Pts',(-4.56019506100006,12.2,0.664560255999986));
#311520=CARTESIAN_POINT('Ctrl Pts',(-4.56019506100006,5.2,0.664560255999986));
#311521=CARTESIAN_POINT('Ctrl Pts',(-4.56019506100006,2.2,0.664560255999986));
#311522=CARTESIAN_POINT('Ctrl Pts',(-4.55827981400006,12.2,0.663053487999985));
#311523=CARTESIAN_POINT('Ctrl Pts',(-4.55827981400006,5.2,0.663053487999985));
#311524=CARTESIAN_POINT('Ctrl Pts',(-4.55827981400006,2.2,0.663053487999985));
#311525=CARTESIAN_POINT('Ctrl Pts',(-4.55636580000006,12.2,0.661550972999985));
#311526=CARTESIAN_POINT('Ctrl Pts',(-4.55636580000006,5.2,0.661550972999985));
#311527=CARTESIAN_POINT('Ctrl Pts',(-4.55636580000006,2.2,0.661550972999985));
#311528=CARTESIAN_POINT('Ctrl Pts',(-4.55445302600006,12.2,0.660052709999985));
#311529=CARTESIAN_POINT('Ctrl Pts',(-4.55445302600006,5.2,0.660052709999985));
#311530=CARTESIAN_POINT('Ctrl Pts',(-4.55445302600006,2.2,0.660052709999985));
#311531=CARTESIAN_POINT('Ctrl Pts',(-4.55254150300005,12.2,0.658558698999983));
#311532=CARTESIAN_POINT('Ctrl Pts',(-4.55254150300005,5.2,0.658558698999983));
#311533=CARTESIAN_POINT('Ctrl Pts',(-4.55254150300005,2.2,0.658558698999983));
#311534=CARTESIAN_POINT('Ctrl Pts',(-4.55063123800006,12.2,0.657068937999985));
#311535=CARTESIAN_POINT('Ctrl Pts',(-4.55063123800006,5.2,0.657068937999985));
#311536=CARTESIAN_POINT('Ctrl Pts',(-4.55063123800006,2.2,0.657068937999985));
#311537=CARTESIAN_POINT('Ctrl Pts',(-4.54872224300006,12.2,0.655583424999988));
#311538=CARTESIAN_POINT('Ctrl Pts',(-4.54872224300006,5.2,0.655583424999988));
#311539=CARTESIAN_POINT('Ctrl Pts',(-4.54872224300006,2.2,0.655583424999988));
#311540=CARTESIAN_POINT('Ctrl Pts',(-4.54681452600005,12.2,0.654102160999983));
#311541=CARTESIAN_POINT('Ctrl Pts',(-4.54681452600005,5.2,0.654102160999983));
#311542=CARTESIAN_POINT('Ctrl Pts',(-4.54681452600005,2.2,0.654102160999983));
#311543=CARTESIAN_POINT('Ctrl Pts',(-4.54490809500006,12.2,0.652625140999987));
#311544=CARTESIAN_POINT('Ctrl Pts',(-4.54490809500006,5.2,0.652625140999987));
#311545=CARTESIAN_POINT('Ctrl Pts',(-4.54490809500006,2.2,0.652625140999987));
#311546=CARTESIAN_POINT('Ctrl Pts',(-4.54300296100006,12.2,0.651152365999987));
#311547=CARTESIAN_POINT('Ctrl Pts',(-4.54300296100006,5.2,0.651152365999987));
#311548=CARTESIAN_POINT('Ctrl Pts',(-4.54300296100006,2.2,0.651152365999987));
#311549=CARTESIAN_POINT('Ctrl Pts',(-4.54109913200006,12.2,0.649683834999983));
#311550=CARTESIAN_POINT('Ctrl Pts',(-4.54109913200006,5.2,0.649683834999983));
#311551=CARTESIAN_POINT('Ctrl Pts',(-4.54109913200006,2.2,0.649683834999983));
#311552=CARTESIAN_POINT('Ctrl Pts',(-4.53919661700006,12.2,0.648219544999984));
#311553=CARTESIAN_POINT('Ctrl Pts',(-4.53919661700006,5.2,0.648219544999984));
#311554=CARTESIAN_POINT('Ctrl Pts',(-4.53919661700006,2.2,0.648219544999984));
#311555=CARTESIAN_POINT('Ctrl Pts',(-4.53729542700006,12.2,0.646759494999984));
#311556=CARTESIAN_POINT('Ctrl Pts',(-4.53729542700006,5.2,0.646759494999984));
#311557=CARTESIAN_POINT('Ctrl Pts',(-4.53729542700006,2.2,0.646759494999984));
#311558=CARTESIAN_POINT('Ctrl Pts',(-4.53539557000005,12.2,0.645303683999985));
#311559=CARTESIAN_POINT('Ctrl Pts',(-4.53539557000005,5.2,0.645303683999985));
#311560=CARTESIAN_POINT('Ctrl Pts',(-4.53539557000005,2.2,0.645303683999985));
#311561=CARTESIAN_POINT('Ctrl Pts',(-4.53349705600006,12.2,0.643852110999985));
#311562=CARTESIAN_POINT('Ctrl Pts',(-4.53349705600006,5.2,0.643852110999985));
#311563=CARTESIAN_POINT('Ctrl Pts',(-4.53349705600006,2.2,0.643852110999985));
#311564=CARTESIAN_POINT('Ctrl Pts',(-4.53159989300006,12.2,0.642404772999985));
#311565=CARTESIAN_POINT('Ctrl Pts',(-4.53159989300006,5.2,0.642404772999985));
#311566=CARTESIAN_POINT('Ctrl Pts',(-4.53159989300006,2.2,0.642404772999985));
#311567=CARTESIAN_POINT('Ctrl Pts',(-4.52970409100006,12.2,0.640961668999989));
#311568=CARTESIAN_POINT('Ctrl Pts',(-4.52970409100006,5.2,0.640961668999989));
#311569=CARTESIAN_POINT('Ctrl Pts',(-4.52970409100006,2.2,0.640961668999989));
#311570=CARTESIAN_POINT('Ctrl Pts',(-4.52780966000006,12.2,0.639522799999988));
#311571=CARTESIAN_POINT('Ctrl Pts',(-4.52780966000006,5.2,0.639522799999988));
#311572=CARTESIAN_POINT('Ctrl Pts',(-4.52780966000006,2.2,0.639522799999988));
#311573=CARTESIAN_POINT('Ctrl Pts',(-4.52591660800006,12.2,0.638088159999985));
#311574=CARTESIAN_POINT('Ctrl Pts',(-4.52591660800006,5.2,0.638088159999985));
#311575=CARTESIAN_POINT('Ctrl Pts',(-4.52591660800006,2.2,0.638088159999985));
#311576=CARTESIAN_POINT('Ctrl Pts',(-4.52402494500006,12.2,0.636657750999987));
#311577=CARTESIAN_POINT('Ctrl Pts',(-4.52402494500006,5.2,0.636657750999987));
#311578=CARTESIAN_POINT('Ctrl Pts',(-4.52402494500006,2.2,0.636657750999987));
#311579=CARTESIAN_POINT('Ctrl Pts',(-4.52213468100005,12.2,0.635231568999988));
#311580=CARTESIAN_POINT('Ctrl Pts',(-4.52213468100005,5.2,0.635231568999988));
#311581=CARTESIAN_POINT('Ctrl Pts',(-4.52213468100005,2.2,0.635231568999988));
#311582=CARTESIAN_POINT('Ctrl Pts',(-4.52024582400006,12.2,0.633809614999983));
#311583=CARTESIAN_POINT('Ctrl Pts',(-4.52024582400006,5.2,0.633809614999983));
#311584=CARTESIAN_POINT('Ctrl Pts',(-4.52024582400006,2.2,0.633809614999983));
#311585=CARTESIAN_POINT('Ctrl Pts',(-4.51835838500006,12.2,0.632391883999985));
#311586=CARTESIAN_POINT('Ctrl Pts',(-4.51835838500006,5.2,0.632391883999985));
#311587=CARTESIAN_POINT('Ctrl Pts',(-4.51835838500006,2.2,0.632391883999985));
#311588=CARTESIAN_POINT('Ctrl Pts',(-4.51647237000006,12.2,0.630978377999987));
#311589=CARTESIAN_POINT('Ctrl Pts',(-4.51647237000006,5.2,0.630978377999987));
#311590=CARTESIAN_POINT('Ctrl Pts',(-4.51647237000006,2.2,0.630978377999987));
#311591=CARTESIAN_POINT('Ctrl Pts',(-4.51458779300006,12.2,0.629569093999987));
#311592=CARTESIAN_POINT('Ctrl Pts',(-4.51458779300006,5.2,0.629569093999987));
#311593=CARTESIAN_POINT('Ctrl Pts',(-4.51458779300006,2.2,0.629569093999987));
#311594=CARTESIAN_POINT('Ctrl Pts',(-4.51270466000006,12.2,0.628164028999985));
#311595=CARTESIAN_POINT('Ctrl Pts',(-4.51270466000006,5.2,0.628164028999985));
#311596=CARTESIAN_POINT('Ctrl Pts',(-4.51270466000006,2.2,0.628164028999985));
#311597=CARTESIAN_POINT('Ctrl Pts',(-4.51082298200006,12.2,0.626763183999985));
#311598=CARTESIAN_POINT('Ctrl Pts',(-4.51082298200006,5.2,0.626763183999985));
#311599=CARTESIAN_POINT('Ctrl Pts',(-4.51082298200006,2.2,0.626763183999985));
#311600=CARTESIAN_POINT('Ctrl Pts',(-4.50894276700006,12.2,0.625366554999989));
#311601=CARTESIAN_POINT('Ctrl Pts',(-4.50894276700006,5.2,0.625366554999989));
#311602=CARTESIAN_POINT('Ctrl Pts',(-4.50894276700006,2.2,0.625366554999989));
#311603=CARTESIAN_POINT('Ctrl Pts',(-4.50706402700006,12.2,0.623974140999985));
#311604=CARTESIAN_POINT('Ctrl Pts',(-4.50706402700006,5.2,0.623974140999985));
#311605=CARTESIAN_POINT('Ctrl Pts',(-4.50706402700006,2.2,0.623974140999985));
#311606=CARTESIAN_POINT('Ctrl Pts',(-4.50518676800006,12.2,0.622585940999985));
#311607=CARTESIAN_POINT('Ctrl Pts',(-4.50518676800006,5.2,0.622585940999985));
#311608=CARTESIAN_POINT('Ctrl Pts',(-4.50518676800006,2.2,0.622585940999985));
#311609=CARTESIAN_POINT('Ctrl Pts',(-4.50331100200006,12.2,0.621201952999986));
#311610=CARTESIAN_POINT('Ctrl Pts',(-4.50331100200006,5.2,0.621201952999986));
#311611=CARTESIAN_POINT('Ctrl Pts',(-4.50331100200006,2.2,0.621201952999986));
#311612=CARTESIAN_POINT('Ctrl Pts',(-4.50143673700006,12.2,0.619822173999989));
#311613=CARTESIAN_POINT('Ctrl Pts',(-4.50143673700006,5.2,0.619822173999989));
#311614=CARTESIAN_POINT('Ctrl Pts',(-4.50143673700006,2.2,0.619822173999989));
#311615=CARTESIAN_POINT('Ctrl Pts',(-4.49956398400006,12.2,0.618446604999985));
#311616=CARTESIAN_POINT('Ctrl Pts',(-4.49956398400006,5.2,0.618446604999985));
#311617=CARTESIAN_POINT('Ctrl Pts',(-4.49956398400006,2.2,0.618446604999985));
#311618=CARTESIAN_POINT('Ctrl Pts',(-4.49769275100006,12.2,0.617075240999987));
#311619=CARTESIAN_POINT('Ctrl Pts',(-4.49769275100006,5.2,0.617075240999987));
#311620=CARTESIAN_POINT('Ctrl Pts',(-4.49769275100006,2.2,0.617075240999987));
#311621=CARTESIAN_POINT('Ctrl Pts',(-4.49582304800006,12.2,0.615708081999986));
#311622=CARTESIAN_POINT('Ctrl Pts',(-4.49582304800006,5.2,0.615708081999986));
#311623=CARTESIAN_POINT('Ctrl Pts',(-4.49582304800006,2.2,0.615708081999986));
#311624=CARTESIAN_POINT('Ctrl Pts',(-4.49395488400006,12.2,0.614345126999982));
#311625=CARTESIAN_POINT('Ctrl Pts',(-4.49395488400006,5.2,0.614345126999982));
#311626=CARTESIAN_POINT('Ctrl Pts',(-4.49395488400006,2.2,0.614345126999982));
#311627=CARTESIAN_POINT('Ctrl Pts',(-4.49208827000006,12.2,0.612986371999984));
#311628=CARTESIAN_POINT('Ctrl Pts',(-4.49208827000006,5.2,0.612986371999984));
#311629=CARTESIAN_POINT('Ctrl Pts',(-4.49208827000006,2.2,0.612986371999984));
#311630=CARTESIAN_POINT('Ctrl Pts',(-4.49022321300006,12.2,0.611631817999987));
#311631=CARTESIAN_POINT('Ctrl Pts',(-4.49022321300006,5.2,0.611631817999987));
#311632=CARTESIAN_POINT('Ctrl Pts',(-4.49022321300006,2.2,0.611631817999987));
#311633=CARTESIAN_POINT('Ctrl Pts',(-4.48835972600006,12.2,0.610281459999986));
#311634=CARTESIAN_POINT('Ctrl Pts',(-4.48835972600006,5.2,0.610281459999986));
#311635=CARTESIAN_POINT('Ctrl Pts',(-4.48835972600006,2.2,0.610281459999986));
#311636=CARTESIAN_POINT('Ctrl Pts',(-4.48649781400006,12.2,0.608935297999986));
#311637=CARTESIAN_POINT('Ctrl Pts',(-4.48649781400006,5.2,0.608935297999986));
#311638=CARTESIAN_POINT('Ctrl Pts',(-4.48649781400006,2.2,0.608935297999986));
#311639=CARTESIAN_POINT('Ctrl Pts',(-4.48463749100006,12.2,0.607593329999983));
#311640=CARTESIAN_POINT('Ctrl Pts',(-4.48463749100006,5.2,0.607593329999983));
#311641=CARTESIAN_POINT('Ctrl Pts',(-4.48463749100006,2.2,0.607593329999983));
#311642=CARTESIAN_POINT('Ctrl Pts',(-4.48277876400006,12.2,0.606255554999984));
#311643=CARTESIAN_POINT('Ctrl Pts',(-4.48277876400006,5.2,0.606255554999984));
#311644=CARTESIAN_POINT('Ctrl Pts',(-4.48277876400006,2.2,0.606255554999984));
#311645=CARTESIAN_POINT('Ctrl Pts',(-4.48092164300006,12.2,0.604921968999985));
#311646=CARTESIAN_POINT('Ctrl Pts',(-4.48092164300006,5.2,0.604921968999985));
#311647=CARTESIAN_POINT('Ctrl Pts',(-4.48092164300006,2.2,0.604921968999985));
#311648=CARTESIAN_POINT('Ctrl Pts',(-4.47906613800006,12.2,0.603592571999982));
#311649=CARTESIAN_POINT('Ctrl Pts',(-4.47906613800006,5.2,0.603592571999982));
#311650=CARTESIAN_POINT('Ctrl Pts',(-4.47906613800006,2.2,0.603592571999982));
#311651=CARTESIAN_POINT('Ctrl Pts',(-4.47721225800006,12.2,0.602267359999988));
#311652=CARTESIAN_POINT('Ctrl Pts',(-4.47721225800006,5.2,0.602267359999988));
#311653=CARTESIAN_POINT('Ctrl Pts',(-4.47721225800006,2.2,0.602267359999988));
#311654=CARTESIAN_POINT('Ctrl Pts',(-4.47536001400006,12.2,0.600946333999985));
#311655=CARTESIAN_POINT('Ctrl Pts',(-4.47536001400006,5.2,0.600946333999985));
#311656=CARTESIAN_POINT('Ctrl Pts',(-4.47536001400006,2.2,0.600946333999985));
#311657=CARTESIAN_POINT('Ctrl Pts',(-4.47350941300006,12.2,0.599629488999986));
#311658=CARTESIAN_POINT('Ctrl Pts',(-4.47350941300006,5.2,0.599629488999986));
#311659=CARTESIAN_POINT('Ctrl Pts',(-4.47350941300006,2.2,0.599629488999986));
#311660=CARTESIAN_POINT('Ctrl Pts',(-4.47166046700006,12.2,0.598316823999987));
#311661=CARTESIAN_POINT('Ctrl Pts',(-4.47166046700006,5.2,0.598316823999987));
#311662=CARTESIAN_POINT('Ctrl Pts',(-4.47166046700006,2.2,0.598316823999987));
#311663=CARTESIAN_POINT('Ctrl Pts',(-4.46981318400006,12.2,0.597008338999987));
#311664=CARTESIAN_POINT('Ctrl Pts',(-4.46981318400006,5.2,0.597008338999987));
#311665=CARTESIAN_POINT('Ctrl Pts',(-4.46981318400006,2.2,0.597008338999987));
#311666=CARTESIAN_POINT('Ctrl Pts',(-4.46796757600006,12.2,0.595704029999986));
#311667=CARTESIAN_POINT('Ctrl Pts',(-4.46796757600006,5.2,0.595704029999986));
#311668=CARTESIAN_POINT('Ctrl Pts',(-4.46796757600006,2.2,0.595704029999986));
#311669=CARTESIAN_POINT('Ctrl Pts',(-4.46612365000005,12.2,0.594403894999989));
#311670=CARTESIAN_POINT('Ctrl Pts',(-4.46612365000005,5.2,0.594403894999989));
#311671=CARTESIAN_POINT('Ctrl Pts',(-4.46612365000005,2.2,0.594403894999989));
#311672=CARTESIAN_POINT('Ctrl Pts',(-4.46428141600006,12.2,0.593107931999985));
#311673=CARTESIAN_POINT('Ctrl Pts',(-4.46428141600006,5.2,0.593107931999985));
#311674=CARTESIAN_POINT('Ctrl Pts',(-4.46428141600006,2.2,0.593107931999985));
#311675=CARTESIAN_POINT('Ctrl Pts',(-4.46244088500006,12.2,0.591816139999986));
#311676=CARTESIAN_POINT('Ctrl Pts',(-4.46244088500006,5.2,0.591816139999986));
#311677=CARTESIAN_POINT('Ctrl Pts',(-4.46244088500006,2.2,0.591816139999986));
#311678=CARTESIAN_POINT('Ctrl Pts',(-4.46060206600006,12.2,0.590528515999988));
#311679=CARTESIAN_POINT('Ctrl Pts',(-4.46060206600006,5.2,0.590528515999988));
#311680=CARTESIAN_POINT('Ctrl Pts',(-4.46060206600006,2.2,0.590528515999988));
#311681=CARTESIAN_POINT('Ctrl Pts',(-4.45876496900006,12.2,0.589245056999985));
#311682=CARTESIAN_POINT('Ctrl Pts',(-4.45876496900006,5.2,0.589245056999985));
#311683=CARTESIAN_POINT('Ctrl Pts',(-4.45876496900006,2.2,0.589245056999985));
#311684=CARTESIAN_POINT('Ctrl Pts',(-4.45692960200006,12.2,0.587965762999985));
#311685=CARTESIAN_POINT('Ctrl Pts',(-4.45692960200006,5.2,0.587965762999985));
#311686=CARTESIAN_POINT('Ctrl Pts',(-4.45692960200006,2.2,0.587965762999985));
#311687=CARTESIAN_POINT('Ctrl Pts',(-4.45509597700006,12.2,0.586690630999982));
#311688=CARTESIAN_POINT('Ctrl Pts',(-4.45509597700006,5.2,0.586690630999982));
#311689=CARTESIAN_POINT('Ctrl Pts',(-4.45509597700006,2.2,0.586690630999982));
#311690=CARTESIAN_POINT('Ctrl Pts',(-4.45326410400006,12.2,0.585419658999986));
#311691=CARTESIAN_POINT('Ctrl Pts',(-4.45326410400006,5.2,0.585419658999986));
#311692=CARTESIAN_POINT('Ctrl Pts',(-4.45326410400006,2.2,0.585419658999986));
#311693=CARTESIAN_POINT('Ctrl Pts',(-4.45143399000006,12.2,0.584152843999988));
#311694=CARTESIAN_POINT('Ctrl Pts',(-4.45143399000006,5.2,0.584152843999988));
#311695=CARTESIAN_POINT('Ctrl Pts',(-4.45143399000006,2.2,0.584152843999988));
#311696=CARTESIAN_POINT('Ctrl Pts',(-4.44960564700006,12.2,0.582890184999982));
#311697=CARTESIAN_POINT('Ctrl Pts',(-4.44960564700006,5.2,0.582890184999982));
#311698=CARTESIAN_POINT('Ctrl Pts',(-4.44960564700006,2.2,0.582890184999982));
#311699=CARTESIAN_POINT('Ctrl Pts',(-4.44777908400006,12.2,0.581631678999983));
#311700=CARTESIAN_POINT('Ctrl Pts',(-4.44777908400006,5.2,0.581631678999983));
#311701=CARTESIAN_POINT('Ctrl Pts',(-4.44777908400006,2.2,0.581631678999983));
#311702=CARTESIAN_POINT('Ctrl Pts',(-4.44595431100006,12.2,0.580377323999985));
#311703=CARTESIAN_POINT('Ctrl Pts',(-4.44595431100006,5.2,0.580377323999985));
#311704=CARTESIAN_POINT('Ctrl Pts',(-4.44595431100006,2.2,0.580377323999985));
#311705=CARTESIAN_POINT('Ctrl Pts',(-4.44413133800006,12.2,0.579127117999985));
#311706=CARTESIAN_POINT('Ctrl Pts',(-4.44413133800006,5.2,0.579127117999985));
#311707=CARTESIAN_POINT('Ctrl Pts',(-4.44413133800006,2.2,0.579127117999985));
#311708=CARTESIAN_POINT('Ctrl Pts',(-4.44231017300006,12.2,0.577881058999985));
#311709=CARTESIAN_POINT('Ctrl Pts',(-4.44231017300006,5.2,0.577881058999985));
#311710=CARTESIAN_POINT('Ctrl Pts',(-4.44231017300006,2.2,0.577881058999985));
#311711=CARTESIAN_POINT('Ctrl Pts',(-4.44049082800006,12.2,0.576639143999986));
#311712=CARTESIAN_POINT('Ctrl Pts',(-4.44049082800006,5.2,0.576639143999986));
#311713=CARTESIAN_POINT('Ctrl Pts',(-4.44049082800006,2.2,0.576639143999986));
#311714=CARTESIAN_POINT('Ctrl Pts',(-4.43867331200006,12.2,0.575401370999984));
#311715=CARTESIAN_POINT('Ctrl Pts',(-4.43867331200006,5.2,0.575401370999984));
#311716=CARTESIAN_POINT('Ctrl Pts',(-4.43867331200006,2.2,0.575401370999984));
#311717=CARTESIAN_POINT('Ctrl Pts',(-4.43685763500006,12.2,0.574167737999982));
#311718=CARTESIAN_POINT('Ctrl Pts',(-4.43685763500006,5.2,0.574167737999982));
#311719=CARTESIAN_POINT('Ctrl Pts',(-4.43685763500006,2.2,0.574167737999982));
#311720=CARTESIAN_POINT('Ctrl Pts',(-4.43504380600006,12.2,0.572938241999985));
#311721=CARTESIAN_POINT('Ctrl Pts',(-4.43504380600006,5.2,0.572938241999985));
#311722=CARTESIAN_POINT('Ctrl Pts',(-4.43504380600006,2.2,0.572938241999985));
#311723=CARTESIAN_POINT('Ctrl Pts',(-4.43323183600006,12.2,0.571712881999984));
#311724=CARTESIAN_POINT('Ctrl Pts',(-4.43323183600006,5.2,0.571712881999984));
#311725=CARTESIAN_POINT('Ctrl Pts',(-4.43323183600006,2.2,0.571712881999984));
#311726=CARTESIAN_POINT('Ctrl Pts',(-4.43142173400005,12.2,0.570491653999987));
#311727=CARTESIAN_POINT('Ctrl Pts',(-4.43142173400005,5.2,0.570491653999987));
#311728=CARTESIAN_POINT('Ctrl Pts',(-4.43142173400005,2.2,0.570491653999987));
#311729=CARTESIAN_POINT('Ctrl Pts',(-4.42961351100006,12.2,0.569274557999986));
#311730=CARTESIAN_POINT('Ctrl Pts',(-4.42961351100006,5.2,0.569274557999986));
#311731=CARTESIAN_POINT('Ctrl Pts',(-4.42961351100006,2.2,0.569274557999986));
#311732=CARTESIAN_POINT('Ctrl Pts',(-4.42780717600006,12.2,0.568061588999988));
#311733=CARTESIAN_POINT('Ctrl Pts',(-4.42780717600006,5.2,0.568061588999988));
#311734=CARTESIAN_POINT('Ctrl Pts',(-4.42780717600006,2.2,0.568061588999988));
#311735=CARTESIAN_POINT('Ctrl Pts',(-4.42600273800006,12.2,0.566852745999986));
#311736=CARTESIAN_POINT('Ctrl Pts',(-4.42600273800006,5.2,0.566852745999986));
#311737=CARTESIAN_POINT('Ctrl Pts',(-4.42600273800006,2.2,0.566852745999986));
#311738=CARTESIAN_POINT('Ctrl Pts',(-4.42420020900006,12.2,0.565648025999987));
#311739=CARTESIAN_POINT('Ctrl Pts',(-4.42420020900006,5.2,0.565648025999987));
#311740=CARTESIAN_POINT('Ctrl Pts',(-4.42420020900006,2.2,0.565648025999987));
#311741=CARTESIAN_POINT('Ctrl Pts',(-4.42239959700006,12.2,0.564447427999983));
#311742=CARTESIAN_POINT('Ctrl Pts',(-4.42239959700006,5.2,0.564447427999983));
#311743=CARTESIAN_POINT('Ctrl Pts',(-4.42239959700006,2.2,0.564447427999983));
#311744=CARTESIAN_POINT('Ctrl Pts',(-4.42060091200006,12.2,0.563250946999982));
#311745=CARTESIAN_POINT('Ctrl Pts',(-4.42060091200006,5.2,0.563250946999982));
#311746=CARTESIAN_POINT('Ctrl Pts',(-4.42060091200006,2.2,0.563250946999982));
#311747=CARTESIAN_POINT('Ctrl Pts',(-4.41880416600006,12.2,0.562058582999985));
#311748=CARTESIAN_POINT('Ctrl Pts',(-4.41880416600006,5.2,0.562058582999985));
#311749=CARTESIAN_POINT('Ctrl Pts',(-4.41880416600006,2.2,0.562058582999985));
#311750=CARTESIAN_POINT('Ctrl Pts',(-4.41700936600006,12.2,0.560870332999985));
#311751=CARTESIAN_POINT('Ctrl Pts',(-4.41700936600006,5.2,0.560870332999985));
#311752=CARTESIAN_POINT('Ctrl Pts',(-4.41700936600006,2.2,0.560870332999985));
#311753=CARTESIAN_POINT('Ctrl Pts',(-4.41521652500006,12.2,0.559686192999984));
#311754=CARTESIAN_POINT('Ctrl Pts',(-4.41521652500006,5.2,0.559686192999984));
#311755=CARTESIAN_POINT('Ctrl Pts',(-4.41521652500006,2.2,0.559686192999984));
#311756=CARTESIAN_POINT('Ctrl Pts',(-4.41342565100006,12.2,0.558506162999985));
#311757=CARTESIAN_POINT('Ctrl Pts',(-4.41342565100006,5.2,0.558506162999985));
#311758=CARTESIAN_POINT('Ctrl Pts',(-4.41342565100006,2.2,0.558506162999985));
#311759=CARTESIAN_POINT('Ctrl Pts',(-4.41163675500006,12.2,0.557330237999984));
#311760=CARTESIAN_POINT('Ctrl Pts',(-4.41163675500006,5.2,0.557330237999984));
#311761=CARTESIAN_POINT('Ctrl Pts',(-4.41163675500006,2.2,0.557330237999984));
#311762=CARTESIAN_POINT('Ctrl Pts',(-4.40984984500005,12.2,0.556158416999986));
#311763=CARTESIAN_POINT('Ctrl Pts',(-4.40984984500005,5.2,0.556158416999986));
#311764=CARTESIAN_POINT('Ctrl Pts',(-4.40984984500005,2.2,0.556158416999986));
#311765=CARTESIAN_POINT('Ctrl Pts',(-4.40806493400006,12.2,0.554990695999984));
#311766=CARTESIAN_POINT('Ctrl Pts',(-4.40806493400006,5.2,0.554990695999984));
#311767=CARTESIAN_POINT('Ctrl Pts',(-4.40806493400006,2.2,0.554990695999984));
#311768=CARTESIAN_POINT('Ctrl Pts',(-4.40628203000006,12.2,0.553827074999984));
#311769=CARTESIAN_POINT('Ctrl Pts',(-4.40628203000006,5.2,0.553827074999984));
#311770=CARTESIAN_POINT('Ctrl Pts',(-4.40628203000006,2.2,0.553827074999984));
#311771=CARTESIAN_POINT('Ctrl Pts',(-4.40450114300006,12.2,0.552667548999985));
#311772=CARTESIAN_POINT('Ctrl Pts',(-4.40450114300006,5.2,0.552667548999985));
#311773=CARTESIAN_POINT('Ctrl Pts',(-4.40450114300006,2.2,0.552667548999985));
#311774=CARTESIAN_POINT('Ctrl Pts',(-4.40272228400006,12.2,0.551512115999984));
#311775=CARTESIAN_POINT('Ctrl Pts',(-4.40272228400006,5.2,0.551512115999984));
#311776=CARTESIAN_POINT('Ctrl Pts',(-4.40272228400006,2.2,0.551512115999984));
#311777=CARTESIAN_POINT('Ctrl Pts',(-4.40094546300006,12.2,0.550360773999987));
#311778=CARTESIAN_POINT('Ctrl Pts',(-4.40094546300006,5.2,0.550360773999987));
#311779=CARTESIAN_POINT('Ctrl Pts',(-4.40094546300006,2.2,0.550360773999987));
#311780=CARTESIAN_POINT('Ctrl Pts',(-4.39917068900006,12.2,0.549213519999987));
#311781=CARTESIAN_POINT('Ctrl Pts',(-4.39917068900006,5.2,0.549213519999987));
#311782=CARTESIAN_POINT('Ctrl Pts',(-4.39917068900006,2.2,0.549213519999987));
#311783=CARTESIAN_POINT('Ctrl Pts',(-4.39739797300006,12.2,0.548070350999983));
#311784=CARTESIAN_POINT('Ctrl Pts',(-4.39739797300006,5.2,0.548070350999983));
#311785=CARTESIAN_POINT('Ctrl Pts',(-4.39739797300006,2.2,0.548070350999983));
#311786=CARTESIAN_POINT('Ctrl Pts',(-4.39562732400006,12.2,0.546931263999983));
#311787=CARTESIAN_POINT('Ctrl Pts',(-4.39562732400006,5.2,0.546931263999983));
#311788=CARTESIAN_POINT('Ctrl Pts',(-4.39562732400006,2.2,0.546931263999983));
#311789=CARTESIAN_POINT('Ctrl Pts',(-4.39385875300006,12.2,0.545796257999989));
#311790=CARTESIAN_POINT('Ctrl Pts',(-4.39385875300006,5.2,0.545796257999989));
#311791=CARTESIAN_POINT('Ctrl Pts',(-4.39385875300006,2.2,0.545796257999989));
#311792=CARTESIAN_POINT('Ctrl Pts',(-4.39209227100006,12.2,0.544665327999985));
#311793=CARTESIAN_POINT('Ctrl Pts',(-4.39209227100006,5.2,0.544665327999985));
#311794=CARTESIAN_POINT('Ctrl Pts',(-4.39209227100006,2.2,0.544665327999985));
#311795=CARTESIAN_POINT('Ctrl Pts',(-4.39032788600006,12.2,0.543538472999985));
#311796=CARTESIAN_POINT('Ctrl Pts',(-4.39032788600006,5.2,0.543538472999985));
#311797=CARTESIAN_POINT('Ctrl Pts',(-4.39032788600006,2.2,0.543538472999985));
#311798=CARTESIAN_POINT('Ctrl Pts',(-4.38856561000006,12.2,0.542415689999984));
#311799=CARTESIAN_POINT('Ctrl Pts',(-4.38856561000006,5.2,0.542415689999984));
#311800=CARTESIAN_POINT('Ctrl Pts',(-4.38856561000006,2.2,0.542415689999984));
#311801=CARTESIAN_POINT('Ctrl Pts',(-4.38680545200006,12.2,0.541296975999987));
#311802=CARTESIAN_POINT('Ctrl Pts',(-4.38680545200006,5.2,0.541296975999987));
#311803=CARTESIAN_POINT('Ctrl Pts',(-4.38680545200006,2.2,0.541296975999987));
#311804=CARTESIAN_POINT('Ctrl Pts',(-4.38504742300006,12.2,0.540182326999985));
#311805=CARTESIAN_POINT('Ctrl Pts',(-4.38504742300006,5.2,0.540182326999985));
#311806=CARTESIAN_POINT('Ctrl Pts',(-4.38504742300006,2.2,0.540182326999985));
#311807=CARTESIAN_POINT('Ctrl Pts',(-4.38329153100006,12.2,0.539071742999986));
#311808=CARTESIAN_POINT('Ctrl Pts',(-4.38329153100006,5.2,0.539071742999986));
#311809=CARTESIAN_POINT('Ctrl Pts',(-4.38329153100006,2.2,0.539071742999986));
#311810=CARTESIAN_POINT('Ctrl Pts',(-4.38153778900006,12.2,0.537965217999985));
#311811=CARTESIAN_POINT('Ctrl Pts',(-4.38153778900006,5.2,0.537965217999985));
#311812=CARTESIAN_POINT('Ctrl Pts',(-4.38153778900006,2.2,0.537965217999985));
#311813=CARTESIAN_POINT('Ctrl Pts',(-4.37978620700005,12.2,0.536862750999987));
#311814=CARTESIAN_POINT('Ctrl Pts',(-4.37978620700005,5.2,0.536862750999987));
#311815=CARTESIAN_POINT('Ctrl Pts',(-4.37978620700005,2.2,0.536862750999987));
#311816=CARTESIAN_POINT('Ctrl Pts',(-4.37803679200006,12.2,0.535764338999982));
#311817=CARTESIAN_POINT('Ctrl Pts',(-4.37803679200006,5.2,0.535764338999982));
#311818=CARTESIAN_POINT('Ctrl Pts',(-4.37803679200006,2.2,0.535764338999982));
#311819=CARTESIAN_POINT('Ctrl Pts',(-4.37628955800006,12.2,0.534669978999984));
#311820=CARTESIAN_POINT('Ctrl Pts',(-4.37628955800006,5.2,0.534669978999984));
#311821=CARTESIAN_POINT('Ctrl Pts',(-4.37628955800006,2.2,0.534669978999984));
#311822=CARTESIAN_POINT('Ctrl Pts',(-4.37454451300006,12.2,0.533579666999984));
#311823=CARTESIAN_POINT('Ctrl Pts',(-4.37454451300006,5.2,0.533579666999984));
#311824=CARTESIAN_POINT('Ctrl Pts',(-4.37454451300006,2.2,0.533579666999984));
#311825=CARTESIAN_POINT('Ctrl Pts',(-4.37280166800006,12.2,0.532493402999985));
#311826=CARTESIAN_POINT('Ctrl Pts',(-4.37280166800006,5.2,0.532493402999985));
#311827=CARTESIAN_POINT('Ctrl Pts',(-4.37280166800006,2.2,0.532493402999985));
#311828=CARTESIAN_POINT('Ctrl Pts',(-4.37106103400006,12.2,0.531411180999988));
#311829=CARTESIAN_POINT('Ctrl Pts',(-4.37106103400006,5.2,0.531411180999988));
#311830=CARTESIAN_POINT('Ctrl Pts',(-4.37106103400006,2.2,0.531411180999988));
#311831=CARTESIAN_POINT('Ctrl Pts',(-4.36932262000005,12.2,0.530332998999987));
#311832=CARTESIAN_POINT('Ctrl Pts',(-4.36932262000005,5.2,0.530332998999987));
#311833=CARTESIAN_POINT('Ctrl Pts',(-4.36932262000005,2.2,0.530332998999987));
#311834=CARTESIAN_POINT('Ctrl Pts',(-4.36758643600006,12.2,0.529258853999988));
#311835=CARTESIAN_POINT('Ctrl Pts',(-4.36758643600006,5.2,0.529258853999988));
#311836=CARTESIAN_POINT('Ctrl Pts',(-4.36758643600006,2.2,0.529258853999988));
#311837=CARTESIAN_POINT('Ctrl Pts',(-4.36585249300006,12.2,0.528188743999984));
#311838=CARTESIAN_POINT('Ctrl Pts',(-4.36585249300006,5.2,0.528188743999984));
#311839=CARTESIAN_POINT('Ctrl Pts',(-4.36585249300006,2.2,0.528188743999984));
#311840=CARTESIAN_POINT('Ctrl Pts',(-4.36412080200006,12.2,0.527122664999986));
#311841=CARTESIAN_POINT('Ctrl Pts',(-4.36412080200006,5.2,0.527122664999986));
#311842=CARTESIAN_POINT('Ctrl Pts',(-4.36412080200006,2.2,0.527122664999986));
#311843=CARTESIAN_POINT('Ctrl Pts',(-4.36239137100006,12.2,0.526060612999988));
#311844=CARTESIAN_POINT('Ctrl Pts',(-4.36239137100006,5.2,0.526060612999988));
#311845=CARTESIAN_POINT('Ctrl Pts',(-4.36239137100006,2.2,0.526060612999988));
#311846=CARTESIAN_POINT('Ctrl Pts',(-4.36066421300006,12.2,0.525002587999985));
#311847=CARTESIAN_POINT('Ctrl Pts',(-4.36066421300006,5.2,0.525002587999985));
#311848=CARTESIAN_POINT('Ctrl Pts',(-4.36066421300006,2.2,0.525002587999985));
#311849=CARTESIAN_POINT('Ctrl Pts',(-4.35893933600005,12.2,0.523948583999987));
#311850=CARTESIAN_POINT('Ctrl Pts',(-4.35893933600005,5.2,0.523948583999987));
#311851=CARTESIAN_POINT('Ctrl Pts',(-4.35893933600005,2.2,0.523948583999987));
#311852=CARTESIAN_POINT('Ctrl Pts',(-4.35721675300006,12.2,0.522898598999983));
#311853=CARTESIAN_POINT('Ctrl Pts',(-4.35721675300006,5.2,0.522898598999983));
#311854=CARTESIAN_POINT('Ctrl Pts',(-4.35721675300006,2.2,0.522898598999983));
#311855=CARTESIAN_POINT('Ctrl Pts',(-4.35549647200006,12.2,0.521852629999984));
#311856=CARTESIAN_POINT('Ctrl Pts',(-4.35549647200006,5.2,0.521852629999984));
#311857=CARTESIAN_POINT('Ctrl Pts',(-4.35549647200006,2.2,0.521852629999984));
#311858=CARTESIAN_POINT('Ctrl Pts',(-4.35377850500006,12.2,0.520810673999983));
#311859=CARTESIAN_POINT('Ctrl Pts',(-4.35377850500006,5.2,0.520810673999983));
#311860=CARTESIAN_POINT('Ctrl Pts',(-4.35377850500006,2.2,0.520810673999983));
#311861=CARTESIAN_POINT('Ctrl Pts',(-4.35206286100006,12.2,0.519772727999985));
#311862=CARTESIAN_POINT('Ctrl Pts',(-4.35206286100006,5.2,0.519772727999985));
#311863=CARTESIAN_POINT('Ctrl Pts',(-4.35206286100006,2.2,0.519772727999985));
#311864=CARTESIAN_POINT('Ctrl Pts',(-4.35034955100006,12.2,0.518738786999986));
#311865=CARTESIAN_POINT('Ctrl Pts',(-4.35034955100006,5.2,0.518738786999986));
#311866=CARTESIAN_POINT('Ctrl Pts',(-4.35034955100006,2.2,0.518738786999986));
#311867=CARTESIAN_POINT('Ctrl Pts',(-4.34863858500006,12.2,0.517708849999985));
#311868=CARTESIAN_POINT('Ctrl Pts',(-4.34863858500006,5.2,0.517708849999985));
#311869=CARTESIAN_POINT('Ctrl Pts',(-4.34863858500006,2.2,0.517708849999985));
#311870=CARTESIAN_POINT('Ctrl Pts',(-4.34692997500005,12.2,0.516682913999986));
#311871=CARTESIAN_POINT('Ctrl Pts',(-4.34692997500005,5.2,0.516682913999986));
#311872=CARTESIAN_POINT('Ctrl Pts',(-4.34692997500005,2.2,0.516682913999986));
#311873=CARTESIAN_POINT('Ctrl Pts',(-4.34522372900005,12.2,0.515660973999985));
#311874=CARTESIAN_POINT('Ctrl Pts',(-4.34522372900005,5.2,0.515660973999985));
#311875=CARTESIAN_POINT('Ctrl Pts',(-4.34522372900005,2.2,0.515660973999985));
#311876=CARTESIAN_POINT('Ctrl Pts',(-4.34351985900006,12.2,0.514643026999986));
#311877=CARTESIAN_POINT('Ctrl Pts',(-4.34351985900006,5.2,0.514643026999986));
#311878=CARTESIAN_POINT('Ctrl Pts',(-4.34351985900006,2.2,0.514643026999986));
#311879=CARTESIAN_POINT('Ctrl Pts',(-4.34181837600006,12.2,0.513629070999984));
#311880=CARTESIAN_POINT('Ctrl Pts',(-4.34181837600006,5.2,0.513629070999984));
#311881=CARTESIAN_POINT('Ctrl Pts',(-4.34181837600006,2.2,0.513629070999984));
#311882=CARTESIAN_POINT('Ctrl Pts',(-4.34011928900006,12.2,0.512619101999987));
#311883=CARTESIAN_POINT('Ctrl Pts',(-4.34011928900006,5.2,0.512619101999987));
#311884=CARTESIAN_POINT('Ctrl Pts',(-4.34011928900006,2.2,0.512619101999987));
#311885=CARTESIAN_POINT('Ctrl Pts',(-4.33842260800006,12.2,0.511613116999987));
#311886=CARTESIAN_POINT('Ctrl Pts',(-4.33842260800006,5.2,0.511613116999987));
#311887=CARTESIAN_POINT('Ctrl Pts',(-4.33842260800006,2.2,0.511613116999987));
#311888=CARTESIAN_POINT('Ctrl Pts',(-4.33672834600006,12.2,0.510611111999988));
#311889=CARTESIAN_POINT('Ctrl Pts',(-4.33672834600006,5.2,0.510611111999988));
#311890=CARTESIAN_POINT('Ctrl Pts',(-4.33672834600006,2.2,0.510611111999988));
#311891=CARTESIAN_POINT('Ctrl Pts',(-4.33503651100006,12.2,0.509613083999985));
#311892=CARTESIAN_POINT('Ctrl Pts',(-4.33503651100006,5.2,0.509613083999985));
#311893=CARTESIAN_POINT('Ctrl Pts',(-4.33503651100006,2.2,0.509613083999985));
#311894=CARTESIAN_POINT('Ctrl Pts',(-4.33334711500006,12.2,0.508619029999986));
#311895=CARTESIAN_POINT('Ctrl Pts',(-4.33334711500006,5.2,0.508619029999986));
#311896=CARTESIAN_POINT('Ctrl Pts',(-4.33334711500006,2.2,0.508619029999986));
#311897=CARTESIAN_POINT('Ctrl Pts',(-4.33166016800006,12.2,0.507628945999983));
#311898=CARTESIAN_POINT('Ctrl Pts',(-4.33166016800006,5.2,0.507628945999983));
#311899=CARTESIAN_POINT('Ctrl Pts',(-4.33166016800006,2.2,0.507628945999983));
#311900=CARTESIAN_POINT('Ctrl Pts',(-4.32997568100006,12.2,0.506642829999984));
#311901=CARTESIAN_POINT('Ctrl Pts',(-4.32997568100006,5.2,0.506642829999984));
#311902=CARTESIAN_POINT('Ctrl Pts',(-4.32997568100006,2.2,0.506642829999984));
#311903=CARTESIAN_POINT('Ctrl Pts',(-4.32829366300005,12.2,0.505660676999984));
#311904=CARTESIAN_POINT('Ctrl Pts',(-4.32829366300005,5.2,0.505660676999984));
#311905=CARTESIAN_POINT('Ctrl Pts',(-4.32829366300005,2.2,0.505660676999984));
#311906=CARTESIAN_POINT('Ctrl Pts',(-4.32661412700006,12.2,0.504682482999983));
#311907=CARTESIAN_POINT('Ctrl Pts',(-4.32661412700006,5.2,0.504682482999983));
#311908=CARTESIAN_POINT('Ctrl Pts',(-4.32661412700006,2.2,0.504682482999983));
#311909=CARTESIAN_POINT('Ctrl Pts',(-4.32493708300006,12.2,0.503708246999985));
#311910=CARTESIAN_POINT('Ctrl Pts',(-4.32493708300006,5.2,0.503708246999985));
#311911=CARTESIAN_POINT('Ctrl Pts',(-4.32493708300006,2.2,0.503708246999985));
#311912=CARTESIAN_POINT('Ctrl Pts',(-4.32326253900006,12.2,0.502737962999986));
#311913=CARTESIAN_POINT('Ctrl Pts',(-4.32326253900006,5.2,0.502737962999986));
#311914=CARTESIAN_POINT('Ctrl Pts',(-4.32326253900006,2.2,0.502737962999986));
#311915=CARTESIAN_POINT('Ctrl Pts',(-4.32159050800006,12.2,0.501771628999985));
#311916=CARTESIAN_POINT('Ctrl Pts',(-4.32159050800006,5.2,0.501771628999985));
#311917=CARTESIAN_POINT('Ctrl Pts',(-4.32159050800006,2.2,0.501771628999985));
#311918=CARTESIAN_POINT('Ctrl Pts',(-4.31992100100006,12.2,0.500809241999987));
#311919=CARTESIAN_POINT('Ctrl Pts',(-4.31992100100006,5.2,0.500809241999987));
#311920=CARTESIAN_POINT('Ctrl Pts',(-4.31992100100006,2.2,0.500809241999987));
#311921=CARTESIAN_POINT('Ctrl Pts',(-4.31825402600006,12.2,0.499850796999985));
#311922=CARTESIAN_POINT('Ctrl Pts',(-4.31825402600006,5.2,0.499850796999985));
#311923=CARTESIAN_POINT('Ctrl Pts',(-4.31825402600006,2.2,0.499850796999985));
#311924=CARTESIAN_POINT('Ctrl Pts',(-4.31658959700005,12.2,0.498896291999986));
#311925=CARTESIAN_POINT('Ctrl Pts',(-4.31658959700005,5.2,0.498896291999986));
#311926=CARTESIAN_POINT('Ctrl Pts',(-4.31658959700005,2.2,0.498896291999986));
#311927=CARTESIAN_POINT('Ctrl Pts',(-4.31492772200006,12.2,0.497945720999984));
#311928=CARTESIAN_POINT('Ctrl Pts',(-4.31492772200006,5.2,0.497945720999984));
#311929=CARTESIAN_POINT('Ctrl Pts',(-4.31492772200006,2.2,0.497945720999984));
#311930=CARTESIAN_POINT('Ctrl Pts',(-4.31326841300006,12.2,0.496999082999987));
#311931=CARTESIAN_POINT('Ctrl Pts',(-4.31326841300006,5.2,0.496999082999987));
#311932=CARTESIAN_POINT('Ctrl Pts',(-4.31326841300006,2.2,0.496999082999987));
#311933=CARTESIAN_POINT('Ctrl Pts',(-4.31161168100005,12.2,0.496056371999987));
#311934=CARTESIAN_POINT('Ctrl Pts',(-4.31161168100005,5.2,0.496056371999987));
#311935=CARTESIAN_POINT('Ctrl Pts',(-4.31161168100005,2.2,0.496056371999987));
#311936=CARTESIAN_POINT('Ctrl Pts',(-4.30995753500006,12.2,0.495117585999987));
#311937=CARTESIAN_POINT('Ctrl Pts',(-4.30995753500006,5.2,0.495117585999987));
#311938=CARTESIAN_POINT('Ctrl Pts',(-4.30995753500006,2.2,0.495117585999987));
#311939=CARTESIAN_POINT('Ctrl Pts',(-4.30830598800005,12.2,0.494182721999987));
#311940=CARTESIAN_POINT('Ctrl Pts',(-4.30830598800005,5.2,0.494182721999987));
#311941=CARTESIAN_POINT('Ctrl Pts',(-4.30830598800005,2.2,0.494182721999987));
#311942=CARTESIAN_POINT('Ctrl Pts',(-4.30665704900006,12.2,0.493251773999983));
#311943=CARTESIAN_POINT('Ctrl Pts',(-4.30665704900006,5.2,0.493251773999983));
#311944=CARTESIAN_POINT('Ctrl Pts',(-4.30665704900006,2.2,0.493251773999983));
#311945=CARTESIAN_POINT('Ctrl Pts',(-4.30501072900006,12.2,0.492324739999983));
#311946=CARTESIAN_POINT('Ctrl Pts',(-4.30501072900006,5.2,0.492324739999983));
#311947=CARTESIAN_POINT('Ctrl Pts',(-4.30501072900006,2.2,0.492324739999983));
#311948=CARTESIAN_POINT('Ctrl Pts',(-4.30336703900006,12.2,0.491401615999987));
#311949=CARTESIAN_POINT('Ctrl Pts',(-4.30336703900006,5.2,0.491401615999987));
#311950=CARTESIAN_POINT('Ctrl Pts',(-4.30336703900006,2.2,0.491401615999987));
#311951=CARTESIAN_POINT('Ctrl Pts',(-4.30172598900006,12.2,0.490482396999985));
#311952=CARTESIAN_POINT('Ctrl Pts',(-4.30172598900006,5.2,0.490482396999985));
#311953=CARTESIAN_POINT('Ctrl Pts',(-4.30172598900006,2.2,0.490482396999985));
#311954=CARTESIAN_POINT('Ctrl Pts',(-4.30008759200006,12.2,0.489567081999986));
#311955=CARTESIAN_POINT('Ctrl Pts',(-4.30008759200006,5.2,0.489567081999986));
#311956=CARTESIAN_POINT('Ctrl Pts',(-4.30008759200006,2.2,0.489567081999986));
#311957=CARTESIAN_POINT('Ctrl Pts',(-4.29845185500006,12.2,0.488655663999986));
#311958=CARTESIAN_POINT('Ctrl Pts',(-4.29845185500006,5.2,0.488655663999986));
#311959=CARTESIAN_POINT('Ctrl Pts',(-4.29845185500006,2.2,0.488655663999986));
#311960=CARTESIAN_POINT('Ctrl Pts',(-4.29681879300006,12.2,0.487748140999984));
#311961=CARTESIAN_POINT('Ctrl Pts',(-4.29681879300006,5.2,0.487748140999984));
#311962=CARTESIAN_POINT('Ctrl Pts',(-4.29681879300006,2.2,0.487748140999984));
#311963=CARTESIAN_POINT('Ctrl Pts',(-4.29518841400006,12.2,0.486844509999984));
#311964=CARTESIAN_POINT('Ctrl Pts',(-4.29518841400006,5.2,0.486844509999984));
#311965=CARTESIAN_POINT('Ctrl Pts',(-4.29518841400006,2.2,0.486844509999984));
#311966=CARTESIAN_POINT('Ctrl Pts',(-4.29356073000006,12.2,0.485944765999986));
#311967=CARTESIAN_POINT('Ctrl Pts',(-4.29356073000006,5.2,0.485944765999986));
#311968=CARTESIAN_POINT('Ctrl Pts',(-4.29356073000006,2.2,0.485944765999986));
#311969=CARTESIAN_POINT('Ctrl Pts',(-4.29193575100006,12.2,0.485048903999985));
#311970=CARTESIAN_POINT('Ctrl Pts',(-4.29193575100006,5.2,0.485048903999985));
#311971=CARTESIAN_POINT('Ctrl Pts',(-4.29193575100006,2.2,0.485048903999985));
#311972=CARTESIAN_POINT('Ctrl Pts',(-4.29031348800006,12.2,0.484156920999985));
#311973=CARTESIAN_POINT('Ctrl Pts',(-4.29031348800006,5.2,0.484156920999985));
#311974=CARTESIAN_POINT('Ctrl Pts',(-4.29031348800006,2.2,0.484156920999985));
#311975=CARTESIAN_POINT('Ctrl Pts',(-4.28869395300006,12.2,0.483268814999986));
#311976=CARTESIAN_POINT('Ctrl Pts',(-4.28869395300006,5.2,0.483268814999986));
#311977=CARTESIAN_POINT('Ctrl Pts',(-4.28869395300006,2.2,0.483268814999986));
#311978=CARTESIAN_POINT('Ctrl Pts',(-4.28707715600006,12.2,0.482384579999984));
#311979=CARTESIAN_POINT('Ctrl Pts',(-4.28707715600006,5.2,0.482384579999984));
#311980=CARTESIAN_POINT('Ctrl Pts',(-4.28707715600006,2.2,0.482384579999984));
#311981=CARTESIAN_POINT('Ctrl Pts',(-4.28546310800006,12.2,0.481504210999986));
#311982=CARTESIAN_POINT('Ctrl Pts',(-4.28546310800006,5.2,0.481504210999986));
#311983=CARTESIAN_POINT('Ctrl Pts',(-4.28546310800006,2.2,0.481504210999986));
#311984=CARTESIAN_POINT('Ctrl Pts',(-4.28385181900006,12.2,0.480627706999983));
#311985=CARTESIAN_POINT('Ctrl Pts',(-4.28385181900006,5.2,0.480627706999983));
#311986=CARTESIAN_POINT('Ctrl Pts',(-4.28385181900006,2.2,0.480627706999983));
#311987=CARTESIAN_POINT('Ctrl Pts',(-4.28224330200006,12.2,0.479755061999985));
#311988=CARTESIAN_POINT('Ctrl Pts',(-4.28224330200006,5.2,0.479755061999985));
#311989=CARTESIAN_POINT('Ctrl Pts',(-4.28224330200006,2.2,0.479755061999985));
#311990=CARTESIAN_POINT('Ctrl Pts',(-4.28063756600006,12.2,0.478886270999985));
#311991=CARTESIAN_POINT('Ctrl Pts',(-4.28063756600006,5.2,0.478886270999985));
#311992=CARTESIAN_POINT('Ctrl Pts',(-4.28063756600006,2.2,0.478886270999985));
#311993=CARTESIAN_POINT('Ctrl Pts',(-4.27903462300006,12.2,0.478021332999985));
#311994=CARTESIAN_POINT('Ctrl Pts',(-4.27903462300006,5.2,0.478021332999985));
#311995=CARTESIAN_POINT('Ctrl Pts',(-4.27903462300006,2.2,0.478021332999985));
#311996=CARTESIAN_POINT('Ctrl Pts',(-4.27743448300006,12.2,0.477160242999983));
#311997=CARTESIAN_POINT('Ctrl Pts',(-4.27743448300006,5.2,0.477160242999983));
#311998=CARTESIAN_POINT('Ctrl Pts',(-4.27743448300006,2.2,0.477160242999983));
#311999=CARTESIAN_POINT('Ctrl Pts',(-4.27583715800006,12.2,0.476302994999984));
#312000=CARTESIAN_POINT('Ctrl Pts',(-4.27583715800006,5.2,0.476302994999984));
#312001=CARTESIAN_POINT('Ctrl Pts',(-4.27583715800006,2.2,0.476302994999984));
#312002=CARTESIAN_POINT('Ctrl Pts',(-4.27424265900005,12.2,0.475449585999983));
#312003=CARTESIAN_POINT('Ctrl Pts',(-4.27424265900005,5.2,0.475449585999983));
#312004=CARTESIAN_POINT('Ctrl Pts',(-4.27424265900005,2.2,0.475449585999983));
#312005=CARTESIAN_POINT('Ctrl Pts',(-4.27265099500006,12.2,0.474600012999984));
#312006=CARTESIAN_POINT('Ctrl Pts',(-4.27265099500006,5.2,0.474600012999984));
#312007=CARTESIAN_POINT('Ctrl Pts',(-4.27265099500006,2.2,0.474600012999984));
#312008=CARTESIAN_POINT('Ctrl Pts',(-4.27106218000006,12.2,0.473754269999986));
#312009=CARTESIAN_POINT('Ctrl Pts',(-4.27106218000006,5.2,0.473754269999986));
#312010=CARTESIAN_POINT('Ctrl Pts',(-4.27106218000006,2.2,0.473754269999986));
#312011=CARTESIAN_POINT('Ctrl Pts',(-4.26947622300006,12.2,0.472912353999986));
#312012=CARTESIAN_POINT('Ctrl Pts',(-4.26947622300006,5.2,0.472912353999986));
#312013=CARTESIAN_POINT('Ctrl Pts',(-4.26947622300006,2.2,0.472912353999986));
#312014=CARTESIAN_POINT('Ctrl Pts',(-4.26789313500006,12.2,0.472074260999986));
#312015=CARTESIAN_POINT('Ctrl Pts',(-4.26789313500006,5.2,0.472074260999986));
#312016=CARTESIAN_POINT('Ctrl Pts',(-4.26789313500006,2.2,0.472074260999986));
#312017=CARTESIAN_POINT('Ctrl Pts',(-4.26631292800006,12.2,0.471239985999983));
#312018=CARTESIAN_POINT('Ctrl Pts',(-4.26631292800006,5.2,0.471239985999983));
#312019=CARTESIAN_POINT('Ctrl Pts',(-4.26631292800006,2.2,0.471239985999983));
#312020=CARTESIAN_POINT('Ctrl Pts',(-4.26473561400006,12.2,0.470409523999984));
#312021=CARTESIAN_POINT('Ctrl Pts',(-4.26473561400006,5.2,0.470409523999984));
#312022=CARTESIAN_POINT('Ctrl Pts',(-4.26473561400006,2.2,0.470409523999984));
#312023=CARTESIAN_POINT('Ctrl Pts',(-4.26316120000005,12.2,0.469582871999985));
#312024=CARTESIAN_POINT('Ctrl Pts',(-4.26316120000005,5.2,0.469582871999985));
#312025=CARTESIAN_POINT('Ctrl Pts',(-4.26316120000005,2.2,0.469582871999985));
#312026=CARTESIAN_POINT('Ctrl Pts',(-4.26158970300006,12.2,0.468760025999986));
#312027=CARTESIAN_POINT('Ctrl Pts',(-4.26158970300006,5.2,0.468760025999986));
#312028=CARTESIAN_POINT('Ctrl Pts',(-4.26158970300006,2.2,0.468760025999986));
#312029=CARTESIAN_POINT('Ctrl Pts',(-4.26002112900006,12.2,0.467940980999986));
#312030=CARTESIAN_POINT('Ctrl Pts',(-4.26002112900006,5.2,0.467940980999986));
#312031=CARTESIAN_POINT('Ctrl Pts',(-4.26002112900006,2.2,0.467940980999986));
#312032=CARTESIAN_POINT('Ctrl Pts',(-4.25845549100006,12.2,0.467125732999989));
#312033=CARTESIAN_POINT('Ctrl Pts',(-4.25845549100006,5.2,0.467125732999989));
#312034=CARTESIAN_POINT('Ctrl Pts',(-4.25845549100006,2.2,0.467125732999989));
#312035=CARTESIAN_POINT('Ctrl Pts',(-4.25689280100006,12.2,0.466314275999986));
#312036=CARTESIAN_POINT('Ctrl Pts',(-4.25689280100006,5.2,0.466314275999986));
#312037=CARTESIAN_POINT('Ctrl Pts',(-4.25689280100006,2.2,0.466314275999986));
#312038=CARTESIAN_POINT('Ctrl Pts',(-4.25533306900006,12.2,0.465506608999986));
#312039=CARTESIAN_POINT('Ctrl Pts',(-4.25533306900006,5.2,0.465506608999986));
#312040=CARTESIAN_POINT('Ctrl Pts',(-4.25533306900006,2.2,0.465506608999986));
#312041=CARTESIAN_POINT('Ctrl Pts',(-4.25377630600006,12.2,0.464702724999988));
#312042=CARTESIAN_POINT('Ctrl Pts',(-4.25377630600006,5.2,0.464702724999988));
#312043=CARTESIAN_POINT('Ctrl Pts',(-4.25377630600006,2.2,0.464702724999988));
#312044=CARTESIAN_POINT('Ctrl Pts',(-4.25222252500006,12.2,0.463902618999987));
#312045=CARTESIAN_POINT('Ctrl Pts',(-4.25222252500006,5.2,0.463902618999987));
#312046=CARTESIAN_POINT('Ctrl Pts',(-4.25222252500006,2.2,0.463902618999987));
#312047=CARTESIAN_POINT('Ctrl Pts',(-4.25067173600006,12.2,0.463106288999988));
#312048=CARTESIAN_POINT('Ctrl Pts',(-4.25067173600006,5.2,0.463106288999988));
#312049=CARTESIAN_POINT('Ctrl Pts',(-4.25067173600006,2.2,0.463106288999988));
#312050=CARTESIAN_POINT('Ctrl Pts',(-4.24912394800006,12.2,0.462313728999986));
#312051=CARTESIAN_POINT('Ctrl Pts',(-4.24912394800006,5.2,0.462313728999986));
#312052=CARTESIAN_POINT('Ctrl Pts',(-4.24912394800006,2.2,0.462313728999986));
#312053=CARTESIAN_POINT('Ctrl Pts',(-4.24757917600005,12.2,0.461524934999984));
#312054=CARTESIAN_POINT('Ctrl Pts',(-4.24757917600005,5.2,0.461524934999984));
#312055=CARTESIAN_POINT('Ctrl Pts',(-4.24757917600005,2.2,0.461524934999984));
#312056=CARTESIAN_POINT('Ctrl Pts',(-4.24603742900006,12.2,0.460739901999982));
#312057=CARTESIAN_POINT('Ctrl Pts',(-4.24603742900006,5.2,0.460739901999982));
#312058=CARTESIAN_POINT('Ctrl Pts',(-4.24603742900006,2.2,0.460739901999982));
#312059=CARTESIAN_POINT('Ctrl Pts',(-4.24449871900006,12.2,0.459958625999985));
#312060=CARTESIAN_POINT('Ctrl Pts',(-4.24449871900006,5.2,0.459958625999985));
#312061=CARTESIAN_POINT('Ctrl Pts',(-4.24449871900006,2.2,0.459958625999985));
#312062=CARTESIAN_POINT('Ctrl Pts',(-4.24296305600006,12.2,0.459181101999988));
#312063=CARTESIAN_POINT('Ctrl Pts',(-4.24296305600006,5.2,0.459181101999988));
#312064=CARTESIAN_POINT('Ctrl Pts',(-4.24296305600006,2.2,0.459181101999988));
#312065=CARTESIAN_POINT('Ctrl Pts',(-4.24143045400006,12.2,0.458407324999985));
#312066=CARTESIAN_POINT('Ctrl Pts',(-4.24143045400006,5.2,0.458407324999985));
#312067=CARTESIAN_POINT('Ctrl Pts',(-4.24143045400006,2.2,0.458407324999985));
#312068=CARTESIAN_POINT('Ctrl Pts',(-4.23990092200006,12.2,0.457637290999986));
#312069=CARTESIAN_POINT('Ctrl Pts',(-4.23990092200006,5.2,0.457637290999986));
#312070=CARTESIAN_POINT('Ctrl Pts',(-4.23990092200006,2.2,0.457637290999986));
#312071=CARTESIAN_POINT('Ctrl Pts',(-4.23837447100006,12.2,0.456870996999985));
#312072=CARTESIAN_POINT('Ctrl Pts',(-4.23837447100006,5.2,0.456870996999985));
#312073=CARTESIAN_POINT('Ctrl Pts',(-4.23837447100006,2.2,0.456870996999985));
#312074=CARTESIAN_POINT('Ctrl Pts',(-4.23685111400006,12.2,0.456108434999987));
#312075=CARTESIAN_POINT('Ctrl Pts',(-4.23685111400006,5.2,0.456108434999987));
#312076=CARTESIAN_POINT('Ctrl Pts',(-4.23685111400006,2.2,0.456108434999987));
#312077=CARTESIAN_POINT('Ctrl Pts',(-4.23533086100006,12.2,0.455349602999986));
#312078=CARTESIAN_POINT('Ctrl Pts',(-4.23533086100006,5.2,0.455349602999986));
#312079=CARTESIAN_POINT('Ctrl Pts',(-4.23533086100006,2.2,0.455349602999986));
#312080=CARTESIAN_POINT('Ctrl Pts',(-4.23381372400006,12.2,0.454594492999987));
#312081=CARTESIAN_POINT('Ctrl Pts',(-4.23381372400006,5.2,0.454594492999987));
#312082=CARTESIAN_POINT('Ctrl Pts',(-4.23381372400006,2.2,0.454594492999987));
#312083=CARTESIAN_POINT('Ctrl Pts',(-4.23229971500006,12.2,0.453843104999985));
#312084=CARTESIAN_POINT('Ctrl Pts',(-4.23229971500006,5.2,0.453843104999985));
#312085=CARTESIAN_POINT('Ctrl Pts',(-4.23229971500006,2.2,0.453843104999985));
#312086=CARTESIAN_POINT('Ctrl Pts',(-4.23078884300006,12.2,0.453095430999984));
#312087=CARTESIAN_POINT('Ctrl Pts',(-4.23078884300006,5.2,0.453095430999984));
#312088=CARTESIAN_POINT('Ctrl Pts',(-4.23078884300006,2.2,0.453095430999984));
#312089=CARTESIAN_POINT('Ctrl Pts',(-4.22928112300006,12.2,0.452351465999987));
#312090=CARTESIAN_POINT('Ctrl Pts',(-4.22928112300006,5.2,0.452351465999987));
#312091=CARTESIAN_POINT('Ctrl Pts',(-4.22928112300006,2.2,0.452351465999987));
#312092=CARTESIAN_POINT('Ctrl Pts',(-4.22777656200005,12.2,0.451611206999987));
#312093=CARTESIAN_POINT('Ctrl Pts',(-4.22777656200005,5.2,0.451611206999987));
#312094=CARTESIAN_POINT('Ctrl Pts',(-4.22777656200005,2.2,0.451611206999987));
#312095=CARTESIAN_POINT('Ctrl Pts',(-4.22627517600006,12.2,0.450874648999986));
#312096=CARTESIAN_POINT('Ctrl Pts',(-4.22627517600006,5.2,0.450874648999986));
#312097=CARTESIAN_POINT('Ctrl Pts',(-4.22627517600006,2.2,0.450874648999986));
#312098=CARTESIAN_POINT('Ctrl Pts',(-4.22477697300006,12.2,0.450141784999989));
#312099=CARTESIAN_POINT('Ctrl Pts',(-4.22477697300006,5.2,0.450141784999989));
#312100=CARTESIAN_POINT('Ctrl Pts',(-4.22477697300006,2.2,0.450141784999989));
#312101=CARTESIAN_POINT('Ctrl Pts',(-4.22328196600006,12.2,0.449412612999982));
#312102=CARTESIAN_POINT('Ctrl Pts',(-4.22328196600006,5.2,0.449412612999982));
#312103=CARTESIAN_POINT('Ctrl Pts',(-4.22328196600006,2.2,0.449412612999982));
#312104=CARTESIAN_POINT('Ctrl Pts',(-4.22179016600006,12.2,0.448687124999987));
#312105=CARTESIAN_POINT('Ctrl Pts',(-4.22179016600006,5.2,0.448687124999987));
#312106=CARTESIAN_POINT('Ctrl Pts',(-4.22179016600006,2.2,0.448687124999987));
#312107=CARTESIAN_POINT('Ctrl Pts',(-4.22030158500006,12.2,0.447965318999985));
#312108=CARTESIAN_POINT('Ctrl Pts',(-4.22030158500006,5.2,0.447965318999985));
#312109=CARTESIAN_POINT('Ctrl Pts',(-4.22030158500006,2.2,0.447965318999985));
#312110=CARTESIAN_POINT('Ctrl Pts',(-4.21881623400005,12.2,0.447247188999986));
#312111=CARTESIAN_POINT('Ctrl Pts',(-4.21881623400005,5.2,0.447247188999986));
#312112=CARTESIAN_POINT('Ctrl Pts',(-4.21881623400005,2.2,0.447247188999986));
#312113=CARTESIAN_POINT('Ctrl Pts',(-4.21733412400005,12.2,0.446532728999984));
#312114=CARTESIAN_POINT('Ctrl Pts',(-4.21733412400005,5.2,0.446532728999984));
#312115=CARTESIAN_POINT('Ctrl Pts',(-4.21733412400005,2.2,0.446532728999984));
#312116=CARTESIAN_POINT('Ctrl Pts',(-4.21585526900006,12.2,0.445821935999984));
#312117=CARTESIAN_POINT('Ctrl Pts',(-4.21585526900006,5.2,0.445821935999984));
#312118=CARTESIAN_POINT('Ctrl Pts',(-4.21585526900006,2.2,0.445821935999984));
#312119=CARTESIAN_POINT('Ctrl Pts',(-4.21437967700006,12.2,0.445114802999989));
#312120=CARTESIAN_POINT('Ctrl Pts',(-4.21437967700006,5.2,0.445114802999989));
#312121=CARTESIAN_POINT('Ctrl Pts',(-4.21437967700006,2.2,0.445114802999989));
#312122=CARTESIAN_POINT('Ctrl Pts',(-4.21290736100006,12.2,0.444411324999985));
#312123=CARTESIAN_POINT('Ctrl Pts',(-4.21290736100006,5.2,0.444411324999985));
#312124=CARTESIAN_POINT('Ctrl Pts',(-4.21290736100006,2.2,0.444411324999985));
#312125=CARTESIAN_POINT('Ctrl Pts',(-4.21143833400006,12.2,0.443711497999986));
#312126=CARTESIAN_POINT('Ctrl Pts',(-4.21143833400006,5.2,0.443711497999986));
#312127=CARTESIAN_POINT('Ctrl Pts',(-4.21143833400006,2.2,0.443711497999986));
#312128=CARTESIAN_POINT('Ctrl Pts',(-4.20997260600006,12.2,0.443015316999986));
#312129=CARTESIAN_POINT('Ctrl Pts',(-4.20997260600006,5.2,0.443015316999986));
#312130=CARTESIAN_POINT('Ctrl Pts',(-4.20997260600006,2.2,0.443015316999986));
#312131=CARTESIAN_POINT('Ctrl Pts',(-4.20851018800006,12.2,0.442322775999986));
#312132=CARTESIAN_POINT('Ctrl Pts',(-4.20851018800006,5.2,0.442322775999986));
#312133=CARTESIAN_POINT('Ctrl Pts',(-4.20851018800006,2.2,0.442322775999986));
#312134=CARTESIAN_POINT('Ctrl Pts',(-4.20705109400005,12.2,0.441633870999985));
#312135=CARTESIAN_POINT('Ctrl Pts',(-4.20705109400005,5.2,0.441633870999985));
#312136=CARTESIAN_POINT('Ctrl Pts',(-4.20705109400005,2.2,0.441633870999985));
#312137=CARTESIAN_POINT('Ctrl Pts',(-4.20559533300006,12.2,0.440948595999986));
#312138=CARTESIAN_POINT('Ctrl Pts',(-4.20559533300006,5.2,0.440948595999986));
#312139=CARTESIAN_POINT('Ctrl Pts',(-4.20559533300006,2.2,0.440948595999986));
#312140=CARTESIAN_POINT('Ctrl Pts',(-4.20414291800006,12.2,0.440266945999985));
#312141=CARTESIAN_POINT('Ctrl Pts',(-4.20414291800006,5.2,0.440266945999985));
#312142=CARTESIAN_POINT('Ctrl Pts',(-4.20414291800006,2.2,0.440266945999985));
#312143=CARTESIAN_POINT('Ctrl Pts',(-4.20269386100006,12.2,0.439588913999986));
#312144=CARTESIAN_POINT('Ctrl Pts',(-4.20269386100006,5.2,0.439588913999986));
#312145=CARTESIAN_POINT('Ctrl Pts',(-4.20269386100006,2.2,0.439588913999986));
#312146=CARTESIAN_POINT('Ctrl Pts',(-4.20124817300006,12.2,0.438914497999985));
#312147=CARTESIAN_POINT('Ctrl Pts',(-4.20124817300006,5.2,0.438914497999985));
#312148=CARTESIAN_POINT('Ctrl Pts',(-4.20124817300006,2.2,0.438914497999985));
#312149=CARTESIAN_POINT('Ctrl Pts',(-4.19980586600006,12.2,0.438243690999984));
#312150=CARTESIAN_POINT('Ctrl Pts',(-4.19980586600006,5.2,0.438243690999984));
#312151=CARTESIAN_POINT('Ctrl Pts',(-4.19980586600006,2.2,0.438243690999984));
#312152=CARTESIAN_POINT('Ctrl Pts',(-4.19836695100006,12.2,0.437576486999984));
#312153=CARTESIAN_POINT('Ctrl Pts',(-4.19836695100006,5.2,0.437576486999984));
#312154=CARTESIAN_POINT('Ctrl Pts',(-4.19836695100006,2.2,0.437576486999984));
#312155=CARTESIAN_POINT('Ctrl Pts',(-4.19693144100005,12.2,0.436912881999985));
#312156=CARTESIAN_POINT('Ctrl Pts',(-4.19693144100005,5.2,0.436912881999985));
#312157=CARTESIAN_POINT('Ctrl Pts',(-4.19693144100005,2.2,0.436912881999985));
#312158=CARTESIAN_POINT('Ctrl Pts',(-4.19549934600006,12.2,0.436252869999985));
#312159=CARTESIAN_POINT('Ctrl Pts',(-4.19549934600006,5.2,0.436252869999985));
#312160=CARTESIAN_POINT('Ctrl Pts',(-4.19549934600006,2.2,0.436252869999985));
#312161=CARTESIAN_POINT('Ctrl Pts',(-4.19407068000006,12.2,0.435596445999984));
#312162=CARTESIAN_POINT('Ctrl Pts',(-4.19407068000006,5.2,0.435596445999984));
#312163=CARTESIAN_POINT('Ctrl Pts',(-4.19407068000006,2.2,0.435596445999984));
#312164=CARTESIAN_POINT('Ctrl Pts',(-4.19264545300006,12.2,0.434943603999987));
#312165=CARTESIAN_POINT('Ctrl Pts',(-4.19264545300006,5.2,0.434943603999987));
#312166=CARTESIAN_POINT('Ctrl Pts',(-4.19264545300006,2.2,0.434943603999987));
#312167=CARTESIAN_POINT('Ctrl Pts',(-4.19122367800006,12.2,0.434294338999983));
#312168=CARTESIAN_POINT('Ctrl Pts',(-4.19122367800006,5.2,0.434294338999983));
#312169=CARTESIAN_POINT('Ctrl Pts',(-4.19122367800006,2.2,0.434294338999983));
#312170=CARTESIAN_POINT('Ctrl Pts',(-4.18980536500006,12.2,0.433648644999987));
#312171=CARTESIAN_POINT('Ctrl Pts',(-4.18980536500006,5.2,0.433648644999987));
#312172=CARTESIAN_POINT('Ctrl Pts',(-4.18980536500006,2.2,0.433648644999987));
#312173=CARTESIAN_POINT('Ctrl Pts',(-4.18839052700006,12.2,0.433006516999987));
#312174=CARTESIAN_POINT('Ctrl Pts',(-4.18839052700006,5.2,0.433006516999987));
#312175=CARTESIAN_POINT('Ctrl Pts',(-4.18839052700006,2.2,0.433006516999987));
#312176=CARTESIAN_POINT('Ctrl Pts',(-4.18697917600006,12.2,0.432367948999985));
#312177=CARTESIAN_POINT('Ctrl Pts',(-4.18697917600006,5.2,0.432367948999985));
#312178=CARTESIAN_POINT('Ctrl Pts',(-4.18697917600006,2.2,0.432367948999985));
#312179=CARTESIAN_POINT('Ctrl Pts',(-4.18557132400006,12.2,0.431732936999989));
#312180=CARTESIAN_POINT('Ctrl Pts',(-4.18557132400006,5.2,0.431732936999989));
#312181=CARTESIAN_POINT('Ctrl Pts',(-4.18557132400006,2.2,0.431732936999989));
#312182=CARTESIAN_POINT('Ctrl Pts',(-4.18416698300006,12.2,0.431101472999984));
#312183=CARTESIAN_POINT('Ctrl Pts',(-4.18416698300006,5.2,0.431101472999984));
#312184=CARTESIAN_POINT('Ctrl Pts',(-4.18416698300006,2.2,0.431101472999984));
#312185=CARTESIAN_POINT('Ctrl Pts',(-4.18276616300005,12.2,0.430473553999988));
#312186=CARTESIAN_POINT('Ctrl Pts',(-4.18276616300005,5.2,0.430473553999988));
#312187=CARTESIAN_POINT('Ctrl Pts',(-4.18276616300005,2.2,0.430473553999988));
#312188=CARTESIAN_POINT('Ctrl Pts',(-4.18136887800006,12.2,0.429849171999983));
#312189=CARTESIAN_POINT('Ctrl Pts',(-4.18136887800006,5.2,0.429849171999983));
#312190=CARTESIAN_POINT('Ctrl Pts',(-4.18136887800006,2.2,0.429849171999983));
#312191=CARTESIAN_POINT('Ctrl Pts',(-4.17997513800006,12.2,0.429228321999986));
#312192=CARTESIAN_POINT('Ctrl Pts',(-4.17997513800006,5.2,0.429228321999986));
#312193=CARTESIAN_POINT('Ctrl Pts',(-4.17997513800006,2.2,0.429228321999986));
#312194=CARTESIAN_POINT('Ctrl Pts',(-4.17858495700006,12.2,0.428610999999983));
#312195=CARTESIAN_POINT('Ctrl Pts',(-4.17858495700006,5.2,0.428610999999983));
#312196=CARTESIAN_POINT('Ctrl Pts',(-4.17858495700006,2.2,0.428610999999983));
#312197=CARTESIAN_POINT('Ctrl Pts',(-4.17719834700006,12.2,0.427997197999983));
#312198=CARTESIAN_POINT('Ctrl Pts',(-4.17719834700006,5.2,0.427997197999983));
#312199=CARTESIAN_POINT('Ctrl Pts',(-4.17719834700006,2.2,0.427997197999983));
#312200=CARTESIAN_POINT('Ctrl Pts',(-4.17581531700006,12.2,0.427386910999985));
#312201=CARTESIAN_POINT('Ctrl Pts',(-4.17581531700006,5.2,0.427386910999985));
#312202=CARTESIAN_POINT('Ctrl Pts',(-4.17581531700006,2.2,0.427386910999985));
#312203=CARTESIAN_POINT('Ctrl Pts',(-4.17443588200006,12.2,0.426780132999984));
#312204=CARTESIAN_POINT('Ctrl Pts',(-4.17443588200006,5.2,0.426780132999984));
#312205=CARTESIAN_POINT('Ctrl Pts',(-4.17443588200006,2.2,0.426780132999984));
#312206=CARTESIAN_POINT('Ctrl Pts',(-4.17306005300006,12.2,0.426176860999985));
#312207=CARTESIAN_POINT('Ctrl Pts',(-4.17306005300006,5.2,0.426176860999985));
#312208=CARTESIAN_POINT('Ctrl Pts',(-4.17306005300006,2.2,0.426176860999985));
#312209=CARTESIAN_POINT('Ctrl Pts',(-4.17168784100006,12.2,0.425577084999986));
#312210=CARTESIAN_POINT('Ctrl Pts',(-4.17168784100006,5.2,0.425577084999986));
#312211=CARTESIAN_POINT('Ctrl Pts',(-4.17168784100006,2.2,0.425577084999986));
#312212=CARTESIAN_POINT('Ctrl Pts',(-4.17031926000006,12.2,0.424980800999983));
#312213=CARTESIAN_POINT('Ctrl Pts',(-4.17031926000006,5.2,0.424980800999983));
#312214=CARTESIAN_POINT('Ctrl Pts',(-4.17031926000006,2.2,0.424980800999983));
#312215=CARTESIAN_POINT('Ctrl Pts',(-4.16895432100006,12.2,0.424388002999985));
#312216=CARTESIAN_POINT('Ctrl Pts',(-4.16895432100006,5.2,0.424388002999985));
#312217=CARTESIAN_POINT('Ctrl Pts',(-4.16895432100006,2.2,0.424388002999985));
#312218=CARTESIAN_POINT('Ctrl Pts',(-4.16759303600006,12.2,0.423798685999985));
#312219=CARTESIAN_POINT('Ctrl Pts',(-4.16759303600006,5.2,0.423798685999985));
#312220=CARTESIAN_POINT('Ctrl Pts',(-4.16759303600006,2.2,0.423798685999985));
#312221=CARTESIAN_POINT('Ctrl Pts',(-4.16623541600006,12.2,0.423212842999985));
#312222=CARTESIAN_POINT('Ctrl Pts',(-4.16623541600006,5.2,0.423212842999985));
#312223=CARTESIAN_POINT('Ctrl Pts',(-4.16623541600006,2.2,0.423212842999985));
#312224=CARTESIAN_POINT('Ctrl Pts',(-4.16488147500006,12.2,0.422630467999987));
#312225=CARTESIAN_POINT('Ctrl Pts',(-4.16488147500006,5.2,0.422630467999987));
#312226=CARTESIAN_POINT('Ctrl Pts',(-4.16488147500006,2.2,0.422630467999987));
#312227=CARTESIAN_POINT('Ctrl Pts',(-4.16353122500006,12.2,0.422051554999987));
#312228=CARTESIAN_POINT('Ctrl Pts',(-4.16353122500006,5.2,0.422051554999987));
#312229=CARTESIAN_POINT('Ctrl Pts',(-4.16353122500006,2.2,0.422051554999987));
#312230=CARTESIAN_POINT('Ctrl Pts',(-4.16218467700006,12.2,0.421476099999989));
#312231=CARTESIAN_POINT('Ctrl Pts',(-4.16218467700006,5.2,0.421476099999989));
#312232=CARTESIAN_POINT('Ctrl Pts',(-4.16218467700006,2.2,0.421476099999989));
#312233=CARTESIAN_POINT('Ctrl Pts',(-4.16084184200006,12.2,0.420904093999983));
#312234=CARTESIAN_POINT('Ctrl Pts',(-4.16084184200006,5.2,0.420904093999983));
#312235=CARTESIAN_POINT('Ctrl Pts',(-4.16084184200006,2.2,0.420904093999983));
#312236=CARTESIAN_POINT('Ctrl Pts',(-4.15950273600005,12.2,0.420335532999987));
#312237=CARTESIAN_POINT('Ctrl Pts',(-4.15950273600005,5.2,0.420335532999987));
#312238=CARTESIAN_POINT('Ctrl Pts',(-4.15950273600005,2.2,0.420335532999987));
#312239=CARTESIAN_POINT('Ctrl Pts',(-4.15816736800006,12.2,0.419770408999987));
#312240=CARTESIAN_POINT('Ctrl Pts',(-4.15816736800006,5.2,0.419770408999987));
#312241=CARTESIAN_POINT('Ctrl Pts',(-4.15816736800006,2.2,0.419770408999987));
#312242=CARTESIAN_POINT('Ctrl Pts',(-4.15683575100006,12.2,0.419208716999986));
#312243=CARTESIAN_POINT('Ctrl Pts',(-4.15683575100006,5.2,0.419208716999986));
#312244=CARTESIAN_POINT('Ctrl Pts',(-4.15683575100006,2.2,0.419208716999986));
#312245=CARTESIAN_POINT('Ctrl Pts',(-4.15550789700006,12.2,0.418650450999984));
#312246=CARTESIAN_POINT('Ctrl Pts',(-4.15550789700006,5.2,0.418650450999984));
#312247=CARTESIAN_POINT('Ctrl Pts',(-4.15550789700006,2.2,0.418650450999984));
#312248=CARTESIAN_POINT('Ctrl Pts',(-4.15418381900006,12.2,0.418095605999986));
#312249=CARTESIAN_POINT('Ctrl Pts',(-4.15418381900006,5.2,0.418095605999986));
#312250=CARTESIAN_POINT('Ctrl Pts',(-4.15418381900006,2.2,0.418095605999986));
#312251=CARTESIAN_POINT('Ctrl Pts',(-4.15286352900006,12.2,0.417544172999986));
#312252=CARTESIAN_POINT('Ctrl Pts',(-4.15286352900006,5.2,0.417544172999986));
#312253=CARTESIAN_POINT('Ctrl Pts',(-4.15286352900006,2.2,0.417544172999986));
#312254=CARTESIAN_POINT('Ctrl Pts',(-4.15154703900006,12.2,0.416996146999988));
#312255=CARTESIAN_POINT('Ctrl Pts',(-4.15154703900006,5.2,0.416996146999988));
#312256=CARTESIAN_POINT('Ctrl Pts',(-4.15154703900006,2.2,0.416996146999988));
#312257=CARTESIAN_POINT('Ctrl Pts',(-4.15023436000006,12.2,0.416451522999988));
#312258=CARTESIAN_POINT('Ctrl Pts',(-4.15023436000006,5.2,0.416451522999988));
#312259=CARTESIAN_POINT('Ctrl Pts',(-4.15023436000006,2.2,0.416451522999988));
#312260=CARTESIAN_POINT('Ctrl Pts',(-4.14892550700006,12.2,0.415910292999988));
#312261=CARTESIAN_POINT('Ctrl Pts',(-4.14892550700006,5.2,0.415910292999988));
#312262=CARTESIAN_POINT('Ctrl Pts',(-4.14892550700006,2.2,0.415910292999988));
#312263=CARTESIAN_POINT('Ctrl Pts',(-4.14762049000006,12.2,0.415372450999989));
#312264=CARTESIAN_POINT('Ctrl Pts',(-4.14762049000006,5.2,0.415372450999989));
#312265=CARTESIAN_POINT('Ctrl Pts',(-4.14762049000006,2.2,0.415372450999989));
#312266=CARTESIAN_POINT('Ctrl Pts',(-4.14631932300006,12.2,0.414837989999985));
#312267=CARTESIAN_POINT('Ctrl Pts',(-4.14631932300006,5.2,0.414837989999985));
#312268=CARTESIAN_POINT('Ctrl Pts',(-4.14631932300006,2.2,0.414837989999985));
#312269=CARTESIAN_POINT('Ctrl Pts',(-4.14502201700006,12.2,0.414306905999986));
#312270=CARTESIAN_POINT('Ctrl Pts',(-4.14502201700006,5.2,0.414306905999986));
#312271=CARTESIAN_POINT('Ctrl Pts',(-4.14502201700006,2.2,0.414306905999986));
#312272=CARTESIAN_POINT('Ctrl Pts',(-4.14372858500006,12.2,0.413779189999985));
#312273=CARTESIAN_POINT('Ctrl Pts',(-4.14372858500006,5.2,0.413779189999985));
#312274=CARTESIAN_POINT('Ctrl Pts',(-4.14372858500006,2.2,0.413779189999985));
#312275=CARTESIAN_POINT('Ctrl Pts',(-4.14243904000006,12.2,0.413254837999983));
#312276=CARTESIAN_POINT('Ctrl Pts',(-4.14243904000006,5.2,0.413254837999983));
#312277=CARTESIAN_POINT('Ctrl Pts',(-4.14243904000006,2.2,0.413254837999983));
#312278=CARTESIAN_POINT('Ctrl Pts',(-4.14115339200006,12.2,0.412733840999984));
#312279=CARTESIAN_POINT('Ctrl Pts',(-4.14115339200006,5.2,0.412733840999984));
#312280=CARTESIAN_POINT('Ctrl Pts',(-4.14115339200006,2.2,0.412733840999984));
#312281=CARTESIAN_POINT('Ctrl Pts',(-4.13987165700005,12.2,0.412216192999986));
#312282=CARTESIAN_POINT('Ctrl Pts',(-4.13987165700005,5.2,0.412216192999986));
#312283=CARTESIAN_POINT('Ctrl Pts',(-4.13987165700005,2.2,0.412216192999986));
#312284=CARTESIAN_POINT('Ctrl Pts',(-4.13859384500006,12.2,0.411701888999985));
#312285=CARTESIAN_POINT('Ctrl Pts',(-4.13859384500006,5.2,0.411701888999985));
#312286=CARTESIAN_POINT('Ctrl Pts',(-4.13859384500006,2.2,0.411701888999985));
#312287=CARTESIAN_POINT('Ctrl Pts',(-4.13731996800006,12.2,0.411190921999989));
#312288=CARTESIAN_POINT('Ctrl Pts',(-4.13731996800006,5.2,0.411190921999989));
#312289=CARTESIAN_POINT('Ctrl Pts',(-4.13731996800006,2.2,0.411190921999989));
#312290=CARTESIAN_POINT('Ctrl Pts',(-4.13605004100006,12.2,0.410683283999984));
#312291=CARTESIAN_POINT('Ctrl Pts',(-4.13605004100006,5.2,0.410683283999984));
#312292=CARTESIAN_POINT('Ctrl Pts',(-4.13605004100006,2.2,0.410683283999984));
#312293=CARTESIAN_POINT('Ctrl Pts',(-4.13478407400006,12.2,0.410178968999984));
#312294=CARTESIAN_POINT('Ctrl Pts',(-4.13478407400006,5.2,0.410178968999984));
#312295=CARTESIAN_POINT('Ctrl Pts',(-4.13478407400006,2.2,0.410178968999984));
#312296=CARTESIAN_POINT('Ctrl Pts',(-4.13352208100005,12.2,0.409677971999987));
#312297=CARTESIAN_POINT('Ctrl Pts',(-4.13352208100005,5.2,0.409677971999987));
#312298=CARTESIAN_POINT('Ctrl Pts',(-4.13352208100005,2.2,0.409677971999987));
#312299=CARTESIAN_POINT('Ctrl Pts',(-4.13226407400006,12.2,0.409180282999984));
#312300=CARTESIAN_POINT('Ctrl Pts',(-4.13226407400006,5.2,0.409180282999984));
#312301=CARTESIAN_POINT('Ctrl Pts',(-4.13226407400006,2.2,0.409180282999984));
#312302=CARTESIAN_POINT('Ctrl Pts',(-4.13101006500006,12.2,0.408685896999987));
#312303=CARTESIAN_POINT('Ctrl Pts',(-4.13101006500006,5.2,0.408685896999987));
#312304=CARTESIAN_POINT('Ctrl Pts',(-4.13101006500006,2.2,0.408685896999987));
#312305=CARTESIAN_POINT('Ctrl Pts',(-4.12976006700006,12.2,0.408194807999984));
#312306=CARTESIAN_POINT('Ctrl Pts',(-4.12976006700006,5.2,0.408194807999984));
#312307=CARTESIAN_POINT('Ctrl Pts',(-4.12976006700006,2.2,0.408194807999984));
#312308=CARTESIAN_POINT('Ctrl Pts',(-4.12851409300006,12.2,0.407707009999987));
#312309=CARTESIAN_POINT('Ctrl Pts',(-4.12851409300006,5.2,0.407707009999987));
#312310=CARTESIAN_POINT('Ctrl Pts',(-4.12851409300006,2.2,0.407707009999987));
#312311=CARTESIAN_POINT('Ctrl Pts',(-4.12727215600006,12.2,0.407222493999986));
#312312=CARTESIAN_POINT('Ctrl Pts',(-4.12727215600006,5.2,0.407222493999986));
#312313=CARTESIAN_POINT('Ctrl Pts',(-4.12727215600006,2.2,0.407222493999986));
#312314=CARTESIAN_POINT('Ctrl Pts',(-4.12603426700006,12.2,0.406741251999985));
#312315=CARTESIAN_POINT('Ctrl Pts',(-4.12603426700006,5.2,0.406741251999985));
#312316=CARTESIAN_POINT('Ctrl Pts',(-4.12603426700006,2.2,0.406741251999985));
#312317=CARTESIAN_POINT('Ctrl Pts',(-4.12480043900006,12.2,0.406263280999983));
#312318=CARTESIAN_POINT('Ctrl Pts',(-4.12480043900006,5.2,0.406263280999983));
#312319=CARTESIAN_POINT('Ctrl Pts',(-4.12480043900006,2.2,0.406263280999983));
#312320=CARTESIAN_POINT('Ctrl Pts',(-4.12357068700006,12.2,0.405788570999985));
#312321=CARTESIAN_POINT('Ctrl Pts',(-4.12357068700006,5.2,0.405788570999985));
#312322=CARTESIAN_POINT('Ctrl Pts',(-4.12357068700006,2.2,0.405788570999985));
#312323=CARTESIAN_POINT('Ctrl Pts',(-4.12234502000006,12.2,0.405317116999986));
#312324=CARTESIAN_POINT('Ctrl Pts',(-4.12234502000006,5.2,0.405317116999986));
#312325=CARTESIAN_POINT('Ctrl Pts',(-4.12234502000006,2.2,0.405317116999986));
#312326=CARTESIAN_POINT('Ctrl Pts',(-4.12112345300006,12.2,0.404848910999984));
#312327=CARTESIAN_POINT('Ctrl Pts',(-4.12112345300006,5.2,0.404848910999984));
#312328=CARTESIAN_POINT('Ctrl Pts',(-4.12112345300006,2.2,0.404848910999984));
#312329=CARTESIAN_POINT('Ctrl Pts',(-4.11990599800006,12.2,0.404383944999989));
#312330=CARTESIAN_POINT('Ctrl Pts',(-4.11990599800006,5.2,0.404383944999989));
#312331=CARTESIAN_POINT('Ctrl Pts',(-4.11990599800006,2.2,0.404383944999989));
#312332=CARTESIAN_POINT('Ctrl Pts',(-4.11869266800006,12.2,0.403922214999985));
#312333=CARTESIAN_POINT('Ctrl Pts',(-4.11869266800006,5.2,0.403922214999985));
#312334=CARTESIAN_POINT('Ctrl Pts',(-4.11869266800006,2.2,0.403922214999985));
#312335=CARTESIAN_POINT('Ctrl Pts',(-4.11748347700006,12.2,0.403463710999983));
#312336=CARTESIAN_POINT('Ctrl Pts',(-4.11748347700006,5.2,0.403463710999983));
#312337=CARTESIAN_POINT('Ctrl Pts',(-4.11748347700006,2.2,0.403463710999983));
#312338=CARTESIAN_POINT('Ctrl Pts',(-4.11627843400006,12.2,0.403008425999989));
#312339=CARTESIAN_POINT('Ctrl Pts',(-4.11627843400006,5.2,0.403008425999989));
#312340=CARTESIAN_POINT('Ctrl Pts',(-4.11627843400006,2.2,0.403008425999989));
#312341=CARTESIAN_POINT('Ctrl Pts',(-4.11507755600006,12.2,0.402556355999986));
#312342=CARTESIAN_POINT('Ctrl Pts',(-4.11507755600006,5.2,0.402556355999986));
#312343=CARTESIAN_POINT('Ctrl Pts',(-4.11507755600006,2.2,0.402556355999986));
#312344=CARTESIAN_POINT('Ctrl Pts',(-4.11388085400006,12.2,0.402107488999985));
#312345=CARTESIAN_POINT('Ctrl Pts',(-4.11388085400006,5.2,0.402107488999985));
#312346=CARTESIAN_POINT('Ctrl Pts',(-4.11388085400006,2.2,0.402107488999985));
#312347=CARTESIAN_POINT('Ctrl Pts',(-4.11268834000006,12.2,0.401661821999983));
#312348=CARTESIAN_POINT('Ctrl Pts',(-4.11268834000006,5.2,0.401661821999983));
#312349=CARTESIAN_POINT('Ctrl Pts',(-4.11268834000006,2.2,0.401661821999983));
#312350=CARTESIAN_POINT('Ctrl Pts',(-4.11150002900006,12.2,0.401219345999984));
#312351=CARTESIAN_POINT('Ctrl Pts',(-4.11150002900006,5.2,0.401219345999984));
#312352=CARTESIAN_POINT('Ctrl Pts',(-4.11150002900006,2.2,0.401219345999984));
#312353=CARTESIAN_POINT('Ctrl Pts',(-4.11031593100006,12.2,0.400780052999985));
#312354=CARTESIAN_POINT('Ctrl Pts',(-4.11031593100006,5.2,0.400780052999985));
#312355=CARTESIAN_POINT('Ctrl Pts',(-4.11031593100006,2.2,0.400780052999985));
#312356=CARTESIAN_POINT('Ctrl Pts',(-4.10913606200006,12.2,0.400343936999987));
#312357=CARTESIAN_POINT('Ctrl Pts',(-4.10913606200006,5.2,0.400343936999987));
#312358=CARTESIAN_POINT('Ctrl Pts',(-4.10913606200006,2.2,0.400343936999987));
#312359=CARTESIAN_POINT('Ctrl Pts',(-4.10796043200006,12.2,0.399910990999985));
#312360=CARTESIAN_POINT('Ctrl Pts',(-4.10796043200006,5.2,0.399910990999985));
#312361=CARTESIAN_POINT('Ctrl Pts',(-4.10796043200006,2.2,0.399910990999985));
#312362=CARTESIAN_POINT('Ctrl Pts',(-4.10678905500006,12.2,0.399481205999983));
#312363=CARTESIAN_POINT('Ctrl Pts',(-4.10678905500006,5.2,0.399481205999983));
#312364=CARTESIAN_POINT('Ctrl Pts',(-4.10678905500006,2.2,0.399481205999983));
#312365=CARTESIAN_POINT('Ctrl Pts',(-4.10562194600006,12.2,0.399054574999984));
#312366=CARTESIAN_POINT('Ctrl Pts',(-4.10562194600006,5.2,0.399054574999984));
#312367=CARTESIAN_POINT('Ctrl Pts',(-4.10562194600006,2.2,0.399054574999984));
#312368=CARTESIAN_POINT('Ctrl Pts',(-4.10445911400006,12.2,0.398631090999988));
#312369=CARTESIAN_POINT('Ctrl Pts',(-4.10445911400006,5.2,0.398631090999988));
#312370=CARTESIAN_POINT('Ctrl Pts',(-4.10445911400006,2.2,0.398631090999988));
#312371=CARTESIAN_POINT('Ctrl Pts',(-4.10330057500006,12.2,0.398210746999985));
#312372=CARTESIAN_POINT('Ctrl Pts',(-4.10330057500006,5.2,0.398210746999985));
#312373=CARTESIAN_POINT('Ctrl Pts',(-4.10330057500006,2.2,0.398210746999985));
#312374=CARTESIAN_POINT('Ctrl Pts',(-4.10214634100006,12.2,0.397793535999984));
#312375=CARTESIAN_POINT('Ctrl Pts',(-4.10214634100006,5.2,0.397793535999984));
#312376=CARTESIAN_POINT('Ctrl Pts',(-4.10214634100006,2.2,0.397793535999984));
#312377=CARTESIAN_POINT('Ctrl Pts',(-4.10099642600006,12.2,0.397379447999988));
#312378=CARTESIAN_POINT('Ctrl Pts',(-4.10099642600006,5.2,0.397379447999988));
#312379=CARTESIAN_POINT('Ctrl Pts',(-4.10099642600006,2.2,0.397379447999988));
#312380=CARTESIAN_POINT('Ctrl Pts',(-4.09985084100006,12.2,0.396968477999984));
#312381=CARTESIAN_POINT('Ctrl Pts',(-4.09985084100006,5.2,0.396968477999984));
#312382=CARTESIAN_POINT('Ctrl Pts',(-4.09985084100006,2.2,0.396968477999984));
#312383=CARTESIAN_POINT('Ctrl Pts',(-4.09870960100006,12.2,0.396560615999988));
#312384=CARTESIAN_POINT('Ctrl Pts',(-4.09870960100006,5.2,0.396560615999988));
#312385=CARTESIAN_POINT('Ctrl Pts',(-4.09870960100006,2.2,0.396560615999988));
#312386=CARTESIAN_POINT('Ctrl Pts',(-4.09757271700006,12.2,0.396155855999982));
#312387=CARTESIAN_POINT('Ctrl Pts',(-4.09757271700006,5.2,0.396155855999982));
#312388=CARTESIAN_POINT('Ctrl Pts',(-4.09757271700006,2.2,0.396155855999982));
#312389=CARTESIAN_POINT('Ctrl Pts',(-4.09644020500005,12.2,0.395754189999984));
#312390=CARTESIAN_POINT('Ctrl Pts',(-4.09644020500005,5.2,0.395754189999984));
#312391=CARTESIAN_POINT('Ctrl Pts',(-4.09644020500005,2.2,0.395754189999984));
#312392=CARTESIAN_POINT('Ctrl Pts',(-4.09531207500006,12.2,0.395355609999988));
#312393=CARTESIAN_POINT('Ctrl Pts',(-4.09531207500006,5.2,0.395355609999988));
#312394=CARTESIAN_POINT('Ctrl Pts',(-4.09531207500006,2.2,0.395355609999988));
#312395=CARTESIAN_POINT('Ctrl Pts',(-4.09418834200006,12.2,0.394960108999989));
#312396=CARTESIAN_POINT('Ctrl Pts',(-4.09418834200006,5.2,0.394960108999989));
#312397=CARTESIAN_POINT('Ctrl Pts',(-4.09418834200006,2.2,0.394960108999989));
#312398=CARTESIAN_POINT('Ctrl Pts',(-4.09306901900006,12.2,0.394567677999986));
#312399=CARTESIAN_POINT('Ctrl Pts',(-4.09306901900006,5.2,0.394567677999986));
#312400=CARTESIAN_POINT('Ctrl Pts',(-4.09306901900006,2.2,0.394567677999986));
#312401=CARTESIAN_POINT('Ctrl Pts',(-4.09195411900006,12.2,0.394178310999984));
#312402=CARTESIAN_POINT('Ctrl Pts',(-4.09195411900006,5.2,0.394178310999984));
#312403=CARTESIAN_POINT('Ctrl Pts',(-4.09195411900006,2.2,0.394178310999984));
#312404=CARTESIAN_POINT('Ctrl Pts',(-4.09084365500005,12.2,0.393791997999986));
#312405=CARTESIAN_POINT('Ctrl Pts',(-4.09084365500005,5.2,0.393791997999986));
#312406=CARTESIAN_POINT('Ctrl Pts',(-4.09084365500005,2.2,0.393791997999986));
#312407=CARTESIAN_POINT('Ctrl Pts',(-4.08973764100006,12.2,0.393408731999987));
#312408=CARTESIAN_POINT('Ctrl Pts',(-4.08973764100006,5.2,0.393408731999987));
#312409=CARTESIAN_POINT('Ctrl Pts',(-4.08973764100006,2.2,0.393408731999987));
#312410=CARTESIAN_POINT('Ctrl Pts',(-4.08863608900006,12.2,0.393028504999986));
#312411=CARTESIAN_POINT('Ctrl Pts',(-4.08863608900006,5.2,0.393028504999986));
#312412=CARTESIAN_POINT('Ctrl Pts',(-4.08863608900006,2.2,0.393028504999986));
#312413=CARTESIAN_POINT('Ctrl Pts',(-4.08753901300006,12.2,0.392651309999987));
#312414=CARTESIAN_POINT('Ctrl Pts',(-4.08753901300006,5.2,0.392651309999987));
#312415=CARTESIAN_POINT('Ctrl Pts',(-4.08753901300006,2.2,0.392651309999987));
#312416=CARTESIAN_POINT('Ctrl Pts',(-4.08644642600006,12.2,0.392277137999986));
#312417=CARTESIAN_POINT('Ctrl Pts',(-4.08644642600006,5.2,0.392277137999986));
#312418=CARTESIAN_POINT('Ctrl Pts',(-4.08644642600006,2.2,0.392277137999986));
#312419=CARTESIAN_POINT('Ctrl Pts',(-4.08535834100006,12.2,0.391905980999985));
#312420=CARTESIAN_POINT('Ctrl Pts',(-4.08535834100006,5.2,0.391905980999985));
#312421=CARTESIAN_POINT('Ctrl Pts',(-4.08535834100006,2.2,0.391905980999985));
#312422=CARTESIAN_POINT('Ctrl Pts',(-4.08427477300005,12.2,0.391537830999984));
#312423=CARTESIAN_POINT('Ctrl Pts',(-4.08427477300005,5.2,0.391537830999984));
#312424=CARTESIAN_POINT('Ctrl Pts',(-4.08427477300005,2.2,0.391537830999984));
#312425=CARTESIAN_POINT('Ctrl Pts',(-4.08319573300005,12.2,0.391172679999983));
#312426=CARTESIAN_POINT('Ctrl Pts',(-4.08319573300005,5.2,0.391172679999983));
#312427=CARTESIAN_POINT('Ctrl Pts',(-4.08319573300005,2.2,0.391172679999983));
#312428=CARTESIAN_POINT('Ctrl Pts',(-4.08212123500006,12.2,0.390810519999985));
#312429=CARTESIAN_POINT('Ctrl Pts',(-4.08212123500006,5.2,0.390810519999985));
#312430=CARTESIAN_POINT('Ctrl Pts',(-4.08212123500006,2.2,0.390810519999985));
#312431=CARTESIAN_POINT('Ctrl Pts',(-4.08105129400006,12.2,0.390451341999984));
#312432=CARTESIAN_POINT('Ctrl Pts',(-4.08105129400006,5.2,0.390451341999984));
#312433=CARTESIAN_POINT('Ctrl Pts',(-4.08105129400006,2.2,0.390451341999984));
#312434=CARTESIAN_POINT('Ctrl Pts',(-4.07998592200006,12.2,0.390095138999986));
#312435=CARTESIAN_POINT('Ctrl Pts',(-4.07998592200006,5.2,0.390095138999986));
#312436=CARTESIAN_POINT('Ctrl Pts',(-4.07998592200006,2.2,0.390095138999986));
#312437=CARTESIAN_POINT('Ctrl Pts',(-4.07892513200006,12.2,0.389741902999985));
#312438=CARTESIAN_POINT('Ctrl Pts',(-4.07892513200006,5.2,0.389741902999985));
#312439=CARTESIAN_POINT('Ctrl Pts',(-4.07892513200006,2.2,0.389741902999985));
#312440=CARTESIAN_POINT('Ctrl Pts',(-4.07786893900006,12.2,0.389391623999984));
#312441=CARTESIAN_POINT('Ctrl Pts',(-4.07786893900006,5.2,0.389391623999984));
#312442=CARTESIAN_POINT('Ctrl Pts',(-4.07786893900006,2.2,0.389391623999984));
#312443=CARTESIAN_POINT('Ctrl Pts',(-4.07681735500006,12.2,0.389044293999987));
#312444=CARTESIAN_POINT('Ctrl Pts',(-4.07681735500006,5.2,0.389044293999987));
#312445=CARTESIAN_POINT('Ctrl Pts',(-4.07681735500006,2.2,0.389044293999987));
#312446=CARTESIAN_POINT('Ctrl Pts',(-4.07577039500006,12.2,0.388699906999985));
#312447=CARTESIAN_POINT('Ctrl Pts',(-4.07577039500006,5.2,0.388699906999985));
#312448=CARTESIAN_POINT('Ctrl Pts',(-4.07577039500006,2.2,0.388699906999985));
#312449=CARTESIAN_POINT('Ctrl Pts',(-4.07472807000006,12.2,0.388358450999986));
#312450=CARTESIAN_POINT('Ctrl Pts',(-4.07472807000006,5.2,0.388358450999986));
#312451=CARTESIAN_POINT('Ctrl Pts',(-4.07472807000006,2.2,0.388358450999986));
#312452=CARTESIAN_POINT('Ctrl Pts',(-4.07369039600006,12.2,0.388019919999985));
#312453=CARTESIAN_POINT('Ctrl Pts',(-4.07369039600006,5.2,0.388019919999985));
#312454=CARTESIAN_POINT('Ctrl Pts',(-4.07369039600006,2.2,0.388019919999985));
#312455=CARTESIAN_POINT('Ctrl Pts',(-4.07265738500006,12.2,0.387684304999985));
#312456=CARTESIAN_POINT('Ctrl Pts',(-4.07265738500006,5.2,0.387684304999985));
#312457=CARTESIAN_POINT('Ctrl Pts',(-4.07265738500006,2.2,0.387684304999985));
#312458=CARTESIAN_POINT('Ctrl Pts',(-4.07162905200006,12.2,0.387351596999985));
#312459=CARTESIAN_POINT('Ctrl Pts',(-4.07162905200006,5.2,0.387351596999985));
#312460=CARTESIAN_POINT('Ctrl Pts',(-4.07162905200006,2.2,0.387351596999985));
#312461=CARTESIAN_POINT('Ctrl Pts',(-4.07060541000006,12.2,0.387021788999986));
#312462=CARTESIAN_POINT('Ctrl Pts',(-4.07060541000006,5.2,0.387021788999986));
#312463=CARTESIAN_POINT('Ctrl Pts',(-4.07060541000006,2.2,0.387021788999986));
#312464=CARTESIAN_POINT('Ctrl Pts',(-4.06958647200006,12.2,0.386694868999986));
#312465=CARTESIAN_POINT('Ctrl Pts',(-4.06958647200006,5.2,0.386694868999986));
#312466=CARTESIAN_POINT('Ctrl Pts',(-4.06958647200006,2.2,0.386694868999986));
#312467=CARTESIAN_POINT('Ctrl Pts',(-4.06857225200006,12.2,0.386370831999985));
#312468=CARTESIAN_POINT('Ctrl Pts',(-4.06857225200006,5.2,0.386370831999985));
#312469=CARTESIAN_POINT('Ctrl Pts',(-4.06857225200006,2.2,0.386370831999985));
#312470=CARTESIAN_POINT('Ctrl Pts',(-4.06756276400006,12.2,0.386049667999986));
#312471=CARTESIAN_POINT('Ctrl Pts',(-4.06756276400006,5.2,0.386049667999986));
#312472=CARTESIAN_POINT('Ctrl Pts',(-4.06756276400006,2.2,0.386049667999986));
#312473=CARTESIAN_POINT('Ctrl Pts',(-4.06655802200006,12.2,0.385731367999984));
#312474=CARTESIAN_POINT('Ctrl Pts',(-4.06655802200006,5.2,0.385731367999984));
#312475=CARTESIAN_POINT('Ctrl Pts',(-4.06655802200006,2.2,0.385731367999984));
#312476=CARTESIAN_POINT('Ctrl Pts',(-4.06555803900006,12.2,0.385415922999983));
#312477=CARTESIAN_POINT('Ctrl Pts',(-4.06555803900006,5.2,0.385415922999983));
#312478=CARTESIAN_POINT('Ctrl Pts',(-4.06555803900006,2.2,0.385415922999983));
#312479=CARTESIAN_POINT('Ctrl Pts',(-4.06456282700006,12.2,0.385103324999987));
#312480=CARTESIAN_POINT('Ctrl Pts',(-4.06456282700006,5.2,0.385103324999987));
#312481=CARTESIAN_POINT('Ctrl Pts',(-4.06456282700006,2.2,0.385103324999987));
#312482=CARTESIAN_POINT('Ctrl Pts',(-4.06357240400006,12.2,0.384793563999986));
#312483=CARTESIAN_POINT('Ctrl Pts',(-4.06357240400006,5.2,0.384793563999986));
#312484=CARTESIAN_POINT('Ctrl Pts',(-4.06357240400006,2.2,0.384793563999986));
#312485=CARTESIAN_POINT('Ctrl Pts',(-4.06258678100006,12.2,0.384486632999987));
#312486=CARTESIAN_POINT('Ctrl Pts',(-4.06258678100006,5.2,0.384486632999987));
#312487=CARTESIAN_POINT('Ctrl Pts',(-4.06258678100006,2.2,0.384486632999987));
#312488=CARTESIAN_POINT('Ctrl Pts',(-4.06160597200006,12.2,0.384182521999987));
#312489=CARTESIAN_POINT('Ctrl Pts',(-4.06160597200006,5.2,0.384182521999987));
#312490=CARTESIAN_POINT('Ctrl Pts',(-4.06160597200006,2.2,0.384182521999987));
#312491=CARTESIAN_POINT('Ctrl Pts',(-4.06062999000006,12.2,0.383881221999989));
#312492=CARTESIAN_POINT('Ctrl Pts',(-4.06062999000006,5.2,0.383881221999989));
#312493=CARTESIAN_POINT('Ctrl Pts',(-4.06062999000006,2.2,0.383881221999989));
#312494=CARTESIAN_POINT('Ctrl Pts',(-4.05965885100006,12.2,0.383582722999982));
#312495=CARTESIAN_POINT('Ctrl Pts',(-4.05965885100006,5.2,0.383582722999982));
#312496=CARTESIAN_POINT('Ctrl Pts',(-4.05965885100006,2.2,0.383582722999982));
#312497=CARTESIAN_POINT('Ctrl Pts',(-4.05869256800006,12.2,0.383287017999985));
#312498=CARTESIAN_POINT('Ctrl Pts',(-4.05869256800006,5.2,0.383287017999985));
#312499=CARTESIAN_POINT('Ctrl Pts',(-4.05869256800006,2.2,0.383287017999985));
#312500=CARTESIAN_POINT('Ctrl Pts',(-4.05773115500006,12.2,0.382994097999987));
#312501=CARTESIAN_POINT('Ctrl Pts',(-4.05773115500006,5.2,0.382994097999987));
#312502=CARTESIAN_POINT('Ctrl Pts',(-4.05773115500006,2.2,0.382994097999987));
#312503=CARTESIAN_POINT('Ctrl Pts',(-4.05677462400006,12.2,0.382703950999983));
#312504=CARTESIAN_POINT('Ctrl Pts',(-4.05677462400006,5.2,0.382703950999983));
#312505=CARTESIAN_POINT('Ctrl Pts',(-4.05677462400006,2.2,0.382703950999983));
#312506=CARTESIAN_POINT('Ctrl Pts',(-4.05582299200006,12.2,0.382416571999986));
#312507=CARTESIAN_POINT('Ctrl Pts',(-4.05582299200006,5.2,0.382416571999986));
#312508=CARTESIAN_POINT('Ctrl Pts',(-4.05582299200006,2.2,0.382416571999986));
#312509=CARTESIAN_POINT('Ctrl Pts',(-4.05487627100006,12.2,0.382131946999986));
#312510=CARTESIAN_POINT('Ctrl Pts',(-4.05487627100006,5.2,0.382131946999986));
#312511=CARTESIAN_POINT('Ctrl Pts',(-4.05487627100006,2.2,0.382131946999986));
#312512=CARTESIAN_POINT('Ctrl Pts',(-4.05393447600006,12.2,0.381850070999987));
#312513=CARTESIAN_POINT('Ctrl Pts',(-4.05393447600006,5.2,0.381850070999987));
#312514=CARTESIAN_POINT('Ctrl Pts',(-4.05393447600006,2.2,0.381850070999987));
#312515=CARTESIAN_POINT('Ctrl Pts',(-4.05299762000006,12.2,0.381570932999988));
#312516=CARTESIAN_POINT('Ctrl Pts',(-4.05299762000006,5.2,0.381570932999988));
#312517=CARTESIAN_POINT('Ctrl Pts',(-4.05299762000006,2.2,0.381570932999988));
#312518=CARTESIAN_POINT('Ctrl Pts',(-4.05206571700006,12.2,0.381294522999984));
#312519=CARTESIAN_POINT('Ctrl Pts',(-4.05206571700006,5.2,0.381294522999984));
#312520=CARTESIAN_POINT('Ctrl Pts',(-4.05206571700006,2.2,0.381294522999984));
#312521=CARTESIAN_POINT('Ctrl Pts',(-4.05113878300006,12.2,0.381020832999983));
#312522=CARTESIAN_POINT('Ctrl Pts',(-4.05113878300006,5.2,0.381020832999983));
#312523=CARTESIAN_POINT('Ctrl Pts',(-4.05113878300006,2.2,0.381020832999983));
#312524=CARTESIAN_POINT('Ctrl Pts',(-4.05021682900006,12.2,0.380749852999984));
#312525=CARTESIAN_POINT('Ctrl Pts',(-4.05021682900006,5.2,0.380749852999984));
#312526=CARTESIAN_POINT('Ctrl Pts',(-4.05021682900006,2.2,0.380749852999984));
#312527=CARTESIAN_POINT('Ctrl Pts',(-4.04929987300005,12.2,0.380481572999987));
#312528=CARTESIAN_POINT('Ctrl Pts',(-4.04929987300005,5.2,0.380481572999987));
#312529=CARTESIAN_POINT('Ctrl Pts',(-4.04929987300005,2.2,0.380481572999987));
#312530=CARTESIAN_POINT('Ctrl Pts',(-4.04838792500006,12.2,0.380215984999985));
#312531=CARTESIAN_POINT('Ctrl Pts',(-4.04838792500006,5.2,0.380215984999985));
#312532=CARTESIAN_POINT('Ctrl Pts',(-4.04838792500006,2.2,0.380215984999985));
#312533=CARTESIAN_POINT('Ctrl Pts',(-4.04748100300006,12.2,0.379953076999984));
#312534=CARTESIAN_POINT('Ctrl Pts',(-4.04748100300006,5.2,0.379953076999984));
#312535=CARTESIAN_POINT('Ctrl Pts',(-4.04748100300006,2.2,0.379953076999984));
#312536=CARTESIAN_POINT('Ctrl Pts',(-4.04657911800006,12.2,0.379692842999986));
#312537=CARTESIAN_POINT('Ctrl Pts',(-4.04657911800006,5.2,0.379692842999986));
#312538=CARTESIAN_POINT('Ctrl Pts',(-4.04657911800006,2.2,0.379692842999986));
#312539=CARTESIAN_POINT('Ctrl Pts',(-4.04568228500006,12.2,0.379435269999986));
#312540=CARTESIAN_POINT('Ctrl Pts',(-4.04568228500006,5.2,0.379435269999986));
#312541=CARTESIAN_POINT('Ctrl Pts',(-4.04568228500006,2.2,0.379435269999986));
#312542=CARTESIAN_POINT('Ctrl Pts',(-4.04479052000006,12.2,0.379180349999988));
#312543=CARTESIAN_POINT('Ctrl Pts',(-4.04479052000006,5.2,0.379180349999988));
#312544=CARTESIAN_POINT('Ctrl Pts',(-4.04479052000006,2.2,0.379180349999988));
#312545=CARTESIAN_POINT('Ctrl Pts',(-4.04390383500006,12.2,0.378928072999987));
#312546=CARTESIAN_POINT('Ctrl Pts',(-4.04390383500006,5.2,0.378928072999987));
#312547=CARTESIAN_POINT('Ctrl Pts',(-4.04390383500006,2.2,0.378928072999987));
#312548=CARTESIAN_POINT('Ctrl Pts',(-4.04302224600006,12.2,0.378678429999986));
#312549=CARTESIAN_POINT('Ctrl Pts',(-4.04302224600006,5.2,0.378678429999986));
#312550=CARTESIAN_POINT('Ctrl Pts',(-4.04302224600006,2.2,0.378678429999986));
#312551=CARTESIAN_POINT('Ctrl Pts',(-4.04214576600006,12.2,0.378431409999984));
#312552=CARTESIAN_POINT('Ctrl Pts',(-4.04214576600006,5.2,0.378431409999984));
#312553=CARTESIAN_POINT('Ctrl Pts',(-4.04214576600006,2.2,0.378431409999984));
#312554=CARTESIAN_POINT('Ctrl Pts',(-4.04127441000006,12.2,0.378187003999986));
#312555=CARTESIAN_POINT('Ctrl Pts',(-4.04127441000006,5.2,0.378187003999986));
#312556=CARTESIAN_POINT('Ctrl Pts',(-4.04127441000006,2.2,0.378187003999986));
#312557=CARTESIAN_POINT('Ctrl Pts',(-4.04040819200006,12.2,0.377945200999985));
#312558=CARTESIAN_POINT('Ctrl Pts',(-4.04040819200006,5.2,0.377945200999985));
#312559=CARTESIAN_POINT('Ctrl Pts',(-4.04040819200006,2.2,0.377945200999985));
#312560=CARTESIAN_POINT('Ctrl Pts',(-4.03954712700005,12.2,0.377705992999986));
#312561=CARTESIAN_POINT('Ctrl Pts',(-4.03954712700005,5.2,0.377705992999986));
#312562=CARTESIAN_POINT('Ctrl Pts',(-4.03954712700005,2.2,0.377705992999986));
#312563=CARTESIAN_POINT('Ctrl Pts',(-4.03869122900006,12.2,0.377469368999983));
#312564=CARTESIAN_POINT('Ctrl Pts',(-4.03869122900006,5.2,0.377469368999983));
#312565=CARTESIAN_POINT('Ctrl Pts',(-4.03869122900006,2.2,0.377469368999983));
#312566=CARTESIAN_POINT('Ctrl Pts',(-4.03784051300006,12.2,0.377235317999984));
#312567=CARTESIAN_POINT('Ctrl Pts',(-4.03784051300006,5.2,0.377235317999984));
#312568=CARTESIAN_POINT('Ctrl Pts',(-4.03784051300006,2.2,0.377235317999984));
#312569=CARTESIAN_POINT('Ctrl Pts',(-4.03699499200005,12.2,0.377003831999985));
#312570=CARTESIAN_POINT('Ctrl Pts',(-4.03699499200005,5.2,0.377003831999985));
#312571=CARTESIAN_POINT('Ctrl Pts',(-4.03699499200005,2.2,0.377003831999985));
#312572=CARTESIAN_POINT('Ctrl Pts',(-4.03615468200006,12.2,0.376774897999983));
#312573=CARTESIAN_POINT('Ctrl Pts',(-4.03615468200006,5.2,0.376774897999983));
#312574=CARTESIAN_POINT('Ctrl Pts',(-4.03615468200006,2.2,0.376774897999983));
#312575=CARTESIAN_POINT('Ctrl Pts',(-4.03531959600006,12.2,0.376548508999988));
#312576=CARTESIAN_POINT('Ctrl Pts',(-4.03531959600006,5.2,0.376548508999988));
#312577=CARTESIAN_POINT('Ctrl Pts',(-4.03531959600006,2.2,0.376548508999988));
#312578=CARTESIAN_POINT('Ctrl Pts',(-4.03448975200006,12.2,0.376324653999984));
#312579=CARTESIAN_POINT('Ctrl Pts',(-4.03448975200006,5.2,0.376324653999984));
#312580=CARTESIAN_POINT('Ctrl Pts',(-4.03448975200006,2.2,0.376324653999984));
#312581=CARTESIAN_POINT('Ctrl Pts',(-4.03366516000006,12.2,0.376103321999985));
#312582=CARTESIAN_POINT('Ctrl Pts',(-4.03366516000006,5.2,0.376103321999985));
#312583=CARTESIAN_POINT('Ctrl Pts',(-4.03366516000006,2.2,0.376103321999985));
#312584=CARTESIAN_POINT('Ctrl Pts',(-4.03284583700006,12.2,0.375884502999986));
#312585=CARTESIAN_POINT('Ctrl Pts',(-4.03284583700006,5.2,0.375884502999986));
#312586=CARTESIAN_POINT('Ctrl Pts',(-4.03284583700006,2.2,0.375884502999986));
#312587=CARTESIAN_POINT('Ctrl Pts',(-4.03203179700006,12.2,0.375668185999984));
#312588=CARTESIAN_POINT('Ctrl Pts',(-4.03203179700006,5.2,0.375668185999984));
#312589=CARTESIAN_POINT('Ctrl Pts',(-4.03203179700006,2.2,0.375668185999984));
#312590=CARTESIAN_POINT('Ctrl Pts',(-4.03122305500006,12.2,0.375454361999985));
#312591=CARTESIAN_POINT('Ctrl Pts',(-4.03122305500006,5.2,0.375454361999985));
#312592=CARTESIAN_POINT('Ctrl Pts',(-4.03122305500006,2.2,0.375454361999985));
#312593=CARTESIAN_POINT('Ctrl Pts',(-4.03041962500006,12.2,0.375243019999987));
#312594=CARTESIAN_POINT('Ctrl Pts',(-4.03041962500006,5.2,0.375243019999987));
#312595=CARTESIAN_POINT('Ctrl Pts',(-4.03041962500006,2.2,0.375243019999987));
#312596=CARTESIAN_POINT('Ctrl Pts',(-4.02962152400006,12.2,0.375034148999984));
#312597=CARTESIAN_POINT('Ctrl Pts',(-4.02962152400006,5.2,0.375034148999984));
#312598=CARTESIAN_POINT('Ctrl Pts',(-4.02962152400006,2.2,0.375034148999984));
#312599=CARTESIAN_POINT('Ctrl Pts',(-4.02882876300006,12.2,0.374827739999986));
#312600=CARTESIAN_POINT('Ctrl Pts',(-4.02882876300006,5.2,0.374827739999986));
#312601=CARTESIAN_POINT('Ctrl Pts',(-4.02882876300006,2.2,0.374827739999986));
#312602=CARTESIAN_POINT('Ctrl Pts',(-4.02804136000006,12.2,0.374623780999985));
#312603=CARTESIAN_POINT('Ctrl Pts',(-4.02804136000006,5.2,0.374623780999985));
#312604=CARTESIAN_POINT('Ctrl Pts',(-4.02804136000006,2.2,0.374623780999985));
#312605=CARTESIAN_POINT('Ctrl Pts',(-4.02725932800006,12.2,0.374422260999987));
#312606=CARTESIAN_POINT('Ctrl Pts',(-4.02725932800006,5.2,0.374422260999987));
#312607=CARTESIAN_POINT('Ctrl Pts',(-4.02725932800006,2.2,0.374422260999987));
#312608=CARTESIAN_POINT('Ctrl Pts',(-4.02648268300006,12.2,0.374223170999985));
#312609=CARTESIAN_POINT('Ctrl Pts',(-4.02648268300006,5.2,0.374223170999985));
#312610=CARTESIAN_POINT('Ctrl Pts',(-4.02648268300006,2.2,0.374223170999985));
#312611=CARTESIAN_POINT('Ctrl Pts',(-4.02571143800006,12.2,0.374026498999989));
#312612=CARTESIAN_POINT('Ctrl Pts',(-4.02571143800006,5.2,0.374026498999989));
#312613=CARTESIAN_POINT('Ctrl Pts',(-4.02571143800006,2.2,0.374026498999989));
#312614=CARTESIAN_POINT('Ctrl Pts',(-4.02494561000006,12.2,0.373832234999987));
#312615=CARTESIAN_POINT('Ctrl Pts',(-4.02494561000006,5.2,0.373832234999987));
#312616=CARTESIAN_POINT('Ctrl Pts',(-4.02494561000006,2.2,0.373832234999987));
#312617=CARTESIAN_POINT('Ctrl Pts',(-4.02418521200006,12.2,0.373640367999983));
#312618=CARTESIAN_POINT('Ctrl Pts',(-4.02418521200006,5.2,0.373640367999983));
#312619=CARTESIAN_POINT('Ctrl Pts',(-4.02418521200006,2.2,0.373640367999983));
#312620=CARTESIAN_POINT('Ctrl Pts',(-4.02343026100006,12.2,0.373450886999986));
#312621=CARTESIAN_POINT('Ctrl Pts',(-4.02343026100006,5.2,0.373450886999986));
#312622=CARTESIAN_POINT('Ctrl Pts',(-4.02343026100006,2.2,0.373450886999986));
#312623=CARTESIAN_POINT('Ctrl Pts',(-4.02268076900006,12.2,0.373263781999986));
#312624=CARTESIAN_POINT('Ctrl Pts',(-4.02268076900006,5.2,0.373263781999986));
#312625=CARTESIAN_POINT('Ctrl Pts',(-4.02268076900006,2.2,0.373263781999986));
#312626=CARTESIAN_POINT('Ctrl Pts',(-4.02193675400006,12.2,0.373079040999986));
#312627=CARTESIAN_POINT('Ctrl Pts',(-4.02193675400006,5.2,0.373079040999986));
#312628=CARTESIAN_POINT('Ctrl Pts',(-4.02193675400006,2.2,0.373079040999986));
#312629=CARTESIAN_POINT('Ctrl Pts',(-4.02119822900006,12.2,0.372896652999986));
#312630=CARTESIAN_POINT('Ctrl Pts',(-4.02119822900006,5.2,0.372896652999986));
#312631=CARTESIAN_POINT('Ctrl Pts',(-4.02119822900006,2.2,0.372896652999986));
#312632=CARTESIAN_POINT('Ctrl Pts',(-4.02046521100006,12.2,0.372716607999983));
#312633=CARTESIAN_POINT('Ctrl Pts',(-4.02046521100006,5.2,0.372716607999983));
#312634=CARTESIAN_POINT('Ctrl Pts',(-4.02046521100006,2.2,0.372716607999983));
#312635=CARTESIAN_POINT('Ctrl Pts',(-4.01973771200006,12.2,0.372538892999987));
#312636=CARTESIAN_POINT('Ctrl Pts',(-4.01973771200006,5.2,0.372538892999987));
#312637=CARTESIAN_POINT('Ctrl Pts',(-4.01973771200006,2.2,0.372538892999987));
#312638=CARTESIAN_POINT('Ctrl Pts',(-4.01901575000006,12.2,0.372363498999988));
#312639=CARTESIAN_POINT('Ctrl Pts',(-4.01901575000006,5.2,0.372363498999988));
#312640=CARTESIAN_POINT('Ctrl Pts',(-4.01901575000006,2.2,0.372363498999988));
#312641=CARTESIAN_POINT('Ctrl Pts',(-4.01829934000006,12.2,0.372190413999984));
#312642=CARTESIAN_POINT('Ctrl Pts',(-4.01829934000006,5.2,0.372190413999984));
#312643=CARTESIAN_POINT('Ctrl Pts',(-4.01829934000006,2.2,0.372190413999984));
#312644=CARTESIAN_POINT('Ctrl Pts',(-4.01758849500006,12.2,0.372019625999984));
#312645=CARTESIAN_POINT('Ctrl Pts',(-4.01758849500006,5.2,0.372019625999984));
#312646=CARTESIAN_POINT('Ctrl Pts',(-4.01758849500006,2.2,0.372019625999984));
#312647=CARTESIAN_POINT('Ctrl Pts',(-4.01688323100006,12.2,0.371851124999987));
#312648=CARTESIAN_POINT('Ctrl Pts',(-4.01688323100006,5.2,0.371851124999987));
#312649=CARTESIAN_POINT('Ctrl Pts',(-4.01688323100006,2.2,0.371851124999987));
#312650=CARTESIAN_POINT('Ctrl Pts',(-4.01618356400006,12.2,0.371684899999987));
#312651=CARTESIAN_POINT('Ctrl Pts',(-4.01618356400006,5.2,0.371684899999987));
#312652=CARTESIAN_POINT('Ctrl Pts',(-4.01618356400006,2.2,0.371684899999987));
#312653=CARTESIAN_POINT('Ctrl Pts',(-4.01548950900006,12.2,0.371520936999987));
#312654=CARTESIAN_POINT('Ctrl Pts',(-4.01548950900006,5.2,0.371520936999987));
#312655=CARTESIAN_POINT('Ctrl Pts',(-4.01548950900006,2.2,0.371520936999987));
#312656=CARTESIAN_POINT('Ctrl Pts',(-4.01480108000006,12.2,0.371359226999988));
#312657=CARTESIAN_POINT('Ctrl Pts',(-4.01480108000006,5.2,0.371359226999988));
#312658=CARTESIAN_POINT('Ctrl Pts',(-4.01480108000006,2.2,0.371359226999988));
#312659=CARTESIAN_POINT('Ctrl Pts',(-4.01411829500006,12.2,0.371199757999987));
#312660=CARTESIAN_POINT('Ctrl Pts',(-4.01411829500006,5.2,0.371199757999987));
#312661=CARTESIAN_POINT('Ctrl Pts',(-4.01411829500006,2.2,0.371199757999987));
#312662=CARTESIAN_POINT('Ctrl Pts',(-4.01344116600006,12.2,0.371042516999989));
#312663=CARTESIAN_POINT('Ctrl Pts',(-4.01344116600006,5.2,0.371042516999989));
#312664=CARTESIAN_POINT('Ctrl Pts',(-4.01344116600006,2.2,0.371042516999989));
#312665=CARTESIAN_POINT('Ctrl Pts',(-4.01276971100006,12.2,0.370887495999987));
#312666=CARTESIAN_POINT('Ctrl Pts',(-4.01276971100006,5.2,0.370887495999987));
#312667=CARTESIAN_POINT('Ctrl Pts',(-4.01276971100006,2.2,0.370887495999987));
#312668=CARTESIAN_POINT('Ctrl Pts',(-4.01210394400006,12.2,0.370734678999987));
#312669=CARTESIAN_POINT('Ctrl Pts',(-4.01210394400006,5.2,0.370734678999987));
#312670=CARTESIAN_POINT('Ctrl Pts',(-4.01210394400006,2.2,0.370734678999987));
#312671=CARTESIAN_POINT('Ctrl Pts',(-4.01144388100006,12.2,0.370584057999985));
#312672=CARTESIAN_POINT('Ctrl Pts',(-4.01144388100006,5.2,0.370584057999985));
#312673=CARTESIAN_POINT('Ctrl Pts',(-4.01144388100006,2.2,0.370584057999985));
#312674=CARTESIAN_POINT('Ctrl Pts',(-4.01078953700006,12.2,0.370435617999987));
#312675=CARTESIAN_POINT('Ctrl Pts',(-4.01078953700006,5.2,0.370435617999987));
#312676=CARTESIAN_POINT('Ctrl Pts',(-4.01078953700006,2.2,0.370435617999987));
#312677=CARTESIAN_POINT('Ctrl Pts',(-4.01014092700006,12.2,0.370289349999986));
#312678=CARTESIAN_POINT('Ctrl Pts',(-4.01014092700006,5.2,0.370289349999986));
#312679=CARTESIAN_POINT('Ctrl Pts',(-4.01014092700006,2.2,0.370289349999986));
#312680=CARTESIAN_POINT('Ctrl Pts',(-4.00949806800006,12.2,0.370145240999986));
#312681=CARTESIAN_POINT('Ctrl Pts',(-4.00949806800006,5.2,0.370145240999986));
#312682=CARTESIAN_POINT('Ctrl Pts',(-4.00949806800006,2.2,0.370145240999986));
#312683=CARTESIAN_POINT('Ctrl Pts',(-4.00886097400006,12.2,0.370003277999986));
#312684=CARTESIAN_POINT('Ctrl Pts',(-4.00886097400006,5.2,0.370003277999986));
#312685=CARTESIAN_POINT('Ctrl Pts',(-4.00886097400006,2.2,0.370003277999986));
#312686=CARTESIAN_POINT('Ctrl Pts',(-4.00822966300006,12.2,0.369863450999985));
#312687=CARTESIAN_POINT('Ctrl Pts',(-4.00822966300006,5.2,0.369863450999985));
#312688=CARTESIAN_POINT('Ctrl Pts',(-4.00822966300006,2.2,0.369863450999985));
#312689=CARTESIAN_POINT('Ctrl Pts',(-4.00760414700006,12.2,0.369725746999983));
#312690=CARTESIAN_POINT('Ctrl Pts',(-4.00760414700006,5.2,0.369725746999983));
#312691=CARTESIAN_POINT('Ctrl Pts',(-4.00760414700006,2.2,0.369725746999983));
#312692=CARTESIAN_POINT('Ctrl Pts',(-4.00698444500006,12.2,0.369590153999986));
#312693=CARTESIAN_POINT('Ctrl Pts',(-4.00698444500006,5.2,0.369590153999986));
#312694=CARTESIAN_POINT('Ctrl Pts',(-4.00698444500006,2.2,0.369590153999986));
#312695=CARTESIAN_POINT('Ctrl Pts',(-4.00637057000006,12.2,0.369456659999985));
#312696=CARTESIAN_POINT('Ctrl Pts',(-4.00637057000006,5.2,0.369456659999985));
#312697=CARTESIAN_POINT('Ctrl Pts',(-4.00637057000006,2.2,0.369456659999985));
#312698=CARTESIAN_POINT('Ctrl Pts',(-4.00576253900006,12.2,0.369325252999988));
#312699=CARTESIAN_POINT('Ctrl Pts',(-4.00576253900006,5.2,0.369325252999988));
#312700=CARTESIAN_POINT('Ctrl Pts',(-4.00576253900006,2.2,0.369325252999988));
#312701=CARTESIAN_POINT('Ctrl Pts',(-4.00516036900005,12.2,0.369195918999985));
#312702=CARTESIAN_POINT('Ctrl Pts',(-4.00516036900005,5.2,0.369195918999985));
#312703=CARTESIAN_POINT('Ctrl Pts',(-4.00516036900005,2.2,0.369195918999985));
#312704=CARTESIAN_POINT('Ctrl Pts',(-4.00456407300006,12.2,0.369068647999988));
#312705=CARTESIAN_POINT('Ctrl Pts',(-4.00456407300006,5.2,0.369068647999988));
#312706=CARTESIAN_POINT('Ctrl Pts',(-4.00456407300006,2.2,0.369068647999988));
#312707=CARTESIAN_POINT('Ctrl Pts',(-4.00397366800005,12.2,0.368943427999984));
#312708=CARTESIAN_POINT('Ctrl Pts',(-4.00397366800005,5.2,0.368943427999984));
#312709=CARTESIAN_POINT('Ctrl Pts',(-4.00397366800005,2.2,0.368943427999984));
#312710=CARTESIAN_POINT('Ctrl Pts',(-4.00338917100005,12.2,0.368820244999988));
#312711=CARTESIAN_POINT('Ctrl Pts',(-4.00338917100005,5.2,0.368820244999988));
#312712=CARTESIAN_POINT('Ctrl Pts',(-4.00338917100005,2.2,0.368820244999988));
#312713=CARTESIAN_POINT('Ctrl Pts',(-4.00281059600006,12.2,0.368699085999986));
#312714=CARTESIAN_POINT('Ctrl Pts',(-4.00281059600006,5.2,0.368699085999986));
#312715=CARTESIAN_POINT('Ctrl Pts',(-4.00281059600006,2.2,0.368699085999986));
#312716=CARTESIAN_POINT('Ctrl Pts',(-4.00223796000006,12.2,0.368579940999982));
#312717=CARTESIAN_POINT('Ctrl Pts',(-4.00223796000006,5.2,0.368579940999982));
#312718=CARTESIAN_POINT('Ctrl Pts',(-4.00223796000006,2.2,0.368579940999982));
#312719=CARTESIAN_POINT('Ctrl Pts',(-4.00167127800006,12.2,0.368462794999989));
#312720=CARTESIAN_POINT('Ctrl Pts',(-4.00167127800006,5.2,0.368462794999989));
#312721=CARTESIAN_POINT('Ctrl Pts',(-4.00167127800006,2.2,0.368462794999989));
#312722=CARTESIAN_POINT('Ctrl Pts',(-4.00111056800006,12.2,0.368347635999986));
#312723=CARTESIAN_POINT('Ctrl Pts',(-4.00111056800006,5.2,0.368347635999986));
#312724=CARTESIAN_POINT('Ctrl Pts',(-4.00111056800006,2.2,0.368347635999986));
#312725=CARTESIAN_POINT('Ctrl Pts',(-4.00055584300006,12.2,0.368234452999987));
#312726=CARTESIAN_POINT('Ctrl Pts',(-4.00055584300006,5.2,0.368234452999987));
#312727=CARTESIAN_POINT('Ctrl Pts',(-4.00055584300006,2.2,0.368234452999987));
#312728=CARTESIAN_POINT('Ctrl Pts',(-4.00000712200006,12.2,0.368123230999986));
#312729=CARTESIAN_POINT('Ctrl Pts',(-4.00000712200006,5.2,0.368123230999986));
#312730=CARTESIAN_POINT('Ctrl Pts',(-4.00000712200006,2.2,0.368123230999986));
#312731=CARTESIAN_POINT('Ctrl Pts',(-3.99946441800005,12.2,0.368013957999986));
#312732=CARTESIAN_POINT('Ctrl Pts',(-3.99946441800005,5.2,0.368013957999986));
#312733=CARTESIAN_POINT('Ctrl Pts',(-3.99946441800005,2.2,0.368013957999986));
#312734=CARTESIAN_POINT('Ctrl Pts',(-3.99892775000006,12.2,0.367906621999987));
#312735=CARTESIAN_POINT('Ctrl Pts',(-3.99892775000006,5.2,0.367906621999987));
#312736=CARTESIAN_POINT('Ctrl Pts',(-3.99892775000006,2.2,0.367906621999987));
#312737=CARTESIAN_POINT('Ctrl Pts',(-3.99839713200006,12.2,0.367801208999987));
#312738=CARTESIAN_POINT('Ctrl Pts',(-3.99839713200006,5.2,0.367801208999987));
#312739=CARTESIAN_POINT('Ctrl Pts',(-3.99839713200006,2.2,0.367801208999987));
#312740=CARTESIAN_POINT('Ctrl Pts',(-3.99787258100006,12.2,0.367697706999985));
#312741=CARTESIAN_POINT('Ctrl Pts',(-3.99787258100006,5.2,0.367697706999985));
#312742=CARTESIAN_POINT('Ctrl Pts',(-3.99787258100006,2.2,0.367697706999985));
#312743=CARTESIAN_POINT('Ctrl Pts',(-3.99735411400005,12.2,0.367596101999985));
#312744=CARTESIAN_POINT('Ctrl Pts',(-3.99735411400005,5.2,0.367596101999985));
#312745=CARTESIAN_POINT('Ctrl Pts',(-3.99735411400005,2.2,0.367596101999985));
#312746=CARTESIAN_POINT('Ctrl Pts',(-3.99684174600006,12.2,0.367496380999985));
#312747=CARTESIAN_POINT('Ctrl Pts',(-3.99684174600006,5.2,0.367496380999985));
#312748=CARTESIAN_POINT('Ctrl Pts',(-3.99684174600006,2.2,0.367496380999985));
#312749=CARTESIAN_POINT('Ctrl Pts',(-3.99633549400006,12.2,0.367398531999985));
#312750=CARTESIAN_POINT('Ctrl Pts',(-3.99633549400006,5.2,0.367398531999985));
#312751=CARTESIAN_POINT('Ctrl Pts',(-3.99633549400006,2.2,0.367398531999985));
#312752=CARTESIAN_POINT('Ctrl Pts',(-3.99583537300006,12.2,0.367302539999983));
#312753=CARTESIAN_POINT('Ctrl Pts',(-3.99583537300006,5.2,0.367302539999983));
#312754=CARTESIAN_POINT('Ctrl Pts',(-3.99583537300006,2.2,0.367302539999983));
#312755=CARTESIAN_POINT('Ctrl Pts',(-3.99534140000006,12.2,0.367208392999987));
#312756=CARTESIAN_POINT('Ctrl Pts',(-3.99534140000006,5.2,0.367208392999987));
#312757=CARTESIAN_POINT('Ctrl Pts',(-3.99534140000006,2.2,0.367208392999987));
#312758=CARTESIAN_POINT('Ctrl Pts',(-3.99485359300006,12.2,0.367116076999987));
#312759=CARTESIAN_POINT('Ctrl Pts',(-3.99485359300006,5.2,0.367116076999987));
#312760=CARTESIAN_POINT('Ctrl Pts',(-3.99485359300006,2.2,0.367116076999987));
#312761=CARTESIAN_POINT('Ctrl Pts',(-3.99437196600006,12.2,0.367025579999982));
#312762=CARTESIAN_POINT('Ctrl Pts',(-3.99437196600006,5.2,0.367025579999982));
#312763=CARTESIAN_POINT('Ctrl Pts',(-3.99437196600006,2.2,0.367025579999982));
#312764=CARTESIAN_POINT('Ctrl Pts',(-3.99389653800006,12.2,0.366936886999985));
#312765=CARTESIAN_POINT('Ctrl Pts',(-3.99389653800006,5.2,0.366936886999985));
#312766=CARTESIAN_POINT('Ctrl Pts',(-3.99389653800006,2.2,0.366936886999985));
#312767=CARTESIAN_POINT('Ctrl Pts',(-3.99342732200005,12.2,0.366849983999984));
#312768=CARTESIAN_POINT('Ctrl Pts',(-3.99342732200005,5.2,0.366849983999984));
#312769=CARTESIAN_POINT('Ctrl Pts',(-3.99342732200005,2.2,0.366849983999984));
#312770=CARTESIAN_POINT('Ctrl Pts',(-3.99296433800005,12.2,0.366764859999984));
#312771=CARTESIAN_POINT('Ctrl Pts',(-3.99296433800005,5.2,0.366764859999984));
#312772=CARTESIAN_POINT('Ctrl Pts',(-3.99296433800005,2.2,0.366764859999984));
#312773=CARTESIAN_POINT('Ctrl Pts',(-3.99250760000006,12.2,0.366681498999988));
#312774=CARTESIAN_POINT('Ctrl Pts',(-3.99250760000006,5.2,0.366681498999988));
#312775=CARTESIAN_POINT('Ctrl Pts',(-3.99250760000006,2.2,0.366681498999988));
#312776=CARTESIAN_POINT('Ctrl Pts',(-3.99205712500006,12.2,0.366599888999986));
#312777=CARTESIAN_POINT('Ctrl Pts',(-3.99205712500006,5.2,0.366599888999986));
#312778=CARTESIAN_POINT('Ctrl Pts',(-3.99205712500006,2.2,0.366599888999986));
#312779=CARTESIAN_POINT('Ctrl Pts',(-3.99161293200006,12.2,0.366520014999985));
#312780=CARTESIAN_POINT('Ctrl Pts',(-3.99161293200006,5.2,0.366520014999985));
#312781=CARTESIAN_POINT('Ctrl Pts',(-3.99161293200006,2.2,0.366520014999985));
#312782=CARTESIAN_POINT('Ctrl Pts',(-3.99117503500006,12.2,0.366441861999984));
#312783=CARTESIAN_POINT('Ctrl Pts',(-3.99117503500006,5.2,0.366441861999984));
#312784=CARTESIAN_POINT('Ctrl Pts',(-3.99117503500006,2.2,0.366441861999984));
#312785=CARTESIAN_POINT('Ctrl Pts',(-3.99074345100006,12.2,0.366365419999983));
#312786=CARTESIAN_POINT('Ctrl Pts',(-3.99074345100006,5.2,0.366365419999983));
#312787=CARTESIAN_POINT('Ctrl Pts',(-3.99074345100006,2.2,0.366365419999983));
#312788=CARTESIAN_POINT('Ctrl Pts',(-3.99031819800006,12.2,0.366290670999985));
#312789=CARTESIAN_POINT('Ctrl Pts',(-3.99031819800006,5.2,0.366290670999985));
#312790=CARTESIAN_POINT('Ctrl Pts',(-3.99031819800006,2.2,0.366290670999985));
#312791=CARTESIAN_POINT('Ctrl Pts',(-3.98989929200006,12.2,0.366217603999988));
#312792=CARTESIAN_POINT('Ctrl Pts',(-3.98989929200006,5.2,0.366217603999988));
#312793=CARTESIAN_POINT('Ctrl Pts',(-3.98989929200006,2.2,0.366217603999988));
#312794=CARTESIAN_POINT('Ctrl Pts',(-3.98948675000006,12.2,0.366146201999986));
#312795=CARTESIAN_POINT('Ctrl Pts',(-3.98948675000006,5.2,0.366146201999986));
#312796=CARTESIAN_POINT('Ctrl Pts',(-3.98948675000006,2.2,0.366146201999986));
#312797=CARTESIAN_POINT('Ctrl Pts',(-3.98908058800005,12.2,0.366076453999984));
#312798=CARTESIAN_POINT('Ctrl Pts',(-3.98908058800005,5.2,0.366076453999984));
#312799=CARTESIAN_POINT('Ctrl Pts',(-3.98908058800005,2.2,0.366076453999984));
#312800=CARTESIAN_POINT('Ctrl Pts',(-3.98868082400006,12.2,0.366008341999984));
#312801=CARTESIAN_POINT('Ctrl Pts',(-3.98868082400006,5.2,0.366008341999984));
#312802=CARTESIAN_POINT('Ctrl Pts',(-3.98868082400006,2.2,0.366008341999984));
#312803=CARTESIAN_POINT('Ctrl Pts',(-3.98828747400006,12.2,0.365941855999985));
#312804=CARTESIAN_POINT('Ctrl Pts',(-3.98828747400006,5.2,0.365941855999985));
#312805=CARTESIAN_POINT('Ctrl Pts',(-3.98828747400006,2.2,0.365941855999985));
#312806=CARTESIAN_POINT('Ctrl Pts',(-3.98790055600006,12.2,0.365876978999986));
#312807=CARTESIAN_POINT('Ctrl Pts',(-3.98790055600006,5.2,0.365876978999986));
#312808=CARTESIAN_POINT('Ctrl Pts',(-3.98790055600006,2.2,0.365876978999986));
#312809=CARTESIAN_POINT('Ctrl Pts',(-3.98752008600006,12.2,0.365813696999986));
#312810=CARTESIAN_POINT('Ctrl Pts',(-3.98752008600006,5.2,0.365813696999986));
#312811=CARTESIAN_POINT('Ctrl Pts',(-3.98752008600006,2.2,0.365813696999986));
#312812=CARTESIAN_POINT('Ctrl Pts',(-3.98714608100006,12.2,0.365751996999983));
#312813=CARTESIAN_POINT('Ctrl Pts',(-3.98714608100006,5.2,0.365751996999983));
#312814=CARTESIAN_POINT('Ctrl Pts',(-3.98714608100006,2.2,0.365751996999983));
#312815=CARTESIAN_POINT('Ctrl Pts',(-3.98677856000006,12.2,0.365691861999986));
#312816=CARTESIAN_POINT('Ctrl Pts',(-3.98677856000006,5.2,0.365691861999986));
#312817=CARTESIAN_POINT('Ctrl Pts',(-3.98677856000006,2.2,0.365691861999986));
#312818=CARTESIAN_POINT('Ctrl Pts',(-3.98641753800006,12.2,0.365633278999984));
#312819=CARTESIAN_POINT('Ctrl Pts',(-3.98641753800006,5.2,0.365633278999984));
#312820=CARTESIAN_POINT('Ctrl Pts',(-3.98641753800006,2.2,0.365633278999984));
#312821=CARTESIAN_POINT('Ctrl Pts',(-3.98606303200006,12.2,0.365576231999984));
#312822=CARTESIAN_POINT('Ctrl Pts',(-3.98606303200006,5.2,0.365576231999984));
#312823=CARTESIAN_POINT('Ctrl Pts',(-3.98606303200006,2.2,0.365576231999984));
#312824=CARTESIAN_POINT('Ctrl Pts',(-3.98571506200006,12.2,0.365520707999987));
#312825=CARTESIAN_POINT('Ctrl Pts',(-3.98571506200006,5.2,0.365520707999987));
#312826=CARTESIAN_POINT('Ctrl Pts',(-3.98571506200006,2.2,0.365520707999987));
#312827=CARTESIAN_POINT('Ctrl Pts',(-3.98537364100005,12.2,0.365466690999985));
#312828=CARTESIAN_POINT('Ctrl Pts',(-3.98537364100005,5.2,0.365466690999985));
#312829=CARTESIAN_POINT('Ctrl Pts',(-3.98537364100005,2.2,0.365466690999985));
#312830=CARTESIAN_POINT('Ctrl Pts',(-3.98503878900006,12.2,0.365414166999987));
#312831=CARTESIAN_POINT('Ctrl Pts',(-3.98503878900006,5.2,0.365414166999987));
#312832=CARTESIAN_POINT('Ctrl Pts',(-3.98503878900006,2.2,0.365414166999987));
#312833=CARTESIAN_POINT('Ctrl Pts',(-3.98471052400006,12.2,0.365363119999986));
#312834=CARTESIAN_POINT('Ctrl Pts',(-3.98471052400006,5.2,0.365363119999986));
#312835=CARTESIAN_POINT('Ctrl Pts',(-3.98471052400006,2.2,0.365363119999986));
#312836=CARTESIAN_POINT('Ctrl Pts',(-3.98438886200006,12.2,0.365313535999987));
#312837=CARTESIAN_POINT('Ctrl Pts',(-3.98438886200006,5.2,0.365313535999987));
#312838=CARTESIAN_POINT('Ctrl Pts',(-3.98438886200006,2.2,0.365313535999987));
#312839=CARTESIAN_POINT('Ctrl Pts',(-3.98407382000006,12.2,0.365265398999988));
#312840=CARTESIAN_POINT('Ctrl Pts',(-3.98407382000006,5.2,0.365265398999988));
#312841=CARTESIAN_POINT('Ctrl Pts',(-3.98407382000006,2.2,0.365265398999988));
#312842=CARTESIAN_POINT('Ctrl Pts',(-3.98376541600006,12.2,0.365218693999987));
#312843=CARTESIAN_POINT('Ctrl Pts',(-3.98376541600006,5.2,0.365218693999987));
#312844=CARTESIAN_POINT('Ctrl Pts',(-3.98376541600006,2.2,0.365218693999987));
#312845=CARTESIAN_POINT('Ctrl Pts',(-3.98346366800006,12.2,0.365173405999983));
#312846=CARTESIAN_POINT('Ctrl Pts',(-3.98346366800006,5.2,0.365173405999983));
#312847=CARTESIAN_POINT('Ctrl Pts',(-3.98346366800006,2.2,0.365173405999983));
#312848=CARTESIAN_POINT('Ctrl Pts',(-3.98316859300006,12.2,0.365129519999985));
#312849=CARTESIAN_POINT('Ctrl Pts',(-3.98316859300006,5.2,0.365129519999985));
#312850=CARTESIAN_POINT('Ctrl Pts',(-3.98316859300006,2.2,0.365129519999985));
#312851=CARTESIAN_POINT('Ctrl Pts',(-3.98288020800006,12.2,0.365087019999986));
#312852=CARTESIAN_POINT('Ctrl Pts',(-3.98288020800006,5.2,0.365087019999986));
#312853=CARTESIAN_POINT('Ctrl Pts',(-3.98288020800006,2.2,0.365087019999986));
#312854=CARTESIAN_POINT('Ctrl Pts',(-3.98259853200006,12.2,0.365045891999984));
#312855=CARTESIAN_POINT('Ctrl Pts',(-3.98259853200006,5.2,0.365045891999984));
#312856=CARTESIAN_POINT('Ctrl Pts',(-3.98259853200006,2.2,0.365045891999984));
#312857=CARTESIAN_POINT('Ctrl Pts',(-3.98232358100006,12.2,0.365006117999984));
#312858=CARTESIAN_POINT('Ctrl Pts',(-3.98232358100006,5.2,0.365006117999984));
#312859=CARTESIAN_POINT('Ctrl Pts',(-3.98232358100006,2.2,0.365006117999984));
#312860=CARTESIAN_POINT('Ctrl Pts',(-3.98205537400006,12.2,0.364967683999984));
#312861=CARTESIAN_POINT('Ctrl Pts',(-3.98205537400006,5.2,0.364967683999984));
#312862=CARTESIAN_POINT('Ctrl Pts',(-3.98205537400006,2.2,0.364967683999984));
#312863=CARTESIAN_POINT('Ctrl Pts',(-3.98179392900006,12.2,0.364930574999986));
#312864=CARTESIAN_POINT('Ctrl Pts',(-3.98179392900006,5.2,0.364930574999986));
#312865=CARTESIAN_POINT('Ctrl Pts',(-3.98179392900006,2.2,0.364930574999986));
#312866=CARTESIAN_POINT('Ctrl Pts',(-3.98153926300005,12.2,0.364894773999982));
#312867=CARTESIAN_POINT('Ctrl Pts',(-3.98153926300005,5.2,0.364894773999982));
#312868=CARTESIAN_POINT('Ctrl Pts',(-3.98153926300005,2.2,0.364894773999982));
#312869=CARTESIAN_POINT('Ctrl Pts',(-3.98129139400006,12.2,0.364860263999987));
#312870=CARTESIAN_POINT('Ctrl Pts',(-3.98129139400006,5.2,0.364860263999987));
#312871=CARTESIAN_POINT('Ctrl Pts',(-3.98129139400006,2.2,0.364860263999987));
#312872=CARTESIAN_POINT('Ctrl Pts',(-3.98105033900006,12.2,0.364827031999986));
#312873=CARTESIAN_POINT('Ctrl Pts',(-3.98105033900006,5.2,0.364827031999986));
#312874=CARTESIAN_POINT('Ctrl Pts',(-3.98105033900006,2.2,0.364827031999986));
#312875=CARTESIAN_POINT('Ctrl Pts',(-3.98081611700006,12.2,0.364795060999987));
#312876=CARTESIAN_POINT('Ctrl Pts',(-3.98081611700006,5.2,0.364795060999987));
#312877=CARTESIAN_POINT('Ctrl Pts',(-3.98081611700006,2.2,0.364795060999987));
#312878=CARTESIAN_POINT('Ctrl Pts',(-3.98058874600006,12.2,0.364764332999985));
#312879=CARTESIAN_POINT('Ctrl Pts',(-3.98058874600006,5.2,0.364764332999985));
#312880=CARTESIAN_POINT('Ctrl Pts',(-3.98058874600006,2.2,0.364764332999985));
#312881=CARTESIAN_POINT('Ctrl Pts',(-3.98036824300006,12.2,0.364734833999982));
#312882=CARTESIAN_POINT('Ctrl Pts',(-3.98036824300006,5.2,0.364734833999982));
#312883=CARTESIAN_POINT('Ctrl Pts',(-3.98036824300006,2.2,0.364734833999982));
#312884=CARTESIAN_POINT('Ctrl Pts',(-3.98015462700006,12.2,0.364706547999987));
#312885=CARTESIAN_POINT('Ctrl Pts',(-3.98015462700006,5.2,0.364706547999987));
#312886=CARTESIAN_POINT('Ctrl Pts',(-3.98015462700006,2.2,0.364706547999987));
#312887=CARTESIAN_POINT('Ctrl Pts',(-3.97994791600006,12.2,0.364679458999984));
#312888=CARTESIAN_POINT('Ctrl Pts',(-3.97994791600006,5.2,0.364679458999984));
#312889=CARTESIAN_POINT('Ctrl Pts',(-3.97994791600006,2.2,0.364679458999984));
#312890=CARTESIAN_POINT('Ctrl Pts',(-3.97974812800006,12.2,0.364653547999985));
#312891=CARTESIAN_POINT('Ctrl Pts',(-3.97974812800006,5.2,0.364653547999985));
#312892=CARTESIAN_POINT('Ctrl Pts',(-3.97974812800006,2.2,0.364653547999985));
#312893=CARTESIAN_POINT('Ctrl Pts',(-3.97955528200006,12.2,0.364628800999984));
#312894=CARTESIAN_POINT('Ctrl Pts',(-3.97955528200006,5.2,0.364628800999984));
#312895=CARTESIAN_POINT('Ctrl Pts',(-3.97955528200006,2.2,0.364628800999984));
#312896=CARTESIAN_POINT('Ctrl Pts',(-3.97936939600006,12.2,0.364605198999985));
#312897=CARTESIAN_POINT('Ctrl Pts',(-3.97936939600006,5.2,0.364605198999985));
#312898=CARTESIAN_POINT('Ctrl Pts',(-3.97936939600006,2.2,0.364605198999985));
#312899=CARTESIAN_POINT('Ctrl Pts',(-3.97919048700006,12.2,0.364582728999987));
#312900=CARTESIAN_POINT('Ctrl Pts',(-3.97919048700006,5.2,0.364582728999987));
#312901=CARTESIAN_POINT('Ctrl Pts',(-3.97919048700006,2.2,0.364582728999987));
#312902=CARTESIAN_POINT('Ctrl Pts',(-3.97901857400006,12.2,0.364561370999983));
#312903=CARTESIAN_POINT('Ctrl Pts',(-3.97901857400006,5.2,0.364561370999983));
#312904=CARTESIAN_POINT('Ctrl Pts',(-3.97901857400006,2.2,0.364561370999983));
#312905=CARTESIAN_POINT('Ctrl Pts',(-3.97885367500006,12.2,0.364541110999985));
#312906=CARTESIAN_POINT('Ctrl Pts',(-3.97885367500006,5.2,0.364541110999985));
#312907=CARTESIAN_POINT('Ctrl Pts',(-3.97885367500006,2.2,0.364541110999985));
#312908=CARTESIAN_POINT('Ctrl Pts',(-3.97869580700006,12.2,0.364521932999988));
#312909=CARTESIAN_POINT('Ctrl Pts',(-3.97869580700006,5.2,0.364521932999988));
#312910=CARTESIAN_POINT('Ctrl Pts',(-3.97869580700006,2.2,0.364521932999988));
#312911=CARTESIAN_POINT('Ctrl Pts',(-3.97854499000006,12.2,0.364503816999986));
#312912=CARTESIAN_POINT('Ctrl Pts',(-3.97854499000006,5.2,0.364503816999986));
#312913=CARTESIAN_POINT('Ctrl Pts',(-3.97854499000006,2.2,0.364503816999986));
#312914=CARTESIAN_POINT('Ctrl Pts',(-3.97840124500005,12.2,0.364486745999986));
#312915=CARTESIAN_POINT('Ctrl Pts',(-3.97840124500005,5.2,0.364486745999986));
#312916=CARTESIAN_POINT('Ctrl Pts',(-3.97840124500005,2.2,0.364486745999986));
#312917=CARTESIAN_POINT('Ctrl Pts',(-3.97826458900005,12.2,0.364470703999986));
#312918=CARTESIAN_POINT('Ctrl Pts',(-3.97826458900005,5.2,0.364470703999986));
#312919=CARTESIAN_POINT('Ctrl Pts',(-3.97826458900005,2.2,0.364470703999986));
#312920=CARTESIAN_POINT('Ctrl Pts',(-3.97813504000006,12.2,0.364455670999986));
#312921=CARTESIAN_POINT('Ctrl Pts',(-3.97813504000006,5.2,0.364455670999986));
#312922=CARTESIAN_POINT('Ctrl Pts',(-3.97813504000006,2.2,0.364455670999986));
#312923=CARTESIAN_POINT('Ctrl Pts',(-3.97801262100006,12.2,0.364441631999988));
#312924=CARTESIAN_POINT('Ctrl Pts',(-3.97801262100006,5.2,0.364441631999988));
#312925=CARTESIAN_POINT('Ctrl Pts',(-3.97801262100006,2.2,0.364441631999988));
#312926=CARTESIAN_POINT('Ctrl Pts',(-3.97789734500006,12.2,0.364428570999986));
#312927=CARTESIAN_POINT('Ctrl Pts',(-3.97789734500006,5.2,0.364428570999986));
#312928=CARTESIAN_POINT('Ctrl Pts',(-3.97789734500006,2.2,0.364428570999986));
#312929=CARTESIAN_POINT('Ctrl Pts',(-3.97778922900006,12.2,0.364416470999984));
#312930=CARTESIAN_POINT('Ctrl Pts',(-3.97778922900006,5.2,0.364416470999984));
#312931=CARTESIAN_POINT('Ctrl Pts',(-3.97778922900006,2.2,0.364416470999984));
#312932=CARTESIAN_POINT('Ctrl Pts',(-3.97768829100006,12.2,0.364405317999985));
#312933=CARTESIAN_POINT('Ctrl Pts',(-3.97768829100006,5.2,0.364405317999985));
#312934=CARTESIAN_POINT('Ctrl Pts',(-3.97768829100006,2.2,0.364405317999985));
#312935=CARTESIAN_POINT('Ctrl Pts',(-3.97759455100006,12.2,0.364395092999987));
#312936=CARTESIAN_POINT('Ctrl Pts',(-3.97759455100006,5.2,0.364395092999987));
#312937=CARTESIAN_POINT('Ctrl Pts',(-3.97759455100006,2.2,0.364395092999987));
#312938=CARTESIAN_POINT('Ctrl Pts',(-3.97750803000006,12.2,0.364385775999985));
#312939=CARTESIAN_POINT('Ctrl Pts',(-3.97750803000006,5.2,0.364385775999985));
#312940=CARTESIAN_POINT('Ctrl Pts',(-3.97750803000006,2.2,0.364385775999985));
#312941=CARTESIAN_POINT('Ctrl Pts',(-3.97742875100006,12.2,0.364377344999984));
#312942=CARTESIAN_POINT('Ctrl Pts',(-3.97742875100006,5.2,0.364377344999984));
#312943=CARTESIAN_POINT('Ctrl Pts',(-3.97742875100006,2.2,0.364377344999984));
#312944=CARTESIAN_POINT('Ctrl Pts',(-3.97735673900006,12.2,0.364369776999984));
#312945=CARTESIAN_POINT('Ctrl Pts',(-3.97735673900006,5.2,0.364369776999984));
#312946=CARTESIAN_POINT('Ctrl Pts',(-3.97735673900006,2.2,0.364369776999984));
#312947=CARTESIAN_POINT('Ctrl Pts',(-3.97729201500006,12.2,0.364363052999988));
#312948=CARTESIAN_POINT('Ctrl Pts',(-3.97729201500006,5.2,0.364363052999988));
#312949=CARTESIAN_POINT('Ctrl Pts',(-3.97729201500006,2.2,0.364363052999988));
#312950=CARTESIAN_POINT('Ctrl Pts',(-3.97723459300006,12.2,0.364357157999984));
#312951=CARTESIAN_POINT('Ctrl Pts',(-3.97723459300006,5.2,0.364357157999984));
#312952=CARTESIAN_POINT('Ctrl Pts',(-3.97723459300006,2.2,0.364357157999984));
#312953=CARTESIAN_POINT('Ctrl Pts',(-3.97717911977753,12.2,0.364351538608712));
#312954=CARTESIAN_POINT('Ctrl Pts',(-3.97717911977753,5.2,0.364351538608712));
#312955=CARTESIAN_POINT('Ctrl Pts',(-3.97717911977753,2.2,0.364351538608712));
#312956=CARTESIAN_POINT('Ctrl Pts',(-3.97714119412776,12.2,0.364347774899514));
#312957=CARTESIAN_POINT('Ctrl Pts',(-3.97714119412776,5.2,0.364347774899514));
#312958=CARTESIAN_POINT('Ctrl Pts',(-3.97714119412776,2.2,0.364347774899514));
#312959=CARTESIAN_POINT('Ctrl Pts',(-3.97711620336759,12.2,0.364345349293931));
#312960=CARTESIAN_POINT('Ctrl Pts',(-3.97711620336759,5.2,0.364345349293931));
#312961=CARTESIAN_POINT('Ctrl Pts',(-3.97711620336759,2.2,0.364345349293931));
#312962=CARTESIAN_POINT('Ctrl Pts',(-3.97710063292244,12.2,0.364343872857997));
#312963=CARTESIAN_POINT('Ctrl Pts',(-3.97710063292244,5.2,0.364343872857997));
#312964=CARTESIAN_POINT('Ctrl Pts',(-3.97710063292244,2.2,0.364343872857997));
#312965=CARTESIAN_POINT('Ctrl Pts',(-3.97709101900006,12.2,0.364342956999986));
#312966=CARTESIAN_POINT('Ctrl Pts',(-3.97709101900006,5.2,0.364342956999986));
#312967=CARTESIAN_POINT('Ctrl Pts',(-3.97709101900006,2.2,0.364342956999986));
#312968=CARTESIAN_POINT('',(-3.97709103800006,2.7,0.364342755999986));
#312969=CARTESIAN_POINT('',(-3.97709103800006,12.2,0.364342755999987));
#312970=CARTESIAN_POINT('Ctrl Pts',(-4.68689806900006,2.7,0.771677711999987));
#312971=CARTESIAN_POINT('Ctrl Pts',(-4.51665756805539,2.7,0.61771045344485));
#312972=CARTESIAN_POINT('Ctrl Pts',(-4.35724736115071,2.69999999999778,
0.51363188389716));
#312973=CARTESIAN_POINT('Ctrl Pts',(-4.07521173625289,2.69999999999778,
0.378371909046352));
#312974=CARTESIAN_POINT('Ctrl Pts',(-3.98972974571173,2.70000000000228,
0.365710767362733));
#312975=CARTESIAN_POINT('Ctrl Pts',(-3.97742731815954,2.70000000000228,
0.364376993680789));
#312976=CARTESIAN_POINT('Ctrl Pts',(-3.97725926445937,2.7,0.36435898468835));
#312977=CARTESIAN_POINT('Ctrl Pts',(-3.97709101900006,2.7,0.364342956999986));
#312978=CARTESIAN_POINT('Origin',(-3.97703993500006,15.2,0.364338073999986));
#312979=CARTESIAN_POINT('',(-3.60988374900006,2.7,0.330702762999984));
#312980=CARTESIAN_POINT('',(-3.60988374900006,2.2,0.330702762999984));
#312981=CARTESIAN_POINT('',(-1.98851996745301,2.7,0.182169037513505));
#312982=CARTESIAN_POINT('Origin',(-5.66300478732629E-14,15.2,-1.77635683940025E-14));
#312983=CARTESIAN_POINT('',(-3.61766281500006,2.7,-0.230522786000017));
#312984=CARTESIAN_POINT('',(-3.61766281500006,12.2,-0.230522786000016));
#312985=CARTESIAN_POINT('Origin',(-5.66300478732629E-14,2.7,-1.92943768261394E-14));
#312986=CARTESIAN_POINT('Origin',(-5.66300478732629E-14,15.2,-1.77635683940025E-14));
#312987=CARTESIAN_POINT('',(-3.98564434100006,2.7,-0.253971109000016));
#312988=CARTESIAN_POINT('',(-3.98564434100006,12.2,-0.253971109000015));
#312989=CARTESIAN_POINT('',(-5.65795294118429E-14,2.7,-1.92911577155913E-14));
#312990=CARTESIAN_POINT('Ctrl Pts',(-3.98564433100006,12.2,-0.253971246000013));
#312991=CARTESIAN_POINT('Ctrl Pts',(-3.98564433100006,5.2,-0.253971246000013));
#312992=CARTESIAN_POINT('Ctrl Pts',(-3.98564433100006,2.2,-0.253971246000013));
#312993=CARTESIAN_POINT('Ctrl Pts',(-3.98565115826319,12.2,-0.253971706950256));
#312994=CARTESIAN_POINT('Ctrl Pts',(-3.98565115826319,5.2,-0.253971706950256));
#312995=CARTESIAN_POINT('Ctrl Pts',(-3.98565115826319,2.2,-0.253971706950256));
#312996=CARTESIAN_POINT('Ctrl Pts',(-3.9856643630646,12.2,-0.253972598617502));
#312997=CARTESIAN_POINT('Ctrl Pts',(-3.9856643630646,5.2,-0.253972598617502));
#312998=CARTESIAN_POINT('Ctrl Pts',(-3.9856643630646,2.2,-0.253972598617502));
#312999=CARTESIAN_POINT('Ctrl Pts',(-3.98568393993797,12.2,-0.253973926488822));
#313000=CARTESIAN_POINT('Ctrl Pts',(-3.98568393993797,5.2,-0.253973926488822));
#313001=CARTESIAN_POINT('Ctrl Pts',(-3.98568393993797,2.2,-0.253973926488822));
#313002=CARTESIAN_POINT('Ctrl Pts',(-3.98570992390786,12.2,-0.253975634437502));
#313003=CARTESIAN_POINT('Ctrl Pts',(-3.98570992390786,5.2,-0.253975634437502));
#313004=CARTESIAN_POINT('Ctrl Pts',(-3.98570992390786,2.2,-0.253975634437502));
#313005=CARTESIAN_POINT('Ctrl Pts',(-3.98575508100006,12.2,-0.253978930000014));
#313006=CARTESIAN_POINT('Ctrl Pts',(-3.98575508100006,5.2,-0.253978930000014));
#313007=CARTESIAN_POINT('Ctrl Pts',(-3.98575508100006,2.2,-0.253978930000014));
#313008=CARTESIAN_POINT('Ctrl Pts',(-3.98580531100006,12.2,-0.253982615000012));
#313009=CARTESIAN_POINT('Ctrl Pts',(-3.98580531100006,5.2,-0.253982615000012));
#313010=CARTESIAN_POINT('Ctrl Pts',(-3.98580531100006,2.2,-0.253982615000012));
#313011=CARTESIAN_POINT('Ctrl Pts',(-3.98586287300006,12.2,-0.253986916000013));
#313012=CARTESIAN_POINT('Ctrl Pts',(-3.98586287300006,5.2,-0.253986916000013));
#313013=CARTESIAN_POINT('Ctrl Pts',(-3.98586287300006,2.2,-0.253986916000013));
#313014=CARTESIAN_POINT('Ctrl Pts',(-3.98592776000006,12.2,-0.253991845000012));
#313015=CARTESIAN_POINT('Ctrl Pts',(-3.98592776000006,5.2,-0.253991845000012));
#313016=CARTESIAN_POINT('Ctrl Pts',(-3.98592776000006,2.2,-0.253991845000012));
#313017=CARTESIAN_POINT('Ctrl Pts',(-3.98599995300006,12.2,-0.253997413000011));
#313018=CARTESIAN_POINT('Ctrl Pts',(-3.98599995300006,5.2,-0.253997413000011));
#313019=CARTESIAN_POINT('Ctrl Pts',(-3.98599995300006,2.2,-0.253997413000011));
#313020=CARTESIAN_POINT('Ctrl Pts',(-3.98607943500005,12.2,-0.254003644000012));
#313021=CARTESIAN_POINT('Ctrl Pts',(-3.98607943500005,5.2,-0.254003644000012));
#313022=CARTESIAN_POINT('Ctrl Pts',(-3.98607943500005,2.2,-0.254003644000012));
#313023=CARTESIAN_POINT('Ctrl Pts',(-3.98616618200006,12.2,-0.254010559000015));
#313024=CARTESIAN_POINT('Ctrl Pts',(-3.98616618200006,5.2,-0.254010559000015));
#313025=CARTESIAN_POINT('Ctrl Pts',(-3.98616618200006,2.2,-0.254010559000015));
#313026=CARTESIAN_POINT('Ctrl Pts',(-3.98626017000006,12.2,-0.254018182000015));
#313027=CARTESIAN_POINT('Ctrl Pts',(-3.98626017000006,5.2,-0.254018182000015));
#313028=CARTESIAN_POINT('Ctrl Pts',(-3.98626017000006,2.2,-0.254018182000015));
#313029=CARTESIAN_POINT('Ctrl Pts',(-3.98636137800006,12.2,-0.254026533000014));
#313030=CARTESIAN_POINT('Ctrl Pts',(-3.98636137800006,5.2,-0.254026533000014));
#313031=CARTESIAN_POINT('Ctrl Pts',(-3.98636137800006,2.2,-0.254026533000014));
#313032=CARTESIAN_POINT('Ctrl Pts',(-3.98646978700006,12.2,-0.254035631000011));
#313033=CARTESIAN_POINT('Ctrl Pts',(-3.98646978700006,5.2,-0.254035631000011));
#313034=CARTESIAN_POINT('Ctrl Pts',(-3.98646978700006,2.2,-0.254035631000011));
#313035=CARTESIAN_POINT('Ctrl Pts',(-3.98658538200006,12.2,-0.254045493000015));
#313036=CARTESIAN_POINT('Ctrl Pts',(-3.98658538200006,5.2,-0.254045493000015));
#313037=CARTESIAN_POINT('Ctrl Pts',(-3.98658538200006,2.2,-0.254045493000015));
#313038=CARTESIAN_POINT('Ctrl Pts',(-3.98670814400006,12.2,-0.254056134000016));
#313039=CARTESIAN_POINT('Ctrl Pts',(-3.98670814400006,5.2,-0.254056134000016));
#313040=CARTESIAN_POINT('Ctrl Pts',(-3.98670814400006,2.2,-0.254056134000016));
#313041=CARTESIAN_POINT('Ctrl Pts',(-3.98683805700006,12.2,-0.254067570000016));
#313042=CARTESIAN_POINT('Ctrl Pts',(-3.98683805700006,5.2,-0.254067570000016));
#313043=CARTESIAN_POINT('Ctrl Pts',(-3.98683805700006,2.2,-0.254067570000016));
#313044=CARTESIAN_POINT('Ctrl Pts',(-3.98697510600006,12.2,-0.254079819000013));
#313045=CARTESIAN_POINT('Ctrl Pts',(-3.98697510600006,5.2,-0.254079819000013));
#313046=CARTESIAN_POINT('Ctrl Pts',(-3.98697510600006,2.2,-0.254079819000013));
#313047=CARTESIAN_POINT('Ctrl Pts',(-3.98711926900006,12.2,-0.254092898000016));
#313048=CARTESIAN_POINT('Ctrl Pts',(-3.98711926900006,5.2,-0.254092898000016));
#313049=CARTESIAN_POINT('Ctrl Pts',(-3.98711926900006,2.2,-0.254092898000016));
#313050=CARTESIAN_POINT('Ctrl Pts',(-3.98727053100006,12.2,-0.254106827000014));
#313051=CARTESIAN_POINT('Ctrl Pts',(-3.98727053100006,5.2,-0.254106827000014));
#313052=CARTESIAN_POINT('Ctrl Pts',(-3.98727053100006,2.2,-0.254106827000014));
#313053=CARTESIAN_POINT('Ctrl Pts',(-3.98742886900005,12.2,-0.254121623000017));
#313054=CARTESIAN_POINT('Ctrl Pts',(-3.98742886900005,5.2,-0.254121623000017));
#313055=CARTESIAN_POINT('Ctrl Pts',(-3.98742886900005,2.2,-0.254121623000017));
#313056=CARTESIAN_POINT('Ctrl Pts',(-3.98759426600006,12.2,-0.254137305000013));
#313057=CARTESIAN_POINT('Ctrl Pts',(-3.98759426600006,5.2,-0.254137305000013));
#313058=CARTESIAN_POINT('Ctrl Pts',(-3.98759426600006,2.2,-0.254137305000013));
#313059=CARTESIAN_POINT('Ctrl Pts',(-3.98776670600006,12.2,-0.254153889000013));
#313060=CARTESIAN_POINT('Ctrl Pts',(-3.98776670600006,5.2,-0.254153889000013));
#313061=CARTESIAN_POINT('Ctrl Pts',(-3.98776670600006,2.2,-0.254153889000013));
#313062=CARTESIAN_POINT('Ctrl Pts',(-3.98794616800005,12.2,-0.254171392000018));
#313063=CARTESIAN_POINT('Ctrl Pts',(-3.98794616800005,5.2,-0.254171392000018));
#313064=CARTESIAN_POINT('Ctrl Pts',(-3.98794616800005,2.2,-0.254171392000018));
#313065=CARTESIAN_POINT('Ctrl Pts',(-3.98813263700006,12.2,-0.254189832000016));
#313066=CARTESIAN_POINT('Ctrl Pts',(-3.98813263700006,5.2,-0.254189832000016));
#313067=CARTESIAN_POINT('Ctrl Pts',(-3.98813263700006,2.2,-0.254189832000016));
#313068=CARTESIAN_POINT('Ctrl Pts',(-3.98832609600006,12.2,-0.254209226000013));
#313069=CARTESIAN_POINT('Ctrl Pts',(-3.98832609600006,5.2,-0.254209226000013));
#313070=CARTESIAN_POINT('Ctrl Pts',(-3.98832609600006,2.2,-0.254209226000013));
#313071=CARTESIAN_POINT('Ctrl Pts',(-3.98852652500006,12.2,-0.254229589000015));
#313072=CARTESIAN_POINT('Ctrl Pts',(-3.98852652500006,5.2,-0.254229589000015));
#313073=CARTESIAN_POINT('Ctrl Pts',(-3.98852652500006,2.2,-0.254229589000015));
#313074=CARTESIAN_POINT('Ctrl Pts',(-3.98873390800006,12.2,-0.254250939000014));
#313075=CARTESIAN_POINT('Ctrl Pts',(-3.98873390800006,5.2,-0.254250939000014));
#313076=CARTESIAN_POINT('Ctrl Pts',(-3.98873390800006,2.2,-0.254250939000014));
#313077=CARTESIAN_POINT('Ctrl Pts',(-3.98894822500006,12.2,-0.254273293000011));
#313078=CARTESIAN_POINT('Ctrl Pts',(-3.98894822500006,5.2,-0.254273293000011));
#313079=CARTESIAN_POINT('Ctrl Pts',(-3.98894822500006,2.2,-0.254273293000011));
#313080=CARTESIAN_POINT('Ctrl Pts',(-3.98916946100006,12.2,-0.254296669000014));
#313081=CARTESIAN_POINT('Ctrl Pts',(-3.98916946100006,5.2,-0.254296669000014));
#313082=CARTESIAN_POINT('Ctrl Pts',(-3.98916946100006,2.2,-0.254296669000014));
#313083=CARTESIAN_POINT('Ctrl Pts',(-3.98939759700006,12.2,-0.254321082000013));
#313084=CARTESIAN_POINT('Ctrl Pts',(-3.98939759700006,5.2,-0.254321082000013));
#313085=CARTESIAN_POINT('Ctrl Pts',(-3.98939759700006,2.2,-0.254321082000013));
#313086=CARTESIAN_POINT('Ctrl Pts',(-3.98963261500006,12.2,-0.254346550000015));
#313087=CARTESIAN_POINT('Ctrl Pts',(-3.98963261500006,5.2,-0.254346550000015));
#313088=CARTESIAN_POINT('Ctrl Pts',(-3.98963261500006,2.2,-0.254346550000015));
#313089=CARTESIAN_POINT('Ctrl Pts',(-3.98987449700006,12.2,-0.254373088000013));
#313090=CARTESIAN_POINT('Ctrl Pts',(-3.98987449700006,5.2,-0.254373088000013));
#313091=CARTESIAN_POINT('Ctrl Pts',(-3.98987449700006,2.2,-0.254373088000013));
#313092=CARTESIAN_POINT('Ctrl Pts',(-3.99012322800006,12.2,-0.254400714000016));
#313093=CARTESIAN_POINT('Ctrl Pts',(-3.99012322800006,5.2,-0.254400714000016));
#313094=CARTESIAN_POINT('Ctrl Pts',(-3.99012322800006,2.2,-0.254400714000016));
#313095=CARTESIAN_POINT('Ctrl Pts',(-3.99037878800006,12.2,-0.254429444000017));
#313096=CARTESIAN_POINT('Ctrl Pts',(-3.99037878800006,5.2,-0.254429444000017));
#313097=CARTESIAN_POINT('Ctrl Pts',(-3.99037878800006,2.2,-0.254429444000017));
#313098=CARTESIAN_POINT('Ctrl Pts',(-3.99064116200006,12.2,-0.254459292000018));
#313099=CARTESIAN_POINT('Ctrl Pts',(-3.99064116200006,5.2,-0.254459292000018));
#313100=CARTESIAN_POINT('Ctrl Pts',(-3.99064116200006,2.2,-0.254459292000018));
#313101=CARTESIAN_POINT('Ctrl Pts',(-3.99091033200006,12.2,-0.254490278000015));
#313102=CARTESIAN_POINT('Ctrl Pts',(-3.99091033200006,5.2,-0.254490278000015));
#313103=CARTESIAN_POINT('Ctrl Pts',(-3.99091033200006,2.2,-0.254490278000015));
#313104=CARTESIAN_POINT('Ctrl Pts',(-3.99118627800005,12.2,-0.254522415000018));
#313105=CARTESIAN_POINT('Ctrl Pts',(-3.99118627800005,5.2,-0.254522415000018));
#313106=CARTESIAN_POINT('Ctrl Pts',(-3.99118627800005,2.2,-0.254522415000018));
#313107=CARTESIAN_POINT('Ctrl Pts',(-3.99146898700006,12.2,-0.254555721000016));
#313108=CARTESIAN_POINT('Ctrl Pts',(-3.99146898700006,5.2,-0.254555721000016));
#313109=CARTESIAN_POINT('Ctrl Pts',(-3.99146898700006,2.2,-0.254555721000016));
#313110=CARTESIAN_POINT('Ctrl Pts',(-3.99175843800006,12.2,-0.254590211000014));
#313111=CARTESIAN_POINT('Ctrl Pts',(-3.99175843800006,5.2,-0.254590211000014));
#313112=CARTESIAN_POINT('Ctrl Pts',(-3.99175843800006,2.2,-0.254590211000014));
#313113=CARTESIAN_POINT('Ctrl Pts',(-3.99205461600006,12.2,-0.254625902000014));
#313114=CARTESIAN_POINT('Ctrl Pts',(-3.99205461600006,5.2,-0.254625902000014));
#313115=CARTESIAN_POINT('Ctrl Pts',(-3.99205461600006,2.2,-0.254625902000014));
#313116=CARTESIAN_POINT('Ctrl Pts',(-3.99235750300006,12.2,-0.254662810000017));
#313117=CARTESIAN_POINT('Ctrl Pts',(-3.99235750300006,5.2,-0.254662810000017));
#313118=CARTESIAN_POINT('Ctrl Pts',(-3.99235750300006,2.2,-0.254662810000017));
#313119=CARTESIAN_POINT('Ctrl Pts',(-3.99266708400006,12.2,-0.254700949000015));
#313120=CARTESIAN_POINT('Ctrl Pts',(-3.99266708400006,5.2,-0.254700949000015));
#313121=CARTESIAN_POINT('Ctrl Pts',(-3.99266708400006,2.2,-0.254700949000015));
#313122=CARTESIAN_POINT('Ctrl Pts',(-3.99298333800005,12.2,-0.254740335000014));
#313123=CARTESIAN_POINT('Ctrl Pts',(-3.99298333800005,5.2,-0.254740335000014));
#313124=CARTESIAN_POINT('Ctrl Pts',(-3.99298333800005,2.2,-0.254740335000014));
#313125=CARTESIAN_POINT('Ctrl Pts',(-3.99330625200006,12.2,-0.254780985000016));
#313126=CARTESIAN_POINT('Ctrl Pts',(-3.99330625200006,5.2,-0.254780985000016));
#313127=CARTESIAN_POINT('Ctrl Pts',(-3.99330625200006,2.2,-0.254780985000016));
#313128=CARTESIAN_POINT('Ctrl Pts',(-3.99363580700006,12.2,-0.254822914000012));
#313129=CARTESIAN_POINT('Ctrl Pts',(-3.99363580700006,5.2,-0.254822914000012));
#313130=CARTESIAN_POINT('Ctrl Pts',(-3.99363580700006,2.2,-0.254822914000012));
#313131=CARTESIAN_POINT('Ctrl Pts',(-3.99397198400006,12.2,-0.254866137000014));
#313132=CARTESIAN_POINT('Ctrl Pts',(-3.99397198400006,5.2,-0.254866137000014));
#313133=CARTESIAN_POINT('Ctrl Pts',(-3.99397198400006,2.2,-0.254866137000014));
#313134=CARTESIAN_POINT('Ctrl Pts',(-3.99431477100006,12.2,-0.254910670000013));
#313135=CARTESIAN_POINT('Ctrl Pts',(-3.99431477100006,5.2,-0.254910670000013));
#313136=CARTESIAN_POINT('Ctrl Pts',(-3.99431477100006,2.2,-0.254910670000013));
#313137=CARTESIAN_POINT('Ctrl Pts',(-3.99466414700006,12.2,-0.254956529000014));
#313138=CARTESIAN_POINT('Ctrl Pts',(-3.99466414700006,5.2,-0.254956529000014));
#313139=CARTESIAN_POINT('Ctrl Pts',(-3.99466414700006,2.2,-0.254956529000014));
#313140=CARTESIAN_POINT('Ctrl Pts',(-3.99502009800006,12.2,-0.255003727000016));
#313141=CARTESIAN_POINT('Ctrl Pts',(-3.99502009800006,5.2,-0.255003727000016));
#313142=CARTESIAN_POINT('Ctrl Pts',(-3.99502009800006,2.2,-0.255003727000016));
#313143=CARTESIAN_POINT('Ctrl Pts',(-3.99538260500006,12.2,-0.255052282000015));
#313144=CARTESIAN_POINT('Ctrl Pts',(-3.99538260500006,5.2,-0.255052282000015));
#313145=CARTESIAN_POINT('Ctrl Pts',(-3.99538260500006,2.2,-0.255052282000015));
#313146=CARTESIAN_POINT('Ctrl Pts',(-3.99575165200006,12.2,-0.255102208000015));
#313147=CARTESIAN_POINT('Ctrl Pts',(-3.99575165200006,5.2,-0.255102208000015));
#313148=CARTESIAN_POINT('Ctrl Pts',(-3.99575165200006,2.2,-0.255102208000015));
#313149=CARTESIAN_POINT('Ctrl Pts',(-3.99612722300006,12.2,-0.255153519000015));
#313150=CARTESIAN_POINT('Ctrl Pts',(-3.99612722300006,5.2,-0.255153519000015));
#313151=CARTESIAN_POINT('Ctrl Pts',(-3.99612722300006,2.2,-0.255153519000015));
#313152=CARTESIAN_POINT('Ctrl Pts',(-3.99650930000006,12.2,-0.255206231000016));
#313153=CARTESIAN_POINT('Ctrl Pts',(-3.99650930000006,5.2,-0.255206231000016));
#313154=CARTESIAN_POINT('Ctrl Pts',(-3.99650930000006,2.2,-0.255206231000016));
#313155=CARTESIAN_POINT('Ctrl Pts',(-3.99689786800006,12.2,-0.255260358000013));
#313156=CARTESIAN_POINT('Ctrl Pts',(-3.99689786800006,5.2,-0.255260358000013));
#313157=CARTESIAN_POINT('Ctrl Pts',(-3.99689786800006,2.2,-0.255260358000013));
#313158=CARTESIAN_POINT('Ctrl Pts',(-3.99729290900006,12.2,-0.255315917000014));
#313159=CARTESIAN_POINT('Ctrl Pts',(-3.99729290900006,5.2,-0.255315917000014));
#313160=CARTESIAN_POINT('Ctrl Pts',(-3.99729290900006,2.2,-0.255315917000014));
#313161=CARTESIAN_POINT('Ctrl Pts',(-3.99769440800006,12.2,-0.255372921000014));
#313162=CARTESIAN_POINT('Ctrl Pts',(-3.99769440800006,5.2,-0.255372921000014));
#313163=CARTESIAN_POINT('Ctrl Pts',(-3.99769440800006,2.2,-0.255372921000014));
#313164=CARTESIAN_POINT('Ctrl Pts',(-3.99810234600006,12.2,-0.255431386000016));
#313165=CARTESIAN_POINT('Ctrl Pts',(-3.99810234600006,5.2,-0.255431386000016));
#313166=CARTESIAN_POINT('Ctrl Pts',(-3.99810234600006,2.2,-0.255431386000016));
#313167=CARTESIAN_POINT('Ctrl Pts',(-3.99851671000006,12.2,-0.255491326000015));
#313168=CARTESIAN_POINT('Ctrl Pts',(-3.99851671000006,5.2,-0.255491326000015));
#313169=CARTESIAN_POINT('Ctrl Pts',(-3.99851671000006,2.2,-0.255491326000015));
#313170=CARTESIAN_POINT('Ctrl Pts',(-3.99893748000006,12.2,-0.255552756000017));
#313171=CARTESIAN_POINT('Ctrl Pts',(-3.99893748000006,5.2,-0.255552756000017));
#313172=CARTESIAN_POINT('Ctrl Pts',(-3.99893748000006,2.2,-0.255552756000017));
#313173=CARTESIAN_POINT('Ctrl Pts',(-3.99936464200006,12.2,-0.255615689000015));
#313174=CARTESIAN_POINT('Ctrl Pts',(-3.99936464200006,5.2,-0.255615689000015));
#313175=CARTESIAN_POINT('Ctrl Pts',(-3.99936464200006,2.2,-0.255615689000015));
#313176=CARTESIAN_POINT('Ctrl Pts',(-3.99979817700006,12.2,-0.255680141000014));
#313177=CARTESIAN_POINT('Ctrl Pts',(-3.99979817700006,5.2,-0.255680141000014));
#313178=CARTESIAN_POINT('Ctrl Pts',(-3.99979817700006,2.2,-0.255680141000014));
#313179=CARTESIAN_POINT('Ctrl Pts',(-4.00023807300006,12.2,-0.255746125000016));
#313180=CARTESIAN_POINT('Ctrl Pts',(-4.00023807300006,5.2,-0.255746125000016));
#313181=CARTESIAN_POINT('Ctrl Pts',(-4.00023807300006,2.2,-0.255746125000016));
#313182=CARTESIAN_POINT('Ctrl Pts',(-4.00068431000006,12.2,-0.255813658000013));
#313183=CARTESIAN_POINT('Ctrl Pts',(-4.00068431000006,5.2,-0.255813658000013));
#313184=CARTESIAN_POINT('Ctrl Pts',(-4.00068431000006,2.2,-0.255813658000013));
#313185=CARTESIAN_POINT('Ctrl Pts',(-4.00113687200006,12.2,-0.255882751000014));
#313186=CARTESIAN_POINT('Ctrl Pts',(-4.00113687200006,5.2,-0.255882751000014));
#313187=CARTESIAN_POINT('Ctrl Pts',(-4.00113687200006,2.2,-0.255882751000014));
#313188=CARTESIAN_POINT('Ctrl Pts',(-4.00159574500006,12.2,-0.255953421000013));
#313189=CARTESIAN_POINT('Ctrl Pts',(-4.00159574500006,5.2,-0.255953421000013));
#313190=CARTESIAN_POINT('Ctrl Pts',(-4.00159574500006,2.2,-0.255953421000013));
#313191=CARTESIAN_POINT('Ctrl Pts',(-4.00206091100006,12.2,-0.256025681000014));
#313192=CARTESIAN_POINT('Ctrl Pts',(-4.00206091100006,5.2,-0.256025681000014));
#313193=CARTESIAN_POINT('Ctrl Pts',(-4.00206091100006,2.2,-0.256025681000014));
#313194=CARTESIAN_POINT('Ctrl Pts',(-4.00253235500006,12.2,-0.256099545000015));
#313195=CARTESIAN_POINT('Ctrl Pts',(-4.00253235500006,5.2,-0.256099545000015));
#313196=CARTESIAN_POINT('Ctrl Pts',(-4.00253235500006,2.2,-0.256099545000015));
#313197=CARTESIAN_POINT('Ctrl Pts',(-4.00301006000006,12.2,-0.256175026000012));
#313198=CARTESIAN_POINT('Ctrl Pts',(-4.00301006000006,5.2,-0.256175026000012));
#313199=CARTESIAN_POINT('Ctrl Pts',(-4.00301006000006,2.2,-0.256175026000012));
#313200=CARTESIAN_POINT('Ctrl Pts',(-4.00349401000006,12.2,-0.256252140000015));
#313201=CARTESIAN_POINT('Ctrl Pts',(-4.00349401000006,5.2,-0.256252140000015));
#313202=CARTESIAN_POINT('Ctrl Pts',(-4.00349401000006,2.2,-0.256252140000015));
#313203=CARTESIAN_POINT('Ctrl Pts',(-4.00398418900005,12.2,-0.256330899000012));
#313204=CARTESIAN_POINT('Ctrl Pts',(-4.00398418900005,5.2,-0.256330899000012));
#313205=CARTESIAN_POINT('Ctrl Pts',(-4.00398418900005,2.2,-0.256330899000012));
#313206=CARTESIAN_POINT('Ctrl Pts',(-4.00448058000006,12.2,-0.256411319000014));
#313207=CARTESIAN_POINT('Ctrl Pts',(-4.00448058000006,5.2,-0.256411319000014));
#313208=CARTESIAN_POINT('Ctrl Pts',(-4.00448058000006,2.2,-0.256411319000014));
#313209=CARTESIAN_POINT('Ctrl Pts',(-4.00498316900006,12.2,-0.256493413000012));
#313210=CARTESIAN_POINT('Ctrl Pts',(-4.00498316900006,5.2,-0.256493413000012));
#313211=CARTESIAN_POINT('Ctrl Pts',(-4.00498316900006,2.2,-0.256493413000012));
#313212=CARTESIAN_POINT('Ctrl Pts',(-4.00549193900006,12.2,-0.256577193000016));
#313213=CARTESIAN_POINT('Ctrl Pts',(-4.00549193900006,5.2,-0.256577193000016));
#313214=CARTESIAN_POINT('Ctrl Pts',(-4.00549193900006,2.2,-0.256577193000016));
#313215=CARTESIAN_POINT('Ctrl Pts',(-4.00600687400006,12.2,-0.256662674000014));
#313216=CARTESIAN_POINT('Ctrl Pts',(-4.00600687400006,5.2,-0.256662674000014));
#313217=CARTESIAN_POINT('Ctrl Pts',(-4.00600687400006,2.2,-0.256662674000014));
#313218=CARTESIAN_POINT('Ctrl Pts',(-4.00652795900006,12.2,-0.256749870000017));
#313219=CARTESIAN_POINT('Ctrl Pts',(-4.00652795900006,5.2,-0.256749870000017));
#313220=CARTESIAN_POINT('Ctrl Pts',(-4.00652795900006,2.2,-0.256749870000017));
#313221=CARTESIAN_POINT('Ctrl Pts',(-4.00705517700006,12.2,-0.256838795000016));
#313222=CARTESIAN_POINT('Ctrl Pts',(-4.00705517700006,5.2,-0.256838795000016));
#313223=CARTESIAN_POINT('Ctrl Pts',(-4.00705517700006,2.2,-0.256838795000016));
#313224=CARTESIAN_POINT('Ctrl Pts',(-4.00758851200006,12.2,-0.256929460000013));
#313225=CARTESIAN_POINT('Ctrl Pts',(-4.00758851200006,5.2,-0.256929460000013));
#313226=CARTESIAN_POINT('Ctrl Pts',(-4.00758851200006,2.2,-0.256929460000013));
#313227=CARTESIAN_POINT('Ctrl Pts',(-4.00812794900006,12.2,-0.257021880000017));
#313228=CARTESIAN_POINT('Ctrl Pts',(-4.00812794900006,5.2,-0.257021880000017));
#313229=CARTESIAN_POINT('Ctrl Pts',(-4.00812794900006,2.2,-0.257021880000017));
#313230=CARTESIAN_POINT('Ctrl Pts',(-4.00867347200006,12.2,-0.257116069000016));
#313231=CARTESIAN_POINT('Ctrl Pts',(-4.00867347200006,5.2,-0.257116069000016));
#313232=CARTESIAN_POINT('Ctrl Pts',(-4.00867347200006,2.2,-0.257116069000016));
#313233=CARTESIAN_POINT('Ctrl Pts',(-4.00922506700006,12.2,-0.257212040000017));
#313234=CARTESIAN_POINT('Ctrl Pts',(-4.00922506700006,5.2,-0.257212040000017));
#313235=CARTESIAN_POINT('Ctrl Pts',(-4.00922506700006,2.2,-0.257212040000017));
#313236=CARTESIAN_POINT('Ctrl Pts',(-4.00978271400006,12.2,-0.257309805000014));
#313237=CARTESIAN_POINT('Ctrl Pts',(-4.00978271400006,5.2,-0.257309805000014));
#313238=CARTESIAN_POINT('Ctrl Pts',(-4.00978271400006,2.2,-0.257309805000014));
#313239=CARTESIAN_POINT('Ctrl Pts',(-4.01034640200006,12.2,-0.257409379000015));
#313240=CARTESIAN_POINT('Ctrl Pts',(-4.01034640200006,5.2,-0.257409379000015));
#313241=CARTESIAN_POINT('Ctrl Pts',(-4.01034640200006,2.2,-0.257409379000015));
#313242=CARTESIAN_POINT('Ctrl Pts',(-4.01091611300005,12.2,-0.257510773000016));
#313243=CARTESIAN_POINT('Ctrl Pts',(-4.01091611300005,5.2,-0.257510773000016));
#313244=CARTESIAN_POINT('Ctrl Pts',(-4.01091611300005,2.2,-0.257510773000016));
#313245=CARTESIAN_POINT('Ctrl Pts',(-4.01149183100006,12.2,-0.257614001000013));
#313246=CARTESIAN_POINT('Ctrl Pts',(-4.01149183100006,5.2,-0.257614001000013));
#313247=CARTESIAN_POINT('Ctrl Pts',(-4.01149183100006,2.2,-0.257614001000013));
#313248=CARTESIAN_POINT('Ctrl Pts',(-4.01207354100006,12.2,-0.257719076000011));
#313249=CARTESIAN_POINT('Ctrl Pts',(-4.01207354100006,5.2,-0.257719076000011));
#313250=CARTESIAN_POINT('Ctrl Pts',(-4.01207354100006,2.2,-0.257719076000011));
#313251=CARTESIAN_POINT('Ctrl Pts',(-4.01266122900005,12.2,-0.257826012000013));
#313252=CARTESIAN_POINT('Ctrl Pts',(-4.01266122900005,5.2,-0.257826012000013));
#313253=CARTESIAN_POINT('Ctrl Pts',(-4.01266122900005,2.2,-0.257826012000013));
#313254=CARTESIAN_POINT('Ctrl Pts',(-4.01325487700006,12.2,-0.257934821000014));
#313255=CARTESIAN_POINT('Ctrl Pts',(-4.01325487700006,5.2,-0.257934821000014));
#313256=CARTESIAN_POINT('Ctrl Pts',(-4.01325487700006,2.2,-0.257934821000014));
#313257=CARTESIAN_POINT('Ctrl Pts',(-4.01385447100005,12.2,-0.258045516000016));
#313258=CARTESIAN_POINT('Ctrl Pts',(-4.01385447100005,5.2,-0.258045516000016));
#313259=CARTESIAN_POINT('Ctrl Pts',(-4.01385447100005,2.2,-0.258045516000016));
#313260=CARTESIAN_POINT('Ctrl Pts',(-4.01445999600006,12.2,-0.258158110000015));
#313261=CARTESIAN_POINT('Ctrl Pts',(-4.01445999600006,5.2,-0.258158110000015));
#313262=CARTESIAN_POINT('Ctrl Pts',(-4.01445999600006,2.2,-0.258158110000015));
#313263=CARTESIAN_POINT('Ctrl Pts',(-4.01507143400006,12.2,-0.258272613000017));
#313264=CARTESIAN_POINT('Ctrl Pts',(-4.01507143400006,5.2,-0.258272613000017));
#313265=CARTESIAN_POINT('Ctrl Pts',(-4.01507143400006,2.2,-0.258272613000017));
#313266=CARTESIAN_POINT('Ctrl Pts',(-4.01568877300006,12.2,-0.258389042000013));
#313267=CARTESIAN_POINT('Ctrl Pts',(-4.01568877300006,5.2,-0.258389042000013));
#313268=CARTESIAN_POINT('Ctrl Pts',(-4.01568877300006,2.2,-0.258389042000013));
#313269=CARTESIAN_POINT('Ctrl Pts',(-4.01631199600006,12.2,-0.258507407000015));
#313270=CARTESIAN_POINT('Ctrl Pts',(-4.01631199600006,5.2,-0.258507407000015));
#313271=CARTESIAN_POINT('Ctrl Pts',(-4.01631199600006,2.2,-0.258507407000015));
#313272=CARTESIAN_POINT('Ctrl Pts',(-4.01694108800006,12.2,-0.258627721000018));
#313273=CARTESIAN_POINT('Ctrl Pts',(-4.01694108800006,5.2,-0.258627721000018));
#313274=CARTESIAN_POINT('Ctrl Pts',(-4.01694108800006,2.2,-0.258627721000018));
#313275=CARTESIAN_POINT('Ctrl Pts',(-4.01757603300006,12.2,-0.258749997000014));
#313276=CARTESIAN_POINT('Ctrl Pts',(-4.01757603300006,5.2,-0.258749997000014));
#313277=CARTESIAN_POINT('Ctrl Pts',(-4.01757603300006,2.2,-0.258749997000014));
#313278=CARTESIAN_POINT('Ctrl Pts',(-4.01821681600006,12.2,-0.258874247000014));
#313279=CARTESIAN_POINT('Ctrl Pts',(-4.01821681600006,5.2,-0.258874247000014));
#313280=CARTESIAN_POINT('Ctrl Pts',(-4.01821681600006,2.2,-0.258874247000014));
#313281=CARTESIAN_POINT('Ctrl Pts',(-4.01886342200005,12.2,-0.259000484000014));
#313282=CARTESIAN_POINT('Ctrl Pts',(-4.01886342200005,5.2,-0.259000484000014));
#313283=CARTESIAN_POINT('Ctrl Pts',(-4.01886342200005,2.2,-0.259000484000014));
#313284=CARTESIAN_POINT('Ctrl Pts',(-4.01951583600006,12.2,-0.259128719000015));
#313285=CARTESIAN_POINT('Ctrl Pts',(-4.01951583600006,5.2,-0.259128719000015));
#313286=CARTESIAN_POINT('Ctrl Pts',(-4.01951583600006,2.2,-0.259128719000015));
#313287=CARTESIAN_POINT('Ctrl Pts',(-4.02017404300006,12.2,-0.259258965000013));
#313288=CARTESIAN_POINT('Ctrl Pts',(-4.02017404300006,5.2,-0.259258965000013));
#313289=CARTESIAN_POINT('Ctrl Pts',(-4.02017404300006,2.2,-0.259258965000013));
#313290=CARTESIAN_POINT('Ctrl Pts',(-4.02083802800006,12.2,-0.259391235000015));
#313291=CARTESIAN_POINT('Ctrl Pts',(-4.02083802800006,5.2,-0.259391235000015));
#313292=CARTESIAN_POINT('Ctrl Pts',(-4.02083802800006,2.2,-0.259391235000015));
#313293=CARTESIAN_POINT('Ctrl Pts',(-4.02150777400006,12.2,-0.259525539000016));
#313294=CARTESIAN_POINT('Ctrl Pts',(-4.02150777400006,5.2,-0.259525539000016));
#313295=CARTESIAN_POINT('Ctrl Pts',(-4.02150777400006,2.2,-0.259525539000016));
#313296=CARTESIAN_POINT('Ctrl Pts',(-4.02218326800006,12.2,-0.259661892000014));
#313297=CARTESIAN_POINT('Ctrl Pts',(-4.02218326800006,5.2,-0.259661892000014));
#313298=CARTESIAN_POINT('Ctrl Pts',(-4.02218326800006,2.2,-0.259661892000014));
#313299=CARTESIAN_POINT('Ctrl Pts',(-4.02286449500005,12.2,-0.259800303000013));
#313300=CARTESIAN_POINT('Ctrl Pts',(-4.02286449500005,5.2,-0.259800303000013));
#313301=CARTESIAN_POINT('Ctrl Pts',(-4.02286449500005,2.2,-0.259800303000013));
#313302=CARTESIAN_POINT('Ctrl Pts',(-4.02355143800006,12.2,-0.259940787000015));
#313303=CARTESIAN_POINT('Ctrl Pts',(-4.02355143800006,5.2,-0.259940787000015));
#313304=CARTESIAN_POINT('Ctrl Pts',(-4.02355143800006,2.2,-0.259940787000015));
#313305=CARTESIAN_POINT('Ctrl Pts',(-4.02424408400006,12.2,-0.260083353000016));
#313306=CARTESIAN_POINT('Ctrl Pts',(-4.02424408400006,5.2,-0.260083353000016));
#313307=CARTESIAN_POINT('Ctrl Pts',(-4.02424408400006,2.2,-0.260083353000016));
#313308=CARTESIAN_POINT('Ctrl Pts',(-4.02494241700006,12.2,-0.260228017000017));
#313309=CARTESIAN_POINT('Ctrl Pts',(-4.02494241700006,5.2,-0.260228017000017));
#313310=CARTESIAN_POINT('Ctrl Pts',(-4.02494241700006,2.2,-0.260228017000017));
#313311=CARTESIAN_POINT('Ctrl Pts',(-4.02564642300006,12.2,-0.260374786000015));
#313312=CARTESIAN_POINT('Ctrl Pts',(-4.02564642300006,5.2,-0.260374786000015));
#313313=CARTESIAN_POINT('Ctrl Pts',(-4.02564642300006,2.2,-0.260374786000015));
#313314=CARTESIAN_POINT('Ctrl Pts',(-4.02635608600006,12.2,-0.260523675000015));
#313315=CARTESIAN_POINT('Ctrl Pts',(-4.02635608600006,5.2,-0.260523675000015));
#313316=CARTESIAN_POINT('Ctrl Pts',(-4.02635608600006,2.2,-0.260523675000015));
#313317=CARTESIAN_POINT('Ctrl Pts',(-4.02707139100006,12.2,-0.260674696000014));
#313318=CARTESIAN_POINT('Ctrl Pts',(-4.02707139100006,5.2,-0.260674696000014));
#313319=CARTESIAN_POINT('Ctrl Pts',(-4.02707139100006,2.2,-0.260674696000014));
#313320=CARTESIAN_POINT('Ctrl Pts',(-4.02779232400006,12.2,-0.260827857000017));
#313321=CARTESIAN_POINT('Ctrl Pts',(-4.02779232400006,5.2,-0.260827857000017));
#313322=CARTESIAN_POINT('Ctrl Pts',(-4.02779232400006,2.2,-0.260827857000017));
#313323=CARTESIAN_POINT('Ctrl Pts',(-4.02851887100006,12.2,-0.260983174000016));
#313324=CARTESIAN_POINT('Ctrl Pts',(-4.02851887100006,5.2,-0.260983174000016));
#313325=CARTESIAN_POINT('Ctrl Pts',(-4.02851887100006,2.2,-0.260983174000016));
#313326=CARTESIAN_POINT('Ctrl Pts',(-4.02925101400006,12.2,-0.261140657000016));
#313327=CARTESIAN_POINT('Ctrl Pts',(-4.02925101400006,5.2,-0.261140657000016));
#313328=CARTESIAN_POINT('Ctrl Pts',(-4.02925101400006,2.2,-0.261140657000016));
#313329=CARTESIAN_POINT('Ctrl Pts',(-4.02998874200006,12.2,-0.261300316000015));
#313330=CARTESIAN_POINT('Ctrl Pts',(-4.02998874200006,5.2,-0.261300316000015));
#313331=CARTESIAN_POINT('Ctrl Pts',(-4.02998874200006,2.2,-0.261300316000015));
#313332=CARTESIAN_POINT('Ctrl Pts',(-4.03073203800006,12.2,-0.261462165000013));
#313333=CARTESIAN_POINT('Ctrl Pts',(-4.03073203800006,5.2,-0.261462165000013));
#313334=CARTESIAN_POINT('Ctrl Pts',(-4.03073203800006,2.2,-0.261462165000013));
#313335=CARTESIAN_POINT('Ctrl Pts',(-4.03148088800005,12.2,-0.261626214000015));
#313336=CARTESIAN_POINT('Ctrl Pts',(-4.03148088800005,5.2,-0.261626214000015));
#313337=CARTESIAN_POINT('Ctrl Pts',(-4.03148088800005,2.2,-0.261626214000015));
#313338=CARTESIAN_POINT('Ctrl Pts',(-4.03223527700006,12.2,-0.261792474000018));
#313339=CARTESIAN_POINT('Ctrl Pts',(-4.03223527700006,5.2,-0.261792474000018));
#313340=CARTESIAN_POINT('Ctrl Pts',(-4.03223527700006,2.2,-0.261792474000018));
#313341=CARTESIAN_POINT('Ctrl Pts',(-4.03299519000006,12.2,-0.261960957000014));
#313342=CARTESIAN_POINT('Ctrl Pts',(-4.03299519000006,5.2,-0.261960957000014));
#313343=CARTESIAN_POINT('Ctrl Pts',(-4.03299519000006,2.2,-0.261960957000014));
#313344=CARTESIAN_POINT('Ctrl Pts',(-4.03376061300006,12.2,-0.262131675000017));
#313345=CARTESIAN_POINT('Ctrl Pts',(-4.03376061300006,5.2,-0.262131675000017));
#313346=CARTESIAN_POINT('Ctrl Pts',(-4.03376061300006,2.2,-0.262131675000017));
#313347=CARTESIAN_POINT('Ctrl Pts',(-4.03453153200005,12.2,-0.262304639000015));
#313348=CARTESIAN_POINT('Ctrl Pts',(-4.03453153200005,5.2,-0.262304639000015));
#313349=CARTESIAN_POINT('Ctrl Pts',(-4.03453153200005,2.2,-0.262304639000015));
#313350=CARTESIAN_POINT('Ctrl Pts',(-4.03530793100006,12.2,-0.262479859000013));
#313351=CARTESIAN_POINT('Ctrl Pts',(-4.03530793100006,5.2,-0.262479859000013));
#313352=CARTESIAN_POINT('Ctrl Pts',(-4.03530793100006,2.2,-0.262479859000013));
#313353=CARTESIAN_POINT('Ctrl Pts',(-4.03608979700006,12.2,-0.262657346000013));
#313354=CARTESIAN_POINT('Ctrl Pts',(-4.03608979700006,5.2,-0.262657346000013));
#313355=CARTESIAN_POINT('Ctrl Pts',(-4.03608979700006,2.2,-0.262657346000013));
#313356=CARTESIAN_POINT('Ctrl Pts',(-4.03687711300006,12.2,-0.262837114000014));
#313357=CARTESIAN_POINT('Ctrl Pts',(-4.03687711300006,5.2,-0.262837114000014));
#313358=CARTESIAN_POINT('Ctrl Pts',(-4.03687711300006,2.2,-0.262837114000014));
#313359=CARTESIAN_POINT('Ctrl Pts',(-4.03766986700006,12.2,-0.263019170000014));
#313360=CARTESIAN_POINT('Ctrl Pts',(-4.03766986700006,5.2,-0.263019170000014));
#313361=CARTESIAN_POINT('Ctrl Pts',(-4.03766986700006,2.2,-0.263019170000014));
#313362=CARTESIAN_POINT('Ctrl Pts',(-4.03846804300006,12.2,-0.263203529000013));
#313363=CARTESIAN_POINT('Ctrl Pts',(-4.03846804300006,5.2,-0.263203529000013));
#313364=CARTESIAN_POINT('Ctrl Pts',(-4.03846804300006,2.2,-0.263203529000013));
#313365=CARTESIAN_POINT('Ctrl Pts',(-4.03927162800006,12.2,-0.263390198000018));
#313366=CARTESIAN_POINT('Ctrl Pts',(-4.03927162800006,5.2,-0.263390198000018));
#313367=CARTESIAN_POINT('Ctrl Pts',(-4.03927162800006,2.2,-0.263390198000018));
#313368=CARTESIAN_POINT('Ctrl Pts',(-4.04008060700006,12.2,-0.263579191000014));
#313369=CARTESIAN_POINT('Ctrl Pts',(-4.04008060700006,5.2,-0.263579191000014));
#313370=CARTESIAN_POINT('Ctrl Pts',(-4.04008060700006,2.2,-0.263579191000014));
#313371=CARTESIAN_POINT('Ctrl Pts',(-4.04089496400006,12.2,-0.263770518000013));
#313372=CARTESIAN_POINT('Ctrl Pts',(-4.04089496400006,5.2,-0.263770518000013));
#313373=CARTESIAN_POINT('Ctrl Pts',(-4.04089496400006,2.2,-0.263770518000013));
#313374=CARTESIAN_POINT('Ctrl Pts',(-4.04171468700006,12.2,-0.263964188000014));
#313375=CARTESIAN_POINT('Ctrl Pts',(-4.04171468700006,5.2,-0.263964188000014));
#313376=CARTESIAN_POINT('Ctrl Pts',(-4.04171468700006,2.2,-0.263964188000014));
#313377=CARTESIAN_POINT('Ctrl Pts',(-4.04253976000006,12.2,-0.264160215000011));
#313378=CARTESIAN_POINT('Ctrl Pts',(-4.04253976000006,5.2,-0.264160215000011));
#313379=CARTESIAN_POINT('Ctrl Pts',(-4.04253976000006,2.2,-0.264160215000011));
#313380=CARTESIAN_POINT('Ctrl Pts',(-4.04337016900006,12.2,-0.264358608000013));
#313381=CARTESIAN_POINT('Ctrl Pts',(-4.04337016900006,5.2,-0.264358608000013));
#313382=CARTESIAN_POINT('Ctrl Pts',(-4.04337016900006,2.2,-0.264358608000013));
#313383=CARTESIAN_POINT('Ctrl Pts',(-4.04420590100006,12.2,-0.264559377000015));
#313384=CARTESIAN_POINT('Ctrl Pts',(-4.04420590100006,5.2,-0.264559377000015));
#313385=CARTESIAN_POINT('Ctrl Pts',(-4.04420590100006,2.2,-0.264559377000015));
#313386=CARTESIAN_POINT('Ctrl Pts',(-4.04504693900006,12.2,-0.264762533000016));
#313387=CARTESIAN_POINT('Ctrl Pts',(-4.04504693900006,5.2,-0.264762533000016));
#313388=CARTESIAN_POINT('Ctrl Pts',(-4.04504693900006,2.2,-0.264762533000016));
#313389=CARTESIAN_POINT('Ctrl Pts',(-4.04589327100005,12.2,-0.264968088000015));
#313390=CARTESIAN_POINT('Ctrl Pts',(-4.04589327100005,5.2,-0.264968088000015));
#313391=CARTESIAN_POINT('Ctrl Pts',(-4.04589327100005,2.2,-0.264968088000015));
#313392=CARTESIAN_POINT('Ctrl Pts',(-4.04674488400006,12.2,-0.265176050000013));
#313393=CARTESIAN_POINT('Ctrl Pts',(-4.04674488400006,5.2,-0.265176050000013));
#313394=CARTESIAN_POINT('Ctrl Pts',(-4.04674488400006,2.2,-0.265176050000013));
#313395=CARTESIAN_POINT('Ctrl Pts',(-4.04760176000006,12.2,-0.265386433000017));
#313396=CARTESIAN_POINT('Ctrl Pts',(-4.04760176000006,5.2,-0.265386433000017));
#313397=CARTESIAN_POINT('Ctrl Pts',(-4.04760176000006,2.2,-0.265386433000017));
#313398=CARTESIAN_POINT('Ctrl Pts',(-4.04846388700006,12.2,-0.265599244000012));
#313399=CARTESIAN_POINT('Ctrl Pts',(-4.04846388700006,5.2,-0.265599244000012));
#313400=CARTESIAN_POINT('Ctrl Pts',(-4.04846388700006,2.2,-0.265599244000012));
#313401=CARTESIAN_POINT('Ctrl Pts',(-4.04933125200006,12.2,-0.265814494000014));
#313402=CARTESIAN_POINT('Ctrl Pts',(-4.04933125200006,5.2,-0.265814494000014));
#313403=CARTESIAN_POINT('Ctrl Pts',(-4.04933125200006,2.2,-0.265814494000014));
#313404=CARTESIAN_POINT('Ctrl Pts',(-4.05020383900006,12.2,-0.266032196000014));
#313405=CARTESIAN_POINT('Ctrl Pts',(-4.05020383900006,5.2,-0.266032196000014));
#313406=CARTESIAN_POINT('Ctrl Pts',(-4.05020383900006,2.2,-0.266032196000014));
#313407=CARTESIAN_POINT('Ctrl Pts',(-4.05108163400006,12.2,-0.266252357000014));
#313408=CARTESIAN_POINT('Ctrl Pts',(-4.05108163400006,5.2,-0.266252357000014));
#313409=CARTESIAN_POINT('Ctrl Pts',(-4.05108163400006,2.2,-0.266252357000014));
#313410=CARTESIAN_POINT('Ctrl Pts',(-4.05196462400006,12.2,-0.266474989000014));
#313411=CARTESIAN_POINT('Ctrl Pts',(-4.05196462400006,5.2,-0.266474989000014));
#313412=CARTESIAN_POINT('Ctrl Pts',(-4.05196462400006,2.2,-0.266474989000014));
#313413=CARTESIAN_POINT('Ctrl Pts',(-4.05285279300006,12.2,-0.266700102000015));
#313414=CARTESIAN_POINT('Ctrl Pts',(-4.05285279300006,5.2,-0.266700102000015));
#313415=CARTESIAN_POINT('Ctrl Pts',(-4.05285279300006,2.2,-0.266700102000015));
#313416=CARTESIAN_POINT('Ctrl Pts',(-4.05374613000006,12.2,-0.266927706000013));
#313417=CARTESIAN_POINT('Ctrl Pts',(-4.05374613000006,5.2,-0.266927706000013));
#313418=CARTESIAN_POINT('Ctrl Pts',(-4.05374613000006,2.2,-0.266927706000013));
#313419=CARTESIAN_POINT('Ctrl Pts',(-4.05464461800006,12.2,-0.267157813000014));
#313420=CARTESIAN_POINT('Ctrl Pts',(-4.05464461800006,5.2,-0.267157813000014));
#313421=CARTESIAN_POINT('Ctrl Pts',(-4.05464461800006,2.2,-0.267157813000014));
#313422=CARTESIAN_POINT('Ctrl Pts',(-4.05554824500006,12.2,-0.267390429000014));
#313423=CARTESIAN_POINT('Ctrl Pts',(-4.05554824500006,5.2,-0.267390429000014));
#313424=CARTESIAN_POINT('Ctrl Pts',(-4.05554824500006,2.2,-0.267390429000014));
#313425=CARTESIAN_POINT('Ctrl Pts',(-4.05645699600006,12.2,-0.267625566000014));
#313426=CARTESIAN_POINT('Ctrl Pts',(-4.05645699600006,5.2,-0.267625566000014));
#313427=CARTESIAN_POINT('Ctrl Pts',(-4.05645699600006,2.2,-0.267625566000014));
#313428=CARTESIAN_POINT('Ctrl Pts',(-4.05737085800006,12.2,-0.267863236000014));
#313429=CARTESIAN_POINT('Ctrl Pts',(-4.05737085800006,5.2,-0.267863236000014));
#313430=CARTESIAN_POINT('Ctrl Pts',(-4.05737085800006,2.2,-0.267863236000014));
#313431=CARTESIAN_POINT('Ctrl Pts',(-4.05828981600005,12.2,-0.268103446000012));
#313432=CARTESIAN_POINT('Ctrl Pts',(-4.05828981600005,5.2,-0.268103446000012));
#313433=CARTESIAN_POINT('Ctrl Pts',(-4.05828981600005,2.2,-0.268103446000012));
#313434=CARTESIAN_POINT('Ctrl Pts',(-4.05921385700006,12.2,-0.268346208000012));
#313435=CARTESIAN_POINT('Ctrl Pts',(-4.05921385700006,5.2,-0.268346208000012));
#313436=CARTESIAN_POINT('Ctrl Pts',(-4.05921385700006,2.2,-0.268346208000012));
#313437=CARTESIAN_POINT('Ctrl Pts',(-4.06014296600006,12.2,-0.268591531000015));
#313438=CARTESIAN_POINT('Ctrl Pts',(-4.06014296600006,5.2,-0.268591531000015));
#313439=CARTESIAN_POINT('Ctrl Pts',(-4.06014296600006,2.2,-0.268591531000015));
#313440=CARTESIAN_POINT('Ctrl Pts',(-4.06107713000006,12.2,-0.268839425000014));
#313441=CARTESIAN_POINT('Ctrl Pts',(-4.06107713000006,5.2,-0.268839425000014));
#313442=CARTESIAN_POINT('Ctrl Pts',(-4.06107713000006,2.2,-0.268839425000014));
#313443=CARTESIAN_POINT('Ctrl Pts',(-4.06201633600006,12.2,-0.269089899000012));
#313444=CARTESIAN_POINT('Ctrl Pts',(-4.06201633600006,5.2,-0.269089899000012));
#313445=CARTESIAN_POINT('Ctrl Pts',(-4.06201633600006,2.2,-0.269089899000012));
#313446=CARTESIAN_POINT('Ctrl Pts',(-4.06296056800006,12.2,-0.269342965000017));
#313447=CARTESIAN_POINT('Ctrl Pts',(-4.06296056800006,5.2,-0.269342965000017));
#313448=CARTESIAN_POINT('Ctrl Pts',(-4.06296056800006,2.2,-0.269342965000017));
#313449=CARTESIAN_POINT('Ctrl Pts',(-4.06390981400006,12.2,-0.269598630000014));
#313450=CARTESIAN_POINT('Ctrl Pts',(-4.06390981400006,5.2,-0.269598630000014));
#313451=CARTESIAN_POINT('Ctrl Pts',(-4.06390981400006,2.2,-0.269598630000014));
#313452=CARTESIAN_POINT('Ctrl Pts',(-4.06486406100006,12.2,-0.269856904000014));
#313453=CARTESIAN_POINT('Ctrl Pts',(-4.06486406100006,5.2,-0.269856904000014));
#313454=CARTESIAN_POINT('Ctrl Pts',(-4.06486406100006,2.2,-0.269856904000014));
#313455=CARTESIAN_POINT('Ctrl Pts',(-4.06582329200006,12.2,-0.270117798000014));
#313456=CARTESIAN_POINT('Ctrl Pts',(-4.06582329200006,5.2,-0.270117798000014));
#313457=CARTESIAN_POINT('Ctrl Pts',(-4.06582329200006,2.2,-0.270117798000014));
#313458=CARTESIAN_POINT('Ctrl Pts',(-4.06678749700006,12.2,-0.270381321000013));
#313459=CARTESIAN_POINT('Ctrl Pts',(-4.06678749700006,5.2,-0.270381321000013));
#313460=CARTESIAN_POINT('Ctrl Pts',(-4.06678749700006,2.2,-0.270381321000013));
#313461=CARTESIAN_POINT('Ctrl Pts',(-4.06775666000006,12.2,-0.270647483000013));
#313462=CARTESIAN_POINT('Ctrl Pts',(-4.06775666000006,5.2,-0.270647483000013));
#313463=CARTESIAN_POINT('Ctrl Pts',(-4.06775666000006,2.2,-0.270647483000013));
#313464=CARTESIAN_POINT('Ctrl Pts',(-4.06873076700006,12.2,-0.270916292000014));
#313465=CARTESIAN_POINT('Ctrl Pts',(-4.06873076700006,5.2,-0.270916292000014));
#313466=CARTESIAN_POINT('Ctrl Pts',(-4.06873076700006,2.2,-0.270916292000014));
#313467=CARTESIAN_POINT('Ctrl Pts',(-4.06970980600006,12.2,-0.271187759000018));
#313468=CARTESIAN_POINT('Ctrl Pts',(-4.06970980600006,5.2,-0.271187759000018));
#313469=CARTESIAN_POINT('Ctrl Pts',(-4.06970980600006,2.2,-0.271187759000018));
#313470=CARTESIAN_POINT('Ctrl Pts',(-4.07069376400006,12.2,-0.271461893000016));
#313471=CARTESIAN_POINT('Ctrl Pts',(-4.07069376400006,5.2,-0.271461893000016));
#313472=CARTESIAN_POINT('Ctrl Pts',(-4.07069376400006,2.2,-0.271461893000016));
#313473=CARTESIAN_POINT('Ctrl Pts',(-4.07168262500006,12.2,-0.271738703000013));
#313474=CARTESIAN_POINT('Ctrl Pts',(-4.07168262500006,5.2,-0.271738703000013));
#313475=CARTESIAN_POINT('Ctrl Pts',(-4.07168262500006,2.2,-0.271738703000013));
#313476=CARTESIAN_POINT('Ctrl Pts',(-4.07267637700006,12.2,-0.272018198000015));
#313477=CARTESIAN_POINT('Ctrl Pts',(-4.07267637700006,5.2,-0.272018198000015));
#313478=CARTESIAN_POINT('Ctrl Pts',(-4.07267637700006,2.2,-0.272018198000015));
#313479=CARTESIAN_POINT('Ctrl Pts',(-4.07367500500006,12.2,-0.272300389000013));
#313480=CARTESIAN_POINT('Ctrl Pts',(-4.07367500500006,5.2,-0.272300389000013));
#313481=CARTESIAN_POINT('Ctrl Pts',(-4.07367500500006,2.2,-0.272300389000013));
#313482=CARTESIAN_POINT('Ctrl Pts',(-4.07467849800006,12.2,-0.272585283000013));
#313483=CARTESIAN_POINT('Ctrl Pts',(-4.07467849800006,5.2,-0.272585283000013));
#313484=CARTESIAN_POINT('Ctrl Pts',(-4.07467849800006,2.2,-0.272585283000013));
#313485=CARTESIAN_POINT('Ctrl Pts',(-4.07568684000006,12.2,-0.272872891000016));
#313486=CARTESIAN_POINT('Ctrl Pts',(-4.07568684000006,5.2,-0.272872891000016));
#313487=CARTESIAN_POINT('Ctrl Pts',(-4.07568684000006,2.2,-0.272872891000016));
#313488=CARTESIAN_POINT('Ctrl Pts',(-4.07670001800006,12.2,-0.273163221000012));
#313489=CARTESIAN_POINT('Ctrl Pts',(-4.07670001800006,5.2,-0.273163221000012));
#313490=CARTESIAN_POINT('Ctrl Pts',(-4.07670001800006,2.2,-0.273163221000012));
#313491=CARTESIAN_POINT('Ctrl Pts',(-4.07771802000005,12.2,-0.273456282000013));
#313492=CARTESIAN_POINT('Ctrl Pts',(-4.07771802000005,5.2,-0.273456282000013));
#313493=CARTESIAN_POINT('Ctrl Pts',(-4.07771802000005,2.2,-0.273456282000013));
#313494=CARTESIAN_POINT('Ctrl Pts',(-4.07874083200006,12.2,-0.273752085000014));
#313495=CARTESIAN_POINT('Ctrl Pts',(-4.07874083200006,5.2,-0.273752085000014));
#313496=CARTESIAN_POINT('Ctrl Pts',(-4.07874083200006,2.2,-0.273752085000014));
#313497=CARTESIAN_POINT('Ctrl Pts',(-4.07976843800006,12.2,-0.274050636000016));
#313498=CARTESIAN_POINT('Ctrl Pts',(-4.07976843800006,5.2,-0.274050636000016));
#313499=CARTESIAN_POINT('Ctrl Pts',(-4.07976843800006,2.2,-0.274050636000016));
#313500=CARTESIAN_POINT('Ctrl Pts',(-4.08080082900006,12.2,-0.274351947000016));
#313501=CARTESIAN_POINT('Ctrl Pts',(-4.08080082900006,5.2,-0.274351947000016));
#313502=CARTESIAN_POINT('Ctrl Pts',(-4.08080082900006,2.2,-0.274351947000016));
#313503=CARTESIAN_POINT('Ctrl Pts',(-4.08183798800006,12.2,-0.274656025000013));
#313504=CARTESIAN_POINT('Ctrl Pts',(-4.08183798800006,5.2,-0.274656025000013));
#313505=CARTESIAN_POINT('Ctrl Pts',(-4.08183798800006,2.2,-0.274656025000013));
#313506=CARTESIAN_POINT('Ctrl Pts',(-4.08287990400006,12.2,-0.274962880000014));
#313507=CARTESIAN_POINT('Ctrl Pts',(-4.08287990400006,5.2,-0.274962880000014));
#313508=CARTESIAN_POINT('Ctrl Pts',(-4.08287990400006,2.2,-0.274962880000014));
#313509=CARTESIAN_POINT('Ctrl Pts',(-4.08392656300006,12.2,-0.275272521000014));
#313510=CARTESIAN_POINT('Ctrl Pts',(-4.08392656300006,5.2,-0.275272521000014));
#313511=CARTESIAN_POINT('Ctrl Pts',(-4.08392656300006,2.2,-0.275272521000014));
#313512=CARTESIAN_POINT('Ctrl Pts',(-4.08497795100006,12.2,-0.275584955000014));
#313513=CARTESIAN_POINT('Ctrl Pts',(-4.08497795100006,5.2,-0.275584955000014));
#313514=CARTESIAN_POINT('Ctrl Pts',(-4.08497795100006,2.2,-0.275584955000014));
#313515=CARTESIAN_POINT('Ctrl Pts',(-4.08603405500005,12.2,-0.275900193000016));
#313516=CARTESIAN_POINT('Ctrl Pts',(-4.08603405500005,5.2,-0.275900193000016));
#313517=CARTESIAN_POINT('Ctrl Pts',(-4.08603405500005,2.2,-0.275900193000016));
#313518=CARTESIAN_POINT('Ctrl Pts',(-4.08709486100006,12.2,-0.276218243000015));
#313519=CARTESIAN_POINT('Ctrl Pts',(-4.08709486100006,5.2,-0.276218243000015));
#313520=CARTESIAN_POINT('Ctrl Pts',(-4.08709486100006,2.2,-0.276218243000015));
#313521=CARTESIAN_POINT('Ctrl Pts',(-4.08816035700006,12.2,-0.276539114000016));
#313522=CARTESIAN_POINT('Ctrl Pts',(-4.08816035700006,5.2,-0.276539114000016));
#313523=CARTESIAN_POINT('Ctrl Pts',(-4.08816035700006,2.2,-0.276539114000016));
#313524=CARTESIAN_POINT('Ctrl Pts',(-4.08923052900006,12.2,-0.276862813000012));
#313525=CARTESIAN_POINT('Ctrl Pts',(-4.08923052900006,5.2,-0.276862813000012));
#313526=CARTESIAN_POINT('Ctrl Pts',(-4.08923052900006,2.2,-0.276862813000012));
#313527=CARTESIAN_POINT('Ctrl Pts',(-4.09030536500006,12.2,-0.277189351000011));
#313528=CARTESIAN_POINT('Ctrl Pts',(-4.09030536500006,5.2,-0.277189351000011));
#313529=CARTESIAN_POINT('Ctrl Pts',(-4.09030536500006,2.2,-0.277189351000011));
#313530=CARTESIAN_POINT('Ctrl Pts',(-4.09138485100006,12.2,-0.277518736000015));
#313531=CARTESIAN_POINT('Ctrl Pts',(-4.09138485100006,5.2,-0.277518736000015));
#313532=CARTESIAN_POINT('Ctrl Pts',(-4.09138485100006,2.2,-0.277518736000015));
#313533=CARTESIAN_POINT('Ctrl Pts',(-4.09246897300005,12.2,-0.277850975000016));
#313534=CARTESIAN_POINT('Ctrl Pts',(-4.09246897300005,5.2,-0.277850975000016));
#313535=CARTESIAN_POINT('Ctrl Pts',(-4.09246897300005,2.2,-0.277850975000016));
#313536=CARTESIAN_POINT('Ctrl Pts',(-4.09355771900006,12.2,-0.278186080000014));
#313537=CARTESIAN_POINT('Ctrl Pts',(-4.09355771900006,5.2,-0.278186080000014));
#313538=CARTESIAN_POINT('Ctrl Pts',(-4.09355771900006,2.2,-0.278186080000014));
#313539=CARTESIAN_POINT('Ctrl Pts',(-4.09465107500006,12.2,-0.278524055000013));
#313540=CARTESIAN_POINT('Ctrl Pts',(-4.09465107500006,5.2,-0.278524055000013));
#313541=CARTESIAN_POINT('Ctrl Pts',(-4.09465107500006,2.2,-0.278524055000013));
#313542=CARTESIAN_POINT('Ctrl Pts',(-4.09574902900006,12.2,-0.278864911000016));
#313543=CARTESIAN_POINT('Ctrl Pts',(-4.09574902900006,5.2,-0.278864911000016));
#313544=CARTESIAN_POINT('Ctrl Pts',(-4.09574902900006,2.2,-0.278864911000016));
#313545=CARTESIAN_POINT('Ctrl Pts',(-4.09685156700006,12.2,-0.279208658000014));
#313546=CARTESIAN_POINT('Ctrl Pts',(-4.09685156700006,5.2,-0.279208658000014));
#313547=CARTESIAN_POINT('Ctrl Pts',(-4.09685156700006,2.2,-0.279208658000014));
#313548=CARTESIAN_POINT('Ctrl Pts',(-4.09795867600006,12.2,-0.279555301000016));
#313549=CARTESIAN_POINT('Ctrl Pts',(-4.09795867600006,5.2,-0.279555301000016));
#313550=CARTESIAN_POINT('Ctrl Pts',(-4.09795867600006,2.2,-0.279555301000016));
#313551=CARTESIAN_POINT('Ctrl Pts',(-4.09907034300006,12.2,-0.279904851000015));
#313552=CARTESIAN_POINT('Ctrl Pts',(-4.09907034300006,5.2,-0.279904851000015));
#313553=CARTESIAN_POINT('Ctrl Pts',(-4.09907034300006,2.2,-0.279904851000015));
#313554=CARTESIAN_POINT('Ctrl Pts',(-4.10018655600005,12.2,-0.280257314000014));
#313555=CARTESIAN_POINT('Ctrl Pts',(-4.10018655600005,5.2,-0.280257314000014));
#313556=CARTESIAN_POINT('Ctrl Pts',(-4.10018655600005,2.2,-0.280257314000014));
#313557=CARTESIAN_POINT('Ctrl Pts',(-4.10130730000006,12.2,-0.280612701000016));
#313558=CARTESIAN_POINT('Ctrl Pts',(-4.10130730000006,5.2,-0.280612701000016));
#313559=CARTESIAN_POINT('Ctrl Pts',(-4.10130730000006,2.2,-0.280612701000016));
#313560=CARTESIAN_POINT('Ctrl Pts',(-4.10243256400006,12.2,-0.280971018000016));
#313561=CARTESIAN_POINT('Ctrl Pts',(-4.10243256400006,5.2,-0.280971018000016));
#313562=CARTESIAN_POINT('Ctrl Pts',(-4.10243256400006,2.2,-0.280971018000016));
#313563=CARTESIAN_POINT('Ctrl Pts',(-4.10356233300006,12.2,-0.281332274000015));
#313564=CARTESIAN_POINT('Ctrl Pts',(-4.10356233300006,5.2,-0.281332274000015));
#313565=CARTESIAN_POINT('Ctrl Pts',(-4.10356233300006,2.2,-0.281332274000015));
#313566=CARTESIAN_POINT('Ctrl Pts',(-4.10469659600006,12.2,-0.281696478000013));
#313567=CARTESIAN_POINT('Ctrl Pts',(-4.10469659600006,5.2,-0.281696478000013));
#313568=CARTESIAN_POINT('Ctrl Pts',(-4.10469659600006,2.2,-0.281696478000013));
#313569=CARTESIAN_POINT('Ctrl Pts',(-4.10583533900006,12.2,-0.282063637000016));
#313570=CARTESIAN_POINT('Ctrl Pts',(-4.10583533900006,5.2,-0.282063637000016));
#313571=CARTESIAN_POINT('Ctrl Pts',(-4.10583533900006,2.2,-0.282063637000016));
#313572=CARTESIAN_POINT('Ctrl Pts',(-4.10697855000006,12.2,-0.282433760000016));
#313573=CARTESIAN_POINT('Ctrl Pts',(-4.10697855000006,5.2,-0.282433760000016));
#313574=CARTESIAN_POINT('Ctrl Pts',(-4.10697855000006,2.2,-0.282433760000016));
#313575=CARTESIAN_POINT('Ctrl Pts',(-4.10812621400006,12.2,-0.282806853000017));
#313576=CARTESIAN_POINT('Ctrl Pts',(-4.10812621400006,5.2,-0.282806853000017));
#313577=CARTESIAN_POINT('Ctrl Pts',(-4.10812621400006,2.2,-0.282806853000017));
#313578=CARTESIAN_POINT('Ctrl Pts',(-4.10927832100006,12.2,-0.283182927000016));
#313579=CARTESIAN_POINT('Ctrl Pts',(-4.10927832100006,5.2,-0.283182927000016));
#313580=CARTESIAN_POINT('Ctrl Pts',(-4.10927832100006,2.2,-0.283182927000016));
#313581=CARTESIAN_POINT('Ctrl Pts',(-4.11043485600006,12.2,-0.283561988000014));
#313582=CARTESIAN_POINT('Ctrl Pts',(-4.11043485600006,5.2,-0.283561988000014));
#313583=CARTESIAN_POINT('Ctrl Pts',(-4.11043485600006,2.2,-0.283561988000014));
#313584=CARTESIAN_POINT('Ctrl Pts',(-4.11159580800006,12.2,-0.283944045000015));
#313585=CARTESIAN_POINT('Ctrl Pts',(-4.11159580800006,5.2,-0.283944045000015));
#313586=CARTESIAN_POINT('Ctrl Pts',(-4.11159580800006,2.2,-0.283944045000015));
#313587=CARTESIAN_POINT('Ctrl Pts',(-4.11276116200006,12.2,-0.284329106000012));
#313588=CARTESIAN_POINT('Ctrl Pts',(-4.11276116200006,5.2,-0.284329106000012));
#313589=CARTESIAN_POINT('Ctrl Pts',(-4.11276116200006,2.2,-0.284329106000012));
#313590=CARTESIAN_POINT('Ctrl Pts',(-4.11393090500006,12.2,-0.284717178000014));
#313591=CARTESIAN_POINT('Ctrl Pts',(-4.11393090500006,5.2,-0.284717178000014));
#313592=CARTESIAN_POINT('Ctrl Pts',(-4.11393090500006,2.2,-0.284717178000014));
#313593=CARTESIAN_POINT('Ctrl Pts',(-4.11510502700006,12.2,-0.285108269000016));
#313594=CARTESIAN_POINT('Ctrl Pts',(-4.11510502700006,5.2,-0.285108269000016));
#313595=CARTESIAN_POINT('Ctrl Pts',(-4.11510502700006,2.2,-0.285108269000016));
#313596=CARTESIAN_POINT('Ctrl Pts',(-4.11628351300006,12.2,-0.285502388000012));
#313597=CARTESIAN_POINT('Ctrl Pts',(-4.11628351300006,5.2,-0.285502388000012));
#313598=CARTESIAN_POINT('Ctrl Pts',(-4.11628351300006,2.2,-0.285502388000012));
#313599=CARTESIAN_POINT('Ctrl Pts',(-4.11746635200006,12.2,-0.285899541000014));
#313600=CARTESIAN_POINT('Ctrl Pts',(-4.11746635200006,5.2,-0.285899541000014));
#313601=CARTESIAN_POINT('Ctrl Pts',(-4.11746635200006,2.2,-0.285899541000014));
#313602=CARTESIAN_POINT('Ctrl Pts',(-4.11865353000006,12.2,-0.286299737000015));
#313603=CARTESIAN_POINT('Ctrl Pts',(-4.11865353000006,5.2,-0.286299737000015));
#313604=CARTESIAN_POINT('Ctrl Pts',(-4.11865353000006,2.2,-0.286299737000015));
#313605=CARTESIAN_POINT('Ctrl Pts',(-4.11984503400006,12.2,-0.286702984000016));
#313606=CARTESIAN_POINT('Ctrl Pts',(-4.11984503400006,5.2,-0.286702984000016));
#313607=CARTESIAN_POINT('Ctrl Pts',(-4.11984503400006,2.2,-0.286702984000016));
#313608=CARTESIAN_POINT('Ctrl Pts',(-4.12104085200006,12.2,-0.287109289000016));
#313609=CARTESIAN_POINT('Ctrl Pts',(-4.12104085200006,5.2,-0.287109289000016));
#313610=CARTESIAN_POINT('Ctrl Pts',(-4.12104085200006,2.2,-0.287109289000016));
#313611=CARTESIAN_POINT('Ctrl Pts',(-4.12224097100006,12.2,-0.287518659000017));
#313612=CARTESIAN_POINT('Ctrl Pts',(-4.12224097100006,5.2,-0.287518659000017));
#313613=CARTESIAN_POINT('Ctrl Pts',(-4.12224097100006,2.2,-0.287518659000017));
#313614=CARTESIAN_POINT('Ctrl Pts',(-4.12344537900006,12.2,-0.287931103000014));
#313615=CARTESIAN_POINT('Ctrl Pts',(-4.12344537900006,5.2,-0.287931103000014));
#313616=CARTESIAN_POINT('Ctrl Pts',(-4.12344537900006,2.2,-0.287931103000014));
#313617=CARTESIAN_POINT('Ctrl Pts',(-4.12465406200006,12.2,-0.288346629000014));
#313618=CARTESIAN_POINT('Ctrl Pts',(-4.12465406200006,5.2,-0.288346629000014));
#313619=CARTESIAN_POINT('Ctrl Pts',(-4.12465406200006,2.2,-0.288346629000014));
#313620=CARTESIAN_POINT('Ctrl Pts',(-4.12586700900006,12.2,-0.288765242000015));
#313621=CARTESIAN_POINT('Ctrl Pts',(-4.12586700900006,5.2,-0.288765242000015));
#313622=CARTESIAN_POINT('Ctrl Pts',(-4.12586700900006,2.2,-0.288765242000015));
#313623=CARTESIAN_POINT('Ctrl Pts',(-4.12708420700006,12.2,-0.289186952000016));
#313624=CARTESIAN_POINT('Ctrl Pts',(-4.12708420700006,5.2,-0.289186952000016));
#313625=CARTESIAN_POINT('Ctrl Pts',(-4.12708420700006,2.2,-0.289186952000016));
#313626=CARTESIAN_POINT('Ctrl Pts',(-4.12830564200006,12.2,-0.289611766000015));
#313627=CARTESIAN_POINT('Ctrl Pts',(-4.12830564200006,5.2,-0.289611766000015));
#313628=CARTESIAN_POINT('Ctrl Pts',(-4.12830564200006,2.2,-0.289611766000015));
#313629=CARTESIAN_POINT('Ctrl Pts',(-4.12953130400005,12.2,-0.290039691000015));
#313630=CARTESIAN_POINT('Ctrl Pts',(-4.12953130400005,5.2,-0.290039691000015));
#313631=CARTESIAN_POINT('Ctrl Pts',(-4.12953130400005,2.2,-0.290039691000015));
#313632=CARTESIAN_POINT('Ctrl Pts',(-4.13076117800006,12.2,-0.290470733000014));
#313633=CARTESIAN_POINT('Ctrl Pts',(-4.13076117800006,5.2,-0.290470733000014));
#313634=CARTESIAN_POINT('Ctrl Pts',(-4.13076117800006,2.2,-0.290470733000014));
#313635=CARTESIAN_POINT('Ctrl Pts',(-4.13199525200006,12.2,-0.290904902000015));
#313636=CARTESIAN_POINT('Ctrl Pts',(-4.13199525200006,5.2,-0.290904902000015));
#313637=CARTESIAN_POINT('Ctrl Pts',(-4.13199525200006,2.2,-0.290904902000015));
#313638=CARTESIAN_POINT('Ctrl Pts',(-4.13323351500006,12.2,-0.291342204000014));
#313639=CARTESIAN_POINT('Ctrl Pts',(-4.13323351500006,5.2,-0.291342204000014));
#313640=CARTESIAN_POINT('Ctrl Pts',(-4.13323351500006,2.2,-0.291342204000014));
#313641=CARTESIAN_POINT('Ctrl Pts',(-4.13447595200005,12.2,-0.291782647000014));
#313642=CARTESIAN_POINT('Ctrl Pts',(-4.13447595200005,5.2,-0.291782647000014));
#313643=CARTESIAN_POINT('Ctrl Pts',(-4.13447595200005,2.2,-0.291782647000014));
#313644=CARTESIAN_POINT('Ctrl Pts',(-4.13572255400006,12.2,-0.292226238000013));
#313645=CARTESIAN_POINT('Ctrl Pts',(-4.13572255400006,5.2,-0.292226238000013));
#313646=CARTESIAN_POINT('Ctrl Pts',(-4.13572255400006,2.2,-0.292226238000013));
#313647=CARTESIAN_POINT('Ctrl Pts',(-4.13697330500006,12.2,-0.292672984000015));
#313648=CARTESIAN_POINT('Ctrl Pts',(-4.13697330500006,5.2,-0.292672984000015));
#313649=CARTESIAN_POINT('Ctrl Pts',(-4.13697330500006,2.2,-0.292672984000015));
#313650=CARTESIAN_POINT('Ctrl Pts',(-4.13822819500006,12.2,-0.293122892000017));
#313651=CARTESIAN_POINT('Ctrl Pts',(-4.13822819500006,5.2,-0.293122892000017));
#313652=CARTESIAN_POINT('Ctrl Pts',(-4.13822819500006,2.2,-0.293122892000017));
#313653=CARTESIAN_POINT('Ctrl Pts',(-4.13948721100006,12.2,-0.293575970000015));
#313654=CARTESIAN_POINT('Ctrl Pts',(-4.13948721100006,5.2,-0.293575970000015));
#313655=CARTESIAN_POINT('Ctrl Pts',(-4.13948721100006,2.2,-0.293575970000015));
#313656=CARTESIAN_POINT('Ctrl Pts',(-4.14075033900006,12.2,-0.294032225000014));
#313657=CARTESIAN_POINT('Ctrl Pts',(-4.14075033900006,5.2,-0.294032225000014));
#313658=CARTESIAN_POINT('Ctrl Pts',(-4.14075033900006,2.2,-0.294032225000014));
#313659=CARTESIAN_POINT('Ctrl Pts',(-4.14201756800006,12.2,-0.294491663000014));
#313660=CARTESIAN_POINT('Ctrl Pts',(-4.14201756800006,5.2,-0.294491663000014));
#313661=CARTESIAN_POINT('Ctrl Pts',(-4.14201756800006,2.2,-0.294491663000014));
#313662=CARTESIAN_POINT('Ctrl Pts',(-4.14328888700005,12.2,-0.294954293000016));
#313663=CARTESIAN_POINT('Ctrl Pts',(-4.14328888700005,5.2,-0.294954293000016));
#313664=CARTESIAN_POINT('Ctrl Pts',(-4.14328888700005,2.2,-0.294954293000016));
#313665=CARTESIAN_POINT('Ctrl Pts',(-4.14456428100006,12.2,-0.295420121000016));
#313666=CARTESIAN_POINT('Ctrl Pts',(-4.14456428100006,5.2,-0.295420121000016));
#313667=CARTESIAN_POINT('Ctrl Pts',(-4.14456428100006,2.2,-0.295420121000016));
#313668=CARTESIAN_POINT('Ctrl Pts',(-4.14584373900006,12.2,-0.295889154000015));
#313669=CARTESIAN_POINT('Ctrl Pts',(-4.14584373900006,5.2,-0.295889154000015));
#313670=CARTESIAN_POINT('Ctrl Pts',(-4.14584373900006,2.2,-0.295889154000015));
#313671=CARTESIAN_POINT('Ctrl Pts',(-4.14712724900006,12.2,-0.296361399000014));
#313672=CARTESIAN_POINT('Ctrl Pts',(-4.14712724900006,5.2,-0.296361399000014));
#313673=CARTESIAN_POINT('Ctrl Pts',(-4.14712724900006,2.2,-0.296361399000014));
#313674=CARTESIAN_POINT('Ctrl Pts',(-4.14841479800006,12.2,-0.296836863000016));
#313675=CARTESIAN_POINT('Ctrl Pts',(-4.14841479800006,5.2,-0.296836863000016));
#313676=CARTESIAN_POINT('Ctrl Pts',(-4.14841479800006,2.2,-0.296836863000016));
#313677=CARTESIAN_POINT('Ctrl Pts',(-4.14970637400006,12.2,-0.297315553000015));
#313678=CARTESIAN_POINT('Ctrl Pts',(-4.14970637400006,5.2,-0.297315553000015));
#313679=CARTESIAN_POINT('Ctrl Pts',(-4.14970637400006,2.2,-0.297315553000015));
#313680=CARTESIAN_POINT('Ctrl Pts',(-4.15100196400005,12.2,-0.297797477000015));
#313681=CARTESIAN_POINT('Ctrl Pts',(-4.15100196400005,5.2,-0.297797477000015));
#313682=CARTESIAN_POINT('Ctrl Pts',(-4.15100196400005,2.2,-0.297797477000015));
#313683=CARTESIAN_POINT('Ctrl Pts',(-4.15230155800006,12.2,-0.298282640000016));
#313684=CARTESIAN_POINT('Ctrl Pts',(-4.15230155800006,5.2,-0.298282640000016));
#313685=CARTESIAN_POINT('Ctrl Pts',(-4.15230155800006,2.2,-0.298282640000016));
#313686=CARTESIAN_POINT('Ctrl Pts',(-4.15360514100006,12.2,-0.298771050000015));
#313687=CARTESIAN_POINT('Ctrl Pts',(-4.15360514100006,5.2,-0.298771050000015));
#313688=CARTESIAN_POINT('Ctrl Pts',(-4.15360514100006,2.2,-0.298771050000015));
#313689=CARTESIAN_POINT('Ctrl Pts',(-4.15491270200006,12.2,-0.299262713000013));
#313690=CARTESIAN_POINT('Ctrl Pts',(-4.15491270200006,5.2,-0.299262713000013));
#313691=CARTESIAN_POINT('Ctrl Pts',(-4.15491270200006,2.2,-0.299262713000013));
#313692=CARTESIAN_POINT('Ctrl Pts',(-4.15622423000006,12.2,-0.299757637000013));
#313693=CARTESIAN_POINT('Ctrl Pts',(-4.15622423000006,5.2,-0.299757637000013));
#313694=CARTESIAN_POINT('Ctrl Pts',(-4.15622423000006,2.2,-0.299757637000013));
#313695=CARTESIAN_POINT('Ctrl Pts',(-4.15753971000006,12.2,-0.300255828000013));
#313696=CARTESIAN_POINT('Ctrl Pts',(-4.15753971000006,5.2,-0.300255828000013));
#313697=CARTESIAN_POINT('Ctrl Pts',(-4.15753971000006,2.2,-0.300255828000013));
#313698=CARTESIAN_POINT('Ctrl Pts',(-4.15885913200006,12.2,-0.300757293000018));
#313699=CARTESIAN_POINT('Ctrl Pts',(-4.15885913200006,5.2,-0.300757293000018));
#313700=CARTESIAN_POINT('Ctrl Pts',(-4.15885913200006,2.2,-0.300757293000018));
#313701=CARTESIAN_POINT('Ctrl Pts',(-4.16018248400006,12.2,-0.301262039000014));
#313702=CARTESIAN_POINT('Ctrl Pts',(-4.16018248400006,5.2,-0.301262039000014));
#313703=CARTESIAN_POINT('Ctrl Pts',(-4.16018248400006,2.2,-0.301262039000014));
#313704=CARTESIAN_POINT('Ctrl Pts',(-4.16150975300006,12.2,-0.301770072000016));
#313705=CARTESIAN_POINT('Ctrl Pts',(-4.16150975300006,5.2,-0.301770072000016));
#313706=CARTESIAN_POINT('Ctrl Pts',(-4.16150975300006,2.2,-0.301770072000016));
#313707=CARTESIAN_POINT('Ctrl Pts',(-4.16284092600006,12.2,-0.302281398000015));
#313708=CARTESIAN_POINT('Ctrl Pts',(-4.16284092600006,5.2,-0.302281398000015));
#313709=CARTESIAN_POINT('Ctrl Pts',(-4.16284092600006,2.2,-0.302281398000015));
#313710=CARTESIAN_POINT('Ctrl Pts',(-4.16417599400006,12.2,-0.302796026000016));
#313711=CARTESIAN_POINT('Ctrl Pts',(-4.16417599400006,5.2,-0.302796026000016));
#313712=CARTESIAN_POINT('Ctrl Pts',(-4.16417599400006,2.2,-0.302796026000016));
#313713=CARTESIAN_POINT('Ctrl Pts',(-4.16551494100006,12.2,-0.303313960000011));
#313714=CARTESIAN_POINT('Ctrl Pts',(-4.16551494100006,5.2,-0.303313960000011));
#313715=CARTESIAN_POINT('Ctrl Pts',(-4.16551494100006,2.2,-0.303313960000011));
#313716=CARTESIAN_POINT('Ctrl Pts',(-4.16685775800006,12.2,-0.303835207000014));
#313717=CARTESIAN_POINT('Ctrl Pts',(-4.16685775800006,5.2,-0.303835207000014));
#313718=CARTESIAN_POINT('Ctrl Pts',(-4.16685775800006,2.2,-0.303835207000014));
#313719=CARTESIAN_POINT('Ctrl Pts',(-4.16820443100006,12.2,-0.304359775000016));
#313720=CARTESIAN_POINT('Ctrl Pts',(-4.16820443100006,5.2,-0.304359775000016));
#313721=CARTESIAN_POINT('Ctrl Pts',(-4.16820443100006,2.2,-0.304359775000016));
#313722=CARTESIAN_POINT('Ctrl Pts',(-4.16955495000006,12.2,-0.304887670000014));
#313723=CARTESIAN_POINT('Ctrl Pts',(-4.16955495000006,5.2,-0.304887670000014));
#313724=CARTESIAN_POINT('Ctrl Pts',(-4.16955495000006,2.2,-0.304887670000014));
#313725=CARTESIAN_POINT('Ctrl Pts',(-4.17090930000006,12.2,-0.305418899000016));
#313726=CARTESIAN_POINT('Ctrl Pts',(-4.17090930000006,5.2,-0.305418899000016));
#313727=CARTESIAN_POINT('Ctrl Pts',(-4.17090930000006,2.2,-0.305418899000016));
#313728=CARTESIAN_POINT('Ctrl Pts',(-4.17226747200006,12.2,-0.305953466000015));
#313729=CARTESIAN_POINT('Ctrl Pts',(-4.17226747200006,5.2,-0.305953466000015));
#313730=CARTESIAN_POINT('Ctrl Pts',(-4.17226747200006,2.2,-0.305953466000015));
#313731=CARTESIAN_POINT('Ctrl Pts',(-4.17362945300006,12.2,-0.306491379000011));
#313732=CARTESIAN_POINT('Ctrl Pts',(-4.17362945300006,5.2,-0.306491379000011));
#313733=CARTESIAN_POINT('Ctrl Pts',(-4.17362945300006,2.2,-0.306491379000011));
#313734=CARTESIAN_POINT('Ctrl Pts',(-4.17499523000005,12.2,-0.307032645000014));
#313735=CARTESIAN_POINT('Ctrl Pts',(-4.17499523000005,5.2,-0.307032645000014));
#313736=CARTESIAN_POINT('Ctrl Pts',(-4.17499523000005,2.2,-0.307032645000014));
#313737=CARTESIAN_POINT('Ctrl Pts',(-4.17636479300006,12.2,-0.307577269000014));
#313738=CARTESIAN_POINT('Ctrl Pts',(-4.17636479300006,5.2,-0.307577269000014));
#313739=CARTESIAN_POINT('Ctrl Pts',(-4.17636479300006,2.2,-0.307577269000014));
#313740=CARTESIAN_POINT('Ctrl Pts',(-4.17773812700006,12.2,-0.308125259000014));
#313741=CARTESIAN_POINT('Ctrl Pts',(-4.17773812700006,5.2,-0.308125259000014));
#313742=CARTESIAN_POINT('Ctrl Pts',(-4.17773812700006,2.2,-0.308125259000014));
#313743=CARTESIAN_POINT('Ctrl Pts',(-4.17911522400006,12.2,-0.308676620000017));
#313744=CARTESIAN_POINT('Ctrl Pts',(-4.17911522400006,5.2,-0.308676620000017));
#313745=CARTESIAN_POINT('Ctrl Pts',(-4.17911522400006,2.2,-0.308676620000017));
#313746=CARTESIAN_POINT('Ctrl Pts',(-4.18049606900006,12.2,-0.309231359000015));
#313747=CARTESIAN_POINT('Ctrl Pts',(-4.18049606900006,5.2,-0.309231359000015));
#313748=CARTESIAN_POINT('Ctrl Pts',(-4.18049606900006,2.2,-0.309231359000015));
#313749=CARTESIAN_POINT('Ctrl Pts',(-4.18188065100006,12.2,-0.309789482000014));
#313750=CARTESIAN_POINT('Ctrl Pts',(-4.18188065100006,5.2,-0.309789482000014));
#313751=CARTESIAN_POINT('Ctrl Pts',(-4.18188065100006,2.2,-0.309789482000014));
#313752=CARTESIAN_POINT('Ctrl Pts',(-4.18326895900006,12.2,-0.310350994000017));
#313753=CARTESIAN_POINT('Ctrl Pts',(-4.18326895900006,5.2,-0.310350994000017));
#313754=CARTESIAN_POINT('Ctrl Pts',(-4.18326895900006,2.2,-0.310350994000017));
#313755=CARTESIAN_POINT('Ctrl Pts',(-4.18466098000006,12.2,-0.310915903000013));
#313756=CARTESIAN_POINT('Ctrl Pts',(-4.18466098000006,5.2,-0.310915903000013));
#313757=CARTESIAN_POINT('Ctrl Pts',(-4.18466098000006,2.2,-0.310915903000013));
#313758=CARTESIAN_POINT('Ctrl Pts',(-4.18605670300006,12.2,-0.311484214000015));
#313759=CARTESIAN_POINT('Ctrl Pts',(-4.18605670300006,5.2,-0.311484214000015));
#313760=CARTESIAN_POINT('Ctrl Pts',(-4.18605670300006,2.2,-0.311484214000015));
#313761=CARTESIAN_POINT('Ctrl Pts',(-4.18745611600006,12.2,-0.312055933000015));
#313762=CARTESIAN_POINT('Ctrl Pts',(-4.18745611600006,5.2,-0.312055933000015));
#313763=CARTESIAN_POINT('Ctrl Pts',(-4.18745611600006,2.2,-0.312055933000015));
#313764=CARTESIAN_POINT('Ctrl Pts',(-4.18885920600006,12.2,-0.312631068000013));
#313765=CARTESIAN_POINT('Ctrl Pts',(-4.18885920600006,5.2,-0.312631068000013));
#313766=CARTESIAN_POINT('Ctrl Pts',(-4.18885920600006,2.2,-0.312631068000013));
#313767=CARTESIAN_POINT('Ctrl Pts',(-4.19026596400006,12.2,-0.313209622000015));
#313768=CARTESIAN_POINT('Ctrl Pts',(-4.19026596400006,5.2,-0.313209622000015));
#313769=CARTESIAN_POINT('Ctrl Pts',(-4.19026596400006,2.2,-0.313209622000015));
#313770=CARTESIAN_POINT('Ctrl Pts',(-4.19167637400006,12.2,-0.313791604000015));
#313771=CARTESIAN_POINT('Ctrl Pts',(-4.19167637400006,5.2,-0.313791604000015));
#313772=CARTESIAN_POINT('Ctrl Pts',(-4.19167637400006,2.2,-0.313791604000015));
#313773=CARTESIAN_POINT('Ctrl Pts',(-4.19309042900006,12.2,-0.314377018000016));
#313774=CARTESIAN_POINT('Ctrl Pts',(-4.19309042900006,5.2,-0.314377018000016));
#313775=CARTESIAN_POINT('Ctrl Pts',(-4.19309042900006,2.2,-0.314377018000016));
#313776=CARTESIAN_POINT('Ctrl Pts',(-4.19450811400006,12.2,-0.314965871000012));
#313777=CARTESIAN_POINT('Ctrl Pts',(-4.19450811400006,5.2,-0.314965871000012));
#313778=CARTESIAN_POINT('Ctrl Pts',(-4.19450811400006,2.2,-0.314965871000012));
#313779=CARTESIAN_POINT('Ctrl Pts',(-4.19592941800006,12.2,-0.315558168000014));
#313780=CARTESIAN_POINT('Ctrl Pts',(-4.19592941800006,5.2,-0.315558168000014));
#313781=CARTESIAN_POINT('Ctrl Pts',(-4.19592941800006,2.2,-0.315558168000014));
#313782=CARTESIAN_POINT('Ctrl Pts',(-4.19735432900006,12.2,-0.316153917000013));
#313783=CARTESIAN_POINT('Ctrl Pts',(-4.19735432900006,5.2,-0.316153917000013));
#313784=CARTESIAN_POINT('Ctrl Pts',(-4.19735432900006,2.2,-0.316153917000013));
#313785=CARTESIAN_POINT('Ctrl Pts',(-4.19878283700006,12.2,-0.316753122000013));
#313786=CARTESIAN_POINT('Ctrl Pts',(-4.19878283700006,5.2,-0.316753122000013));
#313787=CARTESIAN_POINT('Ctrl Pts',(-4.19878283700006,2.2,-0.316753122000013));
#313788=CARTESIAN_POINT('Ctrl Pts',(-4.20021492800006,12.2,-0.317355788000011));
#313789=CARTESIAN_POINT('Ctrl Pts',(-4.20021492800006,5.2,-0.317355788000011));
#313790=CARTESIAN_POINT('Ctrl Pts',(-4.20021492800006,2.2,-0.317355788000011));
#313791=CARTESIAN_POINT('Ctrl Pts',(-4.20165059300006,12.2,-0.317961924000016));
#313792=CARTESIAN_POINT('Ctrl Pts',(-4.20165059300006,5.2,-0.317961924000016));
#313793=CARTESIAN_POINT('Ctrl Pts',(-4.20165059300006,2.2,-0.317961924000016));
#313794=CARTESIAN_POINT('Ctrl Pts',(-4.20308981700006,12.2,-0.318571533000016));
#313795=CARTESIAN_POINT('Ctrl Pts',(-4.20308981700006,5.2,-0.318571533000016));
#313796=CARTESIAN_POINT('Ctrl Pts',(-4.20308981700006,2.2,-0.318571533000016));
#313797=CARTESIAN_POINT('Ctrl Pts',(-4.20453259100006,12.2,-0.319184622000015));
#313798=CARTESIAN_POINT('Ctrl Pts',(-4.20453259100006,5.2,-0.319184622000015));
#313799=CARTESIAN_POINT('Ctrl Pts',(-4.20453259100006,2.2,-0.319184622000015));
#313800=CARTESIAN_POINT('Ctrl Pts',(-4.20597890300006,12.2,-0.319801197000014));
#313801=CARTESIAN_POINT('Ctrl Pts',(-4.20597890300006,5.2,-0.319801197000014));
#313802=CARTESIAN_POINT('Ctrl Pts',(-4.20597890300006,2.2,-0.319801197000014));
#313803=CARTESIAN_POINT('Ctrl Pts',(-4.20742873900006,12.2,-0.320421263000017));
#313804=CARTESIAN_POINT('Ctrl Pts',(-4.20742873900006,5.2,-0.320421263000017));
#313805=CARTESIAN_POINT('Ctrl Pts',(-4.20742873900006,2.2,-0.320421263000017));
#313806=CARTESIAN_POINT('Ctrl Pts',(-4.20888209100006,12.2,-0.321044826000012));
#313807=CARTESIAN_POINT('Ctrl Pts',(-4.20888209100006,5.2,-0.321044826000012));
#313808=CARTESIAN_POINT('Ctrl Pts',(-4.20888209100006,2.2,-0.321044826000012));
#313809=CARTESIAN_POINT('Ctrl Pts',(-4.21033894600006,12.2,-0.321671892000013));
#313810=CARTESIAN_POINT('Ctrl Pts',(-4.21033894600006,5.2,-0.321671892000013));
#313811=CARTESIAN_POINT('Ctrl Pts',(-4.21033894600006,2.2,-0.321671892000013));
#313812=CARTESIAN_POINT('Ctrl Pts',(-4.21179929100005,12.2,-0.322302466000015));
#313813=CARTESIAN_POINT('Ctrl Pts',(-4.21179929100005,5.2,-0.322302466000015));
#313814=CARTESIAN_POINT('Ctrl Pts',(-4.21179929100005,2.2,-0.322302466000015));
#313815=CARTESIAN_POINT('Ctrl Pts',(-4.21326311600006,12.2,-0.322936554000015));
#313816=CARTESIAN_POINT('Ctrl Pts',(-4.21326311600006,5.2,-0.322936554000015));
#313817=CARTESIAN_POINT('Ctrl Pts',(-4.21326311600006,2.2,-0.322936554000015));
#313818=CARTESIAN_POINT('Ctrl Pts',(-4.21473040900006,12.2,-0.323574162000018));
#313819=CARTESIAN_POINT('Ctrl Pts',(-4.21473040900006,5.2,-0.323574162000018));
#313820=CARTESIAN_POINT('Ctrl Pts',(-4.21473040900006,2.2,-0.323574162000018));
#313821=CARTESIAN_POINT('Ctrl Pts',(-4.21620115900006,12.2,-0.324215295000014));
#313822=CARTESIAN_POINT('Ctrl Pts',(-4.21620115900006,5.2,-0.324215295000014));
#313823=CARTESIAN_POINT('Ctrl Pts',(-4.21620115900006,2.2,-0.324215295000014));
#313824=CARTESIAN_POINT('Ctrl Pts',(-4.21767535400006,12.2,-0.324859958000014));
#313825=CARTESIAN_POINT('Ctrl Pts',(-4.21767535400006,5.2,-0.324859958000014));
#313826=CARTESIAN_POINT('Ctrl Pts',(-4.21767535400006,2.2,-0.324859958000014));
#313827=CARTESIAN_POINT('Ctrl Pts',(-4.21915298100005,12.2,-0.325508158000014));
#313828=CARTESIAN_POINT('Ctrl Pts',(-4.21915298100005,5.2,-0.325508158000014));
#313829=CARTESIAN_POINT('Ctrl Pts',(-4.21915298100005,2.2,-0.325508158000014));
#313830=CARTESIAN_POINT('Ctrl Pts',(-4.22063403100006,12.2,-0.326159900000014));
#313831=CARTESIAN_POINT('Ctrl Pts',(-4.22063403100006,5.2,-0.326159900000014));
#313832=CARTESIAN_POINT('Ctrl Pts',(-4.22063403100006,2.2,-0.326159900000014));
#313833=CARTESIAN_POINT('Ctrl Pts',(-4.22211849200006,12.2,-0.326815189000014));
#313834=CARTESIAN_POINT('Ctrl Pts',(-4.22211849200006,5.2,-0.326815189000014));
#313835=CARTESIAN_POINT('Ctrl Pts',(-4.22211849200006,2.2,-0.326815189000014));
#313836=CARTESIAN_POINT('Ctrl Pts',(-4.22360635200006,12.2,-0.327474030000015));
#313837=CARTESIAN_POINT('Ctrl Pts',(-4.22360635200006,5.2,-0.327474030000015));
#313838=CARTESIAN_POINT('Ctrl Pts',(-4.22360635200006,2.2,-0.327474030000015));
#313839=CARTESIAN_POINT('Ctrl Pts',(-4.22509760000006,12.2,-0.328136431000012));
#313840=CARTESIAN_POINT('Ctrl Pts',(-4.22509760000006,5.2,-0.328136431000012));
#313841=CARTESIAN_POINT('Ctrl Pts',(-4.22509760000006,2.2,-0.328136431000012));
#313842=CARTESIAN_POINT('Ctrl Pts',(-4.22659222400006,12.2,-0.328802394000016));
#313843=CARTESIAN_POINT('Ctrl Pts',(-4.22659222400006,5.2,-0.328802394000016));
#313844=CARTESIAN_POINT('Ctrl Pts',(-4.22659222400006,2.2,-0.328802394000016));
#313845=CARTESIAN_POINT('Ctrl Pts',(-4.22809021300006,12.2,-0.329471925000018));
#313846=CARTESIAN_POINT('Ctrl Pts',(-4.22809021300006,5.2,-0.329471925000018));
#313847=CARTESIAN_POINT('Ctrl Pts',(-4.22809021300006,2.2,-0.329471925000018));
#313848=CARTESIAN_POINT('Ctrl Pts',(-4.22959155500005,12.2,-0.330145032000013));
#313849=CARTESIAN_POINT('Ctrl Pts',(-4.22959155500005,5.2,-0.330145032000013));
#313850=CARTESIAN_POINT('Ctrl Pts',(-4.22959155500005,2.2,-0.330145032000013));
#313851=CARTESIAN_POINT('Ctrl Pts',(-4.23109624000006,12.2,-0.330821718000016));
#313852=CARTESIAN_POINT('Ctrl Pts',(-4.23109624000006,5.2,-0.330821718000016));
#313853=CARTESIAN_POINT('Ctrl Pts',(-4.23109624000006,2.2,-0.330821718000016));
#313854=CARTESIAN_POINT('Ctrl Pts',(-4.23260425500006,12.2,-0.331501989000014));
#313855=CARTESIAN_POINT('Ctrl Pts',(-4.23260425500006,5.2,-0.331501989000014));
#313856=CARTESIAN_POINT('Ctrl Pts',(-4.23260425500006,2.2,-0.331501989000014));
#313857=CARTESIAN_POINT('Ctrl Pts',(-4.23411558900006,12.2,-0.332185850000015));
#313858=CARTESIAN_POINT('Ctrl Pts',(-4.23411558900006,5.2,-0.332185850000015));
#313859=CARTESIAN_POINT('Ctrl Pts',(-4.23411558900006,2.2,-0.332185850000015));
#313860=CARTESIAN_POINT('Ctrl Pts',(-4.23563023200006,12.2,-0.332873306000017));
#313861=CARTESIAN_POINT('Ctrl Pts',(-4.23563023200006,5.2,-0.332873306000017));
#313862=CARTESIAN_POINT('Ctrl Pts',(-4.23563023200006,2.2,-0.332873306000017));
#313863=CARTESIAN_POINT('Ctrl Pts',(-4.23714817100006,12.2,-0.333564363000014));
#313864=CARTESIAN_POINT('Ctrl Pts',(-4.23714817100006,5.2,-0.333564363000014));
#313865=CARTESIAN_POINT('Ctrl Pts',(-4.23714817100006,2.2,-0.333564363000014));
#313866=CARTESIAN_POINT('Ctrl Pts',(-4.23866939600006,12.2,-0.334259026000012));
#313867=CARTESIAN_POINT('Ctrl Pts',(-4.23866939600006,5.2,-0.334259026000012));
#313868=CARTESIAN_POINT('Ctrl Pts',(-4.23866939600006,2.2,-0.334259026000012));
#313869=CARTESIAN_POINT('Ctrl Pts',(-4.24019389600006,12.2,-0.334957299000016));
#313870=CARTESIAN_POINT('Ctrl Pts',(-4.24019389600006,5.2,-0.334957299000016));
#313871=CARTESIAN_POINT('Ctrl Pts',(-4.24019389600006,2.2,-0.334957299000016));
#313872=CARTESIAN_POINT('Ctrl Pts',(-4.24172165700006,12.2,-0.335659190000013));
#313873=CARTESIAN_POINT('Ctrl Pts',(-4.24172165700006,5.2,-0.335659190000013));
#313874=CARTESIAN_POINT('Ctrl Pts',(-4.24172165700006,2.2,-0.335659190000013));
#313875=CARTESIAN_POINT('Ctrl Pts',(-4.24325267100006,12.2,-0.336364701000011));
#313876=CARTESIAN_POINT('Ctrl Pts',(-4.24325267100006,5.2,-0.336364701000011));
#313877=CARTESIAN_POINT('Ctrl Pts',(-4.24325267100006,2.2,-0.336364701000011));
#313878=CARTESIAN_POINT('Ctrl Pts',(-4.24478692500006,12.2,-0.337073838000013));
#313879=CARTESIAN_POINT('Ctrl Pts',(-4.24478692500006,5.2,-0.337073838000013));
#313880=CARTESIAN_POINT('Ctrl Pts',(-4.24478692500006,2.2,-0.337073838000013));
#313881=CARTESIAN_POINT('Ctrl Pts',(-4.24632440700006,12.2,-0.337786607000012));
#313882=CARTESIAN_POINT('Ctrl Pts',(-4.24632440700006,5.2,-0.337786607000012));
#313883=CARTESIAN_POINT('Ctrl Pts',(-4.24632440700006,2.2,-0.337786607000012));
#313884=CARTESIAN_POINT('Ctrl Pts',(-4.24786510800006,12.2,-0.338503012000011));
#313885=CARTESIAN_POINT('Ctrl Pts',(-4.24786510800006,5.2,-0.338503012000011));
#313886=CARTESIAN_POINT('Ctrl Pts',(-4.24786510800006,2.2,-0.338503012000011));
#313887=CARTESIAN_POINT('Ctrl Pts',(-4.24940901600006,12.2,-0.339223059000013));
#313888=CARTESIAN_POINT('Ctrl Pts',(-4.24940901600006,5.2,-0.339223059000013));
#313889=CARTESIAN_POINT('Ctrl Pts',(-4.24940901600006,2.2,-0.339223059000013));
#313890=CARTESIAN_POINT('Ctrl Pts',(-4.25095611900006,12.2,-0.339946752000015));
#313891=CARTESIAN_POINT('Ctrl Pts',(-4.25095611900006,5.2,-0.339946752000015));
#313892=CARTESIAN_POINT('Ctrl Pts',(-4.25095611900006,2.2,-0.339946752000015));
#313893=CARTESIAN_POINT('Ctrl Pts',(-4.25250640600006,12.2,-0.340674097000013));
#313894=CARTESIAN_POINT('Ctrl Pts',(-4.25250640600006,5.2,-0.340674097000013));
#313895=CARTESIAN_POINT('Ctrl Pts',(-4.25250640600006,2.2,-0.340674097000013));
#313896=CARTESIAN_POINT('Ctrl Pts',(-4.25405986600006,12.2,-0.341405097000016));
#313897=CARTESIAN_POINT('Ctrl Pts',(-4.25405986600006,5.2,-0.341405097000016));
#313898=CARTESIAN_POINT('Ctrl Pts',(-4.25405986600006,2.2,-0.341405097000016));
#313899=CARTESIAN_POINT('Ctrl Pts',(-4.25561648900006,12.2,-0.342139760000015));
#313900=CARTESIAN_POINT('Ctrl Pts',(-4.25561648900006,5.2,-0.342139760000015));
#313901=CARTESIAN_POINT('Ctrl Pts',(-4.25561648900006,2.2,-0.342139760000015));
#313902=CARTESIAN_POINT('Ctrl Pts',(-4.25717626100006,12.2,-0.342878088000016));
#313903=CARTESIAN_POINT('Ctrl Pts',(-4.25717626100006,5.2,-0.342878088000016));
#313904=CARTESIAN_POINT('Ctrl Pts',(-4.25717626100006,2.2,-0.342878088000016));
#313905=CARTESIAN_POINT('Ctrl Pts',(-4.25873917500006,12.2,-0.343620088000014));
#313906=CARTESIAN_POINT('Ctrl Pts',(-4.25873917500006,5.2,-0.343620088000014));
#313907=CARTESIAN_POINT('Ctrl Pts',(-4.25873917500006,2.2,-0.343620088000014));
#313908=CARTESIAN_POINT('Ctrl Pts',(-4.26030521600006,12.2,-0.344365764000014));
#313909=CARTESIAN_POINT('Ctrl Pts',(-4.26030521600006,5.2,-0.344365764000014));
#313910=CARTESIAN_POINT('Ctrl Pts',(-4.26030521600006,2.2,-0.344365764000014));
#313911=CARTESIAN_POINT('Ctrl Pts',(-4.26187437500006,12.2,-0.345115121000017));
#313912=CARTESIAN_POINT('Ctrl Pts',(-4.26187437500006,5.2,-0.345115121000017));
#313913=CARTESIAN_POINT('Ctrl Pts',(-4.26187437500006,2.2,-0.345115121000017));
#313914=CARTESIAN_POINT('Ctrl Pts',(-4.26344664100006,12.2,-0.345868163000014));
#313915=CARTESIAN_POINT('Ctrl Pts',(-4.26344664100006,5.2,-0.345868163000014));
#313916=CARTESIAN_POINT('Ctrl Pts',(-4.26344664100006,2.2,-0.345868163000014));
#313917=CARTESIAN_POINT('Ctrl Pts',(-4.26502200200006,12.2,-0.346624895000014));
#313918=CARTESIAN_POINT('Ctrl Pts',(-4.26502200200006,5.2,-0.346624895000014));
#313919=CARTESIAN_POINT('Ctrl Pts',(-4.26502200200006,2.2,-0.346624895000014));
#313920=CARTESIAN_POINT('Ctrl Pts',(-4.26660044600006,12.2,-0.347385322000013));
#313921=CARTESIAN_POINT('Ctrl Pts',(-4.26660044600006,5.2,-0.347385322000013));
#313922=CARTESIAN_POINT('Ctrl Pts',(-4.26660044600006,2.2,-0.347385322000013));
#313923=CARTESIAN_POINT('Ctrl Pts',(-4.26818196500006,12.2,-0.348149450000013));
#313924=CARTESIAN_POINT('Ctrl Pts',(-4.26818196500006,5.2,-0.348149450000013));
#313925=CARTESIAN_POINT('Ctrl Pts',(-4.26818196500006,2.2,-0.348149450000013));
#313926=CARTESIAN_POINT('Ctrl Pts',(-4.26976654500006,12.2,-0.348917282000016));
#313927=CARTESIAN_POINT('Ctrl Pts',(-4.26976654500006,5.2,-0.348917282000016));
#313928=CARTESIAN_POINT('Ctrl Pts',(-4.26976654500006,2.2,-0.348917282000016));
#313929=CARTESIAN_POINT('Ctrl Pts',(-4.27135417700006,12.2,-0.349688824000012));
#313930=CARTESIAN_POINT('Ctrl Pts',(-4.27135417700006,5.2,-0.349688824000012));
#313931=CARTESIAN_POINT('Ctrl Pts',(-4.27135417700006,2.2,-0.349688824000012));
#313932=CARTESIAN_POINT('Ctrl Pts',(-4.27294484900006,12.2,-0.350464078000012));
#313933=CARTESIAN_POINT('Ctrl Pts',(-4.27294484900006,5.2,-0.350464078000012));
#313934=CARTESIAN_POINT('Ctrl Pts',(-4.27294484900006,2.2,-0.350464078000012));
#313935=CARTESIAN_POINT('Ctrl Pts',(-4.27453855000006,12.2,-0.351243052000014));
#313936=CARTESIAN_POINT('Ctrl Pts',(-4.27453855000006,5.2,-0.351243052000014));
#313937=CARTESIAN_POINT('Ctrl Pts',(-4.27453855000006,2.2,-0.351243052000014));
#313938=CARTESIAN_POINT('Ctrl Pts',(-4.27613527000006,12.2,-0.352025750000013));
#313939=CARTESIAN_POINT('Ctrl Pts',(-4.27613527000006,5.2,-0.352025750000013));
#313940=CARTESIAN_POINT('Ctrl Pts',(-4.27613527000006,2.2,-0.352025750000013));
#313941=CARTESIAN_POINT('Ctrl Pts',(-4.27773499600006,12.2,-0.352812175000015));
#313942=CARTESIAN_POINT('Ctrl Pts',(-4.27773499600006,5.2,-0.352812175000015));
#313943=CARTESIAN_POINT('Ctrl Pts',(-4.27773499600006,2.2,-0.352812175000015));
#313944=CARTESIAN_POINT('Ctrl Pts',(-4.27933771900006,12.2,-0.353602331000014));
#313945=CARTESIAN_POINT('Ctrl Pts',(-4.27933771900006,5.2,-0.353602331000014));
#313946=CARTESIAN_POINT('Ctrl Pts',(-4.27933771900006,2.2,-0.353602331000014));
#313947=CARTESIAN_POINT('Ctrl Pts',(-4.28094342700006,12.2,-0.354396226000016));
#313948=CARTESIAN_POINT('Ctrl Pts',(-4.28094342700006,5.2,-0.354396226000016));
#313949=CARTESIAN_POINT('Ctrl Pts',(-4.28094342700006,2.2,-0.354396226000016));
#313950=CARTESIAN_POINT('Ctrl Pts',(-4.28255211000006,12.2,-0.355193862000016));
#313951=CARTESIAN_POINT('Ctrl Pts',(-4.28255211000006,5.2,-0.355193862000016));
#313952=CARTESIAN_POINT('Ctrl Pts',(-4.28255211000006,2.2,-0.355193862000016));
#313953=CARTESIAN_POINT('Ctrl Pts',(-4.28416375600006,12.2,-0.355995244000016));
#313954=CARTESIAN_POINT('Ctrl Pts',(-4.28416375600006,5.2,-0.355995244000016));
#313955=CARTESIAN_POINT('Ctrl Pts',(-4.28416375600006,2.2,-0.355995244000016));
#313956=CARTESIAN_POINT('Ctrl Pts',(-4.28577835400006,12.2,-0.356800375000015));
#313957=CARTESIAN_POINT('Ctrl Pts',(-4.28577835400006,5.2,-0.356800375000015));
#313958=CARTESIAN_POINT('Ctrl Pts',(-4.28577835400006,2.2,-0.356800375000015));
#313959=CARTESIAN_POINT('Ctrl Pts',(-4.28739589500006,12.2,-0.357609262000014));
#313960=CARTESIAN_POINT('Ctrl Pts',(-4.28739589500006,5.2,-0.357609262000014));
#313961=CARTESIAN_POINT('Ctrl Pts',(-4.28739589500006,2.2,-0.357609262000014));
#313962=CARTESIAN_POINT('Ctrl Pts',(-4.28901636600005,12.2,-0.358421908000013));
#313963=CARTESIAN_POINT('Ctrl Pts',(-4.28901636600005,5.2,-0.358421908000013));
#313964=CARTESIAN_POINT('Ctrl Pts',(-4.28901636600005,2.2,-0.358421908000013));
#313965=CARTESIAN_POINT('Ctrl Pts',(-4.29063975800006,12.2,-0.359238318000017));
#313966=CARTESIAN_POINT('Ctrl Pts',(-4.29063975800006,5.2,-0.359238318000017));
#313967=CARTESIAN_POINT('Ctrl Pts',(-4.29063975800006,2.2,-0.359238318000017));
#313968=CARTESIAN_POINT('Ctrl Pts',(-4.29226605800006,12.2,-0.360058496000013));
#313969=CARTESIAN_POINT('Ctrl Pts',(-4.29226605800006,5.2,-0.360058496000013));
#313970=CARTESIAN_POINT('Ctrl Pts',(-4.29226605800006,2.2,-0.360058496000013));
#313971=CARTESIAN_POINT('Ctrl Pts',(-4.29389525600006,12.2,-0.360882447000015));
#313972=CARTESIAN_POINT('Ctrl Pts',(-4.29389525600006,5.2,-0.360882447000015));
#313973=CARTESIAN_POINT('Ctrl Pts',(-4.29389525600006,2.2,-0.360882447000015));
#313974=CARTESIAN_POINT('Ctrl Pts',(-4.29552734300006,12.2,-0.361710175000014));
#313975=CARTESIAN_POINT('Ctrl Pts',(-4.29552734300006,5.2,-0.361710175000014));
#313976=CARTESIAN_POINT('Ctrl Pts',(-4.29552734300006,2.2,-0.361710175000014));
#313977=CARTESIAN_POINT('Ctrl Pts',(-4.29716230600006,12.2,-0.362541683000015));
#313978=CARTESIAN_POINT('Ctrl Pts',(-4.29716230600006,5.2,-0.362541683000015));
#313979=CARTESIAN_POINT('Ctrl Pts',(-4.29716230600006,2.2,-0.362541683000015));
#313980=CARTESIAN_POINT('Ctrl Pts',(-4.29880013500005,12.2,-0.363376978000014));
#313981=CARTESIAN_POINT('Ctrl Pts',(-4.29880013500005,5.2,-0.363376978000014));
#313982=CARTESIAN_POINT('Ctrl Pts',(-4.29880013500005,2.2,-0.363376978000014));
#313983=CARTESIAN_POINT('Ctrl Pts',(-4.30044081900006,12.2,-0.364216062000011));
#313984=CARTESIAN_POINT('Ctrl Pts',(-4.30044081900006,5.2,-0.364216062000011));
#313985=CARTESIAN_POINT('Ctrl Pts',(-4.30044081900006,2.2,-0.364216062000011));
#313986=CARTESIAN_POINT('Ctrl Pts',(-4.30208434600006,12.2,-0.365058939000011));
#313987=CARTESIAN_POINT('Ctrl Pts',(-4.30208434600006,5.2,-0.365058939000011));
#313988=CARTESIAN_POINT('Ctrl Pts',(-4.30208434600006,2.2,-0.365058939000011));
#313989=CARTESIAN_POINT('Ctrl Pts',(-4.30373070900006,12.2,-0.365905616000015));
#313990=CARTESIAN_POINT('Ctrl Pts',(-4.30373070900006,5.2,-0.365905616000015));
#313991=CARTESIAN_POINT('Ctrl Pts',(-4.30373070900006,2.2,-0.365905616000015));
#313992=CARTESIAN_POINT('Ctrl Pts',(-4.30537989300006,12.2,-0.366756094000014));
#313993=CARTESIAN_POINT('Ctrl Pts',(-4.30537989300006,5.2,-0.366756094000014));
#313994=CARTESIAN_POINT('Ctrl Pts',(-4.30537989300006,2.2,-0.366756094000014));
#313995=CARTESIAN_POINT('Ctrl Pts',(-4.30703189000006,12.2,-0.367610380000016));
#313996=CARTESIAN_POINT('Ctrl Pts',(-4.30703189000006,5.2,-0.367610380000016));
#313997=CARTESIAN_POINT('Ctrl Pts',(-4.30703189000006,2.2,-0.367610380000016));
#313998=CARTESIAN_POINT('Ctrl Pts',(-4.30868668700006,12.2,-0.368468477000015));
#313999=CARTESIAN_POINT('Ctrl Pts',(-4.30868668700006,5.2,-0.368468477000015));
#314000=CARTESIAN_POINT('Ctrl Pts',(-4.30868668700006,2.2,-0.368468477000015));
#314001=CARTESIAN_POINT('Ctrl Pts',(-4.31034427600006,12.2,-0.369330388000013));
#314002=CARTESIAN_POINT('Ctrl Pts',(-4.31034427600006,5.2,-0.369330388000013));
#314003=CARTESIAN_POINT('Ctrl Pts',(-4.31034427600006,2.2,-0.369330388000013));
#314004=CARTESIAN_POINT('Ctrl Pts',(-4.31200464500006,12.2,-0.370196119000017));
#314005=CARTESIAN_POINT('Ctrl Pts',(-4.31200464500006,5.2,-0.370196119000017));
#314006=CARTESIAN_POINT('Ctrl Pts',(-4.31200464500006,2.2,-0.370196119000017));
#314007=CARTESIAN_POINT('Ctrl Pts',(-4.31366778300006,12.2,-0.371065672000017));
#314008=CARTESIAN_POINT('Ctrl Pts',(-4.31366778300006,5.2,-0.371065672000017));
#314009=CARTESIAN_POINT('Ctrl Pts',(-4.31366778300006,2.2,-0.371065672000017));
#314010=CARTESIAN_POINT('Ctrl Pts',(-4.31533367800006,12.2,-0.371939053000014));
#314011=CARTESIAN_POINT('Ctrl Pts',(-4.31533367800006,5.2,-0.371939053000014));
#314012=CARTESIAN_POINT('Ctrl Pts',(-4.31533367800006,2.2,-0.371939053000014));
#314013=CARTESIAN_POINT('Ctrl Pts',(-4.31700232300006,12.2,-0.372816266000013));
#314014=CARTESIAN_POINT('Ctrl Pts',(-4.31700232300006,5.2,-0.372816266000013));
#314015=CARTESIAN_POINT('Ctrl Pts',(-4.31700232300006,2.2,-0.372816266000013));
#314016=CARTESIAN_POINT('Ctrl Pts',(-4.31867370400006,12.2,-0.373697313000014));
#314017=CARTESIAN_POINT('Ctrl Pts',(-4.31867370400006,5.2,-0.373697313000014));
#314018=CARTESIAN_POINT('Ctrl Pts',(-4.31867370400006,2.2,-0.373697313000014));
#314019=CARTESIAN_POINT('Ctrl Pts',(-4.32034781300006,12.2,-0.374582201000013));
#314020=CARTESIAN_POINT('Ctrl Pts',(-4.32034781300006,5.2,-0.374582201000013));
#314021=CARTESIAN_POINT('Ctrl Pts',(-4.32034781300006,2.2,-0.374582201000013));
#314022=CARTESIAN_POINT('Ctrl Pts',(-4.32202463700006,12.2,-0.375470931000015));
#314023=CARTESIAN_POINT('Ctrl Pts',(-4.32202463700006,5.2,-0.375470931000015));
#314024=CARTESIAN_POINT('Ctrl Pts',(-4.32202463700006,2.2,-0.375470931000015));
#314025=CARTESIAN_POINT('Ctrl Pts',(-4.32370416700006,12.2,-0.376363509000015));
#314026=CARTESIAN_POINT('Ctrl Pts',(-4.32370416700006,5.2,-0.376363509000015));
#314027=CARTESIAN_POINT('Ctrl Pts',(-4.32370416700006,2.2,-0.376363509000015));
#314028=CARTESIAN_POINT('Ctrl Pts',(-4.32538639100006,12.2,-0.377259939000014));
#314029=CARTESIAN_POINT('Ctrl Pts',(-4.32538639100006,5.2,-0.377259939000014));
#314030=CARTESIAN_POINT('Ctrl Pts',(-4.32538639100006,2.2,-0.377259939000014));
#314031=CARTESIAN_POINT('Ctrl Pts',(-4.32707130000006,12.2,-0.378160224000013));
#314032=CARTESIAN_POINT('Ctrl Pts',(-4.32707130000006,5.2,-0.378160224000013));
#314033=CARTESIAN_POINT('Ctrl Pts',(-4.32707130000006,2.2,-0.378160224000013));
#314034=CARTESIAN_POINT('Ctrl Pts',(-4.32875888300006,12.2,-0.379064368000015));
#314035=CARTESIAN_POINT('Ctrl Pts',(-4.32875888300006,5.2,-0.379064368000015));
#314036=CARTESIAN_POINT('Ctrl Pts',(-4.32875888300006,2.2,-0.379064368000015));
#314037=CARTESIAN_POINT('Ctrl Pts',(-4.33044912900006,12.2,-0.379972375000013));
#314038=CARTESIAN_POINT('Ctrl Pts',(-4.33044912900006,5.2,-0.379972375000013));
#314039=CARTESIAN_POINT('Ctrl Pts',(-4.33044912900006,2.2,-0.379972375000013));
#314040=CARTESIAN_POINT('Ctrl Pts',(-4.33214202700006,12.2,-0.380884249000015));
#314041=CARTESIAN_POINT('Ctrl Pts',(-4.33214202700006,5.2,-0.380884249000015));
#314042=CARTESIAN_POINT('Ctrl Pts',(-4.33214202700006,2.2,-0.380884249000015));
#314043=CARTESIAN_POINT('Ctrl Pts',(-4.33383756700006,12.2,-0.381799994000014));
#314044=CARTESIAN_POINT('Ctrl Pts',(-4.33383756700006,5.2,-0.381799994000014));
#314045=CARTESIAN_POINT('Ctrl Pts',(-4.33383756700006,2.2,-0.381799994000014));
#314046=CARTESIAN_POINT('Ctrl Pts',(-4.33553573900006,12.2,-0.382719614000013));
#314047=CARTESIAN_POINT('Ctrl Pts',(-4.33553573900006,5.2,-0.382719614000013));
#314048=CARTESIAN_POINT('Ctrl Pts',(-4.33553573900006,2.2,-0.382719614000013));
#314049=CARTESIAN_POINT('Ctrl Pts',(-4.33723653100006,12.2,-0.383643113000014));
#314050=CARTESIAN_POINT('Ctrl Pts',(-4.33723653100006,5.2,-0.383643113000014));
#314051=CARTESIAN_POINT('Ctrl Pts',(-4.33723653100006,2.2,-0.383643113000014));
#314052=CARTESIAN_POINT('Ctrl Pts',(-4.33893993400006,12.2,-0.384570493000016));
#314053=CARTESIAN_POINT('Ctrl Pts',(-4.33893993400006,5.2,-0.384570493000016));
#314054=CARTESIAN_POINT('Ctrl Pts',(-4.33893993400006,2.2,-0.384570493000016));
#314055=CARTESIAN_POINT('Ctrl Pts',(-4.34064593700006,12.2,-0.385501760000011));
#314056=CARTESIAN_POINT('Ctrl Pts',(-4.34064593700006,5.2,-0.385501760000011));
#314057=CARTESIAN_POINT('Ctrl Pts',(-4.34064593700006,2.2,-0.385501760000011));
#314058=CARTESIAN_POINT('Ctrl Pts',(-4.34235453000006,12.2,-0.386436917000013));
#314059=CARTESIAN_POINT('Ctrl Pts',(-4.34235453000006,5.2,-0.386436917000013));
#314060=CARTESIAN_POINT('Ctrl Pts',(-4.34235453000006,2.2,-0.386436917000013));
#314061=CARTESIAN_POINT('Ctrl Pts',(-4.34406570100006,12.2,-0.387375967000012));
#314062=CARTESIAN_POINT('Ctrl Pts',(-4.34406570100006,5.2,-0.387375967000012));
#314063=CARTESIAN_POINT('Ctrl Pts',(-4.34406570100006,2.2,-0.387375967000012));
#314064=CARTESIAN_POINT('Ctrl Pts',(-4.34577944200006,12.2,-0.388318914000014));
#314065=CARTESIAN_POINT('Ctrl Pts',(-4.34577944200006,5.2,-0.388318914000014));
#314066=CARTESIAN_POINT('Ctrl Pts',(-4.34577944200006,2.2,-0.388318914000014));
#314067=CARTESIAN_POINT('Ctrl Pts',(-4.34749574100006,12.2,-0.389265762000015));
#314068=CARTESIAN_POINT('Ctrl Pts',(-4.34749574100006,5.2,-0.389265762000015));
#314069=CARTESIAN_POINT('Ctrl Pts',(-4.34749574100006,2.2,-0.389265762000015));
#314070=CARTESIAN_POINT('Ctrl Pts',(-4.34921458700006,12.2,-0.390216515000015));
#314071=CARTESIAN_POINT('Ctrl Pts',(-4.34921458700006,5.2,-0.390216515000015));
#314072=CARTESIAN_POINT('Ctrl Pts',(-4.34921458700006,2.2,-0.390216515000015));
#314073=CARTESIAN_POINT('Ctrl Pts',(-4.35093597100006,12.2,-0.391171176000018));
#314074=CARTESIAN_POINT('Ctrl Pts',(-4.35093597100006,5.2,-0.391171176000018));
#314075=CARTESIAN_POINT('Ctrl Pts',(-4.35093597100006,2.2,-0.391171176000018));
#314076=CARTESIAN_POINT('Ctrl Pts',(-4.35265988100006,12.2,-0.392129749000016));
#314077=CARTESIAN_POINT('Ctrl Pts',(-4.35265988100006,5.2,-0.392129749000016));
#314078=CARTESIAN_POINT('Ctrl Pts',(-4.35265988100006,2.2,-0.392129749000016));
#314079=CARTESIAN_POINT('Ctrl Pts',(-4.35438630800006,12.2,-0.393092237000014));
#314080=CARTESIAN_POINT('Ctrl Pts',(-4.35438630800006,5.2,-0.393092237000014));
#314081=CARTESIAN_POINT('Ctrl Pts',(-4.35438630800006,2.2,-0.393092237000014));
#314082=CARTESIAN_POINT('Ctrl Pts',(-4.35611524200006,12.2,-0.394058645000013));
#314083=CARTESIAN_POINT('Ctrl Pts',(-4.35611524200006,5.2,-0.394058645000013));
#314084=CARTESIAN_POINT('Ctrl Pts',(-4.35611524200006,2.2,-0.394058645000013));
#314085=CARTESIAN_POINT('Ctrl Pts',(-4.35784667100005,12.2,-0.395028976000016));
#314086=CARTESIAN_POINT('Ctrl Pts',(-4.35784667100005,5.2,-0.395028976000016));
#314087=CARTESIAN_POINT('Ctrl Pts',(-4.35784667100005,2.2,-0.395028976000016));
#314088=CARTESIAN_POINT('Ctrl Pts',(-4.35958058500006,12.2,-0.396003232000015));
#314089=CARTESIAN_POINT('Ctrl Pts',(-4.35958058500006,5.2,-0.396003232000015));
#314090=CARTESIAN_POINT('Ctrl Pts',(-4.35958058500006,2.2,-0.396003232000015));
#314091=CARTESIAN_POINT('Ctrl Pts',(-4.36131697400006,12.2,-0.396981418000015));
#314092=CARTESIAN_POINT('Ctrl Pts',(-4.36131697400006,5.2,-0.396981418000015));
#314093=CARTESIAN_POINT('Ctrl Pts',(-4.36131697400006,2.2,-0.396981418000015));
#314094=CARTESIAN_POINT('Ctrl Pts',(-4.36305582900006,12.2,-0.397963538000017));
#314095=CARTESIAN_POINT('Ctrl Pts',(-4.36305582900006,5.2,-0.397963538000017));
#314096=CARTESIAN_POINT('Ctrl Pts',(-4.36305582900006,2.2,-0.397963538000017));
#314097=CARTESIAN_POINT('Ctrl Pts',(-4.36479713800006,12.2,-0.398949594000015));
#314098=CARTESIAN_POINT('Ctrl Pts',(-4.36479713800006,5.2,-0.398949594000015));
#314099=CARTESIAN_POINT('Ctrl Pts',(-4.36479713800006,2.2,-0.398949594000015));
#314100=CARTESIAN_POINT('Ctrl Pts',(-4.36654089000006,12.2,-0.399939590000016));
#314101=CARTESIAN_POINT('Ctrl Pts',(-4.36654089000006,5.2,-0.399939590000016));
#314102=CARTESIAN_POINT('Ctrl Pts',(-4.36654089000006,2.2,-0.399939590000016));
#314103=CARTESIAN_POINT('Ctrl Pts',(-4.36828707800006,12.2,-0.400933530000014));
#314104=CARTESIAN_POINT('Ctrl Pts',(-4.36828707800006,5.2,-0.400933530000014));
#314105=CARTESIAN_POINT('Ctrl Pts',(-4.36828707800006,2.2,-0.400933530000014));
#314106=CARTESIAN_POINT('Ctrl Pts',(-4.37003568800006,12.2,-0.401931417000014));
#314107=CARTESIAN_POINT('Ctrl Pts',(-4.37003568800006,5.2,-0.401931417000014));
#314108=CARTESIAN_POINT('Ctrl Pts',(-4.37003568800006,2.2,-0.401931417000014));
#314109=CARTESIAN_POINT('Ctrl Pts',(-4.37178671200006,12.2,-0.402933255000013));
#314110=CARTESIAN_POINT('Ctrl Pts',(-4.37178671200006,5.2,-0.402933255000013));
#314111=CARTESIAN_POINT('Ctrl Pts',(-4.37178671200006,2.2,-0.402933255000013));
#314112=CARTESIAN_POINT('Ctrl Pts',(-4.37354013800006,12.2,-0.403939047000015));
#314113=CARTESIAN_POINT('Ctrl Pts',(-4.37354013800006,5.2,-0.403939047000015));
#314114=CARTESIAN_POINT('Ctrl Pts',(-4.37354013800006,2.2,-0.403939047000015));
#314115=CARTESIAN_POINT('Ctrl Pts',(-4.37529595700005,12.2,-0.404948796000015));
#314116=CARTESIAN_POINT('Ctrl Pts',(-4.37529595700005,5.2,-0.404948796000015));
#314117=CARTESIAN_POINT('Ctrl Pts',(-4.37529595700005,2.2,-0.404948796000015));
#314118=CARTESIAN_POINT('Ctrl Pts',(-4.37705415900006,12.2,-0.405962504000015));
#314119=CARTESIAN_POINT('Ctrl Pts',(-4.37705415900006,5.2,-0.405962504000015));
#314120=CARTESIAN_POINT('Ctrl Pts',(-4.37705415900006,2.2,-0.405962504000015));
#314121=CARTESIAN_POINT('Ctrl Pts',(-4.37881473400005,12.2,-0.406980178000014));
#314122=CARTESIAN_POINT('Ctrl Pts',(-4.37881473400005,5.2,-0.406980178000014));
#314123=CARTESIAN_POINT('Ctrl Pts',(-4.37881473400005,2.2,-0.406980178000014));
#314124=CARTESIAN_POINT('Ctrl Pts',(-4.38057767000006,12.2,-0.408001819000017));
#314125=CARTESIAN_POINT('Ctrl Pts',(-4.38057767000006,5.2,-0.408001819000017));
#314126=CARTESIAN_POINT('Ctrl Pts',(-4.38057767000006,2.2,-0.408001819000017));
#314127=CARTESIAN_POINT('Ctrl Pts',(-4.38234295900005,12.2,-0.409027430000015));
#314128=CARTESIAN_POINT('Ctrl Pts',(-4.38234295900005,5.2,-0.409027430000015));
#314129=CARTESIAN_POINT('Ctrl Pts',(-4.38234295900005,2.2,-0.409027430000015));
#314130=CARTESIAN_POINT('Ctrl Pts',(-4.38411058800006,12.2,-0.410057015000014));
#314131=CARTESIAN_POINT('Ctrl Pts',(-4.38411058800006,5.2,-0.410057015000014));
#314132=CARTESIAN_POINT('Ctrl Pts',(-4.38411058800006,2.2,-0.410057015000014));
#314133=CARTESIAN_POINT('Ctrl Pts',(-4.38588054900006,12.2,-0.411090577000017));
#314134=CARTESIAN_POINT('Ctrl Pts',(-4.38588054900006,5.2,-0.411090577000017));
#314135=CARTESIAN_POINT('Ctrl Pts',(-4.38588054900006,2.2,-0.411090577000017));
#314136=CARTESIAN_POINT('Ctrl Pts',(-4.38765283200006,12.2,-0.412128119000013));
#314137=CARTESIAN_POINT('Ctrl Pts',(-4.38765283200006,5.2,-0.412128119000013));
#314138=CARTESIAN_POINT('Ctrl Pts',(-4.38765283200006,2.2,-0.412128119000013));
#314139=CARTESIAN_POINT('Ctrl Pts',(-4.38942742600006,12.2,-0.413169645000018));
#314140=CARTESIAN_POINT('Ctrl Pts',(-4.38942742600006,5.2,-0.413169645000018));
#314141=CARTESIAN_POINT('Ctrl Pts',(-4.38942742600006,2.2,-0.413169645000018));
#314142=CARTESIAN_POINT('Ctrl Pts',(-4.39120432000006,12.2,-0.414215158000015));
#314143=CARTESIAN_POINT('Ctrl Pts',(-4.39120432000006,5.2,-0.414215158000015));
#314144=CARTESIAN_POINT('Ctrl Pts',(-4.39120432000006,2.2,-0.414215158000015));
#314145=CARTESIAN_POINT('Ctrl Pts',(-4.39298350700006,12.2,-0.415264660000014));
#314146=CARTESIAN_POINT('Ctrl Pts',(-4.39298350700006,5.2,-0.415264660000014));
#314147=CARTESIAN_POINT('Ctrl Pts',(-4.39298350700006,2.2,-0.415264660000014));
#314148=CARTESIAN_POINT('Ctrl Pts',(-4.39476497300006,12.2,-0.416318157000015));
#314149=CARTESIAN_POINT('Ctrl Pts',(-4.39476497300006,5.2,-0.416318157000015));
#314150=CARTESIAN_POINT('Ctrl Pts',(-4.39476497300006,2.2,-0.416318157000015));
#314151=CARTESIAN_POINT('Ctrl Pts',(-4.39654871000006,12.2,-0.417375648000018));
#314152=CARTESIAN_POINT('Ctrl Pts',(-4.39654871000006,5.2,-0.417375648000018));
#314153=CARTESIAN_POINT('Ctrl Pts',(-4.39654871000006,2.2,-0.417375648000018));
#314154=CARTESIAN_POINT('Ctrl Pts',(-4.39833470800005,12.2,-0.418437140000014));
#314155=CARTESIAN_POINT('Ctrl Pts',(-4.39833470800005,5.2,-0.418437140000014));
#314156=CARTESIAN_POINT('Ctrl Pts',(-4.39833470800005,2.2,-0.418437140000014));
#314157=CARTESIAN_POINT('Ctrl Pts',(-4.40012295600006,12.2,-0.419502633000013));
#314158=CARTESIAN_POINT('Ctrl Pts',(-4.40012295600006,5.2,-0.419502633000013));
#314159=CARTESIAN_POINT('Ctrl Pts',(-4.40012295600006,2.2,-0.419502633000013));
#314160=CARTESIAN_POINT('Ctrl Pts',(-4.40191344400006,12.2,-0.420572133000015));
#314161=CARTESIAN_POINT('Ctrl Pts',(-4.40191344400006,5.2,-0.420572133000015));
#314162=CARTESIAN_POINT('Ctrl Pts',(-4.40191344400006,2.2,-0.420572133000015));
#314163=CARTESIAN_POINT('Ctrl Pts',(-4.40370616300005,12.2,-0.421645641000015));
#314164=CARTESIAN_POINT('Ctrl Pts',(-4.40370616300005,5.2,-0.421645641000015));
#314165=CARTESIAN_POINT('Ctrl Pts',(-4.40370616300005,2.2,-0.421645641000015));
#314166=CARTESIAN_POINT('Ctrl Pts',(-4.40550110300006,12.2,-0.422723161000014));
#314167=CARTESIAN_POINT('Ctrl Pts',(-4.40550110300006,5.2,-0.422723161000014));
#314168=CARTESIAN_POINT('Ctrl Pts',(-4.40550110300006,2.2,-0.422723161000014));
#314169=CARTESIAN_POINT('Ctrl Pts',(-4.40729825200005,12.2,-0.423804695000012));
#314170=CARTESIAN_POINT('Ctrl Pts',(-4.40729825200005,5.2,-0.423804695000012));
#314171=CARTESIAN_POINT('Ctrl Pts',(-4.40729825200005,2.2,-0.423804695000012));
#314172=CARTESIAN_POINT('Ctrl Pts',(-4.40909760100006,12.2,-0.424890247000014));
#314173=CARTESIAN_POINT('Ctrl Pts',(-4.40909760100006,5.2,-0.424890247000014));
#314174=CARTESIAN_POINT('Ctrl Pts',(-4.40909760100006,2.2,-0.424890247000014));
#314175=CARTESIAN_POINT('Ctrl Pts',(-4.41089914100006,12.2,-0.425979821000015));
#314176=CARTESIAN_POINT('Ctrl Pts',(-4.41089914100006,5.2,-0.425979821000015));
#314177=CARTESIAN_POINT('Ctrl Pts',(-4.41089914100006,2.2,-0.425979821000015));
#314178=CARTESIAN_POINT('Ctrl Pts',(-4.41270286100006,12.2,-0.427073417000017));
#314179=CARTESIAN_POINT('Ctrl Pts',(-4.41270286100006,5.2,-0.427073417000017));
#314180=CARTESIAN_POINT('Ctrl Pts',(-4.41270286100006,2.2,-0.427073417000017));
#314181=CARTESIAN_POINT('Ctrl Pts',(-4.41450875100006,12.2,-0.428171040000014));
#314182=CARTESIAN_POINT('Ctrl Pts',(-4.41450875100006,5.2,-0.428171040000014));
#314183=CARTESIAN_POINT('Ctrl Pts',(-4.41450875100006,2.2,-0.428171040000014));
#314184=CARTESIAN_POINT('Ctrl Pts',(-4.41631680000006,12.2,-0.429272693000016));
#314185=CARTESIAN_POINT('Ctrl Pts',(-4.41631680000006,5.2,-0.429272693000016));
#314186=CARTESIAN_POINT('Ctrl Pts',(-4.41631680000006,2.2,-0.429272693000016));
#314187=CARTESIAN_POINT('Ctrl Pts',(-4.41812700100006,12.2,-0.430378378000014));
#314188=CARTESIAN_POINT('Ctrl Pts',(-4.41812700100006,5.2,-0.430378378000014));
#314189=CARTESIAN_POINT('Ctrl Pts',(-4.41812700100006,2.2,-0.430378378000014));
#314190=CARTESIAN_POINT('Ctrl Pts',(-4.41993934100006,12.2,-0.431488099000017));
#314191=CARTESIAN_POINT('Ctrl Pts',(-4.41993934100006,5.2,-0.431488099000017));
#314192=CARTESIAN_POINT('Ctrl Pts',(-4.41993934100006,2.2,-0.431488099000017));
#314193=CARTESIAN_POINT('Ctrl Pts',(-4.42175381100006,12.2,-0.432601858000012));
#314194=CARTESIAN_POINT('Ctrl Pts',(-4.42175381100006,5.2,-0.432601858000012));
#314195=CARTESIAN_POINT('Ctrl Pts',(-4.42175381100006,2.2,-0.432601858000012));
#314196=CARTESIAN_POINT('Ctrl Pts',(-4.42357040200006,12.2,-0.433719658000014));
#314197=CARTESIAN_POINT('Ctrl Pts',(-4.42357040200006,5.2,-0.433719658000014));
#314198=CARTESIAN_POINT('Ctrl Pts',(-4.42357040200006,2.2,-0.433719658000014));
#314199=CARTESIAN_POINT('Ctrl Pts',(-4.42538910400006,12.2,-0.434841503000012));
#314200=CARTESIAN_POINT('Ctrl Pts',(-4.42538910400006,5.2,-0.434841503000012));
#314201=CARTESIAN_POINT('Ctrl Pts',(-4.42538910400006,2.2,-0.434841503000012));
#314202=CARTESIAN_POINT('Ctrl Pts',(-4.42720990500006,12.2,-0.435967394000016));
#314203=CARTESIAN_POINT('Ctrl Pts',(-4.42720990500006,5.2,-0.435967394000016));
#314204=CARTESIAN_POINT('Ctrl Pts',(-4.42720990500006,2.2,-0.435967394000016));
#314205=CARTESIAN_POINT('Ctrl Pts',(-4.42903279800006,12.2,-0.437097334000014));
#314206=CARTESIAN_POINT('Ctrl Pts',(-4.42903279800006,5.2,-0.437097334000014));
#314207=CARTESIAN_POINT('Ctrl Pts',(-4.42903279800006,2.2,-0.437097334000014));
#314208=CARTESIAN_POINT('Ctrl Pts',(-4.43085777000006,12.2,-0.438231328000014));
#314209=CARTESIAN_POINT('Ctrl Pts',(-4.43085777000006,5.2,-0.438231328000014));
#314210=CARTESIAN_POINT('Ctrl Pts',(-4.43085777000006,2.2,-0.438231328000014));
#314211=CARTESIAN_POINT('Ctrl Pts',(-4.43268481400006,12.2,-0.439369377000016));
#314212=CARTESIAN_POINT('Ctrl Pts',(-4.43268481400006,5.2,-0.439369377000016));
#314213=CARTESIAN_POINT('Ctrl Pts',(-4.43268481400006,2.2,-0.439369377000016));
#314214=CARTESIAN_POINT('Ctrl Pts',(-4.43451391800005,12.2,-0.440511483000012));
#314215=CARTESIAN_POINT('Ctrl Pts',(-4.43451391800005,5.2,-0.440511483000012));
#314216=CARTESIAN_POINT('Ctrl Pts',(-4.43451391800005,2.2,-0.440511483000012));
#314217=CARTESIAN_POINT('Ctrl Pts',(-4.43634507400006,12.2,-0.441657651000016));
#314218=CARTESIAN_POINT('Ctrl Pts',(-4.43634507400006,5.2,-0.441657651000016));
#314219=CARTESIAN_POINT('Ctrl Pts',(-4.43634507400006,2.2,-0.441657651000016));
#314220=CARTESIAN_POINT('Ctrl Pts',(-4.43817827000006,12.2,-0.442807882000014));
#314221=CARTESIAN_POINT('Ctrl Pts',(-4.43817827000006,5.2,-0.442807882000014));
#314222=CARTESIAN_POINT('Ctrl Pts',(-4.43817827000006,2.2,-0.442807882000014));
#314223=CARTESIAN_POINT('Ctrl Pts',(-4.44001349800006,12.2,-0.443962179000015));
#314224=CARTESIAN_POINT('Ctrl Pts',(-4.44001349800006,5.2,-0.443962179000015));
#314225=CARTESIAN_POINT('Ctrl Pts',(-4.44001349800006,2.2,-0.443962179000015));
#314226=CARTESIAN_POINT('Ctrl Pts',(-4.44185074700005,12.2,-0.445120545000015));
#314227=CARTESIAN_POINT('Ctrl Pts',(-4.44185074700005,5.2,-0.445120545000015));
#314228=CARTESIAN_POINT('Ctrl Pts',(-4.44185074700005,2.2,-0.445120545000015));
#314229=CARTESIAN_POINT('Ctrl Pts',(-4.44369000700005,12.2,-0.446282983000015));
#314230=CARTESIAN_POINT('Ctrl Pts',(-4.44369000700005,5.2,-0.446282983000015));
#314231=CARTESIAN_POINT('Ctrl Pts',(-4.44369000700005,2.2,-0.446282983000015));
#314232=CARTESIAN_POINT('Ctrl Pts',(-4.44553127000006,12.2,-0.447449495000014));
#314233=CARTESIAN_POINT('Ctrl Pts',(-4.44553127000006,5.2,-0.447449495000014));
#314234=CARTESIAN_POINT('Ctrl Pts',(-4.44553127000006,2.2,-0.447449495000014));
#314235=CARTESIAN_POINT('Ctrl Pts',(-4.44737452400005,12.2,-0.448620083000013));
#314236=CARTESIAN_POINT('Ctrl Pts',(-4.44737452400005,5.2,-0.448620083000013));
#314237=CARTESIAN_POINT('Ctrl Pts',(-4.44737452400005,2.2,-0.448620083000013));
#314238=CARTESIAN_POINT('Ctrl Pts',(-4.44921976000006,12.2,-0.449794752000017));
#314239=CARTESIAN_POINT('Ctrl Pts',(-4.44921976000006,5.2,-0.449794752000017));
#314240=CARTESIAN_POINT('Ctrl Pts',(-4.44921976000006,2.2,-0.449794752000017));
#314241=CARTESIAN_POINT('Ctrl Pts',(-4.45106696900006,12.2,-0.450973502000016));
#314242=CARTESIAN_POINT('Ctrl Pts',(-4.45106696900006,5.2,-0.450973502000016));
#314243=CARTESIAN_POINT('Ctrl Pts',(-4.45106696900006,2.2,-0.450973502000016));
#314244=CARTESIAN_POINT('Ctrl Pts',(-4.45291614100006,12.2,-0.452156337000016));
#314245=CARTESIAN_POINT('Ctrl Pts',(-4.45291614100006,5.2,-0.452156337000016));
#314246=CARTESIAN_POINT('Ctrl Pts',(-4.45291614100006,2.2,-0.452156337000016));
#314247=CARTESIAN_POINT('Ctrl Pts',(-4.45476726500006,12.2,-0.453343260000012));
#314248=CARTESIAN_POINT('Ctrl Pts',(-4.45476726500006,5.2,-0.453343260000012));
#314249=CARTESIAN_POINT('Ctrl Pts',(-4.45476726500006,2.2,-0.453343260000012));
#314250=CARTESIAN_POINT('Ctrl Pts',(-4.45662033300006,12.2,-0.454534272000018));
#314251=CARTESIAN_POINT('Ctrl Pts',(-4.45662033300006,5.2,-0.454534272000018));
#314252=CARTESIAN_POINT('Ctrl Pts',(-4.45662033300006,2.2,-0.454534272000018));
#314253=CARTESIAN_POINT('Ctrl Pts',(-4.45847533300006,12.2,-0.455729376000011));
#314254=CARTESIAN_POINT('Ctrl Pts',(-4.45847533300006,5.2,-0.455729376000011));
#314255=CARTESIAN_POINT('Ctrl Pts',(-4.45847533300006,2.2,-0.455729376000011));
#314256=CARTESIAN_POINT('Ctrl Pts',(-4.46033225800006,12.2,-0.456928576000015));
#314257=CARTESIAN_POINT('Ctrl Pts',(-4.46033225800006,5.2,-0.456928576000015));
#314258=CARTESIAN_POINT('Ctrl Pts',(-4.46033225800006,2.2,-0.456928576000015));
#314259=CARTESIAN_POINT('Ctrl Pts',(-4.46219109600006,12.2,-0.458131872000016));
#314260=CARTESIAN_POINT('Ctrl Pts',(-4.46219109600006,5.2,-0.458131872000016));
#314261=CARTESIAN_POINT('Ctrl Pts',(-4.46219109600006,2.2,-0.458131872000016));
#314262=CARTESIAN_POINT('Ctrl Pts',(-4.46405183800006,12.2,-0.459339270000014));
#314263=CARTESIAN_POINT('Ctrl Pts',(-4.46405183800006,5.2,-0.459339270000014));
#314264=CARTESIAN_POINT('Ctrl Pts',(-4.46405183800006,2.2,-0.459339270000014));
#314265=CARTESIAN_POINT('Ctrl Pts',(-4.46591447600006,12.2,-0.460550769000014));
#314266=CARTESIAN_POINT('Ctrl Pts',(-4.46591447600006,5.2,-0.460550769000014));
#314267=CARTESIAN_POINT('Ctrl Pts',(-4.46591447600006,2.2,-0.460550769000014));
#314268=CARTESIAN_POINT('Ctrl Pts',(-4.46777899700006,12.2,-0.461766372000016));
#314269=CARTESIAN_POINT('Ctrl Pts',(-4.46777899700006,5.2,-0.461766372000016));
#314270=CARTESIAN_POINT('Ctrl Pts',(-4.46777899700006,2.2,-0.461766372000016));
#314271=CARTESIAN_POINT('Ctrl Pts',(-4.46964539400006,12.2,-0.462986083000012));
#314272=CARTESIAN_POINT('Ctrl Pts',(-4.46964539400006,5.2,-0.462986083000012));
#314273=CARTESIAN_POINT('Ctrl Pts',(-4.46964539400006,2.2,-0.462986083000012));
#314274=CARTESIAN_POINT('Ctrl Pts',(-4.47151365700006,12.2,-0.464209904000015));
#314275=CARTESIAN_POINT('Ctrl Pts',(-4.47151365700006,5.2,-0.464209904000015));
#314276=CARTESIAN_POINT('Ctrl Pts',(-4.47151365700006,2.2,-0.464209904000015));
#314277=CARTESIAN_POINT('Ctrl Pts',(-4.47338377500006,12.2,-0.465437837000016));
#314278=CARTESIAN_POINT('Ctrl Pts',(-4.47338377500006,5.2,-0.465437837000016));
#314279=CARTESIAN_POINT('Ctrl Pts',(-4.47338377500006,2.2,-0.465437837000016));
#314280=CARTESIAN_POINT('Ctrl Pts',(-4.47525573900006,12.2,-0.466669885000015));
#314281=CARTESIAN_POINT('Ctrl Pts',(-4.47525573900006,5.2,-0.466669885000015));
#314282=CARTESIAN_POINT('Ctrl Pts',(-4.47525573900006,2.2,-0.466669885000015));
#314283=CARTESIAN_POINT('Ctrl Pts',(-4.47712954000006,12.2,-0.467906048000017));
#314284=CARTESIAN_POINT('Ctrl Pts',(-4.47712954000006,5.2,-0.467906048000017));
#314285=CARTESIAN_POINT('Ctrl Pts',(-4.47712954000006,2.2,-0.467906048000017));
#314286=CARTESIAN_POINT('Ctrl Pts',(-4.47900516900006,12.2,-0.469146332000014));
#314287=CARTESIAN_POINT('Ctrl Pts',(-4.47900516900006,5.2,-0.469146332000014));
#314288=CARTESIAN_POINT('Ctrl Pts',(-4.47900516900006,2.2,-0.469146332000014));
#314289=CARTESIAN_POINT('Ctrl Pts',(-4.48088261400006,12.2,-0.470390737000015));
#314290=CARTESIAN_POINT('Ctrl Pts',(-4.48088261400006,5.2,-0.470390737000015));
#314291=CARTESIAN_POINT('Ctrl Pts',(-4.48088261400006,2.2,-0.470390737000015));
#314292=CARTESIAN_POINT('Ctrl Pts',(-4.48276186600006,12.2,-0.471639264000014));
#314293=CARTESIAN_POINT('Ctrl Pts',(-4.48276186600006,5.2,-0.471639264000014));
#314294=CARTESIAN_POINT('Ctrl Pts',(-4.48276186600006,2.2,-0.471639264000014));
#314295=CARTESIAN_POINT('Ctrl Pts',(-4.48464291700006,12.2,-0.472891920000014));
#314296=CARTESIAN_POINT('Ctrl Pts',(-4.48464291700006,5.2,-0.472891920000014));
#314297=CARTESIAN_POINT('Ctrl Pts',(-4.48464291700006,2.2,-0.472891920000014));
#314298=CARTESIAN_POINT('Ctrl Pts',(-4.48652575600006,12.2,-0.474148702000012));
#314299=CARTESIAN_POINT('Ctrl Pts',(-4.48652575600006,5.2,-0.474148702000012));
#314300=CARTESIAN_POINT('Ctrl Pts',(-4.48652575600006,2.2,-0.474148702000012));
#314301=CARTESIAN_POINT('Ctrl Pts',(-4.48841037500006,12.2,-0.475409616000011));
#314302=CARTESIAN_POINT('Ctrl Pts',(-4.48841037500006,5.2,-0.475409616000011));
#314303=CARTESIAN_POINT('Ctrl Pts',(-4.48841037500006,2.2,-0.475409616000011));
#314304=CARTESIAN_POINT('Ctrl Pts',(-4.49029676200006,12.2,-0.476674663000014));
#314305=CARTESIAN_POINT('Ctrl Pts',(-4.49029676200006,5.2,-0.476674663000014));
#314306=CARTESIAN_POINT('Ctrl Pts',(-4.49029676200006,2.2,-0.476674663000014));
#314307=CARTESIAN_POINT('Ctrl Pts',(-4.49218491000006,12.2,-0.477943845000013));
#314308=CARTESIAN_POINT('Ctrl Pts',(-4.49218491000006,5.2,-0.477943845000013));
#314309=CARTESIAN_POINT('Ctrl Pts',(-4.49218491000006,2.2,-0.477943845000013));
#314310=CARTESIAN_POINT('Ctrl Pts',(-4.49407480700006,12.2,-0.479217165000012));
#314311=CARTESIAN_POINT('Ctrl Pts',(-4.49407480700006,5.2,-0.479217165000012));
#314312=CARTESIAN_POINT('Ctrl Pts',(-4.49407480700006,2.2,-0.479217165000012));
#314313=CARTESIAN_POINT('Ctrl Pts',(-4.49596644600006,12.2,-0.480494623000016));
#314314=CARTESIAN_POINT('Ctrl Pts',(-4.49596644600006,5.2,-0.480494623000016));
#314315=CARTESIAN_POINT('Ctrl Pts',(-4.49596644600006,2.2,-0.480494623000016));
#314316=CARTESIAN_POINT('Ctrl Pts',(-4.49785981500006,12.2,-0.481776225000012));
#314317=CARTESIAN_POINT('Ctrl Pts',(-4.49785981500006,5.2,-0.481776225000012));
#314318=CARTESIAN_POINT('Ctrl Pts',(-4.49785981500006,2.2,-0.481776225000012));
#314319=CARTESIAN_POINT('Ctrl Pts',(-4.49975490600006,12.2,-0.483061969000014));
#314320=CARTESIAN_POINT('Ctrl Pts',(-4.49975490600006,5.2,-0.483061969000014));
#314321=CARTESIAN_POINT('Ctrl Pts',(-4.49975490600006,2.2,-0.483061969000014));
#314322=CARTESIAN_POINT('Ctrl Pts',(-4.50165170900005,12.2,-0.484351860000016));
#314323=CARTESIAN_POINT('Ctrl Pts',(-4.50165170900005,5.2,-0.484351860000016));
#314324=CARTESIAN_POINT('Ctrl Pts',(-4.50165170900005,2.2,-0.484351860000016));
#314325=CARTESIAN_POINT('Ctrl Pts',(-4.50355021600005,12.2,-0.485645898000016));
#314326=CARTESIAN_POINT('Ctrl Pts',(-4.50355021600005,5.2,-0.485645898000016));
#314327=CARTESIAN_POINT('Ctrl Pts',(-4.50355021600005,2.2,-0.485645898000016));
#314328=CARTESIAN_POINT('Ctrl Pts',(-4.50545041500006,12.2,-0.486944088000012));
#314329=CARTESIAN_POINT('Ctrl Pts',(-4.50545041500006,5.2,-0.486944088000012));
#314330=CARTESIAN_POINT('Ctrl Pts',(-4.50545041500006,2.2,-0.486944088000012));
#314331=CARTESIAN_POINT('Ctrl Pts',(-4.50735229700006,12.2,-0.488246430000014));
#314332=CARTESIAN_POINT('Ctrl Pts',(-4.50735229700006,5.2,-0.488246430000014));
#314333=CARTESIAN_POINT('Ctrl Pts',(-4.50735229700006,2.2,-0.488246430000014));
#314334=CARTESIAN_POINT('Ctrl Pts',(-4.50925585500006,12.2,-0.489552926000014));
#314335=CARTESIAN_POINT('Ctrl Pts',(-4.50925585500006,5.2,-0.489552926000014));
#314336=CARTESIAN_POINT('Ctrl Pts',(-4.50925585500006,2.2,-0.489552926000014));
#314337=CARTESIAN_POINT('Ctrl Pts',(-4.51116107700006,12.2,-0.490863580000016));
#314338=CARTESIAN_POINT('Ctrl Pts',(-4.51116107700006,5.2,-0.490863580000016));
#314339=CARTESIAN_POINT('Ctrl Pts',(-4.51116107700006,2.2,-0.490863580000016));
#314340=CARTESIAN_POINT('Ctrl Pts',(-4.51306795400006,12.2,-0.492178392000016));
#314341=CARTESIAN_POINT('Ctrl Pts',(-4.51306795400006,5.2,-0.492178392000016));
#314342=CARTESIAN_POINT('Ctrl Pts',(-4.51306795400006,2.2,-0.492178392000016));
#314343=CARTESIAN_POINT('Ctrl Pts',(-4.51497647800006,12.2,-0.493497364000017));
#314344=CARTESIAN_POINT('Ctrl Pts',(-4.51497647800006,5.2,-0.493497364000017));
#314345=CARTESIAN_POINT('Ctrl Pts',(-4.51497647800006,2.2,-0.493497364000017));
#314346=CARTESIAN_POINT('Ctrl Pts',(-4.51688663800006,12.2,-0.494820500000017));
#314347=CARTESIAN_POINT('Ctrl Pts',(-4.51688663800006,5.2,-0.494820500000017));
#314348=CARTESIAN_POINT('Ctrl Pts',(-4.51688663800006,2.2,-0.494820500000017));
#314349=CARTESIAN_POINT('Ctrl Pts',(-4.51879842500006,12.2,-0.496147800000015));
#314350=CARTESIAN_POINT('Ctrl Pts',(-4.51879842500006,5.2,-0.496147800000015));
#314351=CARTESIAN_POINT('Ctrl Pts',(-4.51879842500006,2.2,-0.496147800000015));
#314352=CARTESIAN_POINT('Ctrl Pts',(-4.52071182900006,12.2,-0.497479267000016));
#314353=CARTESIAN_POINT('Ctrl Pts',(-4.52071182900006,5.2,-0.497479267000016));
#314354=CARTESIAN_POINT('Ctrl Pts',(-4.52071182900006,2.2,-0.497479267000016));
#314355=CARTESIAN_POINT('Ctrl Pts',(-4.52262684200006,12.2,-0.498814904000016));
#314356=CARTESIAN_POINT('Ctrl Pts',(-4.52262684200006,5.2,-0.498814904000016));
#314357=CARTESIAN_POINT('Ctrl Pts',(-4.52262684200006,2.2,-0.498814904000016));
#314358=CARTESIAN_POINT('Ctrl Pts',(-4.52454345500006,12.2,-0.500154710000014));
#314359=CARTESIAN_POINT('Ctrl Pts',(-4.52454345500006,5.2,-0.500154710000014));
#314360=CARTESIAN_POINT('Ctrl Pts',(-4.52454345500006,2.2,-0.500154710000014));
#314361=CARTESIAN_POINT('Ctrl Pts',(-4.52646165600005,12.2,-0.501498690000015));
#314362=CARTESIAN_POINT('Ctrl Pts',(-4.52646165600005,5.2,-0.501498690000015));
#314363=CARTESIAN_POINT('Ctrl Pts',(-4.52646165600005,2.2,-0.501498690000015));
#314364=CARTESIAN_POINT('Ctrl Pts',(-4.52838143800006,12.2,-0.502846844000011));
#314365=CARTESIAN_POINT('Ctrl Pts',(-4.52838143800006,5.2,-0.502846844000011));
#314366=CARTESIAN_POINT('Ctrl Pts',(-4.52838143800006,2.2,-0.502846844000011));
#314367=CARTESIAN_POINT('Ctrl Pts',(-4.53030279000005,12.2,-0.504199175000015));
#314368=CARTESIAN_POINT('Ctrl Pts',(-4.53030279000005,5.2,-0.504199175000015));
#314369=CARTESIAN_POINT('Ctrl Pts',(-4.53030279000005,2.2,-0.504199175000015));
#314370=CARTESIAN_POINT('Ctrl Pts',(-4.53222570400006,12.2,-0.505555685000014));
#314371=CARTESIAN_POINT('Ctrl Pts',(-4.53222570400006,5.2,-0.505555685000014));
#314372=CARTESIAN_POINT('Ctrl Pts',(-4.53222570400006,2.2,-0.505555685000014));
#314373=CARTESIAN_POINT('Ctrl Pts',(-4.53415017100006,12.2,-0.506916375000017));
#314374=CARTESIAN_POINT('Ctrl Pts',(-4.53415017100006,5.2,-0.506916375000017));
#314375=CARTESIAN_POINT('Ctrl Pts',(-4.53415017100006,2.2,-0.506916375000017));
#314376=CARTESIAN_POINT('Ctrl Pts',(-4.53607618000006,12.2,-0.508281247000015));
#314377=CARTESIAN_POINT('Ctrl Pts',(-4.53607618000006,5.2,-0.508281247000015));
#314378=CARTESIAN_POINT('Ctrl Pts',(-4.53607618000006,2.2,-0.508281247000015));
#314379=CARTESIAN_POINT('Ctrl Pts',(-4.53800372300006,12.2,-0.509650302000013));
#314380=CARTESIAN_POINT('Ctrl Pts',(-4.53800372300006,5.2,-0.509650302000013));
#314381=CARTESIAN_POINT('Ctrl Pts',(-4.53800372300006,2.2,-0.509650302000013));
#314382=CARTESIAN_POINT('Ctrl Pts',(-4.53993278900006,12.2,-0.511023545000011));
#314383=CARTESIAN_POINT('Ctrl Pts',(-4.53993278900006,5.2,-0.511023545000011));
#314384=CARTESIAN_POINT('Ctrl Pts',(-4.53993278900006,2.2,-0.511023545000011));
#314385=CARTESIAN_POINT('Ctrl Pts',(-4.54186337200006,12.2,-0.512400975000014));
#314386=CARTESIAN_POINT('Ctrl Pts',(-4.54186337200006,5.2,-0.512400975000014));
#314387=CARTESIAN_POINT('Ctrl Pts',(-4.54186337200006,2.2,-0.512400975000014));
#314388=CARTESIAN_POINT('Ctrl Pts',(-4.54379545900006,12.2,-0.513782595000016));
#314389=CARTESIAN_POINT('Ctrl Pts',(-4.54379545900006,5.2,-0.513782595000016));
#314390=CARTESIAN_POINT('Ctrl Pts',(-4.54379545900006,2.2,-0.513782595000016));
#314391=CARTESIAN_POINT('Ctrl Pts',(-4.54572904300006,12.2,-0.515168406000015));
#314392=CARTESIAN_POINT('Ctrl Pts',(-4.54572904300006,5.2,-0.515168406000015));
#314393=CARTESIAN_POINT('Ctrl Pts',(-4.54572904300006,2.2,-0.515168406000015));
#314394=CARTESIAN_POINT('Ctrl Pts',(-4.54766411400006,12.2,-0.516558410000014));
#314395=CARTESIAN_POINT('Ctrl Pts',(-4.54766411400006,5.2,-0.516558410000014));
#314396=CARTESIAN_POINT('Ctrl Pts',(-4.54766411400006,2.2,-0.516558410000014));
#314397=CARTESIAN_POINT('Ctrl Pts',(-4.54960066300006,12.2,-0.517952609000014));
#314398=CARTESIAN_POINT('Ctrl Pts',(-4.54960066300006,5.2,-0.517952609000014));
#314399=CARTESIAN_POINT('Ctrl Pts',(-4.54960066300006,2.2,-0.517952609000014));
#314400=CARTESIAN_POINT('Ctrl Pts',(-4.55153868000005,12.2,-0.519351005000015));
#314401=CARTESIAN_POINT('Ctrl Pts',(-4.55153868000005,5.2,-0.519351005000015));
#314402=CARTESIAN_POINT('Ctrl Pts',(-4.55153868000005,2.2,-0.519351005000015));
#314403=CARTESIAN_POINT('Ctrl Pts',(-4.55347815700006,12.2,-0.520753599000017));
#314404=CARTESIAN_POINT('Ctrl Pts',(-4.55347815700006,5.2,-0.520753599000017));
#314405=CARTESIAN_POINT('Ctrl Pts',(-4.55347815700006,2.2,-0.520753599000017));
#314406=CARTESIAN_POINT('Ctrl Pts',(-4.55541908500006,12.2,-0.522160394000015));
#314407=CARTESIAN_POINT('Ctrl Pts',(-4.55541908500006,5.2,-0.522160394000015));
#314408=CARTESIAN_POINT('Ctrl Pts',(-4.55541908500006,2.2,-0.522160394000015));
#314409=CARTESIAN_POINT('Ctrl Pts',(-4.55736145300006,12.2,-0.523571390000015));
#314410=CARTESIAN_POINT('Ctrl Pts',(-4.55736145300006,5.2,-0.523571390000015));
#314411=CARTESIAN_POINT('Ctrl Pts',(-4.55736145300006,2.2,-0.523571390000015));
#314412=CARTESIAN_POINT('Ctrl Pts',(-4.55930525300006,12.2,-0.524986591000012));
#314413=CARTESIAN_POINT('Ctrl Pts',(-4.55930525300006,5.2,-0.524986591000012));
#314414=CARTESIAN_POINT('Ctrl Pts',(-4.55930525300006,2.2,-0.524986591000012));
#314415=CARTESIAN_POINT('Ctrl Pts',(-4.56125047500006,12.2,-0.526405996000014));
#314416=CARTESIAN_POINT('Ctrl Pts',(-4.56125047500006,5.2,-0.526405996000014));
#314417=CARTESIAN_POINT('Ctrl Pts',(-4.56125047500006,2.2,-0.526405996000014));
#314418=CARTESIAN_POINT('Ctrl Pts',(-4.56319711000006,12.2,-0.527829609000015));
#314419=CARTESIAN_POINT('Ctrl Pts',(-4.56319711000006,5.2,-0.527829609000015));
#314420=CARTESIAN_POINT('Ctrl Pts',(-4.56319711000006,2.2,-0.527829609000015));
#314421=CARTESIAN_POINT('Ctrl Pts',(-4.56514515100006,12.2,-0.529257430000012));
#314422=CARTESIAN_POINT('Ctrl Pts',(-4.56514515100006,5.2,-0.529257430000012));
#314423=CARTESIAN_POINT('Ctrl Pts',(-4.56514515100006,2.2,-0.529257430000012));
#314424=CARTESIAN_POINT('Ctrl Pts',(-4.56709458600006,12.2,-0.530689461000016));
#314425=CARTESIAN_POINT('Ctrl Pts',(-4.56709458600006,5.2,-0.530689461000016));
#314426=CARTESIAN_POINT('Ctrl Pts',(-4.56709458600006,2.2,-0.530689461000016));
#314427=CARTESIAN_POINT('Ctrl Pts',(-4.56904540700006,12.2,-0.532125704000013));
#314428=CARTESIAN_POINT('Ctrl Pts',(-4.56904540700006,5.2,-0.532125704000013));
#314429=CARTESIAN_POINT('Ctrl Pts',(-4.56904540700006,2.2,-0.532125704000013));
#314430=CARTESIAN_POINT('Ctrl Pts',(-4.57099760400006,12.2,-0.533566161000016));
#314431=CARTESIAN_POINT('Ctrl Pts',(-4.57099760400006,5.2,-0.533566161000016));
#314432=CARTESIAN_POINT('Ctrl Pts',(-4.57099760400006,2.2,-0.533566161000016));
#314433=CARTESIAN_POINT('Ctrl Pts',(-4.57295117000006,12.2,-0.535010832000014));
#314434=CARTESIAN_POINT('Ctrl Pts',(-4.57295117000006,5.2,-0.535010832000014));
#314435=CARTESIAN_POINT('Ctrl Pts',(-4.57295117000006,2.2,-0.535010832000014));
#314436=CARTESIAN_POINT('Ctrl Pts',(-4.57490609300006,12.2,-0.536459721000018));
#314437=CARTESIAN_POINT('Ctrl Pts',(-4.57490609300006,5.2,-0.536459721000018));
#314438=CARTESIAN_POINT('Ctrl Pts',(-4.57490609300006,2.2,-0.536459721000018));
#314439=CARTESIAN_POINT('Ctrl Pts',(-4.57686236600006,12.2,-0.537912827000016));
#314440=CARTESIAN_POINT('Ctrl Pts',(-4.57686236600006,5.2,-0.537912827000016));
#314441=CARTESIAN_POINT('Ctrl Pts',(-4.57686236600006,2.2,-0.537912827000016));
#314442=CARTESIAN_POINT('Ctrl Pts',(-4.57881998000006,12.2,-0.539370154000016));
#314443=CARTESIAN_POINT('Ctrl Pts',(-4.57881998000006,5.2,-0.539370154000016));
#314444=CARTESIAN_POINT('Ctrl Pts',(-4.57881998000006,2.2,-0.539370154000016));
#314445=CARTESIAN_POINT('Ctrl Pts',(-4.58077892400006,12.2,-0.540831701000015));
#314446=CARTESIAN_POINT('Ctrl Pts',(-4.58077892400006,5.2,-0.540831701000015));
#314447=CARTESIAN_POINT('Ctrl Pts',(-4.58077892400006,2.2,-0.540831701000015));
#314448=CARTESIAN_POINT('Ctrl Pts',(-4.58273919000006,12.2,-0.542297472000013));
#314449=CARTESIAN_POINT('Ctrl Pts',(-4.58273919000006,5.2,-0.542297472000013));
#314450=CARTESIAN_POINT('Ctrl Pts',(-4.58273919000006,2.2,-0.542297472000013));
#314451=CARTESIAN_POINT('Ctrl Pts',(-4.58470077000006,12.2,-0.543767466000014));
#314452=CARTESIAN_POINT('Ctrl Pts',(-4.58470077000006,5.2,-0.543767466000014));
#314453=CARTESIAN_POINT('Ctrl Pts',(-4.58470077000006,2.2,-0.543767466000014));
#314454=CARTESIAN_POINT('Ctrl Pts',(-4.58666365300005,12.2,-0.545241687000013));
#314455=CARTESIAN_POINT('Ctrl Pts',(-4.58666365300005,5.2,-0.545241687000013));
#314456=CARTESIAN_POINT('Ctrl Pts',(-4.58666365300005,2.2,-0.545241687000013));
#314457=CARTESIAN_POINT('Ctrl Pts',(-4.58862783200006,12.2,-0.546720135000012));
#314458=CARTESIAN_POINT('Ctrl Pts',(-4.58862783200006,5.2,-0.546720135000012));
#314459=CARTESIAN_POINT('Ctrl Pts',(-4.58862783200006,2.2,-0.546720135000012));
#314460=CARTESIAN_POINT('Ctrl Pts',(-4.59059329600006,12.2,-0.548202811000014));
#314461=CARTESIAN_POINT('Ctrl Pts',(-4.59059329600006,5.2,-0.548202811000014));
#314462=CARTESIAN_POINT('Ctrl Pts',(-4.59059329600006,2.2,-0.548202811000014));
#314463=CARTESIAN_POINT('Ctrl Pts',(-4.59256003700006,12.2,-0.549689718000015));
#314464=CARTESIAN_POINT('Ctrl Pts',(-4.59256003700006,5.2,-0.549689718000015));
#314465=CARTESIAN_POINT('Ctrl Pts',(-4.59256003700006,2.2,-0.549689718000015));
#314466=CARTESIAN_POINT('Ctrl Pts',(-4.59452804600006,12.2,-0.551180856000015));
#314467=CARTESIAN_POINT('Ctrl Pts',(-4.59452804600006,5.2,-0.551180856000015));
#314468=CARTESIAN_POINT('Ctrl Pts',(-4.59452804600006,2.2,-0.551180856000015));
#314469=CARTESIAN_POINT('Ctrl Pts',(-4.59649731300006,12.2,-0.552676228000015));
#314470=CARTESIAN_POINT('Ctrl Pts',(-4.59649731300006,5.2,-0.552676228000015));
#314471=CARTESIAN_POINT('Ctrl Pts',(-4.59649731300006,2.2,-0.552676228000015));
#314472=CARTESIAN_POINT('Ctrl Pts',(-4.59846783000006,12.2,-0.554175834000015));
#314473=CARTESIAN_POINT('Ctrl Pts',(-4.59846783000006,5.2,-0.554175834000015));
#314474=CARTESIAN_POINT('Ctrl Pts',(-4.59846783000006,2.2,-0.554175834000015));
#314475=CARTESIAN_POINT('Ctrl Pts',(-4.60043958800005,12.2,-0.555679676000014));
#314476=CARTESIAN_POINT('Ctrl Pts',(-4.60043958800005,5.2,-0.555679676000014));
#314477=CARTESIAN_POINT('Ctrl Pts',(-4.60043958800005,2.2,-0.555679676000014));
#314478=CARTESIAN_POINT('Ctrl Pts',(-4.60241257700006,12.2,-0.557187755000013));
#314479=CARTESIAN_POINT('Ctrl Pts',(-4.60241257700006,5.2,-0.557187755000013));
#314480=CARTESIAN_POINT('Ctrl Pts',(-4.60241257700006,2.2,-0.557187755000013));
#314481=CARTESIAN_POINT('Ctrl Pts',(-4.60438678900006,12.2,-0.558700072000011));
#314482=CARTESIAN_POINT('Ctrl Pts',(-4.60438678900006,5.2,-0.558700072000011));
#314483=CARTESIAN_POINT('Ctrl Pts',(-4.60438678900006,2.2,-0.558700072000011));
#314484=CARTESIAN_POINT('Ctrl Pts',(-4.60636221500006,12.2,-0.560216630000014));
#314485=CARTESIAN_POINT('Ctrl Pts',(-4.60636221500006,5.2,-0.560216630000014));
#314486=CARTESIAN_POINT('Ctrl Pts',(-4.60636221500006,2.2,-0.560216630000014));
#314487=CARTESIAN_POINT('Ctrl Pts',(-4.60833884500006,12.2,-0.561737429000013));
#314488=CARTESIAN_POINT('Ctrl Pts',(-4.60833884500006,5.2,-0.561737429000013));
#314489=CARTESIAN_POINT('Ctrl Pts',(-4.60833884500006,2.2,-0.561737429000013));
#314490=CARTESIAN_POINT('Ctrl Pts',(-4.61031667200006,12.2,-0.563262470000012));
#314491=CARTESIAN_POINT('Ctrl Pts',(-4.61031667200006,5.2,-0.563262470000012));
#314492=CARTESIAN_POINT('Ctrl Pts',(-4.61031667200006,2.2,-0.563262470000012));
#314493=CARTESIAN_POINT('Ctrl Pts',(-4.61229568600006,12.2,-0.564791756000016));
#314494=CARTESIAN_POINT('Ctrl Pts',(-4.61229568600006,5.2,-0.564791756000016));
#314495=CARTESIAN_POINT('Ctrl Pts',(-4.61229568600006,2.2,-0.564791756000016));
#314496=CARTESIAN_POINT('Ctrl Pts',(-4.61427587700006,12.2,-0.566325286000016));
#314497=CARTESIAN_POINT('Ctrl Pts',(-4.61427587700006,5.2,-0.566325286000016));
#314498=CARTESIAN_POINT('Ctrl Pts',(-4.61427587700006,2.2,-0.566325286000016));
#314499=CARTESIAN_POINT('Ctrl Pts',(-4.61625723700006,12.2,-0.567863064000012));
#314500=CARTESIAN_POINT('Ctrl Pts',(-4.61625723700006,5.2,-0.567863064000012));
#314501=CARTESIAN_POINT('Ctrl Pts',(-4.61625723700006,2.2,-0.567863064000012));
#314502=CARTESIAN_POINT('Ctrl Pts',(-4.61823975700006,12.2,-0.569405089000017));
#314503=CARTESIAN_POINT('Ctrl Pts',(-4.61823975700006,5.2,-0.569405089000017));
#314504=CARTESIAN_POINT('Ctrl Pts',(-4.61823975700006,2.2,-0.569405089000017));
#314505=CARTESIAN_POINT('Ctrl Pts',(-4.62022343000006,12.2,-0.570951362000014));
#314506=CARTESIAN_POINT('Ctrl Pts',(-4.62022343000006,5.2,-0.570951362000014));
#314507=CARTESIAN_POINT('Ctrl Pts',(-4.62022343000006,2.2,-0.570951362000014));
#314508=CARTESIAN_POINT('Ctrl Pts',(-4.62220824300006,12.2,-0.572501887000012));
#314509=CARTESIAN_POINT('Ctrl Pts',(-4.62220824300006,5.2,-0.572501887000012));
#314510=CARTESIAN_POINT('Ctrl Pts',(-4.62220824300006,2.2,-0.572501887000012));
#314511=CARTESIAN_POINT('Ctrl Pts',(-4.62419419100006,12.2,-0.574056662000015));
#314512=CARTESIAN_POINT('Ctrl Pts',(-4.62419419100006,5.2,-0.574056662000015));
#314513=CARTESIAN_POINT('Ctrl Pts',(-4.62419419100006,2.2,-0.574056662000015));
#314514=CARTESIAN_POINT('Ctrl Pts',(-4.62618126300006,12.2,-0.575615691000015));
#314515=CARTESIAN_POINT('Ctrl Pts',(-4.62618126300006,5.2,-0.575615691000015));
#314516=CARTESIAN_POINT('Ctrl Pts',(-4.62618126300006,2.2,-0.575615691000015));
#314517=CARTESIAN_POINT('Ctrl Pts',(-4.62816945000006,12.2,-0.577178973000017));
#314518=CARTESIAN_POINT('Ctrl Pts',(-4.62816945000006,5.2,-0.577178973000017));
#314519=CARTESIAN_POINT('Ctrl Pts',(-4.62816945000006,2.2,-0.577178973000017));
#314520=CARTESIAN_POINT('Ctrl Pts',(-4.63015874400006,12.2,-0.578746510000014));
#314521=CARTESIAN_POINT('Ctrl Pts',(-4.63015874400006,5.2,-0.578746510000014));
#314522=CARTESIAN_POINT('Ctrl Pts',(-4.63015874400006,2.2,-0.578746510000014));
#314523=CARTESIAN_POINT('Ctrl Pts',(-4.63214913600006,12.2,-0.580318304000014));
#314524=CARTESIAN_POINT('Ctrl Pts',(-4.63214913600006,5.2,-0.580318304000014));
#314525=CARTESIAN_POINT('Ctrl Pts',(-4.63214913600006,2.2,-0.580318304000014));
#314526=CARTESIAN_POINT('Ctrl Pts',(-4.63414061700006,12.2,-0.581894355000014));
#314527=CARTESIAN_POINT('Ctrl Pts',(-4.63414061700006,5.2,-0.581894355000014));
#314528=CARTESIAN_POINT('Ctrl Pts',(-4.63414061700006,2.2,-0.581894355000014));
#314529=CARTESIAN_POINT('Ctrl Pts',(-4.63613317800006,12.2,-0.583474665000012));
#314530=CARTESIAN_POINT('Ctrl Pts',(-4.63613317800006,5.2,-0.583474665000012));
#314531=CARTESIAN_POINT('Ctrl Pts',(-4.63613317800006,2.2,-0.583474665000012));
#314532=CARTESIAN_POINT('Ctrl Pts',(-4.63812681200006,12.2,-0.585059233000016));
#314533=CARTESIAN_POINT('Ctrl Pts',(-4.63812681200006,5.2,-0.585059233000016));
#314534=CARTESIAN_POINT('Ctrl Pts',(-4.63812681200006,2.2,-0.585059233000016));
#314535=CARTESIAN_POINT('Ctrl Pts',(-4.64012150800006,12.2,-0.586648064000013));
#314536=CARTESIAN_POINT('Ctrl Pts',(-4.64012150800006,5.2,-0.586648064000013));
#314537=CARTESIAN_POINT('Ctrl Pts',(-4.64012150800006,2.2,-0.586648064000013));
#314538=CARTESIAN_POINT('Ctrl Pts',(-4.64211725700006,12.2,-0.588241155000016));
#314539=CARTESIAN_POINT('Ctrl Pts',(-4.64211725700006,5.2,-0.588241155000016));
#314540=CARTESIAN_POINT('Ctrl Pts',(-4.64211725700006,2.2,-0.588241155000016));
#314541=CARTESIAN_POINT('Ctrl Pts',(-4.64411405100006,12.2,-0.589838511000016));
#314542=CARTESIAN_POINT('Ctrl Pts',(-4.64411405100006,5.2,-0.589838511000016));
#314543=CARTESIAN_POINT('Ctrl Pts',(-4.64411405100006,2.2,-0.589838511000016));
#314544=CARTESIAN_POINT('Ctrl Pts',(-4.64611188200006,12.2,-0.591440130000014));
#314545=CARTESIAN_POINT('Ctrl Pts',(-4.64611188200006,5.2,-0.591440130000014));
#314546=CARTESIAN_POINT('Ctrl Pts',(-4.64611188200006,2.2,-0.591440130000014));
#314547=CARTESIAN_POINT('Ctrl Pts',(-4.64811073900006,12.2,-0.593046014000014));
#314548=CARTESIAN_POINT('Ctrl Pts',(-4.64811073900006,5.2,-0.593046014000014));
#314549=CARTESIAN_POINT('Ctrl Pts',(-4.64811073900006,2.2,-0.593046014000014));
#314550=CARTESIAN_POINT('Ctrl Pts',(-4.65011061600006,12.2,-0.594656164000016));
#314551=CARTESIAN_POINT('Ctrl Pts',(-4.65011061600006,5.2,-0.594656164000016));
#314552=CARTESIAN_POINT('Ctrl Pts',(-4.65011061600006,2.2,-0.594656164000016));
#314553=CARTESIAN_POINT('Ctrl Pts',(-4.65211150200005,12.2,-0.596270581000016));
#314554=CARTESIAN_POINT('Ctrl Pts',(-4.65211150200005,5.2,-0.596270581000016));
#314555=CARTESIAN_POINT('Ctrl Pts',(-4.65211150200005,2.2,-0.596270581000016));
#314556=CARTESIAN_POINT('Ctrl Pts',(-4.65411338900006,12.2,-0.597889268000014));
#314557=CARTESIAN_POINT('Ctrl Pts',(-4.65411338900006,5.2,-0.597889268000014));
#314558=CARTESIAN_POINT('Ctrl Pts',(-4.65411338900006,2.2,-0.597889268000014));
#314559=CARTESIAN_POINT('Ctrl Pts',(-4.65611626900006,12.2,-0.599512222000014));
#314560=CARTESIAN_POINT('Ctrl Pts',(-4.65611626900006,5.2,-0.599512222000014));
#314561=CARTESIAN_POINT('Ctrl Pts',(-4.65611626900006,2.2,-0.599512222000014));
#314562=CARTESIAN_POINT('Ctrl Pts',(-4.65812013300006,12.2,-0.601139448000012));
#314563=CARTESIAN_POINT('Ctrl Pts',(-4.65812013300006,5.2,-0.601139448000012));
#314564=CARTESIAN_POINT('Ctrl Pts',(-4.65812013300006,2.2,-0.601139448000012));
#314565=CARTESIAN_POINT('Ctrl Pts',(-4.66012497200006,12.2,-0.602770944000017));
#314566=CARTESIAN_POINT('Ctrl Pts',(-4.66012497200006,5.2,-0.602770944000017));
#314567=CARTESIAN_POINT('Ctrl Pts',(-4.66012497200006,2.2,-0.602770944000017));
#314568=CARTESIAN_POINT('Ctrl Pts',(-4.66213077800006,12.2,-0.604406713000016));
#314569=CARTESIAN_POINT('Ctrl Pts',(-4.66213077800006,5.2,-0.604406713000016));
#314570=CARTESIAN_POINT('Ctrl Pts',(-4.66213077800006,2.2,-0.604406713000016));
#314571=CARTESIAN_POINT('Ctrl Pts',(-4.66413754100006,12.2,-0.606046755000014));
#314572=CARTESIAN_POINT('Ctrl Pts',(-4.66413754100006,5.2,-0.606046755000014));
#314573=CARTESIAN_POINT('Ctrl Pts',(-4.66413754100006,2.2,-0.606046755000014));
#314574=CARTESIAN_POINT('Ctrl Pts',(-4.66614525400006,12.2,-0.607691072000014));
#314575=CARTESIAN_POINT('Ctrl Pts',(-4.66614525400006,5.2,-0.607691072000014));
#314576=CARTESIAN_POINT('Ctrl Pts',(-4.66614525400006,2.2,-0.607691072000014));
#314577=CARTESIAN_POINT('Ctrl Pts',(-4.66815390600006,12.2,-0.609339663000017));
#314578=CARTESIAN_POINT('Ctrl Pts',(-4.66815390600006,5.2,-0.609339663000017));
#314579=CARTESIAN_POINT('Ctrl Pts',(-4.66815390600006,2.2,-0.609339663000017));
#314580=CARTESIAN_POINT('Ctrl Pts',(-4.67016348800006,12.2,-0.610992530000014));
#314581=CARTESIAN_POINT('Ctrl Pts',(-4.67016348800006,5.2,-0.610992530000014));
#314582=CARTESIAN_POINT('Ctrl Pts',(-4.67016348800006,2.2,-0.610992530000014));
#314583=CARTESIAN_POINT('Ctrl Pts',(-4.67217399200006,12.2,-0.612649674000014));
#314584=CARTESIAN_POINT('Ctrl Pts',(-4.67217399200006,5.2,-0.612649674000014));
#314585=CARTESIAN_POINT('Ctrl Pts',(-4.67217399200006,2.2,-0.612649674000014));
#314586=CARTESIAN_POINT('Ctrl Pts',(-4.67418540900006,12.2,-0.614311096000013));
#314587=CARTESIAN_POINT('Ctrl Pts',(-4.67418540900006,5.2,-0.614311096000013));
#314588=CARTESIAN_POINT('Ctrl Pts',(-4.67418540900006,2.2,-0.614311096000013));
#314589=CARTESIAN_POINT('Ctrl Pts',(-4.67619773200005,12.2,-0.615976798000015));
#314590=CARTESIAN_POINT('Ctrl Pts',(-4.67619773200005,5.2,-0.615976798000015));
#314591=CARTESIAN_POINT('Ctrl Pts',(-4.67619773200005,2.2,-0.615976798000015));
#314592=CARTESIAN_POINT('Ctrl Pts',(-4.67821095300006,12.2,-0.617646778000012));
#314593=CARTESIAN_POINT('Ctrl Pts',(-4.67821095300006,5.2,-0.617646778000012));
#314594=CARTESIAN_POINT('Ctrl Pts',(-4.67821095300006,2.2,-0.617646778000012));
#314595=CARTESIAN_POINT('Ctrl Pts',(-4.68022506300006,12.2,-0.619321038000016));
#314596=CARTESIAN_POINT('Ctrl Pts',(-4.68022506300006,5.2,-0.619321038000016));
#314597=CARTESIAN_POINT('Ctrl Pts',(-4.68022506300006,2.2,-0.619321038000016));
#314598=CARTESIAN_POINT('Ctrl Pts',(-4.68224005500006,12.2,-0.620999580000015));
#314599=CARTESIAN_POINT('Ctrl Pts',(-4.68224005500006,5.2,-0.620999580000015));
#314600=CARTESIAN_POINT('Ctrl Pts',(-4.68224005500006,2.2,-0.620999580000015));
#314601=CARTESIAN_POINT('Ctrl Pts',(-4.68425592000006,12.2,-0.622682404000017));
#314602=CARTESIAN_POINT('Ctrl Pts',(-4.68425592000006,5.2,-0.622682404000017));
#314603=CARTESIAN_POINT('Ctrl Pts',(-4.68425592000006,2.2,-0.622682404000017));
#314604=CARTESIAN_POINT('Ctrl Pts',(-4.68627265000006,12.2,-0.624369510000014));
#314605=CARTESIAN_POINT('Ctrl Pts',(-4.68627265000006,5.2,-0.624369510000014));
#314606=CARTESIAN_POINT('Ctrl Pts',(-4.68627265000006,2.2,-0.624369510000014));
#314607=CARTESIAN_POINT('Ctrl Pts',(-4.68829023200006,12.2,-0.626060900000014));
#314608=CARTESIAN_POINT('Ctrl Pts',(-4.68829023200006,5.2,-0.626060900000014));
#314609=CARTESIAN_POINT('Ctrl Pts',(-4.68829023200006,2.2,-0.626060900000014));
#314610=CARTESIAN_POINT('Ctrl Pts',(-4.69030865600006,12.2,-0.627756574000014));
#314611=CARTESIAN_POINT('Ctrl Pts',(-4.69030865600006,5.2,-0.627756574000014));
#314612=CARTESIAN_POINT('Ctrl Pts',(-4.69030865600006,2.2,-0.627756574000014));
#314613=CARTESIAN_POINT('Ctrl Pts',(-4.69232791400006,12.2,-0.629456535000017));
#314614=CARTESIAN_POINT('Ctrl Pts',(-4.69232791400006,5.2,-0.629456535000017));
#314615=CARTESIAN_POINT('Ctrl Pts',(-4.69232791400006,2.2,-0.629456535000017));
#314616=CARTESIAN_POINT('Ctrl Pts',(-4.69434799200006,12.2,-0.631160781000015));
#314617=CARTESIAN_POINT('Ctrl Pts',(-4.69434799200006,5.2,-0.631160781000015));
#314618=CARTESIAN_POINT('Ctrl Pts',(-4.69434799200006,2.2,-0.631160781000015));
#314619=CARTESIAN_POINT('Ctrl Pts',(-4.69636888500006,12.2,-0.632869317000013));
#314620=CARTESIAN_POINT('Ctrl Pts',(-4.69636888500006,5.2,-0.632869317000013));
#314621=CARTESIAN_POINT('Ctrl Pts',(-4.69636888500006,2.2,-0.632869317000013));
#314622=CARTESIAN_POINT('Ctrl Pts',(-4.69839058500006,12.2,-0.634582138000015));
#314623=CARTESIAN_POINT('Ctrl Pts',(-4.69839058500006,5.2,-0.634582138000015));
#314624=CARTESIAN_POINT('Ctrl Pts',(-4.69839058500006,2.2,-0.634582138000015));
#314625=CARTESIAN_POINT('Ctrl Pts',(-4.70041308900006,12.2,-0.636299249000012));
#314626=CARTESIAN_POINT('Ctrl Pts',(-4.70041308900006,5.2,-0.636299249000012));
#314627=CARTESIAN_POINT('Ctrl Pts',(-4.70041308900006,2.2,-0.636299249000012));
#314628=CARTESIAN_POINT('Ctrl Pts',(-4.70243639600006,12.2,-0.638020648000013));
#314629=CARTESIAN_POINT('Ctrl Pts',(-4.70243639600006,5.2,-0.638020648000013));
#314630=CARTESIAN_POINT('Ctrl Pts',(-4.70243639600006,2.2,-0.638020648000013));
#314631=CARTESIAN_POINT('Ctrl Pts',(-4.70405568100006,12.2,-0.639401197000016));
#314632=CARTESIAN_POINT('Ctrl Pts',(-4.70405568100006,5.2,-0.639401197000016));
#314633=CARTESIAN_POINT('Ctrl Pts',(-4.70405568100006,2.2,-0.639401197000016));
#314634=CARTESIAN_POINT('Ctrl Pts',(-4.70527050400006,12.2,-0.640438538000012));
#314635=CARTESIAN_POINT('Ctrl Pts',(-4.70527050400006,5.2,-0.640438538000012));
#314636=CARTESIAN_POINT('Ctrl Pts',(-4.70527050400006,2.2,-0.640438538000012));
#314637=CARTESIAN_POINT('Ctrl Pts',(-4.70608054600006,12.2,-0.641130957000016));
#314638=CARTESIAN_POINT('Ctrl Pts',(-4.70608054600006,5.2,-0.641130957000016));
#314639=CARTESIAN_POINT('Ctrl Pts',(-4.70608054600006,2.2,-0.641130957000016));
#314640=CARTESIAN_POINT('Ctrl Pts',(-4.70648560700006,12.2,-0.641477381000013));
#314641=CARTESIAN_POINT('Ctrl Pts',(-4.70648560700006,5.2,-0.641477381000013));
#314642=CARTESIAN_POINT('Ctrl Pts',(-4.70648560700006,2.2,-0.641477381000013));
#314643=CARTESIAN_POINT('',(-4.70648560700006,2.7,-0.641477381000014));
#314644=CARTESIAN_POINT('',(-4.70648560700006,12.2,-0.641477381000013));
#314645=CARTESIAN_POINT('Ctrl Pts',(-3.98564433100006,2.7,-0.253971246000013));
#314646=CARTESIAN_POINT('Ctrl Pts',(-3.98580310824698,2.7,-0.25398196602194));
#314647=CARTESIAN_POINT('Ctrl Pts',(-3.98596177671456,2.7000000000014,-0.25399427786866));
#314648=CARTESIAN_POINT('Ctrl Pts',(-3.98645074029173,2.7000000000014,-0.254033260508237));
#314649=CARTESIAN_POINT('Ctrl Pts',(-3.98679793600037,2.70000000000153,
-0.254063570547946));
#314650=CARTESIAN_POINT('Ctrl Pts',(-3.98827065862374,2.70000000000153,
-0.254198213319473));
#314651=CARTESIAN_POINT('Ctrl Pts',(-3.98949352013573,2.70000000000098,
-0.254327938167664));
#314652=CARTESIAN_POINT('Ctrl Pts',(-3.99485063526251,2.70000000000098,
-0.2549415055447));
#314653=CARTESIAN_POINT('Ctrl Pts',(-3.9993227241105,2.7,-0.255583772964764));
#314654=CARTESIAN_POINT('Ctrl Pts',(-4.0189152228829,2.7,-0.258723793406327));
#314655=CARTESIAN_POINT('Ctrl Pts',(-4.03518303527141,2.7,-0.262265975327654));
#314656=CARTESIAN_POINT('Ctrl Pts',(-4.09406179711125,2.7,-0.277029537551965));
#314657=CARTESIAN_POINT('Ctrl Pts',(-4.14889894882159,2.7,-0.295015074741555));
#314658=CARTESIAN_POINT('Ctrl Pts',(-4.34245093015488,2.7,-0.378980348471285));
#314659=CARTESIAN_POINT('Ctrl Pts',(-4.51394467642948,2.7,-0.476808851243891));
#314660=CARTESIAN_POINT('Ctrl Pts',(-4.70648560700006,2.7,-0.641477381000013));
#314661=CARTESIAN_POINT('Origin',(-5.66300478732629E-14,15.2,-1.77635683940025E-14));
#314662=CARTESIAN_POINT('',(-4.64916443400006,2.7,-0.973534832000015));
#314663=CARTESIAN_POINT('',(-4.64916443400006,12.2,-0.973534832000014));
#314664=CARTESIAN_POINT('Origin',(-5.66300478732629E-14,2.7,-1.92943768261394E-14));
#314665=CARTESIAN_POINT('Ctrl Pts',(-4.64916443400006,12.2,-0.973534832000014));
#314666=CARTESIAN_POINT('Ctrl Pts',(-4.64916443400006,5.2,-0.973534832000014));
#314667=CARTESIAN_POINT('Ctrl Pts',(-4.64916443400006,2.2,-0.973534832000014));
#314668=CARTESIAN_POINT('Ctrl Pts',(-4.64866667400006,12.2,-0.973725406000017));
#314669=CARTESIAN_POINT('Ctrl Pts',(-4.64866667400006,5.2,-0.973725406000017));
#314670=CARTESIAN_POINT('Ctrl Pts',(-4.64866667400006,2.2,-0.973725406000017));
#314671=CARTESIAN_POINT('Ctrl Pts',(-4.64767137300006,12.2,-0.974106179000014));
#314672=CARTESIAN_POINT('Ctrl Pts',(-4.64767137300006,5.2,-0.974106179000014));
#314673=CARTESIAN_POINT('Ctrl Pts',(-4.64767137300006,2.2,-0.974106179000014));
#314674=CARTESIAN_POINT('Ctrl Pts',(-4.64617907800006,12.2,-0.974676206000016));
#314675=CARTESIAN_POINT('Ctrl Pts',(-4.64617907800006,5.2,-0.974676206000016));
#314676=CARTESIAN_POINT('Ctrl Pts',(-4.64617907800006,2.2,-0.974676206000016));
#314677=CARTESIAN_POINT('Ctrl Pts',(-4.64419066700006,12.2,-0.975433980000013));
#314678=CARTESIAN_POINT('Ctrl Pts',(-4.64419066700006,5.2,-0.975433980000013));
#314679=CARTESIAN_POINT('Ctrl Pts',(-4.64419066700006,2.2,-0.975433980000013));
#314680=CARTESIAN_POINT('Ctrl Pts',(-4.64170734400006,12.2,-0.976377425000017));
#314681=CARTESIAN_POINT('Ctrl Pts',(-4.64170734400006,5.2,-0.976377425000017));
#314682=CARTESIAN_POINT('Ctrl Pts',(-4.64170734400006,2.2,-0.976377425000017));
#314683=CARTESIAN_POINT('Ctrl Pts',(-4.63922621400005,12.2,-0.977317099000015));
#314684=CARTESIAN_POINT('Ctrl Pts',(-4.63922621400005,5.2,-0.977317099000015));
#314685=CARTESIAN_POINT('Ctrl Pts',(-4.63922621400005,2.2,-0.977317099000015));
#314686=CARTESIAN_POINT('Ctrl Pts',(-4.63674727900006,12.2,-0.978253002000016));
#314687=CARTESIAN_POINT('Ctrl Pts',(-4.63674727900006,5.2,-0.978253002000016));
#314688=CARTESIAN_POINT('Ctrl Pts',(-4.63674727900006,2.2,-0.978253002000016));
#314689=CARTESIAN_POINT('Ctrl Pts',(-4.63427054300006,12.2,-0.979185137000016));
#314690=CARTESIAN_POINT('Ctrl Pts',(-4.63427054300006,5.2,-0.979185137000016));
#314691=CARTESIAN_POINT('Ctrl Pts',(-4.63427054300006,2.2,-0.979185137000016));
#314692=CARTESIAN_POINT('Ctrl Pts',(-4.63179601100006,12.2,-0.980113505000015));
#314693=CARTESIAN_POINT('Ctrl Pts',(-4.63179601100006,5.2,-0.980113505000015));
#314694=CARTESIAN_POINT('Ctrl Pts',(-4.63179601100006,2.2,-0.980113505000015));
#314695=CARTESIAN_POINT('Ctrl Pts',(-4.62932369100006,12.2,-0.981038110000014));
#314696=CARTESIAN_POINT('Ctrl Pts',(-4.62932369100006,5.2,-0.981038110000014));
#314697=CARTESIAN_POINT('Ctrl Pts',(-4.62932369100006,2.2,-0.981038110000014));
#314698=CARTESIAN_POINT('Ctrl Pts',(-4.62685359100006,12.2,-0.981958957000018));
#314699=CARTESIAN_POINT('Ctrl Pts',(-4.62685359100006,5.2,-0.981958957000018));
#314700=CARTESIAN_POINT('Ctrl Pts',(-4.62685359100006,2.2,-0.981958957000018));
#314701=CARTESIAN_POINT('Ctrl Pts',(-4.62438572200006,12.2,-0.982876050000012));
#314702=CARTESIAN_POINT('Ctrl Pts',(-4.62438572200006,5.2,-0.982876050000012));
#314703=CARTESIAN_POINT('Ctrl Pts',(-4.62438572200006,2.2,-0.982876050000012));
#314704=CARTESIAN_POINT('Ctrl Pts',(-4.62192009200006,12.2,-0.983789392000016));
#314705=CARTESIAN_POINT('Ctrl Pts',(-4.62192009200006,5.2,-0.983789392000016));
#314706=CARTESIAN_POINT('Ctrl Pts',(-4.62192009200006,2.2,-0.983789392000016));
#314707=CARTESIAN_POINT('Ctrl Pts',(-4.61945671200006,12.2,-0.984698988000012));
#314708=CARTESIAN_POINT('Ctrl Pts',(-4.61945671200006,5.2,-0.984698988000012));
#314709=CARTESIAN_POINT('Ctrl Pts',(-4.61945671200006,2.2,-0.984698988000012));
#314710=CARTESIAN_POINT('Ctrl Pts',(-4.61699559000006,12.2,-0.985604844000014));
#314711=CARTESIAN_POINT('Ctrl Pts',(-4.61699559000006,5.2,-0.985604844000014));
#314712=CARTESIAN_POINT('Ctrl Pts',(-4.61699559000006,2.2,-0.985604844000014));
#314713=CARTESIAN_POINT('Ctrl Pts',(-4.61453673400006,12.2,-0.986506962000018));
#314714=CARTESIAN_POINT('Ctrl Pts',(-4.61453673400006,5.2,-0.986506962000018));
#314715=CARTESIAN_POINT('Ctrl Pts',(-4.61453673400006,2.2,-0.986506962000018));
#314716=CARTESIAN_POINT('Ctrl Pts',(-4.61208015200006,12.2,-0.987405346000014));
#314717=CARTESIAN_POINT('Ctrl Pts',(-4.61208015200006,5.2,-0.987405346000014));
#314718=CARTESIAN_POINT('Ctrl Pts',(-4.61208015200006,2.2,-0.987405346000014));
#314719=CARTESIAN_POINT('Ctrl Pts',(-4.60962585000006,12.2,-0.988299999000013));
#314720=CARTESIAN_POINT('Ctrl Pts',(-4.60962585000006,5.2,-0.988299999000013));
#314721=CARTESIAN_POINT('Ctrl Pts',(-4.60962585000006,2.2,-0.988299999000013));
#314722=CARTESIAN_POINT('Ctrl Pts',(-4.60717383500006,12.2,-0.989190924000014));
#314723=CARTESIAN_POINT('Ctrl Pts',(-4.60717383500006,5.2,-0.989190924000014));
#314724=CARTESIAN_POINT('Ctrl Pts',(-4.60717383500006,2.2,-0.989190924000014));
#314725=CARTESIAN_POINT('Ctrl Pts',(-4.60472411600006,12.2,-0.990078126000018));
#314726=CARTESIAN_POINT('Ctrl Pts',(-4.60472411600006,5.2,-0.990078126000018));
#314727=CARTESIAN_POINT('Ctrl Pts',(-4.60472411600006,2.2,-0.990078126000018));
#314728=CARTESIAN_POINT('Ctrl Pts',(-4.60227669800005,12.2,-0.990961607000016));
#314729=CARTESIAN_POINT('Ctrl Pts',(-4.60227669800005,5.2,-0.990961607000016));
#314730=CARTESIAN_POINT('Ctrl Pts',(-4.60227669800005,2.2,-0.990961607000016));
#314731=CARTESIAN_POINT('Ctrl Pts',(-4.59983159100006,12.2,-0.991841371000017));
#314732=CARTESIAN_POINT('Ctrl Pts',(-4.59983159100006,5.2,-0.991841371000017));
#314733=CARTESIAN_POINT('Ctrl Pts',(-4.59983159100006,2.2,-0.991841371000017));
#314734=CARTESIAN_POINT('Ctrl Pts',(-4.59738880200006,12.2,-0.992717423000014));
#314735=CARTESIAN_POINT('Ctrl Pts',(-4.59738880200006,5.2,-0.992717423000014));
#314736=CARTESIAN_POINT('Ctrl Pts',(-4.59738880200006,2.2,-0.992717423000014));
#314737=CARTESIAN_POINT('Ctrl Pts',(-4.59494834000005,12.2,-0.993589766000014));
#314738=CARTESIAN_POINT('Ctrl Pts',(-4.59494834000005,5.2,-0.993589766000014));
#314739=CARTESIAN_POINT('Ctrl Pts',(-4.59494834000005,2.2,-0.993589766000014));
#314740=CARTESIAN_POINT('Ctrl Pts',(-4.59251021200005,12.2,-0.994458404000014));
#314741=CARTESIAN_POINT('Ctrl Pts',(-4.59251021200005,5.2,-0.994458404000014));
#314742=CARTESIAN_POINT('Ctrl Pts',(-4.59251021200005,2.2,-0.994458404000014));
#314743=CARTESIAN_POINT('Ctrl Pts',(-4.59007442800006,12.2,-0.995323342000014));
#314744=CARTESIAN_POINT('Ctrl Pts',(-4.59007442800006,5.2,-0.995323342000014));
#314745=CARTESIAN_POINT('Ctrl Pts',(-4.59007442800006,2.2,-0.995323342000014));
#314746=CARTESIAN_POINT('Ctrl Pts',(-4.58764099500006,12.2,-0.996184581000015));
#314747=CARTESIAN_POINT('Ctrl Pts',(-4.58764099500006,5.2,-0.996184581000015));
#314748=CARTESIAN_POINT('Ctrl Pts',(-4.58764099500006,2.2,-0.996184581000015));
#314749=CARTESIAN_POINT('Ctrl Pts',(-4.58520992000006,12.2,-0.997042128000012));
#314750=CARTESIAN_POINT('Ctrl Pts',(-4.58520992000006,5.2,-0.997042128000012));
#314751=CARTESIAN_POINT('Ctrl Pts',(-4.58520992000006,2.2,-0.997042128000012));
#314752=CARTESIAN_POINT('Ctrl Pts',(-4.58278121200006,12.2,-0.997895986000015));
#314753=CARTESIAN_POINT('Ctrl Pts',(-4.58278121200006,5.2,-0.997895986000015));
#314754=CARTESIAN_POINT('Ctrl Pts',(-4.58278121200006,2.2,-0.997895986000015));
#314755=CARTESIAN_POINT('Ctrl Pts',(-4.58035487800006,12.2,-0.998746158000015));
#314756=CARTESIAN_POINT('Ctrl Pts',(-4.58035487800006,5.2,-0.998746158000015));
#314757=CARTESIAN_POINT('Ctrl Pts',(-4.58035487800006,2.2,-0.998746158000015));
#314758=CARTESIAN_POINT('Ctrl Pts',(-4.57793092600006,12.2,-0.999592648000016));
#314759=CARTESIAN_POINT('Ctrl Pts',(-4.57793092600006,5.2,-0.999592648000016));
#314760=CARTESIAN_POINT('Ctrl Pts',(-4.57793092600006,2.2,-0.999592648000016));
#314761=CARTESIAN_POINT('Ctrl Pts',(-4.57550936400006,12.2,-1.00043546100002));
#314762=CARTESIAN_POINT('Ctrl Pts',(-4.57550936400006,5.2,-1.00043546100002));
#314763=CARTESIAN_POINT('Ctrl Pts',(-4.57550936400006,2.2,-1.00043546100002));
#314764=CARTESIAN_POINT('Ctrl Pts',(-4.57309019900006,12.2,-1.00127459900001));
#314765=CARTESIAN_POINT('Ctrl Pts',(-4.57309019900006,5.2,-1.00127459900001));
#314766=CARTESIAN_POINT('Ctrl Pts',(-4.57309019900006,2.2,-1.00127459900001));
#314767=CARTESIAN_POINT('Ctrl Pts',(-4.57067344100006,12.2,-1.00211006800001));
#314768=CARTESIAN_POINT('Ctrl Pts',(-4.57067344100006,5.2,-1.00211006800001));
#314769=CARTESIAN_POINT('Ctrl Pts',(-4.57067344100006,2.2,-1.00211006800001));
#314770=CARTESIAN_POINT('Ctrl Pts',(-4.56825909500005,12.2,-1.00294187100001));
#314771=CARTESIAN_POINT('Ctrl Pts',(-4.56825909500005,5.2,-1.00294187100001));
#314772=CARTESIAN_POINT('Ctrl Pts',(-4.56825909500005,2.2,-1.00294187100001));
#314773=CARTESIAN_POINT('Ctrl Pts',(-4.56584717200006,12.2,-1.00377001100002));
#314774=CARTESIAN_POINT('Ctrl Pts',(-4.56584717200006,5.2,-1.00377001100002));
#314775=CARTESIAN_POINT('Ctrl Pts',(-4.56584717200006,2.2,-1.00377001100002));
#314776=CARTESIAN_POINT('Ctrl Pts',(-4.56343767800006,12.2,-1.00459449300002));
#314777=CARTESIAN_POINT('Ctrl Pts',(-4.56343767800006,5.2,-1.00459449300002));
#314778=CARTESIAN_POINT('Ctrl Pts',(-4.56343767800006,2.2,-1.00459449300002));
#314779=CARTESIAN_POINT('Ctrl Pts',(-4.56103062200006,12.2,-1.00541532300001));
#314780=CARTESIAN_POINT('Ctrl Pts',(-4.56103062200006,5.2,-1.00541532300001));
#314781=CARTESIAN_POINT('Ctrl Pts',(-4.56103062200006,2.2,-1.00541532300001));
#314782=CARTESIAN_POINT('Ctrl Pts',(-4.55862601000006,12.2,-1.00623250100002));
#314783=CARTESIAN_POINT('Ctrl Pts',(-4.55862601000006,5.2,-1.00623250100002));
#314784=CARTESIAN_POINT('Ctrl Pts',(-4.55862601000006,2.2,-1.00623250100002));
#314785=CARTESIAN_POINT('Ctrl Pts',(-4.55622385400006,12.2,-1.00704603400001));
#314786=CARTESIAN_POINT('Ctrl Pts',(-4.55622385400006,5.2,-1.00704603400001));
#314787=CARTESIAN_POINT('Ctrl Pts',(-4.55622385400006,2.2,-1.00704603400001));
#314788=CARTESIAN_POINT('Ctrl Pts',(-4.55382415700006,12.2,-1.00785592500001));
#314789=CARTESIAN_POINT('Ctrl Pts',(-4.55382415700006,5.2,-1.00785592500001));
#314790=CARTESIAN_POINT('Ctrl Pts',(-4.55382415700006,2.2,-1.00785592500001));
#314791=CARTESIAN_POINT('Ctrl Pts',(-4.55142693100006,12.2,-1.00866217800001));
#314792=CARTESIAN_POINT('Ctrl Pts',(-4.55142693100006,5.2,-1.00866217800001));
#314793=CARTESIAN_POINT('Ctrl Pts',(-4.55142693100006,2.2,-1.00866217800001));
#314794=CARTESIAN_POINT('Ctrl Pts',(-4.54903218100006,12.2,-1.00946479800001));
#314795=CARTESIAN_POINT('Ctrl Pts',(-4.54903218100006,5.2,-1.00946479800001));
#314796=CARTESIAN_POINT('Ctrl Pts',(-4.54903218100006,2.2,-1.00946479800001));
#314797=CARTESIAN_POINT('Ctrl Pts',(-4.54663991700006,12.2,-1.01026378800002));
#314798=CARTESIAN_POINT('Ctrl Pts',(-4.54663991700006,5.2,-1.01026378800002));
#314799=CARTESIAN_POINT('Ctrl Pts',(-4.54663991700006,2.2,-1.01026378800002));
#314800=CARTESIAN_POINT('Ctrl Pts',(-4.54425014500006,12.2,-1.01105915300002));
#314801=CARTESIAN_POINT('Ctrl Pts',(-4.54425014500006,5.2,-1.01105915300002));
#314802=CARTESIAN_POINT('Ctrl Pts',(-4.54425014500006,2.2,-1.01105915300002));
#314803=CARTESIAN_POINT('Ctrl Pts',(-4.54186287500006,12.2,-1.01185089600001));
#314804=CARTESIAN_POINT('Ctrl Pts',(-4.54186287500006,5.2,-1.01185089600001));
#314805=CARTESIAN_POINT('Ctrl Pts',(-4.54186287500006,2.2,-1.01185089600001));
#314806=CARTESIAN_POINT('Ctrl Pts',(-4.53947811500006,12.2,-1.01263902200001));
#314807=CARTESIAN_POINT('Ctrl Pts',(-4.53947811500006,5.2,-1.01263902200001));
#314808=CARTESIAN_POINT('Ctrl Pts',(-4.53947811500006,2.2,-1.01263902200001));
#314809=CARTESIAN_POINT('Ctrl Pts',(-4.53709587000006,12.2,-1.01342353600002));
#314810=CARTESIAN_POINT('Ctrl Pts',(-4.53709587000006,5.2,-1.01342353600002));
#314811=CARTESIAN_POINT('Ctrl Pts',(-4.53709587000006,2.2,-1.01342353600002));
#314812=CARTESIAN_POINT('Ctrl Pts',(-4.53471615200006,12.2,-1.01420444000001));
#314813=CARTESIAN_POINT('Ctrl Pts',(-4.53471615200006,5.2,-1.01420444000001));
#314814=CARTESIAN_POINT('Ctrl Pts',(-4.53471615200006,2.2,-1.01420444000001));
#314815=CARTESIAN_POINT('Ctrl Pts',(-4.53233896600006,12.2,-1.01498174000001));
#314816=CARTESIAN_POINT('Ctrl Pts',(-4.53233896600006,5.2,-1.01498174000001));
#314817=CARTESIAN_POINT('Ctrl Pts',(-4.53233896600006,2.2,-1.01498174000001));
#314818=CARTESIAN_POINT('Ctrl Pts',(-4.52996432000006,12.2,-1.01575543900001));
#314819=CARTESIAN_POINT('Ctrl Pts',(-4.52996432000006,5.2,-1.01575543900001));
#314820=CARTESIAN_POINT('Ctrl Pts',(-4.52996432000006,2.2,-1.01575543900001));
#314821=CARTESIAN_POINT('Ctrl Pts',(-4.52759222500006,12.2,-1.01652554200002));
#314822=CARTESIAN_POINT('Ctrl Pts',(-4.52759222500006,5.2,-1.01652554200002));
#314823=CARTESIAN_POINT('Ctrl Pts',(-4.52759222500006,2.2,-1.01652554200002));
#314824=CARTESIAN_POINT('Ctrl Pts',(-4.52522268600006,12.2,-1.01729205400002));
#314825=CARTESIAN_POINT('Ctrl Pts',(-4.52522268600006,5.2,-1.01729205400002));
#314826=CARTESIAN_POINT('Ctrl Pts',(-4.52522268600006,2.2,-1.01729205400002));
#314827=CARTESIAN_POINT('Ctrl Pts',(-4.52285571200005,12.2,-1.01805497700001));
#314828=CARTESIAN_POINT('Ctrl Pts',(-4.52285571200005,5.2,-1.01805497700001));
#314829=CARTESIAN_POINT('Ctrl Pts',(-4.52285571200005,2.2,-1.01805497700001));
#314830=CARTESIAN_POINT('Ctrl Pts',(-4.52049131100006,12.2,-1.01881431700001));
#314831=CARTESIAN_POINT('Ctrl Pts',(-4.52049131100006,5.2,-1.01881431700001));
#314832=CARTESIAN_POINT('Ctrl Pts',(-4.52049131100006,2.2,-1.01881431700001));
#314833=CARTESIAN_POINT('Ctrl Pts',(-4.51812949000006,12.2,-1.01957007800001));
#314834=CARTESIAN_POINT('Ctrl Pts',(-4.51812949000006,5.2,-1.01957007800001));
#314835=CARTESIAN_POINT('Ctrl Pts',(-4.51812949000006,2.2,-1.01957007800001));
#314836=CARTESIAN_POINT('Ctrl Pts',(-4.51577025900006,12.2,-1.02032226500001));
#314837=CARTESIAN_POINT('Ctrl Pts',(-4.51577025900006,5.2,-1.02032226500001));
#314838=CARTESIAN_POINT('Ctrl Pts',(-4.51577025900006,2.2,-1.02032226500001));
#314839=CARTESIAN_POINT('Ctrl Pts',(-4.51341362500006,12.2,-1.02107088000002));
#314840=CARTESIAN_POINT('Ctrl Pts',(-4.51341362500006,5.2,-1.02107088000002));
#314841=CARTESIAN_POINT('Ctrl Pts',(-4.51341362500006,2.2,-1.02107088000002));
#314842=CARTESIAN_POINT('Ctrl Pts',(-4.51105959700006,12.2,-1.02181593000001));
#314843=CARTESIAN_POINT('Ctrl Pts',(-4.51105959700006,5.2,-1.02181593000001));
#314844=CARTESIAN_POINT('Ctrl Pts',(-4.51105959700006,2.2,-1.02181593000001));
#314845=CARTESIAN_POINT('Ctrl Pts',(-4.50870818000006,12.2,-1.02255741900001));
#314846=CARTESIAN_POINT('Ctrl Pts',(-4.50870818000006,5.2,-1.02255741900001));
#314847=CARTESIAN_POINT('Ctrl Pts',(-4.50870818000006,2.2,-1.02255741900001));
#314848=CARTESIAN_POINT('Ctrl Pts',(-4.50635938600006,12.2,-1.02329534900001));
#314849=CARTESIAN_POINT('Ctrl Pts',(-4.50635938600006,5.2,-1.02329534900001));
#314850=CARTESIAN_POINT('Ctrl Pts',(-4.50635938600006,2.2,-1.02329534900001));
#314851=CARTESIAN_POINT('Ctrl Pts',(-4.50401322000006,12.2,-1.02402972800002));
#314852=CARTESIAN_POINT('Ctrl Pts',(-4.50401322000006,5.2,-1.02402972800002));
#314853=CARTESIAN_POINT('Ctrl Pts',(-4.50401322000006,2.2,-1.02402972800002));
#314854=CARTESIAN_POINT('Ctrl Pts',(-4.50166969200006,12.2,-1.02476055700001));
#314855=CARTESIAN_POINT('Ctrl Pts',(-4.50166969200006,5.2,-1.02476055700001));
#314856=CARTESIAN_POINT('Ctrl Pts',(-4.50166969200006,2.2,-1.02476055700001));
#314857=CARTESIAN_POINT('Ctrl Pts',(-4.49932880800006,12.2,-1.02548784200001));
#314858=CARTESIAN_POINT('Ctrl Pts',(-4.49932880800006,5.2,-1.02548784200001));
#314859=CARTESIAN_POINT('Ctrl Pts',(-4.49932880800006,2.2,-1.02548784200001));
#314860=CARTESIAN_POINT('Ctrl Pts',(-4.49699057800006,12.2,-1.02621158800002));
#314861=CARTESIAN_POINT('Ctrl Pts',(-4.49699057800006,5.2,-1.02621158800002));
#314862=CARTESIAN_POINT('Ctrl Pts',(-4.49699057800006,2.2,-1.02621158800002));
#314863=CARTESIAN_POINT('Ctrl Pts',(-4.49465500900006,12.2,-1.02693179800001));
#314864=CARTESIAN_POINT('Ctrl Pts',(-4.49465500900006,5.2,-1.02693179800001));
#314865=CARTESIAN_POINT('Ctrl Pts',(-4.49465500900006,2.2,-1.02693179800001));
#314866=CARTESIAN_POINT('Ctrl Pts',(-4.49232210900006,12.2,-1.02764847800001));
#314867=CARTESIAN_POINT('Ctrl Pts',(-4.49232210900006,5.2,-1.02764847800001));
#314868=CARTESIAN_POINT('Ctrl Pts',(-4.49232210900006,2.2,-1.02764847800001));
#314869=CARTESIAN_POINT('Ctrl Pts',(-4.48999188700006,12.2,-1.02836163100001));
#314870=CARTESIAN_POINT('Ctrl Pts',(-4.48999188700006,5.2,-1.02836163100001));
#314871=CARTESIAN_POINT('Ctrl Pts',(-4.48999188700006,2.2,-1.02836163100001));
#314872=CARTESIAN_POINT('Ctrl Pts',(-4.48766435100006,12.2,-1.02907126300002));
#314873=CARTESIAN_POINT('Ctrl Pts',(-4.48766435100006,5.2,-1.02907126300002));
#314874=CARTESIAN_POINT('Ctrl Pts',(-4.48766435100006,2.2,-1.02907126300002));
#314875=CARTESIAN_POINT('Ctrl Pts',(-4.48533950700006,12.2,-1.02977737800002));
#314876=CARTESIAN_POINT('Ctrl Pts',(-4.48533950700006,5.2,-1.02977737800002));
#314877=CARTESIAN_POINT('Ctrl Pts',(-4.48533950700006,2.2,-1.02977737800002));
#314878=CARTESIAN_POINT('Ctrl Pts',(-4.48301736600006,12.2,-1.03047998000001));
#314879=CARTESIAN_POINT('Ctrl Pts',(-4.48301736600006,5.2,-1.03047998000001));
#314880=CARTESIAN_POINT('Ctrl Pts',(-4.48301736600006,2.2,-1.03047998000001));
#314881=CARTESIAN_POINT('Ctrl Pts',(-4.48069793400006,12.2,-1.03117907400001));
#314882=CARTESIAN_POINT('Ctrl Pts',(-4.48069793400006,5.2,-1.03117907400001));
#314883=CARTESIAN_POINT('Ctrl Pts',(-4.48069793400006,2.2,-1.03117907400001));
#314884=CARTESIAN_POINT('Ctrl Pts',(-4.47838122000006,12.2,-1.03187466400001));
#314885=CARTESIAN_POINT('Ctrl Pts',(-4.47838122000006,5.2,-1.03187466400001));
#314886=CARTESIAN_POINT('Ctrl Pts',(-4.47838122000006,2.2,-1.03187466400001));
#314887=CARTESIAN_POINT('Ctrl Pts',(-4.47606723100006,12.2,-1.03256675500001));
#314888=CARTESIAN_POINT('Ctrl Pts',(-4.47606723100006,5.2,-1.03256675500001));
#314889=CARTESIAN_POINT('Ctrl Pts',(-4.47606723100006,2.2,-1.03256675500001));
#314890=CARTESIAN_POINT('Ctrl Pts',(-4.47375597800006,12.2,-1.03325535300002));
#314891=CARTESIAN_POINT('Ctrl Pts',(-4.47375597800006,5.2,-1.03325535300002));
#314892=CARTESIAN_POINT('Ctrl Pts',(-4.47375597800006,2.2,-1.03325535300002));
#314893=CARTESIAN_POINT('Ctrl Pts',(-4.47144746500006,12.2,-1.03394046000002));
#314894=CARTESIAN_POINT('Ctrl Pts',(-4.47144746500006,5.2,-1.03394046000002));
#314895=CARTESIAN_POINT('Ctrl Pts',(-4.47144746500006,2.2,-1.03394046000002));
#314896=CARTESIAN_POINT('Ctrl Pts',(-4.46914170300006,12.2,-1.03462208200002));
#314897=CARTESIAN_POINT('Ctrl Pts',(-4.46914170300006,5.2,-1.03462208200002));
#314898=CARTESIAN_POINT('Ctrl Pts',(-4.46914170300006,2.2,-1.03462208200002));
#314899=CARTESIAN_POINT('Ctrl Pts',(-4.46683869800006,12.2,-1.03530022500002));
#314900=CARTESIAN_POINT('Ctrl Pts',(-4.46683869800006,5.2,-1.03530022500002));
#314901=CARTESIAN_POINT('Ctrl Pts',(-4.46683869800006,2.2,-1.03530022500002));
#314902=CARTESIAN_POINT('Ctrl Pts',(-4.46453846000006,12.2,-1.03597489100002));
#314903=CARTESIAN_POINT('Ctrl Pts',(-4.46453846000006,5.2,-1.03597489100002));
#314904=CARTESIAN_POINT('Ctrl Pts',(-4.46453846000006,2.2,-1.03597489100002));
#314905=CARTESIAN_POINT('Ctrl Pts',(-4.46224099700006,12.2,-1.03664608700001));
#314906=CARTESIAN_POINT('Ctrl Pts',(-4.46224099700006,5.2,-1.03664608700001));
#314907=CARTESIAN_POINT('Ctrl Pts',(-4.46224099700006,2.2,-1.03664608700001));
#314908=CARTESIAN_POINT('Ctrl Pts',(-4.45994631700006,12.2,-1.03731381700001));
#314909=CARTESIAN_POINT('Ctrl Pts',(-4.45994631700006,5.2,-1.03731381700001));
#314910=CARTESIAN_POINT('Ctrl Pts',(-4.45994631700006,2.2,-1.03731381700001));
#314911=CARTESIAN_POINT('Ctrl Pts',(-4.45765442500006,12.2,-1.03797808500001));
#314912=CARTESIAN_POINT('Ctrl Pts',(-4.45765442500006,5.2,-1.03797808500001));
#314913=CARTESIAN_POINT('Ctrl Pts',(-4.45765442500006,2.2,-1.03797808500001));
#314914=CARTESIAN_POINT('Ctrl Pts',(-4.45536533500006,12.2,-1.03863889700001));
#314915=CARTESIAN_POINT('Ctrl Pts',(-4.45536533500006,5.2,-1.03863889700001));
#314916=CARTESIAN_POINT('Ctrl Pts',(-4.45536533500006,2.2,-1.03863889700001));
#314917=CARTESIAN_POINT('Ctrl Pts',(-4.45307905000006,12.2,-1.03929625600002));
#314918=CARTESIAN_POINT('Ctrl Pts',(-4.45307905000006,5.2,-1.03929625600002));
#314919=CARTESIAN_POINT('Ctrl Pts',(-4.45307905000006,2.2,-1.03929625600002));
#314920=CARTESIAN_POINT('Ctrl Pts',(-4.45079557900006,12.2,-1.03995016800001));
#314921=CARTESIAN_POINT('Ctrl Pts',(-4.45079557900006,5.2,-1.03995016800001));
#314922=CARTESIAN_POINT('Ctrl Pts',(-4.45079557900006,2.2,-1.03995016800001));
#314923=CARTESIAN_POINT('Ctrl Pts',(-4.44851493300006,12.2,-1.04060063700001));
#314924=CARTESIAN_POINT('Ctrl Pts',(-4.44851493300006,5.2,-1.04060063700001));
#314925=CARTESIAN_POINT('Ctrl Pts',(-4.44851493300006,2.2,-1.04060063700001));
#314926=CARTESIAN_POINT('Ctrl Pts',(-4.44623711800006,12.2,-1.04124767000001));
#314927=CARTESIAN_POINT('Ctrl Pts',(-4.44623711800006,5.2,-1.04124767000001));
#314928=CARTESIAN_POINT('Ctrl Pts',(-4.44623711800006,2.2,-1.04124767000001));
#314929=CARTESIAN_POINT('Ctrl Pts',(-4.44396214200006,12.2,-1.04189126900001));
#314930=CARTESIAN_POINT('Ctrl Pts',(-4.44396214200006,5.2,-1.04189126900001));
#314931=CARTESIAN_POINT('Ctrl Pts',(-4.44396214200006,2.2,-1.04189126900001));
#314932=CARTESIAN_POINT('Ctrl Pts',(-4.44169001300006,12.2,-1.04253144000001));
#314933=CARTESIAN_POINT('Ctrl Pts',(-4.44169001300006,5.2,-1.04253144000001));
#314934=CARTESIAN_POINT('Ctrl Pts',(-4.44169001300006,2.2,-1.04253144000001));
#314935=CARTESIAN_POINT('Ctrl Pts',(-4.43942074200006,12.2,-1.04316818900001));
#314936=CARTESIAN_POINT('Ctrl Pts',(-4.43942074200006,5.2,-1.04316818900001));
#314937=CARTESIAN_POINT('Ctrl Pts',(-4.43942074200006,2.2,-1.04316818900001));
#314938=CARTESIAN_POINT('Ctrl Pts',(-4.43715433200006,12.2,-1.04380152000001));
#314939=CARTESIAN_POINT('Ctrl Pts',(-4.43715433200006,5.2,-1.04380152000001));
#314940=CARTESIAN_POINT('Ctrl Pts',(-4.43715433200006,2.2,-1.04380152000001));
#314941=CARTESIAN_POINT('Ctrl Pts',(-4.43489079500006,12.2,-1.04443143700002));
#314942=CARTESIAN_POINT('Ctrl Pts',(-4.43489079500006,5.2,-1.04443143700002));
#314943=CARTESIAN_POINT('Ctrl Pts',(-4.43489079500006,2.2,-1.04443143700002));
#314944=CARTESIAN_POINT('Ctrl Pts',(-4.43263013900006,12.2,-1.04505794700001));
#314945=CARTESIAN_POINT('Ctrl Pts',(-4.43263013900006,5.2,-1.04505794700001));
#314946=CARTESIAN_POINT('Ctrl Pts',(-4.43263013900006,2.2,-1.04505794700001));
#314947=CARTESIAN_POINT('Ctrl Pts',(-4.43037237100006,12.2,-1.04568105300002));
#314948=CARTESIAN_POINT('Ctrl Pts',(-4.43037237100006,5.2,-1.04568105300002));
#314949=CARTESIAN_POINT('Ctrl Pts',(-4.43037237100006,2.2,-1.04568105300002));
#314950=CARTESIAN_POINT('Ctrl Pts',(-4.42811749900006,12.2,-1.04630076000001));
#314951=CARTESIAN_POINT('Ctrl Pts',(-4.42811749900006,5.2,-1.04630076000001));
#314952=CARTESIAN_POINT('Ctrl Pts',(-4.42811749900006,2.2,-1.04630076000001));
#314953=CARTESIAN_POINT('Ctrl Pts',(-4.42586553200006,12.2,-1.04691707400002));
#314954=CARTESIAN_POINT('Ctrl Pts',(-4.42586553200006,5.2,-1.04691707400002));
#314955=CARTESIAN_POINT('Ctrl Pts',(-4.42586553200006,2.2,-1.04691707400002));
#314956=CARTESIAN_POINT('Ctrl Pts',(-4.42361647800006,12.2,-1.04753000000001));
#314957=CARTESIAN_POINT('Ctrl Pts',(-4.42361647800006,5.2,-1.04753000000001));
#314958=CARTESIAN_POINT('Ctrl Pts',(-4.42361647800006,2.2,-1.04753000000001));
#314959=CARTESIAN_POINT('Ctrl Pts',(-4.42137034500006,12.2,-1.04813954200001));
#314960=CARTESIAN_POINT('Ctrl Pts',(-4.42137034500006,5.2,-1.04813954200001));
#314961=CARTESIAN_POINT('Ctrl Pts',(-4.42137034500006,2.2,-1.04813954200001));
#314962=CARTESIAN_POINT('Ctrl Pts',(-4.41912714100006,12.2,-1.04874570700002));
#314963=CARTESIAN_POINT('Ctrl Pts',(-4.41912714100006,5.2,-1.04874570700002));
#314964=CARTESIAN_POINT('Ctrl Pts',(-4.41912714100006,2.2,-1.04874570700002));
#314965=CARTESIAN_POINT('Ctrl Pts',(-4.41688687400006,12.2,-1.04934849700001));
#314966=CARTESIAN_POINT('Ctrl Pts',(-4.41688687400006,5.2,-1.04934849700001));
#314967=CARTESIAN_POINT('Ctrl Pts',(-4.41688687400006,2.2,-1.04934849700001));
#314968=CARTESIAN_POINT('Ctrl Pts',(-4.41464955400006,12.2,-1.04994792000001));
#314969=CARTESIAN_POINT('Ctrl Pts',(-4.41464955400006,5.2,-1.04994792000001));
#314970=CARTESIAN_POINT('Ctrl Pts',(-4.41464955400006,2.2,-1.04994792000001));
#314971=CARTESIAN_POINT('Ctrl Pts',(-4.41241518600005,12.2,-1.05054398000001));
#314972=CARTESIAN_POINT('Ctrl Pts',(-4.41241518600005,5.2,-1.05054398000001));
#314973=CARTESIAN_POINT('Ctrl Pts',(-4.41241518600005,2.2,-1.05054398000001));
#314974=CARTESIAN_POINT('Ctrl Pts',(-4.41018378200006,12.2,-1.05113668200001));
#314975=CARTESIAN_POINT('Ctrl Pts',(-4.41018378200006,5.2,-1.05113668200001));
#314976=CARTESIAN_POINT('Ctrl Pts',(-4.41018378200006,2.2,-1.05113668200001));
#314977=CARTESIAN_POINT('Ctrl Pts',(-4.40795534700006,12.2,-1.05172603100002));
#314978=CARTESIAN_POINT('Ctrl Pts',(-4.40795534700006,5.2,-1.05172603100002));
#314979=CARTESIAN_POINT('Ctrl Pts',(-4.40795534700006,2.2,-1.05172603100002));
#314980=CARTESIAN_POINT('Ctrl Pts',(-4.40572989000006,12.2,-1.05231203200002));
#314981=CARTESIAN_POINT('Ctrl Pts',(-4.40572989000006,5.2,-1.05231203200002));
#314982=CARTESIAN_POINT('Ctrl Pts',(-4.40572989000006,2.2,-1.05231203200002));
#314983=CARTESIAN_POINT('Ctrl Pts',(-4.40350742100006,12.2,-1.05289469000001));
#314984=CARTESIAN_POINT('Ctrl Pts',(-4.40350742100006,5.2,-1.05289469000001));
#314985=CARTESIAN_POINT('Ctrl Pts',(-4.40350742100006,2.2,-1.05289469000001));
#314986=CARTESIAN_POINT('Ctrl Pts',(-4.40128794700006,12.2,-1.05347401200001));
#314987=CARTESIAN_POINT('Ctrl Pts',(-4.40128794700006,5.2,-1.05347401200001));
#314988=CARTESIAN_POINT('Ctrl Pts',(-4.40128794700006,2.2,-1.05347401200001));
#314989=CARTESIAN_POINT('Ctrl Pts',(-4.39907147400006,12.2,-1.05405000100002));
#314990=CARTESIAN_POINT('Ctrl Pts',(-4.39907147400006,5.2,-1.05405000100002));
#314991=CARTESIAN_POINT('Ctrl Pts',(-4.39907147400006,2.2,-1.05405000100002));
#314992=CARTESIAN_POINT('Ctrl Pts',(-4.39685801400006,12.2,-1.05462266400002));
#314993=CARTESIAN_POINT('Ctrl Pts',(-4.39685801400006,5.2,-1.05462266400002));
#314994=CARTESIAN_POINT('Ctrl Pts',(-4.39685801400006,2.2,-1.05462266400002));
#314995=CARTESIAN_POINT('Ctrl Pts',(-4.39464757300006,12.2,-1.05519200400002));
#314996=CARTESIAN_POINT('Ctrl Pts',(-4.39464757300006,5.2,-1.05519200400002));
#314997=CARTESIAN_POINT('Ctrl Pts',(-4.39464757300006,2.2,-1.05519200400002));
#314998=CARTESIAN_POINT('Ctrl Pts',(-4.39244016100006,12.2,-1.05575802800002));
#314999=CARTESIAN_POINT('Ctrl Pts',(-4.39244016100006,5.2,-1.05575802800002));
#315000=CARTESIAN_POINT('Ctrl Pts',(-4.39244016100006,2.2,-1.05575802800002));
#315001=CARTESIAN_POINT('Ctrl Pts',(-4.39023578400006,12.2,-1.05632074100001));
#315002=CARTESIAN_POINT('Ctrl Pts',(-4.39023578400006,5.2,-1.05632074100001));
#315003=CARTESIAN_POINT('Ctrl Pts',(-4.39023578400006,2.2,-1.05632074100001));
#315004=CARTESIAN_POINT('Ctrl Pts',(-4.38803445100006,12.2,-1.05688014700001));
#315005=CARTESIAN_POINT('Ctrl Pts',(-4.38803445100006,5.2,-1.05688014700001));
#315006=CARTESIAN_POINT('Ctrl Pts',(-4.38803445100006,2.2,-1.05688014700001));
#315007=CARTESIAN_POINT('Ctrl Pts',(-4.38583617100006,12.2,-1.05743625500001));
#315008=CARTESIAN_POINT('Ctrl Pts',(-4.38583617100006,5.2,-1.05743625500001));
#315009=CARTESIAN_POINT('Ctrl Pts',(-4.38583617100006,2.2,-1.05743625500001));
#315010=CARTESIAN_POINT('Ctrl Pts',(-4.38364095300006,12.2,-1.05798906500001));
#315011=CARTESIAN_POINT('Ctrl Pts',(-4.38364095300006,5.2,-1.05798906500001));
#315012=CARTESIAN_POINT('Ctrl Pts',(-4.38364095300006,2.2,-1.05798906500001));
#315013=CARTESIAN_POINT('Ctrl Pts',(-4.38144880200006,12.2,-1.05853858700002));
#315014=CARTESIAN_POINT('Ctrl Pts',(-4.38144880200006,5.2,-1.05853858700002));
#315015=CARTESIAN_POINT('Ctrl Pts',(-4.38144880200006,2.2,-1.05853858700002));
#315016=CARTESIAN_POINT('Ctrl Pts',(-4.37925972900006,12.2,-1.05908482400002));
#315017=CARTESIAN_POINT('Ctrl Pts',(-4.37925972900006,5.2,-1.05908482400002));
#315018=CARTESIAN_POINT('Ctrl Pts',(-4.37925972900006,2.2,-1.05908482400002));
#315019=CARTESIAN_POINT('Ctrl Pts',(-4.37707374200006,12.2,-1.05962778200002));
#315020=CARTESIAN_POINT('Ctrl Pts',(-4.37707374200006,5.2,-1.05962778200002));
#315021=CARTESIAN_POINT('Ctrl Pts',(-4.37707374200006,2.2,-1.05962778200002));
#315022=CARTESIAN_POINT('Ctrl Pts',(-4.37489084900006,12.2,-1.06016746500002));
#315023=CARTESIAN_POINT('Ctrl Pts',(-4.37489084900006,5.2,-1.06016746500002));
#315024=CARTESIAN_POINT('Ctrl Pts',(-4.37489084900006,2.2,-1.06016746500002));
#315025=CARTESIAN_POINT('Ctrl Pts',(-4.37271105700006,12.2,-1.06070388100001));
#315026=CARTESIAN_POINT('Ctrl Pts',(-4.37271105700006,5.2,-1.06070388100001));
#315027=CARTESIAN_POINT('Ctrl Pts',(-4.37271105700006,2.2,-1.06070388100001));
#315028=CARTESIAN_POINT('Ctrl Pts',(-4.37053437700006,12.2,-1.06123703400002));
#315029=CARTESIAN_POINT('Ctrl Pts',(-4.37053437700006,5.2,-1.06123703400002));
#315030=CARTESIAN_POINT('Ctrl Pts',(-4.37053437700006,2.2,-1.06123703400002));
#315031=CARTESIAN_POINT('Ctrl Pts',(-4.36836081500006,12.2,-1.06176692900001));
#315032=CARTESIAN_POINT('Ctrl Pts',(-4.36836081500006,5.2,-1.06176692900001));
#315033=CARTESIAN_POINT('Ctrl Pts',(-4.36836081500006,2.2,-1.06176692900001));
#315034=CARTESIAN_POINT('Ctrl Pts',(-4.36619038000006,12.2,-1.06229357300001));
#315035=CARTESIAN_POINT('Ctrl Pts',(-4.36619038000006,5.2,-1.06229357300001));
#315036=CARTESIAN_POINT('Ctrl Pts',(-4.36619038000006,2.2,-1.06229357300001));
#315037=CARTESIAN_POINT('Ctrl Pts',(-4.36402308000006,12.2,-1.06281697000002));
#315038=CARTESIAN_POINT('Ctrl Pts',(-4.36402308000006,5.2,-1.06281697000002));
#315039=CARTESIAN_POINT('Ctrl Pts',(-4.36402308000006,2.2,-1.06281697000002));
#315040=CARTESIAN_POINT('Ctrl Pts',(-4.36185892400006,12.2,-1.06333712600001));
#315041=CARTESIAN_POINT('Ctrl Pts',(-4.36185892400006,5.2,-1.06333712600001));
#315042=CARTESIAN_POINT('Ctrl Pts',(-4.36185892400006,2.2,-1.06333712600001));
#315043=CARTESIAN_POINT('Ctrl Pts',(-4.35969792000006,12.2,-1.06385404700001));
#315044=CARTESIAN_POINT('Ctrl Pts',(-4.35969792000006,5.2,-1.06385404700001));
#315045=CARTESIAN_POINT('Ctrl Pts',(-4.35969792000006,2.2,-1.06385404700001));
#315046=CARTESIAN_POINT('Ctrl Pts',(-4.35754007500006,12.2,-1.06436773800001));
#315047=CARTESIAN_POINT('Ctrl Pts',(-4.35754007500006,5.2,-1.06436773800001));
#315048=CARTESIAN_POINT('Ctrl Pts',(-4.35754007500006,2.2,-1.06436773800001));
#315049=CARTESIAN_POINT('Ctrl Pts',(-4.35538539900006,12.2,-1.06487820600002));
#315050=CARTESIAN_POINT('Ctrl Pts',(-4.35538539900006,5.2,-1.06487820600002));
#315051=CARTESIAN_POINT('Ctrl Pts',(-4.35538539900006,2.2,-1.06487820600002));
#315052=CARTESIAN_POINT('Ctrl Pts',(-4.35323390100006,12.2,-1.06538545400001));
#315053=CARTESIAN_POINT('Ctrl Pts',(-4.35323390100006,5.2,-1.06538545400001));
#315054=CARTESIAN_POINT('Ctrl Pts',(-4.35323390100006,2.2,-1.06538545400001));
#315055=CARTESIAN_POINT('Ctrl Pts',(-4.35108558800006,12.2,-1.06588948900002));
#315056=CARTESIAN_POINT('Ctrl Pts',(-4.35108558800006,5.2,-1.06588948900002));
#315057=CARTESIAN_POINT('Ctrl Pts',(-4.35108558800006,2.2,-1.06588948900002));
#315058=CARTESIAN_POINT('Ctrl Pts',(-4.34894046700006,12.2,-1.06639031800002));
#315059=CARTESIAN_POINT('Ctrl Pts',(-4.34894046700006,5.2,-1.06639031800002));
#315060=CARTESIAN_POINT('Ctrl Pts',(-4.34894046700006,2.2,-1.06639031800002));
#315061=CARTESIAN_POINT('Ctrl Pts',(-4.34679854900006,12.2,-1.06688794400001));
#315062=CARTESIAN_POINT('Ctrl Pts',(-4.34679854900006,5.2,-1.06688794400001));
#315063=CARTESIAN_POINT('Ctrl Pts',(-4.34679854900006,2.2,-1.06688794400001));
#315064=CARTESIAN_POINT('Ctrl Pts',(-4.34465984100005,12.2,-1.06738237400001));
#315065=CARTESIAN_POINT('Ctrl Pts',(-4.34465984100005,5.2,-1.06738237400001));
#315066=CARTESIAN_POINT('Ctrl Pts',(-4.34465984100005,2.2,-1.06738237400001));
#315067=CARTESIAN_POINT('Ctrl Pts',(-4.34252435100006,12.2,-1.06787361500002));
#315068=CARTESIAN_POINT('Ctrl Pts',(-4.34252435100006,5.2,-1.06787361500002));
#315069=CARTESIAN_POINT('Ctrl Pts',(-4.34252435100006,2.2,-1.06787361500002));
#315070=CARTESIAN_POINT('Ctrl Pts',(-4.34039208900006,12.2,-1.06836166900001));
#315071=CARTESIAN_POINT('Ctrl Pts',(-4.34039208900006,5.2,-1.06836166900001));
#315072=CARTESIAN_POINT('Ctrl Pts',(-4.34039208900006,2.2,-1.06836166900001));
#315073=CARTESIAN_POINT('Ctrl Pts',(-4.33826306000006,12.2,-1.06884654600002));
#315074=CARTESIAN_POINT('Ctrl Pts',(-4.33826306000006,5.2,-1.06884654600002));
#315075=CARTESIAN_POINT('Ctrl Pts',(-4.33826306000006,2.2,-1.06884654600002));
#315076=CARTESIAN_POINT('Ctrl Pts',(-4.33613727600005,12.2,-1.06932824900001));
#315077=CARTESIAN_POINT('Ctrl Pts',(-4.33613727600005,5.2,-1.06932824900001));
#315078=CARTESIAN_POINT('Ctrl Pts',(-4.33613727600005,2.2,-1.06932824900001));
#315079=CARTESIAN_POINT('Ctrl Pts',(-4.33401474400006,12.2,-1.06980678600001));
#315080=CARTESIAN_POINT('Ctrl Pts',(-4.33401474400006,5.2,-1.06980678600001));
#315081=CARTESIAN_POINT('Ctrl Pts',(-4.33401474400006,2.2,-1.06980678600001));
#315082=CARTESIAN_POINT('Ctrl Pts',(-4.33189547100006,12.2,-1.07028216000002));
#315083=CARTESIAN_POINT('Ctrl Pts',(-4.33189547100006,5.2,-1.07028216000002));
#315084=CARTESIAN_POINT('Ctrl Pts',(-4.33189547100006,2.2,-1.07028216000002));
#315085=CARTESIAN_POINT('Ctrl Pts',(-4.32977946700006,12.2,-1.07075437900002));
#315086=CARTESIAN_POINT('Ctrl Pts',(-4.32977946700006,5.2,-1.07075437900002));
#315087=CARTESIAN_POINT('Ctrl Pts',(-4.32977946700006,2.2,-1.07075437900002));
#315088=CARTESIAN_POINT('Ctrl Pts',(-4.32766674000006,12.2,-1.07122344700001));
#315089=CARTESIAN_POINT('Ctrl Pts',(-4.32766674000006,5.2,-1.07122344700001));
#315090=CARTESIAN_POINT('Ctrl Pts',(-4.32766674000006,2.2,-1.07122344700001));
#315091=CARTESIAN_POINT('Ctrl Pts',(-4.32555729900006,12.2,-1.07168937200001));
#315092=CARTESIAN_POINT('Ctrl Pts',(-4.32555729900006,5.2,-1.07168937200001));
#315093=CARTESIAN_POINT('Ctrl Pts',(-4.32555729900006,2.2,-1.07168937200001));
#315094=CARTESIAN_POINT('Ctrl Pts',(-4.32345115100006,12.2,-1.07215215900001));
#315095=CARTESIAN_POINT('Ctrl Pts',(-4.32345115100006,5.2,-1.07215215900001));
#315096=CARTESIAN_POINT('Ctrl Pts',(-4.32345115100006,2.2,-1.07215215900001));
#315097=CARTESIAN_POINT('Ctrl Pts',(-4.32134830500006,12.2,-1.07261181400002));
#315098=CARTESIAN_POINT('Ctrl Pts',(-4.32134830500006,5.2,-1.07261181400002));
#315099=CARTESIAN_POINT('Ctrl Pts',(-4.32134830500006,2.2,-1.07261181400002));
#315100=CARTESIAN_POINT('Ctrl Pts',(-4.31924877000006,12.2,-1.07306834100001));
#315101=CARTESIAN_POINT('Ctrl Pts',(-4.31924877000006,5.2,-1.07306834100001));
#315102=CARTESIAN_POINT('Ctrl Pts',(-4.31924877000006,2.2,-1.07306834100001));
#315103=CARTESIAN_POINT('Ctrl Pts',(-4.31715255400006,12.2,-1.07352174900001));
#315104=CARTESIAN_POINT('Ctrl Pts',(-4.31715255400006,5.2,-1.07352174900001));
#315105=CARTESIAN_POINT('Ctrl Pts',(-4.31715255400006,2.2,-1.07352174900001));
#315106=CARTESIAN_POINT('Ctrl Pts',(-4.31505966400006,12.2,-1.07397204200002));
#315107=CARTESIAN_POINT('Ctrl Pts',(-4.31505966400006,5.2,-1.07397204200002));
#315108=CARTESIAN_POINT('Ctrl Pts',(-4.31505966400006,2.2,-1.07397204200002));
#315109=CARTESIAN_POINT('Ctrl Pts',(-4.31297011000006,12.2,-1.07441922700001));
#315110=CARTESIAN_POINT('Ctrl Pts',(-4.31297011000006,5.2,-1.07441922700001));
#315111=CARTESIAN_POINT('Ctrl Pts',(-4.31297011000006,2.2,-1.07441922700001));
#315112=CARTESIAN_POINT('Ctrl Pts',(-4.31088390100006,12.2,-1.07486330900001));
#315113=CARTESIAN_POINT('Ctrl Pts',(-4.31088390100006,5.2,-1.07486330900001));
#315114=CARTESIAN_POINT('Ctrl Pts',(-4.31088390100006,2.2,-1.07486330900001));
#315115=CARTESIAN_POINT('Ctrl Pts',(-4.30880104300006,12.2,-1.07530429500001));
#315116=CARTESIAN_POINT('Ctrl Pts',(-4.30880104300006,5.2,-1.07530429500001));
#315117=CARTESIAN_POINT('Ctrl Pts',(-4.30880104300006,2.2,-1.07530429500001));
#315118=CARTESIAN_POINT('Ctrl Pts',(-4.30672154600006,12.2,-1.07574219000002));
#315119=CARTESIAN_POINT('Ctrl Pts',(-4.30672154600006,5.2,-1.07574219000002));
#315120=CARTESIAN_POINT('Ctrl Pts',(-4.30672154600006,2.2,-1.07574219000002));
#315121=CARTESIAN_POINT('Ctrl Pts',(-4.30464541900006,12.2,-1.07617700100001));
#315122=CARTESIAN_POINT('Ctrl Pts',(-4.30464541900006,5.2,-1.07617700100001));
#315123=CARTESIAN_POINT('Ctrl Pts',(-4.30464541900006,2.2,-1.07617700100001));
#315124=CARTESIAN_POINT('Ctrl Pts',(-4.30257267000006,12.2,-1.07660873400001));
#315125=CARTESIAN_POINT('Ctrl Pts',(-4.30257267000006,5.2,-1.07660873400001));
#315126=CARTESIAN_POINT('Ctrl Pts',(-4.30257267000006,2.2,-1.07660873400001));
#315127=CARTESIAN_POINT('Ctrl Pts',(-4.30050330700006,12.2,-1.07703739400002));
#315128=CARTESIAN_POINT('Ctrl Pts',(-4.30050330700006,5.2,-1.07703739400002));
#315129=CARTESIAN_POINT('Ctrl Pts',(-4.30050330700006,2.2,-1.07703739400002));
#315130=CARTESIAN_POINT('Ctrl Pts',(-4.29843733800006,12.2,-1.07746298900001));
#315131=CARTESIAN_POINT('Ctrl Pts',(-4.29843733800006,5.2,-1.07746298900001));
#315132=CARTESIAN_POINT('Ctrl Pts',(-4.29843733800006,2.2,-1.07746298900001));
#315133=CARTESIAN_POINT('Ctrl Pts',(-4.29637477200006,12.2,-1.07788552300002));
#315134=CARTESIAN_POINT('Ctrl Pts',(-4.29637477200006,5.2,-1.07788552300002));
#315135=CARTESIAN_POINT('Ctrl Pts',(-4.29637477200006,2.2,-1.07788552300002));
#315136=CARTESIAN_POINT('Ctrl Pts',(-4.29431561700006,12.2,-1.07830500400001));
#315137=CARTESIAN_POINT('Ctrl Pts',(-4.29431561700006,5.2,-1.07830500400001));
#315138=CARTESIAN_POINT('Ctrl Pts',(-4.29431561700006,2.2,-1.07830500400001));
#315139=CARTESIAN_POINT('Ctrl Pts',(-4.29225988200006,12.2,-1.07872143700002));
#315140=CARTESIAN_POINT('Ctrl Pts',(-4.29225988200006,5.2,-1.07872143700002));
#315141=CARTESIAN_POINT('Ctrl Pts',(-4.29225988200006,2.2,-1.07872143700002));
#315142=CARTESIAN_POINT('Ctrl Pts',(-4.29020757500005,12.2,-1.07913482900001));
#315143=CARTESIAN_POINT('Ctrl Pts',(-4.29020757500005,5.2,-1.07913482900001));
#315144=CARTESIAN_POINT('Ctrl Pts',(-4.29020757500005,2.2,-1.07913482900001));
#315145=CARTESIAN_POINT('Ctrl Pts',(-4.28815870600006,12.2,-1.07954518600001));
#315146=CARTESIAN_POINT('Ctrl Pts',(-4.28815870600006,5.2,-1.07954518600001));
#315147=CARTESIAN_POINT('Ctrl Pts',(-4.28815870600006,2.2,-1.07954518600001));
#315148=CARTESIAN_POINT('Ctrl Pts',(-4.28611328100006,12.2,-1.07995251300002));
#315149=CARTESIAN_POINT('Ctrl Pts',(-4.28611328100006,5.2,-1.07995251300002));
#315150=CARTESIAN_POINT('Ctrl Pts',(-4.28611328100006,2.2,-1.07995251300002));
#315151=CARTESIAN_POINT('Ctrl Pts',(-4.28407131000006,12.2,-1.08035681800001));
#315152=CARTESIAN_POINT('Ctrl Pts',(-4.28407131000006,5.2,-1.08035681800001));
#315153=CARTESIAN_POINT('Ctrl Pts',(-4.28407131000006,2.2,-1.08035681800001));
#315154=CARTESIAN_POINT('Ctrl Pts',(-4.28203280000006,12.2,-1.08075810700001));
#315155=CARTESIAN_POINT('Ctrl Pts',(-4.28203280000006,5.2,-1.08075810700001));
#315156=CARTESIAN_POINT('Ctrl Pts',(-4.28203280000006,2.2,-1.08075810700001));
#315157=CARTESIAN_POINT('Ctrl Pts',(-4.27999776200005,12.2,-1.08115638600002));
#315158=CARTESIAN_POINT('Ctrl Pts',(-4.27999776200005,5.2,-1.08115638600002));
#315159=CARTESIAN_POINT('Ctrl Pts',(-4.27999776200005,2.2,-1.08115638600002));
#315160=CARTESIAN_POINT('Ctrl Pts',(-4.27796620300006,12.2,-1.08155166100001));
#315161=CARTESIAN_POINT('Ctrl Pts',(-4.27796620300006,5.2,-1.08155166100001));
#315162=CARTESIAN_POINT('Ctrl Pts',(-4.27796620300006,2.2,-1.08155166100001));
#315163=CARTESIAN_POINT('Ctrl Pts',(-4.27593813100006,12.2,-1.08194393800002));
#315164=CARTESIAN_POINT('Ctrl Pts',(-4.27593813100006,5.2,-1.08194393800002));
#315165=CARTESIAN_POINT('Ctrl Pts',(-4.27593813100006,2.2,-1.08194393800002));
#315166=CARTESIAN_POINT('Ctrl Pts',(-4.27391355500006,12.2,-1.08233322400002));
#315167=CARTESIAN_POINT('Ctrl Pts',(-4.27391355500006,5.2,-1.08233322400002));
#315168=CARTESIAN_POINT('Ctrl Pts',(-4.27391355500006,2.2,-1.08233322400002));
#315169=CARTESIAN_POINT('Ctrl Pts',(-4.27189248300006,12.2,-1.08271952700001));
#315170=CARTESIAN_POINT('Ctrl Pts',(-4.27189248300006,5.2,-1.08271952700001));
#315171=CARTESIAN_POINT('Ctrl Pts',(-4.27189248300006,2.2,-1.08271952700001));
#315172=CARTESIAN_POINT('Ctrl Pts',(-4.26987492400006,12.2,-1.08310285000002));
#315173=CARTESIAN_POINT('Ctrl Pts',(-4.26987492400006,5.2,-1.08310285000002));
#315174=CARTESIAN_POINT('Ctrl Pts',(-4.26987492400006,2.2,-1.08310285000002));
#315175=CARTESIAN_POINT('Ctrl Pts',(-4.26786088700006,12.2,-1.08348320200002));
#315176=CARTESIAN_POINT('Ctrl Pts',(-4.26786088700006,5.2,-1.08348320200002));
#315177=CARTESIAN_POINT('Ctrl Pts',(-4.26786088700006,2.2,-1.08348320200002));
#315178=CARTESIAN_POINT('Ctrl Pts',(-4.26585037900006,12.2,-1.08386058900001));
#315179=CARTESIAN_POINT('Ctrl Pts',(-4.26585037900006,5.2,-1.08386058900001));
#315180=CARTESIAN_POINT('Ctrl Pts',(-4.26585037900006,2.2,-1.08386058900001));
#315181=CARTESIAN_POINT('Ctrl Pts',(-4.26384341100006,12.2,-1.08423501800001));
#315182=CARTESIAN_POINT('Ctrl Pts',(-4.26384341100006,5.2,-1.08423501800001));
#315183=CARTESIAN_POINT('Ctrl Pts',(-4.26384341100006,2.2,-1.08423501800001));
#315184=CARTESIAN_POINT('Ctrl Pts',(-4.26183998900005,12.2,-1.08460649400001));
#315185=CARTESIAN_POINT('Ctrl Pts',(-4.26183998900005,5.2,-1.08460649400001));
#315186=CARTESIAN_POINT('Ctrl Pts',(-4.26183998900005,2.2,-1.08460649400001));
#315187=CARTESIAN_POINT('Ctrl Pts',(-4.25984012300006,12.2,-1.08497502300001));
#315188=CARTESIAN_POINT('Ctrl Pts',(-4.25984012300006,5.2,-1.08497502300001));
#315189=CARTESIAN_POINT('Ctrl Pts',(-4.25984012300006,2.2,-1.08497502300001));
#315190=CARTESIAN_POINT('Ctrl Pts',(-4.25784382000006,12.2,-1.08534061400002));
#315191=CARTESIAN_POINT('Ctrl Pts',(-4.25784382000006,5.2,-1.08534061400002));
#315192=CARTESIAN_POINT('Ctrl Pts',(-4.25784382000006,2.2,-1.08534061400002));
#315193=CARTESIAN_POINT('Ctrl Pts',(-4.25585109000005,12.2,-1.08570327200002));
#315194=CARTESIAN_POINT('Ctrl Pts',(-4.25585109000005,5.2,-1.08570327200002));
#315195=CARTESIAN_POINT('Ctrl Pts',(-4.25585109000005,2.2,-1.08570327200002));
#315196=CARTESIAN_POINT('Ctrl Pts',(-4.25386194100006,12.2,-1.08606300500002));
#315197=CARTESIAN_POINT('Ctrl Pts',(-4.25386194100006,5.2,-1.08606300500002));
#315198=CARTESIAN_POINT('Ctrl Pts',(-4.25386194100006,2.2,-1.08606300500002));
#315199=CARTESIAN_POINT('Ctrl Pts',(-4.25187638100006,12.2,-1.08641981700002));
#315200=CARTESIAN_POINT('Ctrl Pts',(-4.25187638100006,5.2,-1.08641981700002));
#315201=CARTESIAN_POINT('Ctrl Pts',(-4.25187638100006,2.2,-1.08641981700002));
#315202=CARTESIAN_POINT('Ctrl Pts',(-4.24989441900006,12.2,-1.08677371700002));
#315203=CARTESIAN_POINT('Ctrl Pts',(-4.24989441900006,5.2,-1.08677371700002));
#315204=CARTESIAN_POINT('Ctrl Pts',(-4.24989441900006,2.2,-1.08677371700002));
#315205=CARTESIAN_POINT('Ctrl Pts',(-4.24791606500006,12.2,-1.08712471100001));
#315206=CARTESIAN_POINT('Ctrl Pts',(-4.24791606500006,5.2,-1.08712471100001));
#315207=CARTESIAN_POINT('Ctrl Pts',(-4.24791606500006,2.2,-1.08712471100001));
#315208=CARTESIAN_POINT('Ctrl Pts',(-4.24594132400006,12.2,-1.08747280500001));
#315209=CARTESIAN_POINT('Ctrl Pts',(-4.24594132400006,5.2,-1.08747280500001));
#315210=CARTESIAN_POINT('Ctrl Pts',(-4.24594132400006,2.2,-1.08747280500001));
#315211=CARTESIAN_POINT('Ctrl Pts',(-4.24397020800006,12.2,-1.08781800600001));
#315212=CARTESIAN_POINT('Ctrl Pts',(-4.24397020800006,5.2,-1.08781800600001));
#315213=CARTESIAN_POINT('Ctrl Pts',(-4.24397020800006,2.2,-1.08781800600001));
#315214=CARTESIAN_POINT('Ctrl Pts',(-4.24200272500006,12.2,-1.08816032300001));
#315215=CARTESIAN_POINT('Ctrl Pts',(-4.24200272500006,5.2,-1.08816032300001));
#315216=CARTESIAN_POINT('Ctrl Pts',(-4.24200272500006,2.2,-1.08816032300001));
#315217=CARTESIAN_POINT('Ctrl Pts',(-4.24003888100006,12.2,-1.08849975800001));
#315218=CARTESIAN_POINT('Ctrl Pts',(-4.24003888100006,5.2,-1.08849975800001));
#315219=CARTESIAN_POINT('Ctrl Pts',(-4.24003888100006,2.2,-1.08849975800001));
#315220=CARTESIAN_POINT('Ctrl Pts',(-4.23807868800006,12.2,-1.08883632200001));
#315221=CARTESIAN_POINT('Ctrl Pts',(-4.23807868800006,5.2,-1.08883632200001));
#315222=CARTESIAN_POINT('Ctrl Pts',(-4.23807868800006,2.2,-1.08883632200001));
#315223=CARTESIAN_POINT('Ctrl Pts',(-4.23612215200006,12.2,-1.08917002000001));
#315224=CARTESIAN_POINT('Ctrl Pts',(-4.23612215200006,5.2,-1.08917002000001));
#315225=CARTESIAN_POINT('Ctrl Pts',(-4.23612215200006,2.2,-1.08917002000001));
#315226=CARTESIAN_POINT('Ctrl Pts',(-4.23416928100006,12.2,-1.08950086000001));
#315227=CARTESIAN_POINT('Ctrl Pts',(-4.23416928100006,5.2,-1.08950086000001));
#315228=CARTESIAN_POINT('Ctrl Pts',(-4.23416928100006,2.2,-1.08950086000001));
#315229=CARTESIAN_POINT('Ctrl Pts',(-4.23222008800006,12.2,-1.08982884600001));
#315230=CARTESIAN_POINT('Ctrl Pts',(-4.23222008800006,5.2,-1.08982884600001));
#315231=CARTESIAN_POINT('Ctrl Pts',(-4.23222008800006,2.2,-1.08982884600001));
#315232=CARTESIAN_POINT('Ctrl Pts',(-4.23027457600006,12.2,-1.09015398800001));
#315233=CARTESIAN_POINT('Ctrl Pts',(-4.23027457600006,5.2,-1.09015398800001));
#315234=CARTESIAN_POINT('Ctrl Pts',(-4.23027457600006,2.2,-1.09015398800001));
#315235=CARTESIAN_POINT('Ctrl Pts',(-4.22833275800006,12.2,-1.09047629200001));
#315236=CARTESIAN_POINT('Ctrl Pts',(-4.22833275800006,5.2,-1.09047629200001));
#315237=CARTESIAN_POINT('Ctrl Pts',(-4.22833275800006,2.2,-1.09047629200001));
#315238=CARTESIAN_POINT('Ctrl Pts',(-4.22639464000006,12.2,-1.09079576400001));
#315239=CARTESIAN_POINT('Ctrl Pts',(-4.22639464000006,5.2,-1.09079576400001));
#315240=CARTESIAN_POINT('Ctrl Pts',(-4.22639464000006,2.2,-1.09079576400001));
#315241=CARTESIAN_POINT('Ctrl Pts',(-4.22446023100005,12.2,-1.09111241100001));
#315242=CARTESIAN_POINT('Ctrl Pts',(-4.22446023100005,5.2,-1.09111241100001));
#315243=CARTESIAN_POINT('Ctrl Pts',(-4.22446023100005,2.2,-1.09111241100001));
#315244=CARTESIAN_POINT('Ctrl Pts',(-4.22252954000006,12.2,-1.09142624100001));
#315245=CARTESIAN_POINT('Ctrl Pts',(-4.22252954000006,5.2,-1.09142624100001));
#315246=CARTESIAN_POINT('Ctrl Pts',(-4.22252954000006,2.2,-1.09142624100001));
#315247=CARTESIAN_POINT('Ctrl Pts',(-4.22060257600006,12.2,-1.09173726000002));
#315248=CARTESIAN_POINT('Ctrl Pts',(-4.22060257600006,5.2,-1.09173726000002));
#315249=CARTESIAN_POINT('Ctrl Pts',(-4.22060257600006,2.2,-1.09173726000002));
#315250=CARTESIAN_POINT('Ctrl Pts',(-4.21867934700006,12.2,-1.09204547600001));
#315251=CARTESIAN_POINT('Ctrl Pts',(-4.21867934700006,5.2,-1.09204547600001));
#315252=CARTESIAN_POINT('Ctrl Pts',(-4.21867934700006,2.2,-1.09204547600001));
#315253=CARTESIAN_POINT('Ctrl Pts',(-4.21675986200006,12.2,-1.09235089600002));
#315254=CARTESIAN_POINT('Ctrl Pts',(-4.21675986200006,5.2,-1.09235089600002));
#315255=CARTESIAN_POINT('Ctrl Pts',(-4.21675986200006,2.2,-1.09235089600002));
#315256=CARTESIAN_POINT('Ctrl Pts',(-4.21484413000006,12.2,-1.09265352600001));
#315257=CARTESIAN_POINT('Ctrl Pts',(-4.21484413000006,5.2,-1.09265352600001));
#315258=CARTESIAN_POINT('Ctrl Pts',(-4.21484413000006,2.2,-1.09265352600001));
#315259=CARTESIAN_POINT('Ctrl Pts',(-4.21293215800006,12.2,-1.09295337400001));
#315260=CARTESIAN_POINT('Ctrl Pts',(-4.21293215800006,5.2,-1.09295337400001));
#315261=CARTESIAN_POINT('Ctrl Pts',(-4.21293215800006,2.2,-1.09295337400001));
#315262=CARTESIAN_POINT('Ctrl Pts',(-4.21102395600006,12.2,-1.09325044600002));
#315263=CARTESIAN_POINT('Ctrl Pts',(-4.21102395600006,5.2,-1.09325044600002));
#315264=CARTESIAN_POINT('Ctrl Pts',(-4.21102395600006,2.2,-1.09325044600002));
#315265=CARTESIAN_POINT('Ctrl Pts',(-4.20911953100005,12.2,-1.09354475000002));
#315266=CARTESIAN_POINT('Ctrl Pts',(-4.20911953100005,5.2,-1.09354475000002));
#315267=CARTESIAN_POINT('Ctrl Pts',(-4.20911953100005,2.2,-1.09354475000002));
#315268=CARTESIAN_POINT('Ctrl Pts',(-4.20721889400006,12.2,-1.09383629300002));
#315269=CARTESIAN_POINT('Ctrl Pts',(-4.20721889400006,5.2,-1.09383629300002));
#315270=CARTESIAN_POINT('Ctrl Pts',(-4.20721889400006,2.2,-1.09383629300002));
#315271=CARTESIAN_POINT('Ctrl Pts',(-4.20532205200006,12.2,-1.09412508200001));
#315272=CARTESIAN_POINT('Ctrl Pts',(-4.20532205200006,5.2,-1.09412508200001));
#315273=CARTESIAN_POINT('Ctrl Pts',(-4.20532205200006,2.2,-1.09412508200001));
#315274=CARTESIAN_POINT('Ctrl Pts',(-4.20342901500006,12.2,-1.09441112300001));
#315275=CARTESIAN_POINT('Ctrl Pts',(-4.20342901500006,5.2,-1.09441112300001));
#315276=CARTESIAN_POINT('Ctrl Pts',(-4.20342901500006,2.2,-1.09441112300001));
#315277=CARTESIAN_POINT('Ctrl Pts',(-4.20153979000006,12.2,-1.09469442700002));
#315278=CARTESIAN_POINT('Ctrl Pts',(-4.20153979000006,5.2,-1.09469442700002));
#315279=CARTESIAN_POINT('Ctrl Pts',(-4.20153979000006,2.2,-1.09469442700002));
#315280=CARTESIAN_POINT('Ctrl Pts',(-4.19965438700006,12.2,-1.09497499600002));
#315281=CARTESIAN_POINT('Ctrl Pts',(-4.19965438700006,5.2,-1.09497499600002));
#315282=CARTESIAN_POINT('Ctrl Pts',(-4.19965438700006,2.2,-1.09497499600002));
#315283=CARTESIAN_POINT('Ctrl Pts',(-4.19777281400005,12.2,-1.09525284200001));
#315284=CARTESIAN_POINT('Ctrl Pts',(-4.19777281400005,5.2,-1.09525284200001));
#315285=CARTESIAN_POINT('Ctrl Pts',(-4.19777281400005,2.2,-1.09525284200001));
#315286=CARTESIAN_POINT('Ctrl Pts',(-4.19589508000006,12.2,-1.09552797000001));
#315287=CARTESIAN_POINT('Ctrl Pts',(-4.19589508000006,5.2,-1.09552797000001));
#315288=CARTESIAN_POINT('Ctrl Pts',(-4.19589508000006,2.2,-1.09552797000001));
#315289=CARTESIAN_POINT('Ctrl Pts',(-4.19402119200006,12.2,-1.09580038700001));
#315290=CARTESIAN_POINT('Ctrl Pts',(-4.19402119200006,5.2,-1.09580038700001));
#315291=CARTESIAN_POINT('Ctrl Pts',(-4.19402119200006,2.2,-1.09580038700001));
#315292=CARTESIAN_POINT('Ctrl Pts',(-4.19215116100006,12.2,-1.09607010100001));
#315293=CARTESIAN_POINT('Ctrl Pts',(-4.19215116100006,5.2,-1.09607010100001));
#315294=CARTESIAN_POINT('Ctrl Pts',(-4.19215116100006,2.2,-1.09607010100001));
#315295=CARTESIAN_POINT('Ctrl Pts',(-4.19028499500006,12.2,-1.09633711900001));
#315296=CARTESIAN_POINT('Ctrl Pts',(-4.19028499500006,5.2,-1.09633711900001));
#315297=CARTESIAN_POINT('Ctrl Pts',(-4.19028499500006,2.2,-1.09633711900001));
#315298=CARTESIAN_POINT('Ctrl Pts',(-4.18842270200006,12.2,-1.09660144900001));
#315299=CARTESIAN_POINT('Ctrl Pts',(-4.18842270200006,5.2,-1.09660144900001));
#315300=CARTESIAN_POINT('Ctrl Pts',(-4.18842270200006,2.2,-1.09660144900001));
#315301=CARTESIAN_POINT('Ctrl Pts',(-4.18656429100006,12.2,-1.09686309800002));
#315302=CARTESIAN_POINT('Ctrl Pts',(-4.18656429100006,5.2,-1.09686309800002));
#315303=CARTESIAN_POINT('Ctrl Pts',(-4.18656429100006,2.2,-1.09686309800002));
#315304=CARTESIAN_POINT('Ctrl Pts',(-4.18470977100006,12.2,-1.09712207300001));
#315305=CARTESIAN_POINT('Ctrl Pts',(-4.18470977100006,5.2,-1.09712207300001));
#315306=CARTESIAN_POINT('Ctrl Pts',(-4.18470977100006,2.2,-1.09712207300001));
#315307=CARTESIAN_POINT('Ctrl Pts',(-4.18285915000006,12.2,-1.09737838300001));
#315308=CARTESIAN_POINT('Ctrl Pts',(-4.18285915000006,5.2,-1.09737838300001));
#315309=CARTESIAN_POINT('Ctrl Pts',(-4.18285915000006,2.2,-1.09737838300001));
#315310=CARTESIAN_POINT('Ctrl Pts',(-4.18101243800006,12.2,-1.09763203300002));
#315311=CARTESIAN_POINT('Ctrl Pts',(-4.18101243800006,5.2,-1.09763203300002));
#315312=CARTESIAN_POINT('Ctrl Pts',(-4.18101243800006,2.2,-1.09763203300002));
#315313=CARTESIAN_POINT('Ctrl Pts',(-4.17916964200006,12.2,-1.09788303300002));
#315314=CARTESIAN_POINT('Ctrl Pts',(-4.17916964200006,5.2,-1.09788303300002));
#315315=CARTESIAN_POINT('Ctrl Pts',(-4.17916964200006,2.2,-1.09788303300002));
#315316=CARTESIAN_POINT('Ctrl Pts',(-4.17733077200006,12.2,-1.09813138900002));
#315317=CARTESIAN_POINT('Ctrl Pts',(-4.17733077200006,5.2,-1.09813138900002));
#315318=CARTESIAN_POINT('Ctrl Pts',(-4.17733077200006,2.2,-1.09813138900002));
#315319=CARTESIAN_POINT('Ctrl Pts',(-4.17549583700006,12.2,-1.09837710900001));
#315320=CARTESIAN_POINT('Ctrl Pts',(-4.17549583700006,5.2,-1.09837710900001));
#315321=CARTESIAN_POINT('Ctrl Pts',(-4.17549583700006,2.2,-1.09837710900001));
#315322=CARTESIAN_POINT('Ctrl Pts',(-4.17366484400006,12.2,-1.09862020100001));
#315323=CARTESIAN_POINT('Ctrl Pts',(-4.17366484400006,5.2,-1.09862020100001));
#315324=CARTESIAN_POINT('Ctrl Pts',(-4.17366484400006,2.2,-1.09862020100001));
#315325=CARTESIAN_POINT('Ctrl Pts',(-4.17183780200006,12.2,-1.09886067100001));
#315326=CARTESIAN_POINT('Ctrl Pts',(-4.17183780200006,5.2,-1.09886067100001));
#315327=CARTESIAN_POINT('Ctrl Pts',(-4.17183780200006,2.2,-1.09886067100001));
#315328=CARTESIAN_POINT('Ctrl Pts',(-4.17001472200006,12.2,-1.09909852800001));
#315329=CARTESIAN_POINT('Ctrl Pts',(-4.17001472200006,5.2,-1.09909852800001));
#315330=CARTESIAN_POINT('Ctrl Pts',(-4.17001472200006,2.2,-1.09909852800001));
#315331=CARTESIAN_POINT('Ctrl Pts',(-4.16819561000006,12.2,-1.09933378000001));
#315332=CARTESIAN_POINT('Ctrl Pts',(-4.16819561000006,5.2,-1.09933378000001));
#315333=CARTESIAN_POINT('Ctrl Pts',(-4.16819561000006,2.2,-1.09933378000001));
#315334=CARTESIAN_POINT('Ctrl Pts',(-4.16638047600006,12.2,-1.09956643300002));
#315335=CARTESIAN_POINT('Ctrl Pts',(-4.16638047600006,5.2,-1.09956643300002));
#315336=CARTESIAN_POINT('Ctrl Pts',(-4.16638047600006,2.2,-1.09956643300002));
#315337=CARTESIAN_POINT('Ctrl Pts',(-4.16456932900005,12.2,-1.09979649700001));
#315338=CARTESIAN_POINT('Ctrl Pts',(-4.16456932900005,5.2,-1.09979649700001));
#315339=CARTESIAN_POINT('Ctrl Pts',(-4.16456932900005,2.2,-1.09979649700001));
#315340=CARTESIAN_POINT('Ctrl Pts',(-4.16276217800006,12.2,-1.10002397800002));
#315341=CARTESIAN_POINT('Ctrl Pts',(-4.16276217800006,5.2,-1.10002397800002));
#315342=CARTESIAN_POINT('Ctrl Pts',(-4.16276217800006,2.2,-1.10002397800002));
#315343=CARTESIAN_POINT('Ctrl Pts',(-4.16095903000006,12.2,-1.10024888400002));
#315344=CARTESIAN_POINT('Ctrl Pts',(-4.16095903000006,5.2,-1.10024888400002));
#315345=CARTESIAN_POINT('Ctrl Pts',(-4.16095903000006,2.2,-1.10024888400002));
#315346=CARTESIAN_POINT('Ctrl Pts',(-4.15915989500006,12.2,-1.10047122300001));
#315347=CARTESIAN_POINT('Ctrl Pts',(-4.15915989500006,5.2,-1.10047122300001));
#315348=CARTESIAN_POINT('Ctrl Pts',(-4.15915989500006,2.2,-1.10047122300001));
#315349=CARTESIAN_POINT('Ctrl Pts',(-4.15736478200006,12.2,-1.10069100400001));
#315350=CARTESIAN_POINT('Ctrl Pts',(-4.15736478200006,5.2,-1.10069100400001));
#315351=CARTESIAN_POINT('Ctrl Pts',(-4.15736478200006,2.2,-1.10069100400001));
#315352=CARTESIAN_POINT('Ctrl Pts',(-4.15557369900006,12.2,-1.10090823200002));
#315353=CARTESIAN_POINT('Ctrl Pts',(-4.15557369900006,5.2,-1.10090823200002));
#315354=CARTESIAN_POINT('Ctrl Pts',(-4.15557369900006,2.2,-1.10090823200002));
#315355=CARTESIAN_POINT('Ctrl Pts',(-4.15378665500006,12.2,-1.10112291800001));
#315356=CARTESIAN_POINT('Ctrl Pts',(-4.15378665500006,5.2,-1.10112291800001));
#315357=CARTESIAN_POINT('Ctrl Pts',(-4.15378665500006,2.2,-1.10112291800001));
#315358=CARTESIAN_POINT('Ctrl Pts',(-4.15200365900006,12.2,-1.10133506700001));
#315359=CARTESIAN_POINT('Ctrl Pts',(-4.15200365900006,5.2,-1.10133506700001));
#315360=CARTESIAN_POINT('Ctrl Pts',(-4.15200365900006,2.2,-1.10133506700001));
#315361=CARTESIAN_POINT('Ctrl Pts',(-4.15022472000006,12.2,-1.10154468900001));
#315362=CARTESIAN_POINT('Ctrl Pts',(-4.15022472000006,5.2,-1.10154468900001));
#315363=CARTESIAN_POINT('Ctrl Pts',(-4.15022472000006,2.2,-1.10154468900001));
#315364=CARTESIAN_POINT('Ctrl Pts',(-4.14844984500006,12.2,-1.10175179100001));
#315365=CARTESIAN_POINT('Ctrl Pts',(-4.14844984500006,5.2,-1.10175179100001));
#315366=CARTESIAN_POINT('Ctrl Pts',(-4.14844984500006,2.2,-1.10175179100001));
#315367=CARTESIAN_POINT('Ctrl Pts',(-4.14667904500006,12.2,-1.10195638100001));
#315368=CARTESIAN_POINT('Ctrl Pts',(-4.14667904500006,5.2,-1.10195638100001));
#315369=CARTESIAN_POINT('Ctrl Pts',(-4.14667904500006,2.2,-1.10195638100001));
#315370=CARTESIAN_POINT('Ctrl Pts',(-4.14491232900006,12.2,-1.10215846800001));
#315371=CARTESIAN_POINT('Ctrl Pts',(-4.14491232900006,5.2,-1.10215846800001));
#315372=CARTESIAN_POINT('Ctrl Pts',(-4.14491232900006,2.2,-1.10215846800001));
#315373=CARTESIAN_POINT('Ctrl Pts',(-4.14314970300006,12.2,-1.10235805800002));
#315374=CARTESIAN_POINT('Ctrl Pts',(-4.14314970300006,5.2,-1.10235805800002));
#315375=CARTESIAN_POINT('Ctrl Pts',(-4.14314970300006,2.2,-1.10235805800002));
#315376=CARTESIAN_POINT('Ctrl Pts',(-4.14139117900006,12.2,-1.10255516000001));
#315377=CARTESIAN_POINT('Ctrl Pts',(-4.14139117900006,5.2,-1.10255516000001));
#315378=CARTESIAN_POINT('Ctrl Pts',(-4.14139117900006,2.2,-1.10255516000001));
#315379=CARTESIAN_POINT('Ctrl Pts',(-4.13963676400006,12.2,-1.10274978300001));
#315380=CARTESIAN_POINT('Ctrl Pts',(-4.13963676400006,5.2,-1.10274978300001));
#315381=CARTESIAN_POINT('Ctrl Pts',(-4.13963676400006,2.2,-1.10274978300001));
#315382=CARTESIAN_POINT('Ctrl Pts',(-4.13788646700006,12.2,-1.10294193400001));
#315383=CARTESIAN_POINT('Ctrl Pts',(-4.13788646700006,5.2,-1.10294193400001));
#315384=CARTESIAN_POINT('Ctrl Pts',(-4.13788646700006,2.2,-1.10294193400001));
#315385=CARTESIAN_POINT('Ctrl Pts',(-4.13614029700006,12.2,-1.10313162300002));
#315386=CARTESIAN_POINT('Ctrl Pts',(-4.13614029700006,5.2,-1.10313162300002));
#315387=CARTESIAN_POINT('Ctrl Pts',(-4.13614029700006,2.2,-1.10313162300002));
#315388=CARTESIAN_POINT('Ctrl Pts',(-4.13439826300006,12.2,-1.10331885500001));
#315389=CARTESIAN_POINT('Ctrl Pts',(-4.13439826300006,5.2,-1.10331885500001));
#315390=CARTESIAN_POINT('Ctrl Pts',(-4.13439826300006,2.2,-1.10331885500001));
#315391=CARTESIAN_POINT('Ctrl Pts',(-4.13266037300006,12.2,-1.10350364000002));
#315392=CARTESIAN_POINT('Ctrl Pts',(-4.13266037300006,5.2,-1.10350364000002));
#315393=CARTESIAN_POINT('Ctrl Pts',(-4.13266037300006,2.2,-1.10350364000002));
#315394=CARTESIAN_POINT('Ctrl Pts',(-4.13092663700006,12.2,-1.10368598600001));
#315395=CARTESIAN_POINT('Ctrl Pts',(-4.13092663700006,5.2,-1.10368598600001));
#315396=CARTESIAN_POINT('Ctrl Pts',(-4.13092663700006,2.2,-1.10368598600001));
#315397=CARTESIAN_POINT('Ctrl Pts',(-4.12919706300006,12.2,-1.10386590200001));
#315398=CARTESIAN_POINT('Ctrl Pts',(-4.12919706300006,5.2,-1.10386590200001));
#315399=CARTESIAN_POINT('Ctrl Pts',(-4.12919706300006,2.2,-1.10386590200001));
#315400=CARTESIAN_POINT('Ctrl Pts',(-4.12747166000006,12.2,-1.10404339400001));
#315401=CARTESIAN_POINT('Ctrl Pts',(-4.12747166000006,5.2,-1.10404339400001));
#315402=CARTESIAN_POINT('Ctrl Pts',(-4.12747166000006,2.2,-1.10404339400001));
#315403=CARTESIAN_POINT('Ctrl Pts',(-4.12575043700006,12.2,-1.10421847200001));
#315404=CARTESIAN_POINT('Ctrl Pts',(-4.12575043700006,5.2,-1.10421847200001));
#315405=CARTESIAN_POINT('Ctrl Pts',(-4.12575043700006,2.2,-1.10421847200001));
#315406=CARTESIAN_POINT('Ctrl Pts',(-4.12403340300005,12.2,-1.10439114400001));
#315407=CARTESIAN_POINT('Ctrl Pts',(-4.12403340300005,5.2,-1.10439114400001));
#315408=CARTESIAN_POINT('Ctrl Pts',(-4.12403340300005,2.2,-1.10439114400001));
#315409=CARTESIAN_POINT('Ctrl Pts',(-4.12232056700006,12.2,-1.10456141800002));
#315410=CARTESIAN_POINT('Ctrl Pts',(-4.12232056700006,5.2,-1.10456141800002));
#315411=CARTESIAN_POINT('Ctrl Pts',(-4.12232056700006,2.2,-1.10456141800002));
#315412=CARTESIAN_POINT('Ctrl Pts',(-4.12061193700006,12.2,-1.10472930400002));
#315413=CARTESIAN_POINT('Ctrl Pts',(-4.12061193700006,5.2,-1.10472930400002));
#315414=CARTESIAN_POINT('Ctrl Pts',(-4.12061193700006,2.2,-1.10472930400002));
#315415=CARTESIAN_POINT('Ctrl Pts',(-4.11890752200006,12.2,-1.10489480800001));
#315416=CARTESIAN_POINT('Ctrl Pts',(-4.11890752200006,5.2,-1.10489480800001));
#315417=CARTESIAN_POINT('Ctrl Pts',(-4.11890752200006,2.2,-1.10489480800001));
#315418=CARTESIAN_POINT('Ctrl Pts',(-4.11720733200006,12.2,-1.10505794000002));
#315419=CARTESIAN_POINT('Ctrl Pts',(-4.11720733200006,5.2,-1.10505794000002));
#315420=CARTESIAN_POINT('Ctrl Pts',(-4.11720733200006,2.2,-1.10505794000002));
#315421=CARTESIAN_POINT('Ctrl Pts',(-4.11551137500005,12.2,-1.10521870600001));
#315422=CARTESIAN_POINT('Ctrl Pts',(-4.11551137500005,5.2,-1.10521870600001));
#315423=CARTESIAN_POINT('Ctrl Pts',(-4.11551137500005,2.2,-1.10521870600001));
#315424=CARTESIAN_POINT('Ctrl Pts',(-4.11381965900006,12.2,-1.10537711800001));
#315425=CARTESIAN_POINT('Ctrl Pts',(-4.11381965900006,5.2,-1.10537711800001));
#315426=CARTESIAN_POINT('Ctrl Pts',(-4.11381965900006,2.2,-1.10537711800001));
#315427=CARTESIAN_POINT('Ctrl Pts',(-4.11213219500006,12.2,-1.10553318300001));
#315428=CARTESIAN_POINT('Ctrl Pts',(-4.11213219500006,5.2,-1.10553318300001));
#315429=CARTESIAN_POINT('Ctrl Pts',(-4.11213219500006,2.2,-1.10553318300001));
#315430=CARTESIAN_POINT('Ctrl Pts',(-4.11044899000006,12.2,-1.10568690900001));
#315431=CARTESIAN_POINT('Ctrl Pts',(-4.11044899000006,5.2,-1.10568690900001));
#315432=CARTESIAN_POINT('Ctrl Pts',(-4.11044899000006,2.2,-1.10568690900001));
#315433=CARTESIAN_POINT('Ctrl Pts',(-4.10877005300006,12.2,-1.10583830500001));
#315434=CARTESIAN_POINT('Ctrl Pts',(-4.10877005300006,5.2,-1.10583830500001));
#315435=CARTESIAN_POINT('Ctrl Pts',(-4.10877005300006,2.2,-1.10583830500001));
#315436=CARTESIAN_POINT('Ctrl Pts',(-4.10709539400006,12.2,-1.10598737900002));
#315437=CARTESIAN_POINT('Ctrl Pts',(-4.10709539400006,5.2,-1.10598737900002));
#315438=CARTESIAN_POINT('Ctrl Pts',(-4.10709539400006,2.2,-1.10598737900002));
#315439=CARTESIAN_POINT('Ctrl Pts',(-4.10542502200006,12.2,-1.10613414000001));
#315440=CARTESIAN_POINT('Ctrl Pts',(-4.10542502200006,5.2,-1.10613414000001));
#315441=CARTESIAN_POINT('Ctrl Pts',(-4.10542502200006,2.2,-1.10613414000001));
#315442=CARTESIAN_POINT('Ctrl Pts',(-4.10375894400006,12.2,-1.10627859800001));
#315443=CARTESIAN_POINT('Ctrl Pts',(-4.10375894400006,5.2,-1.10627859800001));
#315444=CARTESIAN_POINT('Ctrl Pts',(-4.10375894400006,2.2,-1.10627859800001));
#315445=CARTESIAN_POINT('Ctrl Pts',(-4.10209717100006,12.2,-1.10642075900001));
#315446=CARTESIAN_POINT('Ctrl Pts',(-4.10209717100006,5.2,-1.10642075900001));
#315447=CARTESIAN_POINT('Ctrl Pts',(-4.10209717100006,2.2,-1.10642075900001));
#315448=CARTESIAN_POINT('Ctrl Pts',(-4.10043971100006,12.2,-1.10656063300001));
#315449=CARTESIAN_POINT('Ctrl Pts',(-4.10043971100006,5.2,-1.10656063300001));
#315450=CARTESIAN_POINT('Ctrl Pts',(-4.10043971100006,2.2,-1.10656063300001));
#315451=CARTESIAN_POINT('Ctrl Pts',(-4.09878657300006,12.2,-1.10669823000002));
#315452=CARTESIAN_POINT('Ctrl Pts',(-4.09878657300006,5.2,-1.10669823000002));
#315453=CARTESIAN_POINT('Ctrl Pts',(-4.09878657300006,2.2,-1.10669823000002));
#315454=CARTESIAN_POINT('Ctrl Pts',(-4.09713776600006,12.2,-1.10683355700001));
#315455=CARTESIAN_POINT('Ctrl Pts',(-4.09713776600006,5.2,-1.10683355700001));
#315456=CARTESIAN_POINT('Ctrl Pts',(-4.09713776600006,2.2,-1.10683355700001));
#315457=CARTESIAN_POINT('Ctrl Pts',(-4.09549329900006,12.2,-1.10696662200001));
#315458=CARTESIAN_POINT('Ctrl Pts',(-4.09549329900006,5.2,-1.10696662200001));
#315459=CARTESIAN_POINT('Ctrl Pts',(-4.09549329900006,2.2,-1.10696662200001));
#315460=CARTESIAN_POINT('Ctrl Pts',(-4.09385318100006,12.2,-1.10709743600002));
#315461=CARTESIAN_POINT('Ctrl Pts',(-4.09385318100006,5.2,-1.10709743600002));
#315462=CARTESIAN_POINT('Ctrl Pts',(-4.09385318100006,2.2,-1.10709743600002));
#315463=CARTESIAN_POINT('Ctrl Pts',(-4.09221742000006,12.2,-1.10722600800001));
#315464=CARTESIAN_POINT('Ctrl Pts',(-4.09221742000006,5.2,-1.10722600800001));
#315465=CARTESIAN_POINT('Ctrl Pts',(-4.09221742000006,2.2,-1.10722600800001));
#315466=CARTESIAN_POINT('Ctrl Pts',(-4.09058602500005,12.2,-1.10735234400002));
#315467=CARTESIAN_POINT('Ctrl Pts',(-4.09058602500005,5.2,-1.10735234400002));
#315468=CARTESIAN_POINT('Ctrl Pts',(-4.09058602500005,2.2,-1.10735234400002));
#315469=CARTESIAN_POINT('Ctrl Pts',(-4.08895900700006,12.2,-1.10747645600001));
#315470=CARTESIAN_POINT('Ctrl Pts',(-4.08895900700006,5.2,-1.10747645600001));
#315471=CARTESIAN_POINT('Ctrl Pts',(-4.08895900700006,2.2,-1.10747645600001));
#315472=CARTESIAN_POINT('Ctrl Pts',(-4.08733637300006,12.2,-1.10759835000001));
#315473=CARTESIAN_POINT('Ctrl Pts',(-4.08733637300006,5.2,-1.10759835000001));
#315474=CARTESIAN_POINT('Ctrl Pts',(-4.08733637300006,2.2,-1.10759835000001));
#315475=CARTESIAN_POINT('Ctrl Pts',(-4.08571813300005,12.2,-1.10771803800001));
#315476=CARTESIAN_POINT('Ctrl Pts',(-4.08571813300005,5.2,-1.10771803800001));
#315477=CARTESIAN_POINT('Ctrl Pts',(-4.08571813300005,2.2,-1.10771803800001));
#315478=CARTESIAN_POINT('Ctrl Pts',(-4.08410429500006,12.2,-1.10783552700001));
#315479=CARTESIAN_POINT('Ctrl Pts',(-4.08410429500006,5.2,-1.10783552700001));
#315480=CARTESIAN_POINT('Ctrl Pts',(-4.08410429500006,2.2,-1.10783552700001));
#315481=CARTESIAN_POINT('Ctrl Pts',(-4.08249486800006,12.2,-1.10795082600001));
#315482=CARTESIAN_POINT('Ctrl Pts',(-4.08249486800006,5.2,-1.10795082600001));
#315483=CARTESIAN_POINT('Ctrl Pts',(-4.08249486800006,2.2,-1.10795082600001));
#315484=CARTESIAN_POINT('Ctrl Pts',(-4.08088986100006,12.2,-1.10806394500001));
#315485=CARTESIAN_POINT('Ctrl Pts',(-4.08088986100006,5.2,-1.10806394500001));
#315486=CARTESIAN_POINT('Ctrl Pts',(-4.08088986100006,2.2,-1.10806394500001));
#315487=CARTESIAN_POINT('Ctrl Pts',(-4.07928928400006,12.2,-1.10817489300001));
#315488=CARTESIAN_POINT('Ctrl Pts',(-4.07928928400006,5.2,-1.10817489300001));
#315489=CARTESIAN_POINT('Ctrl Pts',(-4.07928928400006,2.2,-1.10817489300001));
#315490=CARTESIAN_POINT('Ctrl Pts',(-4.07769314600006,12.2,-1.10828367800002));
#315491=CARTESIAN_POINT('Ctrl Pts',(-4.07769314600006,5.2,-1.10828367800002));
#315492=CARTESIAN_POINT('Ctrl Pts',(-4.07769314600006,2.2,-1.10828367800002));
#315493=CARTESIAN_POINT('Ctrl Pts',(-4.07610145500006,12.2,-1.10839030900001));
#315494=CARTESIAN_POINT('Ctrl Pts',(-4.07610145500006,5.2,-1.10839030900001));
#315495=CARTESIAN_POINT('Ctrl Pts',(-4.07610145500006,2.2,-1.10839030900001));
#315496=CARTESIAN_POINT('Ctrl Pts',(-4.07451422000006,12.2,-1.10849479700001));
#315497=CARTESIAN_POINT('Ctrl Pts',(-4.07451422000006,5.2,-1.10849479700001));
#315498=CARTESIAN_POINT('Ctrl Pts',(-4.07451422000006,2.2,-1.10849479700001));
#315499=CARTESIAN_POINT('Ctrl Pts',(-4.07293145100006,12.2,-1.10859715000001));
#315500=CARTESIAN_POINT('Ctrl Pts',(-4.07293145100006,5.2,-1.10859715000001));
#315501=CARTESIAN_POINT('Ctrl Pts',(-4.07293145100006,2.2,-1.10859715000001));
#315502=CARTESIAN_POINT('Ctrl Pts',(-4.07135315500006,12.2,-1.10869737700002));
#315503=CARTESIAN_POINT('Ctrl Pts',(-4.07135315500006,5.2,-1.10869737700002));
#315504=CARTESIAN_POINT('Ctrl Pts',(-4.07135315500006,2.2,-1.10869737700002));
#315505=CARTESIAN_POINT('Ctrl Pts',(-4.06977934300006,12.2,-1.10879548800002));
#315506=CARTESIAN_POINT('Ctrl Pts',(-4.06977934300006,5.2,-1.10879548800002));
#315507=CARTESIAN_POINT('Ctrl Pts',(-4.06977934300006,2.2,-1.10879548800002));
#315508=CARTESIAN_POINT('Ctrl Pts',(-4.06821002300005,12.2,-1.10889149100001));
#315509=CARTESIAN_POINT('Ctrl Pts',(-4.06821002300005,5.2,-1.10889149100001));
#315510=CARTESIAN_POINT('Ctrl Pts',(-4.06821002300005,2.2,-1.10889149100001));
#315511=CARTESIAN_POINT('Ctrl Pts',(-4.06664520500006,12.2,-1.10898539700001));
#315512=CARTESIAN_POINT('Ctrl Pts',(-4.06664520500006,5.2,-1.10898539700001));
#315513=CARTESIAN_POINT('Ctrl Pts',(-4.06664520500006,2.2,-1.10898539700001));
#315514=CARTESIAN_POINT('Ctrl Pts',(-4.06508489700006,12.2,-1.10907721400002));
#315515=CARTESIAN_POINT('Ctrl Pts',(-4.06508489700006,5.2,-1.10907721400002));
#315516=CARTESIAN_POINT('Ctrl Pts',(-4.06508489700006,2.2,-1.10907721400002));
#315517=CARTESIAN_POINT('Ctrl Pts',(-4.06352910800006,12.2,-1.10916695200002));
#315518=CARTESIAN_POINT('Ctrl Pts',(-4.06352910800006,5.2,-1.10916695200002));
#315519=CARTESIAN_POINT('Ctrl Pts',(-4.06352910800006,2.2,-1.10916695200002));
#315520=CARTESIAN_POINT('Ctrl Pts',(-4.06197784800006,12.2,-1.10925462000001));
#315521=CARTESIAN_POINT('Ctrl Pts',(-4.06197784800006,5.2,-1.10925462000001));
#315522=CARTESIAN_POINT('Ctrl Pts',(-4.06197784800006,2.2,-1.10925462000001));
#315523=CARTESIAN_POINT('Ctrl Pts',(-4.06043112600006,12.2,-1.10934022800001));
#315524=CARTESIAN_POINT('Ctrl Pts',(-4.06043112600006,5.2,-1.10934022800001));
#315525=CARTESIAN_POINT('Ctrl Pts',(-4.06043112600006,2.2,-1.10934022800001));
#315526=CARTESIAN_POINT('Ctrl Pts',(-4.05888894900006,12.2,-1.10942378500001));
#315527=CARTESIAN_POINT('Ctrl Pts',(-4.05888894900006,5.2,-1.10942378500001));
#315528=CARTESIAN_POINT('Ctrl Pts',(-4.05888894900006,2.2,-1.10942378500001));
#315529=CARTESIAN_POINT('Ctrl Pts',(-4.05735132800006,12.2,-1.10950530000002));
#315530=CARTESIAN_POINT('Ctrl Pts',(-4.05735132800006,5.2,-1.10950530000002));
#315531=CARTESIAN_POINT('Ctrl Pts',(-4.05735132800006,2.2,-1.10950530000002));
#315532=CARTESIAN_POINT('Ctrl Pts',(-4.05581827300006,12.2,-1.10958478400002));
#315533=CARTESIAN_POINT('Ctrl Pts',(-4.05581827300006,5.2,-1.10958478400002));
#315534=CARTESIAN_POINT('Ctrl Pts',(-4.05581827300006,2.2,-1.10958478400002));
#315535=CARTESIAN_POINT('Ctrl Pts',(-4.05428979000006,12.2,-1.10966224400002));
#315536=CARTESIAN_POINT('Ctrl Pts',(-4.05428979000006,5.2,-1.10966224400002));
#315537=CARTESIAN_POINT('Ctrl Pts',(-4.05428979000006,2.2,-1.10966224400002));
#315538=CARTESIAN_POINT('Ctrl Pts',(-4.05276589100006,12.2,-1.10973769300001));
#315539=CARTESIAN_POINT('Ctrl Pts',(-4.05276589100006,5.2,-1.10973769300001));
#315540=CARTESIAN_POINT('Ctrl Pts',(-4.05276589100006,2.2,-1.10973769300001));
#315541=CARTESIAN_POINT('Ctrl Pts',(-4.05124658200006,12.2,-1.10981113800001));
#315542=CARTESIAN_POINT('Ctrl Pts',(-4.05124658200006,5.2,-1.10981113800001));
#315543=CARTESIAN_POINT('Ctrl Pts',(-4.05124658200006,2.2,-1.10981113800001));
#315544=CARTESIAN_POINT('Ctrl Pts',(-4.04973187600006,12.2,-1.10988258900001));
#315545=CARTESIAN_POINT('Ctrl Pts',(-4.04973187600006,5.2,-1.10988258900001));
#315546=CARTESIAN_POINT('Ctrl Pts',(-4.04973187600006,2.2,-1.10988258900001));
#315547=CARTESIAN_POINT('Ctrl Pts',(-4.04822177800006,12.2,-1.10995205700001));
#315548=CARTESIAN_POINT('Ctrl Pts',(-4.04822177800006,5.2,-1.10995205700001));
#315549=CARTESIAN_POINT('Ctrl Pts',(-4.04822177800006,2.2,-1.10995205700001));
#315550=CARTESIAN_POINT('Ctrl Pts',(-4.04671630000006,12.2,-1.11001955000001));
#315551=CARTESIAN_POINT('Ctrl Pts',(-4.04671630000006,5.2,-1.11001955000001));
#315552=CARTESIAN_POINT('Ctrl Pts',(-4.04671630000006,2.2,-1.11001955000001));
#315553=CARTESIAN_POINT('Ctrl Pts',(-4.04521545000006,12.2,-1.11008507900001));
#315554=CARTESIAN_POINT('Ctrl Pts',(-4.04521545000006,5.2,-1.11008507900001));
#315555=CARTESIAN_POINT('Ctrl Pts',(-4.04521545000006,2.2,-1.11008507900001));
#315556=CARTESIAN_POINT('Ctrl Pts',(-4.04371923700006,12.2,-1.11014865300001));
#315557=CARTESIAN_POINT('Ctrl Pts',(-4.04371923700006,5.2,-1.11014865300001));
#315558=CARTESIAN_POINT('Ctrl Pts',(-4.04371923700006,2.2,-1.11014865300001));
#315559=CARTESIAN_POINT('Ctrl Pts',(-4.04222767100006,12.2,-1.11021028300001));
#315560=CARTESIAN_POINT('Ctrl Pts',(-4.04222767100006,5.2,-1.11021028300001));
#315561=CARTESIAN_POINT('Ctrl Pts',(-4.04222767100006,2.2,-1.11021028300001));
#315562=CARTESIAN_POINT('Ctrl Pts',(-4.04074075900006,12.2,-1.11026997800002));
#315563=CARTESIAN_POINT('Ctrl Pts',(-4.04074075900006,5.2,-1.11026997800002));
#315564=CARTESIAN_POINT('Ctrl Pts',(-4.04074075900006,2.2,-1.11026997800002));
#315565=CARTESIAN_POINT('Ctrl Pts',(-4.03925851300006,12.2,-1.11032774700002));
#315566=CARTESIAN_POINT('Ctrl Pts',(-4.03925851300006,5.2,-1.11032774700002));
#315567=CARTESIAN_POINT('Ctrl Pts',(-4.03925851300006,2.2,-1.11032774700002));
#315568=CARTESIAN_POINT('Ctrl Pts',(-4.03778093900006,12.2,-1.11038360000002));
#315569=CARTESIAN_POINT('Ctrl Pts',(-4.03778093900006,5.2,-1.11038360000002));
#315570=CARTESIAN_POINT('Ctrl Pts',(-4.03778093900006,2.2,-1.11038360000002));
#315571=CARTESIAN_POINT('Ctrl Pts',(-4.03630804900006,12.2,-1.11043754800002));
#315572=CARTESIAN_POINT('Ctrl Pts',(-4.03630804900006,5.2,-1.11043754800002));
#315573=CARTESIAN_POINT('Ctrl Pts',(-4.03630804900006,2.2,-1.11043754800002));
#315574=CARTESIAN_POINT('Ctrl Pts',(-4.03483985100006,12.2,-1.11048960100002));
#315575=CARTESIAN_POINT('Ctrl Pts',(-4.03483985100006,5.2,-1.11048960100002));
#315576=CARTESIAN_POINT('Ctrl Pts',(-4.03483985100006,2.2,-1.11048960100002));
#315577=CARTESIAN_POINT('Ctrl Pts',(-4.03337635300006,12.2,-1.11053976900001));
#315578=CARTESIAN_POINT('Ctrl Pts',(-4.03337635300006,5.2,-1.11053976900001));
#315579=CARTESIAN_POINT('Ctrl Pts',(-4.03337635300006,2.2,-1.11053976900001));
#315580=CARTESIAN_POINT('Ctrl Pts',(-4.03191756600005,12.2,-1.11058806100001));
#315581=CARTESIAN_POINT('Ctrl Pts',(-4.03191756600005,5.2,-1.11058806100001));
#315582=CARTESIAN_POINT('Ctrl Pts',(-4.03191756600005,2.2,-1.11058806100001));
#315583=CARTESIAN_POINT('Ctrl Pts',(-4.03046349700006,12.2,-1.11063448800001));
#315584=CARTESIAN_POINT('Ctrl Pts',(-4.03046349700006,5.2,-1.11063448800001));
#315585=CARTESIAN_POINT('Ctrl Pts',(-4.03046349700006,2.2,-1.11063448800001));
#315586=CARTESIAN_POINT('Ctrl Pts',(-4.02901415800006,12.2,-1.11067905900001));
#315587=CARTESIAN_POINT('Ctrl Pts',(-4.02901415800006,5.2,-1.11067905900001));
#315588=CARTESIAN_POINT('Ctrl Pts',(-4.02901415800006,2.2,-1.11067905900001));
#315589=CARTESIAN_POINT('Ctrl Pts',(-4.02756955500006,12.2,-1.11072178500002));
#315590=CARTESIAN_POINT('Ctrl Pts',(-4.02756955500006,5.2,-1.11072178500002));
#315591=CARTESIAN_POINT('Ctrl Pts',(-4.02756955500006,2.2,-1.11072178500002));
#315592=CARTESIAN_POINT('Ctrl Pts',(-4.02612970000006,12.2,-1.11076267600001));
#315593=CARTESIAN_POINT('Ctrl Pts',(-4.02612970000006,5.2,-1.11076267600001));
#315594=CARTESIAN_POINT('Ctrl Pts',(-4.02612970000006,2.2,-1.11076267600001));
#315595=CARTESIAN_POINT('Ctrl Pts',(-4.02469460000006,12.2,-1.11080174300001));
#315596=CARTESIAN_POINT('Ctrl Pts',(-4.02469460000006,5.2,-1.11080174300001));
#315597=CARTESIAN_POINT('Ctrl Pts',(-4.02469460000006,2.2,-1.11080174300001));
#315598=CARTESIAN_POINT('Ctrl Pts',(-4.02326426600006,12.2,-1.11083899500001));
#315599=CARTESIAN_POINT('Ctrl Pts',(-4.02326426600006,5.2,-1.11083899500001));
#315600=CARTESIAN_POINT('Ctrl Pts',(-4.02326426600006,2.2,-1.11083899500001));
#315601=CARTESIAN_POINT('Ctrl Pts',(-4.02183870500005,12.2,-1.11087444200002));
#315602=CARTESIAN_POINT('Ctrl Pts',(-4.02183870500005,5.2,-1.11087444200002));
#315603=CARTESIAN_POINT('Ctrl Pts',(-4.02183870500005,2.2,-1.11087444200002));
#315604=CARTESIAN_POINT('Ctrl Pts',(-4.02041792900006,12.2,-1.11090809600002));
#315605=CARTESIAN_POINT('Ctrl Pts',(-4.02041792900006,5.2,-1.11090809600002));
#315606=CARTESIAN_POINT('Ctrl Pts',(-4.02041792900006,2.2,-1.11090809600002));
#315607=CARTESIAN_POINT('Ctrl Pts',(-4.01900194400006,12.2,-1.11093996500002));
#315608=CARTESIAN_POINT('Ctrl Pts',(-4.01900194400006,5.2,-1.11093996500002));
#315609=CARTESIAN_POINT('Ctrl Pts',(-4.01900194400006,2.2,-1.11093996500002));
#315610=CARTESIAN_POINT('Ctrl Pts',(-4.01759076100006,12.2,-1.11097006100001));
#315611=CARTESIAN_POINT('Ctrl Pts',(-4.01759076100006,5.2,-1.11097006100001));
#315612=CARTESIAN_POINT('Ctrl Pts',(-4.01759076100006,2.2,-1.11097006100001));
#315613=CARTESIAN_POINT('Ctrl Pts',(-4.01618439000006,12.2,-1.11099839500001));
#315614=CARTESIAN_POINT('Ctrl Pts',(-4.01618439000006,5.2,-1.11099839500001));
#315615=CARTESIAN_POINT('Ctrl Pts',(-4.01618439000006,2.2,-1.11099839500001));
#315616=CARTESIAN_POINT('Ctrl Pts',(-4.01478283800006,12.2,-1.11102497500001));
#315617=CARTESIAN_POINT('Ctrl Pts',(-4.01478283800006,5.2,-1.11102497500001));
#315618=CARTESIAN_POINT('Ctrl Pts',(-4.01478283800006,2.2,-1.11102497500001));
#315619=CARTESIAN_POINT('Ctrl Pts',(-4.01338611600006,12.2,-1.11104981400001));
#315620=CARTESIAN_POINT('Ctrl Pts',(-4.01338611600006,5.2,-1.11104981400001));
#315621=CARTESIAN_POINT('Ctrl Pts',(-4.01338611600006,2.2,-1.11104981400001));
#315622=CARTESIAN_POINT('Ctrl Pts',(-4.01199423300006,12.2,-1.11107292100002));
#315623=CARTESIAN_POINT('Ctrl Pts',(-4.01199423300006,5.2,-1.11107292100002));
#315624=CARTESIAN_POINT('Ctrl Pts',(-4.01199423300006,2.2,-1.11107292100002));
#315625=CARTESIAN_POINT('Ctrl Pts',(-4.01060719700006,12.2,-1.11109430700001));
#315626=CARTESIAN_POINT('Ctrl Pts',(-4.01060719700006,5.2,-1.11109430700001));
#315627=CARTESIAN_POINT('Ctrl Pts',(-4.01060719700006,2.2,-1.11109430700001));
#315628=CARTESIAN_POINT('Ctrl Pts',(-4.00922501800006,12.2,-1.11111398200002));
#315629=CARTESIAN_POINT('Ctrl Pts',(-4.00922501800006,5.2,-1.11111398200002));
#315630=CARTESIAN_POINT('Ctrl Pts',(-4.00922501800006,2.2,-1.11111398200002));
#315631=CARTESIAN_POINT('Ctrl Pts',(-4.00784770600006,12.2,-1.11113195800002));
#315632=CARTESIAN_POINT('Ctrl Pts',(-4.00784770600006,5.2,-1.11113195800002));
#315633=CARTESIAN_POINT('Ctrl Pts',(-4.00784770600006,2.2,-1.11113195800002));
#315634=CARTESIAN_POINT('Ctrl Pts',(-4.00647526900006,12.2,-1.11114824400001));
#315635=CARTESIAN_POINT('Ctrl Pts',(-4.00647526900006,5.2,-1.11114824400001));
#315636=CARTESIAN_POINT('Ctrl Pts',(-4.00647526900006,2.2,-1.11114824400001));
#315637=CARTESIAN_POINT('Ctrl Pts',(-4.00510771600006,12.2,-1.11116285100001));
#315638=CARTESIAN_POINT('Ctrl Pts',(-4.00510771600006,5.2,-1.11116285100001));
#315639=CARTESIAN_POINT('Ctrl Pts',(-4.00510771600006,2.2,-1.11116285100001));
#315640=CARTESIAN_POINT('Ctrl Pts',(-4.00374505900006,12.2,-1.11117579000001));
#315641=CARTESIAN_POINT('Ctrl Pts',(-4.00374505900006,5.2,-1.11117579000001));
#315642=CARTESIAN_POINT('Ctrl Pts',(-4.00374505900006,2.2,-1.11117579000001));
#315643=CARTESIAN_POINT('Ctrl Pts',(-4.00238730300006,12.2,-1.11118707300002));
#315644=CARTESIAN_POINT('Ctrl Pts',(-4.00238730300006,5.2,-1.11118707300002));
#315645=CARTESIAN_POINT('Ctrl Pts',(-4.00238730300006,2.2,-1.11118707300002));
#315646=CARTESIAN_POINT('Ctrl Pts',(-4.00103446000006,12.2,-1.11119670800001));
#315647=CARTESIAN_POINT('Ctrl Pts',(-4.00103446000006,5.2,-1.11119670800001));
#315648=CARTESIAN_POINT('Ctrl Pts',(-4.00103446000006,2.2,-1.11119670800001));
#315649=CARTESIAN_POINT('Ctrl Pts',(-3.99968653900006,12.2,-1.11120470900001));
#315650=CARTESIAN_POINT('Ctrl Pts',(-3.99968653900006,5.2,-1.11120470900001));
#315651=CARTESIAN_POINT('Ctrl Pts',(-3.99968653900006,2.2,-1.11120470900001));
#315652=CARTESIAN_POINT('Ctrl Pts',(-3.99834355000006,12.2,-1.11121108400001));
#315653=CARTESIAN_POINT('Ctrl Pts',(-3.99834355000006,5.2,-1.11121108400001));
#315654=CARTESIAN_POINT('Ctrl Pts',(-3.99834355000006,2.2,-1.11121108400001));
#315655=CARTESIAN_POINT('Ctrl Pts',(-3.99700550100006,12.2,-1.11121584600001));
#315656=CARTESIAN_POINT('Ctrl Pts',(-3.99700550100006,5.2,-1.11121584600001));
#315657=CARTESIAN_POINT('Ctrl Pts',(-3.99700550100006,2.2,-1.11121584600001));
#315658=CARTESIAN_POINT('Ctrl Pts',(-3.99567240100006,12.2,-1.11121900500001));
#315659=CARTESIAN_POINT('Ctrl Pts',(-3.99567240100006,5.2,-1.11121900500001));
#315660=CARTESIAN_POINT('Ctrl Pts',(-3.99567240100006,2.2,-1.11121900500001));
#315661=CARTESIAN_POINT('Ctrl Pts',(-3.99434425900006,12.2,-1.11122057100001));
#315662=CARTESIAN_POINT('Ctrl Pts',(-3.99434425900006,5.2,-1.11122057100001));
#315663=CARTESIAN_POINT('Ctrl Pts',(-3.99434425900006,2.2,-1.11122057100001));
#315664=CARTESIAN_POINT('Ctrl Pts',(-3.99302108600006,12.2,-1.11122055600001));
#315665=CARTESIAN_POINT('Ctrl Pts',(-3.99302108600006,5.2,-1.11122055600001));
#315666=CARTESIAN_POINT('Ctrl Pts',(-3.99302108600006,2.2,-1.11122055600001));
#315667=CARTESIAN_POINT('Ctrl Pts',(-3.99170289000006,12.2,-1.11121897100002));
#315668=CARTESIAN_POINT('Ctrl Pts',(-3.99170289000006,5.2,-1.11121897100002));
#315669=CARTESIAN_POINT('Ctrl Pts',(-3.99170289000006,2.2,-1.11121897100002));
#315670=CARTESIAN_POINT('Ctrl Pts',(-3.99038968100006,12.2,-1.11121582800001));
#315671=CARTESIAN_POINT('Ctrl Pts',(-3.99038968100006,5.2,-1.11121582800001));
#315672=CARTESIAN_POINT('Ctrl Pts',(-3.99038968100006,2.2,-1.11121582800001));
#315673=CARTESIAN_POINT('Ctrl Pts',(-3.98908146900006,12.2,-1.11121113600001));
#315674=CARTESIAN_POINT('Ctrl Pts',(-3.98908146900006,5.2,-1.11121113600001));
#315675=CARTESIAN_POINT('Ctrl Pts',(-3.98908146900006,2.2,-1.11121113600001));
#315676=CARTESIAN_POINT('Ctrl Pts',(-3.98777826100006,12.2,-1.11120490800001));
#315677=CARTESIAN_POINT('Ctrl Pts',(-3.98777826100006,5.2,-1.11120490800001));
#315678=CARTESIAN_POINT('Ctrl Pts',(-3.98777826100006,2.2,-1.11120490800001));
#315679=CARTESIAN_POINT('Ctrl Pts',(-3.98648006800006,12.2,-1.11119715400001));
#315680=CARTESIAN_POINT('Ctrl Pts',(-3.98648006800006,5.2,-1.11119715400001));
#315681=CARTESIAN_POINT('Ctrl Pts',(-3.98648006800006,2.2,-1.11119715400001));
#315682=CARTESIAN_POINT('Ctrl Pts',(-3.98518690000006,12.2,-1.11118788500002));
#315683=CARTESIAN_POINT('Ctrl Pts',(-3.98518690000006,5.2,-1.11118788500002));
#315684=CARTESIAN_POINT('Ctrl Pts',(-3.98518690000006,2.2,-1.11118788500002));
#315685=CARTESIAN_POINT('Ctrl Pts',(-3.98389876500006,12.2,-1.11117711500002));
#315686=CARTESIAN_POINT('Ctrl Pts',(-3.98389876500006,5.2,-1.11117711500002));
#315687=CARTESIAN_POINT('Ctrl Pts',(-3.98389876500006,2.2,-1.11117711500002));
#315688=CARTESIAN_POINT('Ctrl Pts',(-3.98261567100006,12.2,-1.11116485000001));
#315689=CARTESIAN_POINT('Ctrl Pts',(-3.98261567100006,5.2,-1.11116485000001));
#315690=CARTESIAN_POINT('Ctrl Pts',(-3.98261567100006,2.2,-1.11116485000001));
#315691=CARTESIAN_POINT('Ctrl Pts',(-3.98133763100006,12.2,-1.11115110700001));
#315692=CARTESIAN_POINT('Ctrl Pts',(-3.98133763100006,5.2,-1.11115110700001));
#315693=CARTESIAN_POINT('Ctrl Pts',(-3.98133763100006,2.2,-1.11115110700001));
#315694=CARTESIAN_POINT('Ctrl Pts',(-3.98006465200006,12.2,-1.11113589400002));
#315695=CARTESIAN_POINT('Ctrl Pts',(-3.98006465200006,5.2,-1.11113589400002));
#315696=CARTESIAN_POINT('Ctrl Pts',(-3.98006465200006,2.2,-1.11113589400002));
#315697=CARTESIAN_POINT('Ctrl Pts',(-3.97879674300006,12.2,-1.11111922300001));
#315698=CARTESIAN_POINT('Ctrl Pts',(-3.97879674300006,5.2,-1.11111922300001));
#315699=CARTESIAN_POINT('Ctrl Pts',(-3.97879674300006,2.2,-1.11111922300001));
#315700=CARTESIAN_POINT('Ctrl Pts',(-3.97753391400006,12.2,-1.11110110600002));
#315701=CARTESIAN_POINT('Ctrl Pts',(-3.97753391400006,5.2,-1.11110110600002));
#315702=CARTESIAN_POINT('Ctrl Pts',(-3.97753391400006,2.2,-1.11110110600002));
#315703=CARTESIAN_POINT('Ctrl Pts',(-3.97627617500006,12.2,-1.11108155300002));
#315704=CARTESIAN_POINT('Ctrl Pts',(-3.97627617500006,5.2,-1.11108155300002));
#315705=CARTESIAN_POINT('Ctrl Pts',(-3.97627617500006,2.2,-1.11108155300002));
#315706=CARTESIAN_POINT('Ctrl Pts',(-3.97502353500006,12.2,-1.11106057800002));
#315707=CARTESIAN_POINT('Ctrl Pts',(-3.97502353500006,5.2,-1.11106057800002));
#315708=CARTESIAN_POINT('Ctrl Pts',(-3.97502353500006,2.2,-1.11106057800002));
#315709=CARTESIAN_POINT('Ctrl Pts',(-3.97377600200006,12.2,-1.11103819100002));
#315710=CARTESIAN_POINT('Ctrl Pts',(-3.97377600200006,5.2,-1.11103819100002));
#315711=CARTESIAN_POINT('Ctrl Pts',(-3.97377600200006,2.2,-1.11103819100002));
#315712=CARTESIAN_POINT('Ctrl Pts',(-3.97253358800006,12.2,-1.11101440300001));
#315713=CARTESIAN_POINT('Ctrl Pts',(-3.97253358800006,5.2,-1.11101440300001));
#315714=CARTESIAN_POINT('Ctrl Pts',(-3.97253358800006,2.2,-1.11101440300001));
#315715=CARTESIAN_POINT('Ctrl Pts',(-3.97129630100006,12.2,-1.11098922600001));
#315716=CARTESIAN_POINT('Ctrl Pts',(-3.97129630100006,5.2,-1.11098922600001));
#315717=CARTESIAN_POINT('Ctrl Pts',(-3.97129630100006,2.2,-1.11098922600001));
#315718=CARTESIAN_POINT('Ctrl Pts',(-3.97006415000006,12.2,-1.11096267300002));
#315719=CARTESIAN_POINT('Ctrl Pts',(-3.97006415000006,5.2,-1.11096267300002));
#315720=CARTESIAN_POINT('Ctrl Pts',(-3.97006415000006,2.2,-1.11096267300002));
#315721=CARTESIAN_POINT('Ctrl Pts',(-3.96883714400006,12.2,-1.11093475400001));
#315722=CARTESIAN_POINT('Ctrl Pts',(-3.96883714400006,5.2,-1.11093475400001));
#315723=CARTESIAN_POINT('Ctrl Pts',(-3.96883714400006,2.2,-1.11093475400001));
#315724=CARTESIAN_POINT('Ctrl Pts',(-3.96761529400006,12.2,-1.11090548200002));
#315725=CARTESIAN_POINT('Ctrl Pts',(-3.96761529400006,5.2,-1.11090548200002));
#315726=CARTESIAN_POINT('Ctrl Pts',(-3.96761529400006,2.2,-1.11090548200002));
#315727=CARTESIAN_POINT('Ctrl Pts',(-3.96639860800006,12.2,-1.11087486800002));
#315728=CARTESIAN_POINT('Ctrl Pts',(-3.96639860800006,5.2,-1.11087486800002));
#315729=CARTESIAN_POINT('Ctrl Pts',(-3.96639860800006,2.2,-1.11087486800002));
#315730=CARTESIAN_POINT('Ctrl Pts',(-3.96518709600006,12.2,-1.11084292400002));
#315731=CARTESIAN_POINT('Ctrl Pts',(-3.96518709600006,5.2,-1.11084292400002));
#315732=CARTESIAN_POINT('Ctrl Pts',(-3.96518709600006,2.2,-1.11084292400002));
#315733=CARTESIAN_POINT('Ctrl Pts',(-3.96398076800006,12.2,-1.11080966100001));
#315734=CARTESIAN_POINT('Ctrl Pts',(-3.96398076800006,5.2,-1.11080966100001));
#315735=CARTESIAN_POINT('Ctrl Pts',(-3.96398076800006,2.2,-1.11080966100001));
#315736=CARTESIAN_POINT('Ctrl Pts',(-3.96277963300006,12.2,-1.11077509300001));
#315737=CARTESIAN_POINT('Ctrl Pts',(-3.96277963300006,5.2,-1.11077509300001));
#315738=CARTESIAN_POINT('Ctrl Pts',(-3.96277963300006,2.2,-1.11077509300001));
#315739=CARTESIAN_POINT('Ctrl Pts',(-3.96158370000006,12.2,-1.11073923000002));
#315740=CARTESIAN_POINT('Ctrl Pts',(-3.96158370000006,5.2,-1.11073923000002));
#315741=CARTESIAN_POINT('Ctrl Pts',(-3.96158370000006,2.2,-1.11073923000002));
#315742=CARTESIAN_POINT('Ctrl Pts',(-3.96039297900006,12.2,-1.11070208500001));
#315743=CARTESIAN_POINT('Ctrl Pts',(-3.96039297900006,5.2,-1.11070208500001));
#315744=CARTESIAN_POINT('Ctrl Pts',(-3.96039297900006,2.2,-1.11070208500001));
#315745=CARTESIAN_POINT('Ctrl Pts',(-3.95920747900006,12.2,-1.11066367000001));
#315746=CARTESIAN_POINT('Ctrl Pts',(-3.95920747900006,5.2,-1.11066367000001));
#315747=CARTESIAN_POINT('Ctrl Pts',(-3.95920747900006,2.2,-1.11066367000001));
#315748=CARTESIAN_POINT('Ctrl Pts',(-3.95802721000006,12.2,-1.11062399600002));
#315749=CARTESIAN_POINT('Ctrl Pts',(-3.95802721000006,5.2,-1.11062399600002));
#315750=CARTESIAN_POINT('Ctrl Pts',(-3.95802721000006,2.2,-1.11062399600002));
#315751=CARTESIAN_POINT('Ctrl Pts',(-3.95685218100006,12.2,-1.11058307600001));
#315752=CARTESIAN_POINT('Ctrl Pts',(-3.95685218100006,5.2,-1.11058307600001));
#315753=CARTESIAN_POINT('Ctrl Pts',(-3.95685218100006,2.2,-1.11058307600001));
#315754=CARTESIAN_POINT('Ctrl Pts',(-3.95568240100006,12.2,-1.11054092200002));
#315755=CARTESIAN_POINT('Ctrl Pts',(-3.95568240100006,5.2,-1.11054092200002));
#315756=CARTESIAN_POINT('Ctrl Pts',(-3.95568240100006,2.2,-1.11054092200002));
#315757=CARTESIAN_POINT('Ctrl Pts',(-3.95451788100006,12.2,-1.11049754700002));
#315758=CARTESIAN_POINT('Ctrl Pts',(-3.95451788100006,5.2,-1.11049754700002));
#315759=CARTESIAN_POINT('Ctrl Pts',(-3.95451788100006,2.2,-1.11049754700002));
#315760=CARTESIAN_POINT('Ctrl Pts',(-3.95335862900006,12.2,-1.11045296100002));
#315761=CARTESIAN_POINT('Ctrl Pts',(-3.95335862900006,5.2,-1.11045296100002));
#315762=CARTESIAN_POINT('Ctrl Pts',(-3.95335862900006,2.2,-1.11045296100002));
#315763=CARTESIAN_POINT('Ctrl Pts',(-3.95220465600006,12.2,-1.11040717800002));
#315764=CARTESIAN_POINT('Ctrl Pts',(-3.95220465600006,5.2,-1.11040717800002));
#315765=CARTESIAN_POINT('Ctrl Pts',(-3.95220465600006,2.2,-1.11040717800002));
#315766=CARTESIAN_POINT('Ctrl Pts',(-3.95105597100006,12.2,-1.11036021000002));
#315767=CARTESIAN_POINT('Ctrl Pts',(-3.95105597100006,5.2,-1.11036021000002));
#315768=CARTESIAN_POINT('Ctrl Pts',(-3.95105597100006,2.2,-1.11036021000002));
#315769=CARTESIAN_POINT('Ctrl Pts',(-3.94991258100006,12.2,-1.11031207000002));
#315770=CARTESIAN_POINT('Ctrl Pts',(-3.94991258100006,5.2,-1.11031207000002));
#315771=CARTESIAN_POINT('Ctrl Pts',(-3.94991258100006,2.2,-1.11031207000002));
#315772=CARTESIAN_POINT('Ctrl Pts',(-3.94877449900005,12.2,-1.11026276800001));
#315773=CARTESIAN_POINT('Ctrl Pts',(-3.94877449900005,5.2,-1.11026276800001));
#315774=CARTESIAN_POINT('Ctrl Pts',(-3.94877449900005,2.2,-1.11026276800001));
#315775=CARTESIAN_POINT('Ctrl Pts',(-3.94764173200006,12.2,-1.11021232000001));
#315776=CARTESIAN_POINT('Ctrl Pts',(-3.94764173200006,5.2,-1.11021232000001));
#315777=CARTESIAN_POINT('Ctrl Pts',(-3.94764173200006,2.2,-1.11021232000001));
#315778=CARTESIAN_POINT('Ctrl Pts',(-3.94651429200006,12.2,-1.11016073500001));
#315779=CARTESIAN_POINT('Ctrl Pts',(-3.94651429200006,5.2,-1.11016073500001));
#315780=CARTESIAN_POINT('Ctrl Pts',(-3.94651429200006,2.2,-1.11016073500001));
#315781=CARTESIAN_POINT('Ctrl Pts',(-3.94539218700006,12.2,-1.11010802800001));
#315782=CARTESIAN_POINT('Ctrl Pts',(-3.94539218700006,5.2,-1.11010802800001));
#315783=CARTESIAN_POINT('Ctrl Pts',(-3.94539218700006,2.2,-1.11010802800001));
#315784=CARTESIAN_POINT('Ctrl Pts',(-3.94427542600006,12.2,-1.11005421000002));
#315785=CARTESIAN_POINT('Ctrl Pts',(-3.94427542600006,5.2,-1.11005421000002));
#315786=CARTESIAN_POINT('Ctrl Pts',(-3.94427542600006,2.2,-1.11005421000002));
#315787=CARTESIAN_POINT('Ctrl Pts',(-3.94316401900006,12.2,-1.10999929400001));
#315788=CARTESIAN_POINT('Ctrl Pts',(-3.94316401900006,5.2,-1.10999929400001));
#315789=CARTESIAN_POINT('Ctrl Pts',(-3.94316401900006,2.2,-1.10999929400001));
#315790=CARTESIAN_POINT('Ctrl Pts',(-3.94205797700006,12.2,-1.10994329300001));
#315791=CARTESIAN_POINT('Ctrl Pts',(-3.94205797700006,5.2,-1.10994329300001));
#315792=CARTESIAN_POINT('Ctrl Pts',(-3.94205797700006,2.2,-1.10994329300001));
#315793=CARTESIAN_POINT('Ctrl Pts',(-3.94095730800006,12.2,-1.10988622000002));
#315794=CARTESIAN_POINT('Ctrl Pts',(-3.94095730800006,5.2,-1.10988622000002));
#315795=CARTESIAN_POINT('Ctrl Pts',(-3.94095730800006,2.2,-1.10988622000002));
#315796=CARTESIAN_POINT('Ctrl Pts',(-3.93986202200006,12.2,-1.10982808600002));
#315797=CARTESIAN_POINT('Ctrl Pts',(-3.93986202200006,5.2,-1.10982808600002));
#315798=CARTESIAN_POINT('Ctrl Pts',(-3.93986202200006,2.2,-1.10982808600002));
#315799=CARTESIAN_POINT('Ctrl Pts',(-3.93877212800006,12.2,-1.10976890700002));
#315800=CARTESIAN_POINT('Ctrl Pts',(-3.93877212800006,5.2,-1.10976890700002));
#315801=CARTESIAN_POINT('Ctrl Pts',(-3.93877212800006,2.2,-1.10976890700002));
#315802=CARTESIAN_POINT('Ctrl Pts',(-3.93768763600006,12.2,-1.10970869100001));
#315803=CARTESIAN_POINT('Ctrl Pts',(-3.93768763600006,5.2,-1.10970869100001));
#315804=CARTESIAN_POINT('Ctrl Pts',(-3.93768763600006,2.2,-1.10970869100001));
#315805=CARTESIAN_POINT('Ctrl Pts',(-3.93660855600006,12.2,-1.10964745600001));
#315806=CARTESIAN_POINT('Ctrl Pts',(-3.93660855600006,5.2,-1.10964745600001));
#315807=CARTESIAN_POINT('Ctrl Pts',(-3.93660855600006,2.2,-1.10964745600001));
#315808=CARTESIAN_POINT('Ctrl Pts',(-3.93553489700006,12.2,-1.10958521100001));
#315809=CARTESIAN_POINT('Ctrl Pts',(-3.93553489700006,5.2,-1.10958521100001));
#315810=CARTESIAN_POINT('Ctrl Pts',(-3.93553489700006,2.2,-1.10958521100001));
#315811=CARTESIAN_POINT('Ctrl Pts',(-3.93446666900005,12.2,-1.10952197100001));
#315812=CARTESIAN_POINT('Ctrl Pts',(-3.93446666900005,5.2,-1.10952197100001));
#315813=CARTESIAN_POINT('Ctrl Pts',(-3.93446666900005,2.2,-1.10952197100001));
#315814=CARTESIAN_POINT('Ctrl Pts',(-3.93340388200006,12.2,-1.10945774800001));
#315815=CARTESIAN_POINT('Ctrl Pts',(-3.93340388200006,5.2,-1.10945774800001));
#315816=CARTESIAN_POINT('Ctrl Pts',(-3.93340388200006,2.2,-1.10945774800001));
#315817=CARTESIAN_POINT('Ctrl Pts',(-3.93234654400006,12.2,-1.10939255600002));
#315818=CARTESIAN_POINT('Ctrl Pts',(-3.93234654400006,5.2,-1.10939255600002));
#315819=CARTESIAN_POINT('Ctrl Pts',(-3.93234654400006,2.2,-1.10939255600002));
#315820=CARTESIAN_POINT('Ctrl Pts',(-3.93129466700006,12.2,-1.10932640700002));
#315821=CARTESIAN_POINT('Ctrl Pts',(-3.93129466700006,5.2,-1.10932640700002));
#315822=CARTESIAN_POINT('Ctrl Pts',(-3.93129466700006,2.2,-1.10932640700002));
#315823=CARTESIAN_POINT('Ctrl Pts',(-3.93024825700006,12.2,-1.10925931500002));
#315824=CARTESIAN_POINT('Ctrl Pts',(-3.93024825700006,5.2,-1.10925931500002));
#315825=CARTESIAN_POINT('Ctrl Pts',(-3.93024825700006,2.2,-1.10925931500002));
#315826=CARTESIAN_POINT('Ctrl Pts',(-3.92920732800006,12.2,-1.10919129200001));
#315827=CARTESIAN_POINT('Ctrl Pts',(-3.92920732800006,5.2,-1.10919129200001));
#315828=CARTESIAN_POINT('Ctrl Pts',(-3.92920732800006,2.2,-1.10919129200001));
#315829=CARTESIAN_POINT('Ctrl Pts',(-3.92817188800006,12.2,-1.10912235300002));
#315830=CARTESIAN_POINT('Ctrl Pts',(-3.92817188800006,5.2,-1.10912235300002));
#315831=CARTESIAN_POINT('Ctrl Pts',(-3.92817188800006,2.2,-1.10912235300002));
#315832=CARTESIAN_POINT('Ctrl Pts',(-3.92714194400006,12.2,-1.10905250900001));
#315833=CARTESIAN_POINT('Ctrl Pts',(-3.92714194400006,5.2,-1.10905250900001));
#315834=CARTESIAN_POINT('Ctrl Pts',(-3.92714194400006,2.2,-1.10905250900001));
#315835=CARTESIAN_POINT('Ctrl Pts',(-3.92611750900006,12.2,-1.10898177600002));
#315836=CARTESIAN_POINT('Ctrl Pts',(-3.92611750900006,5.2,-1.10898177600002));
#315837=CARTESIAN_POINT('Ctrl Pts',(-3.92611750900006,2.2,-1.10898177600002));
#315838=CARTESIAN_POINT('Ctrl Pts',(-3.92509859200006,12.2,-1.10891016400001));
#315839=CARTESIAN_POINT('Ctrl Pts',(-3.92509859200006,5.2,-1.10891016400001));
#315840=CARTESIAN_POINT('Ctrl Pts',(-3.92509859200006,2.2,-1.10891016400001));
#315841=CARTESIAN_POINT('Ctrl Pts',(-3.92408520200005,12.2,-1.10883769000001));
#315842=CARTESIAN_POINT('Ctrl Pts',(-3.92408520200005,5.2,-1.10883769000001));
#315843=CARTESIAN_POINT('Ctrl Pts',(-3.92408520200005,2.2,-1.10883769000001));
#315844=CARTESIAN_POINT('Ctrl Pts',(-3.92307734900006,12.2,-1.10876436500002));
#315845=CARTESIAN_POINT('Ctrl Pts',(-3.92307734900006,5.2,-1.10876436500002));
#315846=CARTESIAN_POINT('Ctrl Pts',(-3.92307734900006,2.2,-1.10876436500002));
#315847=CARTESIAN_POINT('Ctrl Pts',(-3.92207504200006,12.2,-1.10869020300001));
#315848=CARTESIAN_POINT('Ctrl Pts',(-3.92207504200006,5.2,-1.10869020300001));
#315849=CARTESIAN_POINT('Ctrl Pts',(-3.92207504200006,2.2,-1.10869020300001));
#315850=CARTESIAN_POINT('Ctrl Pts',(-3.92107829200006,12.2,-1.10861521800001));
#315851=CARTESIAN_POINT('Ctrl Pts',(-3.92107829200006,5.2,-1.10861521800001));
#315852=CARTESIAN_POINT('Ctrl Pts',(-3.92107829200006,2.2,-1.10861521800001));
#315853=CARTESIAN_POINT('Ctrl Pts',(-3.92008710600006,12.2,-1.10853942300002));
#315854=CARTESIAN_POINT('Ctrl Pts',(-3.92008710600006,5.2,-1.10853942300002));
#315855=CARTESIAN_POINT('Ctrl Pts',(-3.92008710600006,2.2,-1.10853942300002));
#315856=CARTESIAN_POINT('Ctrl Pts',(-3.91910149800006,12.2,-1.10846283100001));
#315857=CARTESIAN_POINT('Ctrl Pts',(-3.91910149800006,5.2,-1.10846283100001));
#315858=CARTESIAN_POINT('Ctrl Pts',(-3.91910149800006,2.2,-1.10846283100001));
#315859=CARTESIAN_POINT('Ctrl Pts',(-3.91812147400006,12.2,-1.10838545800001));
#315860=CARTESIAN_POINT('Ctrl Pts',(-3.91812147400006,5.2,-1.10838545800001));
#315861=CARTESIAN_POINT('Ctrl Pts',(-3.91812147400006,2.2,-1.10838545800001));
#315862=CARTESIAN_POINT('Ctrl Pts',(-3.91714704600005,12.2,-1.10830731500001));
#315863=CARTESIAN_POINT('Ctrl Pts',(-3.91714704600005,5.2,-1.10830731500001));
#315864=CARTESIAN_POINT('Ctrl Pts',(-3.91714704600005,2.2,-1.10830731500001));
#315865=CARTESIAN_POINT('Ctrl Pts',(-3.91617822200006,12.2,-1.10822841700001));
#315866=CARTESIAN_POINT('Ctrl Pts',(-3.91617822200006,5.2,-1.10822841700001));
#315867=CARTESIAN_POINT('Ctrl Pts',(-3.91617822200006,2.2,-1.10822841700001));
#315868=CARTESIAN_POINT('Ctrl Pts',(-3.91521501300006,12.2,-1.10814877800001));
#315869=CARTESIAN_POINT('Ctrl Pts',(-3.91521501300006,5.2,-1.10814877800001));
#315870=CARTESIAN_POINT('Ctrl Pts',(-3.91521501300006,2.2,-1.10814877800001));
#315871=CARTESIAN_POINT('Ctrl Pts',(-3.91425742800006,12.2,-1.10806841200001));
#315872=CARTESIAN_POINT('Ctrl Pts',(-3.91425742800006,5.2,-1.10806841200001));
#315873=CARTESIAN_POINT('Ctrl Pts',(-3.91425742800006,2.2,-1.10806841200001));
#315874=CARTESIAN_POINT('Ctrl Pts',(-3.91330547700006,12.2,-1.10798733200001));
#315875=CARTESIAN_POINT('Ctrl Pts',(-3.91330547700006,5.2,-1.10798733200001));
#315876=CARTESIAN_POINT('Ctrl Pts',(-3.91330547700006,2.2,-1.10798733200001));
#315877=CARTESIAN_POINT('Ctrl Pts',(-3.91235917000006,12.2,-1.10790555300001));
#315878=CARTESIAN_POINT('Ctrl Pts',(-3.91235917000006,5.2,-1.10790555300001));
#315879=CARTESIAN_POINT('Ctrl Pts',(-3.91235917000006,2.2,-1.10790555300001));
#315880=CARTESIAN_POINT('Ctrl Pts',(-3.91141851700006,12.2,-1.10782308700001));
#315881=CARTESIAN_POINT('Ctrl Pts',(-3.91141851700006,5.2,-1.10782308700001));
#315882=CARTESIAN_POINT('Ctrl Pts',(-3.91141851700006,2.2,-1.10782308700001));
#315883=CARTESIAN_POINT('Ctrl Pts',(-3.91048352600006,12.2,-1.10773995100002));
#315884=CARTESIAN_POINT('Ctrl Pts',(-3.91048352600006,5.2,-1.10773995100002));
#315885=CARTESIAN_POINT('Ctrl Pts',(-3.91048352600006,2.2,-1.10773995100002));
#315886=CARTESIAN_POINT('Ctrl Pts',(-3.90955420900006,12.2,-1.10765615700001));
#315887=CARTESIAN_POINT('Ctrl Pts',(-3.90955420900006,5.2,-1.10765615700001));
#315888=CARTESIAN_POINT('Ctrl Pts',(-3.90955420900006,2.2,-1.10765615700001));
#315889=CARTESIAN_POINT('Ctrl Pts',(-3.90863057500006,12.2,-1.10757172000001));
#315890=CARTESIAN_POINT('Ctrl Pts',(-3.90863057500006,5.2,-1.10757172000001));
#315891=CARTESIAN_POINT('Ctrl Pts',(-3.90863057500006,2.2,-1.10757172000001));
#315892=CARTESIAN_POINT('Ctrl Pts',(-3.90771263300006,12.2,-1.10748665400001));
#315893=CARTESIAN_POINT('Ctrl Pts',(-3.90771263300006,5.2,-1.10748665400001));
#315894=CARTESIAN_POINT('Ctrl Pts',(-3.90771263300006,2.2,-1.10748665400001));
#315895=CARTESIAN_POINT('Ctrl Pts',(-3.90680039400006,12.2,-1.10740097200001));
#315896=CARTESIAN_POINT('Ctrl Pts',(-3.90680039400006,5.2,-1.10740097200001));
#315897=CARTESIAN_POINT('Ctrl Pts',(-3.90680039400006,2.2,-1.10740097200001));
#315898=CARTESIAN_POINT('Ctrl Pts',(-3.90589386600006,12.2,-1.10731469100001));
#315899=CARTESIAN_POINT('Ctrl Pts',(-3.90589386600006,5.2,-1.10731469100001));
#315900=CARTESIAN_POINT('Ctrl Pts',(-3.90589386600006,2.2,-1.10731469100001));
#315901=CARTESIAN_POINT('Ctrl Pts',(-3.90499306200006,12.2,-1.10722782200002));
#315902=CARTESIAN_POINT('Ctrl Pts',(-3.90499306200006,5.2,-1.10722782200002));
#315903=CARTESIAN_POINT('Ctrl Pts',(-3.90499306200006,2.2,-1.10722782200002));
#315904=CARTESIAN_POINT('Ctrl Pts',(-3.90409798800006,12.2,-1.10714038300001));
#315905=CARTESIAN_POINT('Ctrl Pts',(-3.90409798800006,5.2,-1.10714038300001));
#315906=CARTESIAN_POINT('Ctrl Pts',(-3.90409798800006,2.2,-1.10714038300001));
#315907=CARTESIAN_POINT('Ctrl Pts',(-3.90320865700006,12.2,-1.10705238500001));
#315908=CARTESIAN_POINT('Ctrl Pts',(-3.90320865700006,5.2,-1.10705238500001));
#315909=CARTESIAN_POINT('Ctrl Pts',(-3.90320865700006,2.2,-1.10705238500001));
#315910=CARTESIAN_POINT('Ctrl Pts',(-3.90232507800006,12.2,-1.10696384600002));
#315911=CARTESIAN_POINT('Ctrl Pts',(-3.90232507800006,5.2,-1.10696384600002));
#315912=CARTESIAN_POINT('Ctrl Pts',(-3.90232507800006,2.2,-1.10696384600002));
#315913=CARTESIAN_POINT('Ctrl Pts',(-3.90144726000006,12.2,-1.10687477600001));
#315914=CARTESIAN_POINT('Ctrl Pts',(-3.90144726000006,5.2,-1.10687477600001));
#315915=CARTESIAN_POINT('Ctrl Pts',(-3.90144726000006,2.2,-1.10687477600001));
#315916=CARTESIAN_POINT('Ctrl Pts',(-3.90057521300006,12.2,-1.10678519400001));
#315917=CARTESIAN_POINT('Ctrl Pts',(-3.90057521300006,5.2,-1.10678519400001));
#315918=CARTESIAN_POINT('Ctrl Pts',(-3.90057521300006,2.2,-1.10678519400001));
#315919=CARTESIAN_POINT('Ctrl Pts',(-3.89970894600006,12.2,-1.10669511200001));
#315920=CARTESIAN_POINT('Ctrl Pts',(-3.89970894600006,5.2,-1.10669511200001));
#315921=CARTESIAN_POINT('Ctrl Pts',(-3.89970894600006,2.2,-1.10669511200001));
#315922=CARTESIAN_POINT('Ctrl Pts',(-3.89884847200006,12.2,-1.10660454700001));
#315923=CARTESIAN_POINT('Ctrl Pts',(-3.89884847200006,5.2,-1.10660454700001));
#315924=CARTESIAN_POINT('Ctrl Pts',(-3.89884847200006,2.2,-1.10660454700001));
#315925=CARTESIAN_POINT('Ctrl Pts',(-3.89799379800006,12.2,-1.10651351100001));
#315926=CARTESIAN_POINT('Ctrl Pts',(-3.89799379800006,5.2,-1.10651351100001));
#315927=CARTESIAN_POINT('Ctrl Pts',(-3.89799379800006,2.2,-1.10651351100001));
#315928=CARTESIAN_POINT('Ctrl Pts',(-3.89714493500006,12.2,-1.10642202000002));
#315929=CARTESIAN_POINT('Ctrl Pts',(-3.89714493500006,5.2,-1.10642202000002));
#315930=CARTESIAN_POINT('Ctrl Pts',(-3.89714493500006,2.2,-1.10642202000002));
#315931=CARTESIAN_POINT('Ctrl Pts',(-3.89630189200005,12.2,-1.10633008900002));
#315932=CARTESIAN_POINT('Ctrl Pts',(-3.89630189200005,5.2,-1.10633008900002));
#315933=CARTESIAN_POINT('Ctrl Pts',(-3.89630189200005,2.2,-1.10633008900002));
#315934=CARTESIAN_POINT('Ctrl Pts',(-3.89546468000006,12.2,-1.10623773300001));
#315935=CARTESIAN_POINT('Ctrl Pts',(-3.89546468000006,5.2,-1.10623773300001));
#315936=CARTESIAN_POINT('Ctrl Pts',(-3.89546468000006,2.2,-1.10623773300001));
#315937=CARTESIAN_POINT('Ctrl Pts',(-3.89463330900006,12.2,-1.10614496700002));
#315938=CARTESIAN_POINT('Ctrl Pts',(-3.89463330900006,5.2,-1.10614496700002));
#315939=CARTESIAN_POINT('Ctrl Pts',(-3.89463330900006,2.2,-1.10614496700002));
#315940=CARTESIAN_POINT('Ctrl Pts',(-3.89380778700006,12.2,-1.10605180600002));
#315941=CARTESIAN_POINT('Ctrl Pts',(-3.89380778700006,5.2,-1.10605180600002));
#315942=CARTESIAN_POINT('Ctrl Pts',(-3.89380778700006,2.2,-1.10605180600002));
#315943=CARTESIAN_POINT('Ctrl Pts',(-3.89298812600006,12.2,-1.10595826400001));
#315944=CARTESIAN_POINT('Ctrl Pts',(-3.89298812600006,5.2,-1.10595826400001));
#315945=CARTESIAN_POINT('Ctrl Pts',(-3.89298812600006,2.2,-1.10595826400001));
#315946=CARTESIAN_POINT('Ctrl Pts',(-3.89217433600006,12.2,-1.10586435700001));
#315947=CARTESIAN_POINT('Ctrl Pts',(-3.89217433600006,5.2,-1.10586435700001));
#315948=CARTESIAN_POINT('Ctrl Pts',(-3.89217433600006,2.2,-1.10586435700001));
#315949=CARTESIAN_POINT('Ctrl Pts',(-3.89136642500006,12.2,-1.10577010100001));
#315950=CARTESIAN_POINT('Ctrl Pts',(-3.89136642500006,5.2,-1.10577010100001));
#315951=CARTESIAN_POINT('Ctrl Pts',(-3.89136642500006,2.2,-1.10577010100001));
#315952=CARTESIAN_POINT('Ctrl Pts',(-3.89056440600006,12.2,-1.10567550900001));
#315953=CARTESIAN_POINT('Ctrl Pts',(-3.89056440600006,5.2,-1.10567550900001));
#315954=CARTESIAN_POINT('Ctrl Pts',(-3.89056440600006,2.2,-1.10567550900001));
#315955=CARTESIAN_POINT('Ctrl Pts',(-3.88976828500006,12.2,-1.10558059800002));
#315956=CARTESIAN_POINT('Ctrl Pts',(-3.88976828500006,5.2,-1.10558059800002));
#315957=CARTESIAN_POINT('Ctrl Pts',(-3.88976828500006,2.2,-1.10558059800002));
#315958=CARTESIAN_POINT('Ctrl Pts',(-3.88897807500006,12.2,-1.10548538300002));
#315959=CARTESIAN_POINT('Ctrl Pts',(-3.88897807500006,5.2,-1.10548538300002));
#315960=CARTESIAN_POINT('Ctrl Pts',(-3.88897807500006,2.2,-1.10548538300002));
#315961=CARTESIAN_POINT('Ctrl Pts',(-3.88819378500005,12.2,-1.10538988000001));
#315962=CARTESIAN_POINT('Ctrl Pts',(-3.88819378500005,5.2,-1.10538988000001));
#315963=CARTESIAN_POINT('Ctrl Pts',(-3.88819378500005,2.2,-1.10538988000001));
#315964=CARTESIAN_POINT('Ctrl Pts',(-3.88741542500005,12.2,-1.10529410400002));
#315965=CARTESIAN_POINT('Ctrl Pts',(-3.88741542500005,5.2,-1.10529410400002));
#315966=CARTESIAN_POINT('Ctrl Pts',(-3.88741542500005,2.2,-1.10529410400002));
#315967=CARTESIAN_POINT('Ctrl Pts',(-3.88664300600006,12.2,-1.10519806900002));
#315968=CARTESIAN_POINT('Ctrl Pts',(-3.88664300600006,5.2,-1.10519806900002));
#315969=CARTESIAN_POINT('Ctrl Pts',(-3.88664300600006,2.2,-1.10519806900002));
#315970=CARTESIAN_POINT('Ctrl Pts',(-3.88587653500006,12.2,-1.10510179300002));
#315971=CARTESIAN_POINT('Ctrl Pts',(-3.88587653500006,5.2,-1.10510179300002));
#315972=CARTESIAN_POINT('Ctrl Pts',(-3.88587653500006,2.2,-1.10510179300002));
#315973=CARTESIAN_POINT('Ctrl Pts',(-3.88511602600006,12.2,-1.10500529000001));
#315974=CARTESIAN_POINT('Ctrl Pts',(-3.88511602600006,5.2,-1.10500529000001));
#315975=CARTESIAN_POINT('Ctrl Pts',(-3.88511602600006,2.2,-1.10500529000001));
#315976=CARTESIAN_POINT('Ctrl Pts',(-3.88436148600006,12.2,-1.10490857500002));
#315977=CARTESIAN_POINT('Ctrl Pts',(-3.88436148600006,5.2,-1.10490857500002));
#315978=CARTESIAN_POINT('Ctrl Pts',(-3.88436148600006,2.2,-1.10490857500002));
#315979=CARTESIAN_POINT('Ctrl Pts',(-3.88361292600006,12.2,-1.10481166500001));
#315980=CARTESIAN_POINT('Ctrl Pts',(-3.88361292600006,5.2,-1.10481166500001));
#315981=CARTESIAN_POINT('Ctrl Pts',(-3.88361292600006,2.2,-1.10481166500001));
#315982=CARTESIAN_POINT('Ctrl Pts',(-3.88287035700006,12.2,-1.10471457700001));
#315983=CARTESIAN_POINT('Ctrl Pts',(-3.88287035700006,5.2,-1.10471457700001));
#315984=CARTESIAN_POINT('Ctrl Pts',(-3.88287035700006,2.2,-1.10471457700001));
#315985=CARTESIAN_POINT('Ctrl Pts',(-3.88213378800006,12.2,-1.10461732400001));
#315986=CARTESIAN_POINT('Ctrl Pts',(-3.88213378800006,5.2,-1.10461732400001));
#315987=CARTESIAN_POINT('Ctrl Pts',(-3.88213378800006,2.2,-1.10461732400001));
#315988=CARTESIAN_POINT('Ctrl Pts',(-3.88140322900006,12.2,-1.10451992400002));
#315989=CARTESIAN_POINT('Ctrl Pts',(-3.88140322900006,5.2,-1.10451992400002));
#315990=CARTESIAN_POINT('Ctrl Pts',(-3.88140322900006,2.2,-1.10451992400002));
#315991=CARTESIAN_POINT('Ctrl Pts',(-3.88067869000006,12.2,-1.10442239100002));
#315992=CARTESIAN_POINT('Ctrl Pts',(-3.88067869000006,5.2,-1.10442239100002));
#315993=CARTESIAN_POINT('Ctrl Pts',(-3.88067869000006,2.2,-1.10442239100002));
#315994=CARTESIAN_POINT('Ctrl Pts',(-3.87996018200006,12.2,-1.10432474300001));
#315995=CARTESIAN_POINT('Ctrl Pts',(-3.87996018200006,5.2,-1.10432474300001));
#315996=CARTESIAN_POINT('Ctrl Pts',(-3.87996018200006,2.2,-1.10432474300001));
#315997=CARTESIAN_POINT('Ctrl Pts',(-3.87924771400006,12.2,-1.10422699600001));
#315998=CARTESIAN_POINT('Ctrl Pts',(-3.87924771400006,5.2,-1.10422699600001));
#315999=CARTESIAN_POINT('Ctrl Pts',(-3.87924771400006,2.2,-1.10422699600001));
#316000=CARTESIAN_POINT('Ctrl Pts',(-3.87854129700006,12.2,-1.10412916400001));
#316001=CARTESIAN_POINT('Ctrl Pts',(-3.87854129700006,5.2,-1.10412916400001));
#316002=CARTESIAN_POINT('Ctrl Pts',(-3.87854129700006,2.2,-1.10412916400001));
#316003=CARTESIAN_POINT('Ctrl Pts',(-3.87784093900006,12.2,-1.10403126600001));
#316004=CARTESIAN_POINT('Ctrl Pts',(-3.87784093900006,5.2,-1.10403126600001));
#316005=CARTESIAN_POINT('Ctrl Pts',(-3.87784093900006,2.2,-1.10403126600001));
#316006=CARTESIAN_POINT('Ctrl Pts',(-3.87714665400006,12.2,-1.10393331500001));
#316007=CARTESIAN_POINT('Ctrl Pts',(-3.87714665400006,5.2,-1.10393331500001));
#316008=CARTESIAN_POINT('Ctrl Pts',(-3.87714665400006,2.2,-1.10393331500001));
#316009=CARTESIAN_POINT('Ctrl Pts',(-3.87645844900006,12.2,-1.10383533000002));
#316010=CARTESIAN_POINT('Ctrl Pts',(-3.87645844900006,5.2,-1.10383533000002));
#316011=CARTESIAN_POINT('Ctrl Pts',(-3.87645844900006,2.2,-1.10383533000002));
#316012=CARTESIAN_POINT('Ctrl Pts',(-3.87577633500006,12.2,-1.10373732700001));
#316013=CARTESIAN_POINT('Ctrl Pts',(-3.87577633500006,5.2,-1.10373732700001));
#316014=CARTESIAN_POINT('Ctrl Pts',(-3.87577633500006,2.2,-1.10373732700001));
#316015=CARTESIAN_POINT('Ctrl Pts',(-3.87510032200006,12.2,-1.10363932000002));
#316016=CARTESIAN_POINT('Ctrl Pts',(-3.87510032200006,5.2,-1.10363932000002));
#316017=CARTESIAN_POINT('Ctrl Pts',(-3.87510032200006,2.2,-1.10363932000002));
#316018=CARTESIAN_POINT('Ctrl Pts',(-3.87443042100006,12.2,-1.10354132900001));
#316019=CARTESIAN_POINT('Ctrl Pts',(-3.87443042100006,5.2,-1.10354132900001));
#316020=CARTESIAN_POINT('Ctrl Pts',(-3.87443042100006,2.2,-1.10354132900001));
#316021=CARTESIAN_POINT('Ctrl Pts',(-3.87376664100006,12.2,-1.10344336800001));
#316022=CARTESIAN_POINT('Ctrl Pts',(-3.87376664100006,5.2,-1.10344336800001));
#316023=CARTESIAN_POINT('Ctrl Pts',(-3.87376664100006,2.2,-1.10344336800001));
#316024=CARTESIAN_POINT('Ctrl Pts',(-3.87310899300005,12.2,-1.10334545400002));
#316025=CARTESIAN_POINT('Ctrl Pts',(-3.87310899300005,5.2,-1.10334545400002));
#316026=CARTESIAN_POINT('Ctrl Pts',(-3.87310899300005,2.2,-1.10334545400002));
#316027=CARTESIAN_POINT('Ctrl Pts',(-3.87245748600006,12.2,-1.10324760500002));
#316028=CARTESIAN_POINT('Ctrl Pts',(-3.87245748600006,5.2,-1.10324760500002));
#316029=CARTESIAN_POINT('Ctrl Pts',(-3.87245748600006,2.2,-1.10324760500002));
#316030=CARTESIAN_POINT('Ctrl Pts',(-3.87181213100006,12.2,-1.10314983600002));
#316031=CARTESIAN_POINT('Ctrl Pts',(-3.87181213100006,5.2,-1.10314983600002));
#316032=CARTESIAN_POINT('Ctrl Pts',(-3.87181213100006,2.2,-1.10314983600002));
#316033=CARTESIAN_POINT('Ctrl Pts',(-3.87117293900006,12.2,-1.10305216500001));
#316034=CARTESIAN_POINT('Ctrl Pts',(-3.87117293900006,5.2,-1.10305216500001));
#316035=CARTESIAN_POINT('Ctrl Pts',(-3.87117293900006,2.2,-1.10305216500001));
#316036=CARTESIAN_POINT('Ctrl Pts',(-3.87053991900006,12.2,-1.10295460800002));
#316037=CARTESIAN_POINT('Ctrl Pts',(-3.87053991900006,5.2,-1.10295460800002));
#316038=CARTESIAN_POINT('Ctrl Pts',(-3.87053991900006,2.2,-1.10295460800002));
#316039=CARTESIAN_POINT('Ctrl Pts',(-3.86991308100006,12.2,-1.10285718300001));
#316040=CARTESIAN_POINT('Ctrl Pts',(-3.86991308100006,5.2,-1.10285718300001));
#316041=CARTESIAN_POINT('Ctrl Pts',(-3.86991308100006,2.2,-1.10285718300001));
#316042=CARTESIAN_POINT('Ctrl Pts',(-3.86929243700005,12.2,-1.10275990500002));
#316043=CARTESIAN_POINT('Ctrl Pts',(-3.86929243700005,5.2,-1.10275990500002));
#316044=CARTESIAN_POINT('Ctrl Pts',(-3.86929243700005,2.2,-1.10275990500002));
#316045=CARTESIAN_POINT('Ctrl Pts',(-3.86867799500005,12.2,-1.10266279300001));
#316046=CARTESIAN_POINT('Ctrl Pts',(-3.86867799500005,5.2,-1.10266279300001));
#316047=CARTESIAN_POINT('Ctrl Pts',(-3.86867799500005,2.2,-1.10266279300001));
#316048=CARTESIAN_POINT('Ctrl Pts',(-3.86806976700006,12.2,-1.10256586300002));
#316049=CARTESIAN_POINT('Ctrl Pts',(-3.86806976700006,5.2,-1.10256586300002));
#316050=CARTESIAN_POINT('Ctrl Pts',(-3.86806976700006,2.2,-1.10256586300002));
#316051=CARTESIAN_POINT('Ctrl Pts',(-3.86746776200006,12.2,-1.10246913200001));
#316052=CARTESIAN_POINT('Ctrl Pts',(-3.86746776200006,5.2,-1.10246913200001));
#316053=CARTESIAN_POINT('Ctrl Pts',(-3.86746776200006,2.2,-1.10246913200001));
#316054=CARTESIAN_POINT('Ctrl Pts',(-3.86687199200006,12.2,-1.10237261900001));
#316055=CARTESIAN_POINT('Ctrl Pts',(-3.86687199200006,5.2,-1.10237261900001));
#316056=CARTESIAN_POINT('Ctrl Pts',(-3.86687199200006,2.2,-1.10237261900001));
#316057=CARTESIAN_POINT('Ctrl Pts',(-3.86628246500006,12.2,-1.10227633800001));
#316058=CARTESIAN_POINT('Ctrl Pts',(-3.86628246500006,5.2,-1.10227633800001));
#316059=CARTESIAN_POINT('Ctrl Pts',(-3.86628246500006,2.2,-1.10227633800001));
#316060=CARTESIAN_POINT('Ctrl Pts',(-3.86569919200006,12.2,-1.10218031000001));
#316061=CARTESIAN_POINT('Ctrl Pts',(-3.86569919200006,5.2,-1.10218031000001));
#316062=CARTESIAN_POINT('Ctrl Pts',(-3.86569919200006,2.2,-1.10218031000001));
#316063=CARTESIAN_POINT('Ctrl Pts',(-3.86512218500005,12.2,-1.10208455000001));
#316064=CARTESIAN_POINT('Ctrl Pts',(-3.86512218500005,5.2,-1.10208455000001));
#316065=CARTESIAN_POINT('Ctrl Pts',(-3.86512218500005,2.2,-1.10208455000001));
#316066=CARTESIAN_POINT('Ctrl Pts',(-3.86455145200006,12.2,-1.10198907600001));
#316067=CARTESIAN_POINT('Ctrl Pts',(-3.86455145200006,5.2,-1.10198907600001));
#316068=CARTESIAN_POINT('Ctrl Pts',(-3.86455145200006,2.2,-1.10198907600001));
#316069=CARTESIAN_POINT('Ctrl Pts',(-3.86398700500005,12.2,-1.10189390600001));
#316070=CARTESIAN_POINT('Ctrl Pts',(-3.86398700500005,5.2,-1.10189390600001));
#316071=CARTESIAN_POINT('Ctrl Pts',(-3.86398700500005,2.2,-1.10189390600001));
#316072=CARTESIAN_POINT('Ctrl Pts',(-3.86342885300006,12.2,-1.10179905700001));
#316073=CARTESIAN_POINT('Ctrl Pts',(-3.86342885300006,5.2,-1.10179905700001));
#316074=CARTESIAN_POINT('Ctrl Pts',(-3.86342885300006,2.2,-1.10179905700001));
#316075=CARTESIAN_POINT('Ctrl Pts',(-3.86287700700006,12.2,-1.10170454700001));
#316076=CARTESIAN_POINT('Ctrl Pts',(-3.86287700700006,5.2,-1.10170454700001));
#316077=CARTESIAN_POINT('Ctrl Pts',(-3.86287700700006,2.2,-1.10170454700001));
#316078=CARTESIAN_POINT('Ctrl Pts',(-3.86233147800006,12.2,-1.10161039400001));
#316079=CARTESIAN_POINT('Ctrl Pts',(-3.86233147800006,5.2,-1.10161039400001));
#316080=CARTESIAN_POINT('Ctrl Pts',(-3.86233147800006,2.2,-1.10161039400001));
#316081=CARTESIAN_POINT('Ctrl Pts',(-3.86179227500006,12.2,-1.10151661500002));
#316082=CARTESIAN_POINT('Ctrl Pts',(-3.86179227500006,5.2,-1.10151661500002));
#316083=CARTESIAN_POINT('Ctrl Pts',(-3.86179227500006,2.2,-1.10151661500002));
#316084=CARTESIAN_POINT('Ctrl Pts',(-3.86125940900006,12.2,-1.10142322800002));
#316085=CARTESIAN_POINT('Ctrl Pts',(-3.86125940900006,5.2,-1.10142322800002));
#316086=CARTESIAN_POINT('Ctrl Pts',(-3.86125940900006,2.2,-1.10142322800002));
#316087=CARTESIAN_POINT('Ctrl Pts',(-3.86073289100006,12.2,-1.10133025100001));
#316088=CARTESIAN_POINT('Ctrl Pts',(-3.86073289100006,5.2,-1.10133025100001));
#316089=CARTESIAN_POINT('Ctrl Pts',(-3.86073289100006,2.2,-1.10133025100001));
#316090=CARTESIAN_POINT('Ctrl Pts',(-3.86021273100006,12.2,-1.10123770400001));
#316091=CARTESIAN_POINT('Ctrl Pts',(-3.86021273100006,5.2,-1.10123770400001));
#316092=CARTESIAN_POINT('Ctrl Pts',(-3.86021273100006,2.2,-1.10123770400001));
#316093=CARTESIAN_POINT('Ctrl Pts',(-3.85969893800006,12.2,-1.10114560200001));
#316094=CARTESIAN_POINT('Ctrl Pts',(-3.85969893800006,5.2,-1.10114560200001));
#316095=CARTESIAN_POINT('Ctrl Pts',(-3.85969893800006,2.2,-1.10114560200001));
#316096=CARTESIAN_POINT('Ctrl Pts',(-3.85919152400006,12.2,-1.10105396400002));
#316097=CARTESIAN_POINT('Ctrl Pts',(-3.85919152400006,5.2,-1.10105396400002));
#316098=CARTESIAN_POINT('Ctrl Pts',(-3.85919152400006,2.2,-1.10105396400002));
#316099=CARTESIAN_POINT('Ctrl Pts',(-3.85869050100006,12.2,-1.10096280900001));
#316100=CARTESIAN_POINT('Ctrl Pts',(-3.85869050100006,5.2,-1.10096280900001));
#316101=CARTESIAN_POINT('Ctrl Pts',(-3.85869050100006,2.2,-1.10096280900001));
#316102=CARTESIAN_POINT('Ctrl Pts',(-3.85819587400006,12.2,-1.10087215500001));
#316103=CARTESIAN_POINT('Ctrl Pts',(-3.85819587400006,5.2,-1.10087215500001));
#316104=CARTESIAN_POINT('Ctrl Pts',(-3.85819587400006,2.2,-1.10087215500001));
#316105=CARTESIAN_POINT('Ctrl Pts',(-3.85770765900006,12.2,-1.10078202100001));
#316106=CARTESIAN_POINT('Ctrl Pts',(-3.85770765900006,5.2,-1.10078202100001));
#316107=CARTESIAN_POINT('Ctrl Pts',(-3.85770765900006,2.2,-1.10078202100001));
#316108=CARTESIAN_POINT('Ctrl Pts',(-3.85722586400005,12.2,-1.10069242400002));
#316109=CARTESIAN_POINT('Ctrl Pts',(-3.85722586400005,5.2,-1.10069242400002));
#316110=CARTESIAN_POINT('Ctrl Pts',(-3.85722586400005,2.2,-1.10069242400002));
#316111=CARTESIAN_POINT('Ctrl Pts',(-3.85675050100006,12.2,-1.10060338200002));
#316112=CARTESIAN_POINT('Ctrl Pts',(-3.85675050100006,5.2,-1.10060338200002));
#316113=CARTESIAN_POINT('Ctrl Pts',(-3.85675050100006,2.2,-1.10060338200002));
#316114=CARTESIAN_POINT('Ctrl Pts',(-3.85628157800006,12.2,-1.10051491600001));
#316115=CARTESIAN_POINT('Ctrl Pts',(-3.85628157800006,5.2,-1.10051491600001));
#316116=CARTESIAN_POINT('Ctrl Pts',(-3.85628157800006,2.2,-1.10051491600001));
#316117=CARTESIAN_POINT('Ctrl Pts',(-3.85581910700005,12.2,-1.10042704300001));
#316118=CARTESIAN_POINT('Ctrl Pts',(-3.85581910700005,5.2,-1.10042704300001));
#316119=CARTESIAN_POINT('Ctrl Pts',(-3.85581910700005,2.2,-1.10042704300001));
#316120=CARTESIAN_POINT('Ctrl Pts',(-3.85536309800006,12.2,-1.10033978300002));
#316121=CARTESIAN_POINT('Ctrl Pts',(-3.85536309800006,5.2,-1.10033978300002));
#316122=CARTESIAN_POINT('Ctrl Pts',(-3.85536309800006,2.2,-1.10033978300002));
#316123=CARTESIAN_POINT('Ctrl Pts',(-3.85491356200006,12.2,-1.10025315200001));
#316124=CARTESIAN_POINT('Ctrl Pts',(-3.85491356200006,5.2,-1.10025315200001));
#316125=CARTESIAN_POINT('Ctrl Pts',(-3.85491356200006,2.2,-1.10025315200001));
#316126=CARTESIAN_POINT('Ctrl Pts',(-3.85447051000006,12.2,-1.10016717100001));
#316127=CARTESIAN_POINT('Ctrl Pts',(-3.85447051000006,5.2,-1.10016717100001));
#316128=CARTESIAN_POINT('Ctrl Pts',(-3.85447051000006,2.2,-1.10016717100001));
#316129=CARTESIAN_POINT('Ctrl Pts',(-3.85403395200006,12.2,-1.10008185900002));
#316130=CARTESIAN_POINT('Ctrl Pts',(-3.85403395200006,5.2,-1.10008185900002));
#316131=CARTESIAN_POINT('Ctrl Pts',(-3.85403395200006,2.2,-1.10008185900002));
#316132=CARTESIAN_POINT('Ctrl Pts',(-3.85360389800006,12.2,-1.09999723400001));
#316133=CARTESIAN_POINT('Ctrl Pts',(-3.85360389800006,5.2,-1.09999723400001));
#316134=CARTESIAN_POINT('Ctrl Pts',(-3.85360389800006,2.2,-1.09999723400001));
#316135=CARTESIAN_POINT('Ctrl Pts',(-3.85318035800006,12.2,-1.09991331500002));
#316136=CARTESIAN_POINT('Ctrl Pts',(-3.85318035800006,5.2,-1.09991331500002));
#316137=CARTESIAN_POINT('Ctrl Pts',(-3.85318035800006,2.2,-1.09991331500002));
#316138=CARTESIAN_POINT('Ctrl Pts',(-3.85276334500006,12.2,-1.09983012300002));
#316139=CARTESIAN_POINT('Ctrl Pts',(-3.85276334500006,5.2,-1.09983012300002));
#316140=CARTESIAN_POINT('Ctrl Pts',(-3.85276334500006,2.2,-1.09983012300002));
#316141=CARTESIAN_POINT('Ctrl Pts',(-3.85235286800006,12.2,-1.09974767600002));
#316142=CARTESIAN_POINT('Ctrl Pts',(-3.85235286800006,5.2,-1.09974767600002));
#316143=CARTESIAN_POINT('Ctrl Pts',(-3.85235286800006,2.2,-1.09974767600002));
#316144=CARTESIAN_POINT('Ctrl Pts',(-3.85194893700006,12.2,-1.09966599100002));
#316145=CARTESIAN_POINT('Ctrl Pts',(-3.85194893700006,5.2,-1.09966599100002));
#316146=CARTESIAN_POINT('Ctrl Pts',(-3.85194893700006,2.2,-1.09966599100002));
#316147=CARTESIAN_POINT('Ctrl Pts',(-3.85155156300006,12.2,-1.09958509100001));
#316148=CARTESIAN_POINT('Ctrl Pts',(-3.85155156300006,5.2,-1.09958509100001));
#316149=CARTESIAN_POINT('Ctrl Pts',(-3.85155156300006,2.2,-1.09958509100001));
#316150=CARTESIAN_POINT('Ctrl Pts',(-3.85116075800005,12.2,-1.09950499300002));
#316151=CARTESIAN_POINT('Ctrl Pts',(-3.85116075800005,5.2,-1.09950499300002));
#316152=CARTESIAN_POINT('Ctrl Pts',(-3.85116075800005,2.2,-1.09950499300002));
#316153=CARTESIAN_POINT('Ctrl Pts',(-3.85077653200006,12.2,-1.09942571900001));
#316154=CARTESIAN_POINT('Ctrl Pts',(-3.85077653200006,5.2,-1.09942571900001));
#316155=CARTESIAN_POINT('Ctrl Pts',(-3.85077653200006,2.2,-1.09942571900001));
#316156=CARTESIAN_POINT('Ctrl Pts',(-3.85039889400006,12.2,-1.09934728600001));
#316157=CARTESIAN_POINT('Ctrl Pts',(-3.85039889400006,5.2,-1.09934728600001));
#316158=CARTESIAN_POINT('Ctrl Pts',(-3.85039889400006,2.2,-1.09934728600001));
#316159=CARTESIAN_POINT('Ctrl Pts',(-3.85002785600006,12.2,-1.09926971400002));
#316160=CARTESIAN_POINT('Ctrl Pts',(-3.85002785600006,5.2,-1.09926971400002));
#316161=CARTESIAN_POINT('Ctrl Pts',(-3.85002785600006,2.2,-1.09926971400002));
#316162=CARTESIAN_POINT('Ctrl Pts',(-3.84966343000006,12.2,-1.09919302400002));
#316163=CARTESIAN_POINT('Ctrl Pts',(-3.84966343000006,5.2,-1.09919302400002));
#316164=CARTESIAN_POINT('Ctrl Pts',(-3.84966343000006,2.2,-1.09919302400002));
#316165=CARTESIAN_POINT('Ctrl Pts',(-3.84930562400006,12.2,-1.09911723500002));
#316166=CARTESIAN_POINT('Ctrl Pts',(-3.84930562400006,5.2,-1.09911723500002));
#316167=CARTESIAN_POINT('Ctrl Pts',(-3.84930562400006,2.2,-1.09911723500002));
#316168=CARTESIAN_POINT('Ctrl Pts',(-3.84895445000006,12.2,-1.09904236700002));
#316169=CARTESIAN_POINT('Ctrl Pts',(-3.84895445000006,5.2,-1.09904236700002));
#316170=CARTESIAN_POINT('Ctrl Pts',(-3.84895445000006,2.2,-1.09904236700002));
#316171=CARTESIAN_POINT('Ctrl Pts',(-3.84860991900006,12.2,-1.09896844000001));
#316172=CARTESIAN_POINT('Ctrl Pts',(-3.84860991900006,5.2,-1.09896844000001));
#316173=CARTESIAN_POINT('Ctrl Pts',(-3.84860991900006,2.2,-1.09896844000001));
#316174=CARTESIAN_POINT('Ctrl Pts',(-3.84827204100006,12.2,-1.09889547500002));
#316175=CARTESIAN_POINT('Ctrl Pts',(-3.84827204100006,5.2,-1.09889547500002));
#316176=CARTESIAN_POINT('Ctrl Pts',(-3.84827204100006,2.2,-1.09889547500002));
#316177=CARTESIAN_POINT('Ctrl Pts',(-3.84794082700005,12.2,-1.09882349000001));
#316178=CARTESIAN_POINT('Ctrl Pts',(-3.84794082700005,5.2,-1.09882349000001));
#316179=CARTESIAN_POINT('Ctrl Pts',(-3.84794082700005,2.2,-1.09882349000001));
#316180=CARTESIAN_POINT('Ctrl Pts',(-3.84761628800006,12.2,-1.09875250600002));
#316181=CARTESIAN_POINT('Ctrl Pts',(-3.84761628800006,5.2,-1.09875250600002));
#316182=CARTESIAN_POINT('Ctrl Pts',(-3.84761628800006,2.2,-1.09875250600002));
#316183=CARTESIAN_POINT('Ctrl Pts',(-3.84729843500006,12.2,-1.09868254300002));
#316184=CARTESIAN_POINT('Ctrl Pts',(-3.84729843500006,5.2,-1.09868254300002));
#316185=CARTESIAN_POINT('Ctrl Pts',(-3.84729843500006,2.2,-1.09868254300002));
#316186=CARTESIAN_POINT('Ctrl Pts',(-3.84698727800005,12.2,-1.09861362400002));
#316187=CARTESIAN_POINT('Ctrl Pts',(-3.84698727800005,5.2,-1.09861362400002));
#316188=CARTESIAN_POINT('Ctrl Pts',(-3.84698727800005,2.2,-1.09861362400002));
#316189=CARTESIAN_POINT('Ctrl Pts',(-3.84668282800006,12.2,-1.09854576700001));
#316190=CARTESIAN_POINT('Ctrl Pts',(-3.84668282800006,5.2,-1.09854576700001));
#316191=CARTESIAN_POINT('Ctrl Pts',(-3.84668282800006,2.2,-1.09854576700001));
#316192=CARTESIAN_POINT('Ctrl Pts',(-3.84638509700006,12.2,-1.09847899200001));
#316193=CARTESIAN_POINT('Ctrl Pts',(-3.84638509700006,5.2,-1.09847899200001));
#316194=CARTESIAN_POINT('Ctrl Pts',(-3.84638509700006,2.2,-1.09847899200001));
#316195=CARTESIAN_POINT('Ctrl Pts',(-3.84609409400006,12.2,-1.09841332200002));
#316196=CARTESIAN_POINT('Ctrl Pts',(-3.84609409400006,5.2,-1.09841332200002));
#316197=CARTESIAN_POINT('Ctrl Pts',(-3.84609409400006,2.2,-1.09841332200002));
#316198=CARTESIAN_POINT('Ctrl Pts',(-3.84580983000006,12.2,-1.09834877500001));
#316199=CARTESIAN_POINT('Ctrl Pts',(-3.84580983000006,5.2,-1.09834877500001));
#316200=CARTESIAN_POINT('Ctrl Pts',(-3.84580983000006,2.2,-1.09834877500001));
#316201=CARTESIAN_POINT('Ctrl Pts',(-3.84553231800006,12.2,-1.09828537300002));
#316202=CARTESIAN_POINT('Ctrl Pts',(-3.84553231800006,5.2,-1.09828537300002));
#316203=CARTESIAN_POINT('Ctrl Pts',(-3.84553231800006,2.2,-1.09828537300002));
#316204=CARTESIAN_POINT('Ctrl Pts',(-3.84526156700006,12.2,-1.09822313700001));
#316205=CARTESIAN_POINT('Ctrl Pts',(-3.84526156700006,5.2,-1.09822313700001));
#316206=CARTESIAN_POINT('Ctrl Pts',(-3.84526156700006,2.2,-1.09822313700001));
#316207=CARTESIAN_POINT('Ctrl Pts',(-3.84499758700006,12.2,-1.09816208800002));
#316208=CARTESIAN_POINT('Ctrl Pts',(-3.84499758700006,5.2,-1.09816208800002));
#316209=CARTESIAN_POINT('Ctrl Pts',(-3.84499758700006,2.2,-1.09816208800002));
#316210=CARTESIAN_POINT('Ctrl Pts',(-3.84474039100006,12.2,-1.09810224700002));
#316211=CARTESIAN_POINT('Ctrl Pts',(-3.84474039100006,5.2,-1.09810224700002));
#316212=CARTESIAN_POINT('Ctrl Pts',(-3.84474039100006,2.2,-1.09810224700002));
#316213=CARTESIAN_POINT('Ctrl Pts',(-3.84448998900006,12.2,-1.09804363400002));
#316214=CARTESIAN_POINT('Ctrl Pts',(-3.84448998900006,5.2,-1.09804363400002));
#316215=CARTESIAN_POINT('Ctrl Pts',(-3.84448998900006,2.2,-1.09804363400002));
#316216=CARTESIAN_POINT('Ctrl Pts',(-3.84424639200006,12.2,-1.09798627300002));
#316217=CARTESIAN_POINT('Ctrl Pts',(-3.84424639200006,5.2,-1.09798627300002));
#316218=CARTESIAN_POINT('Ctrl Pts',(-3.84424639200006,2.2,-1.09798627300002));
#316219=CARTESIAN_POINT('Ctrl Pts',(-3.84400961000006,12.2,-1.09793018200001));
#316220=CARTESIAN_POINT('Ctrl Pts',(-3.84400961000006,5.2,-1.09793018200001));
#316221=CARTESIAN_POINT('Ctrl Pts',(-3.84400961000006,2.2,-1.09793018200001));
#316222=CARTESIAN_POINT('Ctrl Pts',(-3.84377965500006,12.2,-1.09787538400001));
#316223=CARTESIAN_POINT('Ctrl Pts',(-3.84377965500006,5.2,-1.09787538400001));
#316224=CARTESIAN_POINT('Ctrl Pts',(-3.84377965500006,2.2,-1.09787538400001));
#316225=CARTESIAN_POINT('Ctrl Pts',(-3.84355653800006,12.2,-1.09782190000002));
#316226=CARTESIAN_POINT('Ctrl Pts',(-3.84355653800006,5.2,-1.09782190000002));
#316227=CARTESIAN_POINT('Ctrl Pts',(-3.84355653800006,2.2,-1.09782190000002));
#316228=CARTESIAN_POINT('Ctrl Pts',(-3.84334026900006,12.2,-1.09776975200001));
#316229=CARTESIAN_POINT('Ctrl Pts',(-3.84334026900006,5.2,-1.09776975200001));
#316230=CARTESIAN_POINT('Ctrl Pts',(-3.84334026900006,2.2,-1.09776975200001));
#316231=CARTESIAN_POINT('Ctrl Pts',(-3.84313086000006,12.2,-1.09771896100002));
#316232=CARTESIAN_POINT('Ctrl Pts',(-3.84313086000006,5.2,-1.09771896100002));
#316233=CARTESIAN_POINT('Ctrl Pts',(-3.84313086000006,2.2,-1.09771896100002));
#316234=CARTESIAN_POINT('Ctrl Pts',(-3.84292832100006,12.2,-1.09766954900001));
#316235=CARTESIAN_POINT('Ctrl Pts',(-3.84292832100006,5.2,-1.09766954900001));
#316236=CARTESIAN_POINT('Ctrl Pts',(-3.84292832100006,2.2,-1.09766954900001));
#316237=CARTESIAN_POINT('Ctrl Pts',(-3.84273266500006,12.2,-1.09762153800002));
#316238=CARTESIAN_POINT('Ctrl Pts',(-3.84273266500006,5.2,-1.09762153800002));
#316239=CARTESIAN_POINT('Ctrl Pts',(-3.84273266500006,2.2,-1.09762153800002));
#316240=CARTESIAN_POINT('Ctrl Pts',(-3.84254390100006,12.2,-1.09757495000002));
#316241=CARTESIAN_POINT('Ctrl Pts',(-3.84254390100006,5.2,-1.09757495000002));
#316242=CARTESIAN_POINT('Ctrl Pts',(-3.84254390100006,2.2,-1.09757495000002));
#316243=CARTESIAN_POINT('Ctrl Pts',(-3.84236204200006,12.2,-1.09752980700002));
#316244=CARTESIAN_POINT('Ctrl Pts',(-3.84236204200006,5.2,-1.09752980700002));
#316245=CARTESIAN_POINT('Ctrl Pts',(-3.84236204200006,2.2,-1.09752980700002));
#316246=CARTESIAN_POINT('Ctrl Pts',(-3.84218709600006,12.2,-1.09748613100002));
#316247=CARTESIAN_POINT('Ctrl Pts',(-3.84218709600006,5.2,-1.09748613100002));
#316248=CARTESIAN_POINT('Ctrl Pts',(-3.84218709600006,2.2,-1.09748613100002));
#316249=CARTESIAN_POINT('Ctrl Pts',(-3.84201907700006,12.2,-1.09744394400002));
#316250=CARTESIAN_POINT('Ctrl Pts',(-3.84201907700006,5.2,-1.09744394400002));
#316251=CARTESIAN_POINT('Ctrl Pts',(-3.84201907700006,2.2,-1.09744394400002));
#316252=CARTESIAN_POINT('Ctrl Pts',(-3.84185799400006,12.2,-1.09740326700001));
#316253=CARTESIAN_POINT('Ctrl Pts',(-3.84185799400006,5.2,-1.09740326700001));
#316254=CARTESIAN_POINT('Ctrl Pts',(-3.84185799400006,2.2,-1.09740326700001));
#316255=CARTESIAN_POINT('Ctrl Pts',(-3.84170386000006,12.2,-1.09736412400002));
#316256=CARTESIAN_POINT('Ctrl Pts',(-3.84170386000006,5.2,-1.09736412400002));
#316257=CARTESIAN_POINT('Ctrl Pts',(-3.84170386000006,2.2,-1.09736412400002));
#316258=CARTESIAN_POINT('Ctrl Pts',(-3.84155668300005,12.2,-1.09732653400001));
#316259=CARTESIAN_POINT('Ctrl Pts',(-3.84155668300005,5.2,-1.09732653400001));
#316260=CARTESIAN_POINT('Ctrl Pts',(-3.84155668300005,2.2,-1.09732653400001));
#316261=CARTESIAN_POINT('Ctrl Pts',(-3.84141647700006,12.2,-1.09729052600001));
#316262=CARTESIAN_POINT('Ctrl Pts',(-3.84141647700006,5.2,-1.09729052600001));
#316263=CARTESIAN_POINT('Ctrl Pts',(-3.84141647700006,2.2,-1.09729052600001));
#316264=CARTESIAN_POINT('Ctrl Pts',(-3.84128325400006,12.2,-1.09725611800001));
#316265=CARTESIAN_POINT('Ctrl Pts',(-3.84128325400006,5.2,-1.09725611800001));
#316266=CARTESIAN_POINT('Ctrl Pts',(-3.84128325400006,2.2,-1.09725611800001));
#316267=CARTESIAN_POINT('Ctrl Pts',(-3.84115702400006,12.2,-1.09722333700002));
#316268=CARTESIAN_POINT('Ctrl Pts',(-3.84115702400006,5.2,-1.09722333700002));
#316269=CARTESIAN_POINT('Ctrl Pts',(-3.84115702400006,2.2,-1.09722333700002));
#316270=CARTESIAN_POINT('Ctrl Pts',(-3.84103780000006,12.2,-1.09719220600001));
#316271=CARTESIAN_POINT('Ctrl Pts',(-3.84103780000006,5.2,-1.09719220600001));
#316272=CARTESIAN_POINT('Ctrl Pts',(-3.84103780000006,2.2,-1.09719220600001));
#316273=CARTESIAN_POINT('Ctrl Pts',(-3.84092559000006,12.2,-1.09716274300002));
#316274=CARTESIAN_POINT('Ctrl Pts',(-3.84092559000006,5.2,-1.09716274300002));
#316275=CARTESIAN_POINT('Ctrl Pts',(-3.84092559000006,2.2,-1.09716274300002));
#316276=CARTESIAN_POINT('Ctrl Pts',(-3.84082040400005,12.2,-1.09713496900001));
#316277=CARTESIAN_POINT('Ctrl Pts',(-3.84082040400005,5.2,-1.09713496900001));
#316278=CARTESIAN_POINT('Ctrl Pts',(-3.84082040400005,2.2,-1.09713496900001));
#316279=CARTESIAN_POINT('Ctrl Pts',(-3.84072225300006,12.2,-1.09710890700002));
#316280=CARTESIAN_POINT('Ctrl Pts',(-3.84072225300006,5.2,-1.09710890700002));
#316281=CARTESIAN_POINT('Ctrl Pts',(-3.84072225300006,2.2,-1.09710890700002));
#316282=CARTESIAN_POINT('Ctrl Pts',(-3.84063114900006,12.2,-1.09708457800001));
#316283=CARTESIAN_POINT('Ctrl Pts',(-3.84063114900006,5.2,-1.09708457800001));
#316284=CARTESIAN_POINT('Ctrl Pts',(-3.84063114900006,2.2,-1.09708457800001));
#316285=CARTESIAN_POINT('Ctrl Pts',(-3.84054710500005,12.2,-1.09706201000002));
#316286=CARTESIAN_POINT('Ctrl Pts',(-3.84054710500005,5.2,-1.09706201000002));
#316287=CARTESIAN_POINT('Ctrl Pts',(-3.84054710500005,2.2,-1.09706201000002));
#316288=CARTESIAN_POINT('Ctrl Pts',(-3.84047013400005,12.2,-1.09704123400002));
#316289=CARTESIAN_POINT('Ctrl Pts',(-3.84047013400005,5.2,-1.09704123400002));
#316290=CARTESIAN_POINT('Ctrl Pts',(-3.84047013400005,2.2,-1.09704123400002));
#316291=CARTESIAN_POINT('Ctrl Pts',(-3.84040025100005,12.2,-1.09702227600001));
#316292=CARTESIAN_POINT('Ctrl Pts',(-3.84040025100005,5.2,-1.09702227600001));
#316293=CARTESIAN_POINT('Ctrl Pts',(-3.84040025100005,2.2,-1.09702227600001));
#316294=CARTESIAN_POINT('Ctrl Pts',(-3.84033746800006,12.2,-1.09700516500002));
#316295=CARTESIAN_POINT('Ctrl Pts',(-3.84033746800006,5.2,-1.09700516500002));
#316296=CARTESIAN_POINT('Ctrl Pts',(-3.84033746800006,2.2,-1.09700516500002));
#316297=CARTESIAN_POINT('Ctrl Pts',(-3.84028179500006,12.2,-1.09698992100002));
#316298=CARTESIAN_POINT('Ctrl Pts',(-3.84028179500006,5.2,-1.09698992100002));
#316299=CARTESIAN_POINT('Ctrl Pts',(-3.84028179500006,2.2,-1.09698992100002));
#316300=CARTESIAN_POINT('Ctrl Pts',(-3.84022803879258,12.2,-1.09697511972126));
#316301=CARTESIAN_POINT('Ctrl Pts',(-3.84022803879258,5.2,-1.09697511972126));
#316302=CARTESIAN_POINT('Ctrl Pts',(-3.84022803879258,2.2,-1.09697511972126));
#316303=CARTESIAN_POINT('Ctrl Pts',(-3.84019131325105,12.2,-1.09696492845847));
#316304=CARTESIAN_POINT('Ctrl Pts',(-3.84019131325105,5.2,-1.09696492845847));
#316305=CARTESIAN_POINT('Ctrl Pts',(-3.84019131325105,2.2,-1.09696492845847));
#316306=CARTESIAN_POINT('Ctrl Pts',(-3.84016713475081,12.2,-1.0969581629428));
#316307=CARTESIAN_POINT('Ctrl Pts',(-3.84016713475081,5.2,-1.0969581629428));
#316308=CARTESIAN_POINT('Ctrl Pts',(-3.84016713475081,2.2,-1.0969581629428));
#316309=CARTESIAN_POINT('Ctrl Pts',(-3.84015208032585,12.2,-1.09695391765456));
#316310=CARTESIAN_POINT('Ctrl Pts',(-3.84015208032585,5.2,-1.09695391765456));
#316311=CARTESIAN_POINT('Ctrl Pts',(-3.84015208032585,2.2,-1.09695391765456));
#316312=CARTESIAN_POINT('Ctrl Pts',(-3.84014278600006,12.2,-1.09695129700001));
#316313=CARTESIAN_POINT('Ctrl Pts',(-3.84014278600006,5.2,-1.09695129700001));
#316314=CARTESIAN_POINT('Ctrl Pts',(-3.84014278600006,2.2,-1.09695129700001));
#316315=CARTESIAN_POINT('',(-3.84014273100005,2.7,-1.09695149100002));
#316316=CARTESIAN_POINT('',(-3.84014273100005,12.2,-1.09695149100002));
#316317=CARTESIAN_POINT('Ctrl Pts',(-4.64916443400006,2.7,-0.973534832000014));
#316318=CARTESIAN_POINT('Ctrl Pts',(-4.39305820566497,2.7,-1.07158848910283));
#316319=CARTESIAN_POINT('Ctrl Pts',(-4.20747959129484,2.70000000001822,
-1.09719287120144));
#316320=CARTESIAN_POINT('Ctrl Pts',(-3.96057902756421,2.70000000001822,
-1.1188234958715));
#316321=CARTESIAN_POINT('Ctrl Pts',(-3.87277126955167,2.70000000001823,
-1.10458234514971));
#316322=CARTESIAN_POINT('Ctrl Pts',(-3.84199433897037,2.70000000001823,
-1.09746781128816));
#316323=CARTESIAN_POINT('Ctrl Pts',(-3.84047363749101,2.7,-1.09704458482765));
#316324=CARTESIAN_POINT('Ctrl Pts',(-3.84014278600006,2.7,-1.09695129700001));
#316325=CARTESIAN_POINT('Origin',(-3.84009338800006,15.2,-1.09693739600001));
#316326=CARTESIAN_POINT('',(-3.48557996500006,2.7,-0.995669277000015));
#316327=CARTESIAN_POINT('',(-3.48557996500006,2.2,-0.995669277000015));
#316328=CARTESIAN_POINT('',(-1.92004669396261,2.7,-0.548468698131102));
#316329=CARTESIAN_POINT('Origin',(-5.66300478732629E-14,15.2,-1.77635683940025E-14));
#316330=CARTESIAN_POINT('',(-3.29009567500006,2.7,-1.52180664000001));
#316331=CARTESIAN_POINT('',(-3.29009567500006,12.2,-1.52180664000001));
#316332=CARTESIAN_POINT('Origin',(-5.66300478732629E-14,2.7,-1.92943768261394E-14));
#316333=CARTESIAN_POINT('Origin',(-5.66300478732629E-14,15.2,-1.77635683940025E-14));
#316334=CARTESIAN_POINT('',(-3.62475771700006,2.7,-1.67660181100001));
#316335=CARTESIAN_POINT('',(-3.62475771700006,12.2,-1.67660181100001));
#316336=CARTESIAN_POINT('',(-5.63267452475378E-14,2.7,-1.91540866959583E-14));
#316337=CARTESIAN_POINT('Ctrl Pts',(-3.62475766000006,12.2,-1.67660193200001));
#316338=CARTESIAN_POINT('Ctrl Pts',(-3.62475766000006,5.2,-1.67660193200001));
#316339=CARTESIAN_POINT('Ctrl Pts',(-3.62475766000006,2.2,-1.67660193200001));
#316340=CARTESIAN_POINT('Ctrl Pts',(-3.62476385949508,12.2,-1.67660482976411));
#316341=CARTESIAN_POINT('Ctrl Pts',(-3.62476385949508,5.2,-1.67660482976411));
#316342=CARTESIAN_POINT('Ctrl Pts',(-3.62476385949508,2.2,-1.67660482976411));
#316343=CARTESIAN_POINT('Ctrl Pts',(-3.62477584957619,12.2,-1.67661043119582));
#316344=CARTESIAN_POINT('Ctrl Pts',(-3.62477584957619,5.2,-1.67661043119582));
#316345=CARTESIAN_POINT('Ctrl Pts',(-3.62477584957619,2.2,-1.67661043119582));
#316346=CARTESIAN_POINT('Ctrl Pts',(-3.62479362506676,12.2,-1.67661873245304));
#316347=CARTESIAN_POINT('Ctrl Pts',(-3.62479362506676,5.2,-1.67661873245304));
#316348=CARTESIAN_POINT('Ctrl Pts',(-3.62479362506676,2.2,-1.67661873245304));
#316349=CARTESIAN_POINT('Ctrl Pts',(-3.62481722099134,12.2,-1.67662978965931));
#316350=CARTESIAN_POINT('Ctrl Pts',(-3.62481722099134,5.2,-1.67662978965931));
#316351=CARTESIAN_POINT('Ctrl Pts',(-3.62481722099134,2.2,-1.67662978965931));
#316352=CARTESIAN_POINT('Ctrl Pts',(-3.62485815500006,12.2,-1.67664910700001));
#316353=CARTESIAN_POINT('Ctrl Pts',(-3.62485815500006,5.2,-1.67664910700001));
#316354=CARTESIAN_POINT('Ctrl Pts',(-3.62485815500006,2.2,-1.67664910700001));
#316355=CARTESIAN_POINT('Ctrl Pts',(-3.62490366200006,12.2,-1.67667068700001));
#316356=CARTESIAN_POINT('Ctrl Pts',(-3.62490366200006,5.2,-1.67667068700001));
#316357=CARTESIAN_POINT('Ctrl Pts',(-3.62490366200006,2.2,-1.67667068700001));
#316358=CARTESIAN_POINT('Ctrl Pts',(-3.62495578300006,12.2,-1.67669549200001));
#316359=CARTESIAN_POINT('Ctrl Pts',(-3.62495578300006,5.2,-1.67669549200001));
#316360=CARTESIAN_POINT('Ctrl Pts',(-3.62495578300006,2.2,-1.67669549200001));
#316361=CARTESIAN_POINT('Ctrl Pts',(-3.62501450700006,12.2,-1.67672352600002));
#316362=CARTESIAN_POINT('Ctrl Pts',(-3.62501450700006,5.2,-1.67672352600002));
#316363=CARTESIAN_POINT('Ctrl Pts',(-3.62501450700006,2.2,-1.67672352600002));
#316364=CARTESIAN_POINT('Ctrl Pts',(-3.62507981500006,12.2,-1.67675479900002));
#316365=CARTESIAN_POINT('Ctrl Pts',(-3.62507981500006,5.2,-1.67675479900002));
#316366=CARTESIAN_POINT('Ctrl Pts',(-3.62507981500006,2.2,-1.67675479900002));
#316367=CARTESIAN_POINT('Ctrl Pts',(-3.62515167800006,12.2,-1.67678932100001));
#316368=CARTESIAN_POINT('Ctrl Pts',(-3.62515167800006,5.2,-1.67678932100001));
#316369=CARTESIAN_POINT('Ctrl Pts',(-3.62515167800006,2.2,-1.67678932100001));
#316370=CARTESIAN_POINT('Ctrl Pts',(-3.62523006900005,12.2,-1.67682710500001));
#316371=CARTESIAN_POINT('Ctrl Pts',(-3.62523006900005,5.2,-1.67682710500001));
#316372=CARTESIAN_POINT('Ctrl Pts',(-3.62523006900005,2.2,-1.67682710500001));
#316373=CARTESIAN_POINT('Ctrl Pts',(-3.62531495600006,12.2,-1.67686816600002));
#316374=CARTESIAN_POINT('Ctrl Pts',(-3.62531495600006,5.2,-1.67686816600002));
#316375=CARTESIAN_POINT('Ctrl Pts',(-3.62531495600006,2.2,-1.67686816600002));
#316376=CARTESIAN_POINT('Ctrl Pts',(-3.62540631300006,12.2,-1.67691251300001));
#316377=CARTESIAN_POINT('Ctrl Pts',(-3.62540631300006,5.2,-1.67691251300001));
#316378=CARTESIAN_POINT('Ctrl Pts',(-3.62540631300006,2.2,-1.67691251300001));
#316379=CARTESIAN_POINT('Ctrl Pts',(-3.62550411600005,12.2,-1.67696015900002));
#316380=CARTESIAN_POINT('Ctrl Pts',(-3.62550411600005,5.2,-1.67696015900002));
#316381=CARTESIAN_POINT('Ctrl Pts',(-3.62550411600005,2.2,-1.67696015900002));
#316382=CARTESIAN_POINT('Ctrl Pts',(-3.62560834100006,12.2,-1.67701111200001));
#316383=CARTESIAN_POINT('Ctrl Pts',(-3.62560834100006,5.2,-1.67701111200001));
#316384=CARTESIAN_POINT('Ctrl Pts',(-3.62560834100006,2.2,-1.67701111200001));
#316385=CARTESIAN_POINT('Ctrl Pts',(-3.62571897000006,12.2,-1.67706538100001));
#316386=CARTESIAN_POINT('Ctrl Pts',(-3.62571897000006,5.2,-1.67706538100001));
#316387=CARTESIAN_POINT('Ctrl Pts',(-3.62571897000006,2.2,-1.67706538100001));
#316388=CARTESIAN_POINT('Ctrl Pts',(-3.62583598000006,12.2,-1.67712297500001));
#316389=CARTESIAN_POINT('Ctrl Pts',(-3.62583598000006,5.2,-1.67712297500001));
#316390=CARTESIAN_POINT('Ctrl Pts',(-3.62583598000006,2.2,-1.67712297500001));
#316391=CARTESIAN_POINT('Ctrl Pts',(-3.62595934900006,12.2,-1.67718390600001));
#316392=CARTESIAN_POINT('Ctrl Pts',(-3.62595934900006,5.2,-1.67718390600001));
#316393=CARTESIAN_POINT('Ctrl Pts',(-3.62595934900006,2.2,-1.67718390600001));
#316394=CARTESIAN_POINT('Ctrl Pts',(-3.62608905300006,12.2,-1.67724817900002));
#316395=CARTESIAN_POINT('Ctrl Pts',(-3.62608905300006,5.2,-1.67724817900002));
#316396=CARTESIAN_POINT('Ctrl Pts',(-3.62608905300006,2.2,-1.67724817900002));
#316397=CARTESIAN_POINT('Ctrl Pts',(-3.62622506700006,12.2,-1.67731580900002));
#316398=CARTESIAN_POINT('Ctrl Pts',(-3.62622506700006,5.2,-1.67731580900002));
#316399=CARTESIAN_POINT('Ctrl Pts',(-3.62622506700006,2.2,-1.67731580900002));
#316400=CARTESIAN_POINT('Ctrl Pts',(-3.62636736800006,12.2,-1.67738680500001));
#316401=CARTESIAN_POINT('Ctrl Pts',(-3.62636736800006,5.2,-1.67738680500001));
#316402=CARTESIAN_POINT('Ctrl Pts',(-3.62636736800006,2.2,-1.67738680500001));
#316403=CARTESIAN_POINT('Ctrl Pts',(-3.62651593200006,12.2,-1.67746117600001));
#316404=CARTESIAN_POINT('Ctrl Pts',(-3.62651593200006,5.2,-1.67746117600001));
#316405=CARTESIAN_POINT('Ctrl Pts',(-3.62651593200006,2.2,-1.67746117600001));
#316406=CARTESIAN_POINT('Ctrl Pts',(-3.62667073600006,12.2,-1.67753893200001));
#316407=CARTESIAN_POINT('Ctrl Pts',(-3.62667073600006,5.2,-1.67753893200001));
#316408=CARTESIAN_POINT('Ctrl Pts',(-3.62667073600006,2.2,-1.67753893200001));
#316409=CARTESIAN_POINT('Ctrl Pts',(-3.62683175700006,12.2,-1.67762008300001));
#316410=CARTESIAN_POINT('Ctrl Pts',(-3.62683175700006,5.2,-1.67762008300001));
#316411=CARTESIAN_POINT('Ctrl Pts',(-3.62683175700006,2.2,-1.67762008300001));
#316412=CARTESIAN_POINT('Ctrl Pts',(-3.62699897200006,12.2,-1.67770463900001));
#316413=CARTESIAN_POINT('Ctrl Pts',(-3.62699897200006,5.2,-1.67770463900001));
#316414=CARTESIAN_POINT('Ctrl Pts',(-3.62699897200006,2.2,-1.67770463900001));
#316415=CARTESIAN_POINT('Ctrl Pts',(-3.62717236200006,12.2,-1.67779260800001));
#316416=CARTESIAN_POINT('Ctrl Pts',(-3.62717236200006,5.2,-1.67779260800001));
#316417=CARTESIAN_POINT('Ctrl Pts',(-3.62717236200006,2.2,-1.67779260800001));
#316418=CARTESIAN_POINT('Ctrl Pts',(-3.62735190100006,12.2,-1.67788399900001));
#316419=CARTESIAN_POINT('Ctrl Pts',(-3.62735190100006,5.2,-1.67788399900001));
#316420=CARTESIAN_POINT('Ctrl Pts',(-3.62735190100006,2.2,-1.67788399900001));
#316421=CARTESIAN_POINT('Ctrl Pts',(-3.62753756600006,12.2,-1.67797882200002));
#316422=CARTESIAN_POINT('Ctrl Pts',(-3.62753756600006,5.2,-1.67797882200002));
#316423=CARTESIAN_POINT('Ctrl Pts',(-3.62753756600006,2.2,-1.67797882200002));
#316424=CARTESIAN_POINT('Ctrl Pts',(-3.62772933700006,12.2,-1.67807708800002));
#316425=CARTESIAN_POINT('Ctrl Pts',(-3.62772933700006,5.2,-1.67807708800002));
#316426=CARTESIAN_POINT('Ctrl Pts',(-3.62772933700006,2.2,-1.67807708800002));
#316427=CARTESIAN_POINT('Ctrl Pts',(-3.62792718900006,12.2,-1.67817880400001));
#316428=CARTESIAN_POINT('Ctrl Pts',(-3.62792718900006,5.2,-1.67817880400001));
#316429=CARTESIAN_POINT('Ctrl Pts',(-3.62792718900006,2.2,-1.67817880400001));
#316430=CARTESIAN_POINT('Ctrl Pts',(-3.62813109900006,12.2,-1.67828398200002));
#316431=CARTESIAN_POINT('Ctrl Pts',(-3.62813109900006,5.2,-1.67828398200002));
#316432=CARTESIAN_POINT('Ctrl Pts',(-3.62813109900006,2.2,-1.67828398200002));
#316433=CARTESIAN_POINT('Ctrl Pts',(-3.62834104700006,12.2,-1.67839262700001));
#316434=CARTESIAN_POINT('Ctrl Pts',(-3.62834104700006,5.2,-1.67839262700001));
#316435=CARTESIAN_POINT('Ctrl Pts',(-3.62834104700006,2.2,-1.67839262700001));
#316436=CARTESIAN_POINT('Ctrl Pts',(-3.62855700900006,12.2,-1.67850475100002));
#316437=CARTESIAN_POINT('Ctrl Pts',(-3.62855700900006,5.2,-1.67850475100002));
#316438=CARTESIAN_POINT('Ctrl Pts',(-3.62855700900006,2.2,-1.67850475100002));
#316439=CARTESIAN_POINT('Ctrl Pts',(-3.62877896400006,12.2,-1.67862036400001));
#316440=CARTESIAN_POINT('Ctrl Pts',(-3.62877896400006,5.2,-1.67862036400001));
#316441=CARTESIAN_POINT('Ctrl Pts',(-3.62877896400006,2.2,-1.67862036400001));
#316442=CARTESIAN_POINT('Ctrl Pts',(-3.62900688900006,12.2,-1.67873947200002));
#316443=CARTESIAN_POINT('Ctrl Pts',(-3.62900688900006,5.2,-1.67873947200002));
#316444=CARTESIAN_POINT('Ctrl Pts',(-3.62900688900006,2.2,-1.67873947200002));
#316445=CARTESIAN_POINT('Ctrl Pts',(-3.62924076300006,12.2,-1.67886208600001));
#316446=CARTESIAN_POINT('Ctrl Pts',(-3.62924076300006,5.2,-1.67886208600001));
#316447=CARTESIAN_POINT('Ctrl Pts',(-3.62924076300006,2.2,-1.67886208600001));
#316448=CARTESIAN_POINT('Ctrl Pts',(-3.62948056200006,12.2,-1.67898821400001));
#316449=CARTESIAN_POINT('Ctrl Pts',(-3.62948056200006,5.2,-1.67898821400001));
#316450=CARTESIAN_POINT('Ctrl Pts',(-3.62948056200006,2.2,-1.67898821400001));
#316451=CARTESIAN_POINT('Ctrl Pts',(-3.62972626600006,12.2,-1.67911786500001));
#316452=CARTESIAN_POINT('Ctrl Pts',(-3.62972626600006,5.2,-1.67911786500001));
#316453=CARTESIAN_POINT('Ctrl Pts',(-3.62972626600006,2.2,-1.67911786500001));
#316454=CARTESIAN_POINT('Ctrl Pts',(-3.62997785200006,12.2,-1.67925104800001));
#316455=CARTESIAN_POINT('Ctrl Pts',(-3.62997785200006,5.2,-1.67925104800001));
#316456=CARTESIAN_POINT('Ctrl Pts',(-3.62997785200006,2.2,-1.67925104800001));
#316457=CARTESIAN_POINT('Ctrl Pts',(-3.63023529700006,12.2,-1.67938777100002));
#316458=CARTESIAN_POINT('Ctrl Pts',(-3.63023529700006,5.2,-1.67938777100002));
#316459=CARTESIAN_POINT('Ctrl Pts',(-3.63023529700006,2.2,-1.67938777100002));
#316460=CARTESIAN_POINT('Ctrl Pts',(-3.63049858300006,12.2,-1.67952804400001));
#316461=CARTESIAN_POINT('Ctrl Pts',(-3.63049858300006,5.2,-1.67952804400001));
#316462=CARTESIAN_POINT('Ctrl Pts',(-3.63049858300006,2.2,-1.67952804400001));
#316463=CARTESIAN_POINT('Ctrl Pts',(-3.63076768500005,12.2,-1.67967187400002));
#316464=CARTESIAN_POINT('Ctrl Pts',(-3.63076768500005,5.2,-1.67967187400002));
#316465=CARTESIAN_POINT('Ctrl Pts',(-3.63076768500005,2.2,-1.67967187400002));
#316466=CARTESIAN_POINT('Ctrl Pts',(-3.63104258200006,12.2,-1.67981927100001));
#316467=CARTESIAN_POINT('Ctrl Pts',(-3.63104258200006,5.2,-1.67981927100001));
#316468=CARTESIAN_POINT('Ctrl Pts',(-3.63104258200006,2.2,-1.67981927100001));
#316469=CARTESIAN_POINT('Ctrl Pts',(-3.63132325200006,12.2,-1.67997024200002));
#316470=CARTESIAN_POINT('Ctrl Pts',(-3.63132325200006,5.2,-1.67997024200002));
#316471=CARTESIAN_POINT('Ctrl Pts',(-3.63132325200006,2.2,-1.67997024200002));
#316472=CARTESIAN_POINT('Ctrl Pts',(-3.63160967600006,12.2,-1.68012479700002));
#316473=CARTESIAN_POINT('Ctrl Pts',(-3.63160967600006,5.2,-1.68012479700002));
#316474=CARTESIAN_POINT('Ctrl Pts',(-3.63160967600006,2.2,-1.68012479700002));
#316475=CARTESIAN_POINT('Ctrl Pts',(-3.63190183000006,12.2,-1.68028294400001));
#316476=CARTESIAN_POINT('Ctrl Pts',(-3.63190183000006,5.2,-1.68028294400001));
#316477=CARTESIAN_POINT('Ctrl Pts',(-3.63190183000006,2.2,-1.68028294400001));
#316478=CARTESIAN_POINT('Ctrl Pts',(-3.63219969300006,12.2,-1.68044468900002));
#316479=CARTESIAN_POINT('Ctrl Pts',(-3.63219969300006,5.2,-1.68044468900002));
#316480=CARTESIAN_POINT('Ctrl Pts',(-3.63219969300006,2.2,-1.68044468900002));
#316481=CARTESIAN_POINT('Ctrl Pts',(-3.63250324400005,12.2,-1.68061004400001));
#316482=CARTESIAN_POINT('Ctrl Pts',(-3.63250324400005,5.2,-1.68061004400001));
#316483=CARTESIAN_POINT('Ctrl Pts',(-3.63250324400005,2.2,-1.68061004400001));
#316484=CARTESIAN_POINT('Ctrl Pts',(-3.63281246200006,12.2,-1.68077901500002));
#316485=CARTESIAN_POINT('Ctrl Pts',(-3.63281246200006,5.2,-1.68077901500002));
#316486=CARTESIAN_POINT('Ctrl Pts',(-3.63281246200006,2.2,-1.68077901500002));
#316487=CARTESIAN_POINT('Ctrl Pts',(-3.63312732600006,12.2,-1.68095161000001));
#316488=CARTESIAN_POINT('Ctrl Pts',(-3.63312732600006,5.2,-1.68095161000001));
#316489=CARTESIAN_POINT('Ctrl Pts',(-3.63312732600006,2.2,-1.68095161000001));
#316490=CARTESIAN_POINT('Ctrl Pts',(-3.63344781300006,12.2,-1.68112783800002));
#316491=CARTESIAN_POINT('Ctrl Pts',(-3.63344781300006,5.2,-1.68112783800002));
#316492=CARTESIAN_POINT('Ctrl Pts',(-3.63344781300006,2.2,-1.68112783800002));
#316493=CARTESIAN_POINT('Ctrl Pts',(-3.63377390500006,12.2,-1.68130770800001));
#316494=CARTESIAN_POINT('Ctrl Pts',(-3.63377390500006,5.2,-1.68130770800001));
#316495=CARTESIAN_POINT('Ctrl Pts',(-3.63377390500006,2.2,-1.68130770800001));
#316496=CARTESIAN_POINT('Ctrl Pts',(-3.63410557800006,12.2,-1.68149122600001));
#316497=CARTESIAN_POINT('Ctrl Pts',(-3.63410557800006,5.2,-1.68149122600001));
#316498=CARTESIAN_POINT('Ctrl Pts',(-3.63410557800006,2.2,-1.68149122600001));
#316499=CARTESIAN_POINT('Ctrl Pts',(-3.63444281300006,12.2,-1.68167840100002));
#316500=CARTESIAN_POINT('Ctrl Pts',(-3.63444281300006,5.2,-1.68167840100002));
#316501=CARTESIAN_POINT('Ctrl Pts',(-3.63444281300006,2.2,-1.68167840100002));
#316502=CARTESIAN_POINT('Ctrl Pts',(-3.63478558800006,12.2,-1.68186924100001));
#316503=CARTESIAN_POINT('Ctrl Pts',(-3.63478558800006,5.2,-1.68186924100001));
#316504=CARTESIAN_POINT('Ctrl Pts',(-3.63478558800006,2.2,-1.68186924100001));
#316505=CARTESIAN_POINT('Ctrl Pts',(-3.63513388200006,12.2,-1.68206375400001));
#316506=CARTESIAN_POINT('Ctrl Pts',(-3.63513388200006,5.2,-1.68206375400001));
#316507=CARTESIAN_POINT('Ctrl Pts',(-3.63513388200006,2.2,-1.68206375400001));
#316508=CARTESIAN_POINT('Ctrl Pts',(-3.63548767700006,12.2,-1.68226194600001));
#316509=CARTESIAN_POINT('Ctrl Pts',(-3.63548767700006,5.2,-1.68226194600001));
#316510=CARTESIAN_POINT('Ctrl Pts',(-3.63548767700006,2.2,-1.68226194600001));
#316511=CARTESIAN_POINT('Ctrl Pts',(-3.63584694800006,12.2,-1.68246382700001));
#316512=CARTESIAN_POINT('Ctrl Pts',(-3.63584694800006,5.2,-1.68246382700001));
#316513=CARTESIAN_POINT('Ctrl Pts',(-3.63584694800006,2.2,-1.68246382700001));
#316514=CARTESIAN_POINT('Ctrl Pts',(-3.63621167800006,12.2,-1.68266940500001));
#316515=CARTESIAN_POINT('Ctrl Pts',(-3.63621167800006,5.2,-1.68266940500001));
#316516=CARTESIAN_POINT('Ctrl Pts',(-3.63621167800006,2.2,-1.68266940500001));
#316517=CARTESIAN_POINT('Ctrl Pts',(-3.63658184400006,12.2,-1.68287868500002));
#316518=CARTESIAN_POINT('Ctrl Pts',(-3.63658184400006,5.2,-1.68287868500002));
#316519=CARTESIAN_POINT('Ctrl Pts',(-3.63658184400006,2.2,-1.68287868500002));
#316520=CARTESIAN_POINT('Ctrl Pts',(-3.63695742600005,12.2,-1.68309167800002));
#316521=CARTESIAN_POINT('Ctrl Pts',(-3.63695742600005,5.2,-1.68309167800002));
#316522=CARTESIAN_POINT('Ctrl Pts',(-3.63695742600005,2.2,-1.68309167800002));
#316523=CARTESIAN_POINT('Ctrl Pts',(-3.63733840400006,12.2,-1.68330838800001));
#316524=CARTESIAN_POINT('Ctrl Pts',(-3.63733840400006,5.2,-1.68330838800001));
#316525=CARTESIAN_POINT('Ctrl Pts',(-3.63733840400006,2.2,-1.68330838800001));
#316526=CARTESIAN_POINT('Ctrl Pts',(-3.63772475700006,12.2,-1.68352882600002));
#316527=CARTESIAN_POINT('Ctrl Pts',(-3.63772475700006,5.2,-1.68352882600002));
#316528=CARTESIAN_POINT('Ctrl Pts',(-3.63772475700006,2.2,-1.68352882600002));
#316529=CARTESIAN_POINT('Ctrl Pts',(-3.63811646600006,12.2,-1.68375299700001));
#316530=CARTESIAN_POINT('Ctrl Pts',(-3.63811646600006,5.2,-1.68375299700001));
#316531=CARTESIAN_POINT('Ctrl Pts',(-3.63811646600006,2.2,-1.68375299700001));
#316532=CARTESIAN_POINT('Ctrl Pts',(-3.63851350900006,12.2,-1.68398091000002));
#316533=CARTESIAN_POINT('Ctrl Pts',(-3.63851350900006,5.2,-1.68398091000002));
#316534=CARTESIAN_POINT('Ctrl Pts',(-3.63851350900006,2.2,-1.68398091000002));
#316535=CARTESIAN_POINT('Ctrl Pts',(-3.63891586600006,12.2,-1.68421257200002));
#316536=CARTESIAN_POINT('Ctrl Pts',(-3.63891586600006,5.2,-1.68421257200002));
#316537=CARTESIAN_POINT('Ctrl Pts',(-3.63891586600006,2.2,-1.68421257200002));
#316538=CARTESIAN_POINT('Ctrl Pts',(-3.63932351700006,12.2,-1.68444798900001));
#316539=CARTESIAN_POINT('Ctrl Pts',(-3.63932351700006,5.2,-1.68444798900001));
#316540=CARTESIAN_POINT('Ctrl Pts',(-3.63932351700006,2.2,-1.68444798900001));
#316541=CARTESIAN_POINT('Ctrl Pts',(-3.63973644200006,12.2,-1.68468717000001));
#316542=CARTESIAN_POINT('Ctrl Pts',(-3.63973644200006,5.2,-1.68468717000001));
#316543=CARTESIAN_POINT('Ctrl Pts',(-3.63973644200006,2.2,-1.68468717000001));
#316544=CARTESIAN_POINT('Ctrl Pts',(-3.64015462100006,12.2,-1.68493012200001));
#316545=CARTESIAN_POINT('Ctrl Pts',(-3.64015462100006,5.2,-1.68493012200001));
#316546=CARTESIAN_POINT('Ctrl Pts',(-3.64015462100006,2.2,-1.68493012200001));
#316547=CARTESIAN_POINT('Ctrl Pts',(-3.64057803400006,12.2,-1.68517685100001));
#316548=CARTESIAN_POINT('Ctrl Pts',(-3.64057803400006,5.2,-1.68517685100001));
#316549=CARTESIAN_POINT('Ctrl Pts',(-3.64057803400006,2.2,-1.68517685100001));
#316550=CARTESIAN_POINT('Ctrl Pts',(-3.64100666200006,12.2,-1.68542736500001));
#316551=CARTESIAN_POINT('Ctrl Pts',(-3.64100666200006,5.2,-1.68542736500001));
#316552=CARTESIAN_POINT('Ctrl Pts',(-3.64100666200006,2.2,-1.68542736500001));
#316553=CARTESIAN_POINT('Ctrl Pts',(-3.64144048200005,12.2,-1.68568167200001));
#316554=CARTESIAN_POINT('Ctrl Pts',(-3.64144048200005,5.2,-1.68568167200001));
#316555=CARTESIAN_POINT('Ctrl Pts',(-3.64144048200005,2.2,-1.68568167200001));
#316556=CARTESIAN_POINT('Ctrl Pts',(-3.64187947600006,12.2,-1.68593977800001));
#316557=CARTESIAN_POINT('Ctrl Pts',(-3.64187947600006,5.2,-1.68593977800001));
#316558=CARTESIAN_POINT('Ctrl Pts',(-3.64187947600006,2.2,-1.68593977800001));
#316559=CARTESIAN_POINT('Ctrl Pts',(-3.64232362600006,12.2,-1.68620168900001));
#316560=CARTESIAN_POINT('Ctrl Pts',(-3.64232362600006,5.2,-1.68620168900001));
#316561=CARTESIAN_POINT('Ctrl Pts',(-3.64232362600006,2.2,-1.68620168900001));
#316562=CARTESIAN_POINT('Ctrl Pts',(-3.64277290900006,12.2,-1.68646741400002));
#316563=CARTESIAN_POINT('Ctrl Pts',(-3.64277290900006,5.2,-1.68646741400002));
#316564=CARTESIAN_POINT('Ctrl Pts',(-3.64277290900006,2.2,-1.68646741400002));
#316565=CARTESIAN_POINT('Ctrl Pts',(-3.64322730700006,12.2,-1.68673696000001));
#316566=CARTESIAN_POINT('Ctrl Pts',(-3.64322730700006,5.2,-1.68673696000001));
#316567=CARTESIAN_POINT('Ctrl Pts',(-3.64322730700006,2.2,-1.68673696000001));
#316568=CARTESIAN_POINT('Ctrl Pts',(-3.64368680000006,12.2,-1.68701033200001));
#316569=CARTESIAN_POINT('Ctrl Pts',(-3.64368680000006,5.2,-1.68701033200001));
#316570=CARTESIAN_POINT('Ctrl Pts',(-3.64368680000006,2.2,-1.68701033200001));
#316571=CARTESIAN_POINT('Ctrl Pts',(-3.64415136800006,12.2,-1.68728753800002));
#316572=CARTESIAN_POINT('Ctrl Pts',(-3.64415136800006,5.2,-1.68728753800002));
#316573=CARTESIAN_POINT('Ctrl Pts',(-3.64415136800006,2.2,-1.68728753800002));
#316574=CARTESIAN_POINT('Ctrl Pts',(-3.64462099200006,12.2,-1.68756858400001));
#316575=CARTESIAN_POINT('Ctrl Pts',(-3.64462099200006,5.2,-1.68756858400001));
#316576=CARTESIAN_POINT('Ctrl Pts',(-3.64462099200006,2.2,-1.68756858400001));
#316577=CARTESIAN_POINT('Ctrl Pts',(-3.64509565300006,12.2,-1.68785347900001));
#316578=CARTESIAN_POINT('Ctrl Pts',(-3.64509565300006,5.2,-1.68785347900001));
#316579=CARTESIAN_POINT('Ctrl Pts',(-3.64509565300006,2.2,-1.68785347900001));
#316580=CARTESIAN_POINT('Ctrl Pts',(-3.64557533000006,12.2,-1.68814222700002));
#316581=CARTESIAN_POINT('Ctrl Pts',(-3.64557533000006,5.2,-1.68814222700002));
#316582=CARTESIAN_POINT('Ctrl Pts',(-3.64557533000006,2.2,-1.68814222700002));
#316583=CARTESIAN_POINT('Ctrl Pts',(-3.64606000500006,12.2,-1.68843483600002));
#316584=CARTESIAN_POINT('Ctrl Pts',(-3.64606000500006,5.2,-1.68843483600002));
#316585=CARTESIAN_POINT('Ctrl Pts',(-3.64606000500006,2.2,-1.68843483600002));
#316586=CARTESIAN_POINT('Ctrl Pts',(-3.64654965700006,12.2,-1.68873131300002));
#316587=CARTESIAN_POINT('Ctrl Pts',(-3.64654965700006,5.2,-1.68873131300002));
#316588=CARTESIAN_POINT('Ctrl Pts',(-3.64654965700006,2.2,-1.68873131300002));
#316589=CARTESIAN_POINT('Ctrl Pts',(-3.64704426900006,12.2,-1.68903166300002));
#316590=CARTESIAN_POINT('Ctrl Pts',(-3.64704426900006,5.2,-1.68903166300002));
#316591=CARTESIAN_POINT('Ctrl Pts',(-3.64704426900006,2.2,-1.68903166300002));
#316592=CARTESIAN_POINT('Ctrl Pts',(-3.64754381900006,12.2,-1.68933589500002));
#316593=CARTESIAN_POINT('Ctrl Pts',(-3.64754381900006,5.2,-1.68933589500002));
#316594=CARTESIAN_POINT('Ctrl Pts',(-3.64754381900006,2.2,-1.68933589500002));
#316595=CARTESIAN_POINT('Ctrl Pts',(-3.64804829100006,12.2,-1.68964401300002));
#316596=CARTESIAN_POINT('Ctrl Pts',(-3.64804829100006,5.2,-1.68964401300002));
#316597=CARTESIAN_POINT('Ctrl Pts',(-3.64804829100006,2.2,-1.68964401300002));
#316598=CARTESIAN_POINT('Ctrl Pts',(-3.64855766400006,12.2,-1.68995602500001));
#316599=CARTESIAN_POINT('Ctrl Pts',(-3.64855766400006,5.2,-1.68995602500001));
#316600=CARTESIAN_POINT('Ctrl Pts',(-3.64855766400006,2.2,-1.68995602500001));
#316601=CARTESIAN_POINT('Ctrl Pts',(-3.64907191800006,12.2,-1.69027193700002));
#316602=CARTESIAN_POINT('Ctrl Pts',(-3.64907191800006,5.2,-1.69027193700002));
#316603=CARTESIAN_POINT('Ctrl Pts',(-3.64907191800006,2.2,-1.69027193700002));
#316604=CARTESIAN_POINT('Ctrl Pts',(-3.64959103500006,12.2,-1.69059175500001));
#316605=CARTESIAN_POINT('Ctrl Pts',(-3.64959103500006,5.2,-1.69059175500001));
#316606=CARTESIAN_POINT('Ctrl Pts',(-3.64959103500006,2.2,-1.69059175500001));
#316607=CARTESIAN_POINT('Ctrl Pts',(-3.65011499700006,12.2,-1.69091548500001));
#316608=CARTESIAN_POINT('Ctrl Pts',(-3.65011499700006,5.2,-1.69091548500001));
#316609=CARTESIAN_POINT('Ctrl Pts',(-3.65011499700006,2.2,-1.69091548500001));
#316610=CARTESIAN_POINT('Ctrl Pts',(-3.65064378300006,12.2,-1.69124313400001));
#316611=CARTESIAN_POINT('Ctrl Pts',(-3.65064378300006,5.2,-1.69124313400001));
#316612=CARTESIAN_POINT('Ctrl Pts',(-3.65064378300006,2.2,-1.69124313400001));
#316613=CARTESIAN_POINT('Ctrl Pts',(-3.65117737500006,12.2,-1.69157470900001));
#316614=CARTESIAN_POINT('Ctrl Pts',(-3.65117737500006,5.2,-1.69157470900001));
#316615=CARTESIAN_POINT('Ctrl Pts',(-3.65117737500006,2.2,-1.69157470900001));
#316616=CARTESIAN_POINT('Ctrl Pts',(-3.65171575500006,12.2,-1.69191021500001));
#316617=CARTESIAN_POINT('Ctrl Pts',(-3.65171575500006,5.2,-1.69191021500001));
#316618=CARTESIAN_POINT('Ctrl Pts',(-3.65171575500006,2.2,-1.69191021500001));
#316619=CARTESIAN_POINT('Ctrl Pts',(-3.65225890200006,12.2,-1.69224966000002));
#316620=CARTESIAN_POINT('Ctrl Pts',(-3.65225890200006,5.2,-1.69224966000002));
#316621=CARTESIAN_POINT('Ctrl Pts',(-3.65225890200006,2.2,-1.69224966000002));
#316622=CARTESIAN_POINT('Ctrl Pts',(-3.65280680000006,12.2,-1.69259304600001));
#316623=CARTESIAN_POINT('Ctrl Pts',(-3.65280680000006,5.2,-1.69259304600001));
#316624=CARTESIAN_POINT('Ctrl Pts',(-3.65280680000006,2.2,-1.69259304600001));
#316625=CARTESIAN_POINT('Ctrl Pts',(-3.65335942900006,12.2,-1.69294038500002));
#316626=CARTESIAN_POINT('Ctrl Pts',(-3.65335942900006,5.2,-1.69294038500002));
#316627=CARTESIAN_POINT('Ctrl Pts',(-3.65335942900006,2.2,-1.69294038500002));
#316628=CARTESIAN_POINT('Ctrl Pts',(-3.65391676900006,12.2,-1.69329167700001));
#316629=CARTESIAN_POINT('Ctrl Pts',(-3.65391676900006,5.2,-1.69329167700001));
#316630=CARTESIAN_POINT('Ctrl Pts',(-3.65391676900006,2.2,-1.69329167700001));
#316631=CARTESIAN_POINT('Ctrl Pts',(-3.65447880300006,12.2,-1.69364693300002));
#316632=CARTESIAN_POINT('Ctrl Pts',(-3.65447880300006,5.2,-1.69364693300002));
#316633=CARTESIAN_POINT('Ctrl Pts',(-3.65447880300006,2.2,-1.69364693300002));
#316634=CARTESIAN_POINT('Ctrl Pts',(-3.65504551200006,12.2,-1.69400615400002));
#316635=CARTESIAN_POINT('Ctrl Pts',(-3.65504551200006,5.2,-1.69400615400002));
#316636=CARTESIAN_POINT('Ctrl Pts',(-3.65504551200006,2.2,-1.69400615400002));
#316637=CARTESIAN_POINT('Ctrl Pts',(-3.65561687800006,12.2,-1.69436935100002));
#316638=CARTESIAN_POINT('Ctrl Pts',(-3.65561687800006,5.2,-1.69436935100002));
#316639=CARTESIAN_POINT('Ctrl Pts',(-3.65561687800006,2.2,-1.69436935100002));
#316640=CARTESIAN_POINT('Ctrl Pts',(-3.65619288200006,12.2,-1.69473652600002));
#316641=CARTESIAN_POINT('Ctrl Pts',(-3.65619288200006,5.2,-1.69473652600002));
#316642=CARTESIAN_POINT('Ctrl Pts',(-3.65619288200006,2.2,-1.69473652600002));
#316643=CARTESIAN_POINT('Ctrl Pts',(-3.65677350500006,12.2,-1.69510768800002));
#316644=CARTESIAN_POINT('Ctrl Pts',(-3.65677350500006,5.2,-1.69510768800002));
#316645=CARTESIAN_POINT('Ctrl Pts',(-3.65677350500006,2.2,-1.69510768800002));
#316646=CARTESIAN_POINT('Ctrl Pts',(-3.65735873000006,12.2,-1.69548284100001));
#316647=CARTESIAN_POINT('Ctrl Pts',(-3.65735873000006,5.2,-1.69548284100001));
#316648=CARTESIAN_POINT('Ctrl Pts',(-3.65735873000006,2.2,-1.69548284100001));
#316649=CARTESIAN_POINT('Ctrl Pts',(-3.65794853700006,12.2,-1.69586199000001));
#316650=CARTESIAN_POINT('Ctrl Pts',(-3.65794853700006,5.2,-1.69586199000001));
#316651=CARTESIAN_POINT('Ctrl Pts',(-3.65794853700006,2.2,-1.69586199000001));
#316652=CARTESIAN_POINT('Ctrl Pts',(-3.65854290900006,12.2,-1.69624514300001));
#316653=CARTESIAN_POINT('Ctrl Pts',(-3.65854290900006,5.2,-1.69624514300001));
#316654=CARTESIAN_POINT('Ctrl Pts',(-3.65854290900006,2.2,-1.69624514300001));
#316655=CARTESIAN_POINT('Ctrl Pts',(-3.65914182700006,12.2,-1.69663230300001));
#316656=CARTESIAN_POINT('Ctrl Pts',(-3.65914182700006,5.2,-1.69663230300001));
#316657=CARTESIAN_POINT('Ctrl Pts',(-3.65914182700006,2.2,-1.69663230300001));
#316658=CARTESIAN_POINT('Ctrl Pts',(-3.65974527300006,12.2,-1.69702347900001));
#316659=CARTESIAN_POINT('Ctrl Pts',(-3.65974527300006,5.2,-1.69702347900001));
#316660=CARTESIAN_POINT('Ctrl Pts',(-3.65974527300006,2.2,-1.69702347900001));
#316661=CARTESIAN_POINT('Ctrl Pts',(-3.66035322900006,12.2,-1.69741867300001));
#316662=CARTESIAN_POINT('Ctrl Pts',(-3.66035322900006,5.2,-1.69741867300001));
#316663=CARTESIAN_POINT('Ctrl Pts',(-3.66035322900006,2.2,-1.69741867300001));
#316664=CARTESIAN_POINT('Ctrl Pts',(-3.66096567700006,12.2,-1.69781789400002));
#316665=CARTESIAN_POINT('Ctrl Pts',(-3.66096567700006,5.2,-1.69781789400002));
#316666=CARTESIAN_POINT('Ctrl Pts',(-3.66096567700006,2.2,-1.69781789400002));
#316667=CARTESIAN_POINT('Ctrl Pts',(-3.66158259800006,12.2,-1.69822114400001));
#316668=CARTESIAN_POINT('Ctrl Pts',(-3.66158259800006,5.2,-1.69822114400001));
#316669=CARTESIAN_POINT('Ctrl Pts',(-3.66158259800006,2.2,-1.69822114400001));
#316670=CARTESIAN_POINT('Ctrl Pts',(-3.66220397600006,12.2,-1.69862843100002));
#316671=CARTESIAN_POINT('Ctrl Pts',(-3.66220397600006,5.2,-1.69862843100002));
#316672=CARTESIAN_POINT('Ctrl Pts',(-3.66220397600006,2.2,-1.69862843100002));
#316673=CARTESIAN_POINT('Ctrl Pts',(-3.66282979000006,12.2,-1.69903976000001));
#316674=CARTESIAN_POINT('Ctrl Pts',(-3.66282979000006,5.2,-1.69903976000001));
#316675=CARTESIAN_POINT('Ctrl Pts',(-3.66282979000006,2.2,-1.69903976000001));
#316676=CARTESIAN_POINT('Ctrl Pts',(-3.66346002500006,12.2,-1.69945513700001));
#316677=CARTESIAN_POINT('Ctrl Pts',(-3.66346002500006,5.2,-1.69945513700001));
#316678=CARTESIAN_POINT('Ctrl Pts',(-3.66346002500006,2.2,-1.69945513700001));
#316679=CARTESIAN_POINT('Ctrl Pts',(-3.66409466100006,12.2,-1.69987456500001));
#316680=CARTESIAN_POINT('Ctrl Pts',(-3.66409466100006,5.2,-1.69987456500001));
#316681=CARTESIAN_POINT('Ctrl Pts',(-3.66409466100006,2.2,-1.69987456500001));
#316682=CARTESIAN_POINT('Ctrl Pts',(-3.66473368100006,12.2,-1.70029805200001));
#316683=CARTESIAN_POINT('Ctrl Pts',(-3.66473368100006,5.2,-1.70029805200001));
#316684=CARTESIAN_POINT('Ctrl Pts',(-3.66473368100006,2.2,-1.70029805200001));
#316685=CARTESIAN_POINT('Ctrl Pts',(-3.66537706800006,12.2,-1.70072560100001));
#316686=CARTESIAN_POINT('Ctrl Pts',(-3.66537706800006,5.2,-1.70072560100001));
#316687=CARTESIAN_POINT('Ctrl Pts',(-3.66537706800006,2.2,-1.70072560100001));
#316688=CARTESIAN_POINT('Ctrl Pts',(-3.66602480300006,12.2,-1.70115722000002));
#316689=CARTESIAN_POINT('Ctrl Pts',(-3.66602480300006,5.2,-1.70115722000002));
#316690=CARTESIAN_POINT('Ctrl Pts',(-3.66602480300006,2.2,-1.70115722000002));
#316691=CARTESIAN_POINT('Ctrl Pts',(-3.66667686900006,12.2,-1.70159291300001));
#316692=CARTESIAN_POINT('Ctrl Pts',(-3.66667686900006,5.2,-1.70159291300001));
#316693=CARTESIAN_POINT('Ctrl Pts',(-3.66667686900006,2.2,-1.70159291300001));
#316694=CARTESIAN_POINT('Ctrl Pts',(-3.66733324700006,12.2,-1.70203268400002));
#316695=CARTESIAN_POINT('Ctrl Pts',(-3.66733324700006,5.2,-1.70203268400002));
#316696=CARTESIAN_POINT('Ctrl Pts',(-3.66733324700006,2.2,-1.70203268400002));
#316697=CARTESIAN_POINT('Ctrl Pts',(-3.66799392100006,12.2,-1.70247654000002));
#316698=CARTESIAN_POINT('Ctrl Pts',(-3.66799392100006,5.2,-1.70247654000002));
#316699=CARTESIAN_POINT('Ctrl Pts',(-3.66799392100006,2.2,-1.70247654000002));
#316700=CARTESIAN_POINT('Ctrl Pts',(-3.66865887300006,12.2,-1.70292448500001));
#316701=CARTESIAN_POINT('Ctrl Pts',(-3.66865887300006,5.2,-1.70292448500001));
#316702=CARTESIAN_POINT('Ctrl Pts',(-3.66865887300006,2.2,-1.70292448500001));
#316703=CARTESIAN_POINT('Ctrl Pts',(-3.66932808400006,12.2,-1.70337652400002));
#316704=CARTESIAN_POINT('Ctrl Pts',(-3.66932808400006,5.2,-1.70337652400002));
#316705=CARTESIAN_POINT('Ctrl Pts',(-3.66932808400006,2.2,-1.70337652400002));
#316706=CARTESIAN_POINT('Ctrl Pts',(-3.67000153900006,12.2,-1.70383266200002));
#316707=CARTESIAN_POINT('Ctrl Pts',(-3.67000153900006,5.2,-1.70383266200002));
#316708=CARTESIAN_POINT('Ctrl Pts',(-3.67000153900006,2.2,-1.70383266200002));
#316709=CARTESIAN_POINT('Ctrl Pts',(-3.67067921900006,12.2,-1.70429290600001));
#316710=CARTESIAN_POINT('Ctrl Pts',(-3.67067921900006,5.2,-1.70429290600001));
#316711=CARTESIAN_POINT('Ctrl Pts',(-3.67067921900006,2.2,-1.70429290600001));
#316712=CARTESIAN_POINT('Ctrl Pts',(-3.67136110600006,12.2,-1.70475725900001));
#316713=CARTESIAN_POINT('Ctrl Pts',(-3.67136110600006,5.2,-1.70475725900001));
#316714=CARTESIAN_POINT('Ctrl Pts',(-3.67136110600006,2.2,-1.70475725900001));
#316715=CARTESIAN_POINT('Ctrl Pts',(-3.67204718400005,12.2,-1.70522572600001));
#316716=CARTESIAN_POINT('Ctrl Pts',(-3.67204718400005,5.2,-1.70522572600001));
#316717=CARTESIAN_POINT('Ctrl Pts',(-3.67204718400005,2.2,-1.70522572600001));
#316718=CARTESIAN_POINT('Ctrl Pts',(-3.67273743400006,12.2,-1.70569831200002));
#316719=CARTESIAN_POINT('Ctrl Pts',(-3.67273743400006,5.2,-1.70569831200002));
#316720=CARTESIAN_POINT('Ctrl Pts',(-3.67273743400006,2.2,-1.70569831200002));
#316721=CARTESIAN_POINT('Ctrl Pts',(-3.67343184100006,12.2,-1.70617502300002));
#316722=CARTESIAN_POINT('Ctrl Pts',(-3.67343184100006,5.2,-1.70617502300002));
#316723=CARTESIAN_POINT('Ctrl Pts',(-3.67343184100006,2.2,-1.70617502300002));
#316724=CARTESIAN_POINT('Ctrl Pts',(-3.67413038600006,12.2,-1.70665586300002));
#316725=CARTESIAN_POINT('Ctrl Pts',(-3.67413038600006,5.2,-1.70665586300002));
#316726=CARTESIAN_POINT('Ctrl Pts',(-3.67413038600006,2.2,-1.70665586300002));
#316727=CARTESIAN_POINT('Ctrl Pts',(-3.67483305200006,12.2,-1.70714083700001));
#316728=CARTESIAN_POINT('Ctrl Pts',(-3.67483305200006,5.2,-1.70714083700001));
#316729=CARTESIAN_POINT('Ctrl Pts',(-3.67483305200006,2.2,-1.70714083700001));
#316730=CARTESIAN_POINT('Ctrl Pts',(-3.67553982200006,12.2,-1.70762995000001));
#316731=CARTESIAN_POINT('Ctrl Pts',(-3.67553982200006,5.2,-1.70762995000001));
#316732=CARTESIAN_POINT('Ctrl Pts',(-3.67553982200006,2.2,-1.70762995000001));
#316733=CARTESIAN_POINT('Ctrl Pts',(-3.67625067900006,12.2,-1.70812320600001));
#316734=CARTESIAN_POINT('Ctrl Pts',(-3.67625067900006,5.2,-1.70812320600001));
#316735=CARTESIAN_POINT('Ctrl Pts',(-3.67625067900006,2.2,-1.70812320600001));
#316736=CARTESIAN_POINT('Ctrl Pts',(-3.67696560600006,12.2,-1.70862061000001));
#316737=CARTESIAN_POINT('Ctrl Pts',(-3.67696560600006,5.2,-1.70862061000001));
#316738=CARTESIAN_POINT('Ctrl Pts',(-3.67696560600006,2.2,-1.70862061000001));
#316739=CARTESIAN_POINT('Ctrl Pts',(-3.67768458500006,12.2,-1.70912216700001));
#316740=CARTESIAN_POINT('Ctrl Pts',(-3.67768458500006,5.2,-1.70912216700001));
#316741=CARTESIAN_POINT('Ctrl Pts',(-3.67768458500006,2.2,-1.70912216700001));
#316742=CARTESIAN_POINT('Ctrl Pts',(-3.67840760000006,12.2,-1.70962788200002));
#316743=CARTESIAN_POINT('Ctrl Pts',(-3.67840760000006,5.2,-1.70962788200002));
#316744=CARTESIAN_POINT('Ctrl Pts',(-3.67840760000006,2.2,-1.70962788200002));
#316745=CARTESIAN_POINT('Ctrl Pts',(-3.67913463400006,12.2,-1.71013775900001));
#316746=CARTESIAN_POINT('Ctrl Pts',(-3.67913463400006,5.2,-1.71013775900001));
#316747=CARTESIAN_POINT('Ctrl Pts',(-3.67913463400006,2.2,-1.71013775900001));
#316748=CARTESIAN_POINT('Ctrl Pts',(-3.67986567000006,12.2,-1.71065180300001));
#316749=CARTESIAN_POINT('Ctrl Pts',(-3.67986567000006,5.2,-1.71065180300001));
#316750=CARTESIAN_POINT('Ctrl Pts',(-3.67986567000006,2.2,-1.71065180300001));
#316751=CARTESIAN_POINT('Ctrl Pts',(-3.68060069000006,12.2,-1.71117001800001));
#316752=CARTESIAN_POINT('Ctrl Pts',(-3.68060069000006,5.2,-1.71117001800001));
#316753=CARTESIAN_POINT('Ctrl Pts',(-3.68060069000006,2.2,-1.71117001800001));
#316754=CARTESIAN_POINT('Ctrl Pts',(-3.68133967700006,12.2,-1.71169240800001));
#316755=CARTESIAN_POINT('Ctrl Pts',(-3.68133967700006,5.2,-1.71169240800001));
#316756=CARTESIAN_POINT('Ctrl Pts',(-3.68133967700006,2.2,-1.71169240800001));
#316757=CARTESIAN_POINT('Ctrl Pts',(-3.68208261700006,12.2,-1.71221897900002));
#316758=CARTESIAN_POINT('Ctrl Pts',(-3.68208261700006,5.2,-1.71221897900002));
#316759=CARTESIAN_POINT('Ctrl Pts',(-3.68208261700006,2.2,-1.71221897900002));
#316760=CARTESIAN_POINT('Ctrl Pts',(-3.68282949100006,12.2,-1.71274973600001));
#316761=CARTESIAN_POINT('Ctrl Pts',(-3.68282949100006,5.2,-1.71274973600001));
#316762=CARTESIAN_POINT('Ctrl Pts',(-3.68282949100006,2.2,-1.71274973600001));
#316763=CARTESIAN_POINT('Ctrl Pts',(-3.68358028100006,12.2,-1.71328468000001));
#316764=CARTESIAN_POINT('Ctrl Pts',(-3.68358028100006,5.2,-1.71328468000001));
#316765=CARTESIAN_POINT('Ctrl Pts',(-3.68358028100006,2.2,-1.71328468000001));
#316766=CARTESIAN_POINT('Ctrl Pts',(-3.68433497400006,12.2,-1.71382381800001));
#316767=CARTESIAN_POINT('Ctrl Pts',(-3.68433497400006,5.2,-1.71382381800001));
#316768=CARTESIAN_POINT('Ctrl Pts',(-3.68433497400006,2.2,-1.71382381800001));
#316769=CARTESIAN_POINT('Ctrl Pts',(-3.68509354900006,12.2,-1.71436715500001));
#316770=CARTESIAN_POINT('Ctrl Pts',(-3.68509354900006,5.2,-1.71436715500001));
#316771=CARTESIAN_POINT('Ctrl Pts',(-3.68509354900006,2.2,-1.71436715500001));
#316772=CARTESIAN_POINT('Ctrl Pts',(-3.68585599300006,12.2,-1.71491469300001));
#316773=CARTESIAN_POINT('Ctrl Pts',(-3.68585599300006,5.2,-1.71491469300001));
#316774=CARTESIAN_POINT('Ctrl Pts',(-3.68585599300006,2.2,-1.71491469300001));
#316775=CARTESIAN_POINT('Ctrl Pts',(-3.68662228700006,12.2,-1.71546643800002));
#316776=CARTESIAN_POINT('Ctrl Pts',(-3.68662228700006,5.2,-1.71546643800002));
#316777=CARTESIAN_POINT('Ctrl Pts',(-3.68662228700006,2.2,-1.71546643800002));
#316778=CARTESIAN_POINT('Ctrl Pts',(-3.68739241600006,12.2,-1.71602239300002));
#316779=CARTESIAN_POINT('Ctrl Pts',(-3.68739241600006,5.2,-1.71602239300002));
#316780=CARTESIAN_POINT('Ctrl Pts',(-3.68739241600006,2.2,-1.71602239300002));
#316781=CARTESIAN_POINT('Ctrl Pts',(-3.68816636300005,12.2,-1.71658256400002));
#316782=CARTESIAN_POINT('Ctrl Pts',(-3.68816636300005,5.2,-1.71658256400002));
#316783=CARTESIAN_POINT('Ctrl Pts',(-3.68816636300005,2.2,-1.71658256400002));
#316784=CARTESIAN_POINT('Ctrl Pts',(-3.68894411100006,12.2,-1.71714695400001));
#316785=CARTESIAN_POINT('Ctrl Pts',(-3.68894411100006,5.2,-1.71714695400001));
#316786=CARTESIAN_POINT('Ctrl Pts',(-3.68894411100006,2.2,-1.71714695400001));
#316787=CARTESIAN_POINT('Ctrl Pts',(-3.68972564300006,12.2,-1.71771556700001));
#316788=CARTESIAN_POINT('Ctrl Pts',(-3.68972564300006,5.2,-1.71771556700001));
#316789=CARTESIAN_POINT('Ctrl Pts',(-3.68972564300006,2.2,-1.71771556700001));
#316790=CARTESIAN_POINT('Ctrl Pts',(-3.69051094500006,12.2,-1.71828840700002));
#316791=CARTESIAN_POINT('Ctrl Pts',(-3.69051094500006,5.2,-1.71828840700002));
#316792=CARTESIAN_POINT('Ctrl Pts',(-3.69051094500006,2.2,-1.71828840700002));
#316793=CARTESIAN_POINT('Ctrl Pts',(-3.69129999800006,12.2,-1.71886548000002));
#316794=CARTESIAN_POINT('Ctrl Pts',(-3.69129999800006,5.2,-1.71886548000002));
#316795=CARTESIAN_POINT('Ctrl Pts',(-3.69129999800006,2.2,-1.71886548000002));
#316796=CARTESIAN_POINT('Ctrl Pts',(-3.69209278600006,12.2,-1.71944678700001));
#316797=CARTESIAN_POINT('Ctrl Pts',(-3.69209278600006,5.2,-1.71944678700001));
#316798=CARTESIAN_POINT('Ctrl Pts',(-3.69209278600006,2.2,-1.71944678700001));
#316799=CARTESIAN_POINT('Ctrl Pts',(-3.69288929500006,12.2,-1.72003233500002));
#316800=CARTESIAN_POINT('Ctrl Pts',(-3.69288929500006,5.2,-1.72003233500002));
#316801=CARTESIAN_POINT('Ctrl Pts',(-3.69288929500006,2.2,-1.72003233500002));
#316802=CARTESIAN_POINT('Ctrl Pts',(-3.69368950600006,12.2,-1.72062212600002));
#316803=CARTESIAN_POINT('Ctrl Pts',(-3.69368950600006,5.2,-1.72062212600002));
#316804=CARTESIAN_POINT('Ctrl Pts',(-3.69368950600006,2.2,-1.72062212600002));
#316805=CARTESIAN_POINT('Ctrl Pts',(-3.69449340500006,12.2,-1.72121616400001));
#316806=CARTESIAN_POINT('Ctrl Pts',(-3.69449340500006,5.2,-1.72121616400001));
#316807=CARTESIAN_POINT('Ctrl Pts',(-3.69449340500006,2.2,-1.72121616400001));
#316808=CARTESIAN_POINT('Ctrl Pts',(-3.69530097400006,12.2,-1.72181445400001));
#316809=CARTESIAN_POINT('Ctrl Pts',(-3.69530097400006,5.2,-1.72181445400001));
#316810=CARTESIAN_POINT('Ctrl Pts',(-3.69530097400006,2.2,-1.72181445400001));
#316811=CARTESIAN_POINT('Ctrl Pts',(-3.69611219600006,12.2,-1.72241700100002));
#316812=CARTESIAN_POINT('Ctrl Pts',(-3.69611219600006,5.2,-1.72241700100002));
#316813=CARTESIAN_POINT('Ctrl Pts',(-3.69611219600006,2.2,-1.72241700100002));
#316814=CARTESIAN_POINT('Ctrl Pts',(-3.69692705800006,12.2,-1.72302380600001));
#316815=CARTESIAN_POINT('Ctrl Pts',(-3.69692705800006,5.2,-1.72302380600001));
#316816=CARTESIAN_POINT('Ctrl Pts',(-3.69692705800006,2.2,-1.72302380600001));
#316817=CARTESIAN_POINT('Ctrl Pts',(-3.69774554200006,12.2,-1.72363487400002));
#316818=CARTESIAN_POINT('Ctrl Pts',(-3.69774554200006,5.2,-1.72363487400002));
#316819=CARTESIAN_POINT('Ctrl Pts',(-3.69774554200006,2.2,-1.72363487400002));
#316820=CARTESIAN_POINT('Ctrl Pts',(-3.69856763300006,12.2,-1.72425021000001));
#316821=CARTESIAN_POINT('Ctrl Pts',(-3.69856763300006,5.2,-1.72425021000001));
#316822=CARTESIAN_POINT('Ctrl Pts',(-3.69856763300006,2.2,-1.72425021000001));
#316823=CARTESIAN_POINT('Ctrl Pts',(-3.69939331300006,12.2,-1.72486981600001));
#316824=CARTESIAN_POINT('Ctrl Pts',(-3.69939331300006,5.2,-1.72486981600001));
#316825=CARTESIAN_POINT('Ctrl Pts',(-3.69939331300006,2.2,-1.72486981600001));
#316826=CARTESIAN_POINT('Ctrl Pts',(-3.70022256800006,12.2,-1.72549369700001));
#316827=CARTESIAN_POINT('Ctrl Pts',(-3.70022256800006,5.2,-1.72549369700001));
#316828=CARTESIAN_POINT('Ctrl Pts',(-3.70022256800006,2.2,-1.72549369700001));
#316829=CARTESIAN_POINT('Ctrl Pts',(-3.70105538100006,12.2,-1.72612185600002));
#316830=CARTESIAN_POINT('Ctrl Pts',(-3.70105538100006,5.2,-1.72612185600002));
#316831=CARTESIAN_POINT('Ctrl Pts',(-3.70105538100006,2.2,-1.72612185600002));
#316832=CARTESIAN_POINT('Ctrl Pts',(-3.70189173600005,12.2,-1.72675429800002));
#316833=CARTESIAN_POINT('Ctrl Pts',(-3.70189173600005,5.2,-1.72675429800002));
#316834=CARTESIAN_POINT('Ctrl Pts',(-3.70189173600005,2.2,-1.72675429800002));
#316835=CARTESIAN_POINT('Ctrl Pts',(-3.70273161800006,12.2,-1.72739102500001));
#316836=CARTESIAN_POINT('Ctrl Pts',(-3.70273161800006,5.2,-1.72739102500001));
#316837=CARTESIAN_POINT('Ctrl Pts',(-3.70273161800006,2.2,-1.72739102500001));
#316838=CARTESIAN_POINT('Ctrl Pts',(-3.70357501000006,12.2,-1.72803204100001));
#316839=CARTESIAN_POINT('Ctrl Pts',(-3.70357501000006,5.2,-1.72803204100001));
#316840=CARTESIAN_POINT('Ctrl Pts',(-3.70357501000006,2.2,-1.72803204100001));
#316841=CARTESIAN_POINT('Ctrl Pts',(-3.70442189700006,12.2,-1.72867735000001));
#316842=CARTESIAN_POINT('Ctrl Pts',(-3.70442189700006,5.2,-1.72867735000001));
#316843=CARTESIAN_POINT('Ctrl Pts',(-3.70442189700006,2.2,-1.72867735000001));
#316844=CARTESIAN_POINT('Ctrl Pts',(-3.70527226300006,12.2,-1.72932695700001));
#316845=CARTESIAN_POINT('Ctrl Pts',(-3.70527226300006,5.2,-1.72932695700001));
#316846=CARTESIAN_POINT('Ctrl Pts',(-3.70527226300006,2.2,-1.72932695700001));
#316847=CARTESIAN_POINT('Ctrl Pts',(-3.70612609200006,12.2,-1.72998086300002));
#316848=CARTESIAN_POINT('Ctrl Pts',(-3.70612609200006,5.2,-1.72998086300002));
#316849=CARTESIAN_POINT('Ctrl Pts',(-3.70612609200006,2.2,-1.72998086300002));
#316850=CARTESIAN_POINT('Ctrl Pts',(-3.70698336900006,12.2,-1.73063907300001));
#316851=CARTESIAN_POINT('Ctrl Pts',(-3.70698336900006,5.2,-1.73063907300001));
#316852=CARTESIAN_POINT('Ctrl Pts',(-3.70698336900006,2.2,-1.73063907300001));
#316853=CARTESIAN_POINT('Ctrl Pts',(-3.70784407800006,12.2,-1.73130159000001));
#316854=CARTESIAN_POINT('Ctrl Pts',(-3.70784407800006,5.2,-1.73130159000001));
#316855=CARTESIAN_POINT('Ctrl Pts',(-3.70784407800006,2.2,-1.73130159000001));
#316856=CARTESIAN_POINT('Ctrl Pts',(-3.70870820300006,12.2,-1.73196841700001));
#316857=CARTESIAN_POINT('Ctrl Pts',(-3.70870820300006,5.2,-1.73196841700001));
#316858=CARTESIAN_POINT('Ctrl Pts',(-3.70870820300006,2.2,-1.73196841700001));
#316859=CARTESIAN_POINT('Ctrl Pts',(-3.70957572800005,12.2,-1.73263955900001));
#316860=CARTESIAN_POINT('Ctrl Pts',(-3.70957572800005,5.2,-1.73263955900001));
#316861=CARTESIAN_POINT('Ctrl Pts',(-3.70957572800005,2.2,-1.73263955900001));
#316862=CARTESIAN_POINT('Ctrl Pts',(-3.71044663900006,12.2,-1.73331501800002));
#316863=CARTESIAN_POINT('Ctrl Pts',(-3.71044663900006,5.2,-1.73331501800002));
#316864=CARTESIAN_POINT('Ctrl Pts',(-3.71044663900006,2.2,-1.73331501800002));
#316865=CARTESIAN_POINT('Ctrl Pts',(-3.71132091800006,12.2,-1.73399479900001));
#316866=CARTESIAN_POINT('Ctrl Pts',(-3.71132091800006,5.2,-1.73399479900001));
#316867=CARTESIAN_POINT('Ctrl Pts',(-3.71132091800006,2.2,-1.73399479900001));
#316868=CARTESIAN_POINT('Ctrl Pts',(-3.71219855200006,12.2,-1.73467890300001));
#316869=CARTESIAN_POINT('Ctrl Pts',(-3.71219855200006,5.2,-1.73467890300001));
#316870=CARTESIAN_POINT('Ctrl Pts',(-3.71219855200006,2.2,-1.73467890300001));
#316871=CARTESIAN_POINT('Ctrl Pts',(-3.71307952400006,12.2,-1.73536733500002));
#316872=CARTESIAN_POINT('Ctrl Pts',(-3.71307952400006,5.2,-1.73536733500002));
#316873=CARTESIAN_POINT('Ctrl Pts',(-3.71307952400006,2.2,-1.73536733500002));
#316874=CARTESIAN_POINT('Ctrl Pts',(-3.71396382000006,12.2,-1.73606009800002));
#316875=CARTESIAN_POINT('Ctrl Pts',(-3.71396382000006,5.2,-1.73606009800002));
#316876=CARTESIAN_POINT('Ctrl Pts',(-3.71396382000006,2.2,-1.73606009800002));
#316877=CARTESIAN_POINT('Ctrl Pts',(-3.71485142300005,12.2,-1.73675719400002));
#316878=CARTESIAN_POINT('Ctrl Pts',(-3.71485142300005,5.2,-1.73675719400002));
#316879=CARTESIAN_POINT('Ctrl Pts',(-3.71485142300005,2.2,-1.73675719400002));
#316880=CARTESIAN_POINT('Ctrl Pts',(-3.71574231800006,12.2,-1.73745862900001));
#316881=CARTESIAN_POINT('Ctrl Pts',(-3.71574231800006,5.2,-1.73745862900001));
#316882=CARTESIAN_POINT('Ctrl Pts',(-3.71574231800006,2.2,-1.73745862900001));
#316883=CARTESIAN_POINT('Ctrl Pts',(-3.71663649000006,12.2,-1.73816440400001));
#316884=CARTESIAN_POINT('Ctrl Pts',(-3.71663649000006,5.2,-1.73816440400001));
#316885=CARTESIAN_POINT('Ctrl Pts',(-3.71663649000006,2.2,-1.73816440400001));
#316886=CARTESIAN_POINT('Ctrl Pts',(-3.71753392300006,12.2,-1.73887452300002));
#316887=CARTESIAN_POINT('Ctrl Pts',(-3.71753392300006,5.2,-1.73887452300002));
#316888=CARTESIAN_POINT('Ctrl Pts',(-3.71753392300006,2.2,-1.73887452300002));
#316889=CARTESIAN_POINT('Ctrl Pts',(-3.71843460200005,12.2,-1.73958898900001));
#316890=CARTESIAN_POINT('Ctrl Pts',(-3.71843460200005,5.2,-1.73958898900001));
#316891=CARTESIAN_POINT('Ctrl Pts',(-3.71843460200005,2.2,-1.73958898900001));
#316892=CARTESIAN_POINT('Ctrl Pts',(-3.71933851300006,12.2,-1.74030780600001));
#316893=CARTESIAN_POINT('Ctrl Pts',(-3.71933851300006,5.2,-1.74030780600001));
#316894=CARTESIAN_POINT('Ctrl Pts',(-3.71933851300006,2.2,-1.74030780600001));
#316895=CARTESIAN_POINT('Ctrl Pts',(-3.72024564000006,12.2,-1.74103097500002));
#316896=CARTESIAN_POINT('Ctrl Pts',(-3.72024564000006,5.2,-1.74103097500002));
#316897=CARTESIAN_POINT('Ctrl Pts',(-3.72024564000006,2.2,-1.74103097500002));
#316898=CARTESIAN_POINT('Ctrl Pts',(-3.72115596700006,12.2,-1.74175850000001));
#316899=CARTESIAN_POINT('Ctrl Pts',(-3.72115596700006,5.2,-1.74175850000001));
#316900=CARTESIAN_POINT('Ctrl Pts',(-3.72115596700006,2.2,-1.74175850000001));
#316901=CARTESIAN_POINT('Ctrl Pts',(-3.72206947900006,12.2,-1.74249038600002));
#316902=CARTESIAN_POINT('Ctrl Pts',(-3.72206947900006,5.2,-1.74249038600002));
#316903=CARTESIAN_POINT('Ctrl Pts',(-3.72206947900006,2.2,-1.74249038600002));
#316904=CARTESIAN_POINT('Ctrl Pts',(-3.72298616200006,12.2,-1.74322663300002));
#316905=CARTESIAN_POINT('Ctrl Pts',(-3.72298616200006,5.2,-1.74322663300002));
#316906=CARTESIAN_POINT('Ctrl Pts',(-3.72298616200006,2.2,-1.74322663300002));
#316907=CARTESIAN_POINT('Ctrl Pts',(-3.72390600000006,12.2,-1.74396724600001));
#316908=CARTESIAN_POINT('Ctrl Pts',(-3.72390600000006,5.2,-1.74396724600001));
#316909=CARTESIAN_POINT('Ctrl Pts',(-3.72390600000006,2.2,-1.74396724600001));
#316910=CARTESIAN_POINT('Ctrl Pts',(-3.72482897800006,12.2,-1.74471222700001));
#316911=CARTESIAN_POINT('Ctrl Pts',(-3.72482897800006,5.2,-1.74471222700001));
#316912=CARTESIAN_POINT('Ctrl Pts',(-3.72482897800006,2.2,-1.74471222700001));
#316913=CARTESIAN_POINT('Ctrl Pts',(-3.72575508100006,12.2,-1.74546158000001));
#316914=CARTESIAN_POINT('Ctrl Pts',(-3.72575508100006,5.2,-1.74546158000001));
#316915=CARTESIAN_POINT('Ctrl Pts',(-3.72575508100006,2.2,-1.74546158000001));
#316916=CARTESIAN_POINT('Ctrl Pts',(-3.72668429500006,12.2,-1.74621530700001));
#316917=CARTESIAN_POINT('Ctrl Pts',(-3.72668429500006,5.2,-1.74621530700001));
#316918=CARTESIAN_POINT('Ctrl Pts',(-3.72668429500006,2.2,-1.74621530700001));
#316919=CARTESIAN_POINT('Ctrl Pts',(-3.72761660300006,12.2,-1.74697341100002));
#316920=CARTESIAN_POINT('Ctrl Pts',(-3.72761660300006,5.2,-1.74697341100002));
#316921=CARTESIAN_POINT('Ctrl Pts',(-3.72761660300006,2.2,-1.74697341100002));
#316922=CARTESIAN_POINT('Ctrl Pts',(-3.72855199100006,12.2,-1.74773589500001));
#316923=CARTESIAN_POINT('Ctrl Pts',(-3.72855199100006,5.2,-1.74773589500001));
#316924=CARTESIAN_POINT('Ctrl Pts',(-3.72855199100006,2.2,-1.74773589500001));
#316925=CARTESIAN_POINT('Ctrl Pts',(-3.72949044500006,12.2,-1.74850276200001));
#316926=CARTESIAN_POINT('Ctrl Pts',(-3.72949044500006,5.2,-1.74850276200001));
#316927=CARTESIAN_POINT('Ctrl Pts',(-3.72949044500006,2.2,-1.74850276200001));
#316928=CARTESIAN_POINT('Ctrl Pts',(-3.73043194900006,12.2,-1.74927401600002));
#316929=CARTESIAN_POINT('Ctrl Pts',(-3.73043194900006,5.2,-1.74927401600002));
#316930=CARTESIAN_POINT('Ctrl Pts',(-3.73043194900006,2.2,-1.74927401600002));
#316931=CARTESIAN_POINT('Ctrl Pts',(-3.73137648800006,12.2,-1.75004965700001));
#316932=CARTESIAN_POINT('Ctrl Pts',(-3.73137648800006,5.2,-1.75004965700001));
#316933=CARTESIAN_POINT('Ctrl Pts',(-3.73137648800006,2.2,-1.75004965700001));
#316934=CARTESIAN_POINT('Ctrl Pts',(-3.73232404900006,12.2,-1.75082969000002));
#316935=CARTESIAN_POINT('Ctrl Pts',(-3.73232404900006,5.2,-1.75082969000002));
#316936=CARTESIAN_POINT('Ctrl Pts',(-3.73232404900006,2.2,-1.75082969000002));
#316937=CARTESIAN_POINT('Ctrl Pts',(-3.73327461500006,12.2,-1.75161411600001));
#316938=CARTESIAN_POINT('Ctrl Pts',(-3.73327461500006,5.2,-1.75161411600001));
#316939=CARTESIAN_POINT('Ctrl Pts',(-3.73327461500006,2.2,-1.75161411600001));
#316940=CARTESIAN_POINT('Ctrl Pts',(-3.73422817300006,12.2,-1.75240294000002));
#316941=CARTESIAN_POINT('Ctrl Pts',(-3.73422817300006,5.2,-1.75240294000002));
#316942=CARTESIAN_POINT('Ctrl Pts',(-3.73422817300006,2.2,-1.75240294000002));
#316943=CARTESIAN_POINT('Ctrl Pts',(-3.73518470700006,12.2,-1.75319616300001));
#316944=CARTESIAN_POINT('Ctrl Pts',(-3.73518470700006,5.2,-1.75319616300001));
#316945=CARTESIAN_POINT('Ctrl Pts',(-3.73518470700006,2.2,-1.75319616300001));
#316946=CARTESIAN_POINT('Ctrl Pts',(-3.73614420300005,12.2,-1.75399378800002));
#316947=CARTESIAN_POINT('Ctrl Pts',(-3.73614420300005,5.2,-1.75399378800002));
#316948=CARTESIAN_POINT('Ctrl Pts',(-3.73614420300005,2.2,-1.75399378800002));
#316949=CARTESIAN_POINT('Ctrl Pts',(-3.73710664500006,12.2,-1.75479581800001));
#316950=CARTESIAN_POINT('Ctrl Pts',(-3.73710664500006,5.2,-1.75479581800001));
#316951=CARTESIAN_POINT('Ctrl Pts',(-3.73710664500006,2.2,-1.75479581800001));
#316952=CARTESIAN_POINT('Ctrl Pts',(-3.73807202000005,12.2,-1.75560225600002));
#316953=CARTESIAN_POINT('Ctrl Pts',(-3.73807202000005,5.2,-1.75560225600002));
#316954=CARTESIAN_POINT('Ctrl Pts',(-3.73807202000005,2.2,-1.75560225600002));
#316955=CARTESIAN_POINT('Ctrl Pts',(-3.73904031300006,12.2,-1.75641310200001));
#316956=CARTESIAN_POINT('Ctrl Pts',(-3.73904031300006,5.2,-1.75641310200001));
#316957=CARTESIAN_POINT('Ctrl Pts',(-3.73904031300006,2.2,-1.75641310200001));
#316958=CARTESIAN_POINT('Ctrl Pts',(-3.74001150900006,12.2,-1.75722836200002));
#316959=CARTESIAN_POINT('Ctrl Pts',(-3.74001150900006,5.2,-1.75722836200002));
#316960=CARTESIAN_POINT('Ctrl Pts',(-3.74001150900006,2.2,-1.75722836200002));
#316961=CARTESIAN_POINT('Ctrl Pts',(-3.74098559300006,12.2,-1.75804803700002));
#316962=CARTESIAN_POINT('Ctrl Pts',(-3.74098559300006,5.2,-1.75804803700002));
#316963=CARTESIAN_POINT('Ctrl Pts',(-3.74098559300006,2.2,-1.75804803700002));
#316964=CARTESIAN_POINT('Ctrl Pts',(-3.74196255300006,12.2,-1.75887213000001));
#316965=CARTESIAN_POINT('Ctrl Pts',(-3.74196255300006,5.2,-1.75887213000001));
#316966=CARTESIAN_POINT('Ctrl Pts',(-3.74196255300006,2.2,-1.75887213000001));
#316967=CARTESIAN_POINT('Ctrl Pts',(-3.74294237100006,12.2,-1.75970064200001));
#316968=CARTESIAN_POINT('Ctrl Pts',(-3.74294237100006,5.2,-1.75970064200001));
#316969=CARTESIAN_POINT('Ctrl Pts',(-3.74294237100006,2.2,-1.75970064200001));
#316970=CARTESIAN_POINT('Ctrl Pts',(-3.74392503400006,12.2,-1.76053357700001));
#316971=CARTESIAN_POINT('Ctrl Pts',(-3.74392503400006,5.2,-1.76053357700001));
#316972=CARTESIAN_POINT('Ctrl Pts',(-3.74392503400006,2.2,-1.76053357700001));
#316973=CARTESIAN_POINT('Ctrl Pts',(-3.74491052900006,12.2,-1.76137093700001));
#316974=CARTESIAN_POINT('Ctrl Pts',(-3.74491052900006,5.2,-1.76137093700001));
#316975=CARTESIAN_POINT('Ctrl Pts',(-3.74491052900006,2.2,-1.76137093700001));
#316976=CARTESIAN_POINT('Ctrl Pts',(-3.74589884000006,12.2,-1.76221272500001));
#316977=CARTESIAN_POINT('Ctrl Pts',(-3.74589884000006,5.2,-1.76221272500001));
#316978=CARTESIAN_POINT('Ctrl Pts',(-3.74589884000006,2.2,-1.76221272500001));
#316979=CARTESIAN_POINT('Ctrl Pts',(-3.74688995300006,12.2,-1.76305894300001));
#316980=CARTESIAN_POINT('Ctrl Pts',(-3.74688995300006,5.2,-1.76305894300001));
#316981=CARTESIAN_POINT('Ctrl Pts',(-3.74688995300006,2.2,-1.76305894300001));
#316982=CARTESIAN_POINT('Ctrl Pts',(-3.74788385300006,12.2,-1.76390959200001));
#316983=CARTESIAN_POINT('Ctrl Pts',(-3.74788385300006,5.2,-1.76390959200001));
#316984=CARTESIAN_POINT('Ctrl Pts',(-3.74788385300006,2.2,-1.76390959200001));
#316985=CARTESIAN_POINT('Ctrl Pts',(-3.74888052700006,12.2,-1.76476467600001));
#316986=CARTESIAN_POINT('Ctrl Pts',(-3.74888052700006,5.2,-1.76476467600001));
#316987=CARTESIAN_POINT('Ctrl Pts',(-3.74888052700006,2.2,-1.76476467600001));
#316988=CARTESIAN_POINT('Ctrl Pts',(-3.74987996000006,12.2,-1.76562419800002));
#316989=CARTESIAN_POINT('Ctrl Pts',(-3.74987996000006,5.2,-1.76562419800002));
#316990=CARTESIAN_POINT('Ctrl Pts',(-3.74987996000006,2.2,-1.76562419800002));
#316991=CARTESIAN_POINT('Ctrl Pts',(-3.75088213700006,12.2,-1.76648815800001));
#316992=CARTESIAN_POINT('Ctrl Pts',(-3.75088213700006,5.2,-1.76648815800001));
#316993=CARTESIAN_POINT('Ctrl Pts',(-3.75088213700006,2.2,-1.76648815800001));
#316994=CARTESIAN_POINT('Ctrl Pts',(-3.75188704500006,12.2,-1.76735656000002));
#316995=CARTESIAN_POINT('Ctrl Pts',(-3.75188704500006,5.2,-1.76735656000002));
#316996=CARTESIAN_POINT('Ctrl Pts',(-3.75188704500006,2.2,-1.76735656000002));
#316997=CARTESIAN_POINT('Ctrl Pts',(-3.75289466900006,12.2,-1.76822940400001));
#316998=CARTESIAN_POINT('Ctrl Pts',(-3.75289466900006,5.2,-1.76822940400001));
#316999=CARTESIAN_POINT('Ctrl Pts',(-3.75289466900006,2.2,-1.76822940400001));
#317000=CARTESIAN_POINT('Ctrl Pts',(-3.75390499500006,12.2,-1.76910669600002));
#317001=CARTESIAN_POINT('Ctrl Pts',(-3.75390499500006,5.2,-1.76910669600002));
#317002=CARTESIAN_POINT('Ctrl Pts',(-3.75390499500006,2.2,-1.76910669600002));
#317003=CARTESIAN_POINT('Ctrl Pts',(-3.75491800900006,12.2,-1.76998843600002));
#317004=CARTESIAN_POINT('Ctrl Pts',(-3.75491800900006,5.2,-1.76998843600002));
#317005=CARTESIAN_POINT('Ctrl Pts',(-3.75491800900006,2.2,-1.76998843600002));
#317006=CARTESIAN_POINT('Ctrl Pts',(-3.75593369800006,12.2,-1.77087462600001));
#317007=CARTESIAN_POINT('Ctrl Pts',(-3.75593369800006,5.2,-1.77087462600001));
#317008=CARTESIAN_POINT('Ctrl Pts',(-3.75593369800006,2.2,-1.77087462600001));
#317009=CARTESIAN_POINT('Ctrl Pts',(-3.75695204500006,12.2,-1.77176526800002));
#317010=CARTESIAN_POINT('Ctrl Pts',(-3.75695204500006,5.2,-1.77176526800002));
#317011=CARTESIAN_POINT('Ctrl Pts',(-3.75695204500006,2.2,-1.77176526800002));
#317012=CARTESIAN_POINT('Ctrl Pts',(-3.75797303800006,12.2,-1.77266036500002));
#317013=CARTESIAN_POINT('Ctrl Pts',(-3.75797303800006,5.2,-1.77266036500002));
#317014=CARTESIAN_POINT('Ctrl Pts',(-3.75797303800006,2.2,-1.77266036500002));
#317015=CARTESIAN_POINT('Ctrl Pts',(-3.75899666400006,12.2,-1.77355991900002));
#317016=CARTESIAN_POINT('Ctrl Pts',(-3.75899666400006,5.2,-1.77355991900002));
#317017=CARTESIAN_POINT('Ctrl Pts',(-3.75899666400006,2.2,-1.77355991900002));
#317018=CARTESIAN_POINT('Ctrl Pts',(-3.76002290600006,12.2,-1.77446393100002));
#317019=CARTESIAN_POINT('Ctrl Pts',(-3.76002290600006,5.2,-1.77446393100002));
#317020=CARTESIAN_POINT('Ctrl Pts',(-3.76002290600006,2.2,-1.77446393100002));
#317021=CARTESIAN_POINT('Ctrl Pts',(-3.76105175200006,12.2,-1.77537240500001));
#317022=CARTESIAN_POINT('Ctrl Pts',(-3.76105175200006,5.2,-1.77537240500001));
#317023=CARTESIAN_POINT('Ctrl Pts',(-3.76105175200006,2.2,-1.77537240500001));
#317024=CARTESIAN_POINT('Ctrl Pts',(-3.76208318700006,12.2,-1.77628534100001));
#317025=CARTESIAN_POINT('Ctrl Pts',(-3.76208318700006,5.2,-1.77628534100001));
#317026=CARTESIAN_POINT('Ctrl Pts',(-3.76208318700006,2.2,-1.77628534100001));
#317027=CARTESIAN_POINT('Ctrl Pts',(-3.76311719900006,12.2,-1.77720274300002));
#317028=CARTESIAN_POINT('Ctrl Pts',(-3.76311719900006,5.2,-1.77720274300002));
#317029=CARTESIAN_POINT('Ctrl Pts',(-3.76311719900006,2.2,-1.77720274300002));
#317030=CARTESIAN_POINT('Ctrl Pts',(-3.76415377300006,12.2,-1.77812461100002));
#317031=CARTESIAN_POINT('Ctrl Pts',(-3.76415377300006,5.2,-1.77812461100002));
#317032=CARTESIAN_POINT('Ctrl Pts',(-3.76415377300006,2.2,-1.77812461100002));
#317033=CARTESIAN_POINT('Ctrl Pts',(-3.76519289400005,12.2,-1.77905094800002));
#317034=CARTESIAN_POINT('Ctrl Pts',(-3.76519289400005,5.2,-1.77905094800002));
#317035=CARTESIAN_POINT('Ctrl Pts',(-3.76519289400005,2.2,-1.77905094800002));
#317036=CARTESIAN_POINT('Ctrl Pts',(-3.76623455000006,12.2,-1.77998175700001));
#317037=CARTESIAN_POINT('Ctrl Pts',(-3.76623455000006,5.2,-1.77998175700001));
#317038=CARTESIAN_POINT('Ctrl Pts',(-3.76623455000006,2.2,-1.77998175700001));
#317039=CARTESIAN_POINT('Ctrl Pts',(-3.76727872400005,12.2,-1.78091703800002));
#317040=CARTESIAN_POINT('Ctrl Pts',(-3.76727872400005,5.2,-1.78091703800002));
#317041=CARTESIAN_POINT('Ctrl Pts',(-3.76727872400005,2.2,-1.78091703800002));
#317042=CARTESIAN_POINT('Ctrl Pts',(-3.76832540600006,12.2,-1.78185679400002));
#317043=CARTESIAN_POINT('Ctrl Pts',(-3.76832540600006,5.2,-1.78185679400002));
#317044=CARTESIAN_POINT('Ctrl Pts',(-3.76832540600006,2.2,-1.78185679400002));
#317045=CARTESIAN_POINT('Ctrl Pts',(-3.76937458100006,12.2,-1.78280102600001));
#317046=CARTESIAN_POINT('Ctrl Pts',(-3.76937458100006,5.2,-1.78280102600001));
#317047=CARTESIAN_POINT('Ctrl Pts',(-3.76937458100006,2.2,-1.78280102600001));
#317048=CARTESIAN_POINT('Ctrl Pts',(-3.77042623500006,12.2,-1.78374973700001));
#317049=CARTESIAN_POINT('Ctrl Pts',(-3.77042623500006,5.2,-1.78374973700001));
#317050=CARTESIAN_POINT('Ctrl Pts',(-3.77042623500006,2.2,-1.78374973700001));
#317051=CARTESIAN_POINT('Ctrl Pts',(-3.77148035400006,12.2,-1.78470292800001));
#317052=CARTESIAN_POINT('Ctrl Pts',(-3.77148035400006,5.2,-1.78470292800001));
#317053=CARTESIAN_POINT('Ctrl Pts',(-3.77148035400006,2.2,-1.78470292800001));
#317054=CARTESIAN_POINT('Ctrl Pts',(-3.77253692400005,12.2,-1.78566060100001));
#317055=CARTESIAN_POINT('Ctrl Pts',(-3.77253692400005,5.2,-1.78566060100001));
#317056=CARTESIAN_POINT('Ctrl Pts',(-3.77253692400005,2.2,-1.78566060100001));
#317057=CARTESIAN_POINT('Ctrl Pts',(-3.77359593200006,12.2,-1.78662275800002));
#317058=CARTESIAN_POINT('Ctrl Pts',(-3.77359593200006,5.2,-1.78662275800002));
#317059=CARTESIAN_POINT('Ctrl Pts',(-3.77359593200006,2.2,-1.78662275800002));
#317060=CARTESIAN_POINT('Ctrl Pts',(-3.77465736400006,12.2,-1.78758940200002));
#317061=CARTESIAN_POINT('Ctrl Pts',(-3.77465736400006,5.2,-1.78758940200002));
#317062=CARTESIAN_POINT('Ctrl Pts',(-3.77465736400006,2.2,-1.78758940200002));
#317063=CARTESIAN_POINT('Ctrl Pts',(-3.77572120600006,12.2,-1.78856053200001));
#317064=CARTESIAN_POINT('Ctrl Pts',(-3.77572120600006,5.2,-1.78856053200001));
#317065=CARTESIAN_POINT('Ctrl Pts',(-3.77572120600006,2.2,-1.78856053200001));
#317066=CARTESIAN_POINT('Ctrl Pts',(-3.77678744700006,12.2,-1.78953615200002));
#317067=CARTESIAN_POINT('Ctrl Pts',(-3.77678744700006,5.2,-1.78953615200002));
#317068=CARTESIAN_POINT('Ctrl Pts',(-3.77678744700006,2.2,-1.78953615200002));
#317069=CARTESIAN_POINT('Ctrl Pts',(-3.77785607000006,12.2,-1.79051626300001));
#317070=CARTESIAN_POINT('Ctrl Pts',(-3.77785607000006,5.2,-1.79051626300001));
#317071=CARTESIAN_POINT('Ctrl Pts',(-3.77785607000006,2.2,-1.79051626300001));
#317072=CARTESIAN_POINT('Ctrl Pts',(-3.77892706200006,12.2,-1.79150086600002));
#317073=CARTESIAN_POINT('Ctrl Pts',(-3.77892706200006,5.2,-1.79150086600002));
#317074=CARTESIAN_POINT('Ctrl Pts',(-3.77892706200006,2.2,-1.79150086600002));
#317075=CARTESIAN_POINT('Ctrl Pts',(-3.78000041200006,12.2,-1.79248996300001));
#317076=CARTESIAN_POINT('Ctrl Pts',(-3.78000041200006,5.2,-1.79248996300001));
#317077=CARTESIAN_POINT('Ctrl Pts',(-3.78000041200006,2.2,-1.79248996300001));
#317078=CARTESIAN_POINT('Ctrl Pts',(-3.78107610400006,12.2,-1.79348355800002));
#317079=CARTESIAN_POINT('Ctrl Pts',(-3.78107610400006,5.2,-1.79348355800002));
#317080=CARTESIAN_POINT('Ctrl Pts',(-3.78107610400006,2.2,-1.79348355800002));
#317081=CARTESIAN_POINT('Ctrl Pts',(-3.78215412600006,12.2,-1.79448164800001));
#317082=CARTESIAN_POINT('Ctrl Pts',(-3.78215412600006,5.2,-1.79448164800001));
#317083=CARTESIAN_POINT('Ctrl Pts',(-3.78215412600006,2.2,-1.79448164800001));
#317084=CARTESIAN_POINT('Ctrl Pts',(-3.78323446300006,12.2,-1.79548423900001));
#317085=CARTESIAN_POINT('Ctrl Pts',(-3.78323446300006,5.2,-1.79548423900001));
#317086=CARTESIAN_POINT('Ctrl Pts',(-3.78323446300006,2.2,-1.79548423900001));
#317087=CARTESIAN_POINT('Ctrl Pts',(-3.78431710400006,12.2,-1.79649133000002));
#317088=CARTESIAN_POINT('Ctrl Pts',(-3.78431710400006,5.2,-1.79649133000002));
#317089=CARTESIAN_POINT('Ctrl Pts',(-3.78431710400006,2.2,-1.79649133000002));
#317090=CARTESIAN_POINT('Ctrl Pts',(-3.78540203300005,12.2,-1.79750292300001));
#317091=CARTESIAN_POINT('Ctrl Pts',(-3.78540203300005,5.2,-1.79750292300001));
#317092=CARTESIAN_POINT('Ctrl Pts',(-3.78540203300005,2.2,-1.79750292300001));
#317093=CARTESIAN_POINT('Ctrl Pts',(-3.78648923700006,12.2,-1.79851902000001));
#317094=CARTESIAN_POINT('Ctrl Pts',(-3.78648923700006,5.2,-1.79851902000001));
#317095=CARTESIAN_POINT('Ctrl Pts',(-3.78648923700006,2.2,-1.79851902000001));
#317096=CARTESIAN_POINT('Ctrl Pts',(-3.78757870600006,12.2,-1.79953962300001));
#317097=CARTESIAN_POINT('Ctrl Pts',(-3.78757870600006,5.2,-1.79953962300001));
#317098=CARTESIAN_POINT('Ctrl Pts',(-3.78757870600006,2.2,-1.79953962300001));
#317099=CARTESIAN_POINT('Ctrl Pts',(-3.78867042200006,12.2,-1.80056473100001));
#317100=CARTESIAN_POINT('Ctrl Pts',(-3.78867042200006,5.2,-1.80056473100001));
#317101=CARTESIAN_POINT('Ctrl Pts',(-3.78867042200006,2.2,-1.80056473100001));
#317102=CARTESIAN_POINT('Ctrl Pts',(-3.78976437500006,12.2,-1.80159435000002));
#317103=CARTESIAN_POINT('Ctrl Pts',(-3.78976437500006,5.2,-1.80159435000002));
#317104=CARTESIAN_POINT('Ctrl Pts',(-3.78976437500006,2.2,-1.80159435000002));
#317105=CARTESIAN_POINT('Ctrl Pts',(-3.79086055000006,12.2,-1.80262847700002));
#317106=CARTESIAN_POINT('Ctrl Pts',(-3.79086055000006,5.2,-1.80262847700002));
#317107=CARTESIAN_POINT('Ctrl Pts',(-3.79086055000006,2.2,-1.80262847700002));
#317108=CARTESIAN_POINT('Ctrl Pts',(-3.79195893400006,12.2,-1.80366711600001));
#317109=CARTESIAN_POINT('Ctrl Pts',(-3.79195893400006,5.2,-1.80366711600001));
#317110=CARTESIAN_POINT('Ctrl Pts',(-3.79195893400006,2.2,-1.80366711600001));
#317111=CARTESIAN_POINT('Ctrl Pts',(-3.79305951500006,12.2,-1.80471026800001));
#317112=CARTESIAN_POINT('Ctrl Pts',(-3.79305951500006,5.2,-1.80471026800001));
#317113=CARTESIAN_POINT('Ctrl Pts',(-3.79305951500006,2.2,-1.80471026800001));
#317114=CARTESIAN_POINT('Ctrl Pts',(-3.79416227800006,12.2,-1.80575793300001));
#317115=CARTESIAN_POINT('Ctrl Pts',(-3.79416227800006,5.2,-1.80575793300001));
#317116=CARTESIAN_POINT('Ctrl Pts',(-3.79416227800006,2.2,-1.80575793300001));
#317117=CARTESIAN_POINT('Ctrl Pts',(-3.79526721200006,12.2,-1.80681011400001));
#317118=CARTESIAN_POINT('Ctrl Pts',(-3.79526721200006,5.2,-1.80681011400001));
#317119=CARTESIAN_POINT('Ctrl Pts',(-3.79526721200006,2.2,-1.80681011400001));
#317120=CARTESIAN_POINT('Ctrl Pts',(-3.79637430300006,12.2,-1.80786681200001));
#317121=CARTESIAN_POINT('Ctrl Pts',(-3.79637430300006,5.2,-1.80786681200001));
#317122=CARTESIAN_POINT('Ctrl Pts',(-3.79637430300006,2.2,-1.80786681200001));
#317123=CARTESIAN_POINT('Ctrl Pts',(-3.79748353500006,12.2,-1.80892802800001));
#317124=CARTESIAN_POINT('Ctrl Pts',(-3.79748353500006,5.2,-1.80892802800001));
#317125=CARTESIAN_POINT('Ctrl Pts',(-3.79748353500006,2.2,-1.80892802800001));
#317126=CARTESIAN_POINT('Ctrl Pts',(-3.79859490000006,12.2,-1.80999376300001));
#317127=CARTESIAN_POINT('Ctrl Pts',(-3.79859490000006,5.2,-1.80999376300001));
#317128=CARTESIAN_POINT('Ctrl Pts',(-3.79859490000006,2.2,-1.80999376300001));
#317129=CARTESIAN_POINT('Ctrl Pts',(-3.79970838200006,12.2,-1.81106401900001));
#317130=CARTESIAN_POINT('Ctrl Pts',(-3.79970838200006,5.2,-1.81106401900001));
#317131=CARTESIAN_POINT('Ctrl Pts',(-3.79970838200006,2.2,-1.81106401900001));
#317132=CARTESIAN_POINT('Ctrl Pts',(-3.80082396700006,12.2,-1.81213879700001));
#317133=CARTESIAN_POINT('Ctrl Pts',(-3.80082396700006,5.2,-1.81213879700001));
#317134=CARTESIAN_POINT('Ctrl Pts',(-3.80082396700006,2.2,-1.81213879700001));
#317135=CARTESIAN_POINT('Ctrl Pts',(-3.80194164400006,12.2,-1.81321809900002));
#317136=CARTESIAN_POINT('Ctrl Pts',(-3.80194164400006,5.2,-1.81321809900002));
#317137=CARTESIAN_POINT('Ctrl Pts',(-3.80194164400006,2.2,-1.81321809900002));
#317138=CARTESIAN_POINT('Ctrl Pts',(-3.80306140000005,12.2,-1.81430192500001));
#317139=CARTESIAN_POINT('Ctrl Pts',(-3.80306140000005,5.2,-1.81430192500001));
#317140=CARTESIAN_POINT('Ctrl Pts',(-3.80306140000005,2.2,-1.81430192500001));
#317141=CARTESIAN_POINT('Ctrl Pts',(-3.80418322100006,12.2,-1.81539027700001));
#317142=CARTESIAN_POINT('Ctrl Pts',(-3.80418322100006,5.2,-1.81539027700001));
#317143=CARTESIAN_POINT('Ctrl Pts',(-3.80418322100006,2.2,-1.81539027700001));
#317144=CARTESIAN_POINT('Ctrl Pts',(-3.80530709400006,12.2,-1.81648315500002));
#317145=CARTESIAN_POINT('Ctrl Pts',(-3.80530709400006,5.2,-1.81648315500002));
#317146=CARTESIAN_POINT('Ctrl Pts',(-3.80530709400006,2.2,-1.81648315500002));
#317147=CARTESIAN_POINT('Ctrl Pts',(-3.80643300700005,12.2,-1.81758056100001));
#317148=CARTESIAN_POINT('Ctrl Pts',(-3.80643300700005,5.2,-1.81758056100001));
#317149=CARTESIAN_POINT('Ctrl Pts',(-3.80643300700005,2.2,-1.81758056100001));
#317150=CARTESIAN_POINT('Ctrl Pts',(-3.80756094600006,12.2,-1.81868249800001));
#317151=CARTESIAN_POINT('Ctrl Pts',(-3.80756094600006,5.2,-1.81868249800001));
#317152=CARTESIAN_POINT('Ctrl Pts',(-3.80756094600006,2.2,-1.81868249800001));
#317153=CARTESIAN_POINT('Ctrl Pts',(-3.80869089900005,12.2,-1.81978896400001));
#317154=CARTESIAN_POINT('Ctrl Pts',(-3.80869089900005,5.2,-1.81978896400001));
#317155=CARTESIAN_POINT('Ctrl Pts',(-3.80869089900005,2.2,-1.81978896400001));
#317156=CARTESIAN_POINT('Ctrl Pts',(-3.80982285300006,12.2,-1.82089996100002));
#317157=CARTESIAN_POINT('Ctrl Pts',(-3.80982285300006,5.2,-1.82089996100002));
#317158=CARTESIAN_POINT('Ctrl Pts',(-3.80982285300006,2.2,-1.82089996100002));
#317159=CARTESIAN_POINT('Ctrl Pts',(-3.81095679500006,12.2,-1.82201549200002));
#317160=CARTESIAN_POINT('Ctrl Pts',(-3.81095679500006,5.2,-1.82201549200002));
#317161=CARTESIAN_POINT('Ctrl Pts',(-3.81095679500006,2.2,-1.82201549200002));
#317162=CARTESIAN_POINT('Ctrl Pts',(-3.81209271100006,12.2,-1.82313555600001));
#317163=CARTESIAN_POINT('Ctrl Pts',(-3.81209271100006,5.2,-1.82313555600001));
#317164=CARTESIAN_POINT('Ctrl Pts',(-3.81209271100006,2.2,-1.82313555600001));
#317165=CARTESIAN_POINT('Ctrl Pts',(-3.81323059200006,12.2,-1.82426015500001));
#317166=CARTESIAN_POINT('Ctrl Pts',(-3.81323059200006,5.2,-1.82426015500001));
#317167=CARTESIAN_POINT('Ctrl Pts',(-3.81323059200006,2.2,-1.82426015500001));
#317168=CARTESIAN_POINT('Ctrl Pts',(-3.81437042100006,12.2,-1.82538929000001));
#317169=CARTESIAN_POINT('Ctrl Pts',(-3.81437042100006,5.2,-1.82538929000001));
#317170=CARTESIAN_POINT('Ctrl Pts',(-3.81437042100006,2.2,-1.82538929000001));
#317171=CARTESIAN_POINT('Ctrl Pts',(-3.81551218700006,12.2,-1.82652296200001));
#317172=CARTESIAN_POINT('Ctrl Pts',(-3.81551218700006,5.2,-1.82652296200001));
#317173=CARTESIAN_POINT('Ctrl Pts',(-3.81551218700006,2.2,-1.82652296200001));
#317174=CARTESIAN_POINT('Ctrl Pts',(-3.81665587800006,12.2,-1.82766117100002));
#317175=CARTESIAN_POINT('Ctrl Pts',(-3.81665587800006,5.2,-1.82766117100002));
#317176=CARTESIAN_POINT('Ctrl Pts',(-3.81665587800006,2.2,-1.82766117100002));
#317177=CARTESIAN_POINT('Ctrl Pts',(-3.81780147900006,12.2,-1.82880391900001));
#317178=CARTESIAN_POINT('Ctrl Pts',(-3.81780147900006,5.2,-1.82880391900001));
#317179=CARTESIAN_POINT('Ctrl Pts',(-3.81780147900006,2.2,-1.82880391900001));
#317180=CARTESIAN_POINT('Ctrl Pts',(-3.81894898000006,12.2,-1.82995120700001));
#317181=CARTESIAN_POINT('Ctrl Pts',(-3.81894898000006,5.2,-1.82995120700001));
#317182=CARTESIAN_POINT('Ctrl Pts',(-3.81894898000006,2.2,-1.82995120700001));
#317183=CARTESIAN_POINT('Ctrl Pts',(-3.82009836800006,12.2,-1.83110303500001));
#317184=CARTESIAN_POINT('Ctrl Pts',(-3.82009836800006,5.2,-1.83110303500001));
#317185=CARTESIAN_POINT('Ctrl Pts',(-3.82009836800006,2.2,-1.83110303500001));
#317186=CARTESIAN_POINT('Ctrl Pts',(-3.82124962800006,12.2,-1.83225940600002));
#317187=CARTESIAN_POINT('Ctrl Pts',(-3.82124962800006,5.2,-1.83225940600002));
#317188=CARTESIAN_POINT('Ctrl Pts',(-3.82124962800006,2.2,-1.83225940600002));
#317189=CARTESIAN_POINT('Ctrl Pts',(-3.82240274900006,12.2,-1.83342031800001));
#317190=CARTESIAN_POINT('Ctrl Pts',(-3.82240274900006,5.2,-1.83342031800001));
#317191=CARTESIAN_POINT('Ctrl Pts',(-3.82240274900006,2.2,-1.83342031800001));
#317192=CARTESIAN_POINT('Ctrl Pts',(-3.82355772000006,12.2,-1.83458577400001));
#317193=CARTESIAN_POINT('Ctrl Pts',(-3.82355772000006,5.2,-1.83458577400001));
#317194=CARTESIAN_POINT('Ctrl Pts',(-3.82355772000006,2.2,-1.83458577400001));
#317195=CARTESIAN_POINT('Ctrl Pts',(-3.82471452500006,12.2,-1.83575577400001));
#317196=CARTESIAN_POINT('Ctrl Pts',(-3.82471452500006,5.2,-1.83575577400001));
#317197=CARTESIAN_POINT('Ctrl Pts',(-3.82471452500006,2.2,-1.83575577400001));
#317198=CARTESIAN_POINT('Ctrl Pts',(-3.82587315500006,12.2,-1.83693032100001));
#317199=CARTESIAN_POINT('Ctrl Pts',(-3.82587315500006,5.2,-1.83693032100001));
#317200=CARTESIAN_POINT('Ctrl Pts',(-3.82587315500006,2.2,-1.83693032100001));
#317201=CARTESIAN_POINT('Ctrl Pts',(-3.82703359500006,12.2,-1.83810941200001));
#317202=CARTESIAN_POINT('Ctrl Pts',(-3.82703359500006,5.2,-1.83810941200001));
#317203=CARTESIAN_POINT('Ctrl Pts',(-3.82703359500006,2.2,-1.83810941200001));
#317204=CARTESIAN_POINT('Ctrl Pts',(-3.82819583300006,12.2,-1.83929305100001));
#317205=CARTESIAN_POINT('Ctrl Pts',(-3.82819583300006,5.2,-1.83929305100001));
#317206=CARTESIAN_POINT('Ctrl Pts',(-3.82819583300006,2.2,-1.83929305100001));
#317207=CARTESIAN_POINT('Ctrl Pts',(-3.82935985800006,12.2,-1.84048123600002));
#317208=CARTESIAN_POINT('Ctrl Pts',(-3.82935985800006,5.2,-1.84048123600002));
#317209=CARTESIAN_POINT('Ctrl Pts',(-3.82935985800006,2.2,-1.84048123600002));
#317210=CARTESIAN_POINT('Ctrl Pts',(-3.83052565500006,12.2,-1.84167397100001));
#317211=CARTESIAN_POINT('Ctrl Pts',(-3.83052565500006,5.2,-1.84167397100001));
#317212=CARTESIAN_POINT('Ctrl Pts',(-3.83052565500006,2.2,-1.84167397100001));
#317213=CARTESIAN_POINT('Ctrl Pts',(-3.83169321400006,12.2,-1.84287125400001));
#317214=CARTESIAN_POINT('Ctrl Pts',(-3.83169321400006,5.2,-1.84287125400001));
#317215=CARTESIAN_POINT('Ctrl Pts',(-3.83169321400006,2.2,-1.84287125400001));
#317216=CARTESIAN_POINT('Ctrl Pts',(-3.83286252200006,12.2,-1.84407308800001));
#317217=CARTESIAN_POINT('Ctrl Pts',(-3.83286252200006,5.2,-1.84407308800001));
#317218=CARTESIAN_POINT('Ctrl Pts',(-3.83286252200006,2.2,-1.84407308800001));
#317219=CARTESIAN_POINT('Ctrl Pts',(-3.83403356500006,12.2,-1.84527947200001));
#317220=CARTESIAN_POINT('Ctrl Pts',(-3.83403356500006,5.2,-1.84527947200001));
#317221=CARTESIAN_POINT('Ctrl Pts',(-3.83403356500006,2.2,-1.84527947200001));
#317222=CARTESIAN_POINT('Ctrl Pts',(-3.83520633300006,12.2,-1.84649040700001));
#317223=CARTESIAN_POINT('Ctrl Pts',(-3.83520633300006,5.2,-1.84649040700001));
#317224=CARTESIAN_POINT('Ctrl Pts',(-3.83520633300006,2.2,-1.84649040700001));
#317225=CARTESIAN_POINT('Ctrl Pts',(-3.83638081200006,12.2,-1.84770589500001));
#317226=CARTESIAN_POINT('Ctrl Pts',(-3.83638081200006,5.2,-1.84770589500001));
#317227=CARTESIAN_POINT('Ctrl Pts',(-3.83638081200006,2.2,-1.84770589500001));
#317228=CARTESIAN_POINT('Ctrl Pts',(-3.83755699000006,12.2,-1.84892593400001));
#317229=CARTESIAN_POINT('Ctrl Pts',(-3.83755699000006,5.2,-1.84892593400001));
#317230=CARTESIAN_POINT('Ctrl Pts',(-3.83755699000006,2.2,-1.84892593400001));
#317231=CARTESIAN_POINT('Ctrl Pts',(-3.83873485500006,12.2,-1.85015052700002));
#317232=CARTESIAN_POINT('Ctrl Pts',(-3.83873485500006,5.2,-1.85015052700002));
#317233=CARTESIAN_POINT('Ctrl Pts',(-3.83873485500006,2.2,-1.85015052700002));
#317234=CARTESIAN_POINT('Ctrl Pts',(-3.83991439500006,12.2,-1.85137967400001));
#317235=CARTESIAN_POINT('Ctrl Pts',(-3.83991439500006,5.2,-1.85137967400001));
#317236=CARTESIAN_POINT('Ctrl Pts',(-3.83991439500006,2.2,-1.85137967400001));
#317237=CARTESIAN_POINT('Ctrl Pts',(-3.84109559700006,12.2,-1.85261337700001));
#317238=CARTESIAN_POINT('Ctrl Pts',(-3.84109559700006,5.2,-1.85261337700001));
#317239=CARTESIAN_POINT('Ctrl Pts',(-3.84109559700006,2.2,-1.85261337700001));
#317240=CARTESIAN_POINT('Ctrl Pts',(-3.84227845000006,12.2,-1.85385163300001));
#317241=CARTESIAN_POINT('Ctrl Pts',(-3.84227845000006,5.2,-1.85385163300001));
#317242=CARTESIAN_POINT('Ctrl Pts',(-3.84227845000006,2.2,-1.85385163300001));
#317243=CARTESIAN_POINT('Ctrl Pts',(-3.84346294100006,12.2,-1.85509444700001));
#317244=CARTESIAN_POINT('Ctrl Pts',(-3.84346294100006,5.2,-1.85509444700001));
#317245=CARTESIAN_POINT('Ctrl Pts',(-3.84346294100006,2.2,-1.85509444700001));
#317246=CARTESIAN_POINT('Ctrl Pts',(-3.84464905800006,12.2,-1.85634181600001));
#317247=CARTESIAN_POINT('Ctrl Pts',(-3.84464905800006,5.2,-1.85634181600001));
#317248=CARTESIAN_POINT('Ctrl Pts',(-3.84464905800006,2.2,-1.85634181600001));
#317249=CARTESIAN_POINT('Ctrl Pts',(-3.84583678800006,12.2,-1.85759374200002));
#317250=CARTESIAN_POINT('Ctrl Pts',(-3.84583678800006,5.2,-1.85759374200002));
#317251=CARTESIAN_POINT('Ctrl Pts',(-3.84583678800006,2.2,-1.85759374200002));
#317252=CARTESIAN_POINT('Ctrl Pts',(-3.84702612000006,12.2,-1.85885022500001));
#317253=CARTESIAN_POINT('Ctrl Pts',(-3.84702612000006,5.2,-1.85885022500001));
#317254=CARTESIAN_POINT('Ctrl Pts',(-3.84702612000006,2.2,-1.85885022500001));
#317255=CARTESIAN_POINT('Ctrl Pts',(-3.84821704000006,12.2,-1.86011126700001));
#317256=CARTESIAN_POINT('Ctrl Pts',(-3.84821704000006,5.2,-1.86011126700001));
#317257=CARTESIAN_POINT('Ctrl Pts',(-3.84821704000006,2.2,-1.86011126700001));
#317258=CARTESIAN_POINT('Ctrl Pts',(-3.84940953900006,12.2,-1.86137686600001));
#317259=CARTESIAN_POINT('Ctrl Pts',(-3.84940953900006,5.2,-1.86137686600001));
#317260=CARTESIAN_POINT('Ctrl Pts',(-3.84940953900006,2.2,-1.86137686600001));
#317261=CARTESIAN_POINT('Ctrl Pts',(-3.85060360200006,12.2,-1.86264702500001));
#317262=CARTESIAN_POINT('Ctrl Pts',(-3.85060360200006,5.2,-1.86264702500001));
#317263=CARTESIAN_POINT('Ctrl Pts',(-3.85060360200006,2.2,-1.86264702500001));
#317264=CARTESIAN_POINT('Ctrl Pts',(-3.85179922000006,12.2,-1.86392174300002));
#317265=CARTESIAN_POINT('Ctrl Pts',(-3.85179922000006,5.2,-1.86392174300002));
#317266=CARTESIAN_POINT('Ctrl Pts',(-3.85179922000006,2.2,-1.86392174300002));
#317267=CARTESIAN_POINT('Ctrl Pts',(-3.85299637800006,12.2,-1.86520102000001));
#317268=CARTESIAN_POINT('Ctrl Pts',(-3.85299637800006,5.2,-1.86520102000001));
#317269=CARTESIAN_POINT('Ctrl Pts',(-3.85299637800006,2.2,-1.86520102000001));
#317270=CARTESIAN_POINT('Ctrl Pts',(-3.85419506500006,12.2,-1.86648485800001));
#317271=CARTESIAN_POINT('Ctrl Pts',(-3.85419506500006,5.2,-1.86648485800001));
#317272=CARTESIAN_POINT('Ctrl Pts',(-3.85419506500006,2.2,-1.86648485800001));
#317273=CARTESIAN_POINT('Ctrl Pts',(-3.85539526900006,12.2,-1.86777325700001));
#317274=CARTESIAN_POINT('Ctrl Pts',(-3.85539526900006,5.2,-1.86777325700001));
#317275=CARTESIAN_POINT('Ctrl Pts',(-3.85539526900006,2.2,-1.86777325700001));
#317276=CARTESIAN_POINT('Ctrl Pts',(-3.85659697900006,12.2,-1.86906621600002));
#317277=CARTESIAN_POINT('Ctrl Pts',(-3.85659697900006,5.2,-1.86906621600002));
#317278=CARTESIAN_POINT('Ctrl Pts',(-3.85659697900006,2.2,-1.86906621600002));
#317279=CARTESIAN_POINT('Ctrl Pts',(-3.85780018200006,12.2,-1.87036373800002));
#317280=CARTESIAN_POINT('Ctrl Pts',(-3.85780018200006,5.2,-1.87036373800002));
#317281=CARTESIAN_POINT('Ctrl Pts',(-3.85780018200006,2.2,-1.87036373800002));
#317282=CARTESIAN_POINT('Ctrl Pts',(-3.85900486600006,12.2,-1.87166582000001));
#317283=CARTESIAN_POINT('Ctrl Pts',(-3.85900486600006,5.2,-1.87166582000001));
#317284=CARTESIAN_POINT('Ctrl Pts',(-3.85900486600006,2.2,-1.87166582000001));
#317285=CARTESIAN_POINT('Ctrl Pts',(-3.86021102000006,12.2,-1.87297246600002));
#317286=CARTESIAN_POINT('Ctrl Pts',(-3.86021102000006,5.2,-1.87297246600002));
#317287=CARTESIAN_POINT('Ctrl Pts',(-3.86021102000006,2.2,-1.87297246600002));
#317288=CARTESIAN_POINT('Ctrl Pts',(-3.86141863100006,12.2,-1.87428367200001));
#317289=CARTESIAN_POINT('Ctrl Pts',(-3.86141863100006,5.2,-1.87428367200001));
#317290=CARTESIAN_POINT('Ctrl Pts',(-3.86141863100006,2.2,-1.87428367200001));
#317291=CARTESIAN_POINT('Ctrl Pts',(-3.86262768800006,12.2,-1.87559944300002));
#317292=CARTESIAN_POINT('Ctrl Pts',(-3.86262768800006,5.2,-1.87559944300002));
#317293=CARTESIAN_POINT('Ctrl Pts',(-3.86262768800006,2.2,-1.87559944300002));
#317294=CARTESIAN_POINT('Ctrl Pts',(-3.86383817800006,12.2,-1.87691977600001));
#317295=CARTESIAN_POINT('Ctrl Pts',(-3.86383817800006,5.2,-1.87691977600001));
#317296=CARTESIAN_POINT('Ctrl Pts',(-3.86383817800006,2.2,-1.87691977600001));
#317297=CARTESIAN_POINT('Ctrl Pts',(-3.86505009100006,12.2,-1.87824467100001));
#317298=CARTESIAN_POINT('Ctrl Pts',(-3.86505009100006,5.2,-1.87824467100001));
#317299=CARTESIAN_POINT('Ctrl Pts',(-3.86505009100006,2.2,-1.87824467100001));
#317300=CARTESIAN_POINT('Ctrl Pts',(-3.86626341400006,12.2,-1.87957413100001));
#317301=CARTESIAN_POINT('Ctrl Pts',(-3.86626341400006,5.2,-1.87957413100001));
#317302=CARTESIAN_POINT('Ctrl Pts',(-3.86626341400006,2.2,-1.87957413100001));
#317303=CARTESIAN_POINT('Ctrl Pts',(-3.86747813500006,12.2,-1.88090815500002));
#317304=CARTESIAN_POINT('Ctrl Pts',(-3.86747813500006,5.2,-1.88090815500002));
#317305=CARTESIAN_POINT('Ctrl Pts',(-3.86747813500006,2.2,-1.88090815500002));
#317306=CARTESIAN_POINT('Ctrl Pts',(-3.86869424300006,12.2,-1.88224674200002));
#317307=CARTESIAN_POINT('Ctrl Pts',(-3.86869424300006,5.2,-1.88224674200002));
#317308=CARTESIAN_POINT('Ctrl Pts',(-3.86869424300006,2.2,-1.88224674200002));
#317309=CARTESIAN_POINT('Ctrl Pts',(-3.86991172500006,12.2,-1.88358989500002));
#317310=CARTESIAN_POINT('Ctrl Pts',(-3.86991172500006,5.2,-1.88358989500002));
#317311=CARTESIAN_POINT('Ctrl Pts',(-3.86991172500006,2.2,-1.88358989500002));
#317312=CARTESIAN_POINT('Ctrl Pts',(-3.87113057200006,12.2,-1.88493761100001));
#317313=CARTESIAN_POINT('Ctrl Pts',(-3.87113057200006,5.2,-1.88493761100001));
#317314=CARTESIAN_POINT('Ctrl Pts',(-3.87113057200006,2.2,-1.88493761100001));
#317315=CARTESIAN_POINT('Ctrl Pts',(-3.87235076900006,12.2,-1.88628989100001));
#317316=CARTESIAN_POINT('Ctrl Pts',(-3.87235076900006,5.2,-1.88628989100001));
#317317=CARTESIAN_POINT('Ctrl Pts',(-3.87235076900006,2.2,-1.88628989100001));
#317318=CARTESIAN_POINT('Ctrl Pts',(-3.87357230700006,12.2,-1.88764673700001));
#317319=CARTESIAN_POINT('Ctrl Pts',(-3.87357230700006,5.2,-1.88764673700001));
#317320=CARTESIAN_POINT('Ctrl Pts',(-3.87357230700006,2.2,-1.88764673700001));
#317321=CARTESIAN_POINT('Ctrl Pts',(-3.87479517200005,12.2,-1.88900814700002));
#317322=CARTESIAN_POINT('Ctrl Pts',(-3.87479517200005,5.2,-1.88900814700002));
#317323=CARTESIAN_POINT('Ctrl Pts',(-3.87479517200005,2.2,-1.88900814700002));
#317324=CARTESIAN_POINT('Ctrl Pts',(-3.87601935400006,12.2,-1.89037412300001));
#317325=CARTESIAN_POINT('Ctrl Pts',(-3.87601935400006,5.2,-1.89037412300001));
#317326=CARTESIAN_POINT('Ctrl Pts',(-3.87601935400006,2.2,-1.89037412300001));
#317327=CARTESIAN_POINT('Ctrl Pts',(-3.87724484000006,12.2,-1.89174466300001));
#317328=CARTESIAN_POINT('Ctrl Pts',(-3.87724484000006,5.2,-1.89174466300001));
#317329=CARTESIAN_POINT('Ctrl Pts',(-3.87724484000006,2.2,-1.89174466300001));
#317330=CARTESIAN_POINT('Ctrl Pts',(-3.87847162000006,12.2,-1.89311977000001));
#317331=CARTESIAN_POINT('Ctrl Pts',(-3.87847162000006,5.2,-1.89311977000001));
#317332=CARTESIAN_POINT('Ctrl Pts',(-3.87847162000006,2.2,-1.89311977000001));
#317333=CARTESIAN_POINT('Ctrl Pts',(-3.87969968200006,12.2,-1.89449944100001));
#317334=CARTESIAN_POINT('Ctrl Pts',(-3.87969968200006,5.2,-1.89449944100001));
#317335=CARTESIAN_POINT('Ctrl Pts',(-3.87969968200006,2.2,-1.89449944100001));
#317336=CARTESIAN_POINT('Ctrl Pts',(-3.88092901400006,12.2,-1.89588367700001));
#317337=CARTESIAN_POINT('Ctrl Pts',(-3.88092901400006,5.2,-1.89588367700001));
#317338=CARTESIAN_POINT('Ctrl Pts',(-3.88092901400006,2.2,-1.89588367700001));
#317339=CARTESIAN_POINT('Ctrl Pts',(-3.88215960400006,12.2,-1.89727248000001));
#317340=CARTESIAN_POINT('Ctrl Pts',(-3.88215960400006,5.2,-1.89727248000001));
#317341=CARTESIAN_POINT('Ctrl Pts',(-3.88215960400006,2.2,-1.89727248000001));
#317342=CARTESIAN_POINT('Ctrl Pts',(-3.88339144100006,12.2,-1.89866584700002));
#317343=CARTESIAN_POINT('Ctrl Pts',(-3.88339144100006,5.2,-1.89866584700002));
#317344=CARTESIAN_POINT('Ctrl Pts',(-3.88339144100006,2.2,-1.89866584700002));
#317345=CARTESIAN_POINT('Ctrl Pts',(-3.88462451500006,12.2,-1.90006378000001));
#317346=CARTESIAN_POINT('Ctrl Pts',(-3.88462451500006,5.2,-1.90006378000001));
#317347=CARTESIAN_POINT('Ctrl Pts',(-3.88462451500006,2.2,-1.90006378000001));
#317348=CARTESIAN_POINT('Ctrl Pts',(-3.88585881200005,12.2,-1.90146627800001));
#317349=CARTESIAN_POINT('Ctrl Pts',(-3.88585881200005,5.2,-1.90146627800001));
#317350=CARTESIAN_POINT('Ctrl Pts',(-3.88585881200005,2.2,-1.90146627800001));
#317351=CARTESIAN_POINT('Ctrl Pts',(-3.88709432100006,12.2,-1.90287334200002));
#317352=CARTESIAN_POINT('Ctrl Pts',(-3.88709432100006,5.2,-1.90287334200002));
#317353=CARTESIAN_POINT('Ctrl Pts',(-3.88709432100006,2.2,-1.90287334200002));
#317354=CARTESIAN_POINT('Ctrl Pts',(-3.88833103200006,12.2,-1.90428497100001));
#317355=CARTESIAN_POINT('Ctrl Pts',(-3.88833103200006,5.2,-1.90428497100001));
#317356=CARTESIAN_POINT('Ctrl Pts',(-3.88833103200006,2.2,-1.90428497100001));
#317357=CARTESIAN_POINT('Ctrl Pts',(-3.88956893300006,12.2,-1.90570116600002));
#317358=CARTESIAN_POINT('Ctrl Pts',(-3.88956893300006,5.2,-1.90570116600002));
#317359=CARTESIAN_POINT('Ctrl Pts',(-3.88956893300006,2.2,-1.90570116600002));
#317360=CARTESIAN_POINT('Ctrl Pts',(-3.89080801200006,12.2,-1.90712192700001));
#317361=CARTESIAN_POINT('Ctrl Pts',(-3.89080801200006,5.2,-1.90712192700001));
#317362=CARTESIAN_POINT('Ctrl Pts',(-3.89080801200006,2.2,-1.90712192700001));
#317363=CARTESIAN_POINT('Ctrl Pts',(-3.89204825700006,12.2,-1.90854725100001));
#317364=CARTESIAN_POINT('Ctrl Pts',(-3.89204825700006,5.2,-1.90854725100001));
#317365=CARTESIAN_POINT('Ctrl Pts',(-3.89204825700006,2.2,-1.90854725100001));
#317366=CARTESIAN_POINT('Ctrl Pts',(-3.89328965800006,12.2,-1.90997714200002));
#317367=CARTESIAN_POINT('Ctrl Pts',(-3.89328965800006,5.2,-1.90997714200002));
#317368=CARTESIAN_POINT('Ctrl Pts',(-3.89328965800006,2.2,-1.90997714200002));
#317369=CARTESIAN_POINT('Ctrl Pts',(-3.89453220400005,12.2,-1.91141159700001));
#317370=CARTESIAN_POINT('Ctrl Pts',(-3.89453220400005,5.2,-1.91141159700001));
#317371=CARTESIAN_POINT('Ctrl Pts',(-3.89453220400005,2.2,-1.91141159700001));
#317372=CARTESIAN_POINT('Ctrl Pts',(-3.89577588200006,12.2,-1.91285061800002));
#317373=CARTESIAN_POINT('Ctrl Pts',(-3.89577588200006,5.2,-1.91285061800002));
#317374=CARTESIAN_POINT('Ctrl Pts',(-3.89577588200006,2.2,-1.91285061800002));
#317375=CARTESIAN_POINT('Ctrl Pts',(-3.89702068200006,12.2,-1.91429420300001));
#317376=CARTESIAN_POINT('Ctrl Pts',(-3.89702068200006,5.2,-1.91429420300001));
#317377=CARTESIAN_POINT('Ctrl Pts',(-3.89702068200006,2.2,-1.91429420300001));
#317378=CARTESIAN_POINT('Ctrl Pts',(-3.89826659300006,12.2,-1.91574235300001));
#317379=CARTESIAN_POINT('Ctrl Pts',(-3.89826659300006,5.2,-1.91574235300001));
#317380=CARTESIAN_POINT('Ctrl Pts',(-3.89826659300006,2.2,-1.91574235300001));
#317381=CARTESIAN_POINT('Ctrl Pts',(-3.89951360200006,12.2,-1.91719506800001));
#317382=CARTESIAN_POINT('Ctrl Pts',(-3.89951360200006,5.2,-1.91719506800001));
#317383=CARTESIAN_POINT('Ctrl Pts',(-3.89951360200006,2.2,-1.91719506800001));
#317384=CARTESIAN_POINT('Ctrl Pts',(-3.90076169900006,12.2,-1.91865234600002));
#317385=CARTESIAN_POINT('Ctrl Pts',(-3.90076169900006,5.2,-1.91865234600002));
#317386=CARTESIAN_POINT('Ctrl Pts',(-3.90076169900006,2.2,-1.91865234600002));
#317387=CARTESIAN_POINT('Ctrl Pts',(-3.90201087200006,12.2,-1.92011418900002));
#317388=CARTESIAN_POINT('Ctrl Pts',(-3.90201087200006,5.2,-1.92011418900002));
#317389=CARTESIAN_POINT('Ctrl Pts',(-3.90201087200006,2.2,-1.92011418900002));
#317390=CARTESIAN_POINT('Ctrl Pts',(-3.90326111100006,12.2,-1.92158059600001));
#317391=CARTESIAN_POINT('Ctrl Pts',(-3.90326111100006,5.2,-1.92158059600001));
#317392=CARTESIAN_POINT('Ctrl Pts',(-3.90326111100006,2.2,-1.92158059600001));
#317393=CARTESIAN_POINT('Ctrl Pts',(-3.90451240400005,12.2,-1.92305156600002));
#317394=CARTESIAN_POINT('Ctrl Pts',(-3.90451240400005,5.2,-1.92305156600002));
#317395=CARTESIAN_POINT('Ctrl Pts',(-3.90451240400005,2.2,-1.92305156600002));
#317396=CARTESIAN_POINT('Ctrl Pts',(-3.90576474000006,12.2,-1.92452709900001));
#317397=CARTESIAN_POINT('Ctrl Pts',(-3.90576474000006,5.2,-1.92452709900001));
#317398=CARTESIAN_POINT('Ctrl Pts',(-3.90576474000006,2.2,-1.92452709900001));
#317399=CARTESIAN_POINT('Ctrl Pts',(-3.90701810700006,12.2,-1.92600719600001));
#317400=CARTESIAN_POINT('Ctrl Pts',(-3.90701810700006,5.2,-1.92600719600001));
#317401=CARTESIAN_POINT('Ctrl Pts',(-3.90701810700006,2.2,-1.92600719600001));
#317402=CARTESIAN_POINT('Ctrl Pts',(-3.90827249600005,12.2,-1.92749185600002));
#317403=CARTESIAN_POINT('Ctrl Pts',(-3.90827249600005,5.2,-1.92749185600002));
#317404=CARTESIAN_POINT('Ctrl Pts',(-3.90827249600005,2.2,-1.92749185600002));
#317405=CARTESIAN_POINT('Ctrl Pts',(-3.90952789300006,12.2,-1.92898107800001));
#317406=CARTESIAN_POINT('Ctrl Pts',(-3.90952789300006,5.2,-1.92898107800001));
#317407=CARTESIAN_POINT('Ctrl Pts',(-3.90952789300006,2.2,-1.92898107800001));
#317408=CARTESIAN_POINT('Ctrl Pts',(-3.91078429000006,12.2,-1.93047486300001));
#317409=CARTESIAN_POINT('Ctrl Pts',(-3.91078429000006,5.2,-1.93047486300001));
#317410=CARTESIAN_POINT('Ctrl Pts',(-3.91078429000006,2.2,-1.93047486300001));
#317411=CARTESIAN_POINT('Ctrl Pts',(-3.91204167400006,12.2,-1.93197320900001));
#317412=CARTESIAN_POINT('Ctrl Pts',(-3.91204167400006,5.2,-1.93197320900001));
#317413=CARTESIAN_POINT('Ctrl Pts',(-3.91204167400006,2.2,-1.93197320900001));
#317414=CARTESIAN_POINT('Ctrl Pts',(-3.91330003300006,12.2,-1.93347611800001));
#317415=CARTESIAN_POINT('Ctrl Pts',(-3.91330003300006,5.2,-1.93347611800001));
#317416=CARTESIAN_POINT('Ctrl Pts',(-3.91330003300006,2.2,-1.93347611800001));
#317417=CARTESIAN_POINT('Ctrl Pts',(-3.91455935800006,12.2,-1.93498358700001));
#317418=CARTESIAN_POINT('Ctrl Pts',(-3.91455935800006,5.2,-1.93498358700001));
#317419=CARTESIAN_POINT('Ctrl Pts',(-3.91455935800006,2.2,-1.93498358700001));
#317420=CARTESIAN_POINT('Ctrl Pts',(-3.91581963700006,12.2,-1.93649561800001));
#317421=CARTESIAN_POINT('Ctrl Pts',(-3.91581963700006,5.2,-1.93649561800001));
#317422=CARTESIAN_POINT('Ctrl Pts',(-3.91581963700006,2.2,-1.93649561800001));
#317423=CARTESIAN_POINT('Ctrl Pts',(-3.91708085900006,12.2,-1.93801220900002));
#317424=CARTESIAN_POINT('Ctrl Pts',(-3.91708085900006,5.2,-1.93801220900002));
#317425=CARTESIAN_POINT('Ctrl Pts',(-3.91708085900006,2.2,-1.93801220900002));
#317426=CARTESIAN_POINT('Ctrl Pts',(-3.91834301300006,12.2,-1.93953336000002));
#317427=CARTESIAN_POINT('Ctrl Pts',(-3.91834301300006,5.2,-1.93953336000002));
#317428=CARTESIAN_POINT('Ctrl Pts',(-3.91834301300006,2.2,-1.93953336000002));
#317429=CARTESIAN_POINT('Ctrl Pts',(-3.91960608900006,12.2,-1.94105907100001));
#317430=CARTESIAN_POINT('Ctrl Pts',(-3.91960608900006,5.2,-1.94105907100001));
#317431=CARTESIAN_POINT('Ctrl Pts',(-3.91960608900006,2.2,-1.94105907100001));
#317432=CARTESIAN_POINT('Ctrl Pts',(-3.92087007500006,12.2,-1.94258934100001));
#317433=CARTESIAN_POINT('Ctrl Pts',(-3.92087007500006,5.2,-1.94258934100001));
#317434=CARTESIAN_POINT('Ctrl Pts',(-3.92087007500006,2.2,-1.94258934100001));
#317435=CARTESIAN_POINT('Ctrl Pts',(-3.92213496000006,12.2,-1.94412417000001));
#317436=CARTESIAN_POINT('Ctrl Pts',(-3.92213496000006,5.2,-1.94412417000001));
#317437=CARTESIAN_POINT('Ctrl Pts',(-3.92213496000006,2.2,-1.94412417000001));
#317438=CARTESIAN_POINT('Ctrl Pts',(-3.92340073400006,12.2,-1.94566355900001));
#317439=CARTESIAN_POINT('Ctrl Pts',(-3.92340073400006,5.2,-1.94566355900001));
#317440=CARTESIAN_POINT('Ctrl Pts',(-3.92340073400006,2.2,-1.94566355900001));
#317441=CARTESIAN_POINT('Ctrl Pts',(-3.92466738500006,12.2,-1.94720750400001));
#317442=CARTESIAN_POINT('Ctrl Pts',(-3.92466738500006,5.2,-1.94720750400001));
#317443=CARTESIAN_POINT('Ctrl Pts',(-3.92466738500006,2.2,-1.94720750400001));
#317444=CARTESIAN_POINT('Ctrl Pts',(-3.92593490200006,12.2,-1.94875600800001));
#317445=CARTESIAN_POINT('Ctrl Pts',(-3.92593490200006,5.2,-1.94875600800001));
#317446=CARTESIAN_POINT('Ctrl Pts',(-3.92593490200006,2.2,-1.94875600800001));
#317447=CARTESIAN_POINT('Ctrl Pts',(-3.92720327500006,12.2,-1.95030906800001));
#317448=CARTESIAN_POINT('Ctrl Pts',(-3.92720327500006,5.2,-1.95030906800001));
#317449=CARTESIAN_POINT('Ctrl Pts',(-3.92720327500006,2.2,-1.95030906800001));
#317450=CARTESIAN_POINT('Ctrl Pts',(-3.92847249300006,12.2,-1.95186668500002));
#317451=CARTESIAN_POINT('Ctrl Pts',(-3.92847249300006,5.2,-1.95186668500002));
#317452=CARTESIAN_POINT('Ctrl Pts',(-3.92847249300006,2.2,-1.95186668500002));
#317453=CARTESIAN_POINT('Ctrl Pts',(-3.92974254600006,12.2,-1.95342885800001));
#317454=CARTESIAN_POINT('Ctrl Pts',(-3.92974254600006,5.2,-1.95342885800001));
#317455=CARTESIAN_POINT('Ctrl Pts',(-3.92974254600006,2.2,-1.95342885800001));
#317456=CARTESIAN_POINT('Ctrl Pts',(-3.93101342100006,12.2,-1.95499558700002));
#317457=CARTESIAN_POINT('Ctrl Pts',(-3.93101342100006,5.2,-1.95499558700002));
#317458=CARTESIAN_POINT('Ctrl Pts',(-3.93101342100006,2.2,-1.95499558700002));
#317459=CARTESIAN_POINT('Ctrl Pts',(-3.93228510900006,12.2,-1.95656686900001));
#317460=CARTESIAN_POINT('Ctrl Pts',(-3.93228510900006,5.2,-1.95656686900001));
#317461=CARTESIAN_POINT('Ctrl Pts',(-3.93228510900006,2.2,-1.95656686900001));
#317462=CARTESIAN_POINT('Ctrl Pts',(-3.93355759800006,12.2,-1.95814270800001));
#317463=CARTESIAN_POINT('Ctrl Pts',(-3.93355759800006,5.2,-1.95814270800001));
#317464=CARTESIAN_POINT('Ctrl Pts',(-3.93355759800006,2.2,-1.95814270800001));
#317465=CARTESIAN_POINT('Ctrl Pts',(-3.93483087900006,12.2,-1.95972309900001));
#317466=CARTESIAN_POINT('Ctrl Pts',(-3.93483087900006,5.2,-1.95972309900001));
#317467=CARTESIAN_POINT('Ctrl Pts',(-3.93483087900006,2.2,-1.95972309900001));
#317468=CARTESIAN_POINT('Ctrl Pts',(-3.93610493900006,12.2,-1.96130804400001));
#317469=CARTESIAN_POINT('Ctrl Pts',(-3.93610493900006,5.2,-1.96130804400001));
#317470=CARTESIAN_POINT('Ctrl Pts',(-3.93610493900006,2.2,-1.96130804400001));
#317471=CARTESIAN_POINT('Ctrl Pts',(-3.93737976900006,12.2,-1.96289754200001));
#317472=CARTESIAN_POINT('Ctrl Pts',(-3.93737976900006,5.2,-1.96289754200001));
#317473=CARTESIAN_POINT('Ctrl Pts',(-3.93737976900006,2.2,-1.96289754200001));
#317474=CARTESIAN_POINT('Ctrl Pts',(-3.93865535800006,12.2,-1.96449159100001));
#317475=CARTESIAN_POINT('Ctrl Pts',(-3.93865535800006,5.2,-1.96449159100001));
#317476=CARTESIAN_POINT('Ctrl Pts',(-3.93865535800006,2.2,-1.96449159100001));
#317477=CARTESIAN_POINT('Ctrl Pts',(-3.93993169500006,12.2,-1.96609019200002));
#317478=CARTESIAN_POINT('Ctrl Pts',(-3.93993169500006,5.2,-1.96609019200002));
#317479=CARTESIAN_POINT('Ctrl Pts',(-3.93993169500006,2.2,-1.96609019200002));
#317480=CARTESIAN_POINT('Ctrl Pts',(-3.94120876900006,12.2,-1.96769334400001));
#317481=CARTESIAN_POINT('Ctrl Pts',(-3.94120876900006,5.2,-1.96769334400001));
#317482=CARTESIAN_POINT('Ctrl Pts',(-3.94120876900006,2.2,-1.96769334400001));
#317483=CARTESIAN_POINT('Ctrl Pts',(-3.94248657000006,12.2,-1.96930104600002));
#317484=CARTESIAN_POINT('Ctrl Pts',(-3.94248657000006,5.2,-1.96930104600002));
#317485=CARTESIAN_POINT('Ctrl Pts',(-3.94248657000006,2.2,-1.96930104600002));
#317486=CARTESIAN_POINT('Ctrl Pts',(-3.94376508600006,12.2,-1.97091329700001));
#317487=CARTESIAN_POINT('Ctrl Pts',(-3.94376508600006,5.2,-1.97091329700001));
#317488=CARTESIAN_POINT('Ctrl Pts',(-3.94376508600006,2.2,-1.97091329700001));
#317489=CARTESIAN_POINT('Ctrl Pts',(-3.94504430900006,12.2,-1.97253009700002));
#317490=CARTESIAN_POINT('Ctrl Pts',(-3.94504430900006,5.2,-1.97253009700002));
#317491=CARTESIAN_POINT('Ctrl Pts',(-3.94504430900006,2.2,-1.97253009700002));
#317492=CARTESIAN_POINT('Ctrl Pts',(-3.94632422700006,12.2,-1.97415144500001));
#317493=CARTESIAN_POINT('Ctrl Pts',(-3.94632422700006,5.2,-1.97415144500001));
#317494=CARTESIAN_POINT('Ctrl Pts',(-3.94632422700006,2.2,-1.97415144500001));
#317495=CARTESIAN_POINT('Ctrl Pts',(-3.94760482800006,12.2,-1.97577734100001));
#317496=CARTESIAN_POINT('Ctrl Pts',(-3.94760482800006,5.2,-1.97577734100001));
#317497=CARTESIAN_POINT('Ctrl Pts',(-3.94760482800006,2.2,-1.97577734100001));
#317498=CARTESIAN_POINT('Ctrl Pts',(-3.94888610300006,12.2,-1.97740778200002));
#317499=CARTESIAN_POINT('Ctrl Pts',(-3.94888610300006,5.2,-1.97740778200002));
#317500=CARTESIAN_POINT('Ctrl Pts',(-3.94888610300006,2.2,-1.97740778200002));
#317501=CARTESIAN_POINT('Ctrl Pts',(-3.95016804100006,12.2,-1.97904277100001));
#317502=CARTESIAN_POINT('Ctrl Pts',(-3.95016804100006,5.2,-1.97904277100001));
#317503=CARTESIAN_POINT('Ctrl Pts',(-3.95016804100006,2.2,-1.97904277100001));
#317504=CARTESIAN_POINT('Ctrl Pts',(-3.95145063200006,12.2,-1.98068230400001));
#317505=CARTESIAN_POINT('Ctrl Pts',(-3.95145063200006,5.2,-1.98068230400001));
#317506=CARTESIAN_POINT('Ctrl Pts',(-3.95145063200006,2.2,-1.98068230400001));
#317507=CARTESIAN_POINT('Ctrl Pts',(-3.95273386500006,12.2,-1.98232638100002));
#317508=CARTESIAN_POINT('Ctrl Pts',(-3.95273386500006,5.2,-1.98232638100002));
#317509=CARTESIAN_POINT('Ctrl Pts',(-3.95273386500006,2.2,-1.98232638100002));
#317510=CARTESIAN_POINT('Ctrl Pts',(-3.95401773000006,12.2,-1.98397500200001));
#317511=CARTESIAN_POINT('Ctrl Pts',(-3.95401773000006,5.2,-1.98397500200001));
#317512=CARTESIAN_POINT('Ctrl Pts',(-3.95401773000006,2.2,-1.98397500200001));
#317513=CARTESIAN_POINT('Ctrl Pts',(-3.95530221600006,12.2,-1.98562816600001));
#317514=CARTESIAN_POINT('Ctrl Pts',(-3.95530221600006,5.2,-1.98562816600001));
#317515=CARTESIAN_POINT('Ctrl Pts',(-3.95530221600006,2.2,-1.98562816600001));
#317516=CARTESIAN_POINT('Ctrl Pts',(-3.95658731200006,12.2,-1.98728587300002));
#317517=CARTESIAN_POINT('Ctrl Pts',(-3.95658731200006,5.2,-1.98728587300002));
#317518=CARTESIAN_POINT('Ctrl Pts',(-3.95658731200006,2.2,-1.98728587300002));
#317519=CARTESIAN_POINT('Ctrl Pts',(-3.95787300900006,12.2,-1.98894812000002));
#317520=CARTESIAN_POINT('Ctrl Pts',(-3.95787300900006,5.2,-1.98894812000002));
#317521=CARTESIAN_POINT('Ctrl Pts',(-3.95787300900006,2.2,-1.98894812000002));
#317522=CARTESIAN_POINT('Ctrl Pts',(-3.95915929600006,12.2,-1.99061490800001));
#317523=CARTESIAN_POINT('Ctrl Pts',(-3.95915929600006,5.2,-1.99061490800001));
#317524=CARTESIAN_POINT('Ctrl Pts',(-3.95915929600006,2.2,-1.99061490800001));
#317525=CARTESIAN_POINT('Ctrl Pts',(-3.96044616200006,12.2,-1.99228623500002));
#317526=CARTESIAN_POINT('Ctrl Pts',(-3.96044616200006,5.2,-1.99228623500002));
#317527=CARTESIAN_POINT('Ctrl Pts',(-3.96044616200006,2.2,-1.99228623500002));
#317528=CARTESIAN_POINT('Ctrl Pts',(-3.96173359600006,12.2,-1.99396210000002));
#317529=CARTESIAN_POINT('Ctrl Pts',(-3.96173359600006,5.2,-1.99396210000002));
#317530=CARTESIAN_POINT('Ctrl Pts',(-3.96173359600006,2.2,-1.99396210000002));
#317531=CARTESIAN_POINT('Ctrl Pts',(-3.96302159000006,12.2,-1.99564250400002));
#317532=CARTESIAN_POINT('Ctrl Pts',(-3.96302159000006,5.2,-1.99564250400002));
#317533=CARTESIAN_POINT('Ctrl Pts',(-3.96302159000006,2.2,-1.99564250400002));
#317534=CARTESIAN_POINT('Ctrl Pts',(-3.96431013200006,12.2,-1.99732744500002));
#317535=CARTESIAN_POINT('Ctrl Pts',(-3.96431013200006,5.2,-1.99732744500002));
#317536=CARTESIAN_POINT('Ctrl Pts',(-3.96431013200006,2.2,-1.99732744500002));
#317537=CARTESIAN_POINT('Ctrl Pts',(-3.96559921100006,12.2,-1.99901692200001));
#317538=CARTESIAN_POINT('Ctrl Pts',(-3.96559921100006,5.2,-1.99901692200001));
#317539=CARTESIAN_POINT('Ctrl Pts',(-3.96559921100006,2.2,-1.99901692200001));
#317540=CARTESIAN_POINT('Ctrl Pts',(-3.96688881800006,12.2,-2.00071093300001));
#317541=CARTESIAN_POINT('Ctrl Pts',(-3.96688881800006,5.2,-2.00071093300001));
#317542=CARTESIAN_POINT('Ctrl Pts',(-3.96688881800006,2.2,-2.00071093300001));
#317543=CARTESIAN_POINT('Ctrl Pts',(-3.96817894300006,12.2,-2.00240947900001));
#317544=CARTESIAN_POINT('Ctrl Pts',(-3.96817894300006,5.2,-2.00240947900001));
#317545=CARTESIAN_POINT('Ctrl Pts',(-3.96817894300006,2.2,-2.00240947900001));
#317546=CARTESIAN_POINT('Ctrl Pts',(-3.96946957500006,12.2,-2.00411255800002));
#317547=CARTESIAN_POINT('Ctrl Pts',(-3.96946957500006,5.2,-2.00411255800002));
#317548=CARTESIAN_POINT('Ctrl Pts',(-3.96946957500006,2.2,-2.00411255800002));
#317549=CARTESIAN_POINT('Ctrl Pts',(-3.97076070300006,12.2,-2.00582017000002));
#317550=CARTESIAN_POINT('Ctrl Pts',(-3.97076070300006,5.2,-2.00582017000002));
#317551=CARTESIAN_POINT('Ctrl Pts',(-3.97076070300006,2.2,-2.00582017000002));
#317552=CARTESIAN_POINT('Ctrl Pts',(-3.97205231700006,12.2,-2.00753231300002));
#317553=CARTESIAN_POINT('Ctrl Pts',(-3.97205231700006,5.2,-2.00753231300002));
#317554=CARTESIAN_POINT('Ctrl Pts',(-3.97205231700006,2.2,-2.00753231300002));
#317555=CARTESIAN_POINT('Ctrl Pts',(-3.97334440800006,12.2,-2.00924898700002));
#317556=CARTESIAN_POINT('Ctrl Pts',(-3.97334440800006,5.2,-2.00924898700002));
#317557=CARTESIAN_POINT('Ctrl Pts',(-3.97334440800006,2.2,-2.00924898700002));
#317558=CARTESIAN_POINT('Ctrl Pts',(-3.97463696500005,12.2,-2.01097019000001));
#317559=CARTESIAN_POINT('Ctrl Pts',(-3.97463696500005,5.2,-2.01097019000001));
#317560=CARTESIAN_POINT('Ctrl Pts',(-3.97463696500005,2.2,-2.01097019000001));
#317561=CARTESIAN_POINT('Ctrl Pts',(-3.97592997700006,12.2,-2.01269592100001));
#317562=CARTESIAN_POINT('Ctrl Pts',(-3.97592997700006,5.2,-2.01269592100001));
#317563=CARTESIAN_POINT('Ctrl Pts',(-3.97592997700006,2.2,-2.01269592100001));
#317564=CARTESIAN_POINT('Ctrl Pts',(-3.97722343500006,12.2,-2.01442618000002));
#317565=CARTESIAN_POINT('Ctrl Pts',(-3.97722343500006,5.2,-2.01442618000002));
#317566=CARTESIAN_POINT('Ctrl Pts',(-3.97722343500006,2.2,-2.01442618000002));
#317567=CARTESIAN_POINT('Ctrl Pts',(-3.97851732900006,12.2,-2.01616096600001));
#317568=CARTESIAN_POINT('Ctrl Pts',(-3.97851732900006,5.2,-2.01616096600001));
#317569=CARTESIAN_POINT('Ctrl Pts',(-3.97851732900006,2.2,-2.01616096600001));
#317570=CARTESIAN_POINT('Ctrl Pts',(-3.97981164700006,12.2,-2.01790027700001));
#317571=CARTESIAN_POINT('Ctrl Pts',(-3.97981164700006,5.2,-2.01790027700001));
#317572=CARTESIAN_POINT('Ctrl Pts',(-3.97981164700006,2.2,-2.01790027700001));
#317573=CARTESIAN_POINT('Ctrl Pts',(-3.98110638100006,12.2,-2.01964411200001));
#317574=CARTESIAN_POINT('Ctrl Pts',(-3.98110638100006,5.2,-2.01964411200001));
#317575=CARTESIAN_POINT('Ctrl Pts',(-3.98110638100006,2.2,-2.01964411200001));
#317576=CARTESIAN_POINT('Ctrl Pts',(-3.98240151900006,12.2,-2.02139247000002));
#317577=CARTESIAN_POINT('Ctrl Pts',(-3.98240151900006,5.2,-2.02139247000002));
#317578=CARTESIAN_POINT('Ctrl Pts',(-3.98240151900006,2.2,-2.02139247000002));
#317579=CARTESIAN_POINT('Ctrl Pts',(-3.98369705200006,12.2,-2.02314535000002));
#317580=CARTESIAN_POINT('Ctrl Pts',(-3.98369705200006,5.2,-2.02314535000002));
#317581=CARTESIAN_POINT('Ctrl Pts',(-3.98369705200006,2.2,-2.02314535000002));
#317582=CARTESIAN_POINT('Ctrl Pts',(-3.98499297100006,12.2,-2.02490275300002));
#317583=CARTESIAN_POINT('Ctrl Pts',(-3.98499297100006,5.2,-2.02490275300002));
#317584=CARTESIAN_POINT('Ctrl Pts',(-3.98499297100006,2.2,-2.02490275300002));
#317585=CARTESIAN_POINT('Ctrl Pts',(-3.98628926300006,12.2,-2.02666467500002));
#317586=CARTESIAN_POINT('Ctrl Pts',(-3.98628926300006,5.2,-2.02666467500002));
#317587=CARTESIAN_POINT('Ctrl Pts',(-3.98628926300006,2.2,-2.02666467500002));
#317588=CARTESIAN_POINT('Ctrl Pts',(-3.98758592100006,12.2,-2.02843111500002));
#317589=CARTESIAN_POINT('Ctrl Pts',(-3.98758592100006,5.2,-2.02843111500002));
#317590=CARTESIAN_POINT('Ctrl Pts',(-3.98758592100006,2.2,-2.02843111500002));
#317591=CARTESIAN_POINT('Ctrl Pts',(-3.98888293200006,12.2,-2.03020207400002));
#317592=CARTESIAN_POINT('Ctrl Pts',(-3.98888293200006,5.2,-2.03020207400002));
#317593=CARTESIAN_POINT('Ctrl Pts',(-3.98888293200006,2.2,-2.03020207400002));
#317594=CARTESIAN_POINT('Ctrl Pts',(-3.99018028800006,12.2,-2.03197754900001));
#317595=CARTESIAN_POINT('Ctrl Pts',(-3.99018028800006,5.2,-2.03197754900001));
#317596=CARTESIAN_POINT('Ctrl Pts',(-3.99018028800006,2.2,-2.03197754900001));
#317597=CARTESIAN_POINT('Ctrl Pts',(-3.99147798000006,12.2,-2.03375754000001));
#317598=CARTESIAN_POINT('Ctrl Pts',(-3.99147798000006,5.2,-2.03375754000001));
#317599=CARTESIAN_POINT('Ctrl Pts',(-3.99147798000006,2.2,-2.03375754000001));
#317600=CARTESIAN_POINT('Ctrl Pts',(-3.99277599500006,12.2,-2.03554204600001));
#317601=CARTESIAN_POINT('Ctrl Pts',(-3.99277599500006,5.2,-2.03554204600001));
#317602=CARTESIAN_POINT('Ctrl Pts',(-3.99277599500006,2.2,-2.03554204600001));
#317603=CARTESIAN_POINT('Ctrl Pts',(-3.99407432400006,12.2,-2.03733106400001));
#317604=CARTESIAN_POINT('Ctrl Pts',(-3.99407432400006,5.2,-2.03733106400001));
#317605=CARTESIAN_POINT('Ctrl Pts',(-3.99407432400006,2.2,-2.03733106400001));
#317606=CARTESIAN_POINT('Ctrl Pts',(-3.99537295900006,12.2,-2.03912459600001));
#317607=CARTESIAN_POINT('Ctrl Pts',(-3.99537295900006,5.2,-2.03912459600001));
#317608=CARTESIAN_POINT('Ctrl Pts',(-3.99537295900006,2.2,-2.03912459600001));
#317609=CARTESIAN_POINT('Ctrl Pts',(-3.99667188700006,12.2,-2.04092263700002));
#317610=CARTESIAN_POINT('Ctrl Pts',(-3.99667188700006,5.2,-2.04092263700002));
#317611=CARTESIAN_POINT('Ctrl Pts',(-3.99667188700006,2.2,-2.04092263700002));
#317612=CARTESIAN_POINT('Ctrl Pts',(-3.99797110100006,12.2,-2.04272518800002));
#317613=CARTESIAN_POINT('Ctrl Pts',(-3.99797110100006,5.2,-2.04272518800002));
#317614=CARTESIAN_POINT('Ctrl Pts',(-3.99797110100006,2.2,-2.04272518800002));
#317615=CARTESIAN_POINT('Ctrl Pts',(-3.99927058900006,12.2,-2.04453224800002));
#317616=CARTESIAN_POINT('Ctrl Pts',(-3.99927058900006,5.2,-2.04453224800002));
#317617=CARTESIAN_POINT('Ctrl Pts',(-3.99927058900006,2.2,-2.04453224800002));
#317618=CARTESIAN_POINT('Ctrl Pts',(-4.00057034200006,12.2,-2.04634381500002));
#317619=CARTESIAN_POINT('Ctrl Pts',(-4.00057034200006,5.2,-2.04634381500002));
#317620=CARTESIAN_POINT('Ctrl Pts',(-4.00057034200006,2.2,-2.04634381500002));
#317621=CARTESIAN_POINT('Ctrl Pts',(-4.00187034900005,12.2,-2.04815988800001));
#317622=CARTESIAN_POINT('Ctrl Pts',(-4.00187034900005,5.2,-2.04815988800001));
#317623=CARTESIAN_POINT('Ctrl Pts',(-4.00187034900005,2.2,-2.04815988800001));
#317624=CARTESIAN_POINT('Ctrl Pts',(-4.00317060200006,12.2,-2.04998046600001));
#317625=CARTESIAN_POINT('Ctrl Pts',(-4.00317060200006,5.2,-2.04998046600001));
#317626=CARTESIAN_POINT('Ctrl Pts',(-4.00317060200006,2.2,-2.04998046600001));
#317627=CARTESIAN_POINT('Ctrl Pts',(-4.00447109000006,12.2,-2.05180554700001));
#317628=CARTESIAN_POINT('Ctrl Pts',(-4.00447109000006,5.2,-2.05180554700001));
#317629=CARTESIAN_POINT('Ctrl Pts',(-4.00447109000006,2.2,-2.05180554700001));
#317630=CARTESIAN_POINT('Ctrl Pts',(-4.00577180300006,12.2,-2.05363513100002));
#317631=CARTESIAN_POINT('Ctrl Pts',(-4.00577180300006,5.2,-2.05363513100002));
#317632=CARTESIAN_POINT('Ctrl Pts',(-4.00577180300006,2.2,-2.05363513100002));
#317633=CARTESIAN_POINT('Ctrl Pts',(-4.00707273200006,12.2,-2.05546921500002));
#317634=CARTESIAN_POINT('Ctrl Pts',(-4.00707273200006,5.2,-2.05546921500002));
#317635=CARTESIAN_POINT('Ctrl Pts',(-4.00707273200006,2.2,-2.05546921500002));
#317636=CARTESIAN_POINT('Ctrl Pts',(-4.00837386700006,12.2,-2.05730780000001));
#317637=CARTESIAN_POINT('Ctrl Pts',(-4.00837386700006,5.2,-2.05730780000001));
#317638=CARTESIAN_POINT('Ctrl Pts',(-4.00837386700006,2.2,-2.05730780000001));
#317639=CARTESIAN_POINT('Ctrl Pts',(-4.00967519800006,12.2,-2.05915088300001));
#317640=CARTESIAN_POINT('Ctrl Pts',(-4.00967519800006,5.2,-2.05915088300001));
#317641=CARTESIAN_POINT('Ctrl Pts',(-4.00967519800006,2.2,-2.05915088300001));
#317642=CARTESIAN_POINT('Ctrl Pts',(-4.01097671400006,12.2,-2.06099846200001));
#317643=CARTESIAN_POINT('Ctrl Pts',(-4.01097671400006,5.2,-2.06099846200001));
#317644=CARTESIAN_POINT('Ctrl Pts',(-4.01097671400006,2.2,-2.06099846200001));
#317645=CARTESIAN_POINT('Ctrl Pts',(-4.01227840700006,12.2,-2.06285053800002));
#317646=CARTESIAN_POINT('Ctrl Pts',(-4.01227840700006,5.2,-2.06285053800002));
#317647=CARTESIAN_POINT('Ctrl Pts',(-4.01227840700006,2.2,-2.06285053800002));
#317648=CARTESIAN_POINT('Ctrl Pts',(-4.01358026700006,12.2,-2.06470710700001));
#317649=CARTESIAN_POINT('Ctrl Pts',(-4.01358026700006,5.2,-2.06470710700001));
#317650=CARTESIAN_POINT('Ctrl Pts',(-4.01358026700006,2.2,-2.06470710700001));
#317651=CARTESIAN_POINT('Ctrl Pts',(-4.01488228300006,12.2,-2.06656817000002));
#317652=CARTESIAN_POINT('Ctrl Pts',(-4.01488228300006,5.2,-2.06656817000002));
#317653=CARTESIAN_POINT('Ctrl Pts',(-4.01488228300006,2.2,-2.06656817000002));
#317654=CARTESIAN_POINT('Ctrl Pts',(-4.01618444700006,12.2,-2.06843372500002));
#317655=CARTESIAN_POINT('Ctrl Pts',(-4.01618444700006,5.2,-2.06843372500002));
#317656=CARTESIAN_POINT('Ctrl Pts',(-4.01618444700006,2.2,-2.06843372500002));
#317657=CARTESIAN_POINT('Ctrl Pts',(-4.01748674700006,12.2,-2.07030376900001));
#317658=CARTESIAN_POINT('Ctrl Pts',(-4.01748674700006,5.2,-2.07030376900001));
#317659=CARTESIAN_POINT('Ctrl Pts',(-4.01748674700006,2.2,-2.07030376900001));
#317660=CARTESIAN_POINT('Ctrl Pts',(-4.01878917600006,12.2,-2.07217830200001));
#317661=CARTESIAN_POINT('Ctrl Pts',(-4.01878917600006,5.2,-2.07217830200001));
#317662=CARTESIAN_POINT('Ctrl Pts',(-4.01878917600006,2.2,-2.07217830200001));
#317663=CARTESIAN_POINT('Ctrl Pts',(-4.02009172300006,12.2,-2.07405732300002));
#317664=CARTESIAN_POINT('Ctrl Pts',(-4.02009172300006,5.2,-2.07405732300002));
#317665=CARTESIAN_POINT('Ctrl Pts',(-4.02009172300006,2.2,-2.07405732300002));
#317666=CARTESIAN_POINT('Ctrl Pts',(-4.02139437900006,12.2,-2.07594083000001));
#317667=CARTESIAN_POINT('Ctrl Pts',(-4.02139437900006,5.2,-2.07594083000001));
#317668=CARTESIAN_POINT('Ctrl Pts',(-4.02139437900006,2.2,-2.07594083000001));
#317669=CARTESIAN_POINT('Ctrl Pts',(-4.02269713300006,12.2,-2.07782882200001));
#317670=CARTESIAN_POINT('Ctrl Pts',(-4.02269713300006,5.2,-2.07782882200001));
#317671=CARTESIAN_POINT('Ctrl Pts',(-4.02269713300006,2.2,-2.07782882200001));
#317672=CARTESIAN_POINT('Ctrl Pts',(-4.02399997600006,12.2,-2.07972129700002));
#317673=CARTESIAN_POINT('Ctrl Pts',(-4.02399997600006,5.2,-2.07972129700002));
#317674=CARTESIAN_POINT('Ctrl Pts',(-4.02399997600006,2.2,-2.07972129700002));
#317675=CARTESIAN_POINT('Ctrl Pts',(-4.02530289900006,12.2,-2.08161825400001));
#317676=CARTESIAN_POINT('Ctrl Pts',(-4.02530289900006,5.2,-2.08161825400001));
#317677=CARTESIAN_POINT('Ctrl Pts',(-4.02530289900006,2.2,-2.08161825400001));
#317678=CARTESIAN_POINT('Ctrl Pts',(-4.02660589200006,12.2,-2.08351969100002));
#317679=CARTESIAN_POINT('Ctrl Pts',(-4.02660589200006,5.2,-2.08351969100002));
#317680=CARTESIAN_POINT('Ctrl Pts',(-4.02660589200006,2.2,-2.08351969100002));
#317681=CARTESIAN_POINT('Ctrl Pts',(-4.02790894500006,12.2,-2.08542560700002));
#317682=CARTESIAN_POINT('Ctrl Pts',(-4.02790894500006,5.2,-2.08542560700002));
#317683=CARTESIAN_POINT('Ctrl Pts',(-4.02790894500006,2.2,-2.08542560700002));
#317684=CARTESIAN_POINT('Ctrl Pts',(-4.02921204900006,12.2,-2.08733600100001));
#317685=CARTESIAN_POINT('Ctrl Pts',(-4.02921204900006,5.2,-2.08733600100001));
#317686=CARTESIAN_POINT('Ctrl Pts',(-4.02921204900006,2.2,-2.08733600100001));
#317687=CARTESIAN_POINT('Ctrl Pts',(-4.03051519400006,12.2,-2.08925087000001));
#317688=CARTESIAN_POINT('Ctrl Pts',(-4.03051519400006,5.2,-2.08925087000001));
#317689=CARTESIAN_POINT('Ctrl Pts',(-4.03051519400006,2.2,-2.08925087000001));
#317690=CARTESIAN_POINT('Ctrl Pts',(-4.03181837200006,12.2,-2.09117021300001));
#317691=CARTESIAN_POINT('Ctrl Pts',(-4.03181837200006,5.2,-2.09117021300001));
#317692=CARTESIAN_POINT('Ctrl Pts',(-4.03181837200006,2.2,-2.09117021300001));
#317693=CARTESIAN_POINT('Ctrl Pts',(-4.03312157100006,12.2,-2.09309403000002));
#317694=CARTESIAN_POINT('Ctrl Pts',(-4.03312157100006,5.2,-2.09309403000002));
#317695=CARTESIAN_POINT('Ctrl Pts',(-4.03312157100006,2.2,-2.09309403000002));
#317696=CARTESIAN_POINT('Ctrl Pts',(-4.03442478300006,12.2,-2.09502231700001));
#317697=CARTESIAN_POINT('Ctrl Pts',(-4.03442478300006,5.2,-2.09502231700001));
#317698=CARTESIAN_POINT('Ctrl Pts',(-4.03442478300006,2.2,-2.09502231700001));
#317699=CARTESIAN_POINT('Ctrl Pts',(-4.03572799900005,12.2,-2.09695507500001));
#317700=CARTESIAN_POINT('Ctrl Pts',(-4.03572799900005,5.2,-2.09695507500001));
#317701=CARTESIAN_POINT('Ctrl Pts',(-4.03572799900005,2.2,-2.09695507500001));
#317702=CARTESIAN_POINT('Ctrl Pts',(-4.03703120800006,12.2,-2.09889230200002));
#317703=CARTESIAN_POINT('Ctrl Pts',(-4.03703120800006,5.2,-2.09889230200002));
#317704=CARTESIAN_POINT('Ctrl Pts',(-4.03703120800006,2.2,-2.09889230200002));
#317705=CARTESIAN_POINT('Ctrl Pts',(-4.03833440100006,12.2,-2.10083399500002));
#317706=CARTESIAN_POINT('Ctrl Pts',(-4.03833440100006,5.2,-2.10083399500002));
#317707=CARTESIAN_POINT('Ctrl Pts',(-4.03833440100006,2.2,-2.10083399500002));
#317708=CARTESIAN_POINT('Ctrl Pts',(-4.03963757000006,12.2,-2.10278015200001));
#317709=CARTESIAN_POINT('Ctrl Pts',(-4.03963757000006,5.2,-2.10278015200001));
#317710=CARTESIAN_POINT('Ctrl Pts',(-4.03963757000006,2.2,-2.10278015200001));
#317711=CARTESIAN_POINT('Ctrl Pts',(-4.04094070300006,12.2,-2.10473077400001));
#317712=CARTESIAN_POINT('Ctrl Pts',(-4.04094070300006,5.2,-2.10473077400001));
#317713=CARTESIAN_POINT('Ctrl Pts',(-4.04094070300006,2.2,-2.10473077400001));
#317714=CARTESIAN_POINT('Ctrl Pts',(-4.04224379200006,12.2,-2.10668585800001));
#317715=CARTESIAN_POINT('Ctrl Pts',(-4.04224379200006,5.2,-2.10668585800001));
#317716=CARTESIAN_POINT('Ctrl Pts',(-4.04224379200006,2.2,-2.10668585800001));
#317717=CARTESIAN_POINT('Ctrl Pts',(-4.04354682900006,12.2,-2.10864540100001));
#317718=CARTESIAN_POINT('Ctrl Pts',(-4.04354682900006,5.2,-2.10864540100001));
#317719=CARTESIAN_POINT('Ctrl Pts',(-4.04354682900006,2.2,-2.10864540100001));
#317720=CARTESIAN_POINT('Ctrl Pts',(-4.04484980300006,12.2,-2.11060940500001));
#317721=CARTESIAN_POINT('Ctrl Pts',(-4.04484980300006,5.2,-2.11060940500001));
#317722=CARTESIAN_POINT('Ctrl Pts',(-4.04484980300006,2.2,-2.11060940500001));
#317723=CARTESIAN_POINT('Ctrl Pts',(-4.04615270400006,12.2,-2.11257786500001));
#317724=CARTESIAN_POINT('Ctrl Pts',(-4.04615270400006,5.2,-2.11257786500001));
#317725=CARTESIAN_POINT('Ctrl Pts',(-4.04615270400006,2.2,-2.11257786500001));
#317726=CARTESIAN_POINT('Ctrl Pts',(-4.04745552300006,12.2,-2.11455078000002));
#317727=CARTESIAN_POINT('Ctrl Pts',(-4.04745552300006,5.2,-2.11455078000002));
#317728=CARTESIAN_POINT('Ctrl Pts',(-4.04745552300006,2.2,-2.11455078000002));
#317729=CARTESIAN_POINT('Ctrl Pts',(-4.04875825300006,12.2,-2.11652814900001));
#317730=CARTESIAN_POINT('Ctrl Pts',(-4.04875825300006,5.2,-2.11652814900001));
#317731=CARTESIAN_POINT('Ctrl Pts',(-4.04875825300006,2.2,-2.11652814900001));
#317732=CARTESIAN_POINT('Ctrl Pts',(-4.05006088200006,12.2,-2.11850997100001));
#317733=CARTESIAN_POINT('Ctrl Pts',(-4.05006088200006,5.2,-2.11850997100001));
#317734=CARTESIAN_POINT('Ctrl Pts',(-4.05006088200006,2.2,-2.11850997100001));
#317735=CARTESIAN_POINT('Ctrl Pts',(-4.05136340100006,12.2,-2.12049624400001));
#317736=CARTESIAN_POINT('Ctrl Pts',(-4.05136340100006,5.2,-2.12049624400001));
#317737=CARTESIAN_POINT('Ctrl Pts',(-4.05136340100006,2.2,-2.12049624400001));
#317738=CARTESIAN_POINT('Ctrl Pts',(-4.05266580100006,12.2,-2.12248696500001));
#317739=CARTESIAN_POINT('Ctrl Pts',(-4.05266580100006,5.2,-2.12248696500001));
#317740=CARTESIAN_POINT('Ctrl Pts',(-4.05266580100006,2.2,-2.12248696500001));
#317741=CARTESIAN_POINT('Ctrl Pts',(-4.05396807400006,12.2,-2.12448213400001));
#317742=CARTESIAN_POINT('Ctrl Pts',(-4.05396807400006,5.2,-2.12448213400001));
#317743=CARTESIAN_POINT('Ctrl Pts',(-4.05396807400006,2.2,-2.12448213400001));
#317744=CARTESIAN_POINT('Ctrl Pts',(-4.05527020900006,12.2,-2.12648174800002));
#317745=CARTESIAN_POINT('Ctrl Pts',(-4.05527020900006,5.2,-2.12648174800002));
#317746=CARTESIAN_POINT('Ctrl Pts',(-4.05527020900006,2.2,-2.12648174800002));
#317747=CARTESIAN_POINT('Ctrl Pts',(-4.05657219900006,12.2,-2.12848580600001));
#317748=CARTESIAN_POINT('Ctrl Pts',(-4.05657219900006,5.2,-2.12848580600001));
#317749=CARTESIAN_POINT('Ctrl Pts',(-4.05657219900006,2.2,-2.12848580600001));
#317750=CARTESIAN_POINT('Ctrl Pts',(-4.05787403100006,12.2,-2.13049430600002));
#317751=CARTESIAN_POINT('Ctrl Pts',(-4.05787403100006,5.2,-2.13049430600002));
#317752=CARTESIAN_POINT('Ctrl Pts',(-4.05787403100006,2.2,-2.13049430600002));
#317753=CARTESIAN_POINT('Ctrl Pts',(-4.05917569900006,12.2,-2.13250724700002));
#317754=CARTESIAN_POINT('Ctrl Pts',(-4.05917569900006,5.2,-2.13250724700002));
#317755=CARTESIAN_POINT('Ctrl Pts',(-4.05917569900006,2.2,-2.13250724700002));
#317756=CARTESIAN_POINT('Ctrl Pts',(-4.06047719200005,12.2,-2.13452462600001));
#317757=CARTESIAN_POINT('Ctrl Pts',(-4.06047719200005,5.2,-2.13452462600001));
#317758=CARTESIAN_POINT('Ctrl Pts',(-4.06047719200005,2.2,-2.13452462600001));
#317759=CARTESIAN_POINT('Ctrl Pts',(-4.06177850300006,12.2,-2.13654644300002));
#317760=CARTESIAN_POINT('Ctrl Pts',(-4.06177850300006,5.2,-2.13654644300002));
#317761=CARTESIAN_POINT('Ctrl Pts',(-4.06177850300006,2.2,-2.13654644300002));
#317762=CARTESIAN_POINT('Ctrl Pts',(-4.06307962000006,12.2,-2.13857269400001));
#317763=CARTESIAN_POINT('Ctrl Pts',(-4.06307962000006,5.2,-2.13857269400001));
#317764=CARTESIAN_POINT('Ctrl Pts',(-4.06307962000006,2.2,-2.13857269400001));
#317765=CARTESIAN_POINT('Ctrl Pts',(-4.06438053600006,12.2,-2.14060338000001));
#317766=CARTESIAN_POINT('Ctrl Pts',(-4.06438053600006,5.2,-2.14060338000001));
#317767=CARTESIAN_POINT('Ctrl Pts',(-4.06438053600006,2.2,-2.14060338000001));
#317768=CARTESIAN_POINT('Ctrl Pts',(-4.06568124100006,12.2,-2.14263849600002));
#317769=CARTESIAN_POINT('Ctrl Pts',(-4.06568124100006,5.2,-2.14263849600002));
#317770=CARTESIAN_POINT('Ctrl Pts',(-4.06568124100006,2.2,-2.14263849600002));
#317771=CARTESIAN_POINT('Ctrl Pts',(-4.06698172500006,12.2,-2.14467804200002));
#317772=CARTESIAN_POINT('Ctrl Pts',(-4.06698172500006,5.2,-2.14467804200002));
#317773=CARTESIAN_POINT('Ctrl Pts',(-4.06698172500006,2.2,-2.14467804200002));
#317774=CARTESIAN_POINT('Ctrl Pts',(-4.06828198000006,12.2,-2.14672201700001));
#317775=CARTESIAN_POINT('Ctrl Pts',(-4.06828198000006,5.2,-2.14672201700001));
#317776=CARTESIAN_POINT('Ctrl Pts',(-4.06828198000006,2.2,-2.14672201700001));
#317777=CARTESIAN_POINT('Ctrl Pts',(-4.06958199700005,12.2,-2.14877041800001));
#317778=CARTESIAN_POINT('Ctrl Pts',(-4.06958199700005,5.2,-2.14877041800001));
#317779=CARTESIAN_POINT('Ctrl Pts',(-4.06958199700005,2.2,-2.14877041800001));
#317780=CARTESIAN_POINT('Ctrl Pts',(-4.07088176800006,12.2,-2.15082324300001));
#317781=CARTESIAN_POINT('Ctrl Pts',(-4.07088176800006,5.2,-2.15082324300001));
#317782=CARTESIAN_POINT('Ctrl Pts',(-4.07088176800006,2.2,-2.15082324300001));
#317783=CARTESIAN_POINT('Ctrl Pts',(-4.07218128100006,12.2,-2.15288049100002));
#317784=CARTESIAN_POINT('Ctrl Pts',(-4.07218128100006,5.2,-2.15288049100002));
#317785=CARTESIAN_POINT('Ctrl Pts',(-4.07218128100006,2.2,-2.15288049100002));
#317786=CARTESIAN_POINT('Ctrl Pts',(-4.07348052800006,12.2,-2.15494216100002));
#317787=CARTESIAN_POINT('Ctrl Pts',(-4.07348052800006,5.2,-2.15494216100002));
#317788=CARTESIAN_POINT('Ctrl Pts',(-4.07348052800006,2.2,-2.15494216100002));
#317789=CARTESIAN_POINT('Ctrl Pts',(-4.07477950200006,12.2,-2.15700824800001));
#317790=CARTESIAN_POINT('Ctrl Pts',(-4.07477950200006,5.2,-2.15700824800001));
#317791=CARTESIAN_POINT('Ctrl Pts',(-4.07477950200006,2.2,-2.15700824800001));
#317792=CARTESIAN_POINT('Ctrl Pts',(-4.07607819100006,12.2,-2.15907875300001));
#317793=CARTESIAN_POINT('Ctrl Pts',(-4.07607819100006,5.2,-2.15907875300001));
#317794=CARTESIAN_POINT('Ctrl Pts',(-4.07607819100006,2.2,-2.15907875300001));
#317795=CARTESIAN_POINT('Ctrl Pts',(-4.07737658800006,12.2,-2.16115367400001));
#317796=CARTESIAN_POINT('Ctrl Pts',(-4.07737658800006,5.2,-2.16115367400001));
#317797=CARTESIAN_POINT('Ctrl Pts',(-4.07737658800006,2.2,-2.16115367400001));
#317798=CARTESIAN_POINT('Ctrl Pts',(-4.07867468300006,12.2,-2.16323300600001));
#317799=CARTESIAN_POINT('Ctrl Pts',(-4.07867468300006,5.2,-2.16323300600001));
#317800=CARTESIAN_POINT('Ctrl Pts',(-4.07867468300006,2.2,-2.16323300600001));
#317801=CARTESIAN_POINT('Ctrl Pts',(-4.07997246700006,12.2,-2.16531675200001));
#317802=CARTESIAN_POINT('Ctrl Pts',(-4.07997246700006,5.2,-2.16531675200001));
#317803=CARTESIAN_POINT('Ctrl Pts',(-4.07997246700006,2.2,-2.16531675200001));
#317804=CARTESIAN_POINT('Ctrl Pts',(-4.08126993200006,12.2,-2.16740490600001));
#317805=CARTESIAN_POINT('Ctrl Pts',(-4.08126993200006,5.2,-2.16740490600001));
#317806=CARTESIAN_POINT('Ctrl Pts',(-4.08126993200006,2.2,-2.16740490600001));
#317807=CARTESIAN_POINT('Ctrl Pts',(-4.08256706800006,12.2,-2.16949746900001));
#317808=CARTESIAN_POINT('Ctrl Pts',(-4.08256706800006,5.2,-2.16949746900001));
#317809=CARTESIAN_POINT('Ctrl Pts',(-4.08256706800006,2.2,-2.16949746900001));
#317810=CARTESIAN_POINT('Ctrl Pts',(-4.08386386600006,12.2,-2.17159443700002));
#317811=CARTESIAN_POINT('Ctrl Pts',(-4.08386386600006,5.2,-2.17159443700002));
#317812=CARTESIAN_POINT('Ctrl Pts',(-4.08386386600006,2.2,-2.17159443700002));
#317813=CARTESIAN_POINT('Ctrl Pts',(-4.08516031900006,12.2,-2.17369580900002));
#317814=CARTESIAN_POINT('Ctrl Pts',(-4.08516031900006,5.2,-2.17369580900002));
#317815=CARTESIAN_POINT('Ctrl Pts',(-4.08516031900006,2.2,-2.17369580900002));
#317816=CARTESIAN_POINT('Ctrl Pts',(-4.08645641600006,12.2,-2.17580158300001));
#317817=CARTESIAN_POINT('Ctrl Pts',(-4.08645641600006,5.2,-2.17580158300001));
#317818=CARTESIAN_POINT('Ctrl Pts',(-4.08645641600006,2.2,-2.17580158300001));
#317819=CARTESIAN_POINT('Ctrl Pts',(-4.08775214800006,12.2,-2.17791175600001));
#317820=CARTESIAN_POINT('Ctrl Pts',(-4.08775214800006,5.2,-2.17791175600001));
#317821=CARTESIAN_POINT('Ctrl Pts',(-4.08775214800006,2.2,-2.17791175600001));
#317822=CARTESIAN_POINT('Ctrl Pts',(-4.08904750600006,12.2,-2.18002632800002));
#317823=CARTESIAN_POINT('Ctrl Pts',(-4.08904750600006,5.2,-2.18002632800002));
#317824=CARTESIAN_POINT('Ctrl Pts',(-4.08904750600006,2.2,-2.18002632800002));
#317825=CARTESIAN_POINT('Ctrl Pts',(-4.09034248300006,12.2,-2.18214529600001));
#317826=CARTESIAN_POINT('Ctrl Pts',(-4.09034248300006,5.2,-2.18214529600001));
#317827=CARTESIAN_POINT('Ctrl Pts',(-4.09034248300006,2.2,-2.18214529600001));
#317828=CARTESIAN_POINT('Ctrl Pts',(-4.09163706900006,12.2,-2.18426865800001));
#317829=CARTESIAN_POINT('Ctrl Pts',(-4.09163706900006,5.2,-2.18426865800001));
#317830=CARTESIAN_POINT('Ctrl Pts',(-4.09163706900006,2.2,-2.18426865800001));
#317831=CARTESIAN_POINT('Ctrl Pts',(-4.09293125500006,12.2,-2.18639641200001));
#317832=CARTESIAN_POINT('Ctrl Pts',(-4.09293125500006,5.2,-2.18639641200001));
#317833=CARTESIAN_POINT('Ctrl Pts',(-4.09293125500006,2.2,-2.18639641200001));
#317834=CARTESIAN_POINT('Ctrl Pts',(-4.09422503200005,12.2,-2.18852855500002));
#317835=CARTESIAN_POINT('Ctrl Pts',(-4.09422503200005,5.2,-2.18852855500002));
#317836=CARTESIAN_POINT('Ctrl Pts',(-4.09422503200005,2.2,-2.18852855500002));
#317837=CARTESIAN_POINT('Ctrl Pts',(-4.09551839200006,12.2,-2.19066508800001));
#317838=CARTESIAN_POINT('Ctrl Pts',(-4.09551839200006,5.2,-2.19066508800001));
#317839=CARTESIAN_POINT('Ctrl Pts',(-4.09551839200006,2.2,-2.19066508800001));
#317840=CARTESIAN_POINT('Ctrl Pts',(-4.09681132600006,12.2,-2.19280600600001));
#317841=CARTESIAN_POINT('Ctrl Pts',(-4.09681132600006,5.2,-2.19280600600001));
#317842=CARTESIAN_POINT('Ctrl Pts',(-4.09681132600006,2.2,-2.19280600600001));
#317843=CARTESIAN_POINT('Ctrl Pts',(-4.09810382400006,12.2,-2.19495130900001));
#317844=CARTESIAN_POINT('Ctrl Pts',(-4.09810382400006,5.2,-2.19495130900001));
#317845=CARTESIAN_POINT('Ctrl Pts',(-4.09810382400006,2.2,-2.19495130900001));
#317846=CARTESIAN_POINT('Ctrl Pts',(-4.09939587800006,12.2,-2.19710099300002));
#317847=CARTESIAN_POINT('Ctrl Pts',(-4.09939587800006,5.2,-2.19710099300002));
#317848=CARTESIAN_POINT('Ctrl Pts',(-4.09939587800006,2.2,-2.19710099300002));
#317849=CARTESIAN_POINT('Ctrl Pts',(-4.10068748000006,12.2,-2.19925505700001));
#317850=CARTESIAN_POINT('Ctrl Pts',(-4.10068748000006,5.2,-2.19925505700001));
#317851=CARTESIAN_POINT('Ctrl Pts',(-4.10068748000006,2.2,-2.19925505700001));
#317852=CARTESIAN_POINT('Ctrl Pts',(-4.10197862000006,12.2,-2.20141350000001));
#317853=CARTESIAN_POINT('Ctrl Pts',(-4.10197862000006,5.2,-2.20141350000001));
#317854=CARTESIAN_POINT('Ctrl Pts',(-4.10197862000006,2.2,-2.20141350000001));
#317855=CARTESIAN_POINT('Ctrl Pts',(-4.10326929000006,12.2,-2.20357631800002));
#317856=CARTESIAN_POINT('Ctrl Pts',(-4.10326929000006,5.2,-2.20357631800002));
#317857=CARTESIAN_POINT('Ctrl Pts',(-4.10326929000006,2.2,-2.20357631800002));
#317858=CARTESIAN_POINT('Ctrl Pts',(-4.10455948100005,12.2,-2.20574351000002));
#317859=CARTESIAN_POINT('Ctrl Pts',(-4.10455948100005,5.2,-2.20574351000002));
#317860=CARTESIAN_POINT('Ctrl Pts',(-4.10455948100005,2.2,-2.20574351000002));
#317861=CARTESIAN_POINT('Ctrl Pts',(-4.10584918400006,12.2,-2.20791507400001));
#317862=CARTESIAN_POINT('Ctrl Pts',(-4.10584918400006,5.2,-2.20791507400001));
#317863=CARTESIAN_POINT('Ctrl Pts',(-4.10584918400006,2.2,-2.20791507400001));
#317864=CARTESIAN_POINT('Ctrl Pts',(-4.10713839100006,12.2,-2.21009100700002));
#317865=CARTESIAN_POINT('Ctrl Pts',(-4.10713839100006,5.2,-2.21009100700002));
#317866=CARTESIAN_POINT('Ctrl Pts',(-4.10713839100006,2.2,-2.21009100700002));
#317867=CARTESIAN_POINT('Ctrl Pts',(-4.10842709300006,12.2,-2.21227130800001));
#317868=CARTESIAN_POINT('Ctrl Pts',(-4.10842709300006,5.2,-2.21227130800001));
#317869=CARTESIAN_POINT('Ctrl Pts',(-4.10842709300006,2.2,-2.21227130800001));
#317870=CARTESIAN_POINT('Ctrl Pts',(-4.10971528100006,12.2,-2.21445597400002));
#317871=CARTESIAN_POINT('Ctrl Pts',(-4.10971528100006,5.2,-2.21445597400002));
#317872=CARTESIAN_POINT('Ctrl Pts',(-4.10971528100006,2.2,-2.21445597400002));
#317873=CARTESIAN_POINT('Ctrl Pts',(-4.11100294700006,12.2,-2.21664500400002));
#317874=CARTESIAN_POINT('Ctrl Pts',(-4.11100294700006,5.2,-2.21664500400002));
#317875=CARTESIAN_POINT('Ctrl Pts',(-4.11100294700006,2.2,-2.21664500400002));
#317876=CARTESIAN_POINT('Ctrl Pts',(-4.11229008200006,12.2,-2.21883839500002));
#317877=CARTESIAN_POINT('Ctrl Pts',(-4.11229008200006,5.2,-2.21883839500002));
#317878=CARTESIAN_POINT('Ctrl Pts',(-4.11229008200006,2.2,-2.21883839500002));
#317879=CARTESIAN_POINT('Ctrl Pts',(-4.11357667600006,12.2,-2.22103614500002));
#317880=CARTESIAN_POINT('Ctrl Pts',(-4.11357667600006,5.2,-2.22103614500002));
#317881=CARTESIAN_POINT('Ctrl Pts',(-4.11357667600006,2.2,-2.22103614500002));
#317882=CARTESIAN_POINT('Ctrl Pts',(-4.11486272300006,12.2,-2.22323825200001));
#317883=CARTESIAN_POINT('Ctrl Pts',(-4.11486272300006,5.2,-2.22323825200001));
#317884=CARTESIAN_POINT('Ctrl Pts',(-4.11486272300006,2.2,-2.22323825200001));
#317885=CARTESIAN_POINT('Ctrl Pts',(-4.11614821300006,12.2,-2.22544471500001));
#317886=CARTESIAN_POINT('Ctrl Pts',(-4.11614821300006,5.2,-2.22544471500001));
#317887=CARTESIAN_POINT('Ctrl Pts',(-4.11614821300006,2.2,-2.22544471500001));
#317888=CARTESIAN_POINT('Ctrl Pts',(-4.11743313600006,12.2,-2.22765552900002));
#317889=CARTESIAN_POINT('Ctrl Pts',(-4.11743313600006,5.2,-2.22765552900002));
#317890=CARTESIAN_POINT('Ctrl Pts',(-4.11743313600006,2.2,-2.22765552900002));
#317891=CARTESIAN_POINT('Ctrl Pts',(-4.11871748700006,12.2,-2.22987069300002));
#317892=CARTESIAN_POINT('Ctrl Pts',(-4.11871748700006,5.2,-2.22987069300002));
#317893=CARTESIAN_POINT('Ctrl Pts',(-4.11871748700006,2.2,-2.22987069300002));
#317894=CARTESIAN_POINT('Ctrl Pts',(-4.12000125400006,12.2,-2.23209020600001));
#317895=CARTESIAN_POINT('Ctrl Pts',(-4.12000125400006,5.2,-2.23209020600001));
#317896=CARTESIAN_POINT('Ctrl Pts',(-4.12000125400006,2.2,-2.23209020600001));
#317897=CARTESIAN_POINT('Ctrl Pts',(-4.12128443000006,12.2,-2.23431406600001));
#317898=CARTESIAN_POINT('Ctrl Pts',(-4.12128443000006,5.2,-2.23431406600001));
#317899=CARTESIAN_POINT('Ctrl Pts',(-4.12128443000006,2.2,-2.23431406600001));
#317900=CARTESIAN_POINT('Ctrl Pts',(-4.12256700600006,12.2,-2.23654226800001));
#317901=CARTESIAN_POINT('Ctrl Pts',(-4.12256700600006,5.2,-2.23654226800001));
#317902=CARTESIAN_POINT('Ctrl Pts',(-4.12256700600006,2.2,-2.23654226800001));
#317903=CARTESIAN_POINT('Ctrl Pts',(-4.12384897300006,12.2,-2.23877481400002));
#317904=CARTESIAN_POINT('Ctrl Pts',(-4.12384897300006,5.2,-2.23877481400002));
#317905=CARTESIAN_POINT('Ctrl Pts',(-4.12384897300006,2.2,-2.23877481400002));
#317906=CARTESIAN_POINT('Ctrl Pts',(-4.12513032400006,12.2,-2.24101169700001));
#317907=CARTESIAN_POINT('Ctrl Pts',(-4.12513032400006,5.2,-2.24101169700001));
#317908=CARTESIAN_POINT('Ctrl Pts',(-4.12513032400006,2.2,-2.24101169700001));
#317909=CARTESIAN_POINT('Ctrl Pts',(-4.12641104900006,12.2,-2.24325291900001));
#317910=CARTESIAN_POINT('Ctrl Pts',(-4.12641104900006,5.2,-2.24325291900001));
#317911=CARTESIAN_POINT('Ctrl Pts',(-4.12641104900006,2.2,-2.24325291900001));
#317912=CARTESIAN_POINT('Ctrl Pts',(-4.12769114100006,12.2,-2.24549847600001));
#317913=CARTESIAN_POINT('Ctrl Pts',(-4.12769114100006,5.2,-2.24549847600001));
#317914=CARTESIAN_POINT('Ctrl Pts',(-4.12769114100006,2.2,-2.24549847600001));
#317915=CARTESIAN_POINT('Ctrl Pts',(-4.12897059200006,12.2,-2.24774836500002));
#317916=CARTESIAN_POINT('Ctrl Pts',(-4.12897059200006,5.2,-2.24774836500002));
#317917=CARTESIAN_POINT('Ctrl Pts',(-4.12897059200006,2.2,-2.24774836500002));
#317918=CARTESIAN_POINT('Ctrl Pts',(-4.13024939300006,12.2,-2.25000258600002));
#317919=CARTESIAN_POINT('Ctrl Pts',(-4.13024939300006,5.2,-2.25000258600002));
#317920=CARTESIAN_POINT('Ctrl Pts',(-4.13024939300006,2.2,-2.25000258600002));
#317921=CARTESIAN_POINT('Ctrl Pts',(-4.13152753300006,12.2,-2.25226113500002));
#317922=CARTESIAN_POINT('Ctrl Pts',(-4.13152753300006,5.2,-2.25226113500002));
#317923=CARTESIAN_POINT('Ctrl Pts',(-4.13152753300006,2.2,-2.25226113500002));
#317924=CARTESIAN_POINT('Ctrl Pts',(-4.13280500400006,12.2,-2.25452400900001));
#317925=CARTESIAN_POINT('Ctrl Pts',(-4.13280500400006,5.2,-2.25452400900001));
#317926=CARTESIAN_POINT('Ctrl Pts',(-4.13280500400006,2.2,-2.25452400900001));
#317927=CARTESIAN_POINT('Ctrl Pts',(-4.13408180000006,12.2,-2.25679120600002));
#317928=CARTESIAN_POINT('Ctrl Pts',(-4.13408180000006,5.2,-2.25679120600002));
#317929=CARTESIAN_POINT('Ctrl Pts',(-4.13408180000006,2.2,-2.25679120600002));
#317930=CARTESIAN_POINT('Ctrl Pts',(-4.13535791000006,12.2,-2.25906272500001));
#317931=CARTESIAN_POINT('Ctrl Pts',(-4.13535791000006,5.2,-2.25906272500001));
#317932=CARTESIAN_POINT('Ctrl Pts',(-4.13535791000006,2.2,-2.25906272500001));
#317933=CARTESIAN_POINT('Ctrl Pts',(-4.13663332500006,12.2,-2.26133856300001));
#317934=CARTESIAN_POINT('Ctrl Pts',(-4.13663332500006,5.2,-2.26133856300001));
#317935=CARTESIAN_POINT('Ctrl Pts',(-4.13663332500006,2.2,-2.26133856300001));
#317936=CARTESIAN_POINT('Ctrl Pts',(-4.13790803900006,12.2,-2.26361871800002));
#317937=CARTESIAN_POINT('Ctrl Pts',(-4.13790803900006,5.2,-2.26361871800002));
#317938=CARTESIAN_POINT('Ctrl Pts',(-4.13790803900006,2.2,-2.26361871800002));
#317939=CARTESIAN_POINT('Ctrl Pts',(-4.13918204600006,12.2,-2.26590318700001));
#317940=CARTESIAN_POINT('Ctrl Pts',(-4.13918204600006,5.2,-2.26590318700001));
#317941=CARTESIAN_POINT('Ctrl Pts',(-4.13918204600006,2.2,-2.26590318700001));
#317942=CARTESIAN_POINT('Ctrl Pts',(-4.14045533500006,12.2,-2.26819196900002));
#317943=CARTESIAN_POINT('Ctrl Pts',(-4.14045533500006,5.2,-2.26819196900002));
#317944=CARTESIAN_POINT('Ctrl Pts',(-4.14045533500006,2.2,-2.26819196900002));
#317945=CARTESIAN_POINT('Ctrl Pts',(-4.14172790000006,12.2,-2.27048506200001));
#317946=CARTESIAN_POINT('Ctrl Pts',(-4.14172790000006,5.2,-2.27048506200001));
#317947=CARTESIAN_POINT('Ctrl Pts',(-4.14172790000006,2.2,-2.27048506200001));
#317948=CARTESIAN_POINT('Ctrl Pts',(-4.14299973200006,12.2,-2.27278246300001));
#317949=CARTESIAN_POINT('Ctrl Pts',(-4.14299973200006,5.2,-2.27278246300001));
#317950=CARTESIAN_POINT('Ctrl Pts',(-4.14299973200006,2.2,-2.27278246300001));
#317951=CARTESIAN_POINT('Ctrl Pts',(-4.14427082400006,12.2,-2.27508416800001));
#317952=CARTESIAN_POINT('Ctrl Pts',(-4.14427082400006,5.2,-2.27508416800001));
#317953=CARTESIAN_POINT('Ctrl Pts',(-4.14427082400006,2.2,-2.27508416800001));
#317954=CARTESIAN_POINT('Ctrl Pts',(-4.14554116200006,12.2,-2.27739017700001));
#317955=CARTESIAN_POINT('Ctrl Pts',(-4.14554116200006,5.2,-2.27739017700001));
#317956=CARTESIAN_POINT('Ctrl Pts',(-4.14554116200006,2.2,-2.27739017700001));
#317957=CARTESIAN_POINT('Ctrl Pts',(-4.14681073900006,12.2,-2.27970048600001));
#317958=CARTESIAN_POINT('Ctrl Pts',(-4.14681073900006,5.2,-2.27970048600001));
#317959=CARTESIAN_POINT('Ctrl Pts',(-4.14681073900006,2.2,-2.27970048600001));
#317960=CARTESIAN_POINT('Ctrl Pts',(-4.14807954300006,12.2,-2.28201509200002));
#317961=CARTESIAN_POINT('Ctrl Pts',(-4.14807954300006,5.2,-2.28201509200002));
#317962=CARTESIAN_POINT('Ctrl Pts',(-4.14807954300006,2.2,-2.28201509200002));
#317963=CARTESIAN_POINT('Ctrl Pts',(-4.14934756500006,12.2,-2.28433399200001));
#317964=CARTESIAN_POINT('Ctrl Pts',(-4.14934756500006,5.2,-2.28433399200001));
#317965=CARTESIAN_POINT('Ctrl Pts',(-4.14934756500006,2.2,-2.28433399200001));
#317966=CARTESIAN_POINT('Ctrl Pts',(-4.15061479800006,12.2,-2.28665718400002));
#317967=CARTESIAN_POINT('Ctrl Pts',(-4.15061479800006,5.2,-2.28665718400002));
#317968=CARTESIAN_POINT('Ctrl Pts',(-4.15061479800006,2.2,-2.28665718400002));
#317969=CARTESIAN_POINT('Ctrl Pts',(-4.15188123500006,12.2,-2.28898466500001));
#317970=CARTESIAN_POINT('Ctrl Pts',(-4.15188123500006,5.2,-2.28898466500001));
#317971=CARTESIAN_POINT('Ctrl Pts',(-4.15188123500006,2.2,-2.28898466500001));
#317972=CARTESIAN_POINT('Ctrl Pts',(-4.15314687200006,12.2,-2.29131643500001));
#317973=CARTESIAN_POINT('Ctrl Pts',(-4.15314687200006,5.2,-2.29131643500001));
#317974=CARTESIAN_POINT('Ctrl Pts',(-4.15314687200006,2.2,-2.29131643500001));
#317975=CARTESIAN_POINT('Ctrl Pts',(-4.15441170800006,12.2,-2.29365249400002));
#317976=CARTESIAN_POINT('Ctrl Pts',(-4.15441170800006,5.2,-2.29365249400002));
#317977=CARTESIAN_POINT('Ctrl Pts',(-4.15441170800006,2.2,-2.29365249400002));
#317978=CARTESIAN_POINT('Ctrl Pts',(-4.15542293400006,12.2,-2.29552477100002));
#317979=CARTESIAN_POINT('Ctrl Pts',(-4.15542293400006,5.2,-2.29552477100002));
#317980=CARTESIAN_POINT('Ctrl Pts',(-4.15542293400006,2.2,-2.29552477100002));
#317981=CARTESIAN_POINT('Ctrl Pts',(-4.15618099200006,12.2,-2.29693090800001));
#317982=CARTESIAN_POINT('Ctrl Pts',(-4.15618099200006,5.2,-2.29693090800001));
#317983=CARTESIAN_POINT('Ctrl Pts',(-4.15618099200006,2.2,-2.29693090800001));
#317984=CARTESIAN_POINT('Ctrl Pts',(-4.15668620300006,12.2,-2.29786919000002));
#317985=CARTESIAN_POINT('Ctrl Pts',(-4.15668620300006,5.2,-2.29786919000002));
#317986=CARTESIAN_POINT('Ctrl Pts',(-4.15668620300006,2.2,-2.29786919000002));
#317987=CARTESIAN_POINT('Ctrl Pts',(-4.15693876900006,12.2,-2.29833854600002));
#317988=CARTESIAN_POINT('Ctrl Pts',(-4.15693876900006,5.2,-2.29833854600002));
#317989=CARTESIAN_POINT('Ctrl Pts',(-4.15693876900006,2.2,-2.29833854600002));
#317990=CARTESIAN_POINT('',(-4.15693876900006,2.7,-2.29833854600002));
#317991=CARTESIAN_POINT('',(-4.15693876900006,12.2,-2.29833854600002));
#317992=CARTESIAN_POINT('Ctrl Pts',(-3.62475766000006,2.7,-1.67660193200001));
#317993=CARTESIAN_POINT('Ctrl Pts',(-3.62490182724496,2.7,-1.67666931856351));
#317994=CARTESIAN_POINT('Ctrl Pts',(-3.62504534863998,2.69999999999987,
-1.67673808461024));
#317995=CARTESIAN_POINT('Ctrl Pts',(-3.62548714022601,2.69999999999987,
-1.67695103313952));
#317996=CARTESIAN_POINT('Ctrl Pts',(-3.62580033592221,2.7,-1.67710491378894));
#317997=CARTESIAN_POINT('Ctrl Pts',(-3.62712381957932,2.7,-1.67776190097245));
#317998=CARTESIAN_POINT('Ctrl Pts',(-3.62821615035642,2.7,-1.67832401661082));
#317999=CARTESIAN_POINT('Ctrl Pts',(-3.63299368465797,2.7,-1.68083337629142));
#318000=CARTESIAN_POINT('Ctrl Pts',(-3.63693276565636,2.7,-1.68304846860218));
#318001=CARTESIAN_POINT('Ctrl Pts',(-3.65406401132597,2.7,-1.69305178840937));
#318002=CARTESIAN_POINT('Ctrl Pts',(-3.66795497508814,2.7,-1.70223215619653));
#318003=CARTESIAN_POINT('Ctrl Pts',(-3.71732841422647,2.7,-1.73712959869733));
#318004=CARTESIAN_POINT('Ctrl Pts',(-3.76195508351362,2.7,-1.77364496801825));
#318005=CARTESIAN_POINT('Ctrl Pts',(-3.90832243976127,2.7,-1.91812530395877));
#318006=CARTESIAN_POINT('Ctrl Pts',(-4.03404336095063,2.7,-2.06995587715245));
#318007=CARTESIAN_POINT('Ctrl Pts',(-4.15693876900006,2.7,-2.29833854600002));
#318008=CARTESIAN_POINT('Origin',(-5.66300478732629E-14,15.2,-1.77635683940025E-14));
#318009=CARTESIAN_POINT('',(-3.98353538000006,2.7,-2.58726610100002));
#318010=CARTESIAN_POINT('',(-3.98353538000006,12.2,-2.58726610100001));
#318011=CARTESIAN_POINT('Origin',(-5.66300478732629E-14,2.7,-1.92943768261394E-14));
#318012=CARTESIAN_POINT('Ctrl Pts',(-3.98353538000006,12.2,-2.58726610100001));
#318013=CARTESIAN_POINT('Ctrl Pts',(-3.98353538000006,5.2,-2.58726610100001));
#318014=CARTESIAN_POINT('Ctrl Pts',(-3.98353538000006,2.2,-2.58726610100001));
#318015=CARTESIAN_POINT('Ctrl Pts',(-3.98300238900006,12.2,-2.58726399500001));
#318016=CARTESIAN_POINT('Ctrl Pts',(-3.98300238900006,5.2,-2.58726399500001));
#318017=CARTESIAN_POINT('Ctrl Pts',(-3.98300238900006,2.2,-2.58726399500001));
#318018=CARTESIAN_POINT('Ctrl Pts',(-3.98193674700006,12.2,-2.58725951100002));
#318019=CARTESIAN_POINT('Ctrl Pts',(-3.98193674700006,5.2,-2.58725951100002));
#318020=CARTESIAN_POINT('Ctrl Pts',(-3.98193674700006,2.2,-2.58725951100002));
#318021=CARTESIAN_POINT('Ctrl Pts',(-3.98033930600006,12.2,-2.58725196700002));
#318022=CARTESIAN_POINT('Ctrl Pts',(-3.98033930600006,5.2,-2.58725196700002));
#318023=CARTESIAN_POINT('Ctrl Pts',(-3.98033930600006,2.2,-2.58725196700002));
#318024=CARTESIAN_POINT('Ctrl Pts',(-3.97821142800006,12.2,-2.58724027300001));
#318025=CARTESIAN_POINT('Ctrl Pts',(-3.97821142800006,5.2,-2.58724027300001));
#318026=CARTESIAN_POINT('Ctrl Pts',(-3.97821142800006,2.2,-2.58724027300001));
#318027=CARTESIAN_POINT('Ctrl Pts',(-3.97555498800005,12.2,-2.58722293000002));
#318028=CARTESIAN_POINT('Ctrl Pts',(-3.97555498800005,5.2,-2.58722293000002));
#318029=CARTESIAN_POINT('Ctrl Pts',(-3.97555498800005,2.2,-2.58722293000002));
#318030=CARTESIAN_POINT('Ctrl Pts',(-3.97290195400006,12.2,-2.58720286100001));
#318031=CARTESIAN_POINT('Ctrl Pts',(-3.97290195400006,5.2,-2.58720286100001));
#318032=CARTESIAN_POINT('Ctrl Pts',(-3.97290195400006,2.2,-2.58720286100001));
#318033=CARTESIAN_POINT('Ctrl Pts',(-3.97025232800006,12.2,-2.58718007100001));
#318034=CARTESIAN_POINT('Ctrl Pts',(-3.97025232800006,5.2,-2.58718007100001));
#318035=CARTESIAN_POINT('Ctrl Pts',(-3.97025232800006,2.2,-2.58718007100001));
#318036=CARTESIAN_POINT('Ctrl Pts',(-3.96760611500006,12.2,-2.58715456000001));
#318037=CARTESIAN_POINT('Ctrl Pts',(-3.96760611500006,5.2,-2.58715456000001));
#318038=CARTESIAN_POINT('Ctrl Pts',(-3.96760611500006,2.2,-2.58715456000001));
#318039=CARTESIAN_POINT('Ctrl Pts',(-3.96496331700006,12.2,-2.58712633300001));
#318040=CARTESIAN_POINT('Ctrl Pts',(-3.96496331700006,5.2,-2.58712633300001));
#318041=CARTESIAN_POINT('Ctrl Pts',(-3.96496331700006,2.2,-2.58712633300001));
#318042=CARTESIAN_POINT('Ctrl Pts',(-3.96232394100006,12.2,-2.58709539700002));
#318043=CARTESIAN_POINT('Ctrl Pts',(-3.96232394100006,5.2,-2.58709539700002));
#318044=CARTESIAN_POINT('Ctrl Pts',(-3.96232394100006,2.2,-2.58709539700002));
#318045=CARTESIAN_POINT('Ctrl Pts',(-3.95968799400006,12.2,-2.58706175800001));
#318046=CARTESIAN_POINT('Ctrl Pts',(-3.95968799400006,5.2,-2.58706175800001));
#318047=CARTESIAN_POINT('Ctrl Pts',(-3.95968799400006,2.2,-2.58706175800001));
#318048=CARTESIAN_POINT('Ctrl Pts',(-3.95705548200006,12.2,-2.58702542400002));
#318049=CARTESIAN_POINT('Ctrl Pts',(-3.95705548200006,5.2,-2.58702542400002));
#318050=CARTESIAN_POINT('Ctrl Pts',(-3.95705548200006,2.2,-2.58702542400002));
#318051=CARTESIAN_POINT('Ctrl Pts',(-3.95442641300006,12.2,-2.58698640200001));
#318052=CARTESIAN_POINT('Ctrl Pts',(-3.95442641300006,5.2,-2.58698640200001));
#318053=CARTESIAN_POINT('Ctrl Pts',(-3.95442641300006,2.2,-2.58698640200001));
#318054=CARTESIAN_POINT('Ctrl Pts',(-3.95180079600006,12.2,-2.58694470000002));
#318055=CARTESIAN_POINT('Ctrl Pts',(-3.95180079600006,5.2,-2.58694470000002));
#318056=CARTESIAN_POINT('Ctrl Pts',(-3.95180079600006,2.2,-2.58694470000002));
#318057=CARTESIAN_POINT('Ctrl Pts',(-3.94917863600006,12.2,-2.58690032500001));
#318058=CARTESIAN_POINT('Ctrl Pts',(-3.94917863600006,5.2,-2.58690032500001));
#318059=CARTESIAN_POINT('Ctrl Pts',(-3.94917863600006,2.2,-2.58690032500001));
#318060=CARTESIAN_POINT('Ctrl Pts',(-3.94655993800006,12.2,-2.58685328400002));
#318061=CARTESIAN_POINT('Ctrl Pts',(-3.94655993800006,5.2,-2.58685328400002));
#318062=CARTESIAN_POINT('Ctrl Pts',(-3.94655993800006,2.2,-2.58685328400002));
#318063=CARTESIAN_POINT('Ctrl Pts',(-3.94394470900005,12.2,-2.58680358300001));
#318064=CARTESIAN_POINT('Ctrl Pts',(-3.94394470900005,5.2,-2.58680358300001));
#318065=CARTESIAN_POINT('Ctrl Pts',(-3.94394470900005,2.2,-2.58680358300001));
#318066=CARTESIAN_POINT('Ctrl Pts',(-3.94133295400006,12.2,-2.58675122600001));
#318067=CARTESIAN_POINT('Ctrl Pts',(-3.94133295400006,5.2,-2.58675122600001));
#318068=CARTESIAN_POINT('Ctrl Pts',(-3.94133295400006,2.2,-2.58675122600001));
#318069=CARTESIAN_POINT('Ctrl Pts',(-3.93872467900006,12.2,-2.58669621900002));
#318070=CARTESIAN_POINT('Ctrl Pts',(-3.93872467900006,5.2,-2.58669621900002));
#318071=CARTESIAN_POINT('Ctrl Pts',(-3.93872467900006,2.2,-2.58669621900002));
#318072=CARTESIAN_POINT('Ctrl Pts',(-3.93611989000005,12.2,-2.58663856900001));
#318073=CARTESIAN_POINT('Ctrl Pts',(-3.93611989000005,5.2,-2.58663856900001));
#318074=CARTESIAN_POINT('Ctrl Pts',(-3.93611989000005,2.2,-2.58663856900001));
#318075=CARTESIAN_POINT('Ctrl Pts',(-3.93351859100005,12.2,-2.58657828100001));
#318076=CARTESIAN_POINT('Ctrl Pts',(-3.93351859100005,5.2,-2.58657828100001));
#318077=CARTESIAN_POINT('Ctrl Pts',(-3.93351859100005,2.2,-2.58657828100001));
#318078=CARTESIAN_POINT('Ctrl Pts',(-3.93092078900006,12.2,-2.58651536300002));
#318079=CARTESIAN_POINT('Ctrl Pts',(-3.93092078900006,5.2,-2.58651536300002));
#318080=CARTESIAN_POINT('Ctrl Pts',(-3.93092078900006,2.2,-2.58651536300002));
#318081=CARTESIAN_POINT('Ctrl Pts',(-3.92832648900006,12.2,-2.58644982000002));
#318082=CARTESIAN_POINT('Ctrl Pts',(-3.92832648900006,5.2,-2.58644982000002));
#318083=CARTESIAN_POINT('Ctrl Pts',(-3.92832648900006,2.2,-2.58644982000002));
#318084=CARTESIAN_POINT('Ctrl Pts',(-3.92573570000006,12.2,-2.58638165900001));
#318085=CARTESIAN_POINT('Ctrl Pts',(-3.92573570000006,5.2,-2.58638165900001));
#318086=CARTESIAN_POINT('Ctrl Pts',(-3.92573570000006,2.2,-2.58638165900001));
#318087=CARTESIAN_POINT('Ctrl Pts',(-3.92314842600006,12.2,-2.58631088600001));
#318088=CARTESIAN_POINT('Ctrl Pts',(-3.92314842600006,5.2,-2.58631088600001));
#318089=CARTESIAN_POINT('Ctrl Pts',(-3.92314842600006,2.2,-2.58631088600001));
#318090=CARTESIAN_POINT('Ctrl Pts',(-3.92056467300006,12.2,-2.58623750900002));
#318091=CARTESIAN_POINT('Ctrl Pts',(-3.92056467300006,5.2,-2.58623750900002));
#318092=CARTESIAN_POINT('Ctrl Pts',(-3.92056467300006,2.2,-2.58623750900002));
#318093=CARTESIAN_POINT('Ctrl Pts',(-3.91798444800005,12.2,-2.58616153400002));
#318094=CARTESIAN_POINT('Ctrl Pts',(-3.91798444800005,5.2,-2.58616153400002));
#318095=CARTESIAN_POINT('Ctrl Pts',(-3.91798444800005,2.2,-2.58616153400002));
#318096=CARTESIAN_POINT('Ctrl Pts',(-3.91540775700006,12.2,-2.58608296800002));
#318097=CARTESIAN_POINT('Ctrl Pts',(-3.91540775700006,5.2,-2.58608296800002));
#318098=CARTESIAN_POINT('Ctrl Pts',(-3.91540775700006,2.2,-2.58608296800002));
#318099=CARTESIAN_POINT('Ctrl Pts',(-3.91283460500006,12.2,-2.58600181500002));
#318100=CARTESIAN_POINT('Ctrl Pts',(-3.91283460500006,5.2,-2.58600181500002));
#318101=CARTESIAN_POINT('Ctrl Pts',(-3.91283460500006,2.2,-2.58600181500002));
#318102=CARTESIAN_POINT('Ctrl Pts',(-3.91026499800006,12.2,-2.58591808400002));
#318103=CARTESIAN_POINT('Ctrl Pts',(-3.91026499800006,5.2,-2.58591808400002));
#318104=CARTESIAN_POINT('Ctrl Pts',(-3.91026499800006,2.2,-2.58591808400002));
#318105=CARTESIAN_POINT('Ctrl Pts',(-3.90769894300006,12.2,-2.58583178100002));
#318106=CARTESIAN_POINT('Ctrl Pts',(-3.90769894300006,5.2,-2.58583178100002));
#318107=CARTESIAN_POINT('Ctrl Pts',(-3.90769894300006,2.2,-2.58583178100002));
#318108=CARTESIAN_POINT('Ctrl Pts',(-3.90513644400006,12.2,-2.58574291000001));
#318109=CARTESIAN_POINT('Ctrl Pts',(-3.90513644400006,5.2,-2.58574291000001));
#318110=CARTESIAN_POINT('Ctrl Pts',(-3.90513644400006,2.2,-2.58574291000001));
#318111=CARTESIAN_POINT('Ctrl Pts',(-3.90257750900005,12.2,-2.58565148100002));
#318112=CARTESIAN_POINT('Ctrl Pts',(-3.90257750900005,5.2,-2.58565148100002));
#318113=CARTESIAN_POINT('Ctrl Pts',(-3.90257750900005,2.2,-2.58565148100002));
#318114=CARTESIAN_POINT('Ctrl Pts',(-3.90002214200006,12.2,-2.58555749800002));
#318115=CARTESIAN_POINT('Ctrl Pts',(-3.90002214200006,5.2,-2.58555749800002));
#318116=CARTESIAN_POINT('Ctrl Pts',(-3.90002214200006,2.2,-2.58555749800002));
#318117=CARTESIAN_POINT('Ctrl Pts',(-3.89747035000005,12.2,-2.58546096800002));
#318118=CARTESIAN_POINT('Ctrl Pts',(-3.89747035000005,5.2,-2.58546096800002));
#318119=CARTESIAN_POINT('Ctrl Pts',(-3.89747035000005,2.2,-2.58546096800002));
#318120=CARTESIAN_POINT('Ctrl Pts',(-3.89492214000006,12.2,-2.58536190000001));
#318121=CARTESIAN_POINT('Ctrl Pts',(-3.89492214000006,5.2,-2.58536190000001));
#318122=CARTESIAN_POINT('Ctrl Pts',(-3.89492214000006,2.2,-2.58536190000001));
#318123=CARTESIAN_POINT('Ctrl Pts',(-3.89237751600006,12.2,-2.58526029800001));
#318124=CARTESIAN_POINT('Ctrl Pts',(-3.89237751600006,5.2,-2.58526029800001));
#318125=CARTESIAN_POINT('Ctrl Pts',(-3.89237751600006,2.2,-2.58526029800001));
#318126=CARTESIAN_POINT('Ctrl Pts',(-3.88983648600006,12.2,-2.58515616800001));
#318127=CARTESIAN_POINT('Ctrl Pts',(-3.88983648600006,5.2,-2.58515616800001));
#318128=CARTESIAN_POINT('Ctrl Pts',(-3.88983648600006,2.2,-2.58515616800001));
#318129=CARTESIAN_POINT('Ctrl Pts',(-3.88729905400006,12.2,-2.58504951900001));
#318130=CARTESIAN_POINT('Ctrl Pts',(-3.88729905400006,5.2,-2.58504951900001));
#318131=CARTESIAN_POINT('Ctrl Pts',(-3.88729905400006,2.2,-2.58504951900001));
#318132=CARTESIAN_POINT('Ctrl Pts',(-3.88476522700006,12.2,-2.58494035600001));
#318133=CARTESIAN_POINT('Ctrl Pts',(-3.88476522700006,5.2,-2.58494035600001));
#318134=CARTESIAN_POINT('Ctrl Pts',(-3.88476522700006,2.2,-2.58494035600001));
#318135=CARTESIAN_POINT('Ctrl Pts',(-3.88223501100006,12.2,-2.58482868700002));
#318136=CARTESIAN_POINT('Ctrl Pts',(-3.88223501100006,5.2,-2.58482868700002));
#318137=CARTESIAN_POINT('Ctrl Pts',(-3.88223501100006,2.2,-2.58482868700002));
#318138=CARTESIAN_POINT('Ctrl Pts',(-3.87970841200006,12.2,-2.58471451800002));
#318139=CARTESIAN_POINT('Ctrl Pts',(-3.87970841200006,5.2,-2.58471451800002));
#318140=CARTESIAN_POINT('Ctrl Pts',(-3.87970841200006,2.2,-2.58471451800002));
#318141=CARTESIAN_POINT('Ctrl Pts',(-3.87718543400006,12.2,-2.58459785500001));
#318142=CARTESIAN_POINT('Ctrl Pts',(-3.87718543400006,5.2,-2.58459785500001));
#318143=CARTESIAN_POINT('Ctrl Pts',(-3.87718543400006,2.2,-2.58459785500001));
#318144=CARTESIAN_POINT('Ctrl Pts',(-3.87466608600006,12.2,-2.58447870600001));
#318145=CARTESIAN_POINT('Ctrl Pts',(-3.87466608600006,5.2,-2.58447870600001));
#318146=CARTESIAN_POINT('Ctrl Pts',(-3.87466608600006,2.2,-2.58447870600001));
#318147=CARTESIAN_POINT('Ctrl Pts',(-3.87215037100006,12.2,-2.58435707700002));
#318148=CARTESIAN_POINT('Ctrl Pts',(-3.87215037100006,5.2,-2.58435707700002));
#318149=CARTESIAN_POINT('Ctrl Pts',(-3.87215037100006,2.2,-2.58435707700002));
#318150=CARTESIAN_POINT('Ctrl Pts',(-3.86963829700006,12.2,-2.58423297400002));
#318151=CARTESIAN_POINT('Ctrl Pts',(-3.86963829700006,5.2,-2.58423297400002));
#318152=CARTESIAN_POINT('Ctrl Pts',(-3.86963829700006,2.2,-2.58423297400002));
#318153=CARTESIAN_POINT('Ctrl Pts',(-3.86712987000006,12.2,-2.58410640500002));
#318154=CARTESIAN_POINT('Ctrl Pts',(-3.86712987000006,5.2,-2.58410640500002));
#318155=CARTESIAN_POINT('Ctrl Pts',(-3.86712987000006,2.2,-2.58410640500002));
#318156=CARTESIAN_POINT('Ctrl Pts',(-3.86462509500006,12.2,-2.58397737600002));
#318157=CARTESIAN_POINT('Ctrl Pts',(-3.86462509500006,5.2,-2.58397737600002));
#318158=CARTESIAN_POINT('Ctrl Pts',(-3.86462509500006,2.2,-2.58397737600002));
#318159=CARTESIAN_POINT('Ctrl Pts',(-3.86212397800006,12.2,-2.58384589300002));
#318160=CARTESIAN_POINT('Ctrl Pts',(-3.86212397800006,5.2,-2.58384589300002));
#318161=CARTESIAN_POINT('Ctrl Pts',(-3.86212397800006,2.2,-2.58384589300002));
#318162=CARTESIAN_POINT('Ctrl Pts',(-3.85962652500006,12.2,-2.58371196500002));
#318163=CARTESIAN_POINT('Ctrl Pts',(-3.85962652500006,5.2,-2.58371196500002));
#318164=CARTESIAN_POINT('Ctrl Pts',(-3.85962652500006,2.2,-2.58371196500002));
#318165=CARTESIAN_POINT('Ctrl Pts',(-3.85713274200006,12.2,-2.58357559700002));
#318166=CARTESIAN_POINT('Ctrl Pts',(-3.85713274200006,5.2,-2.58357559700002));
#318167=CARTESIAN_POINT('Ctrl Pts',(-3.85713274200006,2.2,-2.58357559700002));
#318168=CARTESIAN_POINT('Ctrl Pts',(-3.85464263400006,12.2,-2.58343679700001));
#318169=CARTESIAN_POINT('Ctrl Pts',(-3.85464263400006,5.2,-2.58343679700001));
#318170=CARTESIAN_POINT('Ctrl Pts',(-3.85464263400006,2.2,-2.58343679700001));
#318171=CARTESIAN_POINT('Ctrl Pts',(-3.85215621000006,12.2,-2.58329557100001));
#318172=CARTESIAN_POINT('Ctrl Pts',(-3.85215621000006,5.2,-2.58329557100001));
#318173=CARTESIAN_POINT('Ctrl Pts',(-3.85215621000006,2.2,-2.58329557100001));
#318174=CARTESIAN_POINT('Ctrl Pts',(-3.84967347300006,12.2,-2.58315192700001));
#318175=CARTESIAN_POINT('Ctrl Pts',(-3.84967347300006,5.2,-2.58315192700001));
#318176=CARTESIAN_POINT('Ctrl Pts',(-3.84967347300006,2.2,-2.58315192700001));
#318177=CARTESIAN_POINT('Ctrl Pts',(-3.84719442900006,12.2,-2.58300587100001));
#318178=CARTESIAN_POINT('Ctrl Pts',(-3.84719442900006,5.2,-2.58300587100001));
#318179=CARTESIAN_POINT('Ctrl Pts',(-3.84719442900006,2.2,-2.58300587100001));
#318180=CARTESIAN_POINT('Ctrl Pts',(-3.84471908500006,12.2,-2.58285740900002));
#318181=CARTESIAN_POINT('Ctrl Pts',(-3.84471908500006,5.2,-2.58285740900002));
#318182=CARTESIAN_POINT('Ctrl Pts',(-3.84471908500006,2.2,-2.58285740900002));
#318183=CARTESIAN_POINT('Ctrl Pts',(-3.84224744700006,12.2,-2.58270654900001));
#318184=CARTESIAN_POINT('Ctrl Pts',(-3.84224744700006,5.2,-2.58270654900001));
#318185=CARTESIAN_POINT('Ctrl Pts',(-3.84224744700006,2.2,-2.58270654900001));
#318186=CARTESIAN_POINT('Ctrl Pts',(-3.83977951900006,12.2,-2.58255329800001));
#318187=CARTESIAN_POINT('Ctrl Pts',(-3.83977951900006,5.2,-2.58255329800001));
#318188=CARTESIAN_POINT('Ctrl Pts',(-3.83977951900006,2.2,-2.58255329800001));
#318189=CARTESIAN_POINT('Ctrl Pts',(-3.83731530900006,12.2,-2.58239766400001));
#318190=CARTESIAN_POINT('Ctrl Pts',(-3.83731530900006,5.2,-2.58239766400001));
#318191=CARTESIAN_POINT('Ctrl Pts',(-3.83731530900006,2.2,-2.58239766400001));
#318192=CARTESIAN_POINT('Ctrl Pts',(-3.83485482300006,12.2,-2.58223965200001));
#318193=CARTESIAN_POINT('Ctrl Pts',(-3.83485482300006,5.2,-2.58223965200001));
#318194=CARTESIAN_POINT('Ctrl Pts',(-3.83485482300006,2.2,-2.58223965200001));
#318195=CARTESIAN_POINT('Ctrl Pts',(-3.83239806600006,12.2,-2.58207926900001));
#318196=CARTESIAN_POINT('Ctrl Pts',(-3.83239806600006,5.2,-2.58207926900001));
#318197=CARTESIAN_POINT('Ctrl Pts',(-3.83239806600006,2.2,-2.58207926900001));
#318198=CARTESIAN_POINT('Ctrl Pts',(-3.82994504400005,12.2,-2.58191652300002));
#318199=CARTESIAN_POINT('Ctrl Pts',(-3.82994504400005,5.2,-2.58191652300002));
#318200=CARTESIAN_POINT('Ctrl Pts',(-3.82994504400005,2.2,-2.58191652300002));
#318201=CARTESIAN_POINT('Ctrl Pts',(-3.82749576200006,12.2,-2.58175142100002));
#318202=CARTESIAN_POINT('Ctrl Pts',(-3.82749576200006,5.2,-2.58175142100002));
#318203=CARTESIAN_POINT('Ctrl Pts',(-3.82749576200006,2.2,-2.58175142100002));
#318204=CARTESIAN_POINT('Ctrl Pts',(-3.82505022800006,12.2,-2.58158396900001));
#318205=CARTESIAN_POINT('Ctrl Pts',(-3.82505022800006,5.2,-2.58158396900001));
#318206=CARTESIAN_POINT('Ctrl Pts',(-3.82505022800006,2.2,-2.58158396900001));
#318207=CARTESIAN_POINT('Ctrl Pts',(-3.82260844600006,12.2,-2.58141417600001));
#318208=CARTESIAN_POINT('Ctrl Pts',(-3.82260844600006,5.2,-2.58141417600001));
#318209=CARTESIAN_POINT('Ctrl Pts',(-3.82260844600006,2.2,-2.58141417600001));
#318210=CARTESIAN_POINT('Ctrl Pts',(-3.82017042300006,12.2,-2.58124204700001));
#318211=CARTESIAN_POINT('Ctrl Pts',(-3.82017042300006,5.2,-2.58124204700001));
#318212=CARTESIAN_POINT('Ctrl Pts',(-3.82017042300006,2.2,-2.58124204700001));
#318213=CARTESIAN_POINT('Ctrl Pts',(-3.81773616400006,12.2,-2.58106759100002));
#318214=CARTESIAN_POINT('Ctrl Pts',(-3.81773616400006,5.2,-2.58106759100002));
#318215=CARTESIAN_POINT('Ctrl Pts',(-3.81773616400006,2.2,-2.58106759100002));
#318216=CARTESIAN_POINT('Ctrl Pts',(-3.81530567700006,12.2,-2.58089081300001));
#318217=CARTESIAN_POINT('Ctrl Pts',(-3.81530567700006,5.2,-2.58089081300001));
#318218=CARTESIAN_POINT('Ctrl Pts',(-3.81530567700006,2.2,-2.58089081300001));
#318219=CARTESIAN_POINT('Ctrl Pts',(-3.81287896500006,12.2,-2.58071172200002));
#318220=CARTESIAN_POINT('Ctrl Pts',(-3.81287896500006,5.2,-2.58071172200002));
#318221=CARTESIAN_POINT('Ctrl Pts',(-3.81287896500006,2.2,-2.58071172200002));
#318222=CARTESIAN_POINT('Ctrl Pts',(-3.81045603500006,12.2,-2.58053032400001));
#318223=CARTESIAN_POINT('Ctrl Pts',(-3.81045603500006,5.2,-2.58053032400001));
#318224=CARTESIAN_POINT('Ctrl Pts',(-3.81045603500006,2.2,-2.58053032400001));
#318225=CARTESIAN_POINT('Ctrl Pts',(-3.80803689300006,12.2,-2.58034662600001));
#318226=CARTESIAN_POINT('Ctrl Pts',(-3.80803689300006,5.2,-2.58034662600001));
#318227=CARTESIAN_POINT('Ctrl Pts',(-3.80803689300006,2.2,-2.58034662600001));
#318228=CARTESIAN_POINT('Ctrl Pts',(-3.80562154500006,12.2,-2.58016063700001));
#318229=CARTESIAN_POINT('Ctrl Pts',(-3.80562154500006,5.2,-2.58016063700001));
#318230=CARTESIAN_POINT('Ctrl Pts',(-3.80562154500006,2.2,-2.58016063700001));
#318231=CARTESIAN_POINT('Ctrl Pts',(-3.80320999800006,12.2,-2.57997236200001));
#318232=CARTESIAN_POINT('Ctrl Pts',(-3.80320999800006,5.2,-2.57997236200001));
#318233=CARTESIAN_POINT('Ctrl Pts',(-3.80320999800006,2.2,-2.57997236200001));
#318234=CARTESIAN_POINT('Ctrl Pts',(-3.80080225500006,12.2,-2.57978180800002));
#318235=CARTESIAN_POINT('Ctrl Pts',(-3.80080225500006,5.2,-2.57978180800002));
#318236=CARTESIAN_POINT('Ctrl Pts',(-3.80080225500006,2.2,-2.57978180800002));
#318237=CARTESIAN_POINT('Ctrl Pts',(-3.79839832500006,12.2,-2.57958898500001));
#318238=CARTESIAN_POINT('Ctrl Pts',(-3.79839832500006,5.2,-2.57958898500001));
#318239=CARTESIAN_POINT('Ctrl Pts',(-3.79839832500006,2.2,-2.57958898500001));
#318240=CARTESIAN_POINT('Ctrl Pts',(-3.79599821200006,12.2,-2.57939389800002));
#318241=CARTESIAN_POINT('Ctrl Pts',(-3.79599821200006,5.2,-2.57939389800002));
#318242=CARTESIAN_POINT('Ctrl Pts',(-3.79599821200006,2.2,-2.57939389800002));
#318243=CARTESIAN_POINT('Ctrl Pts',(-3.79360192100005,12.2,-2.57919655500002));
#318244=CARTESIAN_POINT('Ctrl Pts',(-3.79360192100005,5.2,-2.57919655500002));
#318245=CARTESIAN_POINT('Ctrl Pts',(-3.79360192100005,2.2,-2.57919655500002));
#318246=CARTESIAN_POINT('Ctrl Pts',(-3.79120946100006,12.2,-2.57899696300001));
#318247=CARTESIAN_POINT('Ctrl Pts',(-3.79120946100006,5.2,-2.57899696300001));
#318248=CARTESIAN_POINT('Ctrl Pts',(-3.79120946100006,2.2,-2.57899696300001));
#318249=CARTESIAN_POINT('Ctrl Pts',(-3.78882083600006,12.2,-2.57879512800002));
#318250=CARTESIAN_POINT('Ctrl Pts',(-3.78882083600006,5.2,-2.57879512800002));
#318251=CARTESIAN_POINT('Ctrl Pts',(-3.78882083600006,2.2,-2.57879512800002));
#318252=CARTESIAN_POINT('Ctrl Pts',(-3.78643605100006,12.2,-2.57859106000002));
#318253=CARTESIAN_POINT('Ctrl Pts',(-3.78643605100006,5.2,-2.57859106000002));
#318254=CARTESIAN_POINT('Ctrl Pts',(-3.78643605100006,2.2,-2.57859106000002));
#318255=CARTESIAN_POINT('Ctrl Pts',(-3.78405511300006,12.2,-2.57838476500002));
#318256=CARTESIAN_POINT('Ctrl Pts',(-3.78405511300006,5.2,-2.57838476500002));
#318257=CARTESIAN_POINT('Ctrl Pts',(-3.78405511300006,2.2,-2.57838476500002));
#318258=CARTESIAN_POINT('Ctrl Pts',(-3.78167802700006,12.2,-2.57817625000001));
#318259=CARTESIAN_POINT('Ctrl Pts',(-3.78167802700006,5.2,-2.57817625000001));
#318260=CARTESIAN_POINT('Ctrl Pts',(-3.78167802700006,2.2,-2.57817625000001));
#318261=CARTESIAN_POINT('Ctrl Pts',(-3.77930480100006,12.2,-2.57796552400002));
#318262=CARTESIAN_POINT('Ctrl Pts',(-3.77930480100006,5.2,-2.57796552400002));
#318263=CARTESIAN_POINT('Ctrl Pts',(-3.77930480100006,2.2,-2.57796552400002));
#318264=CARTESIAN_POINT('Ctrl Pts',(-3.77693543800006,12.2,-2.57775259100002));
#318265=CARTESIAN_POINT('Ctrl Pts',(-3.77693543800006,5.2,-2.57775259100002));
#318266=CARTESIAN_POINT('Ctrl Pts',(-3.77693543800006,2.2,-2.57775259100002));
#318267=CARTESIAN_POINT('Ctrl Pts',(-3.77456994600006,12.2,-2.57753746300001));
#318268=CARTESIAN_POINT('Ctrl Pts',(-3.77456994600006,5.2,-2.57753746300001));
#318269=CARTESIAN_POINT('Ctrl Pts',(-3.77456994600006,2.2,-2.57753746300001));
#318270=CARTESIAN_POINT('Ctrl Pts',(-3.77220833000006,12.2,-2.57732014200001));
#318271=CARTESIAN_POINT('Ctrl Pts',(-3.77220833000006,5.2,-2.57732014200001));
#318272=CARTESIAN_POINT('Ctrl Pts',(-3.77220833000006,2.2,-2.57732014200001));
#318273=CARTESIAN_POINT('Ctrl Pts',(-3.76985059500006,12.2,-2.57710064000001));
#318274=CARTESIAN_POINT('Ctrl Pts',(-3.76985059500006,5.2,-2.57710064000001));
#318275=CARTESIAN_POINT('Ctrl Pts',(-3.76985059500006,2.2,-2.57710064000001));
#318276=CARTESIAN_POINT('Ctrl Pts',(-3.76749674800006,12.2,-2.57687896300002));
#318277=CARTESIAN_POINT('Ctrl Pts',(-3.76749674800006,5.2,-2.57687896300002));
#318278=CARTESIAN_POINT('Ctrl Pts',(-3.76749674800006,2.2,-2.57687896300002));
#318279=CARTESIAN_POINT('Ctrl Pts',(-3.76514679500006,12.2,-2.57665511800001));
#318280=CARTESIAN_POINT('Ctrl Pts',(-3.76514679500006,5.2,-2.57665511800001));
#318281=CARTESIAN_POINT('Ctrl Pts',(-3.76514679500006,2.2,-2.57665511800001));
#318282=CARTESIAN_POINT('Ctrl Pts',(-3.76280074100006,12.2,-2.57642911300001));
#318283=CARTESIAN_POINT('Ctrl Pts',(-3.76280074100006,5.2,-2.57642911300001));
#318284=CARTESIAN_POINT('Ctrl Pts',(-3.76280074100006,2.2,-2.57642911300001));
#318285=CARTESIAN_POINT('Ctrl Pts',(-3.76045859300006,12.2,-2.57620095400001));
#318286=CARTESIAN_POINT('Ctrl Pts',(-3.76045859300006,5.2,-2.57620095400001));
#318287=CARTESIAN_POINT('Ctrl Pts',(-3.76045859300006,2.2,-2.57620095400001));
#318288=CARTESIAN_POINT('Ctrl Pts',(-3.75812035500006,12.2,-2.57597065100001));
#318289=CARTESIAN_POINT('Ctrl Pts',(-3.75812035500006,5.2,-2.57597065100001));
#318290=CARTESIAN_POINT('Ctrl Pts',(-3.75812035500006,2.2,-2.57597065100001));
#318291=CARTESIAN_POINT('Ctrl Pts',(-3.75578603400006,12.2,-2.57573821000001));
#318292=CARTESIAN_POINT('Ctrl Pts',(-3.75578603400006,5.2,-2.57573821000001));
#318293=CARTESIAN_POINT('Ctrl Pts',(-3.75578603400006,2.2,-2.57573821000001));
#318294=CARTESIAN_POINT('Ctrl Pts',(-3.75345563600006,12.2,-2.57550363900001));
#318295=CARTESIAN_POINT('Ctrl Pts',(-3.75345563600006,5.2,-2.57550363900001));
#318296=CARTESIAN_POINT('Ctrl Pts',(-3.75345563600006,2.2,-2.57550363900001));
#318297=CARTESIAN_POINT('Ctrl Pts',(-3.75112916600005,12.2,-2.57526694600001));
#318298=CARTESIAN_POINT('Ctrl Pts',(-3.75112916600005,5.2,-2.57526694600001));
#318299=CARTESIAN_POINT('Ctrl Pts',(-3.75112916600005,2.2,-2.57526694600001));
#318300=CARTESIAN_POINT('Ctrl Pts',(-3.74880663200006,12.2,-2.57502813700001));
#318301=CARTESIAN_POINT('Ctrl Pts',(-3.74880663200006,5.2,-2.57502813700001));
#318302=CARTESIAN_POINT('Ctrl Pts',(-3.74880663200006,2.2,-2.57502813700001));
#318303=CARTESIAN_POINT('Ctrl Pts',(-3.74648803600006,12.2,-2.57478722100001));
#318304=CARTESIAN_POINT('Ctrl Pts',(-3.74648803600006,5.2,-2.57478722100001));
#318305=CARTESIAN_POINT('Ctrl Pts',(-3.74648803600006,2.2,-2.57478722100001));
#318306=CARTESIAN_POINT('Ctrl Pts',(-3.74417338800006,12.2,-2.57454420600002));
#318307=CARTESIAN_POINT('Ctrl Pts',(-3.74417338800006,5.2,-2.57454420600002));
#318308=CARTESIAN_POINT('Ctrl Pts',(-3.74417338800006,2.2,-2.57454420600002));
#318309=CARTESIAN_POINT('Ctrl Pts',(-3.74186269100006,12.2,-2.57429909800001));
#318310=CARTESIAN_POINT('Ctrl Pts',(-3.74186269100006,5.2,-2.57429909800001));
#318311=CARTESIAN_POINT('Ctrl Pts',(-3.74186269100006,2.2,-2.57429909800001));
#318312=CARTESIAN_POINT('Ctrl Pts',(-3.73955595100006,12.2,-2.57405190600001));
#318313=CARTESIAN_POINT('Ctrl Pts',(-3.73955595100006,5.2,-2.57405190600001));
#318314=CARTESIAN_POINT('Ctrl Pts',(-3.73955595100006,2.2,-2.57405190600001));
#318315=CARTESIAN_POINT('Ctrl Pts',(-3.73725317500006,12.2,-2.57380263800002));
#318316=CARTESIAN_POINT('Ctrl Pts',(-3.73725317500006,5.2,-2.57380263800002));
#318317=CARTESIAN_POINT('Ctrl Pts',(-3.73725317500006,2.2,-2.57380263800002));
#318318=CARTESIAN_POINT('Ctrl Pts',(-3.73495436900006,12.2,-2.57355130100001));
#318319=CARTESIAN_POINT('Ctrl Pts',(-3.73495436900006,5.2,-2.57355130100001));
#318320=CARTESIAN_POINT('Ctrl Pts',(-3.73495436900006,2.2,-2.57355130100001));
#318321=CARTESIAN_POINT('Ctrl Pts',(-3.73265953700006,12.2,-2.57329790300002));
#318322=CARTESIAN_POINT('Ctrl Pts',(-3.73265953700006,5.2,-2.57329790300002));
#318323=CARTESIAN_POINT('Ctrl Pts',(-3.73265953700006,2.2,-2.57329790300002));
#318324=CARTESIAN_POINT('Ctrl Pts',(-3.73036868600006,12.2,-2.57304245100002));
#318325=CARTESIAN_POINT('Ctrl Pts',(-3.73036868600006,5.2,-2.57304245100002));
#318326=CARTESIAN_POINT('Ctrl Pts',(-3.73036868600006,2.2,-2.57304245100002));
#318327=CARTESIAN_POINT('Ctrl Pts',(-3.72808182200006,12.2,-2.57278495300001));
#318328=CARTESIAN_POINT('Ctrl Pts',(-3.72808182200006,5.2,-2.57278495300001));
#318329=CARTESIAN_POINT('Ctrl Pts',(-3.72808182200006,2.2,-2.57278495300001));
#318330=CARTESIAN_POINT('Ctrl Pts',(-3.72579894900006,12.2,-2.57252541700002));
#318331=CARTESIAN_POINT('Ctrl Pts',(-3.72579894900006,5.2,-2.57252541700002));
#318332=CARTESIAN_POINT('Ctrl Pts',(-3.72579894900006,2.2,-2.57252541700002));
#318333=CARTESIAN_POINT('Ctrl Pts',(-3.72352007600006,12.2,-2.57226385100001));
#318334=CARTESIAN_POINT('Ctrl Pts',(-3.72352007600006,5.2,-2.57226385100001));
#318335=CARTESIAN_POINT('Ctrl Pts',(-3.72352007600006,2.2,-2.57226385100001));
#318336=CARTESIAN_POINT('Ctrl Pts',(-3.72124520700006,12.2,-2.57200026400001));
#318337=CARTESIAN_POINT('Ctrl Pts',(-3.72124520700006,5.2,-2.57200026400001));
#318338=CARTESIAN_POINT('Ctrl Pts',(-3.72124520700006,2.2,-2.57200026400001));
#318339=CARTESIAN_POINT('Ctrl Pts',(-3.71897434700006,12.2,-2.57173466100001));
#318340=CARTESIAN_POINT('Ctrl Pts',(-3.71897434700006,5.2,-2.57173466100001));
#318341=CARTESIAN_POINT('Ctrl Pts',(-3.71897434700006,2.2,-2.57173466100001));
#318342=CARTESIAN_POINT('Ctrl Pts',(-3.71670750300006,12.2,-2.57146705200002));
#318343=CARTESIAN_POINT('Ctrl Pts',(-3.71670750300006,5.2,-2.57146705200002));
#318344=CARTESIAN_POINT('Ctrl Pts',(-3.71670750300006,2.2,-2.57146705200002));
#318345=CARTESIAN_POINT('Ctrl Pts',(-3.71444468100006,12.2,-2.57119744400002));
#318346=CARTESIAN_POINT('Ctrl Pts',(-3.71444468100006,5.2,-2.57119744400002));
#318347=CARTESIAN_POINT('Ctrl Pts',(-3.71444468100006,2.2,-2.57119744400002));
#318348=CARTESIAN_POINT('Ctrl Pts',(-3.71218588500006,12.2,-2.57092584600001));
#318349=CARTESIAN_POINT('Ctrl Pts',(-3.71218588500006,5.2,-2.57092584600001));
#318350=CARTESIAN_POINT('Ctrl Pts',(-3.71218588500006,2.2,-2.57092584600001));
#318351=CARTESIAN_POINT('Ctrl Pts',(-3.70993112200006,12.2,-2.57065226500002));
#318352=CARTESIAN_POINT('Ctrl Pts',(-3.70993112200006,5.2,-2.57065226500002));
#318353=CARTESIAN_POINT('Ctrl Pts',(-3.70993112200006,2.2,-2.57065226500002));
#318354=CARTESIAN_POINT('Ctrl Pts',(-3.70768039800006,12.2,-2.57037670700001));
#318355=CARTESIAN_POINT('Ctrl Pts',(-3.70768039800006,5.2,-2.57037670700001));
#318356=CARTESIAN_POINT('Ctrl Pts',(-3.70768039800006,2.2,-2.57037670700001));
#318357=CARTESIAN_POINT('Ctrl Pts',(-3.70543371900006,12.2,-2.57009918400001));
#318358=CARTESIAN_POINT('Ctrl Pts',(-3.70543371900006,5.2,-2.57009918400001));
#318359=CARTESIAN_POINT('Ctrl Pts',(-3.70543371900006,2.2,-2.57009918400001));
#318360=CARTESIAN_POINT('Ctrl Pts',(-3.70319109000006,12.2,-2.56981970100002));
#318361=CARTESIAN_POINT('Ctrl Pts',(-3.70319109000006,5.2,-2.56981970100002));
#318362=CARTESIAN_POINT('Ctrl Pts',(-3.70319109000006,2.2,-2.56981970100002));
#318363=CARTESIAN_POINT('Ctrl Pts',(-3.70095251600006,12.2,-2.56953826700002));
#318364=CARTESIAN_POINT('Ctrl Pts',(-3.70095251600006,5.2,-2.56953826700002));
#318365=CARTESIAN_POINT('Ctrl Pts',(-3.70095251600006,2.2,-2.56953826700002));
#318366=CARTESIAN_POINT('Ctrl Pts',(-3.69871800500006,12.2,-2.56925489100002));
#318367=CARTESIAN_POINT('Ctrl Pts',(-3.69871800500006,5.2,-2.56925489100002));
#318368=CARTESIAN_POINT('Ctrl Pts',(-3.69871800500006,2.2,-2.56925489100002));
#318369=CARTESIAN_POINT('Ctrl Pts',(-3.69648756100006,12.2,-2.56896958000001));
#318370=CARTESIAN_POINT('Ctrl Pts',(-3.69648756100006,5.2,-2.56896958000001));
#318371=CARTESIAN_POINT('Ctrl Pts',(-3.69648756100006,2.2,-2.56896958000001));
#318372=CARTESIAN_POINT('Ctrl Pts',(-3.69426119100006,12.2,-2.56868234100001));
#318373=CARTESIAN_POINT('Ctrl Pts',(-3.69426119100006,5.2,-2.56868234100001));
#318374=CARTESIAN_POINT('Ctrl Pts',(-3.69426119100006,2.2,-2.56868234100001));
#318375=CARTESIAN_POINT('Ctrl Pts',(-3.69203889900006,12.2,-2.56839318400001));
#318376=CARTESIAN_POINT('Ctrl Pts',(-3.69203889900006,5.2,-2.56839318400001));
#318377=CARTESIAN_POINT('Ctrl Pts',(-3.69203889900006,2.2,-2.56839318400001));
#318378=CARTESIAN_POINT('Ctrl Pts',(-3.68982069300006,12.2,-2.56810211500001));
#318379=CARTESIAN_POINT('Ctrl Pts',(-3.68982069300006,5.2,-2.56810211500001));
#318380=CARTESIAN_POINT('Ctrl Pts',(-3.68982069300006,2.2,-2.56810211500001));
#318381=CARTESIAN_POINT('Ctrl Pts',(-3.68760657700006,12.2,-2.56780914400002));
#318382=CARTESIAN_POINT('Ctrl Pts',(-3.68760657700006,5.2,-2.56780914400002));
#318383=CARTESIAN_POINT('Ctrl Pts',(-3.68760657700006,2.2,-2.56780914400002));
#318384=CARTESIAN_POINT('Ctrl Pts',(-3.68539655700006,12.2,-2.56751427900001));
#318385=CARTESIAN_POINT('Ctrl Pts',(-3.68539655700006,5.2,-2.56751427900001));
#318386=CARTESIAN_POINT('Ctrl Pts',(-3.68539655700006,2.2,-2.56751427900001));
#318387=CARTESIAN_POINT('Ctrl Pts',(-3.68319064000006,12.2,-2.56721752600002));
#318388=CARTESIAN_POINT('Ctrl Pts',(-3.68319064000006,5.2,-2.56721752600002));
#318389=CARTESIAN_POINT('Ctrl Pts',(-3.68319064000006,2.2,-2.56721752600002));
#318390=CARTESIAN_POINT('Ctrl Pts',(-3.68098883000005,12.2,-2.56691889600001));
#318391=CARTESIAN_POINT('Ctrl Pts',(-3.68098883000005,5.2,-2.56691889600001));
#318392=CARTESIAN_POINT('Ctrl Pts',(-3.68098883000005,2.2,-2.56691889600001));
#318393=CARTESIAN_POINT('Ctrl Pts',(-3.67879113400006,12.2,-2.56661839500001));
#318394=CARTESIAN_POINT('Ctrl Pts',(-3.67879113400006,5.2,-2.56661839500001));
#318395=CARTESIAN_POINT('Ctrl Pts',(-3.67879113400006,2.2,-2.56661839500001));
#318396=CARTESIAN_POINT('Ctrl Pts',(-3.67659755700006,12.2,-2.56631603300002));
#318397=CARTESIAN_POINT('Ctrl Pts',(-3.67659755700006,5.2,-2.56631603300002));
#318398=CARTESIAN_POINT('Ctrl Pts',(-3.67659755700006,2.2,-2.56631603300002));
#318399=CARTESIAN_POINT('Ctrl Pts',(-3.67440810500006,12.2,-2.56601181700002));
#318400=CARTESIAN_POINT('Ctrl Pts',(-3.67440810500006,5.2,-2.56601181700002));
#318401=CARTESIAN_POINT('Ctrl Pts',(-3.67440810500006,2.2,-2.56601181700002));
#318402=CARTESIAN_POINT('Ctrl Pts',(-3.67222278300006,12.2,-2.56570575600001));
#318403=CARTESIAN_POINT('Ctrl Pts',(-3.67222278300006,5.2,-2.56570575600001));
#318404=CARTESIAN_POINT('Ctrl Pts',(-3.67222278300006,2.2,-2.56570575600001));
#318405=CARTESIAN_POINT('Ctrl Pts',(-3.67004159800006,12.2,-2.56539785700001));
#318406=CARTESIAN_POINT('Ctrl Pts',(-3.67004159800006,5.2,-2.56539785700001));
#318407=CARTESIAN_POINT('Ctrl Pts',(-3.67004159800006,2.2,-2.56539785700001));
#318408=CARTESIAN_POINT('Ctrl Pts',(-3.66786455500006,12.2,-2.56508813000002));
#318409=CARTESIAN_POINT('Ctrl Pts',(-3.66786455500006,5.2,-2.56508813000002));
#318410=CARTESIAN_POINT('Ctrl Pts',(-3.66786455500006,2.2,-2.56508813000002));
#318411=CARTESIAN_POINT('Ctrl Pts',(-3.66569166000006,12.2,-2.56477658100001));
#318412=CARTESIAN_POINT('Ctrl Pts',(-3.66569166000006,5.2,-2.56477658100001));
#318413=CARTESIAN_POINT('Ctrl Pts',(-3.66569166000006,2.2,-2.56477658100001));
#318414=CARTESIAN_POINT('Ctrl Pts',(-3.66352291900006,12.2,-2.56446322200001));
#318415=CARTESIAN_POINT('Ctrl Pts',(-3.66352291900006,5.2,-2.56446322200001));
#318416=CARTESIAN_POINT('Ctrl Pts',(-3.66352291900006,2.2,-2.56446322200001));
#318417=CARTESIAN_POINT('Ctrl Pts',(-3.66135833700006,12.2,-2.56414805700001));
#318418=CARTESIAN_POINT('Ctrl Pts',(-3.66135833700006,5.2,-2.56414805700001));
#318419=CARTESIAN_POINT('Ctrl Pts',(-3.66135833700006,2.2,-2.56414805700001));
#318420=CARTESIAN_POINT('Ctrl Pts',(-3.65919792000006,12.2,-2.56383109800002));
#318421=CARTESIAN_POINT('Ctrl Pts',(-3.65919792000006,5.2,-2.56383109800002));
#318422=CARTESIAN_POINT('Ctrl Pts',(-3.65919792000006,2.2,-2.56383109800002));
#318423=CARTESIAN_POINT('Ctrl Pts',(-3.65704167500006,12.2,-2.56351235100002));
#318424=CARTESIAN_POINT('Ctrl Pts',(-3.65704167500006,5.2,-2.56351235100002));
#318425=CARTESIAN_POINT('Ctrl Pts',(-3.65704167500006,2.2,-2.56351235100002));
#318426=CARTESIAN_POINT('Ctrl Pts',(-3.65488960400006,12.2,-2.56319182500001));
#318427=CARTESIAN_POINT('Ctrl Pts',(-3.65488960400006,5.2,-2.56319182500001));
#318428=CARTESIAN_POINT('Ctrl Pts',(-3.65488960400006,2.2,-2.56319182500001));
#318429=CARTESIAN_POINT('Ctrl Pts',(-3.65274171600006,12.2,-2.56286952900001));
#318430=CARTESIAN_POINT('Ctrl Pts',(-3.65274171600006,5.2,-2.56286952900001));
#318431=CARTESIAN_POINT('Ctrl Pts',(-3.65274171600006,2.2,-2.56286952900001));
#318432=CARTESIAN_POINT('Ctrl Pts',(-3.65059801700006,12.2,-2.56254547100002));
#318433=CARTESIAN_POINT('Ctrl Pts',(-3.65059801700006,5.2,-2.56254547100002));
#318434=CARTESIAN_POINT('Ctrl Pts',(-3.65059801700006,2.2,-2.56254547100002));
#318435=CARTESIAN_POINT('Ctrl Pts',(-3.64845851100006,12.2,-2.56221966000002));
#318436=CARTESIAN_POINT('Ctrl Pts',(-3.64845851100006,5.2,-2.56221966000002));
#318437=CARTESIAN_POINT('Ctrl Pts',(-3.64845851100006,2.2,-2.56221966000002));
#318438=CARTESIAN_POINT('Ctrl Pts',(-3.64632320400006,12.2,-2.56189210400001));
#318439=CARTESIAN_POINT('Ctrl Pts',(-3.64632320400006,5.2,-2.56189210400001));
#318440=CARTESIAN_POINT('Ctrl Pts',(-3.64632320400006,2.2,-2.56189210400001));
#318441=CARTESIAN_POINT('Ctrl Pts',(-3.64419210100006,12.2,-2.56156281100001));
#318442=CARTESIAN_POINT('Ctrl Pts',(-3.64419210100006,5.2,-2.56156281100001));
#318443=CARTESIAN_POINT('Ctrl Pts',(-3.64419210100006,2.2,-2.56156281100001));
#318444=CARTESIAN_POINT('Ctrl Pts',(-3.64206521000006,12.2,-2.56123179000001));
#318445=CARTESIAN_POINT('Ctrl Pts',(-3.64206521000006,5.2,-2.56123179000001));
#318446=CARTESIAN_POINT('Ctrl Pts',(-3.64206521000006,2.2,-2.56123179000001));
#318447=CARTESIAN_POINT('Ctrl Pts',(-3.63994253400006,12.2,-2.56089905100001));
#318448=CARTESIAN_POINT('Ctrl Pts',(-3.63994253400006,5.2,-2.56089905100001));
#318449=CARTESIAN_POINT('Ctrl Pts',(-3.63994253400006,2.2,-2.56089905100001));
#318450=CARTESIAN_POINT('Ctrl Pts',(-3.63782408100006,12.2,-2.56056460000002));
#318451=CARTESIAN_POINT('Ctrl Pts',(-3.63782408100006,5.2,-2.56056460000002));
#318452=CARTESIAN_POINT('Ctrl Pts',(-3.63782408100006,2.2,-2.56056460000002));
#318453=CARTESIAN_POINT('Ctrl Pts',(-3.63570985500006,12.2,-2.56022844700002));
#318454=CARTESIAN_POINT('Ctrl Pts',(-3.63570985500006,5.2,-2.56022844700002));
#318455=CARTESIAN_POINT('Ctrl Pts',(-3.63570985500006,2.2,-2.56022844700002));
#318456=CARTESIAN_POINT('Ctrl Pts',(-3.63359986300006,12.2,-2.55989060100001));
#318457=CARTESIAN_POINT('Ctrl Pts',(-3.63359986300006,5.2,-2.55989060100001));
#318458=CARTESIAN_POINT('Ctrl Pts',(-3.63359986300006,2.2,-2.55989060100001));
#318459=CARTESIAN_POINT('Ctrl Pts',(-3.63149410900006,12.2,-2.55955106900001));
#318460=CARTESIAN_POINT('Ctrl Pts',(-3.63149410900006,5.2,-2.55955106900001));
#318461=CARTESIAN_POINT('Ctrl Pts',(-3.63149410900006,2.2,-2.55955106900001));
#318462=CARTESIAN_POINT('Ctrl Pts',(-3.62939259900006,12.2,-2.55920986100001));
#318463=CARTESIAN_POINT('Ctrl Pts',(-3.62939259900006,5.2,-2.55920986100001));
#318464=CARTESIAN_POINT('Ctrl Pts',(-3.62939259900006,2.2,-2.55920986100001));
#318465=CARTESIAN_POINT('Ctrl Pts',(-3.62729534200006,12.2,-2.55886698600001));
#318466=CARTESIAN_POINT('Ctrl Pts',(-3.62729534200006,5.2,-2.55886698600001));
#318467=CARTESIAN_POINT('Ctrl Pts',(-3.62729534200006,2.2,-2.55886698600001));
#318468=CARTESIAN_POINT('Ctrl Pts',(-3.62520233900006,12.2,-2.55852245200002));
#318469=CARTESIAN_POINT('Ctrl Pts',(-3.62520233900006,5.2,-2.55852245200002));
#318470=CARTESIAN_POINT('Ctrl Pts',(-3.62520233900006,2.2,-2.55852245200002));
#318471=CARTESIAN_POINT('Ctrl Pts',(-3.62311359700006,12.2,-2.55817626700001));
#318472=CARTESIAN_POINT('Ctrl Pts',(-3.62311359700006,5.2,-2.55817626700001));
#318473=CARTESIAN_POINT('Ctrl Pts',(-3.62311359700006,2.2,-2.55817626700001));
#318474=CARTESIAN_POINT('Ctrl Pts',(-3.62102912300006,12.2,-2.55782844000001));
#318475=CARTESIAN_POINT('Ctrl Pts',(-3.62102912300006,5.2,-2.55782844000001));
#318476=CARTESIAN_POINT('Ctrl Pts',(-3.62102912300006,2.2,-2.55782844000001));
#318477=CARTESIAN_POINT('Ctrl Pts',(-3.61894892200006,12.2,-2.55747898100001));
#318478=CARTESIAN_POINT('Ctrl Pts',(-3.61894892200006,5.2,-2.55747898100001));
#318479=CARTESIAN_POINT('Ctrl Pts',(-3.61894892200006,2.2,-2.55747898100001));
#318480=CARTESIAN_POINT('Ctrl Pts',(-3.61687299900006,12.2,-2.55712789800001));
#318481=CARTESIAN_POINT('Ctrl Pts',(-3.61687299900006,5.2,-2.55712789800001));
#318482=CARTESIAN_POINT('Ctrl Pts',(-3.61687299900006,2.2,-2.55712789800001));
#318483=CARTESIAN_POINT('Ctrl Pts',(-3.61480136100006,12.2,-2.55677520000001));
#318484=CARTESIAN_POINT('Ctrl Pts',(-3.61480136100006,5.2,-2.55677520000001));
#318485=CARTESIAN_POINT('Ctrl Pts',(-3.61480136100006,2.2,-2.55677520000001));
#318486=CARTESIAN_POINT('Ctrl Pts',(-3.61273401200005,12.2,-2.55642089500002));
#318487=CARTESIAN_POINT('Ctrl Pts',(-3.61273401200005,5.2,-2.55642089500002));
#318488=CARTESIAN_POINT('Ctrl Pts',(-3.61273401200005,2.2,-2.55642089500002));
#318489=CARTESIAN_POINT('Ctrl Pts',(-3.61067095900006,12.2,-2.55606499200002));
#318490=CARTESIAN_POINT('Ctrl Pts',(-3.61067095900006,5.2,-2.55606499200002));
#318491=CARTESIAN_POINT('Ctrl Pts',(-3.61067095900006,2.2,-2.55606499200002));
#318492=CARTESIAN_POINT('Ctrl Pts',(-3.60861220700006,12.2,-2.55570750100001));
#318493=CARTESIAN_POINT('Ctrl Pts',(-3.60861220700006,5.2,-2.55570750100001));
#318494=CARTESIAN_POINT('Ctrl Pts',(-3.60861220700006,2.2,-2.55570750100001));
#318495=CARTESIAN_POINT('Ctrl Pts',(-3.60655776100006,12.2,-2.55534843100001));
#318496=CARTESIAN_POINT('Ctrl Pts',(-3.60655776100006,5.2,-2.55534843100001));
#318497=CARTESIAN_POINT('Ctrl Pts',(-3.60655776100006,2.2,-2.55534843100001));
#318498=CARTESIAN_POINT('Ctrl Pts',(-3.60450762800006,12.2,-2.55498778800002));
#318499=CARTESIAN_POINT('Ctrl Pts',(-3.60450762800006,5.2,-2.55498778800002));
#318500=CARTESIAN_POINT('Ctrl Pts',(-3.60450762800006,2.2,-2.55498778800002));
#318501=CARTESIAN_POINT('Ctrl Pts',(-3.60246181300006,12.2,-2.55462558500001));
#318502=CARTESIAN_POINT('Ctrl Pts',(-3.60246181300006,5.2,-2.55462558500001));
#318503=CARTESIAN_POINT('Ctrl Pts',(-3.60246181300006,2.2,-2.55462558500001));
#318504=CARTESIAN_POINT('Ctrl Pts',(-3.60042032100006,12.2,-2.55426182800001));
#318505=CARTESIAN_POINT('Ctrl Pts',(-3.60042032100006,5.2,-2.55426182800001));
#318506=CARTESIAN_POINT('Ctrl Pts',(-3.60042032100006,2.2,-2.55426182800001));
#318507=CARTESIAN_POINT('Ctrl Pts',(-3.59838315900006,12.2,-2.55389652700002));
#318508=CARTESIAN_POINT('Ctrl Pts',(-3.59838315900006,5.2,-2.55389652700002));
#318509=CARTESIAN_POINT('Ctrl Pts',(-3.59838315900006,2.2,-2.55389652700002));
#318510=CARTESIAN_POINT('Ctrl Pts',(-3.59635033100006,12.2,-2.55352969000001));
#318511=CARTESIAN_POINT('Ctrl Pts',(-3.59635033100006,5.2,-2.55352969000001));
#318512=CARTESIAN_POINT('Ctrl Pts',(-3.59635033100006,2.2,-2.55352969000001));
#318513=CARTESIAN_POINT('Ctrl Pts',(-3.59432184300006,12.2,-2.55316132800001));
#318514=CARTESIAN_POINT('Ctrl Pts',(-3.59432184300006,5.2,-2.55316132800001));
#318515=CARTESIAN_POINT('Ctrl Pts',(-3.59432184300006,2.2,-2.55316132800001));
#318516=CARTESIAN_POINT('Ctrl Pts',(-3.59229770100006,12.2,-2.55279144900001));
#318517=CARTESIAN_POINT('Ctrl Pts',(-3.59229770100006,5.2,-2.55279144900001));
#318518=CARTESIAN_POINT('Ctrl Pts',(-3.59229770100006,2.2,-2.55279144900001));
#318519=CARTESIAN_POINT('Ctrl Pts',(-3.59027791200006,12.2,-2.55242006200001));
#318520=CARTESIAN_POINT('Ctrl Pts',(-3.59027791200006,5.2,-2.55242006200001));
#318521=CARTESIAN_POINT('Ctrl Pts',(-3.59027791200006,2.2,-2.55242006200001));
#318522=CARTESIAN_POINT('Ctrl Pts',(-3.58826247900006,12.2,-2.55204717600002));
#318523=CARTESIAN_POINT('Ctrl Pts',(-3.58826247900006,5.2,-2.55204717600002));
#318524=CARTESIAN_POINT('Ctrl Pts',(-3.58826247900006,2.2,-2.55204717600002));
#318525=CARTESIAN_POINT('Ctrl Pts',(-3.58625140900006,12.2,-2.55167279900002));
#318526=CARTESIAN_POINT('Ctrl Pts',(-3.58625140900006,5.2,-2.55167279900002));
#318527=CARTESIAN_POINT('Ctrl Pts',(-3.58625140900006,2.2,-2.55167279900002));
#318528=CARTESIAN_POINT('Ctrl Pts',(-3.58424470700006,12.2,-2.55129694200001));
#318529=CARTESIAN_POINT('Ctrl Pts',(-3.58424470700006,5.2,-2.55129694200001));
#318530=CARTESIAN_POINT('Ctrl Pts',(-3.58424470700006,2.2,-2.55129694200001));
#318531=CARTESIAN_POINT('Ctrl Pts',(-3.58224237900005,12.2,-2.55091961300002));
#318532=CARTESIAN_POINT('Ctrl Pts',(-3.58224237900005,5.2,-2.55091961300002));
#318533=CARTESIAN_POINT('Ctrl Pts',(-3.58224237900005,2.2,-2.55091961300002));
#318534=CARTESIAN_POINT('Ctrl Pts',(-3.58024443100006,12.2,-2.55054082300001));
#318535=CARTESIAN_POINT('Ctrl Pts',(-3.58024443100006,5.2,-2.55054082300001));
#318536=CARTESIAN_POINT('Ctrl Pts',(-3.58024443100006,2.2,-2.55054082300001));
#318537=CARTESIAN_POINT('Ctrl Pts',(-3.57825086800006,12.2,-2.55016057800002));
#318538=CARTESIAN_POINT('Ctrl Pts',(-3.57825086800006,5.2,-2.55016057800002));
#318539=CARTESIAN_POINT('Ctrl Pts',(-3.57825086800006,2.2,-2.55016057800002));
#318540=CARTESIAN_POINT('Ctrl Pts',(-3.57626169500006,12.2,-2.54977888900001));
#318541=CARTESIAN_POINT('Ctrl Pts',(-3.57626169500006,5.2,-2.54977888900001));
#318542=CARTESIAN_POINT('Ctrl Pts',(-3.57626169500006,2.2,-2.54977888900001));
#318543=CARTESIAN_POINT('Ctrl Pts',(-3.57427691800006,12.2,-2.54939576600002));
#318544=CARTESIAN_POINT('Ctrl Pts',(-3.57427691800006,5.2,-2.54939576600002));
#318545=CARTESIAN_POINT('Ctrl Pts',(-3.57427691800006,2.2,-2.54939576600002));
#318546=CARTESIAN_POINT('Ctrl Pts',(-3.57229654300006,12.2,-2.54901121700001));
#318547=CARTESIAN_POINT('Ctrl Pts',(-3.57229654300006,5.2,-2.54901121700001));
#318548=CARTESIAN_POINT('Ctrl Pts',(-3.57229654300006,2.2,-2.54901121700001));
#318549=CARTESIAN_POINT('Ctrl Pts',(-3.57032057600006,12.2,-2.54862525200001));
#318550=CARTESIAN_POINT('Ctrl Pts',(-3.57032057600006,5.2,-2.54862525200001));
#318551=CARTESIAN_POINT('Ctrl Pts',(-3.57032057600006,2.2,-2.54862525200001));
#318552=CARTESIAN_POINT('Ctrl Pts',(-3.56834902100006,12.2,-2.54823787900001));
#318553=CARTESIAN_POINT('Ctrl Pts',(-3.56834902100006,5.2,-2.54823787900001));
#318554=CARTESIAN_POINT('Ctrl Pts',(-3.56834902100006,2.2,-2.54823787900001));
#318555=CARTESIAN_POINT('Ctrl Pts',(-3.56638188500006,12.2,-2.54784911000002));
#318556=CARTESIAN_POINT('Ctrl Pts',(-3.56638188500006,5.2,-2.54784911000002));
#318557=CARTESIAN_POINT('Ctrl Pts',(-3.56638188500006,2.2,-2.54784911000002));
#318558=CARTESIAN_POINT('Ctrl Pts',(-3.56441917200006,12.2,-2.54745895100001));
#318559=CARTESIAN_POINT('Ctrl Pts',(-3.56441917200006,5.2,-2.54745895100001));
#318560=CARTESIAN_POINT('Ctrl Pts',(-3.56441917200006,2.2,-2.54745895100001));
#318561=CARTESIAN_POINT('Ctrl Pts',(-3.56246089000006,12.2,-2.54706741300001));
#318562=CARTESIAN_POINT('Ctrl Pts',(-3.56246089000006,5.2,-2.54706741300001));
#318563=CARTESIAN_POINT('Ctrl Pts',(-3.56246089000006,2.2,-2.54706741300001));
#318564=CARTESIAN_POINT('Ctrl Pts',(-3.56050704200006,12.2,-2.54667450600001));
#318565=CARTESIAN_POINT('Ctrl Pts',(-3.56050704200006,5.2,-2.54667450600001));
#318566=CARTESIAN_POINT('Ctrl Pts',(-3.56050704200006,2.2,-2.54667450600001));
#318567=CARTESIAN_POINT('Ctrl Pts',(-3.55855763500006,12.2,-2.54628023900001));
#318568=CARTESIAN_POINT('Ctrl Pts',(-3.55855763500006,5.2,-2.54628023900001));
#318569=CARTESIAN_POINT('Ctrl Pts',(-3.55855763500006,2.2,-2.54628023900001));
#318570=CARTESIAN_POINT('Ctrl Pts',(-3.55661267300006,12.2,-2.54588462100001));
#318571=CARTESIAN_POINT('Ctrl Pts',(-3.55661267300006,5.2,-2.54588462100001));
#318572=CARTESIAN_POINT('Ctrl Pts',(-3.55661267300006,2.2,-2.54588462100001));
#318573=CARTESIAN_POINT('Ctrl Pts',(-3.55467216400006,12.2,-2.54548766100001));
#318574=CARTESIAN_POINT('Ctrl Pts',(-3.55467216400006,5.2,-2.54548766100001));
#318575=CARTESIAN_POINT('Ctrl Pts',(-3.55467216400006,2.2,-2.54548766100001));
#318576=CARTESIAN_POINT('Ctrl Pts',(-3.55273611200006,12.2,-2.54508937000002));
#318577=CARTESIAN_POINT('Ctrl Pts',(-3.55273611200006,5.2,-2.54508937000002));
#318578=CARTESIAN_POINT('Ctrl Pts',(-3.55273611200006,2.2,-2.54508937000002));
#318579=CARTESIAN_POINT('Ctrl Pts',(-3.55080452200006,12.2,-2.54468975600001));
#318580=CARTESIAN_POINT('Ctrl Pts',(-3.55080452200006,5.2,-2.54468975600001));
#318581=CARTESIAN_POINT('Ctrl Pts',(-3.55080452200006,2.2,-2.54468975600001));
#318582=CARTESIAN_POINT('Ctrl Pts',(-3.54887740000006,12.2,-2.54428882900001));
#318583=CARTESIAN_POINT('Ctrl Pts',(-3.54887740000006,5.2,-2.54428882900001));
#318584=CARTESIAN_POINT('Ctrl Pts',(-3.54887740000006,2.2,-2.54428882900001));
#318585=CARTESIAN_POINT('Ctrl Pts',(-3.54695475300006,12.2,-2.54388659900001));
#318586=CARTESIAN_POINT('Ctrl Pts',(-3.54695475300006,5.2,-2.54388659900001));
#318587=CARTESIAN_POINT('Ctrl Pts',(-3.54695475300006,2.2,-2.54388659900001));
#318588=CARTESIAN_POINT('Ctrl Pts',(-3.54503658400006,12.2,-2.54348307500001));
#318589=CARTESIAN_POINT('Ctrl Pts',(-3.54503658400006,5.2,-2.54348307500001));
#318590=CARTESIAN_POINT('Ctrl Pts',(-3.54503658400006,2.2,-2.54348307500001));
#318591=CARTESIAN_POINT('Ctrl Pts',(-3.54312290000006,12.2,-2.54307826700002));
#318592=CARTESIAN_POINT('Ctrl Pts',(-3.54312290000006,5.2,-2.54307826700002));
#318593=CARTESIAN_POINT('Ctrl Pts',(-3.54312290000006,2.2,-2.54307826700002));
#318594=CARTESIAN_POINT('Ctrl Pts',(-3.54121370600006,12.2,-2.54267218400001));
#318595=CARTESIAN_POINT('Ctrl Pts',(-3.54121370600006,5.2,-2.54267218400001));
#318596=CARTESIAN_POINT('Ctrl Pts',(-3.54121370600006,2.2,-2.54267218400001));
#318597=CARTESIAN_POINT('Ctrl Pts',(-3.53930900900005,12.2,-2.54226483700001));
#318598=CARTESIAN_POINT('Ctrl Pts',(-3.53930900900005,5.2,-2.54226483700001));
#318599=CARTESIAN_POINT('Ctrl Pts',(-3.53930900900005,2.2,-2.54226483700001));
#318600=CARTESIAN_POINT('Ctrl Pts',(-3.53740881100006,12.2,-2.54185623400002));
#318601=CARTESIAN_POINT('Ctrl Pts',(-3.53740881100006,5.2,-2.54185623400002));
#318602=CARTESIAN_POINT('Ctrl Pts',(-3.53740881100006,2.2,-2.54185623400002));
#318603=CARTESIAN_POINT('Ctrl Pts',(-3.53551312200006,12.2,-2.54144638500001));
#318604=CARTESIAN_POINT('Ctrl Pts',(-3.53551312200006,5.2,-2.54144638500001));
#318605=CARTESIAN_POINT('Ctrl Pts',(-3.53551312200006,2.2,-2.54144638500001));
#318606=CARTESIAN_POINT('Ctrl Pts',(-3.53362194400006,12.2,-2.54103530100001));
#318607=CARTESIAN_POINT('Ctrl Pts',(-3.53362194400006,5.2,-2.54103530100001));
#318608=CARTESIAN_POINT('Ctrl Pts',(-3.53362194400006,2.2,-2.54103530100001));
#318609=CARTESIAN_POINT('Ctrl Pts',(-3.53173528300006,12.2,-2.54062299000001));
#318610=CARTESIAN_POINT('Ctrl Pts',(-3.53173528300006,5.2,-2.54062299000001));
#318611=CARTESIAN_POINT('Ctrl Pts',(-3.53173528300006,2.2,-2.54062299000001));
#318612=CARTESIAN_POINT('Ctrl Pts',(-3.52985314600006,12.2,-2.54020946300002));
#318613=CARTESIAN_POINT('Ctrl Pts',(-3.52985314600006,5.2,-2.54020946300002));
#318614=CARTESIAN_POINT('Ctrl Pts',(-3.52985314600006,2.2,-2.54020946300002));
#318615=CARTESIAN_POINT('Ctrl Pts',(-3.52797553700006,12.2,-2.53979472900001));
#318616=CARTESIAN_POINT('Ctrl Pts',(-3.52797553700006,5.2,-2.53979472900001));
#318617=CARTESIAN_POINT('Ctrl Pts',(-3.52797553700006,2.2,-2.53979472900001));
#318618=CARTESIAN_POINT('Ctrl Pts',(-3.52610246200006,12.2,-2.53937879900001));
#318619=CARTESIAN_POINT('Ctrl Pts',(-3.52610246200006,5.2,-2.53937879900001));
#318620=CARTESIAN_POINT('Ctrl Pts',(-3.52610246200006,2.2,-2.53937879900001));
#318621=CARTESIAN_POINT('Ctrl Pts',(-3.52423392700006,12.2,-2.53896168100002));
#318622=CARTESIAN_POINT('Ctrl Pts',(-3.52423392700006,5.2,-2.53896168100002));
#318623=CARTESIAN_POINT('Ctrl Pts',(-3.52423392700006,2.2,-2.53896168100002));
#318624=CARTESIAN_POINT('Ctrl Pts',(-3.52236993700005,12.2,-2.53854338700001));
#318625=CARTESIAN_POINT('Ctrl Pts',(-3.52236993700005,5.2,-2.53854338700001));
#318626=CARTESIAN_POINT('Ctrl Pts',(-3.52236993700005,2.2,-2.53854338700001));
#318627=CARTESIAN_POINT('Ctrl Pts',(-3.52051049600006,12.2,-2.53812392400001));
#318628=CARTESIAN_POINT('Ctrl Pts',(-3.52051049600006,5.2,-2.53812392400001));
#318629=CARTESIAN_POINT('Ctrl Pts',(-3.52051049600006,2.2,-2.53812392400001));
#318630=CARTESIAN_POINT('Ctrl Pts',(-3.51865561200006,12.2,-2.53770330500001));
#318631=CARTESIAN_POINT('Ctrl Pts',(-3.51865561200006,5.2,-2.53770330500001));
#318632=CARTESIAN_POINT('Ctrl Pts',(-3.51865561200006,2.2,-2.53770330500001));
#318633=CARTESIAN_POINT('Ctrl Pts',(-3.51680529000006,12.2,-2.53728153800001));
#318634=CARTESIAN_POINT('Ctrl Pts',(-3.51680529000006,5.2,-2.53728153800001));
#318635=CARTESIAN_POINT('Ctrl Pts',(-3.51680529000006,2.2,-2.53728153800001));
#318636=CARTESIAN_POINT('Ctrl Pts',(-3.51495953300006,12.2,-2.53685863300001));
#318637=CARTESIAN_POINT('Ctrl Pts',(-3.51495953300006,5.2,-2.53685863300001));
#318638=CARTESIAN_POINT('Ctrl Pts',(-3.51495953300006,2.2,-2.53685863300001));
#318639=CARTESIAN_POINT('Ctrl Pts',(-3.51311835000006,12.2,-2.53643460000001));
#318640=CARTESIAN_POINT('Ctrl Pts',(-3.51311835000006,5.2,-2.53643460000001));
#318641=CARTESIAN_POINT('Ctrl Pts',(-3.51311835000006,2.2,-2.53643460000001));
#318642=CARTESIAN_POINT('Ctrl Pts',(-3.51128174300006,12.2,-2.53600945100001));
#318643=CARTESIAN_POINT('Ctrl Pts',(-3.51128174300006,5.2,-2.53600945100001));
#318644=CARTESIAN_POINT('Ctrl Pts',(-3.51128174300006,2.2,-2.53600945100001));
#318645=CARTESIAN_POINT('Ctrl Pts',(-3.50944972000006,12.2,-2.53558319400002));
#318646=CARTESIAN_POINT('Ctrl Pts',(-3.50944972000006,5.2,-2.53558319400002));
#318647=CARTESIAN_POINT('Ctrl Pts',(-3.50944972000006,2.2,-2.53558319400002));
#318648=CARTESIAN_POINT('Ctrl Pts',(-3.50762228500006,12.2,-2.53515583900001));
#318649=CARTESIAN_POINT('Ctrl Pts',(-3.50762228500006,5.2,-2.53515583900001));
#318650=CARTESIAN_POINT('Ctrl Pts',(-3.50762228500006,2.2,-2.53515583900001));
#318651=CARTESIAN_POINT('Ctrl Pts',(-3.50579944300006,12.2,-2.53472739600001));
#318652=CARTESIAN_POINT('Ctrl Pts',(-3.50579944300006,5.2,-2.53472739600001));
#318653=CARTESIAN_POINT('Ctrl Pts',(-3.50579944300006,2.2,-2.53472739600001));
#318654=CARTESIAN_POINT('Ctrl Pts',(-3.50398120200006,12.2,-2.53429787500002));
#318655=CARTESIAN_POINT('Ctrl Pts',(-3.50398120200006,5.2,-2.53429787500002));
#318656=CARTESIAN_POINT('Ctrl Pts',(-3.50398120200006,2.2,-2.53429787500002));
#318657=CARTESIAN_POINT('Ctrl Pts',(-3.50216756400005,12.2,-2.53386728800002));
#318658=CARTESIAN_POINT('Ctrl Pts',(-3.50216756400005,5.2,-2.53386728800002));
#318659=CARTESIAN_POINT('Ctrl Pts',(-3.50216756400005,2.2,-2.53386728800002));
#318660=CARTESIAN_POINT('Ctrl Pts',(-3.50035853800006,12.2,-2.53343564400001));
#318661=CARTESIAN_POINT('Ctrl Pts',(-3.50035853800006,5.2,-2.53343564400001));
#318662=CARTESIAN_POINT('Ctrl Pts',(-3.50035853800006,2.2,-2.53343564400001));
#318663=CARTESIAN_POINT('Ctrl Pts',(-3.49855412600005,12.2,-2.53300295300001));
#318664=CARTESIAN_POINT('Ctrl Pts',(-3.49855412600005,5.2,-2.53300295300001));
#318665=CARTESIAN_POINT('Ctrl Pts',(-3.49855412600005,2.2,-2.53300295300001));
#318666=CARTESIAN_POINT('Ctrl Pts',(-3.49675433400006,12.2,-2.53256922500002));
#318667=CARTESIAN_POINT('Ctrl Pts',(-3.49675433400006,5.2,-2.53256922500002));
#318668=CARTESIAN_POINT('Ctrl Pts',(-3.49675433400006,2.2,-2.53256922500002));
#318669=CARTESIAN_POINT('Ctrl Pts',(-3.49495917000006,12.2,-2.53213446900002));
#318670=CARTESIAN_POINT('Ctrl Pts',(-3.49495917000006,5.2,-2.53213446900002));
#318671=CARTESIAN_POINT('Ctrl Pts',(-3.49495917000006,2.2,-2.53213446900002));
#318672=CARTESIAN_POINT('Ctrl Pts',(-3.49316863700006,12.2,-2.53169869800002));
#318673=CARTESIAN_POINT('Ctrl Pts',(-3.49316863700006,5.2,-2.53169869800002));
#318674=CARTESIAN_POINT('Ctrl Pts',(-3.49316863700006,2.2,-2.53169869800002));
#318675=CARTESIAN_POINT('Ctrl Pts',(-3.49138274100006,12.2,-2.53126192100002));
#318676=CARTESIAN_POINT('Ctrl Pts',(-3.49138274100006,5.2,-2.53126192100002));
#318677=CARTESIAN_POINT('Ctrl Pts',(-3.49138274100006,2.2,-2.53126192100002));
#318678=CARTESIAN_POINT('Ctrl Pts',(-3.48960148600006,12.2,-2.53082414800001));
#318679=CARTESIAN_POINT('Ctrl Pts',(-3.48960148600006,5.2,-2.53082414800001));
#318680=CARTESIAN_POINT('Ctrl Pts',(-3.48960148600006,2.2,-2.53082414800001));
#318681=CARTESIAN_POINT('Ctrl Pts',(-3.48782488200006,12.2,-2.53038538900002));
#318682=CARTESIAN_POINT('Ctrl Pts',(-3.48782488200006,5.2,-2.53038538900002));
#318683=CARTESIAN_POINT('Ctrl Pts',(-3.48782488200006,2.2,-2.53038538900002));
#318684=CARTESIAN_POINT('Ctrl Pts',(-3.48605292900006,12.2,-2.52994565500002));
#318685=CARTESIAN_POINT('Ctrl Pts',(-3.48605292900006,5.2,-2.52994565500002));
#318686=CARTESIAN_POINT('Ctrl Pts',(-3.48605292900006,2.2,-2.52994565500002));
#318687=CARTESIAN_POINT('Ctrl Pts',(-3.48428563300006,12.2,-2.52950495600002));
#318688=CARTESIAN_POINT('Ctrl Pts',(-3.48428563300006,5.2,-2.52950495600002));
#318689=CARTESIAN_POINT('Ctrl Pts',(-3.48428563300006,2.2,-2.52950495600002));
#318690=CARTESIAN_POINT('Ctrl Pts',(-3.48252300300006,12.2,-2.52906330300001));
#318691=CARTESIAN_POINT('Ctrl Pts',(-3.48252300300006,5.2,-2.52906330300001));
#318692=CARTESIAN_POINT('Ctrl Pts',(-3.48252300300006,2.2,-2.52906330300001));
#318693=CARTESIAN_POINT('Ctrl Pts',(-3.48076504100006,12.2,-2.52862070600001));
#318694=CARTESIAN_POINT('Ctrl Pts',(-3.48076504100006,5.2,-2.52862070600001));
#318695=CARTESIAN_POINT('Ctrl Pts',(-3.48076504100006,2.2,-2.52862070600001));
#318696=CARTESIAN_POINT('Ctrl Pts',(-3.47901175400006,12.2,-2.52817717500001));
#318697=CARTESIAN_POINT('Ctrl Pts',(-3.47901175400006,5.2,-2.52817717500001));
#318698=CARTESIAN_POINT('Ctrl Pts',(-3.47901175400006,2.2,-2.52817717500001));
#318699=CARTESIAN_POINT('Ctrl Pts',(-3.47726314700005,12.2,-2.52773272000002));
#318700=CARTESIAN_POINT('Ctrl Pts',(-3.47726314700005,5.2,-2.52773272000002));
#318701=CARTESIAN_POINT('Ctrl Pts',(-3.47726314700005,2.2,-2.52773272000002));
#318702=CARTESIAN_POINT('Ctrl Pts',(-3.47551922500006,12.2,-2.52728735400002));
#318703=CARTESIAN_POINT('Ctrl Pts',(-3.47551922500006,5.2,-2.52728735400002));
#318704=CARTESIAN_POINT('Ctrl Pts',(-3.47551922500006,2.2,-2.52728735400002));
#318705=CARTESIAN_POINT('Ctrl Pts',(-3.47377999300006,12.2,-2.52684108500001));
#318706=CARTESIAN_POINT('Ctrl Pts',(-3.47377999300006,5.2,-2.52684108500001));
#318707=CARTESIAN_POINT('Ctrl Pts',(-3.47377999300006,2.2,-2.52684108500001));
#318708=CARTESIAN_POINT('Ctrl Pts',(-3.47204545800006,12.2,-2.52639392400001));
#318709=CARTESIAN_POINT('Ctrl Pts',(-3.47204545800006,5.2,-2.52639392400001));
#318710=CARTESIAN_POINT('Ctrl Pts',(-3.47204545800006,2.2,-2.52639392400001));
#318711=CARTESIAN_POINT('Ctrl Pts',(-3.47031562400006,12.2,-2.52594588300001));
#318712=CARTESIAN_POINT('Ctrl Pts',(-3.47031562400006,5.2,-2.52594588300001));
#318713=CARTESIAN_POINT('Ctrl Pts',(-3.47031562400006,2.2,-2.52594588300001));
#318714=CARTESIAN_POINT('Ctrl Pts',(-3.46859049400006,12.2,-2.52549697100001));
#318715=CARTESIAN_POINT('Ctrl Pts',(-3.46859049400006,5.2,-2.52549697100001));
#318716=CARTESIAN_POINT('Ctrl Pts',(-3.46859049400006,2.2,-2.52549697100001));
#318717=CARTESIAN_POINT('Ctrl Pts',(-3.46687007900006,12.2,-2.52504719900001));
#318718=CARTESIAN_POINT('Ctrl Pts',(-3.46687007900006,5.2,-2.52504719900001));
#318719=CARTESIAN_POINT('Ctrl Pts',(-3.46687007900006,2.2,-2.52504719900001));
#318720=CARTESIAN_POINT('Ctrl Pts',(-3.46515437900006,12.2,-2.52459657800001));
#318721=CARTESIAN_POINT('Ctrl Pts',(-3.46515437900006,5.2,-2.52459657800001));
#318722=CARTESIAN_POINT('Ctrl Pts',(-3.46515437900006,2.2,-2.52459657800001));
#318723=CARTESIAN_POINT('Ctrl Pts',(-3.46344340300006,12.2,-2.52414511800001));
#318724=CARTESIAN_POINT('Ctrl Pts',(-3.46344340300006,5.2,-2.52414511800001));
#318725=CARTESIAN_POINT('Ctrl Pts',(-3.46344340300006,2.2,-2.52414511800001));
#318726=CARTESIAN_POINT('Ctrl Pts',(-3.46173715200006,12.2,-2.52369283100002));
#318727=CARTESIAN_POINT('Ctrl Pts',(-3.46173715200006,5.2,-2.52369283100002));
#318728=CARTESIAN_POINT('Ctrl Pts',(-3.46173715200006,2.2,-2.52369283100002));
#318729=CARTESIAN_POINT('Ctrl Pts',(-3.46003563600005,12.2,-2.52323972700002));
#318730=CARTESIAN_POINT('Ctrl Pts',(-3.46003563600005,5.2,-2.52323972700002));
#318731=CARTESIAN_POINT('Ctrl Pts',(-3.46003563600005,2.2,-2.52323972700002));
#318732=CARTESIAN_POINT('Ctrl Pts',(-3.45833885900006,12.2,-2.52278581600001));
#318733=CARTESIAN_POINT('Ctrl Pts',(-3.45833885900006,5.2,-2.52278581600001));
#318734=CARTESIAN_POINT('Ctrl Pts',(-3.45833885900006,2.2,-2.52278581600001));
#318735=CARTESIAN_POINT('Ctrl Pts',(-3.45664682400006,12.2,-2.52233111000002));
#318736=CARTESIAN_POINT('Ctrl Pts',(-3.45664682400006,5.2,-2.52233111000002));
#318737=CARTESIAN_POINT('Ctrl Pts',(-3.45664682400006,2.2,-2.52233111000002));
#318738=CARTESIAN_POINT('Ctrl Pts',(-3.45495953800006,12.2,-2.52187561800001));
#318739=CARTESIAN_POINT('Ctrl Pts',(-3.45495953800006,5.2,-2.52187561800001));
#318740=CARTESIAN_POINT('Ctrl Pts',(-3.45495953800006,2.2,-2.52187561800001));
#318741=CARTESIAN_POINT('Ctrl Pts',(-3.45327700600006,12.2,-2.52141935300001));
#318742=CARTESIAN_POINT('Ctrl Pts',(-3.45327700600006,5.2,-2.52141935300001));
#318743=CARTESIAN_POINT('Ctrl Pts',(-3.45327700600006,2.2,-2.52141935300001));
#318744=CARTESIAN_POINT('Ctrl Pts',(-3.45159923300006,12.2,-2.52096232500001));
#318745=CARTESIAN_POINT('Ctrl Pts',(-3.45159923300006,5.2,-2.52096232500001));
#318746=CARTESIAN_POINT('Ctrl Pts',(-3.45159923300006,2.2,-2.52096232500001));
#318747=CARTESIAN_POINT('Ctrl Pts',(-3.44992622600006,12.2,-2.52050454400001));
#318748=CARTESIAN_POINT('Ctrl Pts',(-3.44992622600006,5.2,-2.52050454400001));
#318749=CARTESIAN_POINT('Ctrl Pts',(-3.44992622600006,2.2,-2.52050454400001));
#318750=CARTESIAN_POINT('Ctrl Pts',(-3.44825798800006,12.2,-2.52004602200001));
#318751=CARTESIAN_POINT('Ctrl Pts',(-3.44825798800006,5.2,-2.52004602200001));
#318752=CARTESIAN_POINT('Ctrl Pts',(-3.44825798800006,2.2,-2.52004602200001));
#318753=CARTESIAN_POINT('Ctrl Pts',(-3.44659452500006,12.2,-2.51958677000002));
#318754=CARTESIAN_POINT('Ctrl Pts',(-3.44659452500006,5.2,-2.51958677000002));
#318755=CARTESIAN_POINT('Ctrl Pts',(-3.44659452500006,2.2,-2.51958677000002));
#318756=CARTESIAN_POINT('Ctrl Pts',(-3.44493584300006,12.2,-2.51912679800002));
#318757=CARTESIAN_POINT('Ctrl Pts',(-3.44493584300006,5.2,-2.51912679800002));
#318758=CARTESIAN_POINT('Ctrl Pts',(-3.44493584300006,2.2,-2.51912679800002));
#318759=CARTESIAN_POINT('Ctrl Pts',(-3.44328194500005,12.2,-2.51866611900001));
#318760=CARTESIAN_POINT('Ctrl Pts',(-3.44328194500005,5.2,-2.51866611900001));
#318761=CARTESIAN_POINT('Ctrl Pts',(-3.44328194500005,2.2,-2.51866611900001));
#318762=CARTESIAN_POINT('Ctrl Pts',(-3.44163283900006,12.2,-2.51820474000001));
#318763=CARTESIAN_POINT('Ctrl Pts',(-3.44163283900006,5.2,-2.51820474000001));
#318764=CARTESIAN_POINT('Ctrl Pts',(-3.44163283900006,2.2,-2.51820474000001));
#318765=CARTESIAN_POINT('Ctrl Pts',(-3.43998852900006,12.2,-2.51774267700001));
#318766=CARTESIAN_POINT('Ctrl Pts',(-3.43998852900006,5.2,-2.51774267700001));
#318767=CARTESIAN_POINT('Ctrl Pts',(-3.43998852900006,2.2,-2.51774267700001));
#318768=CARTESIAN_POINT('Ctrl Pts',(-3.43834901900005,12.2,-2.51727993800001));
#318769=CARTESIAN_POINT('Ctrl Pts',(-3.43834901900005,5.2,-2.51727993800001));
#318770=CARTESIAN_POINT('Ctrl Pts',(-3.43834901900005,2.2,-2.51727993800001));
#318771=CARTESIAN_POINT('Ctrl Pts',(-3.43671431700006,12.2,-2.51681653400002));
#318772=CARTESIAN_POINT('Ctrl Pts',(-3.43671431700006,5.2,-2.51681653400002));
#318773=CARTESIAN_POINT('Ctrl Pts',(-3.43671431700006,2.2,-2.51681653400002));
#318774=CARTESIAN_POINT('Ctrl Pts',(-3.43508442600006,12.2,-2.51635247700001));
#318775=CARTESIAN_POINT('Ctrl Pts',(-3.43508442600006,5.2,-2.51635247700001));
#318776=CARTESIAN_POINT('Ctrl Pts',(-3.43508442600006,2.2,-2.51635247700001));
#318777=CARTESIAN_POINT('Ctrl Pts',(-3.43345935200006,12.2,-2.51588777800002));
#318778=CARTESIAN_POINT('Ctrl Pts',(-3.43345935200006,5.2,-2.51588777800002));
#318779=CARTESIAN_POINT('Ctrl Pts',(-3.43345935200006,2.2,-2.51588777800002));
#318780=CARTESIAN_POINT('Ctrl Pts',(-3.43183910100006,12.2,-2.51542244900001));
#318781=CARTESIAN_POINT('Ctrl Pts',(-3.43183910100006,5.2,-2.51542244900001));
#318782=CARTESIAN_POINT('Ctrl Pts',(-3.43183910100006,2.2,-2.51542244900001));
#318783=CARTESIAN_POINT('Ctrl Pts',(-3.43022367500006,12.2,-2.51495650100001));
#318784=CARTESIAN_POINT('Ctrl Pts',(-3.43022367500006,5.2,-2.51495650100001));
#318785=CARTESIAN_POINT('Ctrl Pts',(-3.43022367500006,2.2,-2.51495650100001));
#318786=CARTESIAN_POINT('Ctrl Pts',(-3.42861308300006,12.2,-2.51448994300001));
#318787=CARTESIAN_POINT('Ctrl Pts',(-3.42861308300006,5.2,-2.51448994300001));
#318788=CARTESIAN_POINT('Ctrl Pts',(-3.42861308300006,2.2,-2.51448994300001));
#318789=CARTESIAN_POINT('Ctrl Pts',(-3.42700732800005,12.2,-2.51402278900001));
#318790=CARTESIAN_POINT('Ctrl Pts',(-3.42700732800005,5.2,-2.51402278900001));
#318791=CARTESIAN_POINT('Ctrl Pts',(-3.42700732800005,2.2,-2.51402278900001));
#318792=CARTESIAN_POINT('Ctrl Pts',(-3.42540641600006,12.2,-2.51355504800001));
#318793=CARTESIAN_POINT('Ctrl Pts',(-3.42540641600006,5.2,-2.51355504800001));
#318794=CARTESIAN_POINT('Ctrl Pts',(-3.42540641600006,2.2,-2.51355504800001));
#318795=CARTESIAN_POINT('Ctrl Pts',(-3.42381035200006,12.2,-2.51308673500001));
#318796=CARTESIAN_POINT('Ctrl Pts',(-3.42381035200006,5.2,-2.51308673500001));
#318797=CARTESIAN_POINT('Ctrl Pts',(-3.42381035200006,2.2,-2.51308673500001));
#318798=CARTESIAN_POINT('Ctrl Pts',(-3.42221914100006,12.2,-2.51261785700001));
#318799=CARTESIAN_POINT('Ctrl Pts',(-3.42221914100006,5.2,-2.51261785700001));
#318800=CARTESIAN_POINT('Ctrl Pts',(-3.42221914100006,2.2,-2.51261785700001));
#318801=CARTESIAN_POINT('Ctrl Pts',(-3.42063278900006,12.2,-2.51214842700001));
#318802=CARTESIAN_POINT('Ctrl Pts',(-3.42063278900006,5.2,-2.51214842700001));
#318803=CARTESIAN_POINT('Ctrl Pts',(-3.42063278900006,2.2,-2.51214842700001));
#318804=CARTESIAN_POINT('Ctrl Pts',(-3.41905130000006,12.2,-2.51167845800001));
#318805=CARTESIAN_POINT('Ctrl Pts',(-3.41905130000006,5.2,-2.51167845800001));
#318806=CARTESIAN_POINT('Ctrl Pts',(-3.41905130000006,2.2,-2.51167845800001));
#318807=CARTESIAN_POINT('Ctrl Pts',(-3.41747467900006,12.2,-2.51120795900002));
#318808=CARTESIAN_POINT('Ctrl Pts',(-3.41747467900006,5.2,-2.51120795900002));
#318809=CARTESIAN_POINT('Ctrl Pts',(-3.41747467900006,2.2,-2.51120795900002));
#318810=CARTESIAN_POINT('Ctrl Pts',(-3.41590293200006,12.2,-2.51073694300001));
#318811=CARTESIAN_POINT('Ctrl Pts',(-3.41590293200006,5.2,-2.51073694300001));
#318812=CARTESIAN_POINT('Ctrl Pts',(-3.41590293200006,2.2,-2.51073694300001));
#318813=CARTESIAN_POINT('Ctrl Pts',(-3.41433606500006,12.2,-2.51026542000002));
#318814=CARTESIAN_POINT('Ctrl Pts',(-3.41433606500006,5.2,-2.51026542000002));
#318815=CARTESIAN_POINT('Ctrl Pts',(-3.41433606500006,2.2,-2.51026542000002));
#318816=CARTESIAN_POINT('Ctrl Pts',(-3.41277408100006,12.2,-2.50979340400002));
#318817=CARTESIAN_POINT('Ctrl Pts',(-3.41277408100006,5.2,-2.50979340400002));
#318818=CARTESIAN_POINT('Ctrl Pts',(-3.41277408100006,2.2,-2.50979340400002));
#318819=CARTESIAN_POINT('Ctrl Pts',(-3.41121698600006,12.2,-2.50932090400001));
#318820=CARTESIAN_POINT('Ctrl Pts',(-3.41121698600006,5.2,-2.50932090400001));
#318821=CARTESIAN_POINT('Ctrl Pts',(-3.41121698600006,2.2,-2.50932090400001));
#318822=CARTESIAN_POINT('Ctrl Pts',(-3.40966478600006,12.2,-2.50884793400001));
#318823=CARTESIAN_POINT('Ctrl Pts',(-3.40966478600006,5.2,-2.50884793400001));
#318824=CARTESIAN_POINT('Ctrl Pts',(-3.40966478600006,2.2,-2.50884793400001));
#318825=CARTESIAN_POINT('Ctrl Pts',(-3.40811748400006,12.2,-2.50837450300001));
#318826=CARTESIAN_POINT('Ctrl Pts',(-3.40811748400006,5.2,-2.50837450300001));
#318827=CARTESIAN_POINT('Ctrl Pts',(-3.40811748400006,2.2,-2.50837450300001));
#318828=CARTESIAN_POINT('Ctrl Pts',(-3.40657508900006,12.2,-2.50790062500001));
#318829=CARTESIAN_POINT('Ctrl Pts',(-3.40657508900006,5.2,-2.50790062500001));
#318830=CARTESIAN_POINT('Ctrl Pts',(-3.40657508900006,2.2,-2.50790062500001));
#318831=CARTESIAN_POINT('Ctrl Pts',(-3.40503760100006,12.2,-2.50742631000001));
#318832=CARTESIAN_POINT('Ctrl Pts',(-3.40503760100006,5.2,-2.50742631000001));
#318833=CARTESIAN_POINT('Ctrl Pts',(-3.40503760100006,2.2,-2.50742631000001));
#318834=CARTESIAN_POINT('Ctrl Pts',(-3.40350502900006,12.2,-2.50695157000001));
#318835=CARTESIAN_POINT('Ctrl Pts',(-3.40350502900006,5.2,-2.50695157000001));
#318836=CARTESIAN_POINT('Ctrl Pts',(-3.40350502900006,2.2,-2.50695157000001));
#318837=CARTESIAN_POINT('Ctrl Pts',(-3.40197737600006,12.2,-2.50647641700001));
#318838=CARTESIAN_POINT('Ctrl Pts',(-3.40197737600006,5.2,-2.50647641700001));
#318839=CARTESIAN_POINT('Ctrl Pts',(-3.40197737600006,2.2,-2.50647641700001));
#318840=CARTESIAN_POINT('Ctrl Pts',(-3.40045464900005,12.2,-2.50600086300001));
#318841=CARTESIAN_POINT('Ctrl Pts',(-3.40045464900005,5.2,-2.50600086300001));
#318842=CARTESIAN_POINT('Ctrl Pts',(-3.40045464900005,2.2,-2.50600086300001));
#318843=CARTESIAN_POINT('Ctrl Pts',(-3.39893685000006,12.2,-2.50552492000002));
#318844=CARTESIAN_POINT('Ctrl Pts',(-3.39893685000006,5.2,-2.50552492000002));
#318845=CARTESIAN_POINT('Ctrl Pts',(-3.39893685000006,2.2,-2.50552492000002));
#318846=CARTESIAN_POINT('Ctrl Pts',(-3.39742398800006,12.2,-2.50504859900001));
#318847=CARTESIAN_POINT('Ctrl Pts',(-3.39742398800006,5.2,-2.50504859900001));
#318848=CARTESIAN_POINT('Ctrl Pts',(-3.39742398800006,2.2,-2.50504859900001));
#318849=CARTESIAN_POINT('Ctrl Pts',(-3.39591606600006,12.2,-2.50457191200002));
#318850=CARTESIAN_POINT('Ctrl Pts',(-3.39591606600006,5.2,-2.50457191200002));
#318851=CARTESIAN_POINT('Ctrl Pts',(-3.39591606600006,2.2,-2.50457191200002));
#318852=CARTESIAN_POINT('Ctrl Pts',(-3.39441308800006,12.2,-2.50409487100002));
#318853=CARTESIAN_POINT('Ctrl Pts',(-3.39441308800006,5.2,-2.50409487100002));
#318854=CARTESIAN_POINT('Ctrl Pts',(-3.39441308800006,2.2,-2.50409487100002));
#318855=CARTESIAN_POINT('Ctrl Pts',(-3.39291506000006,12.2,-2.50361748800001));
#318856=CARTESIAN_POINT('Ctrl Pts',(-3.39291506000006,5.2,-2.50361748800001));
#318857=CARTESIAN_POINT('Ctrl Pts',(-3.39291506000006,2.2,-2.50361748800001));
#318858=CARTESIAN_POINT('Ctrl Pts',(-3.39142198700006,12.2,-2.50313977500001));
#318859=CARTESIAN_POINT('Ctrl Pts',(-3.39142198700006,5.2,-2.50313977500001));
#318860=CARTESIAN_POINT('Ctrl Pts',(-3.39142198700006,2.2,-2.50313977500001));
#318861=CARTESIAN_POINT('Ctrl Pts',(-3.38993387600006,12.2,-2.50266174300001));
#318862=CARTESIAN_POINT('Ctrl Pts',(-3.38993387600006,5.2,-2.50266174300001));
#318863=CARTESIAN_POINT('Ctrl Pts',(-3.38993387600006,2.2,-2.50266174300001));
#318864=CARTESIAN_POINT('Ctrl Pts',(-3.38845072900006,12.2,-2.50218340600001));
#318865=CARTESIAN_POINT('Ctrl Pts',(-3.38845072900006,5.2,-2.50218340600001));
#318866=CARTESIAN_POINT('Ctrl Pts',(-3.38845072900006,2.2,-2.50218340600001));
#318867=CARTESIAN_POINT('Ctrl Pts',(-3.38697255200006,12.2,-2.50170477500001));
#318868=CARTESIAN_POINT('Ctrl Pts',(-3.38697255200006,5.2,-2.50170477500001));
#318869=CARTESIAN_POINT('Ctrl Pts',(-3.38697255200006,2.2,-2.50170477500001));
#318870=CARTESIAN_POINT('Ctrl Pts',(-3.38549935200006,12.2,-2.50122586100002));
#318871=CARTESIAN_POINT('Ctrl Pts',(-3.38549935200006,5.2,-2.50122586100002));
#318872=CARTESIAN_POINT('Ctrl Pts',(-3.38549935200006,2.2,-2.50122586100002));
#318873=CARTESIAN_POINT('Ctrl Pts',(-3.38403113100005,12.2,-2.50074667700002));
#318874=CARTESIAN_POINT('Ctrl Pts',(-3.38403113100005,5.2,-2.50074667700002));
#318875=CARTESIAN_POINT('Ctrl Pts',(-3.38403113100005,2.2,-2.50074667700002));
#318876=CARTESIAN_POINT('Ctrl Pts',(-3.38256789600006,12.2,-2.50026723500001));
#318877=CARTESIAN_POINT('Ctrl Pts',(-3.38256789600006,5.2,-2.50026723500001));
#318878=CARTESIAN_POINT('Ctrl Pts',(-3.38256789600006,2.2,-2.50026723500001));
#318879=CARTESIAN_POINT('Ctrl Pts',(-3.38110965100006,12.2,-2.49978754700001));
#318880=CARTESIAN_POINT('Ctrl Pts',(-3.38110965100006,5.2,-2.49978754700001));
#318881=CARTESIAN_POINT('Ctrl Pts',(-3.38110965100006,2.2,-2.49978754700001));
#318882=CARTESIAN_POINT('Ctrl Pts',(-3.37965640100006,12.2,-2.49930762600002));
#318883=CARTESIAN_POINT('Ctrl Pts',(-3.37965640100006,5.2,-2.49930762600002));
#318884=CARTESIAN_POINT('Ctrl Pts',(-3.37965640100006,2.2,-2.49930762600002));
#318885=CARTESIAN_POINT('Ctrl Pts',(-3.37820815200006,12.2,-2.49882748400001));
#318886=CARTESIAN_POINT('Ctrl Pts',(-3.37820815200006,5.2,-2.49882748400001));
#318887=CARTESIAN_POINT('Ctrl Pts',(-3.37820815200006,2.2,-2.49882748400001));
#318888=CARTESIAN_POINT('Ctrl Pts',(-3.37676490800006,12.2,-2.49834713200002));
#318889=CARTESIAN_POINT('Ctrl Pts',(-3.37676490800006,5.2,-2.49834713200002));
#318890=CARTESIAN_POINT('Ctrl Pts',(-3.37676490800006,2.2,-2.49834713200002));
#318891=CARTESIAN_POINT('Ctrl Pts',(-3.37532667400006,12.2,-2.49786658300001));
#318892=CARTESIAN_POINT('Ctrl Pts',(-3.37532667400006,5.2,-2.49786658300001));
#318893=CARTESIAN_POINT('Ctrl Pts',(-3.37532667400006,2.2,-2.49786658300001));
#318894=CARTESIAN_POINT('Ctrl Pts',(-3.37389345600006,12.2,-2.49738584900001));
#318895=CARTESIAN_POINT('Ctrl Pts',(-3.37389345600006,5.2,-2.49738584900001));
#318896=CARTESIAN_POINT('Ctrl Pts',(-3.37389345600006,2.2,-2.49738584900001));
#318897=CARTESIAN_POINT('Ctrl Pts',(-3.37246525800006,12.2,-2.49690494400001));
#318898=CARTESIAN_POINT('Ctrl Pts',(-3.37246525800006,5.2,-2.49690494400001));
#318899=CARTESIAN_POINT('Ctrl Pts',(-3.37246525800006,2.2,-2.49690494400001));
#318900=CARTESIAN_POINT('Ctrl Pts',(-3.37104208500006,12.2,-2.49642387800002));
#318901=CARTESIAN_POINT('Ctrl Pts',(-3.37104208500006,5.2,-2.49642387800002));
#318902=CARTESIAN_POINT('Ctrl Pts',(-3.37104208500006,2.2,-2.49642387800002));
#318903=CARTESIAN_POINT('Ctrl Pts',(-3.36962394300006,12.2,-2.49594266500001));
#318904=CARTESIAN_POINT('Ctrl Pts',(-3.36962394300006,5.2,-2.49594266500001));
#318905=CARTESIAN_POINT('Ctrl Pts',(-3.36962394300006,2.2,-2.49594266500001));
#318906=CARTESIAN_POINT('Ctrl Pts',(-3.36821083500006,12.2,-2.49546131700002));
#318907=CARTESIAN_POINT('Ctrl Pts',(-3.36821083500006,5.2,-2.49546131700002));
#318908=CARTESIAN_POINT('Ctrl Pts',(-3.36821083500006,2.2,-2.49546131700002));
#318909=CARTESIAN_POINT('Ctrl Pts',(-3.36680276800006,12.2,-2.49497984500001));
#318910=CARTESIAN_POINT('Ctrl Pts',(-3.36680276800006,5.2,-2.49497984500001));
#318911=CARTESIAN_POINT('Ctrl Pts',(-3.36680276800006,2.2,-2.49497984500001));
#318912=CARTESIAN_POINT('Ctrl Pts',(-3.36539974500006,12.2,-2.49449826400001));
#318913=CARTESIAN_POINT('Ctrl Pts',(-3.36539974500006,5.2,-2.49449826400001));
#318914=CARTESIAN_POINT('Ctrl Pts',(-3.36539974500006,2.2,-2.49449826400001));
#318915=CARTESIAN_POINT('Ctrl Pts',(-3.36400177300006,12.2,-2.49401658500001));
#318916=CARTESIAN_POINT('Ctrl Pts',(-3.36400177300006,5.2,-2.49401658500001));
#318917=CARTESIAN_POINT('Ctrl Pts',(-3.36400177300006,2.2,-2.49401658500001));
#318918=CARTESIAN_POINT('Ctrl Pts',(-3.36260885500006,12.2,-2.49353482100001));
#318919=CARTESIAN_POINT('Ctrl Pts',(-3.36260885500006,5.2,-2.49353482100001));
#318920=CARTESIAN_POINT('Ctrl Pts',(-3.36260885500006,2.2,-2.49353482100001));
#318921=CARTESIAN_POINT('Ctrl Pts',(-3.36122099700006,12.2,-2.49305298500001));
#318922=CARTESIAN_POINT('Ctrl Pts',(-3.36122099700006,5.2,-2.49305298500001));
#318923=CARTESIAN_POINT('Ctrl Pts',(-3.36122099700006,2.2,-2.49305298500001));
#318924=CARTESIAN_POINT('Ctrl Pts',(-3.35983820300005,12.2,-2.49257108800002));
#318925=CARTESIAN_POINT('Ctrl Pts',(-3.35983820300005,5.2,-2.49257108800002));
#318926=CARTESIAN_POINT('Ctrl Pts',(-3.35983820300005,2.2,-2.49257108800002));
#318927=CARTESIAN_POINT('Ctrl Pts',(-3.35846048000006,12.2,-2.49208914400001));
#318928=CARTESIAN_POINT('Ctrl Pts',(-3.35846048000006,5.2,-2.49208914400001));
#318929=CARTESIAN_POINT('Ctrl Pts',(-3.35846048000006,2.2,-2.49208914400001));
#318930=CARTESIAN_POINT('Ctrl Pts',(-3.35708783000006,12.2,-2.49160716600001));
#318931=CARTESIAN_POINT('Ctrl Pts',(-3.35708783000006,5.2,-2.49160716600001));
#318932=CARTESIAN_POINT('Ctrl Pts',(-3.35708783000006,2.2,-2.49160716600001));
#318933=CARTESIAN_POINT('Ctrl Pts',(-3.35572026000006,12.2,-2.49112516600002));
#318934=CARTESIAN_POINT('Ctrl Pts',(-3.35572026000006,5.2,-2.49112516600002));
#318935=CARTESIAN_POINT('Ctrl Pts',(-3.35572026000006,2.2,-2.49112516600002));
#318936=CARTESIAN_POINT('Ctrl Pts',(-3.35435777400006,12.2,-2.49064315600001));
#318937=CARTESIAN_POINT('Ctrl Pts',(-3.35435777400006,5.2,-2.49064315600001));
#318938=CARTESIAN_POINT('Ctrl Pts',(-3.35435777400006,2.2,-2.49064315600001));
#318939=CARTESIAN_POINT('Ctrl Pts',(-3.35300037700006,12.2,-2.49016115000002));
#318940=CARTESIAN_POINT('Ctrl Pts',(-3.35300037700006,5.2,-2.49016115000002));
#318941=CARTESIAN_POINT('Ctrl Pts',(-3.35300037700006,2.2,-2.49016115000002));
#318942=CARTESIAN_POINT('Ctrl Pts',(-3.35164807400006,12.2,-2.48967916000002));
#318943=CARTESIAN_POINT('Ctrl Pts',(-3.35164807400006,5.2,-2.48967916000002));
#318944=CARTESIAN_POINT('Ctrl Pts',(-3.35164807400006,2.2,-2.48967916000002));
#318945=CARTESIAN_POINT('Ctrl Pts',(-3.35030087000006,12.2,-2.48919720100002));
#318946=CARTESIAN_POINT('Ctrl Pts',(-3.35030087000006,5.2,-2.48919720100002));
#318947=CARTESIAN_POINT('Ctrl Pts',(-3.35030087000006,2.2,-2.48919720100002));
#318948=CARTESIAN_POINT('Ctrl Pts',(-3.34895877000006,12.2,-2.48871528200001));
#318949=CARTESIAN_POINT('Ctrl Pts',(-3.34895877000006,5.2,-2.48871528200001));
#318950=CARTESIAN_POINT('Ctrl Pts',(-3.34895877000006,2.2,-2.48871528200001));
#318951=CARTESIAN_POINT('Ctrl Pts',(-3.34762177700005,12.2,-2.48823341900001));
#318952=CARTESIAN_POINT('Ctrl Pts',(-3.34762177700005,5.2,-2.48823341900001));
#318953=CARTESIAN_POINT('Ctrl Pts',(-3.34762177700005,2.2,-2.48823341900001));
#318954=CARTESIAN_POINT('Ctrl Pts',(-3.34628989900006,12.2,-2.48775162500001));
#318955=CARTESIAN_POINT('Ctrl Pts',(-3.34628989900006,5.2,-2.48775162500001));
#318956=CARTESIAN_POINT('Ctrl Pts',(-3.34628989900006,2.2,-2.48775162500001));
#318957=CARTESIAN_POINT('Ctrl Pts',(-3.34496313800006,12.2,-2.48726991000002));
#318958=CARTESIAN_POINT('Ctrl Pts',(-3.34496313800006,5.2,-2.48726991000002));
#318959=CARTESIAN_POINT('Ctrl Pts',(-3.34496313800006,2.2,-2.48726991000002));
#318960=CARTESIAN_POINT('Ctrl Pts',(-3.34364150100006,12.2,-2.48678829000001));
#318961=CARTESIAN_POINT('Ctrl Pts',(-3.34364150100006,5.2,-2.48678829000001));
#318962=CARTESIAN_POINT('Ctrl Pts',(-3.34364150100006,2.2,-2.48678829000001));
#318963=CARTESIAN_POINT('Ctrl Pts',(-3.34232499000006,12.2,-2.48630677700001));
#318964=CARTESIAN_POINT('Ctrl Pts',(-3.34232499000006,5.2,-2.48630677700001));
#318965=CARTESIAN_POINT('Ctrl Pts',(-3.34232499000006,2.2,-2.48630677700001));
#318966=CARTESIAN_POINT('Ctrl Pts',(-3.34101361300006,12.2,-2.48582538400001));
#318967=CARTESIAN_POINT('Ctrl Pts',(-3.34101361300006,5.2,-2.48582538400001));
#318968=CARTESIAN_POINT('Ctrl Pts',(-3.34101361300006,2.2,-2.48582538400001));
#318969=CARTESIAN_POINT('Ctrl Pts',(-3.33970737300006,12.2,-2.48534412500002));
#318970=CARTESIAN_POINT('Ctrl Pts',(-3.33970737300006,5.2,-2.48534412500002));
#318971=CARTESIAN_POINT('Ctrl Pts',(-3.33970737300006,2.2,-2.48534412500002));
#318972=CARTESIAN_POINT('Ctrl Pts',(-3.33840627500006,12.2,-2.48486301100002));
#318973=CARTESIAN_POINT('Ctrl Pts',(-3.33840627500006,5.2,-2.48486301100002));
#318974=CARTESIAN_POINT('Ctrl Pts',(-3.33840627500006,2.2,-2.48486301100002));
#318975=CARTESIAN_POINT('Ctrl Pts',(-3.33711032500006,12.2,-2.48438205700001));
#318976=CARTESIAN_POINT('Ctrl Pts',(-3.33711032500006,5.2,-2.48438205700001));
#318977=CARTESIAN_POINT('Ctrl Pts',(-3.33711032500006,2.2,-2.48438205700001));
#318978=CARTESIAN_POINT('Ctrl Pts',(-3.33581952600006,12.2,-2.48390127600001));
#318979=CARTESIAN_POINT('Ctrl Pts',(-3.33581952600006,5.2,-2.48390127600001));
#318980=CARTESIAN_POINT('Ctrl Pts',(-3.33581952600006,2.2,-2.48390127600001));
#318981=CARTESIAN_POINT('Ctrl Pts',(-3.33453388300006,12.2,-2.48342068100001));
#318982=CARTESIAN_POINT('Ctrl Pts',(-3.33453388300006,5.2,-2.48342068100001));
#318983=CARTESIAN_POINT('Ctrl Pts',(-3.33453388300006,2.2,-2.48342068100001));
#318984=CARTESIAN_POINT('Ctrl Pts',(-3.33325340200005,12.2,-2.48294028500001));
#318985=CARTESIAN_POINT('Ctrl Pts',(-3.33325340200005,5.2,-2.48294028500001));
#318986=CARTESIAN_POINT('Ctrl Pts',(-3.33325340200005,2.2,-2.48294028500001));
#318987=CARTESIAN_POINT('Ctrl Pts',(-3.33197808600006,12.2,-2.48246010200001));
#318988=CARTESIAN_POINT('Ctrl Pts',(-3.33197808600006,5.2,-2.48246010200001));
#318989=CARTESIAN_POINT('Ctrl Pts',(-3.33197808600006,2.2,-2.48246010200001));
#318990=CARTESIAN_POINT('Ctrl Pts',(-3.33070794200006,12.2,-2.48198014500002));
#318991=CARTESIAN_POINT('Ctrl Pts',(-3.33070794200006,5.2,-2.48198014500002));
#318992=CARTESIAN_POINT('Ctrl Pts',(-3.33070794200006,2.2,-2.48198014500002));
#318993=CARTESIAN_POINT('Ctrl Pts',(-3.32944297300005,12.2,-2.48150042700002));
#318994=CARTESIAN_POINT('Ctrl Pts',(-3.32944297300005,5.2,-2.48150042700002));
#318995=CARTESIAN_POINT('Ctrl Pts',(-3.32944297300005,2.2,-2.48150042700002));
#318996=CARTESIAN_POINT('Ctrl Pts',(-3.32818318400005,12.2,-2.48102096200002));
#318997=CARTESIAN_POINT('Ctrl Pts',(-3.32818318400005,5.2,-2.48102096200002));
#318998=CARTESIAN_POINT('Ctrl Pts',(-3.32818318400005,2.2,-2.48102096200002));
#318999=CARTESIAN_POINT('Ctrl Pts',(-3.32692858000006,12.2,-2.48054176300001));
#319000=CARTESIAN_POINT('Ctrl Pts',(-3.32692858000006,5.2,-2.48054176300001));
#319001=CARTESIAN_POINT('Ctrl Pts',(-3.32692858000006,2.2,-2.48054176300001));
#319002=CARTESIAN_POINT('Ctrl Pts',(-3.32567916700006,12.2,-2.48006284300001));
#319003=CARTESIAN_POINT('Ctrl Pts',(-3.32567916700006,5.2,-2.48006284300001));
#319004=CARTESIAN_POINT('Ctrl Pts',(-3.32567916700006,2.2,-2.48006284300001));
#319005=CARTESIAN_POINT('Ctrl Pts',(-3.32443494700006,12.2,-2.47958421700002));
#319006=CARTESIAN_POINT('Ctrl Pts',(-3.32443494700006,5.2,-2.47958421700002));
#319007=CARTESIAN_POINT('Ctrl Pts',(-3.32443494700006,2.2,-2.47958421700002));
#319008=CARTESIAN_POINT('Ctrl Pts',(-3.32319592500005,12.2,-2.47910589800002));
#319009=CARTESIAN_POINT('Ctrl Pts',(-3.32319592500005,5.2,-2.47910589800002));
#319010=CARTESIAN_POINT('Ctrl Pts',(-3.32319592500005,2.2,-2.47910589800002));
#319011=CARTESIAN_POINT('Ctrl Pts',(-3.32196210900006,12.2,-2.47862789900001));
#319012=CARTESIAN_POINT('Ctrl Pts',(-3.32196210900006,5.2,-2.47862789900001));
#319013=CARTESIAN_POINT('Ctrl Pts',(-3.32196210900006,2.2,-2.47862789900001));
#319014=CARTESIAN_POINT('Ctrl Pts',(-3.32073350000006,12.2,-2.47815023400001));
#319015=CARTESIAN_POINT('Ctrl Pts',(-3.32073350000006,5.2,-2.47815023400001));
#319016=CARTESIAN_POINT('Ctrl Pts',(-3.32073350000006,2.2,-2.47815023400001));
#319017=CARTESIAN_POINT('Ctrl Pts',(-3.31951010500006,12.2,-2.47767291800002));
#319018=CARTESIAN_POINT('Ctrl Pts',(-3.31951010500006,5.2,-2.47767291800002));
#319019=CARTESIAN_POINT('Ctrl Pts',(-3.31951010500006,2.2,-2.47767291800002));
#319020=CARTESIAN_POINT('Ctrl Pts',(-3.31829192800006,12.2,-2.47719596200001));
#319021=CARTESIAN_POINT('Ctrl Pts',(-3.31829192800006,5.2,-2.47719596200001));
#319022=CARTESIAN_POINT('Ctrl Pts',(-3.31829192800006,2.2,-2.47719596200001));
#319023=CARTESIAN_POINT('Ctrl Pts',(-3.31707897300006,12.2,-2.47671938100002));
#319024=CARTESIAN_POINT('Ctrl Pts',(-3.31707897300006,5.2,-2.47671938100002));
#319025=CARTESIAN_POINT('Ctrl Pts',(-3.31707897300006,2.2,-2.47671938100002));
#319026=CARTESIAN_POINT('Ctrl Pts',(-3.31587124500006,12.2,-2.47624318900002));
#319027=CARTESIAN_POINT('Ctrl Pts',(-3.31587124500006,5.2,-2.47624318900002));
#319028=CARTESIAN_POINT('Ctrl Pts',(-3.31587124500006,2.2,-2.47624318900002));
#319029=CARTESIAN_POINT('Ctrl Pts',(-3.31466875000006,12.2,-2.47576740100001));
#319030=CARTESIAN_POINT('Ctrl Pts',(-3.31466875000006,5.2,-2.47576740100001));
#319031=CARTESIAN_POINT('Ctrl Pts',(-3.31466875000006,2.2,-2.47576740100001));
#319032=CARTESIAN_POINT('Ctrl Pts',(-3.31347149000006,12.2,-2.47529202900001));
#319033=CARTESIAN_POINT('Ctrl Pts',(-3.31347149000006,5.2,-2.47529202900001));
#319034=CARTESIAN_POINT('Ctrl Pts',(-3.31347149000006,2.2,-2.47529202900001));
#319035=CARTESIAN_POINT('Ctrl Pts',(-3.31227947200006,12.2,-2.47481708700001));
#319036=CARTESIAN_POINT('Ctrl Pts',(-3.31227947200006,5.2,-2.47481708700001));
#319037=CARTESIAN_POINT('Ctrl Pts',(-3.31227947200006,2.2,-2.47481708700001));
#319038=CARTESIAN_POINT('Ctrl Pts',(-3.31109269900006,12.2,-2.47434258900002));
#319039=CARTESIAN_POINT('Ctrl Pts',(-3.31109269900006,5.2,-2.47434258900002));
#319040=CARTESIAN_POINT('Ctrl Pts',(-3.31109269900006,2.2,-2.47434258900002));
#319041=CARTESIAN_POINT('Ctrl Pts',(-3.30991117600006,12.2,-2.47386855000002));
#319042=CARTESIAN_POINT('Ctrl Pts',(-3.30991117600006,5.2,-2.47386855000002));
#319043=CARTESIAN_POINT('Ctrl Pts',(-3.30991117600006,2.2,-2.47386855000002));
#319044=CARTESIAN_POINT('Ctrl Pts',(-3.30873490900006,12.2,-2.47339498400001));
#319045=CARTESIAN_POINT('Ctrl Pts',(-3.30873490900006,5.2,-2.47339498400001));
#319046=CARTESIAN_POINT('Ctrl Pts',(-3.30873490900006,2.2,-2.47339498400001));
#319047=CARTESIAN_POINT('Ctrl Pts',(-3.30756390200006,12.2,-2.47292190300001));
#319048=CARTESIAN_POINT('Ctrl Pts',(-3.30756390200006,5.2,-2.47292190300001));
#319049=CARTESIAN_POINT('Ctrl Pts',(-3.30756390200006,2.2,-2.47292190300001));
#319050=CARTESIAN_POINT('Ctrl Pts',(-3.30639815800006,12.2,-2.47244932300001));
#319051=CARTESIAN_POINT('Ctrl Pts',(-3.30639815800006,5.2,-2.47244932300001));
#319052=CARTESIAN_POINT('Ctrl Pts',(-3.30639815800006,2.2,-2.47244932300001));
#319053=CARTESIAN_POINT('Ctrl Pts',(-3.30523768300006,12.2,-2.47197725900001));
#319054=CARTESIAN_POINT('Ctrl Pts',(-3.30523768300006,5.2,-2.47197725900001));
#319055=CARTESIAN_POINT('Ctrl Pts',(-3.30523768300006,2.2,-2.47197725900001));
#319056=CARTESIAN_POINT('Ctrl Pts',(-3.30408248100006,12.2,-2.47150572200002));
#319057=CARTESIAN_POINT('Ctrl Pts',(-3.30408248100006,5.2,-2.47150572200002));
#319058=CARTESIAN_POINT('Ctrl Pts',(-3.30408248100006,2.2,-2.47150572200002));
#319059=CARTESIAN_POINT('Ctrl Pts',(-3.30293255700005,12.2,-2.47103473000001));
#319060=CARTESIAN_POINT('Ctrl Pts',(-3.30293255700005,5.2,-2.47103473000001));
#319061=CARTESIAN_POINT('Ctrl Pts',(-3.30293255700005,2.2,-2.47103473000001));
#319062=CARTESIAN_POINT('Ctrl Pts',(-3.30178791500006,12.2,-2.47056429300001));
#319063=CARTESIAN_POINT('Ctrl Pts',(-3.30178791500006,5.2,-2.47056429300001));
#319064=CARTESIAN_POINT('Ctrl Pts',(-3.30178791500006,2.2,-2.47056429300001));
#319065=CARTESIAN_POINT('Ctrl Pts',(-3.30064856100006,12.2,-2.47009442900001));
#319066=CARTESIAN_POINT('Ctrl Pts',(-3.30064856100006,5.2,-2.47009442900001));
#319067=CARTESIAN_POINT('Ctrl Pts',(-3.30064856100006,2.2,-2.47009442900001));
#319068=CARTESIAN_POINT('Ctrl Pts',(-3.29951449800005,12.2,-2.46962514900002));
#319069=CARTESIAN_POINT('Ctrl Pts',(-3.29951449800005,5.2,-2.46962514900002));
#319070=CARTESIAN_POINT('Ctrl Pts',(-3.29951449800005,2.2,-2.46962514900002));
#319071=CARTESIAN_POINT('Ctrl Pts',(-3.29838573100006,12.2,-2.46915647100002));
#319072=CARTESIAN_POINT('Ctrl Pts',(-3.29838573100006,5.2,-2.46915647100002));
#319073=CARTESIAN_POINT('Ctrl Pts',(-3.29838573100006,2.2,-2.46915647100002));
#319074=CARTESIAN_POINT('Ctrl Pts',(-3.29726226400005,12.2,-2.46868840700001));
#319075=CARTESIAN_POINT('Ctrl Pts',(-3.29726226400005,5.2,-2.46868840700001));
#319076=CARTESIAN_POINT('Ctrl Pts',(-3.29726226400005,2.2,-2.46868840700001));
#319077=CARTESIAN_POINT('Ctrl Pts',(-3.29614410300006,12.2,-2.46822097100001));
#319078=CARTESIAN_POINT('Ctrl Pts',(-3.29614410300006,5.2,-2.46822097100001));
#319079=CARTESIAN_POINT('Ctrl Pts',(-3.29614410300006,2.2,-2.46822097100001));
#319080=CARTESIAN_POINT('Ctrl Pts',(-3.29503125100006,12.2,-2.46775417800002));
#319081=CARTESIAN_POINT('Ctrl Pts',(-3.29503125100006,5.2,-2.46775417800002));
#319082=CARTESIAN_POINT('Ctrl Pts',(-3.29503125100006,2.2,-2.46775417800002));
#319083=CARTESIAN_POINT('Ctrl Pts',(-3.29392371400006,12.2,-2.46728804500002));
#319084=CARTESIAN_POINT('Ctrl Pts',(-3.29392371400006,5.2,-2.46728804500002));
#319085=CARTESIAN_POINT('Ctrl Pts',(-3.29392371400006,2.2,-2.46728804500002));
#319086=CARTESIAN_POINT('Ctrl Pts',(-3.29282149400006,12.2,-2.46682258300002));
#319087=CARTESIAN_POINT('Ctrl Pts',(-3.29282149400006,5.2,-2.46682258300002));
#319088=CARTESIAN_POINT('Ctrl Pts',(-3.29282149400006,2.2,-2.46682258300002));
#319089=CARTESIAN_POINT('Ctrl Pts',(-3.29172459900006,12.2,-2.46635780800001));
#319090=CARTESIAN_POINT('Ctrl Pts',(-3.29172459900006,5.2,-2.46635780800001));
#319091=CARTESIAN_POINT('Ctrl Pts',(-3.29172459900006,2.2,-2.46635780800001));
#319092=CARTESIAN_POINT('Ctrl Pts',(-3.29063303000006,12.2,-2.46589373500001));
#319093=CARTESIAN_POINT('Ctrl Pts',(-3.29063303000006,5.2,-2.46589373500001));
#319094=CARTESIAN_POINT('Ctrl Pts',(-3.29063303000006,2.2,-2.46589373500001));
#319095=CARTESIAN_POINT('Ctrl Pts',(-3.28954679400006,12.2,-2.46543037800001));
#319096=CARTESIAN_POINT('Ctrl Pts',(-3.28954679400006,5.2,-2.46543037800001));
#319097=CARTESIAN_POINT('Ctrl Pts',(-3.28954679400006,2.2,-2.46543037800001));
#319098=CARTESIAN_POINT('Ctrl Pts',(-3.28846589400006,12.2,-2.46496775200002));
#319099=CARTESIAN_POINT('Ctrl Pts',(-3.28846589400006,5.2,-2.46496775200002));
#319100=CARTESIAN_POINT('Ctrl Pts',(-3.28846589400006,2.2,-2.46496775200002));
#319101=CARTESIAN_POINT('Ctrl Pts',(-3.28739033400006,12.2,-2.46450587100002));
#319102=CARTESIAN_POINT('Ctrl Pts',(-3.28739033400006,5.2,-2.46450587100002));
#319103=CARTESIAN_POINT('Ctrl Pts',(-3.28739033400006,2.2,-2.46450587100002));
#319104=CARTESIAN_POINT('Ctrl Pts',(-3.28632012100006,12.2,-2.46404475100002));
#319105=CARTESIAN_POINT('Ctrl Pts',(-3.28632012100006,5.2,-2.46404475100002));
#319106=CARTESIAN_POINT('Ctrl Pts',(-3.28632012100006,2.2,-2.46404475100002));
#319107=CARTESIAN_POINT('Ctrl Pts',(-3.28525525700006,12.2,-2.46358440600002));
#319108=CARTESIAN_POINT('Ctrl Pts',(-3.28525525700006,5.2,-2.46358440600002));
#319109=CARTESIAN_POINT('Ctrl Pts',(-3.28525525700006,2.2,-2.46358440600002));
#319110=CARTESIAN_POINT('Ctrl Pts',(-3.28419574700006,12.2,-2.46312485200002));
#319111=CARTESIAN_POINT('Ctrl Pts',(-3.28419574700006,5.2,-2.46312485200002));
#319112=CARTESIAN_POINT('Ctrl Pts',(-3.28419574700006,2.2,-2.46312485200002));
#319113=CARTESIAN_POINT('Ctrl Pts',(-3.28314159600006,12.2,-2.46266610200002));
#319114=CARTESIAN_POINT('Ctrl Pts',(-3.28314159600006,5.2,-2.46266610200002));
#319115=CARTESIAN_POINT('Ctrl Pts',(-3.28314159600006,2.2,-2.46266610200002));
#319116=CARTESIAN_POINT('Ctrl Pts',(-3.28209280800006,12.2,-2.46220817300001));
#319117=CARTESIAN_POINT('Ctrl Pts',(-3.28209280800006,5.2,-2.46220817300001));
#319118=CARTESIAN_POINT('Ctrl Pts',(-3.28209280800006,2.2,-2.46220817300001));
#319119=CARTESIAN_POINT('Ctrl Pts',(-3.28104938800006,12.2,-2.46175107800001));
#319120=CARTESIAN_POINT('Ctrl Pts',(-3.28104938800006,5.2,-2.46175107800001));
#319121=CARTESIAN_POINT('Ctrl Pts',(-3.28104938800006,2.2,-2.46175107800001));
#319122=CARTESIAN_POINT('Ctrl Pts',(-3.28001133900006,12.2,-2.46129483400002));
#319123=CARTESIAN_POINT('Ctrl Pts',(-3.28001133900006,5.2,-2.46129483400002));
#319124=CARTESIAN_POINT('Ctrl Pts',(-3.28001133900006,2.2,-2.46129483400002));
#319125=CARTESIAN_POINT('Ctrl Pts',(-3.27897866600006,12.2,-2.46083945400001));
#319126=CARTESIAN_POINT('Ctrl Pts',(-3.27897866600006,5.2,-2.46083945400001));
#319127=CARTESIAN_POINT('Ctrl Pts',(-3.27897866600006,2.2,-2.46083945400001));
#319128=CARTESIAN_POINT('Ctrl Pts',(-3.27795137500006,12.2,-2.46038495500001));
#319129=CARTESIAN_POINT('Ctrl Pts',(-3.27795137500006,5.2,-2.46038495500001));
#319130=CARTESIAN_POINT('Ctrl Pts',(-3.27795137500006,2.2,-2.46038495500001));
#319131=CARTESIAN_POINT('Ctrl Pts',(-3.27692946800005,12.2,-2.45993135100001));
#319132=CARTESIAN_POINT('Ctrl Pts',(-3.27692946800005,5.2,-2.45993135100001));
#319133=CARTESIAN_POINT('Ctrl Pts',(-3.27692946800005,2.2,-2.45993135100001));
#319134=CARTESIAN_POINT('Ctrl Pts',(-3.27591295000006,12.2,-2.45947865700002));
#319135=CARTESIAN_POINT('Ctrl Pts',(-3.27591295000006,5.2,-2.45947865700002));
#319136=CARTESIAN_POINT('Ctrl Pts',(-3.27591295000006,2.2,-2.45947865700002));
#319137=CARTESIAN_POINT('Ctrl Pts',(-3.27490182500005,12.2,-2.45902688900001));
#319138=CARTESIAN_POINT('Ctrl Pts',(-3.27490182500005,5.2,-2.45902688900001));
#319139=CARTESIAN_POINT('Ctrl Pts',(-3.27490182500005,2.2,-2.45902688900001));
#319140=CARTESIAN_POINT('Ctrl Pts',(-3.27389610000006,12.2,-2.45857606200001));
#319141=CARTESIAN_POINT('Ctrl Pts',(-3.27389610000006,5.2,-2.45857606200001));
#319142=CARTESIAN_POINT('Ctrl Pts',(-3.27389610000006,2.2,-2.45857606200001));
#319143=CARTESIAN_POINT('Ctrl Pts',(-3.27289577600005,12.2,-2.45812619100001));
#319144=CARTESIAN_POINT('Ctrl Pts',(-3.27289577600005,5.2,-2.45812619100001));
#319145=CARTESIAN_POINT('Ctrl Pts',(-3.27289577600005,2.2,-2.45812619100001));
#319146=CARTESIAN_POINT('Ctrl Pts',(-3.27190085800006,12.2,-2.45767729200002));
#319147=CARTESIAN_POINT('Ctrl Pts',(-3.27190085800006,5.2,-2.45767729200002));
#319148=CARTESIAN_POINT('Ctrl Pts',(-3.27190085800006,2.2,-2.45767729200002));
#319149=CARTESIAN_POINT('Ctrl Pts',(-3.27091135200006,12.2,-2.45722938000001));
#319150=CARTESIAN_POINT('Ctrl Pts',(-3.27091135200006,5.2,-2.45722938000001));
#319151=CARTESIAN_POINT('Ctrl Pts',(-3.27091135200006,2.2,-2.45722938000001));
#319152=CARTESIAN_POINT('Ctrl Pts',(-3.26992726100006,12.2,-2.45678247000002));
#319153=CARTESIAN_POINT('Ctrl Pts',(-3.26992726100006,5.2,-2.45678247000002));
#319154=CARTESIAN_POINT('Ctrl Pts',(-3.26992726100006,2.2,-2.45678247000002));
#319155=CARTESIAN_POINT('Ctrl Pts',(-3.26894858800005,12.2,-2.45633657900001));
#319156=CARTESIAN_POINT('Ctrl Pts',(-3.26894858800005,5.2,-2.45633657900001));
#319157=CARTESIAN_POINT('Ctrl Pts',(-3.26894858800005,2.2,-2.45633657900001));
#319158=CARTESIAN_POINT('Ctrl Pts',(-3.26797534100006,12.2,-2.45589172000001));
#319159=CARTESIAN_POINT('Ctrl Pts',(-3.26797534100006,5.2,-2.45589172000001));
#319160=CARTESIAN_POINT('Ctrl Pts',(-3.26797534100006,2.2,-2.45589172000001));
#319161=CARTESIAN_POINT('Ctrl Pts',(-3.26700752100006,12.2,-2.45544791100002));
#319162=CARTESIAN_POINT('Ctrl Pts',(-3.26700752100006,5.2,-2.45544791100002));
#319163=CARTESIAN_POINT('Ctrl Pts',(-3.26700752100006,2.2,-2.45544791100002));
#319164=CARTESIAN_POINT('Ctrl Pts',(-3.26604513300006,12.2,-2.45500516800002));
#319165=CARTESIAN_POINT('Ctrl Pts',(-3.26604513300006,5.2,-2.45500516800002));
#319166=CARTESIAN_POINT('Ctrl Pts',(-3.26604513300006,2.2,-2.45500516800002));
#319167=CARTESIAN_POINT('Ctrl Pts',(-3.26508818200006,12.2,-2.45456350400001));
#319168=CARTESIAN_POINT('Ctrl Pts',(-3.26508818200006,5.2,-2.45456350400001));
#319169=CARTESIAN_POINT('Ctrl Pts',(-3.26508818200006,2.2,-2.45456350400001));
#319170=CARTESIAN_POINT('Ctrl Pts',(-3.26413667200006,12.2,-2.45412293500001));
#319171=CARTESIAN_POINT('Ctrl Pts',(-3.26413667200006,5.2,-2.45412293500001));
#319172=CARTESIAN_POINT('Ctrl Pts',(-3.26413667200006,2.2,-2.45412293500001));
#319173=CARTESIAN_POINT('Ctrl Pts',(-3.26319060600006,12.2,-2.45368347900001));
#319174=CARTESIAN_POINT('Ctrl Pts',(-3.26319060600006,5.2,-2.45368347900001));
#319175=CARTESIAN_POINT('Ctrl Pts',(-3.26319060600006,2.2,-2.45368347900001));
#319176=CARTESIAN_POINT('Ctrl Pts',(-3.26224999000006,12.2,-2.45324515000001));
#319177=CARTESIAN_POINT('Ctrl Pts',(-3.26224999000006,5.2,-2.45324515000001));
#319178=CARTESIAN_POINT('Ctrl Pts',(-3.26224999000006,2.2,-2.45324515000001));
#319179=CARTESIAN_POINT('Ctrl Pts',(-3.26131482700006,12.2,-2.45280796500001));
#319180=CARTESIAN_POINT('Ctrl Pts',(-3.26131482700006,5.2,-2.45280796500001));
#319181=CARTESIAN_POINT('Ctrl Pts',(-3.26131482700006,2.2,-2.45280796500001));
#319182=CARTESIAN_POINT('Ctrl Pts',(-3.26038512300005,12.2,-2.45237194000001));
#319183=CARTESIAN_POINT('Ctrl Pts',(-3.26038512300005,5.2,-2.45237194000001));
#319184=CARTESIAN_POINT('Ctrl Pts',(-3.26038512300005,2.2,-2.45237194000001));
#319185=CARTESIAN_POINT('Ctrl Pts',(-3.25946087900005,12.2,-2.45193708800001));
#319186=CARTESIAN_POINT('Ctrl Pts',(-3.25946087900005,5.2,-2.45193708800001));
#319187=CARTESIAN_POINT('Ctrl Pts',(-3.25946087900005,2.2,-2.45193708800001));
#319188=CARTESIAN_POINT('Ctrl Pts',(-3.25854210200006,12.2,-2.45150342900001));
#319189=CARTESIAN_POINT('Ctrl Pts',(-3.25854210200006,5.2,-2.45150342900001));
#319190=CARTESIAN_POINT('Ctrl Pts',(-3.25854210200006,2.2,-2.45150342900001));
#319191=CARTESIAN_POINT('Ctrl Pts',(-3.25762879500005,12.2,-2.45107097800001));
#319192=CARTESIAN_POINT('Ctrl Pts',(-3.25762879500005,5.2,-2.45107097800001));
#319193=CARTESIAN_POINT('Ctrl Pts',(-3.25762879500005,2.2,-2.45107097800001));
#319194=CARTESIAN_POINT('Ctrl Pts',(-3.25672096200006,12.2,-2.45063974800001));
#319195=CARTESIAN_POINT('Ctrl Pts',(-3.25672096200006,5.2,-2.45063974800001));
#319196=CARTESIAN_POINT('Ctrl Pts',(-3.25672096200006,2.2,-2.45063974800001));
#319197=CARTESIAN_POINT('Ctrl Pts',(-3.25581860800006,12.2,-2.45020975800001));
#319198=CARTESIAN_POINT('Ctrl Pts',(-3.25581860800006,5.2,-2.45020975800001));
#319199=CARTESIAN_POINT('Ctrl Pts',(-3.25581860800006,2.2,-2.45020975800001));
#319200=CARTESIAN_POINT('Ctrl Pts',(-3.25492173600006,12.2,-2.44978102500002));
#319201=CARTESIAN_POINT('Ctrl Pts',(-3.25492173600006,5.2,-2.44978102500002));
#319202=CARTESIAN_POINT('Ctrl Pts',(-3.25492173600006,2.2,-2.44978102500002));
#319203=CARTESIAN_POINT('Ctrl Pts',(-3.25403035100006,12.2,-2.44935356300001));
#319204=CARTESIAN_POINT('Ctrl Pts',(-3.25403035100006,5.2,-2.44935356300001));
#319205=CARTESIAN_POINT('Ctrl Pts',(-3.25403035100006,2.2,-2.44935356300001));
#319206=CARTESIAN_POINT('Ctrl Pts',(-3.25314445700006,12.2,-2.44892738900001));
#319207=CARTESIAN_POINT('Ctrl Pts',(-3.25314445700006,5.2,-2.44892738900001));
#319208=CARTESIAN_POINT('Ctrl Pts',(-3.25314445700006,2.2,-2.44892738900001));
#319209=CARTESIAN_POINT('Ctrl Pts',(-3.25226405800006,12.2,-2.44850251900001));
#319210=CARTESIAN_POINT('Ctrl Pts',(-3.25226405800006,5.2,-2.44850251900001));
#319211=CARTESIAN_POINT('Ctrl Pts',(-3.25226405800006,2.2,-2.44850251900001));
#319212=CARTESIAN_POINT('Ctrl Pts',(-3.25138915700005,12.2,-2.44807896900001));
#319213=CARTESIAN_POINT('Ctrl Pts',(-3.25138915700005,5.2,-2.44807896900001));
#319214=CARTESIAN_POINT('Ctrl Pts',(-3.25138915700005,2.2,-2.44807896900001));
#319215=CARTESIAN_POINT('Ctrl Pts',(-3.25051976000006,12.2,-2.44765675600001));
#319216=CARTESIAN_POINT('Ctrl Pts',(-3.25051976000006,5.2,-2.44765675600001));
#319217=CARTESIAN_POINT('Ctrl Pts',(-3.25051976000006,2.2,-2.44765675600001));
#319218=CARTESIAN_POINT('Ctrl Pts',(-3.24965587200006,12.2,-2.44723589800001));
#319219=CARTESIAN_POINT('Ctrl Pts',(-3.24965587200006,5.2,-2.44723589800001));
#319220=CARTESIAN_POINT('Ctrl Pts',(-3.24965587200006,2.2,-2.44723589800001));
#319221=CARTESIAN_POINT('Ctrl Pts',(-3.24879749300006,12.2,-2.44681640900001));
#319222=CARTESIAN_POINT('Ctrl Pts',(-3.24879749300006,5.2,-2.44681640900001));
#319223=CARTESIAN_POINT('Ctrl Pts',(-3.24879749300006,2.2,-2.44681640900001));
#319224=CARTESIAN_POINT('Ctrl Pts',(-3.24794462900006,12.2,-2.44639830600001));
#319225=CARTESIAN_POINT('Ctrl Pts',(-3.24794462900006,5.2,-2.44639830600001));
#319226=CARTESIAN_POINT('Ctrl Pts',(-3.24794462900006,2.2,-2.44639830600001));
#319227=CARTESIAN_POINT('Ctrl Pts',(-3.24709728600005,12.2,-2.44598160600002));
#319228=CARTESIAN_POINT('Ctrl Pts',(-3.24709728600005,5.2,-2.44598160600002));
#319229=CARTESIAN_POINT('Ctrl Pts',(-3.24709728600005,2.2,-2.44598160600002));
#319230=CARTESIAN_POINT('Ctrl Pts',(-3.24625546600006,12.2,-2.44556632600001));
#319231=CARTESIAN_POINT('Ctrl Pts',(-3.24625546600006,5.2,-2.44556632600001));
#319232=CARTESIAN_POINT('Ctrl Pts',(-3.24625546600006,2.2,-2.44556632600001));
#319233=CARTESIAN_POINT('Ctrl Pts',(-3.24541917300006,12.2,-2.44515248200001));
#319234=CARTESIAN_POINT('Ctrl Pts',(-3.24541917300006,5.2,-2.44515248200001));
#319235=CARTESIAN_POINT('Ctrl Pts',(-3.24541917300006,2.2,-2.44515248200001));
#319236=CARTESIAN_POINT('Ctrl Pts',(-3.24458841200005,12.2,-2.44474009200002));
#319237=CARTESIAN_POINT('Ctrl Pts',(-3.24458841200005,5.2,-2.44474009200002));
#319238=CARTESIAN_POINT('Ctrl Pts',(-3.24458841200005,2.2,-2.44474009200002));
#319239=CARTESIAN_POINT('Ctrl Pts',(-3.24376318700006,12.2,-2.44432917200001));
#319240=CARTESIAN_POINT('Ctrl Pts',(-3.24376318700006,5.2,-2.44432917200001));
#319241=CARTESIAN_POINT('Ctrl Pts',(-3.24376318700006,2.2,-2.44432917200001));
#319242=CARTESIAN_POINT('Ctrl Pts',(-3.24294350100006,12.2,-2.44391973700001));
#319243=CARTESIAN_POINT('Ctrl Pts',(-3.24294350100006,5.2,-2.44391973700001));
#319244=CARTESIAN_POINT('Ctrl Pts',(-3.24294350100006,2.2,-2.44391973700001));
#319245=CARTESIAN_POINT('Ctrl Pts',(-3.24212935800006,12.2,-2.44351180700002));
#319246=CARTESIAN_POINT('Ctrl Pts',(-3.24212935800006,5.2,-2.44351180700002));
#319247=CARTESIAN_POINT('Ctrl Pts',(-3.24212935800006,2.2,-2.44351180700002));
#319248=CARTESIAN_POINT('Ctrl Pts',(-3.24132076300006,12.2,-2.44310539600002));
#319249=CARTESIAN_POINT('Ctrl Pts',(-3.24132076300006,5.2,-2.44310539600002));
#319250=CARTESIAN_POINT('Ctrl Pts',(-3.24132076300006,2.2,-2.44310539600002));
#319251=CARTESIAN_POINT('Ctrl Pts',(-3.24051771900006,12.2,-2.44270052300001));
#319252=CARTESIAN_POINT('Ctrl Pts',(-3.24051771900006,5.2,-2.44270052300001));
#319253=CARTESIAN_POINT('Ctrl Pts',(-3.24051771900006,2.2,-2.44270052300001));
#319254=CARTESIAN_POINT('Ctrl Pts',(-3.23972023100006,12.2,-2.44229720500002));
#319255=CARTESIAN_POINT('Ctrl Pts',(-3.23972023100006,5.2,-2.44229720500002));
#319256=CARTESIAN_POINT('Ctrl Pts',(-3.23972023100006,2.2,-2.44229720500002));
#319257=CARTESIAN_POINT('Ctrl Pts',(-3.23892830200006,12.2,-2.44189545800001));
#319258=CARTESIAN_POINT('Ctrl Pts',(-3.23892830200006,5.2,-2.44189545800001));
#319259=CARTESIAN_POINT('Ctrl Pts',(-3.23892830200006,2.2,-2.44189545800001));
#319260=CARTESIAN_POINT('Ctrl Pts',(-3.23814193600006,12.2,-2.44149529900001));
#319261=CARTESIAN_POINT('Ctrl Pts',(-3.23814193600006,5.2,-2.44149529900001));
#319262=CARTESIAN_POINT('Ctrl Pts',(-3.23814193600006,2.2,-2.44149529900001));
#319263=CARTESIAN_POINT('Ctrl Pts',(-3.23736113700006,12.2,-2.44109674600002));
#319264=CARTESIAN_POINT('Ctrl Pts',(-3.23736113700006,5.2,-2.44109674600002));
#319265=CARTESIAN_POINT('Ctrl Pts',(-3.23736113700006,2.2,-2.44109674600002));
#319266=CARTESIAN_POINT('Ctrl Pts',(-3.23658590900005,12.2,-2.44069981600001));
#319267=CARTESIAN_POINT('Ctrl Pts',(-3.23658590900005,5.2,-2.44069981600001));
#319268=CARTESIAN_POINT('Ctrl Pts',(-3.23658590900005,2.2,-2.44069981600001));
#319269=CARTESIAN_POINT('Ctrl Pts',(-3.23581625600006,12.2,-2.44030452700001));
#319270=CARTESIAN_POINT('Ctrl Pts',(-3.23581625600006,5.2,-2.44030452700001));
#319271=CARTESIAN_POINT('Ctrl Pts',(-3.23581625600006,2.2,-2.44030452700001));
#319272=CARTESIAN_POINT('Ctrl Pts',(-3.23505218300005,12.2,-2.43991089400001));
#319273=CARTESIAN_POINT('Ctrl Pts',(-3.23505218300005,5.2,-2.43991089400001));
#319274=CARTESIAN_POINT('Ctrl Pts',(-3.23505218300005,2.2,-2.43991089400001));
#319275=CARTESIAN_POINT('Ctrl Pts',(-3.23429369200006,12.2,-2.43951893700002));
#319276=CARTESIAN_POINT('Ctrl Pts',(-3.23429369200006,5.2,-2.43951893700002));
#319277=CARTESIAN_POINT('Ctrl Pts',(-3.23429369200006,2.2,-2.43951893700002));
#319278=CARTESIAN_POINT('Ctrl Pts',(-3.23354078700006,12.2,-2.43912867200001));
#319279=CARTESIAN_POINT('Ctrl Pts',(-3.23354078700006,5.2,-2.43912867200001));
#319280=CARTESIAN_POINT('Ctrl Pts',(-3.23354078700006,2.2,-2.43912867200001));
#319281=CARTESIAN_POINT('Ctrl Pts',(-3.23279347300006,12.2,-2.43874011600001));
#319282=CARTESIAN_POINT('Ctrl Pts',(-3.23279347300006,5.2,-2.43874011600001));
#319283=CARTESIAN_POINT('Ctrl Pts',(-3.23279347300006,2.2,-2.43874011600001));
#319284=CARTESIAN_POINT('Ctrl Pts',(-3.23205175300005,12.2,-2.43835328900001));
#319285=CARTESIAN_POINT('Ctrl Pts',(-3.23205175300005,5.2,-2.43835328900001));
#319286=CARTESIAN_POINT('Ctrl Pts',(-3.23205175300005,2.2,-2.43835328900001));
#319287=CARTESIAN_POINT('Ctrl Pts',(-3.23131563100006,12.2,-2.43796820600001));
#319288=CARTESIAN_POINT('Ctrl Pts',(-3.23131563100006,5.2,-2.43796820600001));
#319289=CARTESIAN_POINT('Ctrl Pts',(-3.23131563100006,2.2,-2.43796820600001));
#319290=CARTESIAN_POINT('Ctrl Pts',(-3.23058511200006,12.2,-2.43758488500001));
#319291=CARTESIAN_POINT('Ctrl Pts',(-3.23058511200006,5.2,-2.43758488500001));
#319292=CARTESIAN_POINT('Ctrl Pts',(-3.23058511200006,2.2,-2.43758488500001));
#319293=CARTESIAN_POINT('Ctrl Pts',(-3.22986019800005,12.2,-2.43720334500001));
#319294=CARTESIAN_POINT('Ctrl Pts',(-3.22986019800005,5.2,-2.43720334500001));
#319295=CARTESIAN_POINT('Ctrl Pts',(-3.22986019800005,2.2,-2.43720334500001));
#319296=CARTESIAN_POINT('Ctrl Pts',(-3.22914089300005,12.2,-2.43682360200001));
#319297=CARTESIAN_POINT('Ctrl Pts',(-3.22914089300005,5.2,-2.43682360200001));
#319298=CARTESIAN_POINT('Ctrl Pts',(-3.22914089300005,2.2,-2.43682360200001));
#319299=CARTESIAN_POINT('Ctrl Pts',(-3.22842720200006,12.2,-2.43644567500001));
#319300=CARTESIAN_POINT('Ctrl Pts',(-3.22842720200006,5.2,-2.43644567500001));
#319301=CARTESIAN_POINT('Ctrl Pts',(-3.22842720200006,2.2,-2.43644567500001));
#319302=CARTESIAN_POINT('Ctrl Pts',(-3.22771912700006,12.2,-2.43606958200001));
#319303=CARTESIAN_POINT('Ctrl Pts',(-3.22771912700006,5.2,-2.43606958200001));
#319304=CARTESIAN_POINT('Ctrl Pts',(-3.22771912700006,2.2,-2.43606958200001));
#319305=CARTESIAN_POINT('Ctrl Pts',(-3.22701667400006,12.2,-2.43569534000001));
#319306=CARTESIAN_POINT('Ctrl Pts',(-3.22701667400006,5.2,-2.43569534000001));
#319307=CARTESIAN_POINT('Ctrl Pts',(-3.22701667400006,2.2,-2.43569534000001));
#319308=CARTESIAN_POINT('Ctrl Pts',(-3.22631984500005,12.2,-2.43532296700002));
#319309=CARTESIAN_POINT('Ctrl Pts',(-3.22631984500005,5.2,-2.43532296700002));
#319310=CARTESIAN_POINT('Ctrl Pts',(-3.22631984500005,2.2,-2.43532296700002));
#319311=CARTESIAN_POINT('Ctrl Pts',(-3.22562864500005,12.2,-2.43495248300002));
#319312=CARTESIAN_POINT('Ctrl Pts',(-3.22562864500005,5.2,-2.43495248300002));
#319313=CARTESIAN_POINT('Ctrl Pts',(-3.22562864500005,2.2,-2.43495248300002));
#319314=CARTESIAN_POINT('Ctrl Pts',(-3.22494307600006,12.2,-2.43458390200002));
#319315=CARTESIAN_POINT('Ctrl Pts',(-3.22494307600006,5.2,-2.43458390200002));
#319316=CARTESIAN_POINT('Ctrl Pts',(-3.22494307600006,2.2,-2.43458390200002));
#319317=CARTESIAN_POINT('Ctrl Pts',(-3.22426314400006,12.2,-2.43421724700001));
#319318=CARTESIAN_POINT('Ctrl Pts',(-3.22426314400006,5.2,-2.43421724700001));
#319319=CARTESIAN_POINT('Ctrl Pts',(-3.22426314400006,2.2,-2.43421724700001));
#319320=CARTESIAN_POINT('Ctrl Pts',(-3.22358885100006,12.2,-2.43385253200001));
#319321=CARTESIAN_POINT('Ctrl Pts',(-3.22358885100006,5.2,-2.43385253200001));
#319322=CARTESIAN_POINT('Ctrl Pts',(-3.22358885100006,2.2,-2.43385253200001));
#319323=CARTESIAN_POINT('Ctrl Pts',(-3.22292020000006,12.2,-2.43348977700002));
#319324=CARTESIAN_POINT('Ctrl Pts',(-3.22292020000006,5.2,-2.43348977700002));
#319325=CARTESIAN_POINT('Ctrl Pts',(-3.22292020000006,2.2,-2.43348977700002));
#319326=CARTESIAN_POINT('Ctrl Pts',(-3.22225719700006,12.2,-2.43312900100001));
#319327=CARTESIAN_POINT('Ctrl Pts',(-3.22225719700006,5.2,-2.43312900100001));
#319328=CARTESIAN_POINT('Ctrl Pts',(-3.22225719700006,2.2,-2.43312900100001));
#319329=CARTESIAN_POINT('Ctrl Pts',(-3.22159984400006,12.2,-2.43277022100001));
#319330=CARTESIAN_POINT('Ctrl Pts',(-3.22159984400006,5.2,-2.43277022100001));
#319331=CARTESIAN_POINT('Ctrl Pts',(-3.22159984400006,2.2,-2.43277022100001));
#319332=CARTESIAN_POINT('Ctrl Pts',(-3.22094814500006,12.2,-2.43241345700001));
#319333=CARTESIAN_POINT('Ctrl Pts',(-3.22094814500006,5.2,-2.43241345700001));
#319334=CARTESIAN_POINT('Ctrl Pts',(-3.22094814500006,2.2,-2.43241345700001));
#319335=CARTESIAN_POINT('Ctrl Pts',(-3.22030210500006,12.2,-2.43205872500001));
#319336=CARTESIAN_POINT('Ctrl Pts',(-3.22030210500006,5.2,-2.43205872500001));
#319337=CARTESIAN_POINT('Ctrl Pts',(-3.22030210500006,2.2,-2.43205872500001));
#319338=CARTESIAN_POINT('Ctrl Pts',(-3.21966172400006,12.2,-2.43170604600001));
#319339=CARTESIAN_POINT('Ctrl Pts',(-3.21966172400006,5.2,-2.43170604600001));
#319340=CARTESIAN_POINT('Ctrl Pts',(-3.21966172400006,2.2,-2.43170604600001));
#319341=CARTESIAN_POINT('Ctrl Pts',(-3.21902701000006,12.2,-2.43135543600001));
#319342=CARTESIAN_POINT('Ctrl Pts',(-3.21902701000006,5.2,-2.43135543600001));
#319343=CARTESIAN_POINT('Ctrl Pts',(-3.21902701000006,2.2,-2.43135543600001));
#319344=CARTESIAN_POINT('Ctrl Pts',(-3.21839796500006,12.2,-2.43100691700001));
#319345=CARTESIAN_POINT('Ctrl Pts',(-3.21839796500006,5.2,-2.43100691700001));
#319346=CARTESIAN_POINT('Ctrl Pts',(-3.21839796500006,2.2,-2.43100691700001));
#319347=CARTESIAN_POINT('Ctrl Pts',(-3.21777459100006,12.2,-2.43066050400001));
#319348=CARTESIAN_POINT('Ctrl Pts',(-3.21777459100006,5.2,-2.43066050400001));
#319349=CARTESIAN_POINT('Ctrl Pts',(-3.21777459100006,2.2,-2.43066050400001));
#319350=CARTESIAN_POINT('Ctrl Pts',(-3.21715689300006,12.2,-2.43031621800001));
#319351=CARTESIAN_POINT('Ctrl Pts',(-3.21715689300006,5.2,-2.43031621800001));
#319352=CARTESIAN_POINT('Ctrl Pts',(-3.21715689300006,2.2,-2.43031621800001));
#319353=CARTESIAN_POINT('Ctrl Pts',(-3.21654487500005,12.2,-2.42997407700001));
#319354=CARTESIAN_POINT('Ctrl Pts',(-3.21654487500005,5.2,-2.42997407700001));
#319355=CARTESIAN_POINT('Ctrl Pts',(-3.21654487500005,2.2,-2.42997407700001));
#319356=CARTESIAN_POINT('Ctrl Pts',(-3.21593853800006,12.2,-2.42963410000002));
#319357=CARTESIAN_POINT('Ctrl Pts',(-3.21593853800006,5.2,-2.42963410000002));
#319358=CARTESIAN_POINT('Ctrl Pts',(-3.21593853800006,2.2,-2.42963410000002));
#319359=CARTESIAN_POINT('Ctrl Pts',(-3.21533788800005,12.2,-2.42929630700001));
#319360=CARTESIAN_POINT('Ctrl Pts',(-3.21533788800005,5.2,-2.42929630700001));
#319361=CARTESIAN_POINT('Ctrl Pts',(-3.21533788800005,2.2,-2.42929630700001));
#319362=CARTESIAN_POINT('Ctrl Pts',(-3.21474292900006,12.2,-2.42896071500001));
#319363=CARTESIAN_POINT('Ctrl Pts',(-3.21474292900006,5.2,-2.42896071500001));
#319364=CARTESIAN_POINT('Ctrl Pts',(-3.21474292900006,2.2,-2.42896071500001));
#319365=CARTESIAN_POINT('Ctrl Pts',(-3.21415366400006,12.2,-2.42862734300001));
#319366=CARTESIAN_POINT('Ctrl Pts',(-3.21415366400006,5.2,-2.42862734300001));
#319367=CARTESIAN_POINT('Ctrl Pts',(-3.21415366400006,2.2,-2.42862734300001));
#319368=CARTESIAN_POINT('Ctrl Pts',(-3.21357009500006,12.2,-2.42829621200002));
#319369=CARTESIAN_POINT('Ctrl Pts',(-3.21357009500006,5.2,-2.42829621200002));
#319370=CARTESIAN_POINT('Ctrl Pts',(-3.21357009500006,2.2,-2.42829621200002));
#319371=CARTESIAN_POINT('Ctrl Pts',(-3.21299222700006,12.2,-2.42796734200001));
#319372=CARTESIAN_POINT('Ctrl Pts',(-3.21299222700006,5.2,-2.42796734200001));
#319373=CARTESIAN_POINT('Ctrl Pts',(-3.21299222700006,2.2,-2.42796734200001));
#319374=CARTESIAN_POINT('Ctrl Pts',(-3.21242006200006,12.2,-2.42764074800002));
#319375=CARTESIAN_POINT('Ctrl Pts',(-3.21242006200006,5.2,-2.42764074800002));
#319376=CARTESIAN_POINT('Ctrl Pts',(-3.21242006200006,2.2,-2.42764074800002));
#319377=CARTESIAN_POINT('Ctrl Pts',(-3.21185360400006,12.2,-2.42731645200001));
#319378=CARTESIAN_POINT('Ctrl Pts',(-3.21185360400006,5.2,-2.42731645200001));
#319379=CARTESIAN_POINT('Ctrl Pts',(-3.21185360400006,2.2,-2.42731645200001));
#319380=CARTESIAN_POINT('Ctrl Pts',(-3.21129285900006,12.2,-2.42699447300001));
#319381=CARTESIAN_POINT('Ctrl Pts',(-3.21129285900006,5.2,-2.42699447300001));
#319382=CARTESIAN_POINT('Ctrl Pts',(-3.21129285900006,2.2,-2.42699447300001));
#319383=CARTESIAN_POINT('Ctrl Pts',(-3.21073782700006,12.2,-2.42667483200002));
#319384=CARTESIAN_POINT('Ctrl Pts',(-3.21073782700006,5.2,-2.42667483200002));
#319385=CARTESIAN_POINT('Ctrl Pts',(-3.21073782700006,2.2,-2.42667483200002));
#319386=CARTESIAN_POINT('Ctrl Pts',(-3.21018851300006,12.2,-2.42635754500002));
#319387=CARTESIAN_POINT('Ctrl Pts',(-3.21018851300006,5.2,-2.42635754500002));
#319388=CARTESIAN_POINT('Ctrl Pts',(-3.21018851300006,2.2,-2.42635754500002));
#319389=CARTESIAN_POINT('Ctrl Pts',(-3.20964491900006,12.2,-2.42604263400001));
#319390=CARTESIAN_POINT('Ctrl Pts',(-3.20964491900006,5.2,-2.42604263400001));
#319391=CARTESIAN_POINT('Ctrl Pts',(-3.20964491900006,2.2,-2.42604263400001));
#319392=CARTESIAN_POINT('Ctrl Pts',(-3.20910705000006,12.2,-2.42573011800001));
#319393=CARTESIAN_POINT('Ctrl Pts',(-3.20910705000006,5.2,-2.42573011800001));
#319394=CARTESIAN_POINT('Ctrl Pts',(-3.20910705000006,2.2,-2.42573011800001));
#319395=CARTESIAN_POINT('Ctrl Pts',(-3.20857491000006,12.2,-2.42542001600001));
#319396=CARTESIAN_POINT('Ctrl Pts',(-3.20857491000006,5.2,-2.42542001600001));
#319397=CARTESIAN_POINT('Ctrl Pts',(-3.20857491000006,2.2,-2.42542001600001));
#319398=CARTESIAN_POINT('Ctrl Pts',(-3.20804850000005,12.2,-2.42511234900002));
#319399=CARTESIAN_POINT('Ctrl Pts',(-3.20804850000005,5.2,-2.42511234900002));
#319400=CARTESIAN_POINT('Ctrl Pts',(-3.20804850000005,2.2,-2.42511234900002));
#319401=CARTESIAN_POINT('Ctrl Pts',(-3.20752782500006,12.2,-2.42480713400001));
#319402=CARTESIAN_POINT('Ctrl Pts',(-3.20752782500006,5.2,-2.42480713400001));
#319403=CARTESIAN_POINT('Ctrl Pts',(-3.20752782500006,2.2,-2.42480713400001));
#319404=CARTESIAN_POINT('Ctrl Pts',(-3.20701288800006,12.2,-2.42450439400002));
#319405=CARTESIAN_POINT('Ctrl Pts',(-3.20701288800006,5.2,-2.42450439400002));
#319406=CARTESIAN_POINT('Ctrl Pts',(-3.20701288800006,2.2,-2.42450439400002));
#319407=CARTESIAN_POINT('Ctrl Pts',(-3.20650369300005,12.2,-2.42420414800002));
#319408=CARTESIAN_POINT('Ctrl Pts',(-3.20650369300005,5.2,-2.42420414800002));
#319409=CARTESIAN_POINT('Ctrl Pts',(-3.20650369300005,2.2,-2.42420414800002));
#319410=CARTESIAN_POINT('Ctrl Pts',(-3.20600024200006,12.2,-2.42390641500001));
#319411=CARTESIAN_POINT('Ctrl Pts',(-3.20600024200006,5.2,-2.42390641500001));
#319412=CARTESIAN_POINT('Ctrl Pts',(-3.20600024200006,2.2,-2.42390641500001));
#319413=CARTESIAN_POINT('Ctrl Pts',(-3.20550253900006,12.2,-2.42361121600001));
#319414=CARTESIAN_POINT('Ctrl Pts',(-3.20550253900006,5.2,-2.42361121600001));
#319415=CARTESIAN_POINT('Ctrl Pts',(-3.20550253900006,2.2,-2.42361121600001));
#319416=CARTESIAN_POINT('Ctrl Pts',(-3.20501058600006,12.2,-2.42331857100002));
#319417=CARTESIAN_POINT('Ctrl Pts',(-3.20501058600006,5.2,-2.42331857100002));
#319418=CARTESIAN_POINT('Ctrl Pts',(-3.20501058600006,2.2,-2.42331857100002));
#319419=CARTESIAN_POINT('Ctrl Pts',(-3.20452438900006,12.2,-2.42302849900002));
#319420=CARTESIAN_POINT('Ctrl Pts',(-3.20452438900006,5.2,-2.42302849900002));
#319421=CARTESIAN_POINT('Ctrl Pts',(-3.20452438900006,2.2,-2.42302849900002));
#319422=CARTESIAN_POINT('Ctrl Pts',(-3.20404394900006,12.2,-2.42274102200001));
#319423=CARTESIAN_POINT('Ctrl Pts',(-3.20404394900006,5.2,-2.42274102200001));
#319424=CARTESIAN_POINT('Ctrl Pts',(-3.20404394900006,2.2,-2.42274102200001));
#319425=CARTESIAN_POINT('Ctrl Pts',(-3.20356926900006,12.2,-2.42245615800002));
#319426=CARTESIAN_POINT('Ctrl Pts',(-3.20356926900006,5.2,-2.42245615800002));
#319427=CARTESIAN_POINT('Ctrl Pts',(-3.20356926900006,2.2,-2.42245615800002));
#319428=CARTESIAN_POINT('Ctrl Pts',(-3.20310035500006,12.2,-2.42217393000002));
#319429=CARTESIAN_POINT('Ctrl Pts',(-3.20310035500006,5.2,-2.42217393000002));
#319430=CARTESIAN_POINT('Ctrl Pts',(-3.20310035500006,2.2,-2.42217393000002));
#319431=CARTESIAN_POINT('Ctrl Pts',(-3.20263720800006,12.2,-2.42189435600002));
#319432=CARTESIAN_POINT('Ctrl Pts',(-3.20263720800006,5.2,-2.42189435600002));
#319433=CARTESIAN_POINT('Ctrl Pts',(-3.20263720800006,2.2,-2.42189435600002));
#319434=CARTESIAN_POINT('Ctrl Pts',(-3.20217983100005,12.2,-2.42161745700002));
#319435=CARTESIAN_POINT('Ctrl Pts',(-3.20217983100005,5.2,-2.42161745700002));
#319436=CARTESIAN_POINT('Ctrl Pts',(-3.20217983100005,2.2,-2.42161745700002));
#319437=CARTESIAN_POINT('Ctrl Pts',(-3.20172822800005,12.2,-2.42134325500002));
#319438=CARTESIAN_POINT('Ctrl Pts',(-3.20172822800005,5.2,-2.42134325500002));
#319439=CARTESIAN_POINT('Ctrl Pts',(-3.20172822800005,2.2,-2.42134325500002));
#319440=CARTESIAN_POINT('Ctrl Pts',(-3.20128240200006,12.2,-2.42107177000001));
#319441=CARTESIAN_POINT('Ctrl Pts',(-3.20128240200006,5.2,-2.42107177000001));
#319442=CARTESIAN_POINT('Ctrl Pts',(-3.20128240200006,2.2,-2.42107177000001));
#319443=CARTESIAN_POINT('Ctrl Pts',(-3.20084235600006,12.2,-2.42080302100002));
#319444=CARTESIAN_POINT('Ctrl Pts',(-3.20084235600006,5.2,-2.42080302100002));
#319445=CARTESIAN_POINT('Ctrl Pts',(-3.20084235600006,2.2,-2.42080302100002));
#319446=CARTESIAN_POINT('Ctrl Pts',(-3.20040809300006,12.2,-2.42053703100002));
#319447=CARTESIAN_POINT('Ctrl Pts',(-3.20040809300006,5.2,-2.42053703100002));
#319448=CARTESIAN_POINT('Ctrl Pts',(-3.20040809300006,2.2,-2.42053703100002));
#319449=CARTESIAN_POINT('Ctrl Pts',(-3.19997961700006,12.2,-2.42027381900002));
#319450=CARTESIAN_POINT('Ctrl Pts',(-3.19997961700006,5.2,-2.42027381900002));
#319451=CARTESIAN_POINT('Ctrl Pts',(-3.19997961700006,2.2,-2.42027381900002));
#319452=CARTESIAN_POINT('Ctrl Pts',(-3.19955693100006,12.2,-2.42001340800002));
#319453=CARTESIAN_POINT('Ctrl Pts',(-3.19955693100006,5.2,-2.42001340800002));
#319454=CARTESIAN_POINT('Ctrl Pts',(-3.19955693100006,2.2,-2.42001340800002));
#319455=CARTESIAN_POINT('Ctrl Pts',(-3.19914003600006,12.2,-2.41975581600002));
#319456=CARTESIAN_POINT('Ctrl Pts',(-3.19914003600006,5.2,-2.41975581600002));
#319457=CARTESIAN_POINT('Ctrl Pts',(-3.19914003600006,2.2,-2.41975581600002));
#319458=CARTESIAN_POINT('Ctrl Pts',(-3.19872893800006,12.2,-2.41950106700001));
#319459=CARTESIAN_POINT('Ctrl Pts',(-3.19872893800006,5.2,-2.41950106700001));
#319460=CARTESIAN_POINT('Ctrl Pts',(-3.19872893800006,2.2,-2.41950106700001));
#319461=CARTESIAN_POINT('Ctrl Pts',(-3.19832363800006,12.2,-2.41924917900001));
#319462=CARTESIAN_POINT('Ctrl Pts',(-3.19832363800006,5.2,-2.41924917900001));
#319463=CARTESIAN_POINT('Ctrl Pts',(-3.19832363800006,2.2,-2.41924917900001));
#319464=CARTESIAN_POINT('Ctrl Pts',(-3.19792414100006,12.2,-2.41900017700001));
#319465=CARTESIAN_POINT('Ctrl Pts',(-3.19792414100006,5.2,-2.41900017700001));
#319466=CARTESIAN_POINT('Ctrl Pts',(-3.19792414100006,2.2,-2.41900017700001));
#319467=CARTESIAN_POINT('Ctrl Pts',(-3.19753044800006,12.2,-2.41875407900002));
#319468=CARTESIAN_POINT('Ctrl Pts',(-3.19753044800006,5.2,-2.41875407900002));
#319469=CARTESIAN_POINT('Ctrl Pts',(-3.19753044800006,2.2,-2.41875407900002));
#319470=CARTESIAN_POINT('Ctrl Pts',(-3.19714256200006,12.2,-2.41851090700001));
#319471=CARTESIAN_POINT('Ctrl Pts',(-3.19714256200006,5.2,-2.41851090700001));
#319472=CARTESIAN_POINT('Ctrl Pts',(-3.19714256200006,2.2,-2.41851090700001));
#319473=CARTESIAN_POINT('Ctrl Pts',(-3.19676048800006,12.2,-2.41827068400001));
#319474=CARTESIAN_POINT('Ctrl Pts',(-3.19676048800006,5.2,-2.41827068400001));
#319475=CARTESIAN_POINT('Ctrl Pts',(-3.19676048800006,2.2,-2.41827068400001));
#319476=CARTESIAN_POINT('Ctrl Pts',(-3.19638422800006,12.2,-2.41803342900001));
#319477=CARTESIAN_POINT('Ctrl Pts',(-3.19638422800006,5.2,-2.41803342900001));
#319478=CARTESIAN_POINT('Ctrl Pts',(-3.19638422800006,2.2,-2.41803342900001));
#319479=CARTESIAN_POINT('Ctrl Pts',(-3.19601378400006,12.2,-2.41779916600001));
#319480=CARTESIAN_POINT('Ctrl Pts',(-3.19601378400006,5.2,-2.41779916600001));
#319481=CARTESIAN_POINT('Ctrl Pts',(-3.19601378400006,2.2,-2.41779916600001));
#319482=CARTESIAN_POINT('Ctrl Pts',(-3.19564916000005,12.2,-2.41756791400002));
#319483=CARTESIAN_POINT('Ctrl Pts',(-3.19564916000005,5.2,-2.41756791400002));
#319484=CARTESIAN_POINT('Ctrl Pts',(-3.19564916000005,2.2,-2.41756791400002));
#319485=CARTESIAN_POINT('Ctrl Pts',(-3.19529036000006,12.2,-2.41733969700002));
#319486=CARTESIAN_POINT('Ctrl Pts',(-3.19529036000006,5.2,-2.41733969700002));
#319487=CARTESIAN_POINT('Ctrl Pts',(-3.19529036000006,2.2,-2.41733969700002));
#319488=CARTESIAN_POINT('Ctrl Pts',(-3.19493738400006,12.2,-2.41711453400002));
#319489=CARTESIAN_POINT('Ctrl Pts',(-3.19493738400006,5.2,-2.41711453400002));
#319490=CARTESIAN_POINT('Ctrl Pts',(-3.19493738400006,2.2,-2.41711453400002));
#319491=CARTESIAN_POINT('Ctrl Pts',(-3.19459023800006,12.2,-2.41689245000002));
#319492=CARTESIAN_POINT('Ctrl Pts',(-3.19459023800006,5.2,-2.41689245000002));
#319493=CARTESIAN_POINT('Ctrl Pts',(-3.19459023800006,2.2,-2.41689245000002));
#319494=CARTESIAN_POINT('Ctrl Pts',(-3.19424892300006,12.2,-2.41667346500002));
#319495=CARTESIAN_POINT('Ctrl Pts',(-3.19424892300006,5.2,-2.41667346500002));
#319496=CARTESIAN_POINT('Ctrl Pts',(-3.19424892300006,2.2,-2.41667346500002));
#319497=CARTESIAN_POINT('Ctrl Pts',(-3.19391344200006,12.2,-2.41645760200001));
#319498=CARTESIAN_POINT('Ctrl Pts',(-3.19391344200006,5.2,-2.41645760200001));
#319499=CARTESIAN_POINT('Ctrl Pts',(-3.19391344200006,2.2,-2.41645760200001));
#319500=CARTESIAN_POINT('Ctrl Pts',(-3.19358379900006,12.2,-2.41624488100001));
#319501=CARTESIAN_POINT('Ctrl Pts',(-3.19358379900006,5.2,-2.41624488100001));
#319502=CARTESIAN_POINT('Ctrl Pts',(-3.19358379900006,2.2,-2.41624488100001));
#319503=CARTESIAN_POINT('Ctrl Pts',(-3.19325999500006,12.2,-2.41603532600001));
#319504=CARTESIAN_POINT('Ctrl Pts',(-3.19325999500006,5.2,-2.41603532600001));
#319505=CARTESIAN_POINT('Ctrl Pts',(-3.19325999500006,2.2,-2.41603532600001));
#319506=CARTESIAN_POINT('Ctrl Pts',(-3.19294203600006,12.2,-2.41582895800001));
#319507=CARTESIAN_POINT('Ctrl Pts',(-3.19294203600006,5.2,-2.41582895800001));
#319508=CARTESIAN_POINT('Ctrl Pts',(-3.19294203600006,2.2,-2.41582895800001));
#319509=CARTESIAN_POINT('Ctrl Pts',(-3.19262992100006,12.2,-2.41562580100001));
#319510=CARTESIAN_POINT('Ctrl Pts',(-3.19262992100006,5.2,-2.41562580100001));
#319511=CARTESIAN_POINT('Ctrl Pts',(-3.19262992100006,2.2,-2.41562580100001));
#319512=CARTESIAN_POINT('Ctrl Pts',(-3.19232365500006,12.2,-2.41542587600001));
#319513=CARTESIAN_POINT('Ctrl Pts',(-3.19232365500006,5.2,-2.41542587600001));
#319514=CARTESIAN_POINT('Ctrl Pts',(-3.19232365500006,2.2,-2.41542587600001));
#319515=CARTESIAN_POINT('Ctrl Pts',(-3.19202324000006,12.2,-2.41522920400001));
#319516=CARTESIAN_POINT('Ctrl Pts',(-3.19202324000006,5.2,-2.41522920400001));
#319517=CARTESIAN_POINT('Ctrl Pts',(-3.19202324000006,2.2,-2.41522920400001));
#319518=CARTESIAN_POINT('Ctrl Pts',(-3.19172868100006,12.2,-2.41503581100002));
#319519=CARTESIAN_POINT('Ctrl Pts',(-3.19172868100006,5.2,-2.41503581100002));
#319520=CARTESIAN_POINT('Ctrl Pts',(-3.19172868100006,2.2,-2.41503581100002));
#319521=CARTESIAN_POINT('Ctrl Pts',(-3.19143997700006,12.2,-2.41484571600001));
#319522=CARTESIAN_POINT('Ctrl Pts',(-3.19143997700006,5.2,-2.41484571600001));
#319523=CARTESIAN_POINT('Ctrl Pts',(-3.19143997700006,2.2,-2.41484571600001));
#319524=CARTESIAN_POINT('Ctrl Pts',(-3.19115713300006,12.2,-2.41465894400001));
#319525=CARTESIAN_POINT('Ctrl Pts',(-3.19115713300006,5.2,-2.41465894400001));
#319526=CARTESIAN_POINT('Ctrl Pts',(-3.19115713300006,2.2,-2.41465894400001));
#319527=CARTESIAN_POINT('Ctrl Pts',(-3.19088015200006,12.2,-2.41447551700002));
#319528=CARTESIAN_POINT('Ctrl Pts',(-3.19088015200006,5.2,-2.41447551700002));
#319529=CARTESIAN_POINT('Ctrl Pts',(-3.19088015200006,2.2,-2.41447551700002));
#319530=CARTESIAN_POINT('Ctrl Pts',(-3.19060903600006,12.2,-2.41429545800001));
#319531=CARTESIAN_POINT('Ctrl Pts',(-3.19060903600006,5.2,-2.41429545800001));
#319532=CARTESIAN_POINT('Ctrl Pts',(-3.19060903600006,2.2,-2.41429545800001));
#319533=CARTESIAN_POINT('Ctrl Pts',(-3.19034378700006,12.2,-2.41411878900001));
#319534=CARTESIAN_POINT('Ctrl Pts',(-3.19034378700006,5.2,-2.41411878900001));
#319535=CARTESIAN_POINT('Ctrl Pts',(-3.19034378700006,2.2,-2.41411878900001));
#319536=CARTESIAN_POINT('Ctrl Pts',(-3.19008441000005,12.2,-2.41394553400001));
#319537=CARTESIAN_POINT('Ctrl Pts',(-3.19008441000005,5.2,-2.41394553400001));
#319538=CARTESIAN_POINT('Ctrl Pts',(-3.19008441000005,2.2,-2.41394553400001));
#319539=CARTESIAN_POINT('Ctrl Pts',(-3.18983090500006,12.2,-2.41377571600002));
#319540=CARTESIAN_POINT('Ctrl Pts',(-3.18983090500006,5.2,-2.41377571600002));
#319541=CARTESIAN_POINT('Ctrl Pts',(-3.18983090500006,2.2,-2.41377571600002));
#319542=CARTESIAN_POINT('Ctrl Pts',(-3.18958327600006,12.2,-2.41360935700001));
#319543=CARTESIAN_POINT('Ctrl Pts',(-3.18958327600006,5.2,-2.41360935700001));
#319544=CARTESIAN_POINT('Ctrl Pts',(-3.18958327600006,2.2,-2.41360935700001));
#319545=CARTESIAN_POINT('Ctrl Pts',(-3.18934152500006,12.2,-2.41344648100001));
#319546=CARTESIAN_POINT('Ctrl Pts',(-3.18934152500006,5.2,-2.41344648100001));
#319547=CARTESIAN_POINT('Ctrl Pts',(-3.18934152500006,2.2,-2.41344648100001));
#319548=CARTESIAN_POINT('Ctrl Pts',(-3.18910565500006,12.2,-2.41328711200001));
#319549=CARTESIAN_POINT('Ctrl Pts',(-3.18910565500006,5.2,-2.41328711200001));
#319550=CARTESIAN_POINT('Ctrl Pts',(-3.18910565500006,2.2,-2.41328711200001));
#319551=CARTESIAN_POINT('Ctrl Pts',(-3.18887567000006,12.2,-2.41313127200002));
#319552=CARTESIAN_POINT('Ctrl Pts',(-3.18887567000006,5.2,-2.41313127200002));
#319553=CARTESIAN_POINT('Ctrl Pts',(-3.18887567000006,2.2,-2.41313127200002));
#319554=CARTESIAN_POINT('Ctrl Pts',(-3.18865157000006,12.2,-2.41297898500001));
#319555=CARTESIAN_POINT('Ctrl Pts',(-3.18865157000006,5.2,-2.41297898500001));
#319556=CARTESIAN_POINT('Ctrl Pts',(-3.18865157000006,2.2,-2.41297898500001));
#319557=CARTESIAN_POINT('Ctrl Pts',(-3.18843335800006,12.2,-2.41283027500002));
#319558=CARTESIAN_POINT('Ctrl Pts',(-3.18843335800006,5.2,-2.41283027500002));
#319559=CARTESIAN_POINT('Ctrl Pts',(-3.18843335800006,2.2,-2.41283027500002));
#319560=CARTESIAN_POINT('Ctrl Pts',(-3.18822103800006,12.2,-2.41268516500002));
#319561=CARTESIAN_POINT('Ctrl Pts',(-3.18822103800006,5.2,-2.41268516500002));
#319562=CARTESIAN_POINT('Ctrl Pts',(-3.18822103800006,2.2,-2.41268516500002));
#319563=CARTESIAN_POINT('Ctrl Pts',(-3.18801461200006,12.2,-2.41254367900002));
#319564=CARTESIAN_POINT('Ctrl Pts',(-3.18801461200006,5.2,-2.41254367900002));
#319565=CARTESIAN_POINT('Ctrl Pts',(-3.18801461200006,2.2,-2.41254367900002));
#319566=CARTESIAN_POINT('Ctrl Pts',(-3.18781408200006,12.2,-2.41240584100002));
#319567=CARTESIAN_POINT('Ctrl Pts',(-3.18781408200006,5.2,-2.41240584100002));
#319568=CARTESIAN_POINT('Ctrl Pts',(-3.18781408200006,2.2,-2.41240584100002));
#319569=CARTESIAN_POINT('Ctrl Pts',(-3.18761945100006,12.2,-2.41227167400002));
#319570=CARTESIAN_POINT('Ctrl Pts',(-3.18761945100006,5.2,-2.41227167400002));
#319571=CARTESIAN_POINT('Ctrl Pts',(-3.18761945100006,2.2,-2.41227167400002));
#319572=CARTESIAN_POINT('Ctrl Pts',(-3.18743072200005,12.2,-2.41214120200001));
#319573=CARTESIAN_POINT('Ctrl Pts',(-3.18743072200005,5.2,-2.41214120200001));
#319574=CARTESIAN_POINT('Ctrl Pts',(-3.18743072200005,2.2,-2.41214120200001));
#319575=CARTESIAN_POINT('Ctrl Pts',(-3.18724789400005,12.2,-2.41201445000002));
#319576=CARTESIAN_POINT('Ctrl Pts',(-3.18724789400005,5.2,-2.41201445000002));
#319577=CARTESIAN_POINT('Ctrl Pts',(-3.18724789400005,2.2,-2.41201445000002));
#319578=CARTESIAN_POINT('Ctrl Pts',(-3.18707097400006,12.2,-2.41189144200002));
#319579=CARTESIAN_POINT('Ctrl Pts',(-3.18707097400006,5.2,-2.41189144200002));
#319580=CARTESIAN_POINT('Ctrl Pts',(-3.18707097400006,2.2,-2.41189144200002));
#319581=CARTESIAN_POINT('Ctrl Pts',(-3.18689996300006,12.2,-2.41177220100001));
#319582=CARTESIAN_POINT('Ctrl Pts',(-3.18689996300006,5.2,-2.41177220100001));
#319583=CARTESIAN_POINT('Ctrl Pts',(-3.18689996300006,2.2,-2.41177220100001));
#319584=CARTESIAN_POINT('Ctrl Pts',(-3.18673486200006,12.2,-2.41165675300001));
#319585=CARTESIAN_POINT('Ctrl Pts',(-3.18673486200006,5.2,-2.41165675300001));
#319586=CARTESIAN_POINT('Ctrl Pts',(-3.18673486200006,2.2,-2.41165675300001));
#319587=CARTESIAN_POINT('Ctrl Pts',(-3.18657567500006,12.2,-2.41154512200001));
#319588=CARTESIAN_POINT('Ctrl Pts',(-3.18657567500006,5.2,-2.41154512200001));
#319589=CARTESIAN_POINT('Ctrl Pts',(-3.18657567500006,2.2,-2.41154512200001));
#319590=CARTESIAN_POINT('Ctrl Pts',(-3.18642240300006,12.2,-2.41143733200001));
#319591=CARTESIAN_POINT('Ctrl Pts',(-3.18642240300006,5.2,-2.41143733200001));
#319592=CARTESIAN_POINT('Ctrl Pts',(-3.18642240300006,2.2,-2.41143733200001));
#319593=CARTESIAN_POINT('Ctrl Pts',(-3.18627504900005,12.2,-2.41133340900001));
#319594=CARTESIAN_POINT('Ctrl Pts',(-3.18627504900005,5.2,-2.41133340900001));
#319595=CARTESIAN_POINT('Ctrl Pts',(-3.18627504900005,2.2,-2.41133340900001));
#319596=CARTESIAN_POINT('Ctrl Pts',(-3.18613361600006,12.2,-2.41123337500001));
#319597=CARTESIAN_POINT('Ctrl Pts',(-3.18613361600006,5.2,-2.41123337500001));
#319598=CARTESIAN_POINT('Ctrl Pts',(-3.18613361600006,2.2,-2.41123337500001));
#319599=CARTESIAN_POINT('Ctrl Pts',(-3.18599810500006,12.2,-2.41113725500002));
#319600=CARTESIAN_POINT('Ctrl Pts',(-3.18599810500006,5.2,-2.41113725500002));
#319601=CARTESIAN_POINT('Ctrl Pts',(-3.18599810500006,2.2,-2.41113725500002));
#319602=CARTESIAN_POINT('Ctrl Pts',(-3.18586851800006,12.2,-2.41104507300001));
#319603=CARTESIAN_POINT('Ctrl Pts',(-3.18586851800006,5.2,-2.41104507300001));
#319604=CARTESIAN_POINT('Ctrl Pts',(-3.18586851800006,2.2,-2.41104507300001));
#319605=CARTESIAN_POINT('Ctrl Pts',(-3.18574485900006,12.2,-2.41095685700001));
#319606=CARTESIAN_POINT('Ctrl Pts',(-3.18574485900006,5.2,-2.41095685700001));
#319607=CARTESIAN_POINT('Ctrl Pts',(-3.18574485900006,2.2,-2.41095685700001));
#319608=CARTESIAN_POINT('Ctrl Pts',(-3.18562713000006,12.2,-2.41087263100002));
#319609=CARTESIAN_POINT('Ctrl Pts',(-3.18562713000006,5.2,-2.41087263100002));
#319610=CARTESIAN_POINT('Ctrl Pts',(-3.18562713000006,2.2,-2.41087263100002));
#319611=CARTESIAN_POINT('Ctrl Pts',(-3.18551533200006,12.2,-2.41079242200001));
#319612=CARTESIAN_POINT('Ctrl Pts',(-3.18551533200006,5.2,-2.41079242200001));
#319613=CARTESIAN_POINT('Ctrl Pts',(-3.18551533200006,2.2,-2.41079242200001));
#319614=CARTESIAN_POINT('Ctrl Pts',(-3.18540946800006,12.2,-2.41071625600001));
#319615=CARTESIAN_POINT('Ctrl Pts',(-3.18540946800006,5.2,-2.41071625600001));
#319616=CARTESIAN_POINT('Ctrl Pts',(-3.18540946800006,2.2,-2.41071625600001));
#319617=CARTESIAN_POINT('Ctrl Pts',(-3.18530953900006,12.2,-2.41064415700002));
#319618=CARTESIAN_POINT('Ctrl Pts',(-3.18530953900006,5.2,-2.41064415700002));
#319619=CARTESIAN_POINT('Ctrl Pts',(-3.18530953900006,2.2,-2.41064415700002));
#319620=CARTESIAN_POINT('Ctrl Pts',(-3.18521554900005,12.2,-2.41057614800001));
#319621=CARTESIAN_POINT('Ctrl Pts',(-3.18521554900005,5.2,-2.41057614800001));
#319622=CARTESIAN_POINT('Ctrl Pts',(-3.18521554900005,2.2,-2.41057614800001));
#319623=CARTESIAN_POINT('Ctrl Pts',(-3.18512750000005,12.2,-2.41051225300001));
#319624=CARTESIAN_POINT('Ctrl Pts',(-3.18512750000005,5.2,-2.41051225300001));
#319625=CARTESIAN_POINT('Ctrl Pts',(-3.18512750000005,2.2,-2.41051225300001));
#319626=CARTESIAN_POINT('Ctrl Pts',(-3.18504539300006,12.2,-2.41045249400001));
#319627=CARTESIAN_POINT('Ctrl Pts',(-3.18504539300006,5.2,-2.41045249400001));
#319628=CARTESIAN_POINT('Ctrl Pts',(-3.18504539300006,2.2,-2.41045249400001));
#319629=CARTESIAN_POINT('Ctrl Pts',(-3.18496922900006,12.2,-2.41039689700001));
#319630=CARTESIAN_POINT('Ctrl Pts',(-3.18496922900006,5.2,-2.41039689700001));
#319631=CARTESIAN_POINT('Ctrl Pts',(-3.18496922900006,2.2,-2.41039689700001));
#319632=CARTESIAN_POINT('Ctrl Pts',(-3.18489901200006,12.2,-2.41034549400001));
#319633=CARTESIAN_POINT('Ctrl Pts',(-3.18489901200006,5.2,-2.41034549400001));
#319634=CARTESIAN_POINT('Ctrl Pts',(-3.18489901200006,2.2,-2.41034549400001));
#319635=CARTESIAN_POINT('Ctrl Pts',(-3.18483474500006,12.2,-2.41029831500001));
#319636=CARTESIAN_POINT('Ctrl Pts',(-3.18483474500006,5.2,-2.41029831500001));
#319637=CARTESIAN_POINT('Ctrl Pts',(-3.18483474500006,2.2,-2.41029831500001));
#319638=CARTESIAN_POINT('Ctrl Pts',(-3.18477642900006,12.2,-2.41025539300002));
#319639=CARTESIAN_POINT('Ctrl Pts',(-3.18477642900006,5.2,-2.41025539300002));
#319640=CARTESIAN_POINT('Ctrl Pts',(-3.18477642900006,2.2,-2.41025539300002));
#319641=CARTESIAN_POINT('Ctrl Pts',(-3.18472406700006,12.2,-2.41021675800001));
#319642=CARTESIAN_POINT('Ctrl Pts',(-3.18472406700006,5.2,-2.41021675800001));
#319643=CARTESIAN_POINT('Ctrl Pts',(-3.18472406700006,2.2,-2.41021675800001));
#319644=CARTESIAN_POINT('Ctrl Pts',(-3.18467766000006,12.2,-2.41018243000001));
#319645=CARTESIAN_POINT('Ctrl Pts',(-3.18467766000006,5.2,-2.41018243000001));
#319646=CARTESIAN_POINT('Ctrl Pts',(-3.18467766000006,2.2,-2.41018243000001));
#319647=CARTESIAN_POINT('Ctrl Pts',(-3.18463288082923,12.2,-2.41014921067249));
#319648=CARTESIAN_POINT('Ctrl Pts',(-3.18463288082923,5.2,-2.41014921067249));
#319649=CARTESIAN_POINT('Ctrl Pts',(-3.18463288082923,2.2,-2.41014921067249));
#319650=CARTESIAN_POINT('Ctrl Pts',(-3.18460231601978,12.2,-2.41012644147867));
#319651=CARTESIAN_POINT('Ctrl Pts',(-3.18460231601978,5.2,-2.41012644147867));
#319652=CARTESIAN_POINT('Ctrl Pts',(-3.18460231601978,2.2,-2.41012644147867));
#319653=CARTESIAN_POINT('Ctrl Pts',(-3.18458221430919,12.2,-2.41011139784499));
#319654=CARTESIAN_POINT('Ctrl Pts',(-3.18458221430919,5.2,-2.41011139784499));
#319655=CARTESIAN_POINT('Ctrl Pts',(-3.18458221430919,2.2,-2.41011139784499));
#319656=CARTESIAN_POINT('Ctrl Pts',(-3.18456971176712,12.2,-2.41010199879104));
#319657=CARTESIAN_POINT('Ctrl Pts',(-3.18456971176712,5.2,-2.41010199879104));
#319658=CARTESIAN_POINT('Ctrl Pts',(-3.18456971176712,2.2,-2.41010199879104));
#319659=CARTESIAN_POINT('Ctrl Pts',(-3.18456199000006,12.2,-2.41009620000002));
#319660=CARTESIAN_POINT('Ctrl Pts',(-3.18456199000006,5.2,-2.41009620000002));
#319661=CARTESIAN_POINT('Ctrl Pts',(-3.18456199000006,2.2,-2.41009620000002));
#319662=CARTESIAN_POINT('',(-3.18456186900006,2.7,-2.41009636100001));
#319663=CARTESIAN_POINT('',(-3.18456186900006,12.2,-2.41009636100001));
#319664=CARTESIAN_POINT('Ctrl Pts',(-3.98353538000006,2.7,-2.58726610100001));
#319665=CARTESIAN_POINT('Ctrl Pts',(-3.72873002607504,2.7,-2.58625929211275));
#319666=CARTESIAN_POINT('Ctrl Pts',(-3.54026174963293,2.69999999999094,
-2.54811998493994));
#319667=CARTESIAN_POINT('Ctrl Pts',(-3.26663347427495,2.69999999999094,
-2.46586464912604));
#319668=CARTESIAN_POINT('Ctrl Pts',(-3.19489970037899,2.69999999999544,
-2.41765563987494));
#319669=CARTESIAN_POINT('Ctrl Pts',(-3.18483344867918,2.69999999999544,
-2.4102976087089));
#319670=CARTESIAN_POINT('Ctrl Pts',(-3.18469713278844,2.7,-2.41019768775304));
#319671=CARTESIAN_POINT('Ctrl Pts',(-3.18456199000006,2.7,-2.41009620000002));
#319672=CARTESIAN_POINT('Origin',(-3.18452095000006,15.2,-2.41006539300002));
#319673=CARTESIAN_POINT('',(-2.89052929200006,2.7,-2.18757066500002));
#319674=CARTESIAN_POINT('',(-2.89052929200006,2.2,-2.18757066500002));
#319675=CARTESIAN_POINT('',(-1.59226047414512,2.7,-1.20503269762968));
#319676=CARTESIAN_POINT('Origin',(-5.66300478732629E-14,15.2,-1.77635683940025E-14));
#319677=CARTESIAN_POINT('',(-2.51818288300006,2.7,-2.60756207400001));
#319678=CARTESIAN_POINT('',(-2.51818288300006,12.2,-2.60756207400001));
#319679=CARTESIAN_POINT('Origin',(-5.66300478732629E-14,2.7,-1.92943768261394E-14));
#319680=CARTESIAN_POINT('Origin',(-5.66300478732629E-14,15.2,-1.77635683940025E-14));
#319681=CARTESIAN_POINT('',(-2.77432748000006,2.7,-2.87279814400002));
#319682=CARTESIAN_POINT('',(-2.77432748000006,12.2,-2.87279814400001));
#319683=CARTESIAN_POINT('',(-5.6232279645039E-14,2.7,-1.88824904010619E-14));
#319684=CARTESIAN_POINT('Ctrl Pts',(-2.77432738100006,12.2,-2.87279823800001));
#319685=CARTESIAN_POINT('Ctrl Pts',(-2.77432738100006,5.2,-2.87279823800001));
#319686=CARTESIAN_POINT('Ctrl Pts',(-2.77432738100006,2.2,-2.87279823800001));
#319687=CARTESIAN_POINT('Ctrl Pts',(-2.77433211472047,12.2,-2.87280317870827));
#319688=CARTESIAN_POINT('Ctrl Pts',(-2.77433211472047,5.2,-2.87280317870827));
#319689=CARTESIAN_POINT('Ctrl Pts',(-2.77433211472047,2.2,-2.87280317870827));
#319690=CARTESIAN_POINT('Ctrl Pts',(-2.77434127117772,12.2,-2.87281273360882));
#319691=CARTESIAN_POINT('Ctrl Pts',(-2.77434127117772,5.2,-2.87281273360882));
#319692=CARTESIAN_POINT('Ctrl Pts',(-2.77434127117772,2.2,-2.87281273360882));
#319693=CARTESIAN_POINT('Ctrl Pts',(-2.77435485557306,12.2,-2.87282690333949));
#319694=CARTESIAN_POINT('Ctrl Pts',(-2.77435485557306,5.2,-2.87282690333949));
#319695=CARTESIAN_POINT('Ctrl Pts',(-2.77435485557306,2.2,-2.87282690333949));
#319696=CARTESIAN_POINT('Ctrl Pts',(-2.77437283287678,12.2,-2.8728456878981));
#319697=CARTESIAN_POINT('Ctrl Pts',(-2.77437283287678,5.2,-2.8728456878981));
#319698=CARTESIAN_POINT('Ctrl Pts',(-2.77437283287678,2.2,-2.8728456878981));
#319699=CARTESIAN_POINT('Ctrl Pts',(-2.77440404800006,12.2,-2.87287852900001));
#319700=CARTESIAN_POINT('Ctrl Pts',(-2.77440404800006,5.2,-2.87287852900001));
#319701=CARTESIAN_POINT('Ctrl Pts',(-2.77440404800006,2.2,-2.87287852900001));
#319702=CARTESIAN_POINT('Ctrl Pts',(-2.77443868700006,12.2,-2.87291509200001));
#319703=CARTESIAN_POINT('Ctrl Pts',(-2.77443868700006,5.2,-2.87291509200001));
#319704=CARTESIAN_POINT('Ctrl Pts',(-2.77443868700006,2.2,-2.87291509200001));
#319705=CARTESIAN_POINT('Ctrl Pts',(-2.77447832800005,12.2,-2.87295705000002));
#319706=CARTESIAN_POINT('Ctrl Pts',(-2.77447832800005,5.2,-2.87295705000002));
#319707=CARTESIAN_POINT('Ctrl Pts',(-2.77447832800005,2.2,-2.87295705000002));
#319708=CARTESIAN_POINT('Ctrl Pts',(-2.77452295900006,12.2,-2.87300440500001));
#319709=CARTESIAN_POINT('Ctrl Pts',(-2.77452295900006,5.2,-2.87300440500001));
#319710=CARTESIAN_POINT('Ctrl Pts',(-2.77452295900006,2.2,-2.87300440500001));
#319711=CARTESIAN_POINT('Ctrl Pts',(-2.77457255900006,12.2,-2.87305715700001));
#319712=CARTESIAN_POINT('Ctrl Pts',(-2.77457255900006,5.2,-2.87305715700001));
#319713=CARTESIAN_POINT('Ctrl Pts',(-2.77457255900006,2.2,-2.87305715700001));
#319714=CARTESIAN_POINT('Ctrl Pts',(-2.77462709900006,12.2,-2.87311530900002));
#319715=CARTESIAN_POINT('Ctrl Pts',(-2.77462709900006,5.2,-2.87311530900002));
#319716=CARTESIAN_POINT('Ctrl Pts',(-2.77462709900006,2.2,-2.87311530900002));
#319717=CARTESIAN_POINT('Ctrl Pts',(-2.77468654700006,12.2,-2.87317886000002));
#319718=CARTESIAN_POINT('Ctrl Pts',(-2.77468654700006,5.2,-2.87317886000002));
#319719=CARTESIAN_POINT('Ctrl Pts',(-2.77468654700006,2.2,-2.87317886000002));
#319720=CARTESIAN_POINT('Ctrl Pts',(-2.77475087000006,12.2,-2.87324781200001));
#319721=CARTESIAN_POINT('Ctrl Pts',(-2.77475087000006,5.2,-2.87324781200001));
#319722=CARTESIAN_POINT('Ctrl Pts',(-2.77475087000006,2.2,-2.87324781200001));
#319723=CARTESIAN_POINT('Ctrl Pts',(-2.77482003700006,12.2,-2.87332216700001));
#319724=CARTESIAN_POINT('Ctrl Pts',(-2.77482003700006,5.2,-2.87332216700001));
#319725=CARTESIAN_POINT('Ctrl Pts',(-2.77482003700006,2.2,-2.87332216700001));
#319726=CARTESIAN_POINT('Ctrl Pts',(-2.77489402300006,12.2,-2.87340192500002));
#319727=CARTESIAN_POINT('Ctrl Pts',(-2.77489402300006,5.2,-2.87340192500002));
#319728=CARTESIAN_POINT('Ctrl Pts',(-2.77489402300006,2.2,-2.87340192500002));
#319729=CARTESIAN_POINT('Ctrl Pts',(-2.77497280400006,12.2,-2.87348708800002));
#319730=CARTESIAN_POINT('Ctrl Pts',(-2.77497280400006,5.2,-2.87348708800002));
#319731=CARTESIAN_POINT('Ctrl Pts',(-2.77497280400006,2.2,-2.87348708800002));
#319732=CARTESIAN_POINT('Ctrl Pts',(-2.77505635800006,12.2,-2.87357765600001));
#319733=CARTESIAN_POINT('Ctrl Pts',(-2.77505635800006,5.2,-2.87357765600001));
#319734=CARTESIAN_POINT('Ctrl Pts',(-2.77505635800006,2.2,-2.87357765600001));
#319735=CARTESIAN_POINT('Ctrl Pts',(-2.77514466100006,12.2,-2.87367363100001));
#319736=CARTESIAN_POINT('Ctrl Pts',(-2.77514466100006,5.2,-2.87367363100001));
#319737=CARTESIAN_POINT('Ctrl Pts',(-2.77514466100006,2.2,-2.87367363100001));
#319738=CARTESIAN_POINT('Ctrl Pts',(-2.77523769000006,12.2,-2.87377501100002));
#319739=CARTESIAN_POINT('Ctrl Pts',(-2.77523769000006,5.2,-2.87377501100002));
#319740=CARTESIAN_POINT('Ctrl Pts',(-2.77523769000006,2.2,-2.87377501100002));
#319741=CARTESIAN_POINT('Ctrl Pts',(-2.77533541600006,12.2,-2.87388180000002));
#319742=CARTESIAN_POINT('Ctrl Pts',(-2.77533541600006,5.2,-2.87388180000002));
#319743=CARTESIAN_POINT('Ctrl Pts',(-2.77533541600006,2.2,-2.87388180000002));
#319744=CARTESIAN_POINT('Ctrl Pts',(-2.77543781500006,12.2,-2.87399399700002));
#319745=CARTESIAN_POINT('Ctrl Pts',(-2.77543781500006,5.2,-2.87399399700002));
#319746=CARTESIAN_POINT('Ctrl Pts',(-2.77543781500006,2.2,-2.87399399700002));
#319747=CARTESIAN_POINT('Ctrl Pts',(-2.77554486000006,12.2,-2.87411160400001));
#319748=CARTESIAN_POINT('Ctrl Pts',(-2.77554486000006,5.2,-2.87411160400001));
#319749=CARTESIAN_POINT('Ctrl Pts',(-2.77554486000006,2.2,-2.87411160400001));
#319750=CARTESIAN_POINT('Ctrl Pts',(-2.77565652600006,12.2,-2.87423462000001));
#319751=CARTESIAN_POINT('Ctrl Pts',(-2.77565652600006,5.2,-2.87423462000001));
#319752=CARTESIAN_POINT('Ctrl Pts',(-2.77565652600006,2.2,-2.87423462000001));
#319753=CARTESIAN_POINT('Ctrl Pts',(-2.77577278800006,12.2,-2.87436304800002));
#319754=CARTESIAN_POINT('Ctrl Pts',(-2.77577278800006,5.2,-2.87436304800002));
#319755=CARTESIAN_POINT('Ctrl Pts',(-2.77577278800006,2.2,-2.87436304800002));
#319756=CARTESIAN_POINT('Ctrl Pts',(-2.77589362000006,12.2,-2.87449688600002));
#319757=CARTESIAN_POINT('Ctrl Pts',(-2.77589362000006,5.2,-2.87449688600002));
#319758=CARTESIAN_POINT('Ctrl Pts',(-2.77589362000006,2.2,-2.87449688600002));
#319759=CARTESIAN_POINT('Ctrl Pts',(-2.77601899900006,12.2,-2.87463613700002));
#319760=CARTESIAN_POINT('Ctrl Pts',(-2.77601899900006,5.2,-2.87463613700002));
#319761=CARTESIAN_POINT('Ctrl Pts',(-2.77601899900006,2.2,-2.87463613700002));
#319762=CARTESIAN_POINT('Ctrl Pts',(-2.77614890100006,12.2,-2.87478080100001));
#319763=CARTESIAN_POINT('Ctrl Pts',(-2.77614890100006,5.2,-2.87478080100001));
#319764=CARTESIAN_POINT('Ctrl Pts',(-2.77614890100006,2.2,-2.87478080100001));
#319765=CARTESIAN_POINT('Ctrl Pts',(-2.77628330200006,12.2,-2.87493087700001));
#319766=CARTESIAN_POINT('Ctrl Pts',(-2.77628330200006,5.2,-2.87493087700001));
#319767=CARTESIAN_POINT('Ctrl Pts',(-2.77628330200006,2.2,-2.87493087700001));
#319768=CARTESIAN_POINT('Ctrl Pts',(-2.77642217600006,12.2,-2.87508636800001));
#319769=CARTESIAN_POINT('Ctrl Pts',(-2.77642217600006,5.2,-2.87508636800001));
#319770=CARTESIAN_POINT('Ctrl Pts',(-2.77642217600006,2.2,-2.87508636800001));
#319771=CARTESIAN_POINT('Ctrl Pts',(-2.77656549900006,12.2,-2.87524727300001));
#319772=CARTESIAN_POINT('Ctrl Pts',(-2.77656549900006,5.2,-2.87524727300001));
#319773=CARTESIAN_POINT('Ctrl Pts',(-2.77656549900006,2.2,-2.87524727300001));
#319774=CARTESIAN_POINT('Ctrl Pts',(-2.77671324600006,12.2,-2.87541359300001));
#319775=CARTESIAN_POINT('Ctrl Pts',(-2.77671324600006,5.2,-2.87541359300001));
#319776=CARTESIAN_POINT('Ctrl Pts',(-2.77671324600006,2.2,-2.87541359300001));
#319777=CARTESIAN_POINT('Ctrl Pts',(-2.77686539300006,12.2,-2.87558532900002));
#319778=CARTESIAN_POINT('Ctrl Pts',(-2.77686539300006,5.2,-2.87558532900002));
#319779=CARTESIAN_POINT('Ctrl Pts',(-2.77686539300006,2.2,-2.87558532900002));
#319780=CARTESIAN_POINT('Ctrl Pts',(-2.77702191600006,12.2,-2.87576248100001));
#319781=CARTESIAN_POINT('Ctrl Pts',(-2.77702191600006,5.2,-2.87576248100001));
#319782=CARTESIAN_POINT('Ctrl Pts',(-2.77702191600006,2.2,-2.87576248100001));
#319783=CARTESIAN_POINT('Ctrl Pts',(-2.77718279000006,12.2,-2.87594504800001));
#319784=CARTESIAN_POINT('Ctrl Pts',(-2.77718279000006,5.2,-2.87594504800001));
#319785=CARTESIAN_POINT('Ctrl Pts',(-2.77718279000006,2.2,-2.87594504800001));
#319786=CARTESIAN_POINT('Ctrl Pts',(-2.77734799400006,12.2,-2.87613303200001));
#319787=CARTESIAN_POINT('Ctrl Pts',(-2.77734799400006,5.2,-2.87613303200001));
#319788=CARTESIAN_POINT('Ctrl Pts',(-2.77734799400006,2.2,-2.87613303200001));
#319789=CARTESIAN_POINT('Ctrl Pts',(-2.77751750000006,12.2,-2.87632643300002));
#319790=CARTESIAN_POINT('Ctrl Pts',(-2.77751750000006,5.2,-2.87632643300002));
#319791=CARTESIAN_POINT('Ctrl Pts',(-2.77751750000006,2.2,-2.87632643300002));
#319792=CARTESIAN_POINT('Ctrl Pts',(-2.77769128800006,12.2,-2.87652525200001));
#319793=CARTESIAN_POINT('Ctrl Pts',(-2.77769128800006,5.2,-2.87652525200001));
#319794=CARTESIAN_POINT('Ctrl Pts',(-2.77769128800006,2.2,-2.87652525200001));
#319795=CARTESIAN_POINT('Ctrl Pts',(-2.77786933100006,12.2,-2.87672948900001));
#319796=CARTESIAN_POINT('Ctrl Pts',(-2.77786933100006,5.2,-2.87672948900001));
#319797=CARTESIAN_POINT('Ctrl Pts',(-2.77786933100006,2.2,-2.87672948900001));
#319798=CARTESIAN_POINT('Ctrl Pts',(-2.77805160800006,12.2,-2.87693914300001));
#319799=CARTESIAN_POINT('Ctrl Pts',(-2.77805160800006,5.2,-2.87693914300001));
#319800=CARTESIAN_POINT('Ctrl Pts',(-2.77805160800006,2.2,-2.87693914300001));
#319801=CARTESIAN_POINT('Ctrl Pts',(-2.77823809300005,12.2,-2.87715421600002));
#319802=CARTESIAN_POINT('Ctrl Pts',(-2.77823809300005,5.2,-2.87715421600002));
#319803=CARTESIAN_POINT('Ctrl Pts',(-2.77823809300005,2.2,-2.87715421600002));
#319804=CARTESIAN_POINT('Ctrl Pts',(-2.77842876500006,12.2,-2.87737470600002));
#319805=CARTESIAN_POINT('Ctrl Pts',(-2.77842876500006,5.2,-2.87737470600002));
#319806=CARTESIAN_POINT('Ctrl Pts',(-2.77842876500006,2.2,-2.87737470600002));
#319807=CARTESIAN_POINT('Ctrl Pts',(-2.77862359800006,12.2,-2.87760061600002));
#319808=CARTESIAN_POINT('Ctrl Pts',(-2.77862359800006,5.2,-2.87760061600002));
#319809=CARTESIAN_POINT('Ctrl Pts',(-2.77862359800006,2.2,-2.87760061600002));
#319810=CARTESIAN_POINT('Ctrl Pts',(-2.77882257000006,12.2,-2.87783194500001));
#319811=CARTESIAN_POINT('Ctrl Pts',(-2.77882257000006,5.2,-2.87783194500001));
#319812=CARTESIAN_POINT('Ctrl Pts',(-2.77882257000006,2.2,-2.87783194500001));
#319813=CARTESIAN_POINT('Ctrl Pts',(-2.77902565900006,12.2,-2.87806869300002));
#319814=CARTESIAN_POINT('Ctrl Pts',(-2.77902565900006,5.2,-2.87806869300002));
#319815=CARTESIAN_POINT('Ctrl Pts',(-2.77902565900006,2.2,-2.87806869300002));
#319816=CARTESIAN_POINT('Ctrl Pts',(-2.77923283900006,12.2,-2.87831085900002));
#319817=CARTESIAN_POINT('Ctrl Pts',(-2.77923283900006,5.2,-2.87831085900002));
#319818=CARTESIAN_POINT('Ctrl Pts',(-2.77923283900006,2.2,-2.87831085900002));
#319819=CARTESIAN_POINT('Ctrl Pts',(-2.77944409000006,12.2,-2.87855844500001));
#319820=CARTESIAN_POINT('Ctrl Pts',(-2.77944409000006,5.2,-2.87855844500001));
#319821=CARTESIAN_POINT('Ctrl Pts',(-2.77944409000006,2.2,-2.87855844500001));
#319822=CARTESIAN_POINT('Ctrl Pts',(-2.77965938600006,12.2,-2.87881145000001));
#319823=CARTESIAN_POINT('Ctrl Pts',(-2.77965938600006,5.2,-2.87881145000001));
#319824=CARTESIAN_POINT('Ctrl Pts',(-2.77965938600006,2.2,-2.87881145000001));
#319825=CARTESIAN_POINT('Ctrl Pts',(-2.77987870500006,12.2,-2.87906987400001));
#319826=CARTESIAN_POINT('Ctrl Pts',(-2.77987870500006,5.2,-2.87906987400001));
#319827=CARTESIAN_POINT('Ctrl Pts',(-2.77987870500006,2.2,-2.87906987400001));
#319828=CARTESIAN_POINT('Ctrl Pts',(-2.78010202600006,12.2,-2.87933371800001));
#319829=CARTESIAN_POINT('Ctrl Pts',(-2.78010202600006,5.2,-2.87933371800001));
#319830=CARTESIAN_POINT('Ctrl Pts',(-2.78010202600006,2.2,-2.87933371800001));
#319831=CARTESIAN_POINT('Ctrl Pts',(-2.78032932400006,12.2,-2.87960298100002));
#319832=CARTESIAN_POINT('Ctrl Pts',(-2.78032932400006,5.2,-2.87960298100002));
#319833=CARTESIAN_POINT('Ctrl Pts',(-2.78032932400006,2.2,-2.87960298100002));
#319834=CARTESIAN_POINT('Ctrl Pts',(-2.78056057600006,12.2,-2.87987766400001));
#319835=CARTESIAN_POINT('Ctrl Pts',(-2.78056057600006,5.2,-2.87987766400001));
#319836=CARTESIAN_POINT('Ctrl Pts',(-2.78056057600006,2.2,-2.87987766400001));
#319837=CARTESIAN_POINT('Ctrl Pts',(-2.78079576200006,12.2,-2.88015776600002));
#319838=CARTESIAN_POINT('Ctrl Pts',(-2.78079576200006,5.2,-2.88015776600002));
#319839=CARTESIAN_POINT('Ctrl Pts',(-2.78079576200006,2.2,-2.88015776600002));
#319840=CARTESIAN_POINT('Ctrl Pts',(-2.78103485600006,12.2,-2.88044328600002));
#319841=CARTESIAN_POINT('Ctrl Pts',(-2.78103485600006,5.2,-2.88044328600002));
#319842=CARTESIAN_POINT('Ctrl Pts',(-2.78103485600006,2.2,-2.88044328600002));
#319843=CARTESIAN_POINT('Ctrl Pts',(-2.78127783800006,12.2,-2.88073422700001));
#319844=CARTESIAN_POINT('Ctrl Pts',(-2.78127783800006,5.2,-2.88073422700001));
#319845=CARTESIAN_POINT('Ctrl Pts',(-2.78127783800006,2.2,-2.88073422700001));
#319846=CARTESIAN_POINT('Ctrl Pts',(-2.78152468400005,12.2,-2.88103058500001));
#319847=CARTESIAN_POINT('Ctrl Pts',(-2.78152468400005,5.2,-2.88103058500001));
#319848=CARTESIAN_POINT('Ctrl Pts',(-2.78152468400005,2.2,-2.88103058500001));
#319849=CARTESIAN_POINT('Ctrl Pts',(-2.78177537400006,12.2,-2.88133236300002));
#319850=CARTESIAN_POINT('Ctrl Pts',(-2.78177537400006,5.2,-2.88133236300002));
#319851=CARTESIAN_POINT('Ctrl Pts',(-2.78177537400006,2.2,-2.88133236300002));
#319852=CARTESIAN_POINT('Ctrl Pts',(-2.78202988300006,12.2,-2.88163955900002));
#319853=CARTESIAN_POINT('Ctrl Pts',(-2.78202988300006,5.2,-2.88163955900002));
#319854=CARTESIAN_POINT('Ctrl Pts',(-2.78202988300006,2.2,-2.88163955900002));
#319855=CARTESIAN_POINT('Ctrl Pts',(-2.78228819100006,12.2,-2.88195217300002));
#319856=CARTESIAN_POINT('Ctrl Pts',(-2.78228819100006,5.2,-2.88195217300002));
#319857=CARTESIAN_POINT('Ctrl Pts',(-2.78228819100006,2.2,-2.88195217300002));
#319858=CARTESIAN_POINT('Ctrl Pts',(-2.78255027400005,12.2,-2.88227020500001));
#319859=CARTESIAN_POINT('Ctrl Pts',(-2.78255027400005,5.2,-2.88227020500001));
#319860=CARTESIAN_POINT('Ctrl Pts',(-2.78255027400005,2.2,-2.88227020500001));
#319861=CARTESIAN_POINT('Ctrl Pts',(-2.78281611000006,12.2,-2.88259365600001));
#319862=CARTESIAN_POINT('Ctrl Pts',(-2.78281611000006,5.2,-2.88259365600001));
#319863=CARTESIAN_POINT('Ctrl Pts',(-2.78281611000006,2.2,-2.88259365600001));
#319864=CARTESIAN_POINT('Ctrl Pts',(-2.78308567900006,12.2,-2.88292252400002));
#319865=CARTESIAN_POINT('Ctrl Pts',(-2.78308567900006,5.2,-2.88292252400002));
#319866=CARTESIAN_POINT('Ctrl Pts',(-2.78308567900006,2.2,-2.88292252400002));
#319867=CARTESIAN_POINT('Ctrl Pts',(-2.78335895700006,12.2,-2.88325680900002));
#319868=CARTESIAN_POINT('Ctrl Pts',(-2.78335895700006,5.2,-2.88325680900002));
#319869=CARTESIAN_POINT('Ctrl Pts',(-2.78335895700006,2.2,-2.88325680900002));
#319870=CARTESIAN_POINT('Ctrl Pts',(-2.78363592400006,12.2,-2.88359651200001));
#319871=CARTESIAN_POINT('Ctrl Pts',(-2.78363592400006,5.2,-2.88359651200001));
#319872=CARTESIAN_POINT('Ctrl Pts',(-2.78363592400006,2.2,-2.88359651200001));
#319873=CARTESIAN_POINT('Ctrl Pts',(-2.78391655600006,12.2,-2.88394163000001));
#319874=CARTESIAN_POINT('Ctrl Pts',(-2.78391655600006,5.2,-2.88394163000001));
#319875=CARTESIAN_POINT('Ctrl Pts',(-2.78391655600006,2.2,-2.88394163000001));
#319876=CARTESIAN_POINT('Ctrl Pts',(-2.78420083300006,12.2,-2.88429216500001));
#319877=CARTESIAN_POINT('Ctrl Pts',(-2.78420083300006,5.2,-2.88429216500001));
#319878=CARTESIAN_POINT('Ctrl Pts',(-2.78420083300006,2.2,-2.88429216500001));
#319879=CARTESIAN_POINT('Ctrl Pts',(-2.78448873300006,12.2,-2.88464811600001));
#319880=CARTESIAN_POINT('Ctrl Pts',(-2.78448873300006,5.2,-2.88464811600001));
#319881=CARTESIAN_POINT('Ctrl Pts',(-2.78448873300006,2.2,-2.88464811600001));
#319882=CARTESIAN_POINT('Ctrl Pts',(-2.78478023400006,12.2,-2.88500948100001));
#319883=CARTESIAN_POINT('Ctrl Pts',(-2.78478023400006,5.2,-2.88500948100001));
#319884=CARTESIAN_POINT('Ctrl Pts',(-2.78478023400006,2.2,-2.88500948100001));
#319885=CARTESIAN_POINT('Ctrl Pts',(-2.78507531500006,12.2,-2.88537626300001));
#319886=CARTESIAN_POINT('Ctrl Pts',(-2.78507531500006,5.2,-2.88537626300001));
#319887=CARTESIAN_POINT('Ctrl Pts',(-2.78507531500006,2.2,-2.88537626300001));
#319888=CARTESIAN_POINT('Ctrl Pts',(-2.78537395400006,12.2,-2.88574845800001));
#319889=CARTESIAN_POINT('Ctrl Pts',(-2.78537395400006,5.2,-2.88574845800001));
#319890=CARTESIAN_POINT('Ctrl Pts',(-2.78537395400006,2.2,-2.88574845800001));
#319891=CARTESIAN_POINT('Ctrl Pts',(-2.78567613100006,12.2,-2.88612606700001));
#319892=CARTESIAN_POINT('Ctrl Pts',(-2.78567613100006,5.2,-2.88612606700001));
#319893=CARTESIAN_POINT('Ctrl Pts',(-2.78567613100006,2.2,-2.88612606700001));
#319894=CARTESIAN_POINT('Ctrl Pts',(-2.78598182300006,12.2,-2.88650909000001));
#319895=CARTESIAN_POINT('Ctrl Pts',(-2.78598182300006,5.2,-2.88650909000001));
#319896=CARTESIAN_POINT('Ctrl Pts',(-2.78598182300006,2.2,-2.88650909000001));
#319897=CARTESIAN_POINT('Ctrl Pts',(-2.78629100900006,12.2,-2.88689752600002));
#319898=CARTESIAN_POINT('Ctrl Pts',(-2.78629100900006,5.2,-2.88689752600002));
#319899=CARTESIAN_POINT('Ctrl Pts',(-2.78629100900006,2.2,-2.88689752600002));
#319900=CARTESIAN_POINT('Ctrl Pts',(-2.78660366900006,12.2,-2.88729137400002));
#319901=CARTESIAN_POINT('Ctrl Pts',(-2.78660366900006,5.2,-2.88729137400002));
#319902=CARTESIAN_POINT('Ctrl Pts',(-2.78660366900006,2.2,-2.88729137400002));
#319903=CARTESIAN_POINT('Ctrl Pts',(-2.78691978100006,12.2,-2.88769063300002));
#319904=CARTESIAN_POINT('Ctrl Pts',(-2.78691978100006,5.2,-2.88769063300002));
#319905=CARTESIAN_POINT('Ctrl Pts',(-2.78691978100006,2.2,-2.88769063300002));
#319906=CARTESIAN_POINT('Ctrl Pts',(-2.78723932300006,12.2,-2.88809530300002));
#319907=CARTESIAN_POINT('Ctrl Pts',(-2.78723932300006,5.2,-2.88809530300002));
#319908=CARTESIAN_POINT('Ctrl Pts',(-2.78723932300006,2.2,-2.88809530300002));
#319909=CARTESIAN_POINT('Ctrl Pts',(-2.78756227700006,12.2,-2.88850538500002));
#319910=CARTESIAN_POINT('Ctrl Pts',(-2.78756227700006,5.2,-2.88850538500002));
#319911=CARTESIAN_POINT('Ctrl Pts',(-2.78756227700006,2.2,-2.88850538500002));
#319912=CARTESIAN_POINT('Ctrl Pts',(-2.78788861900006,12.2,-2.88892087500002));
#319913=CARTESIAN_POINT('Ctrl Pts',(-2.78788861900006,5.2,-2.88892087500002));
#319914=CARTESIAN_POINT('Ctrl Pts',(-2.78788861900006,2.2,-2.88892087500002));
#319915=CARTESIAN_POINT('Ctrl Pts',(-2.78821833000006,12.2,-2.88934177600002));
#319916=CARTESIAN_POINT('Ctrl Pts',(-2.78821833000006,5.2,-2.88934177600002));
#319917=CARTESIAN_POINT('Ctrl Pts',(-2.78821833000006,2.2,-2.88934177600002));
#319918=CARTESIAN_POINT('Ctrl Pts',(-2.78855138900005,12.2,-2.88976808400002));
#319919=CARTESIAN_POINT('Ctrl Pts',(-2.78855138900005,5.2,-2.88976808400002));
#319920=CARTESIAN_POINT('Ctrl Pts',(-2.78855138900005,2.2,-2.88976808400002));
#319921=CARTESIAN_POINT('Ctrl Pts',(-2.78888777500006,12.2,-2.89019980000001));
#319922=CARTESIAN_POINT('Ctrl Pts',(-2.78888777500006,5.2,-2.89019980000001));
#319923=CARTESIAN_POINT('Ctrl Pts',(-2.78888777500006,2.2,-2.89019980000001));
#319924=CARTESIAN_POINT('Ctrl Pts',(-2.78922746700006,12.2,-2.89063692400001));
#319925=CARTESIAN_POINT('Ctrl Pts',(-2.78922746700006,5.2,-2.89063692400001));
#319926=CARTESIAN_POINT('Ctrl Pts',(-2.78922746700006,2.2,-2.89063692400001));
#319927=CARTESIAN_POINT('Ctrl Pts',(-2.78957044400005,12.2,-2.89107945200001));
#319928=CARTESIAN_POINT('Ctrl Pts',(-2.78957044400005,5.2,-2.89107945200001));
#319929=CARTESIAN_POINT('Ctrl Pts',(-2.78957044400005,2.2,-2.89107945200001));
#319930=CARTESIAN_POINT('Ctrl Pts',(-2.78991668800006,12.2,-2.89152738600002));
#319931=CARTESIAN_POINT('Ctrl Pts',(-2.78991668800006,5.2,-2.89152738600002));
#319932=CARTESIAN_POINT('Ctrl Pts',(-2.78991668800006,2.2,-2.89152738600002));
#319933=CARTESIAN_POINT('Ctrl Pts',(-2.79026617500006,12.2,-2.89198072600001));
#319934=CARTESIAN_POINT('Ctrl Pts',(-2.79026617500006,5.2,-2.89198072600001));
#319935=CARTESIAN_POINT('Ctrl Pts',(-2.79026617500006,2.2,-2.89198072600001));
#319936=CARTESIAN_POINT('Ctrl Pts',(-2.79061888800006,12.2,-2.89243946900001));
#319937=CARTESIAN_POINT('Ctrl Pts',(-2.79061888800006,5.2,-2.89243946900001));
#319938=CARTESIAN_POINT('Ctrl Pts',(-2.79061888800006,2.2,-2.89243946900001));
#319939=CARTESIAN_POINT('Ctrl Pts',(-2.79097480400006,12.2,-2.89290361400001));
#319940=CARTESIAN_POINT('Ctrl Pts',(-2.79097480400006,5.2,-2.89290361400001));
#319941=CARTESIAN_POINT('Ctrl Pts',(-2.79097480400006,2.2,-2.89290361400001));
#319942=CARTESIAN_POINT('Ctrl Pts',(-2.79133390500005,12.2,-2.89337316200001));
#319943=CARTESIAN_POINT('Ctrl Pts',(-2.79133390500005,5.2,-2.89337316200001));
#319944=CARTESIAN_POINT('Ctrl Pts',(-2.79133390500005,2.2,-2.89337316200001));
#319945=CARTESIAN_POINT('Ctrl Pts',(-2.79169616900006,12.2,-2.89384811200001));
#319946=CARTESIAN_POINT('Ctrl Pts',(-2.79169616900006,5.2,-2.89384811200001));
#319947=CARTESIAN_POINT('Ctrl Pts',(-2.79169616900006,2.2,-2.89384811200001));
#319948=CARTESIAN_POINT('Ctrl Pts',(-2.79206157600006,12.2,-2.89432846000001));
#319949=CARTESIAN_POINT('Ctrl Pts',(-2.79206157600006,5.2,-2.89432846000001));
#319950=CARTESIAN_POINT('Ctrl Pts',(-2.79206157600006,2.2,-2.89432846000001));
#319951=CARTESIAN_POINT('Ctrl Pts',(-2.79243010700006,12.2,-2.89481420900001));
#319952=CARTESIAN_POINT('Ctrl Pts',(-2.79243010700006,5.2,-2.89481420900001));
#319953=CARTESIAN_POINT('Ctrl Pts',(-2.79243010700006,2.2,-2.89481420900001));
#319954=CARTESIAN_POINT('Ctrl Pts',(-2.79280174100006,12.2,-2.89530535500001));
#319955=CARTESIAN_POINT('Ctrl Pts',(-2.79280174100006,5.2,-2.89530535500001));
#319956=CARTESIAN_POINT('Ctrl Pts',(-2.79280174100006,2.2,-2.89530535500001));
#319957=CARTESIAN_POINT('Ctrl Pts',(-2.79317645900006,12.2,-2.89580189800001));
#319958=CARTESIAN_POINT('Ctrl Pts',(-2.79317645900006,5.2,-2.89580189800001));
#319959=CARTESIAN_POINT('Ctrl Pts',(-2.79317645900006,2.2,-2.89580189800001));
#319960=CARTESIAN_POINT('Ctrl Pts',(-2.79355424000005,12.2,-2.89630383900001));
#319961=CARTESIAN_POINT('Ctrl Pts',(-2.79355424000005,5.2,-2.89630383900001));
#319962=CARTESIAN_POINT('Ctrl Pts',(-2.79355424000005,2.2,-2.89630383900001));
#319963=CARTESIAN_POINT('Ctrl Pts',(-2.79393506600006,12.2,-2.89681117400002));
#319964=CARTESIAN_POINT('Ctrl Pts',(-2.79393506600006,5.2,-2.89681117400002));
#319965=CARTESIAN_POINT('Ctrl Pts',(-2.79393506600006,2.2,-2.89681117400002));
#319966=CARTESIAN_POINT('Ctrl Pts',(-2.79431891500006,12.2,-2.89732390400002));
#319967=CARTESIAN_POINT('Ctrl Pts',(-2.79431891500006,5.2,-2.89732390400002));
#319968=CARTESIAN_POINT('Ctrl Pts',(-2.79431891500006,2.2,-2.89732390400002));
#319969=CARTESIAN_POINT('Ctrl Pts',(-2.79470576700006,12.2,-2.89784202700002));
#319970=CARTESIAN_POINT('Ctrl Pts',(-2.79470576700006,5.2,-2.89784202700002));
#319971=CARTESIAN_POINT('Ctrl Pts',(-2.79470576700006,2.2,-2.89784202700002));
#319972=CARTESIAN_POINT('Ctrl Pts',(-2.79509560600005,12.2,-2.89836554100001));
#319973=CARTESIAN_POINT('Ctrl Pts',(-2.79509560600005,5.2,-2.89836554100001));
#319974=CARTESIAN_POINT('Ctrl Pts',(-2.79509560600005,2.2,-2.89836554100001));
#319975=CARTESIAN_POINT('Ctrl Pts',(-2.79548840900006,12.2,-2.89889444600002));
#319976=CARTESIAN_POINT('Ctrl Pts',(-2.79548840900006,5.2,-2.89889444600002));
#319977=CARTESIAN_POINT('Ctrl Pts',(-2.79548840900006,2.2,-2.89889444600002));
#319978=CARTESIAN_POINT('Ctrl Pts',(-2.79588415700006,12.2,-2.89942874200001));
#319979=CARTESIAN_POINT('Ctrl Pts',(-2.79588415700006,5.2,-2.89942874200001));
#319980=CARTESIAN_POINT('Ctrl Pts',(-2.79588415700006,2.2,-2.89942874200001));
#319981=CARTESIAN_POINT('Ctrl Pts',(-2.79628283100006,12.2,-2.89996842600001));
#319982=CARTESIAN_POINT('Ctrl Pts',(-2.79628283100006,5.2,-2.89996842600001));
#319983=CARTESIAN_POINT('Ctrl Pts',(-2.79628283100006,2.2,-2.89996842600001));
#319984=CARTESIAN_POINT('Ctrl Pts',(-2.79668441300006,12.2,-2.90051349800001));
#319985=CARTESIAN_POINT('Ctrl Pts',(-2.79668441300006,5.2,-2.90051349800001));
#319986=CARTESIAN_POINT('Ctrl Pts',(-2.79668441300006,2.2,-2.90051349800001));
#319987=CARTESIAN_POINT('Ctrl Pts',(-2.79708888100005,12.2,-2.90106395600001));
#319988=CARTESIAN_POINT('Ctrl Pts',(-2.79708888100005,5.2,-2.90106395600001));
#319989=CARTESIAN_POINT('Ctrl Pts',(-2.79708888100005,2.2,-2.90106395600001));
#319990=CARTESIAN_POINT('Ctrl Pts',(-2.79749621700006,12.2,-2.90161979900001));
#319991=CARTESIAN_POINT('Ctrl Pts',(-2.79749621700006,5.2,-2.90161979900001));
#319992=CARTESIAN_POINT('Ctrl Pts',(-2.79749621700006,2.2,-2.90161979900001));
#319993=CARTESIAN_POINT('Ctrl Pts',(-2.79790640200006,12.2,-2.90218102600001));
#319994=CARTESIAN_POINT('Ctrl Pts',(-2.79790640200006,5.2,-2.90218102600001));
#319995=CARTESIAN_POINT('Ctrl Pts',(-2.79790640200006,2.2,-2.90218102600001));
#319996=CARTESIAN_POINT('Ctrl Pts',(-2.79831941600006,12.2,-2.90274763500001));
#319997=CARTESIAN_POINT('Ctrl Pts',(-2.79831941600006,5.2,-2.90274763500001));
#319998=CARTESIAN_POINT('Ctrl Pts',(-2.79831941600006,2.2,-2.90274763500001));
#319999=CARTESIAN_POINT('Ctrl Pts',(-2.79873524100006,12.2,-2.90331962600002));
#320000=CARTESIAN_POINT('Ctrl Pts',(-2.79873524100006,5.2,-2.90331962600002));
#320001=CARTESIAN_POINT('Ctrl Pts',(-2.79873524100006,2.2,-2.90331962600002));
#320002=CARTESIAN_POINT('Ctrl Pts',(-2.79915385700006,12.2,-2.90389699700001));
#320003=CARTESIAN_POINT('Ctrl Pts',(-2.79915385700006,5.2,-2.90389699700001));
#320004=CARTESIAN_POINT('Ctrl Pts',(-2.79915385700006,2.2,-2.90389699700001));
#320005=CARTESIAN_POINT('Ctrl Pts',(-2.79957524500006,12.2,-2.90447974700001));
#320006=CARTESIAN_POINT('Ctrl Pts',(-2.79957524500006,5.2,-2.90447974700001));
#320007=CARTESIAN_POINT('Ctrl Pts',(-2.79957524500006,2.2,-2.90447974700001));
#320008=CARTESIAN_POINT('Ctrl Pts',(-2.79999938600006,12.2,-2.90506787400002));
#320009=CARTESIAN_POINT('Ctrl Pts',(-2.79999938600006,5.2,-2.90506787400002));
#320010=CARTESIAN_POINT('Ctrl Pts',(-2.79999938600006,2.2,-2.90506787400002));
#320011=CARTESIAN_POINT('Ctrl Pts',(-2.80042626200005,12.2,-2.90566137700001));
#320012=CARTESIAN_POINT('Ctrl Pts',(-2.80042626200005,5.2,-2.90566137700001));
#320013=CARTESIAN_POINT('Ctrl Pts',(-2.80042626200005,2.2,-2.90566137700001));
#320014=CARTESIAN_POINT('Ctrl Pts',(-2.80085585300006,12.2,-2.90626025500002));
#320015=CARTESIAN_POINT('Ctrl Pts',(-2.80085585300006,5.2,-2.90626025500002));
#320016=CARTESIAN_POINT('Ctrl Pts',(-2.80085585300006,2.2,-2.90626025500002));
#320017=CARTESIAN_POINT('Ctrl Pts',(-2.80128814100005,12.2,-2.90686450600001));
#320018=CARTESIAN_POINT('Ctrl Pts',(-2.80128814100005,5.2,-2.90686450600001));
#320019=CARTESIAN_POINT('Ctrl Pts',(-2.80128814100005,2.2,-2.90686450600001));
#320020=CARTESIAN_POINT('Ctrl Pts',(-2.80172310700006,12.2,-2.90747412900001));
#320021=CARTESIAN_POINT('Ctrl Pts',(-2.80172310700006,5.2,-2.90747412900001));
#320022=CARTESIAN_POINT('Ctrl Pts',(-2.80172310700006,2.2,-2.90747412900001));
#320023=CARTESIAN_POINT('Ctrl Pts',(-2.80216073100005,12.2,-2.90808912300001));
#320024=CARTESIAN_POINT('Ctrl Pts',(-2.80216073100005,5.2,-2.90808912300001));
#320025=CARTESIAN_POINT('Ctrl Pts',(-2.80216073100005,2.2,-2.90808912300001));
#320026=CARTESIAN_POINT('Ctrl Pts',(-2.80260099700006,12.2,-2.90870948500002));
#320027=CARTESIAN_POINT('Ctrl Pts',(-2.80260099700006,5.2,-2.90870948500002));
#320028=CARTESIAN_POINT('Ctrl Pts',(-2.80260099700006,2.2,-2.90870948500002));
#320029=CARTESIAN_POINT('Ctrl Pts',(-2.80304388500006,12.2,-2.90933521600001));
#320030=CARTESIAN_POINT('Ctrl Pts',(-2.80304388500006,5.2,-2.90933521600001));
#320031=CARTESIAN_POINT('Ctrl Pts',(-2.80304388500006,2.2,-2.90933521600001));
#320032=CARTESIAN_POINT('Ctrl Pts',(-2.80348937700006,12.2,-2.90996631300001));
#320033=CARTESIAN_POINT('Ctrl Pts',(-2.80348937700006,5.2,-2.90996631300001));
#320034=CARTESIAN_POINT('Ctrl Pts',(-2.80348937700006,2.2,-2.90996631300001));
#320035=CARTESIAN_POINT('Ctrl Pts',(-2.80393745200006,12.2,-2.91060277400002));
#320036=CARTESIAN_POINT('Ctrl Pts',(-2.80393745200006,5.2,-2.91060277400002));
#320037=CARTESIAN_POINT('Ctrl Pts',(-2.80393745200006,2.2,-2.91060277400002));
#320038=CARTESIAN_POINT('Ctrl Pts',(-2.80438809600006,12.2,-2.91124459800002));
#320039=CARTESIAN_POINT('Ctrl Pts',(-2.80438809600006,5.2,-2.91124459800002));
#320040=CARTESIAN_POINT('Ctrl Pts',(-2.80438809600006,2.2,-2.91124459800002));
#320041=CARTESIAN_POINT('Ctrl Pts',(-2.80484128600006,12.2,-2.91189178400002));
#320042=CARTESIAN_POINT('Ctrl Pts',(-2.80484128600006,5.2,-2.91189178400002));
#320043=CARTESIAN_POINT('Ctrl Pts',(-2.80484128600006,2.2,-2.91189178400002));
#320044=CARTESIAN_POINT('Ctrl Pts',(-2.80529700700006,12.2,-2.91254432900002));
#320045=CARTESIAN_POINT('Ctrl Pts',(-2.80529700700006,5.2,-2.91254432900002));
#320046=CARTESIAN_POINT('Ctrl Pts',(-2.80529700700006,2.2,-2.91254432900002));
#320047=CARTESIAN_POINT('Ctrl Pts',(-2.80575524000006,12.2,-2.91320223400001));
#320048=CARTESIAN_POINT('Ctrl Pts',(-2.80575524000006,5.2,-2.91320223400001));
#320049=CARTESIAN_POINT('Ctrl Pts',(-2.80575524000006,2.2,-2.91320223400001));
#320050=CARTESIAN_POINT('Ctrl Pts',(-2.80621596600006,12.2,-2.91386549600002));
#320051=CARTESIAN_POINT('Ctrl Pts',(-2.80621596600006,5.2,-2.91386549600002));
#320052=CARTESIAN_POINT('Ctrl Pts',(-2.80621596600006,2.2,-2.91386549600002));
#320053=CARTESIAN_POINT('Ctrl Pts',(-2.80667916700006,12.2,-2.91453411200001));
#320054=CARTESIAN_POINT('Ctrl Pts',(-2.80667916700006,5.2,-2.91453411200001));
#320055=CARTESIAN_POINT('Ctrl Pts',(-2.80667916700006,2.2,-2.91453411200001));
#320056=CARTESIAN_POINT('Ctrl Pts',(-2.80714482500006,12.2,-2.91520808200001));
#320057=CARTESIAN_POINT('Ctrl Pts',(-2.80714482500006,5.2,-2.91520808200001));
#320058=CARTESIAN_POINT('Ctrl Pts',(-2.80714482500006,2.2,-2.91520808200001));
#320059=CARTESIAN_POINT('Ctrl Pts',(-2.80761292300005,12.2,-2.91588740400002));
#320060=CARTESIAN_POINT('Ctrl Pts',(-2.80761292300005,5.2,-2.91588740400002));
#320061=CARTESIAN_POINT('Ctrl Pts',(-2.80761292300005,2.2,-2.91588740400002));
#320062=CARTESIAN_POINT('Ctrl Pts',(-2.80808344100006,12.2,-2.91657207700001));
#320063=CARTESIAN_POINT('Ctrl Pts',(-2.80808344100006,5.2,-2.91657207700001));
#320064=CARTESIAN_POINT('Ctrl Pts',(-2.80808344100006,2.2,-2.91657207700001));
#320065=CARTESIAN_POINT('Ctrl Pts',(-2.80855636300006,12.2,-2.91726209800002));
#320066=CARTESIAN_POINT('Ctrl Pts',(-2.80855636300006,5.2,-2.91726209800002));
#320067=CARTESIAN_POINT('Ctrl Pts',(-2.80855636300006,2.2,-2.91726209800002));
#320068=CARTESIAN_POINT('Ctrl Pts',(-2.80903167000006,12.2,-2.91795746600001));
#320069=CARTESIAN_POINT('Ctrl Pts',(-2.80903167000006,5.2,-2.91795746600001));
#320070=CARTESIAN_POINT('Ctrl Pts',(-2.80903167000006,2.2,-2.91795746600001));
#320071=CARTESIAN_POINT('Ctrl Pts',(-2.80950934500006,12.2,-2.91865818000002));
#320072=CARTESIAN_POINT('Ctrl Pts',(-2.80950934500006,5.2,-2.91865818000002));
#320073=CARTESIAN_POINT('Ctrl Pts',(-2.80950934500006,2.2,-2.91865818000002));
#320074=CARTESIAN_POINT('Ctrl Pts',(-2.80998936800006,12.2,-2.91936423700002));
#320075=CARTESIAN_POINT('Ctrl Pts',(-2.80998936800006,5.2,-2.91936423700002));
#320076=CARTESIAN_POINT('Ctrl Pts',(-2.80998936800006,2.2,-2.91936423700002));
#320077=CARTESIAN_POINT('Ctrl Pts',(-2.81047172400006,12.2,-2.92007563600002));
#320078=CARTESIAN_POINT('Ctrl Pts',(-2.81047172400006,5.2,-2.92007563600002));
#320079=CARTESIAN_POINT('Ctrl Pts',(-2.81047172400006,2.2,-2.92007563600002));
#320080=CARTESIAN_POINT('Ctrl Pts',(-2.81095639400006,12.2,-2.92079237500001));
#320081=CARTESIAN_POINT('Ctrl Pts',(-2.81095639400006,5.2,-2.92079237500001));
#320082=CARTESIAN_POINT('Ctrl Pts',(-2.81095639400006,2.2,-2.92079237500001));
#320083=CARTESIAN_POINT('Ctrl Pts',(-2.81144336000006,12.2,-2.92151445100002));
#320084=CARTESIAN_POINT('Ctrl Pts',(-2.81144336000006,5.2,-2.92151445100002));
#320085=CARTESIAN_POINT('Ctrl Pts',(-2.81144336000006,2.2,-2.92151445100002));
#320086=CARTESIAN_POINT('Ctrl Pts',(-2.81193260400005,12.2,-2.92224186500002));
#320087=CARTESIAN_POINT('Ctrl Pts',(-2.81193260400005,5.2,-2.92224186500002));
#320088=CARTESIAN_POINT('Ctrl Pts',(-2.81193260400005,2.2,-2.92224186500002));
#320089=CARTESIAN_POINT('Ctrl Pts',(-2.81242411000005,12.2,-2.92297461300001));
#320090=CARTESIAN_POINT('Ctrl Pts',(-2.81242411000005,5.2,-2.92297461300001));
#320091=CARTESIAN_POINT('Ctrl Pts',(-2.81242411000005,2.2,-2.92297461300001));
#320092=CARTESIAN_POINT('Ctrl Pts',(-2.81291786100006,12.2,-2.92371269400002));
#320093=CARTESIAN_POINT('Ctrl Pts',(-2.81291786100006,5.2,-2.92371269400002));
#320094=CARTESIAN_POINT('Ctrl Pts',(-2.81291786100006,2.2,-2.92371269400002));
#320095=CARTESIAN_POINT('Ctrl Pts',(-2.81341383700005,12.2,-2.92445610600002));
#320096=CARTESIAN_POINT('Ctrl Pts',(-2.81341383700005,5.2,-2.92445610600002));
#320097=CARTESIAN_POINT('Ctrl Pts',(-2.81341383700005,2.2,-2.92445610600002));
#320098=CARTESIAN_POINT('Ctrl Pts',(-2.81391202300005,12.2,-2.92520484700002));
#320099=CARTESIAN_POINT('Ctrl Pts',(-2.81391202300005,5.2,-2.92520484700002));
#320100=CARTESIAN_POINT('Ctrl Pts',(-2.81391202300005,2.2,-2.92520484700002));
#320101=CARTESIAN_POINT('Ctrl Pts',(-2.81441239800006,12.2,-2.92595891500001));
#320102=CARTESIAN_POINT('Ctrl Pts',(-2.81441239800006,5.2,-2.92595891500001));
#320103=CARTESIAN_POINT('Ctrl Pts',(-2.81441239800006,2.2,-2.92595891500001));
#320104=CARTESIAN_POINT('Ctrl Pts',(-2.81491495000005,12.2,-2.92671830800002));
#320105=CARTESIAN_POINT('Ctrl Pts',(-2.81491495000005,5.2,-2.92671830800002));
#320106=CARTESIAN_POINT('Ctrl Pts',(-2.81491495000005,2.2,-2.92671830800002));
#320107=CARTESIAN_POINT('Ctrl Pts',(-2.81541965700006,12.2,-2.92748302500002));
#320108=CARTESIAN_POINT('Ctrl Pts',(-2.81541965700006,5.2,-2.92748302500002));
#320109=CARTESIAN_POINT('Ctrl Pts',(-2.81541965700006,2.2,-2.92748302500002));
#320110=CARTESIAN_POINT('Ctrl Pts',(-2.81592650500006,12.2,-2.92825306300001));
#320111=CARTESIAN_POINT('Ctrl Pts',(-2.81592650500006,5.2,-2.92825306300001));
#320112=CARTESIAN_POINT('Ctrl Pts',(-2.81592650500006,2.2,-2.92825306300001));
#320113=CARTESIAN_POINT('Ctrl Pts',(-2.81643547500006,12.2,-2.92902842100002));
#320114=CARTESIAN_POINT('Ctrl Pts',(-2.81643547500006,5.2,-2.92902842100002));
#320115=CARTESIAN_POINT('Ctrl Pts',(-2.81643547500006,2.2,-2.92902842100002));
#320116=CARTESIAN_POINT('Ctrl Pts',(-2.81694655000006,12.2,-2.92980909600002));
#320117=CARTESIAN_POINT('Ctrl Pts',(-2.81694655000006,5.2,-2.92980909600002));
#320118=CARTESIAN_POINT('Ctrl Pts',(-2.81694655000006,2.2,-2.92980909600002));
#320119=CARTESIAN_POINT('Ctrl Pts',(-2.81745971400006,12.2,-2.93059508700001));
#320120=CARTESIAN_POINT('Ctrl Pts',(-2.81745971400006,5.2,-2.93059508700001));
#320121=CARTESIAN_POINT('Ctrl Pts',(-2.81745971400006,2.2,-2.93059508700001));
#320122=CARTESIAN_POINT('Ctrl Pts',(-2.81797494900006,12.2,-2.93138639100002));
#320123=CARTESIAN_POINT('Ctrl Pts',(-2.81797494900006,5.2,-2.93138639100002));
#320124=CARTESIAN_POINT('Ctrl Pts',(-2.81797494900006,2.2,-2.93138639100002));
#320125=CARTESIAN_POINT('Ctrl Pts',(-2.81849223900006,12.2,-2.93218300800001));
#320126=CARTESIAN_POINT('Ctrl Pts',(-2.81849223900006,5.2,-2.93218300800001));
#320127=CARTESIAN_POINT('Ctrl Pts',(-2.81849223900006,2.2,-2.93218300800001));
#320128=CARTESIAN_POINT('Ctrl Pts',(-2.81901156500005,12.2,-2.93298493300002));
#320129=CARTESIAN_POINT('Ctrl Pts',(-2.81901156500005,5.2,-2.93298493300002));
#320130=CARTESIAN_POINT('Ctrl Pts',(-2.81901156500005,2.2,-2.93298493300002));
#320131=CARTESIAN_POINT('Ctrl Pts',(-2.81953291300006,12.2,-2.93379216500002));
#320132=CARTESIAN_POINT('Ctrl Pts',(-2.81953291300006,5.2,-2.93379216500002));
#320133=CARTESIAN_POINT('Ctrl Pts',(-2.81953291300006,2.2,-2.93379216500002));
#320134=CARTESIAN_POINT('Ctrl Pts',(-2.82005626300006,12.2,-2.93460470400001));
#320135=CARTESIAN_POINT('Ctrl Pts',(-2.82005626300006,5.2,-2.93460470400001));
#320136=CARTESIAN_POINT('Ctrl Pts',(-2.82005626300006,2.2,-2.93460470400001));
#320137=CARTESIAN_POINT('Ctrl Pts',(-2.82058160100005,12.2,-2.93542254400001));
#320138=CARTESIAN_POINT('Ctrl Pts',(-2.82058160100005,5.2,-2.93542254400001));
#320139=CARTESIAN_POINT('Ctrl Pts',(-2.82058160100005,2.2,-2.93542254400001));
#320140=CARTESIAN_POINT('Ctrl Pts',(-2.82110890800006,12.2,-2.93624568700002));
#320141=CARTESIAN_POINT('Ctrl Pts',(-2.82110890800006,5.2,-2.93624568700002));
#320142=CARTESIAN_POINT('Ctrl Pts',(-2.82110890800006,2.2,-2.93624568700002));
#320143=CARTESIAN_POINT('Ctrl Pts',(-2.82163817000006,12.2,-2.93707412900002));
#320144=CARTESIAN_POINT('Ctrl Pts',(-2.82163817000006,5.2,-2.93707412900002));
#320145=CARTESIAN_POINT('Ctrl Pts',(-2.82163817000006,2.2,-2.93707412900002));
#320146=CARTESIAN_POINT('Ctrl Pts',(-2.82216936700005,12.2,-2.93790786800002));
#320147=CARTESIAN_POINT('Ctrl Pts',(-2.82216936700005,5.2,-2.93790786800002));
#320148=CARTESIAN_POINT('Ctrl Pts',(-2.82216936700005,2.2,-2.93790786800002));
#320149=CARTESIAN_POINT('Ctrl Pts',(-2.82270248500006,12.2,-2.93874690100001));
#320150=CARTESIAN_POINT('Ctrl Pts',(-2.82270248500006,5.2,-2.93874690100001));
#320151=CARTESIAN_POINT('Ctrl Pts',(-2.82270248500006,2.2,-2.93874690100001));
#320152=CARTESIAN_POINT('Ctrl Pts',(-2.82323750600006,12.2,-2.93959122700001));
#320153=CARTESIAN_POINT('Ctrl Pts',(-2.82323750600006,5.2,-2.93959122700001));
#320154=CARTESIAN_POINT('Ctrl Pts',(-2.82323750600006,2.2,-2.93959122700001));
#320155=CARTESIAN_POINT('Ctrl Pts',(-2.82377441500006,12.2,-2.94044084400001));
#320156=CARTESIAN_POINT('Ctrl Pts',(-2.82377441500006,5.2,-2.94044084400001));
#320157=CARTESIAN_POINT('Ctrl Pts',(-2.82377441500006,2.2,-2.94044084400001));
#320158=CARTESIAN_POINT('Ctrl Pts',(-2.82431319300006,12.2,-2.94129574900001));
#320159=CARTESIAN_POINT('Ctrl Pts',(-2.82431319300006,5.2,-2.94129574900001));
#320160=CARTESIAN_POINT('Ctrl Pts',(-2.82431319300006,2.2,-2.94129574900001));
#320161=CARTESIAN_POINT('Ctrl Pts',(-2.82485382600006,12.2,-2.94215594000002));
#320162=CARTESIAN_POINT('Ctrl Pts',(-2.82485382600006,5.2,-2.94215594000002));
#320163=CARTESIAN_POINT('Ctrl Pts',(-2.82485382600006,2.2,-2.94215594000002));
#320164=CARTESIAN_POINT('Ctrl Pts',(-2.82539629600006,12.2,-2.94302141400001));
#320165=CARTESIAN_POINT('Ctrl Pts',(-2.82539629600006,5.2,-2.94302141400001));
#320166=CARTESIAN_POINT('Ctrl Pts',(-2.82539629600006,2.2,-2.94302141400001));
#320167=CARTESIAN_POINT('Ctrl Pts',(-2.82594058800006,12.2,-2.94389217100001));
#320168=CARTESIAN_POINT('Ctrl Pts',(-2.82594058800006,5.2,-2.94389217100001));
#320169=CARTESIAN_POINT('Ctrl Pts',(-2.82594058800006,2.2,-2.94389217100001));
#320170=CARTESIAN_POINT('Ctrl Pts',(-2.82648668400005,12.2,-2.94476820700002));
#320171=CARTESIAN_POINT('Ctrl Pts',(-2.82648668400005,5.2,-2.94476820700002));
#320172=CARTESIAN_POINT('Ctrl Pts',(-2.82648668400005,2.2,-2.94476820700002));
#320173=CARTESIAN_POINT('Ctrl Pts',(-2.82703456900005,12.2,-2.94564952000002));
#320174=CARTESIAN_POINT('Ctrl Pts',(-2.82703456900005,5.2,-2.94564952000002));
#320175=CARTESIAN_POINT('Ctrl Pts',(-2.82703456900005,2.2,-2.94564952000002));
#320176=CARTESIAN_POINT('Ctrl Pts',(-2.82758422700006,12.2,-2.94653610700002));
#320177=CARTESIAN_POINT('Ctrl Pts',(-2.82758422700006,5.2,-2.94653610700002));
#320178=CARTESIAN_POINT('Ctrl Pts',(-2.82758422700006,2.2,-2.94653610700002));
#320179=CARTESIAN_POINT('Ctrl Pts',(-2.82813564100006,12.2,-2.94742796800001));
#320180=CARTESIAN_POINT('Ctrl Pts',(-2.82813564100006,5.2,-2.94742796800001));
#320181=CARTESIAN_POINT('Ctrl Pts',(-2.82813564100006,2.2,-2.94742796800001));
#320182=CARTESIAN_POINT('Ctrl Pts',(-2.82868879500006,12.2,-2.94832509800001));
#320183=CARTESIAN_POINT('Ctrl Pts',(-2.82868879500006,5.2,-2.94832509800001));
#320184=CARTESIAN_POINT('Ctrl Pts',(-2.82868879500006,2.2,-2.94832509800001));
#320185=CARTESIAN_POINT('Ctrl Pts',(-2.82924367300006,12.2,-2.94922749700001));
#320186=CARTESIAN_POINT('Ctrl Pts',(-2.82924367300006,5.2,-2.94922749700001));
#320187=CARTESIAN_POINT('Ctrl Pts',(-2.82924367300006,2.2,-2.94922749700001));
#320188=CARTESIAN_POINT('Ctrl Pts',(-2.82980025900006,12.2,-2.95013516100001));
#320189=CARTESIAN_POINT('Ctrl Pts',(-2.82980025900006,5.2,-2.95013516100001));
#320190=CARTESIAN_POINT('Ctrl Pts',(-2.82980025900006,2.2,-2.95013516100001));
#320191=CARTESIAN_POINT('Ctrl Pts',(-2.83035853700006,12.2,-2.95104808800001));
#320192=CARTESIAN_POINT('Ctrl Pts',(-2.83035853700006,5.2,-2.95104808800001));
#320193=CARTESIAN_POINT('Ctrl Pts',(-2.83035853700006,2.2,-2.95104808800001));
#320194=CARTESIAN_POINT('Ctrl Pts',(-2.83091849000006,12.2,-2.95196627600002));
#320195=CARTESIAN_POINT('Ctrl Pts',(-2.83091849000006,5.2,-2.95196627600002));
#320196=CARTESIAN_POINT('Ctrl Pts',(-2.83091849000006,2.2,-2.95196627600002));
#320197=CARTESIAN_POINT('Ctrl Pts',(-2.83148010400006,12.2,-2.95288972300002));
#320198=CARTESIAN_POINT('Ctrl Pts',(-2.83148010400006,5.2,-2.95288972300002));
#320199=CARTESIAN_POINT('Ctrl Pts',(-2.83148010400006,2.2,-2.95288972300002));
#320200=CARTESIAN_POINT('Ctrl Pts',(-2.83204336300006,12.2,-2.95381842500001));
#320201=CARTESIAN_POINT('Ctrl Pts',(-2.83204336300006,5.2,-2.95381842500001));
#320202=CARTESIAN_POINT('Ctrl Pts',(-2.83204336300006,2.2,-2.95381842500001));
#320203=CARTESIAN_POINT('Ctrl Pts',(-2.83260824900006,12.2,-2.95475238100002));
#320204=CARTESIAN_POINT('Ctrl Pts',(-2.83260824900006,5.2,-2.95475238100002));
#320205=CARTESIAN_POINT('Ctrl Pts',(-2.83260824900006,2.2,-2.95475238100002));
#320206=CARTESIAN_POINT('Ctrl Pts',(-2.83317474800006,12.2,-2.95569158900001));
#320207=CARTESIAN_POINT('Ctrl Pts',(-2.83317474800006,5.2,-2.95569158900001));
#320208=CARTESIAN_POINT('Ctrl Pts',(-2.83317474800006,2.2,-2.95569158900001));
#320209=CARTESIAN_POINT('Ctrl Pts',(-2.83374284300006,12.2,-2.95663604500001));
#320210=CARTESIAN_POINT('Ctrl Pts',(-2.83374284300006,5.2,-2.95663604500001));
#320211=CARTESIAN_POINT('Ctrl Pts',(-2.83374284300006,2.2,-2.95663604500001));
#320212=CARTESIAN_POINT('Ctrl Pts',(-2.83431252100006,12.2,-2.95758574700002));
#320213=CARTESIAN_POINT('Ctrl Pts',(-2.83431252100006,5.2,-2.95758574700002));
#320214=CARTESIAN_POINT('Ctrl Pts',(-2.83431252100006,2.2,-2.95758574700002));
#320215=CARTESIAN_POINT('Ctrl Pts',(-2.83488376300005,12.2,-2.95854069400002));
#320216=CARTESIAN_POINT('Ctrl Pts',(-2.83488376300005,5.2,-2.95854069400002));
#320217=CARTESIAN_POINT('Ctrl Pts',(-2.83488376300005,2.2,-2.95854069400002));
#320218=CARTESIAN_POINT('Ctrl Pts',(-2.83545655400005,12.2,-2.95950088100001));
#320219=CARTESIAN_POINT('Ctrl Pts',(-2.83545655400005,5.2,-2.95950088100001));
#320220=CARTESIAN_POINT('Ctrl Pts',(-2.83545655400005,2.2,-2.95950088100001));
#320221=CARTESIAN_POINT('Ctrl Pts',(-2.83603088100006,12.2,-2.96046630800001));
#320222=CARTESIAN_POINT('Ctrl Pts',(-2.83603088100006,5.2,-2.96046630800001));
#320223=CARTESIAN_POINT('Ctrl Pts',(-2.83603088100006,2.2,-2.96046630800001));
#320224=CARTESIAN_POINT('Ctrl Pts',(-2.83660672500006,12.2,-2.96143697100002));
#320225=CARTESIAN_POINT('Ctrl Pts',(-2.83660672500006,5.2,-2.96143697100002));
#320226=CARTESIAN_POINT('Ctrl Pts',(-2.83660672500006,2.2,-2.96143697100002));
#320227=CARTESIAN_POINT('Ctrl Pts',(-2.83718407300006,12.2,-2.96241286700001));
#320228=CARTESIAN_POINT('Ctrl Pts',(-2.83718407300006,5.2,-2.96241286700001));
#320229=CARTESIAN_POINT('Ctrl Pts',(-2.83718407300006,2.2,-2.96241286700001));
#320230=CARTESIAN_POINT('Ctrl Pts',(-2.83776290800006,12.2,-2.96339399500001));
#320231=CARTESIAN_POINT('Ctrl Pts',(-2.83776290800006,5.2,-2.96339399500001));
#320232=CARTESIAN_POINT('Ctrl Pts',(-2.83776290800006,2.2,-2.96339399500001));
#320233=CARTESIAN_POINT('Ctrl Pts',(-2.83834321500006,12.2,-2.96438035200001));
#320234=CARTESIAN_POINT('Ctrl Pts',(-2.83834321500006,5.2,-2.96438035200001));
#320235=CARTESIAN_POINT('Ctrl Pts',(-2.83834321500006,2.2,-2.96438035200001));
#320236=CARTESIAN_POINT('Ctrl Pts',(-2.83892497800006,12.2,-2.96537193400002));
#320237=CARTESIAN_POINT('Ctrl Pts',(-2.83892497800006,5.2,-2.96537193400002));
#320238=CARTESIAN_POINT('Ctrl Pts',(-2.83892497800006,2.2,-2.96537193400002));
#320239=CARTESIAN_POINT('Ctrl Pts',(-2.83950818400006,12.2,-2.96636874000002));
#320240=CARTESIAN_POINT('Ctrl Pts',(-2.83950818400006,5.2,-2.96636874000002));
#320241=CARTESIAN_POINT('Ctrl Pts',(-2.83950818400006,2.2,-2.96636874000002));
#320242=CARTESIAN_POINT('Ctrl Pts',(-2.84009281500006,12.2,-2.96737076700001));
#320243=CARTESIAN_POINT('Ctrl Pts',(-2.84009281500006,5.2,-2.96737076700001));
#320244=CARTESIAN_POINT('Ctrl Pts',(-2.84009281500006,2.2,-2.96737076700001));
#320245=CARTESIAN_POINT('Ctrl Pts',(-2.84067885800006,12.2,-2.96837801300001));
#320246=CARTESIAN_POINT('Ctrl Pts',(-2.84067885800006,5.2,-2.96837801300001));
#320247=CARTESIAN_POINT('Ctrl Pts',(-2.84067885800006,2.2,-2.96837801300001));
#320248=CARTESIAN_POINT('Ctrl Pts',(-2.84126629500005,12.2,-2.96939047400001));
#320249=CARTESIAN_POINT('Ctrl Pts',(-2.84126629500005,5.2,-2.96939047400001));
#320250=CARTESIAN_POINT('Ctrl Pts',(-2.84126629500005,2.2,-2.96939047400001));
#320251=CARTESIAN_POINT('Ctrl Pts',(-2.84185511300006,12.2,-2.97040814900001));
#320252=CARTESIAN_POINT('Ctrl Pts',(-2.84185511300006,5.2,-2.97040814900001));
#320253=CARTESIAN_POINT('Ctrl Pts',(-2.84185511300006,2.2,-2.97040814900001));
#320254=CARTESIAN_POINT('Ctrl Pts',(-2.84244529600006,12.2,-2.97143103400002));
#320255=CARTESIAN_POINT('Ctrl Pts',(-2.84244529600006,5.2,-2.97143103400002));
#320256=CARTESIAN_POINT('Ctrl Pts',(-2.84244529600006,2.2,-2.97143103400002));
#320257=CARTESIAN_POINT('Ctrl Pts',(-2.84303682900005,12.2,-2.97245912600001));
#320258=CARTESIAN_POINT('Ctrl Pts',(-2.84303682900005,5.2,-2.97245912600001));
#320259=CARTESIAN_POINT('Ctrl Pts',(-2.84303682900005,2.2,-2.97245912600001));
#320260=CARTESIAN_POINT('Ctrl Pts',(-2.84362969700005,12.2,-2.97349242400001));
#320261=CARTESIAN_POINT('Ctrl Pts',(-2.84362969700005,5.2,-2.97349242400001));
#320262=CARTESIAN_POINT('Ctrl Pts',(-2.84362969700005,2.2,-2.97349242400001));
#320263=CARTESIAN_POINT('Ctrl Pts',(-2.84422388600006,12.2,-2.97453092400001));
#320264=CARTESIAN_POINT('Ctrl Pts',(-2.84422388600006,5.2,-2.97453092400001));
#320265=CARTESIAN_POINT('Ctrl Pts',(-2.84422388600006,2.2,-2.97453092400001));
#320266=CARTESIAN_POINT('Ctrl Pts',(-2.84481937800006,12.2,-2.97557462400002));
#320267=CARTESIAN_POINT('Ctrl Pts',(-2.84481937800006,5.2,-2.97557462400002));
#320268=CARTESIAN_POINT('Ctrl Pts',(-2.84481937800006,2.2,-2.97557462400002));
#320269=CARTESIAN_POINT('Ctrl Pts',(-2.84541616100006,12.2,-2.97662352000001));
#320270=CARTESIAN_POINT('Ctrl Pts',(-2.84541616100006,5.2,-2.97662352000001));
#320271=CARTESIAN_POINT('Ctrl Pts',(-2.84541616100006,2.2,-2.97662352000001));
#320272=CARTESIAN_POINT('Ctrl Pts',(-2.84601421800006,12.2,-2.97767761100001));
#320273=CARTESIAN_POINT('Ctrl Pts',(-2.84601421800006,5.2,-2.97767761100001));
#320274=CARTESIAN_POINT('Ctrl Pts',(-2.84601421800006,2.2,-2.97767761100001));
#320275=CARTESIAN_POINT('Ctrl Pts',(-2.84661353600006,12.2,-2.97873689300001));
#320276=CARTESIAN_POINT('Ctrl Pts',(-2.84661353600006,5.2,-2.97873689300001));
#320277=CARTESIAN_POINT('Ctrl Pts',(-2.84661353600006,2.2,-2.97873689300001));
#320278=CARTESIAN_POINT('Ctrl Pts',(-2.84721410000006,12.2,-2.97980136500001));
#320279=CARTESIAN_POINT('Ctrl Pts',(-2.84721410000006,5.2,-2.97980136500001));
#320280=CARTESIAN_POINT('Ctrl Pts',(-2.84721410000006,2.2,-2.97980136500001));
#320281=CARTESIAN_POINT('Ctrl Pts',(-2.84781589300006,12.2,-2.98087102200002));
#320282=CARTESIAN_POINT('Ctrl Pts',(-2.84781589300006,5.2,-2.98087102200002));
#320283=CARTESIAN_POINT('Ctrl Pts',(-2.84781589300006,2.2,-2.98087102200002));
#320284=CARTESIAN_POINT('Ctrl Pts',(-2.84841890200005,12.2,-2.98194586200001));
#320285=CARTESIAN_POINT('Ctrl Pts',(-2.84841890200005,5.2,-2.98194586200001));
#320286=CARTESIAN_POINT('Ctrl Pts',(-2.84841890200005,2.2,-2.98194586200001));
#320287=CARTESIAN_POINT('Ctrl Pts',(-2.84902311100006,12.2,-2.98302588300002));
#320288=CARTESIAN_POINT('Ctrl Pts',(-2.84902311100006,5.2,-2.98302588300002));
#320289=CARTESIAN_POINT('Ctrl Pts',(-2.84902311100006,2.2,-2.98302588300002));
#320290=CARTESIAN_POINT('Ctrl Pts',(-2.84962850700006,12.2,-2.98411108200002));
#320291=CARTESIAN_POINT('Ctrl Pts',(-2.84962850700006,5.2,-2.98411108200002));
#320292=CARTESIAN_POINT('Ctrl Pts',(-2.84962850700006,2.2,-2.98411108200002));
#320293=CARTESIAN_POINT('Ctrl Pts',(-2.85023507500005,12.2,-2.98520145500001));
#320294=CARTESIAN_POINT('Ctrl Pts',(-2.85023507500005,5.2,-2.98520145500001));
#320295=CARTESIAN_POINT('Ctrl Pts',(-2.85023507500005,2.2,-2.98520145500001));
#320296=CARTESIAN_POINT('Ctrl Pts',(-2.85084280000006,12.2,-2.98629699900001));
#320297=CARTESIAN_POINT('Ctrl Pts',(-2.85084280000006,5.2,-2.98629699900001));
#320298=CARTESIAN_POINT('Ctrl Pts',(-2.85084280000006,2.2,-2.98629699900001));
#320299=CARTESIAN_POINT('Ctrl Pts',(-2.85145166600006,12.2,-2.98739771400002));
#320300=CARTESIAN_POINT('Ctrl Pts',(-2.85145166600006,5.2,-2.98739771400002));
#320301=CARTESIAN_POINT('Ctrl Pts',(-2.85145166600006,2.2,-2.98739771400002));
#320302=CARTESIAN_POINT('Ctrl Pts',(-2.85206166100005,12.2,-2.98850359400001));
#320303=CARTESIAN_POINT('Ctrl Pts',(-2.85206166100005,5.2,-2.98850359400001));
#320304=CARTESIAN_POINT('Ctrl Pts',(-2.85206166100005,2.2,-2.98850359400001));
#320305=CARTESIAN_POINT('Ctrl Pts',(-2.85267276900006,12.2,-2.98961463700001));
#320306=CARTESIAN_POINT('Ctrl Pts',(-2.85267276900006,5.2,-2.98961463700001));
#320307=CARTESIAN_POINT('Ctrl Pts',(-2.85267276900006,2.2,-2.98961463700001));
#320308=CARTESIAN_POINT('Ctrl Pts',(-2.85328497500006,12.2,-2.99073084200002));
#320309=CARTESIAN_POINT('Ctrl Pts',(-2.85328497500006,5.2,-2.99073084200002));
#320310=CARTESIAN_POINT('Ctrl Pts',(-2.85328497500006,2.2,-2.99073084200002));
#320311=CARTESIAN_POINT('Ctrl Pts',(-2.85389826500006,12.2,-2.99185220200001));
#320312=CARTESIAN_POINT('Ctrl Pts',(-2.85389826500006,5.2,-2.99185220200001));
#320313=CARTESIAN_POINT('Ctrl Pts',(-2.85389826500006,2.2,-2.99185220200001));
#320314=CARTESIAN_POINT('Ctrl Pts',(-2.85451262500006,12.2,-2.99297871900002));
#320315=CARTESIAN_POINT('Ctrl Pts',(-2.85451262500006,5.2,-2.99297871900002));
#320316=CARTESIAN_POINT('Ctrl Pts',(-2.85451262500006,2.2,-2.99297871900002));
#320317=CARTESIAN_POINT('Ctrl Pts',(-2.85512804100006,12.2,-2.99411038700002));
#320318=CARTESIAN_POINT('Ctrl Pts',(-2.85512804100006,5.2,-2.99411038700002));
#320319=CARTESIAN_POINT('Ctrl Pts',(-2.85512804100006,2.2,-2.99411038700002));
#320320=CARTESIAN_POINT('Ctrl Pts',(-2.85574449800006,12.2,-2.99524720400001));
#320321=CARTESIAN_POINT('Ctrl Pts',(-2.85574449800006,5.2,-2.99524720400001));
#320322=CARTESIAN_POINT('Ctrl Pts',(-2.85574449800006,2.2,-2.99524720400001));
#320323=CARTESIAN_POINT('Ctrl Pts',(-2.85636198200006,12.2,-2.99638916700002));
#320324=CARTESIAN_POINT('Ctrl Pts',(-2.85636198200006,5.2,-2.99638916700002));
#320325=CARTESIAN_POINT('Ctrl Pts',(-2.85636198200006,2.2,-2.99638916700002));
#320326=CARTESIAN_POINT('Ctrl Pts',(-2.85698047800006,12.2,-2.99753627200001));
#320327=CARTESIAN_POINT('Ctrl Pts',(-2.85698047800006,5.2,-2.99753627200001));
#320328=CARTESIAN_POINT('Ctrl Pts',(-2.85698047800006,2.2,-2.99753627200001));
#320329=CARTESIAN_POINT('Ctrl Pts',(-2.85759997200006,12.2,-2.99868851700001));
#320330=CARTESIAN_POINT('Ctrl Pts',(-2.85759997200006,5.2,-2.99868851700001));
#320331=CARTESIAN_POINT('Ctrl Pts',(-2.85759997200006,2.2,-2.99868851700001));
#320332=CARTESIAN_POINT('Ctrl Pts',(-2.85822045100006,12.2,-2.99984590000001));
#320333=CARTESIAN_POINT('Ctrl Pts',(-2.85822045100006,5.2,-2.99984590000001));
#320334=CARTESIAN_POINT('Ctrl Pts',(-2.85822045100006,2.2,-2.99984590000001));
#320335=CARTESIAN_POINT('Ctrl Pts',(-2.85884189900006,12.2,-3.00100841600001));
#320336=CARTESIAN_POINT('Ctrl Pts',(-2.85884189900006,5.2,-3.00100841600001));
#320337=CARTESIAN_POINT('Ctrl Pts',(-2.85884189900006,2.2,-3.00100841600001));
#320338=CARTESIAN_POINT('Ctrl Pts',(-2.85946430300006,12.2,-3.00217606300002));
#320339=CARTESIAN_POINT('Ctrl Pts',(-2.85946430300006,5.2,-3.00217606300002));
#320340=CARTESIAN_POINT('Ctrl Pts',(-2.85946430300006,2.2,-3.00217606300002));
#320341=CARTESIAN_POINT('Ctrl Pts',(-2.86008764900005,12.2,-3.00334883900002));
#320342=CARTESIAN_POINT('Ctrl Pts',(-2.86008764900005,5.2,-3.00334883900002));
#320343=CARTESIAN_POINT('Ctrl Pts',(-2.86008764900005,2.2,-3.00334883900002));
#320344=CARTESIAN_POINT('Ctrl Pts',(-2.86071192200006,12.2,-3.00452673900002));
#320345=CARTESIAN_POINT('Ctrl Pts',(-2.86071192200006,5.2,-3.00452673900002));
#320346=CARTESIAN_POINT('Ctrl Pts',(-2.86071192200006,2.2,-3.00452673900002));
#320347=CARTESIAN_POINT('Ctrl Pts',(-2.86133710900006,12.2,-3.00570976000001));
#320348=CARTESIAN_POINT('Ctrl Pts',(-2.86133710900006,5.2,-3.00570976000001));
#320349=CARTESIAN_POINT('Ctrl Pts',(-2.86133710900006,2.2,-3.00570976000001));
#320350=CARTESIAN_POINT('Ctrl Pts',(-2.86196319600006,12.2,-3.00689790100002));
#320351=CARTESIAN_POINT('Ctrl Pts',(-2.86196319600006,5.2,-3.00689790100002));
#320352=CARTESIAN_POINT('Ctrl Pts',(-2.86196319600006,2.2,-3.00689790100002));
#320353=CARTESIAN_POINT('Ctrl Pts',(-2.86259016800006,12.2,-3.00809115700002));
#320354=CARTESIAN_POINT('Ctrl Pts',(-2.86259016800006,5.2,-3.00809115700002));
#320355=CARTESIAN_POINT('Ctrl Pts',(-2.86259016800006,2.2,-3.00809115700002));
#320356=CARTESIAN_POINT('Ctrl Pts',(-2.86321801200006,12.2,-3.00928952600001));
#320357=CARTESIAN_POINT('Ctrl Pts',(-2.86321801200006,5.2,-3.00928952600001));
#320358=CARTESIAN_POINT('Ctrl Pts',(-2.86321801200006,2.2,-3.00928952600001));
#320359=CARTESIAN_POINT('Ctrl Pts',(-2.86384671300006,12.2,-3.01049300400001));
#320360=CARTESIAN_POINT('Ctrl Pts',(-2.86384671300006,5.2,-3.01049300400001));
#320361=CARTESIAN_POINT('Ctrl Pts',(-2.86384671300006,2.2,-3.01049300400001));
#320362=CARTESIAN_POINT('Ctrl Pts',(-2.86447625900006,12.2,-3.01170158900002));
#320363=CARTESIAN_POINT('Ctrl Pts',(-2.86447625900006,5.2,-3.01170158900002));
#320364=CARTESIAN_POINT('Ctrl Pts',(-2.86447625900006,2.2,-3.01170158900002));
#320365=CARTESIAN_POINT('Ctrl Pts',(-2.86510663400006,12.2,-3.01291527700001));
#320366=CARTESIAN_POINT('Ctrl Pts',(-2.86510663400006,5.2,-3.01291527700001));
#320367=CARTESIAN_POINT('Ctrl Pts',(-2.86510663400006,2.2,-3.01291527700001));
#320368=CARTESIAN_POINT('Ctrl Pts',(-2.86573782700006,12.2,-3.01413406600001));
#320369=CARTESIAN_POINT('Ctrl Pts',(-2.86573782700006,5.2,-3.01413406600001));
#320370=CARTESIAN_POINT('Ctrl Pts',(-2.86573782700006,2.2,-3.01413406600001));
#320371=CARTESIAN_POINT('Ctrl Pts',(-2.86636982100006,12.2,-3.01535795100001));
#320372=CARTESIAN_POINT('Ctrl Pts',(-2.86636982100006,5.2,-3.01535795100001));
#320373=CARTESIAN_POINT('Ctrl Pts',(-2.86636982100006,2.2,-3.01535795100001));
#320374=CARTESIAN_POINT('Ctrl Pts',(-2.86700260500006,12.2,-3.01658693000002));
#320375=CARTESIAN_POINT('Ctrl Pts',(-2.86700260500006,5.2,-3.01658693000002));
#320376=CARTESIAN_POINT('Ctrl Pts',(-2.86700260500006,2.2,-3.01658693000002));
#320377=CARTESIAN_POINT('Ctrl Pts',(-2.86763616300005,12.2,-3.01782100100001));
#320378=CARTESIAN_POINT('Ctrl Pts',(-2.86763616300005,5.2,-3.01782100100001));
#320379=CARTESIAN_POINT('Ctrl Pts',(-2.86763616300005,2.2,-3.01782100100001));
#320380=CARTESIAN_POINT('Ctrl Pts',(-2.86827048300006,12.2,-3.01906015800002));
#320381=CARTESIAN_POINT('Ctrl Pts',(-2.86827048300006,5.2,-3.01906015800002));
#320382=CARTESIAN_POINT('Ctrl Pts',(-2.86827048300006,2.2,-3.01906015800002));
#320383=CARTESIAN_POINT('Ctrl Pts',(-2.86890555100006,12.2,-3.02030440000001));
#320384=CARTESIAN_POINT('Ctrl Pts',(-2.86890555100006,5.2,-3.02030440000001));
#320385=CARTESIAN_POINT('Ctrl Pts',(-2.86890555100006,2.2,-3.02030440000001));
#320386=CARTESIAN_POINT('Ctrl Pts',(-2.86954135300005,12.2,-3.02155372400001));
#320387=CARTESIAN_POINT('Ctrl Pts',(-2.86954135300005,5.2,-3.02155372400001));
#320388=CARTESIAN_POINT('Ctrl Pts',(-2.86954135300005,2.2,-3.02155372400001));
#320389=CARTESIAN_POINT('Ctrl Pts',(-2.87017787600006,12.2,-3.02280812500001));
#320390=CARTESIAN_POINT('Ctrl Pts',(-2.87017787600006,5.2,-3.02280812500001));
#320391=CARTESIAN_POINT('Ctrl Pts',(-2.87017787600006,2.2,-3.02280812500001));
#320392=CARTESIAN_POINT('Ctrl Pts',(-2.87081510600005,12.2,-3.02406760100002));
#320393=CARTESIAN_POINT('Ctrl Pts',(-2.87081510600005,5.2,-3.02406760100002));
#320394=CARTESIAN_POINT('Ctrl Pts',(-2.87081510600005,2.2,-3.02406760100002));
#320395=CARTESIAN_POINT('Ctrl Pts',(-2.87145303000006,12.2,-3.02533214800001));
#320396=CARTESIAN_POINT('Ctrl Pts',(-2.87145303000006,5.2,-3.02533214800001));
#320397=CARTESIAN_POINT('Ctrl Pts',(-2.87145303000006,2.2,-3.02533214800001));
#320398=CARTESIAN_POINT('Ctrl Pts',(-2.87209163400005,12.2,-3.02660176500002));
#320399=CARTESIAN_POINT('Ctrl Pts',(-2.87209163400005,5.2,-3.02660176500002));
#320400=CARTESIAN_POINT('Ctrl Pts',(-2.87209163400005,2.2,-3.02660176500002));
#320401=CARTESIAN_POINT('Ctrl Pts',(-2.87273090500006,12.2,-3.02787644600001));
#320402=CARTESIAN_POINT('Ctrl Pts',(-2.87273090500006,5.2,-3.02787644600001));
#320403=CARTESIAN_POINT('Ctrl Pts',(-2.87273090500006,2.2,-3.02787644600001));
#320404=CARTESIAN_POINT('Ctrl Pts',(-2.87337083000006,12.2,-3.02915618800002));
#320405=CARTESIAN_POINT('Ctrl Pts',(-2.87337083000006,5.2,-3.02915618800002));
#320406=CARTESIAN_POINT('Ctrl Pts',(-2.87337083000006,2.2,-3.02915618800002));
#320407=CARTESIAN_POINT('Ctrl Pts',(-2.87401139300006,12.2,-3.03044099000001));
#320408=CARTESIAN_POINT('Ctrl Pts',(-2.87401139300006,5.2,-3.03044099000001));
#320409=CARTESIAN_POINT('Ctrl Pts',(-2.87401139300006,2.2,-3.03044099000001));
#320410=CARTESIAN_POINT('Ctrl Pts',(-2.87465258400006,12.2,-3.03173084600001));
#320411=CARTESIAN_POINT('Ctrl Pts',(-2.87465258400006,5.2,-3.03173084600001));
#320412=CARTESIAN_POINT('Ctrl Pts',(-2.87465258400006,2.2,-3.03173084600001));
#320413=CARTESIAN_POINT('Ctrl Pts',(-2.87529438900005,12.2,-3.03302575500001));
#320414=CARTESIAN_POINT('Ctrl Pts',(-2.87529438900005,5.2,-3.03302575500001));
#320415=CARTESIAN_POINT('Ctrl Pts',(-2.87529438900005,2.2,-3.03302575500001));
#320416=CARTESIAN_POINT('Ctrl Pts',(-2.87593679400006,12.2,-3.03432571200001));
#320417=CARTESIAN_POINT('Ctrl Pts',(-2.87593679400006,5.2,-3.03432571200001));
#320418=CARTESIAN_POINT('Ctrl Pts',(-2.87593679400006,2.2,-3.03432571200001));
#320419=CARTESIAN_POINT('Ctrl Pts',(-2.87657978500006,12.2,-3.03563071500002));
#320420=CARTESIAN_POINT('Ctrl Pts',(-2.87657978500006,5.2,-3.03563071500002));
#320421=CARTESIAN_POINT('Ctrl Pts',(-2.87657978500006,2.2,-3.03563071500002));
#320422=CARTESIAN_POINT('Ctrl Pts',(-2.87722335000006,12.2,-3.03694075900002));
#320423=CARTESIAN_POINT('Ctrl Pts',(-2.87722335000006,5.2,-3.03694075900002));
#320424=CARTESIAN_POINT('Ctrl Pts',(-2.87722335000006,2.2,-3.03694075900002));
#320425=CARTESIAN_POINT('Ctrl Pts',(-2.87786747600005,12.2,-3.03825584200001));
#320426=CARTESIAN_POINT('Ctrl Pts',(-2.87786747600005,5.2,-3.03825584200001));
#320427=CARTESIAN_POINT('Ctrl Pts',(-2.87786747600005,2.2,-3.03825584200001));
#320428=CARTESIAN_POINT('Ctrl Pts',(-2.87851214900006,12.2,-3.03957596100001));
#320429=CARTESIAN_POINT('Ctrl Pts',(-2.87851214900006,5.2,-3.03957596100001));
#320430=CARTESIAN_POINT('Ctrl Pts',(-2.87851214900006,2.2,-3.03957596100001));
#320431=CARTESIAN_POINT('Ctrl Pts',(-2.87915735600006,12.2,-3.04090111200002));
#320432=CARTESIAN_POINT('Ctrl Pts',(-2.87915735600006,5.2,-3.04090111200002));
#320433=CARTESIAN_POINT('Ctrl Pts',(-2.87915735600006,2.2,-3.04090111200002));
#320434=CARTESIAN_POINT('Ctrl Pts',(-2.87980308500006,12.2,-3.04223129000002));
#320435=CARTESIAN_POINT('Ctrl Pts',(-2.87980308500006,5.2,-3.04223129000002));
#320436=CARTESIAN_POINT('Ctrl Pts',(-2.87980308500006,2.2,-3.04223129000002));
#320437=CARTESIAN_POINT('Ctrl Pts',(-2.88044932200005,12.2,-3.04356649500001));
#320438=CARTESIAN_POINT('Ctrl Pts',(-2.88044932200005,5.2,-3.04356649500001));
#320439=CARTESIAN_POINT('Ctrl Pts',(-2.88044932200005,2.2,-3.04356649500001));
#320440=CARTESIAN_POINT('Ctrl Pts',(-2.88109605400006,12.2,-3.04490672100002));
#320441=CARTESIAN_POINT('Ctrl Pts',(-2.88109605400006,5.2,-3.04490672100002));
#320442=CARTESIAN_POINT('Ctrl Pts',(-2.88109605400006,2.2,-3.04490672100002));
#320443=CARTESIAN_POINT('Ctrl Pts',(-2.88174326800006,12.2,-3.04625196600002));
#320444=CARTESIAN_POINT('Ctrl Pts',(-2.88174326800006,5.2,-3.04625196600002));
#320445=CARTESIAN_POINT('Ctrl Pts',(-2.88174326800006,2.2,-3.04625196600002));
#320446=CARTESIAN_POINT('Ctrl Pts',(-2.88239095100006,12.2,-3.04760222600001));
#320447=CARTESIAN_POINT('Ctrl Pts',(-2.88239095100006,5.2,-3.04760222600001));
#320448=CARTESIAN_POINT('Ctrl Pts',(-2.88239095100006,2.2,-3.04760222600001));
#320449=CARTESIAN_POINT('Ctrl Pts',(-2.88303909100006,12.2,-3.04895749700002));
#320450=CARTESIAN_POINT('Ctrl Pts',(-2.88303909100006,5.2,-3.04895749700002));
#320451=CARTESIAN_POINT('Ctrl Pts',(-2.88303909100006,2.2,-3.04895749700002));
#320452=CARTESIAN_POINT('Ctrl Pts',(-2.88368767300006,12.2,-3.05031777600002));
#320453=CARTESIAN_POINT('Ctrl Pts',(-2.88368767300006,5.2,-3.05031777600002));
#320454=CARTESIAN_POINT('Ctrl Pts',(-2.88368767300006,2.2,-3.05031777600002));
#320455=CARTESIAN_POINT('Ctrl Pts',(-2.88433668700006,12.2,-3.05168306000001));
#320456=CARTESIAN_POINT('Ctrl Pts',(-2.88433668700006,5.2,-3.05168306000001));
#320457=CARTESIAN_POINT('Ctrl Pts',(-2.88433668700006,2.2,-3.05168306000001));
#320458=CARTESIAN_POINT('Ctrl Pts',(-2.88498611800006,12.2,-3.05305334600002));
#320459=CARTESIAN_POINT('Ctrl Pts',(-2.88498611800006,5.2,-3.05305334600002));
#320460=CARTESIAN_POINT('Ctrl Pts',(-2.88498611800006,2.2,-3.05305334600002));
#320461=CARTESIAN_POINT('Ctrl Pts',(-2.88563595400006,12.2,-3.05442862900001));
#320462=CARTESIAN_POINT('Ctrl Pts',(-2.88563595400006,5.2,-3.05442862900001));
#320463=CARTESIAN_POINT('Ctrl Pts',(-2.88563595400006,2.2,-3.05442862900001));
#320464=CARTESIAN_POINT('Ctrl Pts',(-2.88628618200006,12.2,-3.05580890700002));
#320465=CARTESIAN_POINT('Ctrl Pts',(-2.88628618200006,5.2,-3.05580890700002));
#320466=CARTESIAN_POINT('Ctrl Pts',(-2.88628618200006,2.2,-3.05580890700002));
#320467=CARTESIAN_POINT('Ctrl Pts',(-2.88693679000006,12.2,-3.05719417500002));
#320468=CARTESIAN_POINT('Ctrl Pts',(-2.88693679000006,5.2,-3.05719417500002));
#320469=CARTESIAN_POINT('Ctrl Pts',(-2.88693679000006,2.2,-3.05719417500002));
#320470=CARTESIAN_POINT('Ctrl Pts',(-2.88758776400006,12.2,-3.05858443100002));
#320471=CARTESIAN_POINT('Ctrl Pts',(-2.88758776400006,5.2,-3.05858443100002));
#320472=CARTESIAN_POINT('Ctrl Pts',(-2.88758776400006,2.2,-3.05858443100002));
#320473=CARTESIAN_POINT('Ctrl Pts',(-2.88823909200006,12.2,-3.05997967000001));
#320474=CARTESIAN_POINT('Ctrl Pts',(-2.88823909200006,5.2,-3.05997967000001));
#320475=CARTESIAN_POINT('Ctrl Pts',(-2.88823909200006,2.2,-3.05997967000001));
#320476=CARTESIAN_POINT('Ctrl Pts',(-2.88889076200006,12.2,-3.06137989000002));
#320477=CARTESIAN_POINT('Ctrl Pts',(-2.88889076200006,5.2,-3.06137989000002));
#320478=CARTESIAN_POINT('Ctrl Pts',(-2.88889076200006,2.2,-3.06137989000002));
#320479=CARTESIAN_POINT('Ctrl Pts',(-2.88954276000006,12.2,-3.06278508700002));
#320480=CARTESIAN_POINT('Ctrl Pts',(-2.88954276000006,5.2,-3.06278508700002));
#320481=CARTESIAN_POINT('Ctrl Pts',(-2.88954276000006,2.2,-3.06278508700002));
#320482=CARTESIAN_POINT('Ctrl Pts',(-2.89019507400006,12.2,-3.06419525700001));
#320483=CARTESIAN_POINT('Ctrl Pts',(-2.89019507400006,5.2,-3.06419525700001));
#320484=CARTESIAN_POINT('Ctrl Pts',(-2.89019507400006,2.2,-3.06419525700001));
#320485=CARTESIAN_POINT('Ctrl Pts',(-2.89084769200006,12.2,-3.06561039700001));
#320486=CARTESIAN_POINT('Ctrl Pts',(-2.89084769200006,5.2,-3.06561039700001));
#320487=CARTESIAN_POINT('Ctrl Pts',(-2.89084769200006,2.2,-3.06561039700001));
#320488=CARTESIAN_POINT('Ctrl Pts',(-2.89150060100006,12.2,-3.06703050300001));
#320489=CARTESIAN_POINT('Ctrl Pts',(-2.89150060100006,5.2,-3.06703050300001));
#320490=CARTESIAN_POINT('Ctrl Pts',(-2.89150060100006,2.2,-3.06703050300001));
#320491=CARTESIAN_POINT('Ctrl Pts',(-2.89215378800006,12.2,-3.06845557200001));
#320492=CARTESIAN_POINT('Ctrl Pts',(-2.89215378800006,5.2,-3.06845557200001));
#320493=CARTESIAN_POINT('Ctrl Pts',(-2.89215378800006,2.2,-3.06845557200001));
#320494=CARTESIAN_POINT('Ctrl Pts',(-2.89280724100006,12.2,-3.06988560000002));
#320495=CARTESIAN_POINT('Ctrl Pts',(-2.89280724100006,5.2,-3.06988560000002));
#320496=CARTESIAN_POINT('Ctrl Pts',(-2.89280724100006,2.2,-3.06988560000002));
#320497=CARTESIAN_POINT('Ctrl Pts',(-2.89346094900006,12.2,-3.07132058300001));
#320498=CARTESIAN_POINT('Ctrl Pts',(-2.89346094900006,5.2,-3.07132058300001));
#320499=CARTESIAN_POINT('Ctrl Pts',(-2.89346094900006,2.2,-3.07132058300001));
#320500=CARTESIAN_POINT('Ctrl Pts',(-2.89411489600006,12.2,-3.07276051900002));
#320501=CARTESIAN_POINT('Ctrl Pts',(-2.89411489600006,5.2,-3.07276051900002));
#320502=CARTESIAN_POINT('Ctrl Pts',(-2.89411489600006,2.2,-3.07276051900002));
#320503=CARTESIAN_POINT('Ctrl Pts',(-2.89476907300006,12.2,-3.07420540200001));
#320504=CARTESIAN_POINT('Ctrl Pts',(-2.89476907300006,5.2,-3.07420540200001));
#320505=CARTESIAN_POINT('Ctrl Pts',(-2.89476907300006,2.2,-3.07420540200001));
#320506=CARTESIAN_POINT('Ctrl Pts',(-2.89542346700005,12.2,-3.07565523000001));
#320507=CARTESIAN_POINT('Ctrl Pts',(-2.89542346700005,5.2,-3.07565523000001));
#320508=CARTESIAN_POINT('Ctrl Pts',(-2.89542346700005,2.2,-3.07565523000001));
#320509=CARTESIAN_POINT('Ctrl Pts',(-2.89607806400006,12.2,-3.07711000000001));
#320510=CARTESIAN_POINT('Ctrl Pts',(-2.89607806400006,5.2,-3.07711000000001));
#320511=CARTESIAN_POINT('Ctrl Pts',(-2.89607806400006,2.2,-3.07711000000001));
#320512=CARTESIAN_POINT('Ctrl Pts',(-2.89673285300006,12.2,-3.07856970600001));
#320513=CARTESIAN_POINT('Ctrl Pts',(-2.89673285300006,5.2,-3.07856970600001));
#320514=CARTESIAN_POINT('Ctrl Pts',(-2.89673285300006,2.2,-3.07856970600001));
#320515=CARTESIAN_POINT('Ctrl Pts',(-2.89738782100006,12.2,-3.08003434700002));
#320516=CARTESIAN_POINT('Ctrl Pts',(-2.89738782100006,5.2,-3.08003434700002));
#320517=CARTESIAN_POINT('Ctrl Pts',(-2.89738782100006,2.2,-3.08003434700002));
#320518=CARTESIAN_POINT('Ctrl Pts',(-2.89804295700006,12.2,-3.08150391700002));
#320519=CARTESIAN_POINT('Ctrl Pts',(-2.89804295700006,5.2,-3.08150391700002));
#320520=CARTESIAN_POINT('Ctrl Pts',(-2.89804295700006,2.2,-3.08150391700002));
#320521=CARTESIAN_POINT('Ctrl Pts',(-2.89869824800005,12.2,-3.08297841400002));
#320522=CARTESIAN_POINT('Ctrl Pts',(-2.89869824800005,5.2,-3.08297841400002));
#320523=CARTESIAN_POINT('Ctrl Pts',(-2.89869824800005,2.2,-3.08297841400002));
#320524=CARTESIAN_POINT('Ctrl Pts',(-2.89935368200006,12.2,-3.08445783500002));
#320525=CARTESIAN_POINT('Ctrl Pts',(-2.89935368200006,5.2,-3.08445783500002));
#320526=CARTESIAN_POINT('Ctrl Pts',(-2.89935368200006,2.2,-3.08445783500002));
#320527=CARTESIAN_POINT('Ctrl Pts',(-2.90000924700006,12.2,-3.08594217400001));
#320528=CARTESIAN_POINT('Ctrl Pts',(-2.90000924700006,5.2,-3.08594217400001));
#320529=CARTESIAN_POINT('Ctrl Pts',(-2.90000924700006,2.2,-3.08594217400001));
#320530=CARTESIAN_POINT('Ctrl Pts',(-2.90066492900006,12.2,-3.08743142800001));
#320531=CARTESIAN_POINT('Ctrl Pts',(-2.90066492900006,5.2,-3.08743142800001));
#320532=CARTESIAN_POINT('Ctrl Pts',(-2.90066492900006,2.2,-3.08743142800001));
#320533=CARTESIAN_POINT('Ctrl Pts',(-2.90132071900006,12.2,-3.08892559500002));
#320534=CARTESIAN_POINT('Ctrl Pts',(-2.90132071900006,5.2,-3.08892559500002));
#320535=CARTESIAN_POINT('Ctrl Pts',(-2.90132071900006,2.2,-3.08892559500002));
#320536=CARTESIAN_POINT('Ctrl Pts',(-2.90197660300006,12.2,-3.09042467000001));
#320537=CARTESIAN_POINT('Ctrl Pts',(-2.90197660300006,5.2,-3.09042467000001));
#320538=CARTESIAN_POINT('Ctrl Pts',(-2.90197660300006,2.2,-3.09042467000001));
#320539=CARTESIAN_POINT('Ctrl Pts',(-2.90263256900006,12.2,-3.09192864800002));
#320540=CARTESIAN_POINT('Ctrl Pts',(-2.90263256900006,5.2,-3.09192864800002));
#320541=CARTESIAN_POINT('Ctrl Pts',(-2.90263256900006,2.2,-3.09192864800002));
#320542=CARTESIAN_POINT('Ctrl Pts',(-2.90328860500006,12.2,-3.09343752800002));
#320543=CARTESIAN_POINT('Ctrl Pts',(-2.90328860500006,5.2,-3.09343752800002));
#320544=CARTESIAN_POINT('Ctrl Pts',(-2.90328860500006,2.2,-3.09343752800002));
#320545=CARTESIAN_POINT('Ctrl Pts',(-2.90394470100006,12.2,-3.09495130400002));
#320546=CARTESIAN_POINT('Ctrl Pts',(-2.90394470100006,5.2,-3.09495130400002));
#320547=CARTESIAN_POINT('Ctrl Pts',(-2.90394470100006,2.2,-3.09495130400002));
#320548=CARTESIAN_POINT('Ctrl Pts',(-2.90460084100005,12.2,-3.09646997400002));
#320549=CARTESIAN_POINT('Ctrl Pts',(-2.90460084100005,5.2,-3.09646997400002));
#320550=CARTESIAN_POINT('Ctrl Pts',(-2.90460084100005,2.2,-3.09646997400002));
#320551=CARTESIAN_POINT('Ctrl Pts',(-2.90525701700005,12.2,-3.09799353300001));
#320552=CARTESIAN_POINT('Ctrl Pts',(-2.90525701700005,5.2,-3.09799353300001));
#320553=CARTESIAN_POINT('Ctrl Pts',(-2.90525701700005,2.2,-3.09799353300001));
#320554=CARTESIAN_POINT('Ctrl Pts',(-2.90591321500006,12.2,-3.09952197700001));
#320555=CARTESIAN_POINT('Ctrl Pts',(-2.90591321500006,5.2,-3.09952197700001));
#320556=CARTESIAN_POINT('Ctrl Pts',(-2.90591321500006,2.2,-3.09952197700001));
#320557=CARTESIAN_POINT('Ctrl Pts',(-2.90656942400005,12.2,-3.10105530400001));
#320558=CARTESIAN_POINT('Ctrl Pts',(-2.90656942400005,5.2,-3.10105530400001));
#320559=CARTESIAN_POINT('Ctrl Pts',(-2.90656942400005,2.2,-3.10105530400001));
#320560=CARTESIAN_POINT('Ctrl Pts',(-2.90722563100006,12.2,-3.10259350800001));
#320561=CARTESIAN_POINT('Ctrl Pts',(-2.90722563100006,5.2,-3.10259350800001));
#320562=CARTESIAN_POINT('Ctrl Pts',(-2.90722563100006,2.2,-3.10259350800001));
#320563=CARTESIAN_POINT('Ctrl Pts',(-2.90788182600005,12.2,-3.10413658700002));
#320564=CARTESIAN_POINT('Ctrl Pts',(-2.90788182600005,5.2,-3.10413658700002));
#320565=CARTESIAN_POINT('Ctrl Pts',(-2.90788182600005,2.2,-3.10413658700002));
#320566=CARTESIAN_POINT('Ctrl Pts',(-2.90853799500006,12.2,-3.10568453500002));
#320567=CARTESIAN_POINT('Ctrl Pts',(-2.90853799500006,5.2,-3.10568453500002));
#320568=CARTESIAN_POINT('Ctrl Pts',(-2.90853799500006,2.2,-3.10568453500002));
#320569=CARTESIAN_POINT('Ctrl Pts',(-2.90919412800006,12.2,-3.10723735200002));
#320570=CARTESIAN_POINT('Ctrl Pts',(-2.90919412800006,5.2,-3.10723735200002));
#320571=CARTESIAN_POINT('Ctrl Pts',(-2.90919412800006,2.2,-3.10723735200002));
#320572=CARTESIAN_POINT('Ctrl Pts',(-2.90985021200005,12.2,-3.10879503100002));
#320573=CARTESIAN_POINT('Ctrl Pts',(-2.90985021200005,5.2,-3.10879503100002));
#320574=CARTESIAN_POINT('Ctrl Pts',(-2.90985021200005,2.2,-3.10879503100002));
#320575=CARTESIAN_POINT('Ctrl Pts',(-2.91050623700006,12.2,-3.11035756900001));
#320576=CARTESIAN_POINT('Ctrl Pts',(-2.91050623700006,5.2,-3.11035756900001));
#320577=CARTESIAN_POINT('Ctrl Pts',(-2.91050623700006,2.2,-3.11035756900001));
#320578=CARTESIAN_POINT('Ctrl Pts',(-2.91116218900005,12.2,-3.11192496300002));
#320579=CARTESIAN_POINT('Ctrl Pts',(-2.91116218900005,5.2,-3.11192496300002));
#320580=CARTESIAN_POINT('Ctrl Pts',(-2.91116218900005,2.2,-3.11192496300002));
#320581=CARTESIAN_POINT('Ctrl Pts',(-2.91181805800006,12.2,-3.11349720700001));
#320582=CARTESIAN_POINT('Ctrl Pts',(-2.91181805800006,5.2,-3.11349720700001));
#320583=CARTESIAN_POINT('Ctrl Pts',(-2.91181805800006,2.2,-3.11349720700001));
#320584=CARTESIAN_POINT('Ctrl Pts',(-2.91247383300006,12.2,-3.11507429900002));
#320585=CARTESIAN_POINT('Ctrl Pts',(-2.91247383300006,5.2,-3.11507429900002));
#320586=CARTESIAN_POINT('Ctrl Pts',(-2.91247383300006,2.2,-3.11507429900002));
#320587=CARTESIAN_POINT('Ctrl Pts',(-2.91312949900006,12.2,-3.11665623500001));
#320588=CARTESIAN_POINT('Ctrl Pts',(-2.91312949900006,5.2,-3.11665623500001));
#320589=CARTESIAN_POINT('Ctrl Pts',(-2.91312949900006,2.2,-3.11665623500001));
#320590=CARTESIAN_POINT('Ctrl Pts',(-2.91378504800006,12.2,-3.11824301100001));
#320591=CARTESIAN_POINT('Ctrl Pts',(-2.91378504800006,5.2,-3.11824301100001));
#320592=CARTESIAN_POINT('Ctrl Pts',(-2.91378504800006,2.2,-3.11824301100001));
#320593=CARTESIAN_POINT('Ctrl Pts',(-2.91444046800006,12.2,-3.11983462300002));
#320594=CARTESIAN_POINT('Ctrl Pts',(-2.91444046800006,5.2,-3.11983462300002));
#320595=CARTESIAN_POINT('Ctrl Pts',(-2.91444046800006,2.2,-3.11983462300002));
#320596=CARTESIAN_POINT('Ctrl Pts',(-2.91509574500005,12.2,-3.12143106700002));
#320597=CARTESIAN_POINT('Ctrl Pts',(-2.91509574500005,5.2,-3.12143106700002));
#320598=CARTESIAN_POINT('Ctrl Pts',(-2.91509574500005,2.2,-3.12143106700002));
#320599=CARTESIAN_POINT('Ctrl Pts',(-2.91575086900006,12.2,-3.12303233800002));
#320600=CARTESIAN_POINT('Ctrl Pts',(-2.91575086900006,5.2,-3.12303233800002));
#320601=CARTESIAN_POINT('Ctrl Pts',(-2.91575086900006,2.2,-3.12303233800002));
#320602=CARTESIAN_POINT('Ctrl Pts',(-2.91640583000006,12.2,-3.12463843500002));
#320603=CARTESIAN_POINT('Ctrl Pts',(-2.91640583000006,5.2,-3.12463843500002));
#320604=CARTESIAN_POINT('Ctrl Pts',(-2.91640583000006,2.2,-3.12463843500002));
#320605=CARTESIAN_POINT('Ctrl Pts',(-2.91706061400005,12.2,-3.12624935200001));
#320606=CARTESIAN_POINT('Ctrl Pts',(-2.91706061400005,5.2,-3.12624935200001));
#320607=CARTESIAN_POINT('Ctrl Pts',(-2.91706061400005,2.2,-3.12624935200001));
#320608=CARTESIAN_POINT('Ctrl Pts',(-2.91771521100006,12.2,-3.12786508500002));
#320609=CARTESIAN_POINT('Ctrl Pts',(-2.91771521100006,5.2,-3.12786508500002));
#320610=CARTESIAN_POINT('Ctrl Pts',(-2.91771521100006,2.2,-3.12786508500002));
#320611=CARTESIAN_POINT('Ctrl Pts',(-2.91836961000006,12.2,-3.12948563000001));
#320612=CARTESIAN_POINT('Ctrl Pts',(-2.91836961000006,5.2,-3.12948563000001));
#320613=CARTESIAN_POINT('Ctrl Pts',(-2.91836961000006,2.2,-3.12948563000001));
#320614=CARTESIAN_POINT('Ctrl Pts',(-2.91902379700006,12.2,-3.13111098500002));
#320615=CARTESIAN_POINT('Ctrl Pts',(-2.91902379700006,5.2,-3.13111098500002));
#320616=CARTESIAN_POINT('Ctrl Pts',(-2.91902379700006,2.2,-3.13111098500002));
#320617=CARTESIAN_POINT('Ctrl Pts',(-2.91967776400006,12.2,-3.13274114400001));
#320618=CARTESIAN_POINT('Ctrl Pts',(-2.91967776400006,5.2,-3.13274114400001));
#320619=CARTESIAN_POINT('Ctrl Pts',(-2.91967776400006,2.2,-3.13274114400001));
#320620=CARTESIAN_POINT('Ctrl Pts',(-2.92033149900006,12.2,-3.13437610400001));
#320621=CARTESIAN_POINT('Ctrl Pts',(-2.92033149900006,5.2,-3.13437610400001));
#320622=CARTESIAN_POINT('Ctrl Pts',(-2.92033149900006,2.2,-3.13437610400001));
#320623=CARTESIAN_POINT('Ctrl Pts',(-2.92098498800006,12.2,-3.13601586100001));
#320624=CARTESIAN_POINT('Ctrl Pts',(-2.92098498800006,5.2,-3.13601586100001));
#320625=CARTESIAN_POINT('Ctrl Pts',(-2.92098498800006,2.2,-3.13601586100001));
#320626=CARTESIAN_POINT('Ctrl Pts',(-2.92163822300005,12.2,-3.13766041000001));
#320627=CARTESIAN_POINT('Ctrl Pts',(-2.92163822300005,5.2,-3.13766041000001));
#320628=CARTESIAN_POINT('Ctrl Pts',(-2.92163822300005,2.2,-3.13766041000001));
#320629=CARTESIAN_POINT('Ctrl Pts',(-2.92229119100006,12.2,-3.13930974800002));
#320630=CARTESIAN_POINT('Ctrl Pts',(-2.92229119100006,5.2,-3.13930974800002));
#320631=CARTESIAN_POINT('Ctrl Pts',(-2.92229119100006,2.2,-3.13930974800002));
#320632=CARTESIAN_POINT('Ctrl Pts',(-2.92294388100005,12.2,-3.14096387100002));
#320633=CARTESIAN_POINT('Ctrl Pts',(-2.92294388100005,5.2,-3.14096387100002));
#320634=CARTESIAN_POINT('Ctrl Pts',(-2.92294388100005,2.2,-3.14096387100002));
#320635=CARTESIAN_POINT('Ctrl Pts',(-2.92359628300006,12.2,-3.14262277500001));
#320636=CARTESIAN_POINT('Ctrl Pts',(-2.92359628300006,5.2,-3.14262277500001));
#320637=CARTESIAN_POINT('Ctrl Pts',(-2.92359628300006,2.2,-3.14262277500001));
#320638=CARTESIAN_POINT('Ctrl Pts',(-2.92424838300006,12.2,-3.14428645500001));
#320639=CARTESIAN_POINT('Ctrl Pts',(-2.92424838300006,5.2,-3.14428645500001));
#320640=CARTESIAN_POINT('Ctrl Pts',(-2.92424838300006,2.2,-3.14428645500001));
#320641=CARTESIAN_POINT('Ctrl Pts',(-2.92490017300006,12.2,-3.14595490900002));
#320642=CARTESIAN_POINT('Ctrl Pts',(-2.92490017300006,5.2,-3.14595490900002));
#320643=CARTESIAN_POINT('Ctrl Pts',(-2.92490017300006,2.2,-3.14595490900002));
#320644=CARTESIAN_POINT('Ctrl Pts',(-2.92555164100006,12.2,-3.14762813100002));
#320645=CARTESIAN_POINT('Ctrl Pts',(-2.92555164100006,5.2,-3.14762813100002));
#320646=CARTESIAN_POINT('Ctrl Pts',(-2.92555164100006,2.2,-3.14762813100002));
#320647=CARTESIAN_POINT('Ctrl Pts',(-2.92620277400006,12.2,-3.14930611800001));
#320648=CARTESIAN_POINT('Ctrl Pts',(-2.92620277400006,5.2,-3.14930611800001));
#320649=CARTESIAN_POINT('Ctrl Pts',(-2.92620277400006,2.2,-3.14930611800001));
#320650=CARTESIAN_POINT('Ctrl Pts',(-2.92685356300006,12.2,-3.15098886600001));
#320651=CARTESIAN_POINT('Ctrl Pts',(-2.92685356300006,5.2,-3.15098886600001));
#320652=CARTESIAN_POINT('Ctrl Pts',(-2.92685356300006,2.2,-3.15098886600001));
#320653=CARTESIAN_POINT('Ctrl Pts',(-2.92750399600005,12.2,-3.15267637000002));
#320654=CARTESIAN_POINT('Ctrl Pts',(-2.92750399600005,5.2,-3.15267637000002));
#320655=CARTESIAN_POINT('Ctrl Pts',(-2.92750399600005,2.2,-3.15267637000002));
#320656=CARTESIAN_POINT('Ctrl Pts',(-2.92815406200006,12.2,-3.15436862800002));
#320657=CARTESIAN_POINT('Ctrl Pts',(-2.92815406200006,5.2,-3.15436862800002));
#320658=CARTESIAN_POINT('Ctrl Pts',(-2.92815406200006,2.2,-3.15436862800002));
#320659=CARTESIAN_POINT('Ctrl Pts',(-2.92880375100005,12.2,-3.15606563300001));
#320660=CARTESIAN_POINT('Ctrl Pts',(-2.92880375100005,5.2,-3.15606563300001));
#320661=CARTESIAN_POINT('Ctrl Pts',(-2.92880375100005,2.2,-3.15606563300001));
#320662=CARTESIAN_POINT('Ctrl Pts',(-2.92945305200006,12.2,-3.15776738400002));
#320663=CARTESIAN_POINT('Ctrl Pts',(-2.92945305200006,5.2,-3.15776738400002));
#320664=CARTESIAN_POINT('Ctrl Pts',(-2.92945305200006,2.2,-3.15776738400002));
#320665=CARTESIAN_POINT('Ctrl Pts',(-2.93010195200006,12.2,-3.15947387500001));
#320666=CARTESIAN_POINT('Ctrl Pts',(-2.93010195200006,5.2,-3.15947387500001));
#320667=CARTESIAN_POINT('Ctrl Pts',(-2.93010195200006,2.2,-3.15947387500001));
#320668=CARTESIAN_POINT('Ctrl Pts',(-2.93075044200005,12.2,-3.16118510200001));
#320669=CARTESIAN_POINT('Ctrl Pts',(-2.93075044200005,5.2,-3.16118510200001));
#320670=CARTESIAN_POINT('Ctrl Pts',(-2.93075044200005,2.2,-3.16118510200001));
#320671=CARTESIAN_POINT('Ctrl Pts',(-2.93139851000006,12.2,-3.16290106200002));
#320672=CARTESIAN_POINT('Ctrl Pts',(-2.93139851000006,5.2,-3.16290106200002));
#320673=CARTESIAN_POINT('Ctrl Pts',(-2.93139851000006,2.2,-3.16290106200002));
#320674=CARTESIAN_POINT('Ctrl Pts',(-2.93204614600006,12.2,-3.16462175100002));
#320675=CARTESIAN_POINT('Ctrl Pts',(-2.93204614600006,5.2,-3.16462175100002));
#320676=CARTESIAN_POINT('Ctrl Pts',(-2.93204614600006,2.2,-3.16462175100002));
#320677=CARTESIAN_POINT('Ctrl Pts',(-2.93269333900006,12.2,-3.16634716300001));
#320678=CARTESIAN_POINT('Ctrl Pts',(-2.93269333900006,5.2,-3.16634716300001));
#320679=CARTESIAN_POINT('Ctrl Pts',(-2.93269333900006,2.2,-3.16634716300001));
#320680=CARTESIAN_POINT('Ctrl Pts',(-2.93334007700006,12.2,-3.16807729400002));
#320681=CARTESIAN_POINT('Ctrl Pts',(-2.93334007700006,5.2,-3.16807729400002));
#320682=CARTESIAN_POINT('Ctrl Pts',(-2.93334007700006,2.2,-3.16807729400002));
#320683=CARTESIAN_POINT('Ctrl Pts',(-2.93398635100006,12.2,-3.16981214300001));
#320684=CARTESIAN_POINT('Ctrl Pts',(-2.93398635100006,5.2,-3.16981214300001));
#320685=CARTESIAN_POINT('Ctrl Pts',(-2.93398635100006,2.2,-3.16981214300001));
#320686=CARTESIAN_POINT('Ctrl Pts',(-2.93463214900005,12.2,-3.17155170200001));
#320687=CARTESIAN_POINT('Ctrl Pts',(-2.93463214900005,5.2,-3.17155170200001));
#320688=CARTESIAN_POINT('Ctrl Pts',(-2.93463214900005,2.2,-3.17155170200001));
#320689=CARTESIAN_POINT('Ctrl Pts',(-2.93527746200006,12.2,-3.17329597000001));
#320690=CARTESIAN_POINT('Ctrl Pts',(-2.93527746200006,5.2,-3.17329597000001));
#320691=CARTESIAN_POINT('Ctrl Pts',(-2.93527746200006,2.2,-3.17329597000001));
#320692=CARTESIAN_POINT('Ctrl Pts',(-2.93592227600006,12.2,-3.17504494100001));
#320693=CARTESIAN_POINT('Ctrl Pts',(-2.93592227600006,5.2,-3.17504494100001));
#320694=CARTESIAN_POINT('Ctrl Pts',(-2.93592227600006,2.2,-3.17504494100001));
#320695=CARTESIAN_POINT('Ctrl Pts',(-2.93656658300006,12.2,-3.17679861200002));
#320696=CARTESIAN_POINT('Ctrl Pts',(-2.93656658300006,5.2,-3.17679861200002));
#320697=CARTESIAN_POINT('Ctrl Pts',(-2.93656658300006,2.2,-3.17679861200002));
#320698=CARTESIAN_POINT('Ctrl Pts',(-2.93721037100005,12.2,-3.17855697700002));
#320699=CARTESIAN_POINT('Ctrl Pts',(-2.93721037100005,5.2,-3.17855697700002));
#320700=CARTESIAN_POINT('Ctrl Pts',(-2.93721037100005,2.2,-3.17855697700002));
#320701=CARTESIAN_POINT('Ctrl Pts',(-2.93785363000006,12.2,-3.18032003400001));
#320702=CARTESIAN_POINT('Ctrl Pts',(-2.93785363000006,5.2,-3.18032003400001));
#320703=CARTESIAN_POINT('Ctrl Pts',(-2.93785363000006,2.2,-3.18032003400001));
#320704=CARTESIAN_POINT('Ctrl Pts',(-2.93849634900006,12.2,-3.18208777600002));
#320705=CARTESIAN_POINT('Ctrl Pts',(-2.93849634900006,5.2,-3.18208777600002));
#320706=CARTESIAN_POINT('Ctrl Pts',(-2.93849634900006,2.2,-3.18208777600002));
#320707=CARTESIAN_POINT('Ctrl Pts',(-2.93913851800006,12.2,-3.18386020300002));
#320708=CARTESIAN_POINT('Ctrl Pts',(-2.93913851800006,5.2,-3.18386020300002));
#320709=CARTESIAN_POINT('Ctrl Pts',(-2.93913851800006,2.2,-3.18386020300002));
#320710=CARTESIAN_POINT('Ctrl Pts',(-2.93978012600005,12.2,-3.18563730800001));
#320711=CARTESIAN_POINT('Ctrl Pts',(-2.93978012600005,5.2,-3.18563730800001));
#320712=CARTESIAN_POINT('Ctrl Pts',(-2.93978012600005,2.2,-3.18563730800001));
#320713=CARTESIAN_POINT('Ctrl Pts',(-2.94042116200006,12.2,-3.18741908600002));
#320714=CARTESIAN_POINT('Ctrl Pts',(-2.94042116200006,5.2,-3.18741908600002));
#320715=CARTESIAN_POINT('Ctrl Pts',(-2.94042116200006,2.2,-3.18741908600002));
#320716=CARTESIAN_POINT('Ctrl Pts',(-2.94106161700005,12.2,-3.18920553600002));
#320717=CARTESIAN_POINT('Ctrl Pts',(-2.94106161700005,5.2,-3.18920553600002));
#320718=CARTESIAN_POINT('Ctrl Pts',(-2.94106161700005,2.2,-3.18920553600002));
#320719=CARTESIAN_POINT('Ctrl Pts',(-2.94170147800005,12.2,-3.19099665100001));
#320720=CARTESIAN_POINT('Ctrl Pts',(-2.94170147800005,5.2,-3.19099665100001));
#320721=CARTESIAN_POINT('Ctrl Pts',(-2.94170147800005,2.2,-3.19099665100001));
#320722=CARTESIAN_POINT('Ctrl Pts',(-2.94234073600005,12.2,-3.19279242700001));
#320723=CARTESIAN_POINT('Ctrl Pts',(-2.94234073600005,5.2,-3.19279242700001));
#320724=CARTESIAN_POINT('Ctrl Pts',(-2.94234073600005,2.2,-3.19279242700001));
#320725=CARTESIAN_POINT('Ctrl Pts',(-2.94297938100006,12.2,-3.19459286200001));
#320726=CARTESIAN_POINT('Ctrl Pts',(-2.94297938100006,5.2,-3.19459286200001));
#320727=CARTESIAN_POINT('Ctrl Pts',(-2.94297938100006,2.2,-3.19459286200001));
#320728=CARTESIAN_POINT('Ctrl Pts',(-2.94361740100006,12.2,-3.19639794900001));
#320729=CARTESIAN_POINT('Ctrl Pts',(-2.94361740100006,5.2,-3.19639794900001));
#320730=CARTESIAN_POINT('Ctrl Pts',(-2.94361740100006,2.2,-3.19639794900001));
#320731=CARTESIAN_POINT('Ctrl Pts',(-2.94425478800005,12.2,-3.19820768600001));
#320732=CARTESIAN_POINT('Ctrl Pts',(-2.94425478800005,5.2,-3.19820768600001));
#320733=CARTESIAN_POINT('Ctrl Pts',(-2.94425478800005,2.2,-3.19820768600001));
#320734=CARTESIAN_POINT('Ctrl Pts',(-2.94489152800006,12.2,-3.20002206700002));
#320735=CARTESIAN_POINT('Ctrl Pts',(-2.94489152800006,5.2,-3.20002206700002));
#320736=CARTESIAN_POINT('Ctrl Pts',(-2.94489152800006,2.2,-3.20002206700002));
#320737=CARTESIAN_POINT('Ctrl Pts',(-2.94552761500006,12.2,-3.20184108900001));
#320738=CARTESIAN_POINT('Ctrl Pts',(-2.94552761500006,5.2,-3.20184108900001));
#320739=CARTESIAN_POINT('Ctrl Pts',(-2.94552761500006,2.2,-3.20184108900001));
#320740=CARTESIAN_POINT('Ctrl Pts',(-2.94616303400006,12.2,-3.20366474800001));
#320741=CARTESIAN_POINT('Ctrl Pts',(-2.94616303400006,5.2,-3.20366474800001));
#320742=CARTESIAN_POINT('Ctrl Pts',(-2.94616303400006,2.2,-3.20366474800001));
#320743=CARTESIAN_POINT('Ctrl Pts',(-2.94679777900006,12.2,-3.20549303700002));
#320744=CARTESIAN_POINT('Ctrl Pts',(-2.94679777900006,5.2,-3.20549303700002));
#320745=CARTESIAN_POINT('Ctrl Pts',(-2.94679777900006,2.2,-3.20549303700002));
#320746=CARTESIAN_POINT('Ctrl Pts',(-2.94743183700006,12.2,-3.20732595500001));
#320747=CARTESIAN_POINT('Ctrl Pts',(-2.94743183700006,5.2,-3.20732595500001));
#320748=CARTESIAN_POINT('Ctrl Pts',(-2.94743183700006,2.2,-3.20732595500001));
#320749=CARTESIAN_POINT('Ctrl Pts',(-2.94806519800006,12.2,-3.20916349600001));
#320750=CARTESIAN_POINT('Ctrl Pts',(-2.94806519800006,5.2,-3.20916349600001));
#320751=CARTESIAN_POINT('Ctrl Pts',(-2.94806519800006,2.2,-3.20916349600001));
#320752=CARTESIAN_POINT('Ctrl Pts',(-2.94869785300006,12.2,-3.21100565700001));
#320753=CARTESIAN_POINT('Ctrl Pts',(-2.94869785300006,5.2,-3.21100565700001));
#320754=CARTESIAN_POINT('Ctrl Pts',(-2.94869785300006,2.2,-3.21100565700001));
#320755=CARTESIAN_POINT('Ctrl Pts',(-2.94932979000006,12.2,-3.21285243200002));
#320756=CARTESIAN_POINT('Ctrl Pts',(-2.94932979000006,5.2,-3.21285243200002));
#320757=CARTESIAN_POINT('Ctrl Pts',(-2.94932979000006,2.2,-3.21285243200002));
#320758=CARTESIAN_POINT('Ctrl Pts',(-2.94996099900006,12.2,-3.21470381800002));
#320759=CARTESIAN_POINT('Ctrl Pts',(-2.94996099900006,5.2,-3.21470381800002));
#320760=CARTESIAN_POINT('Ctrl Pts',(-2.94996099900006,2.2,-3.21470381800002));
#320761=CARTESIAN_POINT('Ctrl Pts',(-2.95059147200006,12.2,-3.21655981000001));
#320762=CARTESIAN_POINT('Ctrl Pts',(-2.95059147200006,5.2,-3.21655981000001));
#320763=CARTESIAN_POINT('Ctrl Pts',(-2.95059147200006,2.2,-3.21655981000001));
#320764=CARTESIAN_POINT('Ctrl Pts',(-2.95122119700005,12.2,-3.21842040400002));
#320765=CARTESIAN_POINT('Ctrl Pts',(-2.95122119700005,5.2,-3.21842040400002));
#320766=CARTESIAN_POINT('Ctrl Pts',(-2.95122119700005,2.2,-3.21842040400002));
#320767=CARTESIAN_POINT('Ctrl Pts',(-2.95185016300006,12.2,-3.22028559600001));
#320768=CARTESIAN_POINT('Ctrl Pts',(-2.95185016300006,5.2,-3.22028559600001));
#320769=CARTESIAN_POINT('Ctrl Pts',(-2.95185016300006,2.2,-3.22028559600001));
#320770=CARTESIAN_POINT('Ctrl Pts',(-2.95247836200006,12.2,-3.22215538200001));
#320771=CARTESIAN_POINT('Ctrl Pts',(-2.95247836200006,5.2,-3.22215538200001));
#320772=CARTESIAN_POINT('Ctrl Pts',(-2.95247836200006,2.2,-3.22215538200001));
#320773=CARTESIAN_POINT('Ctrl Pts',(-2.95310578300006,12.2,-3.22402975500002));
#320774=CARTESIAN_POINT('Ctrl Pts',(-2.95310578300006,5.2,-3.22402975500002));
#320775=CARTESIAN_POINT('Ctrl Pts',(-2.95310578300006,2.2,-3.22402975500002));
#320776=CARTESIAN_POINT('Ctrl Pts',(-2.95373241500006,12.2,-3.22590871400001));
#320777=CARTESIAN_POINT('Ctrl Pts',(-2.95373241500006,5.2,-3.22590871400001));
#320778=CARTESIAN_POINT('Ctrl Pts',(-2.95373241500006,2.2,-3.22590871400001));
#320779=CARTESIAN_POINT('Ctrl Pts',(-2.95435824900005,12.2,-3.22779225300001));
#320780=CARTESIAN_POINT('Ctrl Pts',(-2.95435824900005,5.2,-3.22779225300001));
#320781=CARTESIAN_POINT('Ctrl Pts',(-2.95435824900005,2.2,-3.22779225300001));
#320782=CARTESIAN_POINT('Ctrl Pts',(-2.95498327600006,12.2,-3.22968036800001));
#320783=CARTESIAN_POINT('Ctrl Pts',(-2.95498327600006,5.2,-3.22968036800001));
#320784=CARTESIAN_POINT('Ctrl Pts',(-2.95498327600006,2.2,-3.22968036800001));
#320785=CARTESIAN_POINT('Ctrl Pts',(-2.95560748300006,12.2,-3.23157305400001));
#320786=CARTESIAN_POINT('Ctrl Pts',(-2.95560748300006,5.2,-3.23157305400001));
#320787=CARTESIAN_POINT('Ctrl Pts',(-2.95560748300006,2.2,-3.23157305400001));
#320788=CARTESIAN_POINT('Ctrl Pts',(-2.95623086300006,12.2,-3.23347030800001));
#320789=CARTESIAN_POINT('Ctrl Pts',(-2.95623086300006,5.2,-3.23347030800001));
#320790=CARTESIAN_POINT('Ctrl Pts',(-2.95623086300006,2.2,-3.23347030800001));
#320791=CARTESIAN_POINT('Ctrl Pts',(-2.95685340400006,12.2,-3.23537212400002));
#320792=CARTESIAN_POINT('Ctrl Pts',(-2.95685340400006,5.2,-3.23537212400002));
#320793=CARTESIAN_POINT('Ctrl Pts',(-2.95685340400006,2.2,-3.23537212400002));
#320794=CARTESIAN_POINT('Ctrl Pts',(-2.95747509600006,12.2,-3.23727849900001));
#320795=CARTESIAN_POINT('Ctrl Pts',(-2.95747509600006,5.2,-3.23727849900001));
#320796=CARTESIAN_POINT('Ctrl Pts',(-2.95747509600006,2.2,-3.23727849900001));
#320797=CARTESIAN_POINT('Ctrl Pts',(-2.95809593100006,12.2,-3.23918942800002));
#320798=CARTESIAN_POINT('Ctrl Pts',(-2.95809593100006,5.2,-3.23918942800002));
#320799=CARTESIAN_POINT('Ctrl Pts',(-2.95809593100006,2.2,-3.23918942800002));
#320800=CARTESIAN_POINT('Ctrl Pts',(-2.95871589700006,12.2,-3.24110490600001));
#320801=CARTESIAN_POINT('Ctrl Pts',(-2.95871589700006,5.2,-3.24110490600001));
#320802=CARTESIAN_POINT('Ctrl Pts',(-2.95871589700006,2.2,-3.24110490600001));
#320803=CARTESIAN_POINT('Ctrl Pts',(-2.95933498600006,12.2,-3.24302493100001));
#320804=CARTESIAN_POINT('Ctrl Pts',(-2.95933498600006,5.2,-3.24302493100001));
#320805=CARTESIAN_POINT('Ctrl Pts',(-2.95933498600006,2.2,-3.24302493100001));
#320806=CARTESIAN_POINT('Ctrl Pts',(-2.95995318600006,12.2,-3.24494949500002));
#320807=CARTESIAN_POINT('Ctrl Pts',(-2.95995318600006,5.2,-3.24494949500002));
#320808=CARTESIAN_POINT('Ctrl Pts',(-2.95995318600006,2.2,-3.24494949500002));
#320809=CARTESIAN_POINT('Ctrl Pts',(-2.96057048900006,12.2,-3.24687859600001));
#320810=CARTESIAN_POINT('Ctrl Pts',(-2.96057048900006,5.2,-3.24687859600001));
#320811=CARTESIAN_POINT('Ctrl Pts',(-2.96057048900006,2.2,-3.24687859600001));
#320812=CARTESIAN_POINT('Ctrl Pts',(-2.96118688400006,12.2,-3.24881223000002));
#320813=CARTESIAN_POINT('Ctrl Pts',(-2.96118688400006,5.2,-3.24881223000002));
#320814=CARTESIAN_POINT('Ctrl Pts',(-2.96118688400006,2.2,-3.24881223000002));
#320815=CARTESIAN_POINT('Ctrl Pts',(-2.96180236200006,12.2,-3.25075039000001));
#320816=CARTESIAN_POINT('Ctrl Pts',(-2.96180236200006,5.2,-3.25075039000001));
#320817=CARTESIAN_POINT('Ctrl Pts',(-2.96180236200006,2.2,-3.25075039000001));
#320818=CARTESIAN_POINT('Ctrl Pts',(-2.96241691300006,12.2,-3.25269307400001));
#320819=CARTESIAN_POINT('Ctrl Pts',(-2.96241691300006,5.2,-3.25269307400001));
#320820=CARTESIAN_POINT('Ctrl Pts',(-2.96241691300006,2.2,-3.25269307400001));
#320821=CARTESIAN_POINT('Ctrl Pts',(-2.96303052700006,12.2,-3.25464027700002));
#320822=CARTESIAN_POINT('Ctrl Pts',(-2.96303052700006,5.2,-3.25464027700002));
#320823=CARTESIAN_POINT('Ctrl Pts',(-2.96303052700006,2.2,-3.25464027700002));
#320824=CARTESIAN_POINT('Ctrl Pts',(-2.96364319400006,12.2,-3.25659199500001));
#320825=CARTESIAN_POINT('Ctrl Pts',(-2.96364319400006,5.2,-3.25659199500001));
#320826=CARTESIAN_POINT('Ctrl Pts',(-2.96364319400006,2.2,-3.25659199500001));
#320827=CARTESIAN_POINT('Ctrl Pts',(-2.96425490500006,12.2,-3.25854822100001));
#320828=CARTESIAN_POINT('Ctrl Pts',(-2.96425490500006,5.2,-3.25854822100001));
#320829=CARTESIAN_POINT('Ctrl Pts',(-2.96425490500006,2.2,-3.25854822100001));
#320830=CARTESIAN_POINT('Ctrl Pts',(-2.96486565000006,12.2,-3.26050895400002));
#320831=CARTESIAN_POINT('Ctrl Pts',(-2.96486565000006,5.2,-3.26050895400002));
#320832=CARTESIAN_POINT('Ctrl Pts',(-2.96486565000006,2.2,-3.26050895400002));
#320833=CARTESIAN_POINT('Ctrl Pts',(-2.96547541900006,12.2,-3.26247418600001));
#320834=CARTESIAN_POINT('Ctrl Pts',(-2.96547541900006,5.2,-3.26247418600001));
#320835=CARTESIAN_POINT('Ctrl Pts',(-2.96547541900006,2.2,-3.26247418600001));
#320836=CARTESIAN_POINT('Ctrl Pts',(-2.96608420300006,12.2,-3.26444391600001));
#320837=CARTESIAN_POINT('Ctrl Pts',(-2.96608420300006,5.2,-3.26444391600001));
#320838=CARTESIAN_POINT('Ctrl Pts',(-2.96608420300006,2.2,-3.26444391600001));
#320839=CARTESIAN_POINT('Ctrl Pts',(-2.96669199100006,12.2,-3.26641813800002));
#320840=CARTESIAN_POINT('Ctrl Pts',(-2.96669199100006,5.2,-3.26641813800002));
#320841=CARTESIAN_POINT('Ctrl Pts',(-2.96669199100006,2.2,-3.26641813800002));
#320842=CARTESIAN_POINT('Ctrl Pts',(-2.96729877500006,12.2,-3.26839684700001));
#320843=CARTESIAN_POINT('Ctrl Pts',(-2.96729877500006,5.2,-3.26839684700001));
#320844=CARTESIAN_POINT('Ctrl Pts',(-2.96729877500006,2.2,-3.26839684700001));
#320845=CARTESIAN_POINT('Ctrl Pts',(-2.96790454500006,12.2,-3.27038003900002));
#320846=CARTESIAN_POINT('Ctrl Pts',(-2.96790454500006,5.2,-3.27038003900002));
#320847=CARTESIAN_POINT('Ctrl Pts',(-2.96790454500006,2.2,-3.27038003900002));
#320848=CARTESIAN_POINT('Ctrl Pts',(-2.96850929200006,12.2,-3.27236770900001));
#320849=CARTESIAN_POINT('Ctrl Pts',(-2.96850929200006,5.2,-3.27236770900001));
#320850=CARTESIAN_POINT('Ctrl Pts',(-2.96850929200006,2.2,-3.27236770900001));
#320851=CARTESIAN_POINT('Ctrl Pts',(-2.96911300500006,12.2,-3.27435985300002));
#320852=CARTESIAN_POINT('Ctrl Pts',(-2.96911300500006,5.2,-3.27435985300002));
#320853=CARTESIAN_POINT('Ctrl Pts',(-2.96911300500006,2.2,-3.27435985300002));
#320854=CARTESIAN_POINT('Ctrl Pts',(-2.96971567500006,12.2,-3.27635646800001));
#320855=CARTESIAN_POINT('Ctrl Pts',(-2.96971567500006,5.2,-3.27635646800001));
#320856=CARTESIAN_POINT('Ctrl Pts',(-2.96971567500006,2.2,-3.27635646800001));
#320857=CARTESIAN_POINT('Ctrl Pts',(-2.97031729300006,12.2,-3.27835754600001));
#320858=CARTESIAN_POINT('Ctrl Pts',(-2.97031729300006,5.2,-3.27835754600001));
#320859=CARTESIAN_POINT('Ctrl Pts',(-2.97031729300006,2.2,-3.27835754600001));
#320860=CARTESIAN_POINT('Ctrl Pts',(-2.97091784700006,12.2,-3.28036308600002));
#320861=CARTESIAN_POINT('Ctrl Pts',(-2.97091784700006,5.2,-3.28036308600002));
#320862=CARTESIAN_POINT('Ctrl Pts',(-2.97091784700006,2.2,-3.28036308600002));
#320863=CARTESIAN_POINT('Ctrl Pts',(-2.97151733200006,12.2,-3.28237308100002));
#320864=CARTESIAN_POINT('Ctrl Pts',(-2.97151733200006,5.2,-3.28237308100002));
#320865=CARTESIAN_POINT('Ctrl Pts',(-2.97151733200006,2.2,-3.28237308100002));
#320866=CARTESIAN_POINT('Ctrl Pts',(-2.97211573600006,12.2,-3.28438752800002));
#320867=CARTESIAN_POINT('Ctrl Pts',(-2.97211573600006,5.2,-3.28438752800002));
#320868=CARTESIAN_POINT('Ctrl Pts',(-2.97211573600006,2.2,-3.28438752800002));
#320869=CARTESIAN_POINT('Ctrl Pts',(-2.97271304900006,12.2,-3.28640642100002));
#320870=CARTESIAN_POINT('Ctrl Pts',(-2.97271304900006,5.2,-3.28640642100002));
#320871=CARTESIAN_POINT('Ctrl Pts',(-2.97271304900006,2.2,-3.28640642100002));
#320872=CARTESIAN_POINT('Ctrl Pts',(-2.97330926200006,12.2,-3.28842975700002));
#320873=CARTESIAN_POINT('Ctrl Pts',(-2.97330926200006,5.2,-3.28842975700002));
#320874=CARTESIAN_POINT('Ctrl Pts',(-2.97330926200006,2.2,-3.28842975700002));
#320875=CARTESIAN_POINT('Ctrl Pts',(-2.97390436700006,12.2,-3.29045753100001));
#320876=CARTESIAN_POINT('Ctrl Pts',(-2.97390436700006,5.2,-3.29045753100001));
#320877=CARTESIAN_POINT('Ctrl Pts',(-2.97390436700006,2.2,-3.29045753100001));
#320878=CARTESIAN_POINT('Ctrl Pts',(-2.97449835400006,12.2,-3.29248973700001));
#320879=CARTESIAN_POINT('Ctrl Pts',(-2.97449835400006,5.2,-3.29248973700001));
#320880=CARTESIAN_POINT('Ctrl Pts',(-2.97449835400006,2.2,-3.29248973700001));
#320881=CARTESIAN_POINT('Ctrl Pts',(-2.97509121300005,12.2,-3.29452637300002));
#320882=CARTESIAN_POINT('Ctrl Pts',(-2.97509121300005,5.2,-3.29452637300002));
#320883=CARTESIAN_POINT('Ctrl Pts',(-2.97509121300005,2.2,-3.29452637300002));
#320884=CARTESIAN_POINT('Ctrl Pts',(-2.97568293500006,12.2,-3.29656743200001));
#320885=CARTESIAN_POINT('Ctrl Pts',(-2.97568293500006,5.2,-3.29656743200001));
#320886=CARTESIAN_POINT('Ctrl Pts',(-2.97568293500006,2.2,-3.29656743200001));
#320887=CARTESIAN_POINT('Ctrl Pts',(-2.97627351000005,12.2,-3.29861291100002));
#320888=CARTESIAN_POINT('Ctrl Pts',(-2.97627351000005,5.2,-3.29861291100002));
#320889=CARTESIAN_POINT('Ctrl Pts',(-2.97627351000005,2.2,-3.29861291100002));
#320890=CARTESIAN_POINT('Ctrl Pts',(-2.97686292900006,12.2,-3.30066280500001));
#320891=CARTESIAN_POINT('Ctrl Pts',(-2.97686292900006,5.2,-3.30066280500001));
#320892=CARTESIAN_POINT('Ctrl Pts',(-2.97686292900006,2.2,-3.30066280500001));
#320893=CARTESIAN_POINT('Ctrl Pts',(-2.97745118400006,12.2,-3.30271710800002));
#320894=CARTESIAN_POINT('Ctrl Pts',(-2.97745118400006,5.2,-3.30271710800002));
#320895=CARTESIAN_POINT('Ctrl Pts',(-2.97745118400006,2.2,-3.30271710800002));
#320896=CARTESIAN_POINT('Ctrl Pts',(-2.97803826500005,12.2,-3.30477581800002));
#320897=CARTESIAN_POINT('Ctrl Pts',(-2.97803826500005,5.2,-3.30477581800002));
#320898=CARTESIAN_POINT('Ctrl Pts',(-2.97803826500005,2.2,-3.30477581800002));
#320899=CARTESIAN_POINT('Ctrl Pts',(-2.97862416200006,12.2,-3.30683892800002));
#320900=CARTESIAN_POINT('Ctrl Pts',(-2.97862416200006,5.2,-3.30683892800002));
#320901=CARTESIAN_POINT('Ctrl Pts',(-2.97862416200006,2.2,-3.30683892800002));
#320902=CARTESIAN_POINT('Ctrl Pts',(-2.97920886600005,12.2,-3.30890643600001));
#320903=CARTESIAN_POINT('Ctrl Pts',(-2.97920886600005,5.2,-3.30890643600001));
#320904=CARTESIAN_POINT('Ctrl Pts',(-2.97920886600005,2.2,-3.30890643600001));
#320905=CARTESIAN_POINT('Ctrl Pts',(-2.97979236900006,12.2,-3.31097833600001));
#320906=CARTESIAN_POINT('Ctrl Pts',(-2.97979236900006,5.2,-3.31097833600001));
#320907=CARTESIAN_POINT('Ctrl Pts',(-2.97979236900006,2.2,-3.31097833600001));
#320908=CARTESIAN_POINT('Ctrl Pts',(-2.98037466100005,12.2,-3.31305462200001));
#320909=CARTESIAN_POINT('Ctrl Pts',(-2.98037466100005,5.2,-3.31305462200001));
#320910=CARTESIAN_POINT('Ctrl Pts',(-2.98037466100005,2.2,-3.31305462200001));
#320911=CARTESIAN_POINT('Ctrl Pts',(-2.98095573300006,12.2,-3.31513529200001));
#320912=CARTESIAN_POINT('Ctrl Pts',(-2.98095573300006,5.2,-3.31513529200001));
#320913=CARTESIAN_POINT('Ctrl Pts',(-2.98095573300006,2.2,-3.31513529200001));
#320914=CARTESIAN_POINT('Ctrl Pts',(-2.98153557700005,12.2,-3.31722033900002));
#320915=CARTESIAN_POINT('Ctrl Pts',(-2.98153557700005,5.2,-3.31722033900002));
#320916=CARTESIAN_POINT('Ctrl Pts',(-2.98153557700005,2.2,-3.31722033900002));
#320917=CARTESIAN_POINT('Ctrl Pts',(-2.98211418100006,12.2,-3.31930976000002));
#320918=CARTESIAN_POINT('Ctrl Pts',(-2.98211418100006,5.2,-3.31930976000002));
#320919=CARTESIAN_POINT('Ctrl Pts',(-2.98211418100006,2.2,-3.31930976000002));
#320920=CARTESIAN_POINT('Ctrl Pts',(-2.98269153900006,12.2,-3.32140354900002));
#320921=CARTESIAN_POINT('Ctrl Pts',(-2.98269153900006,5.2,-3.32140354900002));
#320922=CARTESIAN_POINT('Ctrl Pts',(-2.98269153900006,2.2,-3.32140354900002));
#320923=CARTESIAN_POINT('Ctrl Pts',(-2.98326763900006,12.2,-3.32350170300002));
#320924=CARTESIAN_POINT('Ctrl Pts',(-2.98326763900006,5.2,-3.32350170300002));
#320925=CARTESIAN_POINT('Ctrl Pts',(-2.98326763900006,2.2,-3.32350170300002));
#320926=CARTESIAN_POINT('Ctrl Pts',(-2.98384247500006,12.2,-3.32560421600002));
#320927=CARTESIAN_POINT('Ctrl Pts',(-2.98384247500006,5.2,-3.32560421600002));
#320928=CARTESIAN_POINT('Ctrl Pts',(-2.98384247500006,2.2,-3.32560421600002));
#320929=CARTESIAN_POINT('Ctrl Pts',(-2.98441603600006,12.2,-3.32771108400001));
#320930=CARTESIAN_POINT('Ctrl Pts',(-2.98441603600006,5.2,-3.32771108400001));
#320931=CARTESIAN_POINT('Ctrl Pts',(-2.98441603600006,2.2,-3.32771108400001));
#320932=CARTESIAN_POINT('Ctrl Pts',(-2.98498831300006,12.2,-3.32982230300002));
#320933=CARTESIAN_POINT('Ctrl Pts',(-2.98498831300006,5.2,-3.32982230300002));
#320934=CARTESIAN_POINT('Ctrl Pts',(-2.98498831300006,2.2,-3.32982230300002));
#320935=CARTESIAN_POINT('Ctrl Pts',(-2.98555929700006,12.2,-3.33193786600001));
#320936=CARTESIAN_POINT('Ctrl Pts',(-2.98555929700006,5.2,-3.33193786600001));
#320937=CARTESIAN_POINT('Ctrl Pts',(-2.98555929700006,2.2,-3.33193786600001));
#320938=CARTESIAN_POINT('Ctrl Pts',(-2.98612898100005,12.2,-3.33405777100001));
#320939=CARTESIAN_POINT('Ctrl Pts',(-2.98612898100005,5.2,-3.33405777100001));
#320940=CARTESIAN_POINT('Ctrl Pts',(-2.98612898100005,2.2,-3.33405777100001));
#320941=CARTESIAN_POINT('Ctrl Pts',(-2.98669735400006,12.2,-3.33618201100002));
#320942=CARTESIAN_POINT('Ctrl Pts',(-2.98669735400006,5.2,-3.33618201100002));
#320943=CARTESIAN_POINT('Ctrl Pts',(-2.98669735400006,2.2,-3.33618201100002));
#320944=CARTESIAN_POINT('Ctrl Pts',(-2.98726440700006,12.2,-3.33831058400001));
#320945=CARTESIAN_POINT('Ctrl Pts',(-2.98726440700006,5.2,-3.33831058400001));
#320946=CARTESIAN_POINT('Ctrl Pts',(-2.98726440700006,2.2,-3.33831058400001));
#320947=CARTESIAN_POINT('Ctrl Pts',(-2.98783013300006,12.2,-3.34044348300001));
#320948=CARTESIAN_POINT('Ctrl Pts',(-2.98783013300006,5.2,-3.34044348300001));
#320949=CARTESIAN_POINT('Ctrl Pts',(-2.98783013300006,2.2,-3.34044348300001));
#320950=CARTESIAN_POINT('Ctrl Pts',(-2.98839452200005,12.2,-3.34258070300002));
#320951=CARTESIAN_POINT('Ctrl Pts',(-2.98839452200005,5.2,-3.34258070300002));
#320952=CARTESIAN_POINT('Ctrl Pts',(-2.98839452200005,2.2,-3.34258070300002));
#320953=CARTESIAN_POINT('Ctrl Pts',(-2.98895756400006,12.2,-3.34472224200002));
#320954=CARTESIAN_POINT('Ctrl Pts',(-2.98895756400006,5.2,-3.34472224200002));
#320955=CARTESIAN_POINT('Ctrl Pts',(-2.98895756400006,2.2,-3.34472224200002));
#320956=CARTESIAN_POINT('Ctrl Pts',(-2.98951925100006,12.2,-3.34686809300001));
#320957=CARTESIAN_POINT('Ctrl Pts',(-2.98951925100006,5.2,-3.34686809300001));
#320958=CARTESIAN_POINT('Ctrl Pts',(-2.98951925100006,2.2,-3.34686809300001));
#320959=CARTESIAN_POINT('Ctrl Pts',(-2.99007957400006,12.2,-3.34901825200001));
#320960=CARTESIAN_POINT('Ctrl Pts',(-2.99007957400006,5.2,-3.34901825200001));
#320961=CARTESIAN_POINT('Ctrl Pts',(-2.99007957400006,2.2,-3.34901825200001));
#320962=CARTESIAN_POINT('Ctrl Pts',(-2.99063852600006,12.2,-3.35117271400001));
#320963=CARTESIAN_POINT('Ctrl Pts',(-2.99063852600006,5.2,-3.35117271400001));
#320964=CARTESIAN_POINT('Ctrl Pts',(-2.99063852600006,2.2,-3.35117271400001));
#320965=CARTESIAN_POINT('Ctrl Pts',(-2.99119609600006,12.2,-3.35333147500001));
#320966=CARTESIAN_POINT('Ctrl Pts',(-2.99119609600006,5.2,-3.35333147500001));
#320967=CARTESIAN_POINT('Ctrl Pts',(-2.99119609600006,2.2,-3.35333147500001));
#320968=CARTESIAN_POINT('Ctrl Pts',(-2.99175227600006,12.2,-3.35549453000001));
#320969=CARTESIAN_POINT('Ctrl Pts',(-2.99175227600006,5.2,-3.35549453000001));
#320970=CARTESIAN_POINT('Ctrl Pts',(-2.99175227600006,2.2,-3.35549453000001));
#320971=CARTESIAN_POINT('Ctrl Pts',(-2.99230705700006,12.2,-3.35766187400001));
#320972=CARTESIAN_POINT('Ctrl Pts',(-2.99230705700006,5.2,-3.35766187400001));
#320973=CARTESIAN_POINT('Ctrl Pts',(-2.99230705700006,2.2,-3.35766187400001));
#320974=CARTESIAN_POINT('Ctrl Pts',(-2.99286043000006,12.2,-3.35983350200001));
#320975=CARTESIAN_POINT('Ctrl Pts',(-2.99286043000006,5.2,-3.35983350200001));
#320976=CARTESIAN_POINT('Ctrl Pts',(-2.99286043000006,2.2,-3.35983350200001));
#320977=CARTESIAN_POINT('Ctrl Pts',(-2.99341238800006,12.2,-3.36200941000001));
#320978=CARTESIAN_POINT('Ctrl Pts',(-2.99341238800006,5.2,-3.36200941000001));
#320979=CARTESIAN_POINT('Ctrl Pts',(-2.99341238800006,2.2,-3.36200941000001));
#320980=CARTESIAN_POINT('Ctrl Pts',(-2.99396292000006,12.2,-3.36418959200001));
#320981=CARTESIAN_POINT('Ctrl Pts',(-2.99396292000006,5.2,-3.36418959200001));
#320982=CARTESIAN_POINT('Ctrl Pts',(-2.99396292000006,2.2,-3.36418959200001));
#320983=CARTESIAN_POINT('Ctrl Pts',(-2.99451201800006,12.2,-3.36637404500001));
#320984=CARTESIAN_POINT('Ctrl Pts',(-2.99451201800006,5.2,-3.36637404500001));
#320985=CARTESIAN_POINT('Ctrl Pts',(-2.99451201800006,2.2,-3.36637404500001));
#320986=CARTESIAN_POINT('Ctrl Pts',(-2.99505967500005,12.2,-3.36856276300002));
#320987=CARTESIAN_POINT('Ctrl Pts',(-2.99505967500005,5.2,-3.36856276300002));
#320988=CARTESIAN_POINT('Ctrl Pts',(-2.99505967500005,2.2,-3.36856276300002));
#320989=CARTESIAN_POINT('Ctrl Pts',(-2.99560588000006,12.2,-3.37075574200002));
#320990=CARTESIAN_POINT('Ctrl Pts',(-2.99560588000006,5.2,-3.37075574200002));
#320991=CARTESIAN_POINT('Ctrl Pts',(-2.99560588000006,2.2,-3.37075574200002));
#320992=CARTESIAN_POINT('Ctrl Pts',(-2.99615062600005,12.2,-3.37295297600001));
#320993=CARTESIAN_POINT('Ctrl Pts',(-2.99615062600005,5.2,-3.37295297600001));
#320994=CARTESIAN_POINT('Ctrl Pts',(-2.99615062600005,2.2,-3.37295297600001));
#320995=CARTESIAN_POINT('Ctrl Pts',(-2.99669390300005,12.2,-3.37515446200001));
#320996=CARTESIAN_POINT('Ctrl Pts',(-2.99669390300005,5.2,-3.37515446200001));
#320997=CARTESIAN_POINT('Ctrl Pts',(-2.99669390300005,2.2,-3.37515446200001));
#320998=CARTESIAN_POINT('Ctrl Pts',(-2.99723570400006,12.2,-3.37736019300001));
#320999=CARTESIAN_POINT('Ctrl Pts',(-2.99723570400006,5.2,-3.37736019300001));
#321000=CARTESIAN_POINT('Ctrl Pts',(-2.99723570400006,2.2,-3.37736019300001));
#321001=CARTESIAN_POINT('Ctrl Pts',(-2.99777601900006,12.2,-3.37957016700001));
#321002=CARTESIAN_POINT('Ctrl Pts',(-2.99777601900006,5.2,-3.37957016700001));
#321003=CARTESIAN_POINT('Ctrl Pts',(-2.99777601900006,2.2,-3.37957016700001));
#321004=CARTESIAN_POINT('Ctrl Pts',(-2.99831484100006,12.2,-3.38178437700002));
#321005=CARTESIAN_POINT('Ctrl Pts',(-2.99831484100006,5.2,-3.38178437700002));
#321006=CARTESIAN_POINT('Ctrl Pts',(-2.99831484100006,2.2,-3.38178437700002));
#321007=CARTESIAN_POINT('Ctrl Pts',(-2.99885216000006,12.2,-3.38400281900002));
#321008=CARTESIAN_POINT('Ctrl Pts',(-2.99885216000006,5.2,-3.38400281900002));
#321009=CARTESIAN_POINT('Ctrl Pts',(-2.99885216000006,2.2,-3.38400281900002));
#321010=CARTESIAN_POINT('Ctrl Pts',(-2.99938796800005,12.2,-3.38622548900001));
#321011=CARTESIAN_POINT('Ctrl Pts',(-2.99938796800005,5.2,-3.38622548900001));
#321012=CARTESIAN_POINT('Ctrl Pts',(-2.99938796800005,2.2,-3.38622548900001));
#321013=CARTESIAN_POINT('Ctrl Pts',(-2.99992225700006,12.2,-3.38845237900002));
#321014=CARTESIAN_POINT('Ctrl Pts',(-2.99992225700006,5.2,-3.38845237900002));
#321015=CARTESIAN_POINT('Ctrl Pts',(-2.99992225700006,2.2,-3.38845237900002));
#321016=CARTESIAN_POINT('Ctrl Pts',(-3.00045501800006,12.2,-3.39068348900001));
#321017=CARTESIAN_POINT('Ctrl Pts',(-3.00045501800006,5.2,-3.39068348900001));
#321018=CARTESIAN_POINT('Ctrl Pts',(-3.00045501800006,2.2,-3.39068348900001));
#321019=CARTESIAN_POINT('Ctrl Pts',(-3.00098624200006,12.2,-3.39291881100001));
#321020=CARTESIAN_POINT('Ctrl Pts',(-3.00098624200006,5.2,-3.39291881100001));
#321021=CARTESIAN_POINT('Ctrl Pts',(-3.00098624200006,2.2,-3.39291881100001));
#321022=CARTESIAN_POINT('Ctrl Pts',(-3.00151592200006,12.2,-3.39515834000002));
#321023=CARTESIAN_POINT('Ctrl Pts',(-3.00151592200006,5.2,-3.39515834000002));
#321024=CARTESIAN_POINT('Ctrl Pts',(-3.00151592200006,2.2,-3.39515834000002));
#321025=CARTESIAN_POINT('Ctrl Pts',(-3.00204404800006,12.2,-3.39740207200002));
#321026=CARTESIAN_POINT('Ctrl Pts',(-3.00204404800006,5.2,-3.39740207200002));
#321027=CARTESIAN_POINT('Ctrl Pts',(-3.00204404800006,2.2,-3.39740207200002));
#321028=CARTESIAN_POINT('Ctrl Pts',(-3.00257061300006,12.2,-3.39965000400001));
#321029=CARTESIAN_POINT('Ctrl Pts',(-3.00257061300006,5.2,-3.39965000400001));
#321030=CARTESIAN_POINT('Ctrl Pts',(-3.00257061300006,2.2,-3.39965000400001));
#321031=CARTESIAN_POINT('Ctrl Pts',(-3.00309560800006,12.2,-3.40190212700001));
#321032=CARTESIAN_POINT('Ctrl Pts',(-3.00309560800006,5.2,-3.40190212700001));
#321033=CARTESIAN_POINT('Ctrl Pts',(-3.00309560800006,2.2,-3.40190212700001));
#321034=CARTESIAN_POINT('Ctrl Pts',(-3.00361902400006,12.2,-3.40415844100002));
#321035=CARTESIAN_POINT('Ctrl Pts',(-3.00361902400006,5.2,-3.40415844100002));
#321036=CARTESIAN_POINT('Ctrl Pts',(-3.00361902400006,2.2,-3.40415844100002));
#321037=CARTESIAN_POINT('Ctrl Pts',(-3.00414085400006,12.2,-3.40641893700001));
#321038=CARTESIAN_POINT('Ctrl Pts',(-3.00414085400006,5.2,-3.40641893700001));
#321039=CARTESIAN_POINT('Ctrl Pts',(-3.00414085400006,2.2,-3.40641893700001));
#321040=CARTESIAN_POINT('Ctrl Pts',(-3.00466108800005,12.2,-3.40868361300001));
#321041=CARTESIAN_POINT('Ctrl Pts',(-3.00466108800005,5.2,-3.40868361300001));
#321042=CARTESIAN_POINT('Ctrl Pts',(-3.00466108800005,2.2,-3.40868361300001));
#321043=CARTESIAN_POINT('Ctrl Pts',(-3.00517971900006,12.2,-3.41095246200001));
#321044=CARTESIAN_POINT('Ctrl Pts',(-3.00517971900006,5.2,-3.41095246200001));
#321045=CARTESIAN_POINT('Ctrl Pts',(-3.00517971900006,2.2,-3.41095246200001));
#321046=CARTESIAN_POINT('Ctrl Pts',(-3.00569673900006,12.2,-3.41322548000001));
#321047=CARTESIAN_POINT('Ctrl Pts',(-3.00569673900006,5.2,-3.41322548000001));
#321048=CARTESIAN_POINT('Ctrl Pts',(-3.00569673900006,2.2,-3.41322548000001));
#321049=CARTESIAN_POINT('Ctrl Pts',(-3.00621213800006,12.2,-3.41550266300001));
#321050=CARTESIAN_POINT('Ctrl Pts',(-3.00621213800006,5.2,-3.41550266300001));
#321051=CARTESIAN_POINT('Ctrl Pts',(-3.00621213800006,2.2,-3.41550266300001));
#321052=CARTESIAN_POINT('Ctrl Pts',(-3.00672591000006,12.2,-3.41778400600001));
#321053=CARTESIAN_POINT('Ctrl Pts',(-3.00672591000006,5.2,-3.41778400600001));
#321054=CARTESIAN_POINT('Ctrl Pts',(-3.00672591000006,2.2,-3.41778400600001));
#321055=CARTESIAN_POINT('Ctrl Pts',(-3.00723804500006,12.2,-3.42006950300001));
#321056=CARTESIAN_POINT('Ctrl Pts',(-3.00723804500006,5.2,-3.42006950300001));
#321057=CARTESIAN_POINT('Ctrl Pts',(-3.00723804500006,2.2,-3.42006950300001));
#321058=CARTESIAN_POINT('Ctrl Pts',(-3.00774853500006,12.2,-3.42235915000002));
#321059=CARTESIAN_POINT('Ctrl Pts',(-3.00774853500006,5.2,-3.42235915000002));
#321060=CARTESIAN_POINT('Ctrl Pts',(-3.00774853500006,2.2,-3.42235915000002));
#321061=CARTESIAN_POINT('Ctrl Pts',(-3.00825737200006,12.2,-3.42465294000001));
#321062=CARTESIAN_POINT('Ctrl Pts',(-3.00825737200006,5.2,-3.42465294000001));
#321063=CARTESIAN_POINT('Ctrl Pts',(-3.00825737200006,2.2,-3.42465294000001));
#321064=CARTESIAN_POINT('Ctrl Pts',(-3.00876454800005,12.2,-3.42695087200001));
#321065=CARTESIAN_POINT('Ctrl Pts',(-3.00876454800005,5.2,-3.42695087200001));
#321066=CARTESIAN_POINT('Ctrl Pts',(-3.00876454800005,2.2,-3.42695087200001));
#321067=CARTESIAN_POINT('Ctrl Pts',(-3.00927005500006,12.2,-3.42925293800001));
#321068=CARTESIAN_POINT('Ctrl Pts',(-3.00927005500006,5.2,-3.42925293800001));
#321069=CARTESIAN_POINT('Ctrl Pts',(-3.00927005500006,2.2,-3.42925293800001));
#321070=CARTESIAN_POINT('Ctrl Pts',(-3.00977388500006,12.2,-3.43155913500001));
#321071=CARTESIAN_POINT('Ctrl Pts',(-3.00977388500006,5.2,-3.43155913500001));
#321072=CARTESIAN_POINT('Ctrl Pts',(-3.00977388500006,2.2,-3.43155913500001));
#321073=CARTESIAN_POINT('Ctrl Pts',(-3.01027602900006,12.2,-3.43386945700002));
#321074=CARTESIAN_POINT('Ctrl Pts',(-3.01027602900006,5.2,-3.43386945700002));
#321075=CARTESIAN_POINT('Ctrl Pts',(-3.01027602900006,2.2,-3.43386945700002));
#321076=CARTESIAN_POINT('Ctrl Pts',(-3.01077647900006,12.2,-3.43618389900001));
#321077=CARTESIAN_POINT('Ctrl Pts',(-3.01077647900006,5.2,-3.43618389900001));
#321078=CARTESIAN_POINT('Ctrl Pts',(-3.01077647900006,2.2,-3.43618389900001));
#321079=CARTESIAN_POINT('Ctrl Pts',(-3.01127522800006,12.2,-3.43850245700001));
#321080=CARTESIAN_POINT('Ctrl Pts',(-3.01127522800006,5.2,-3.43850245700001));
#321081=CARTESIAN_POINT('Ctrl Pts',(-3.01127522800006,2.2,-3.43850245700001));
#321082=CARTESIAN_POINT('Ctrl Pts',(-3.01177226700006,12.2,-3.44082512600002));
#321083=CARTESIAN_POINT('Ctrl Pts',(-3.01177226700006,5.2,-3.44082512600002));
#321084=CARTESIAN_POINT('Ctrl Pts',(-3.01177226700006,2.2,-3.44082512600002));
#321085=CARTESIAN_POINT('Ctrl Pts',(-3.01226758800006,12.2,-3.44315189900001));
#321086=CARTESIAN_POINT('Ctrl Pts',(-3.01226758800006,5.2,-3.44315189900001));
#321087=CARTESIAN_POINT('Ctrl Pts',(-3.01226758800006,2.2,-3.44315189900001));
#321088=CARTESIAN_POINT('Ctrl Pts',(-3.01276118200006,12.2,-3.44548277300001));
#321089=CARTESIAN_POINT('Ctrl Pts',(-3.01276118200006,5.2,-3.44548277300001));
#321090=CARTESIAN_POINT('Ctrl Pts',(-3.01276118200006,2.2,-3.44548277300001));
#321091=CARTESIAN_POINT('Ctrl Pts',(-3.01325304300006,12.2,-3.44781774300001));
#321092=CARTESIAN_POINT('Ctrl Pts',(-3.01325304300006,5.2,-3.44781774300001));
#321093=CARTESIAN_POINT('Ctrl Pts',(-3.01325304300006,2.2,-3.44781774300001));
#321094=CARTESIAN_POINT('Ctrl Pts',(-3.01374316200006,12.2,-3.45015680500001));
#321095=CARTESIAN_POINT('Ctrl Pts',(-3.01374316200006,5.2,-3.45015680500001));
#321096=CARTESIAN_POINT('Ctrl Pts',(-3.01374316200006,2.2,-3.45015680500001));
#321097=CARTESIAN_POINT('Ctrl Pts',(-3.01423153200005,12.2,-3.45249995200001));
#321098=CARTESIAN_POINT('Ctrl Pts',(-3.01423153200005,5.2,-3.45249995200001));
#321099=CARTESIAN_POINT('Ctrl Pts',(-3.01423153200005,2.2,-3.45249995200001));
#321100=CARTESIAN_POINT('Ctrl Pts',(-3.01471814300006,12.2,-3.45484718000002));
#321101=CARTESIAN_POINT('Ctrl Pts',(-3.01471814300006,5.2,-3.45484718000002));
#321102=CARTESIAN_POINT('Ctrl Pts',(-3.01471814300006,2.2,-3.45484718000002));
#321103=CARTESIAN_POINT('Ctrl Pts',(-3.01520298700006,12.2,-3.45719848300002));
#321104=CARTESIAN_POINT('Ctrl Pts',(-3.01520298700006,5.2,-3.45719848300002));
#321105=CARTESIAN_POINT('Ctrl Pts',(-3.01520298700006,2.2,-3.45719848300002));
#321106=CARTESIAN_POINT('Ctrl Pts',(-3.01568605800006,12.2,-3.45955385800002));
#321107=CARTESIAN_POINT('Ctrl Pts',(-3.01568605800006,5.2,-3.45955385800002));
#321108=CARTESIAN_POINT('Ctrl Pts',(-3.01568605800006,2.2,-3.45955385800002));
#321109=CARTESIAN_POINT('Ctrl Pts',(-3.01616734800006,12.2,-3.46191329900002));
#321110=CARTESIAN_POINT('Ctrl Pts',(-3.01616734800006,5.2,-3.46191329900002));
#321111=CARTESIAN_POINT('Ctrl Pts',(-3.01616734800006,2.2,-3.46191329900002));
#321112=CARTESIAN_POINT('Ctrl Pts',(-3.01664684800006,12.2,-3.46427680200001));
#321113=CARTESIAN_POINT('Ctrl Pts',(-3.01664684800006,5.2,-3.46427680200001));
#321114=CARTESIAN_POINT('Ctrl Pts',(-3.01664684800006,2.2,-3.46427680200001));
#321115=CARTESIAN_POINT('Ctrl Pts',(-3.01712455000006,12.2,-3.46664436100002));
#321116=CARTESIAN_POINT('Ctrl Pts',(-3.01712455000006,5.2,-3.46664436100002));
#321117=CARTESIAN_POINT('Ctrl Pts',(-3.01712455000006,2.2,-3.46664436100002));
#321118=CARTESIAN_POINT('Ctrl Pts',(-3.01760044700006,12.2,-3.46901597100001));
#321119=CARTESIAN_POINT('Ctrl Pts',(-3.01760044700006,5.2,-3.46901597100001));
#321120=CARTESIAN_POINT('Ctrl Pts',(-3.01760044700006,2.2,-3.46901597100001));
#321121=CARTESIAN_POINT('Ctrl Pts',(-3.01807453000006,12.2,-3.47139162600001));
#321122=CARTESIAN_POINT('Ctrl Pts',(-3.01807453000006,5.2,-3.47139162600001));
#321123=CARTESIAN_POINT('Ctrl Pts',(-3.01807453000006,2.2,-3.47139162600001));
#321124=CARTESIAN_POINT('Ctrl Pts',(-3.01854679200006,12.2,-3.47377132400001));
#321125=CARTESIAN_POINT('Ctrl Pts',(-3.01854679200006,5.2,-3.47377132400001));
#321126=CARTESIAN_POINT('Ctrl Pts',(-3.01854679200006,2.2,-3.47377132400001));
#321127=CARTESIAN_POINT('Ctrl Pts',(-3.01901722500005,12.2,-3.47615505700002));
#321128=CARTESIAN_POINT('Ctrl Pts',(-3.01901722500005,5.2,-3.47615505700002));
#321129=CARTESIAN_POINT('Ctrl Pts',(-3.01901722500005,2.2,-3.47615505700002));
#321130=CARTESIAN_POINT('Ctrl Pts',(-3.01948582200006,12.2,-3.47854282200001));
#321131=CARTESIAN_POINT('Ctrl Pts',(-3.01948582200006,5.2,-3.47854282200001));
#321132=CARTESIAN_POINT('Ctrl Pts',(-3.01948582200006,2.2,-3.47854282200001));
#321133=CARTESIAN_POINT('Ctrl Pts',(-3.01995257400006,12.2,-3.48093461300001));
#321134=CARTESIAN_POINT('Ctrl Pts',(-3.01995257400006,5.2,-3.48093461300001));
#321135=CARTESIAN_POINT('Ctrl Pts',(-3.01995257400006,2.2,-3.48093461300001));
#321136=CARTESIAN_POINT('Ctrl Pts',(-3.02041747200006,12.2,-3.48333042600002));
#321137=CARTESIAN_POINT('Ctrl Pts',(-3.02041747200006,5.2,-3.48333042600002));
#321138=CARTESIAN_POINT('Ctrl Pts',(-3.02041747200006,2.2,-3.48333042600002));
#321139=CARTESIAN_POINT('Ctrl Pts',(-3.02088051200006,12.2,-3.48573025600002));
#321140=CARTESIAN_POINT('Ctrl Pts',(-3.02088051200006,5.2,-3.48573025600002));
#321141=CARTESIAN_POINT('Ctrl Pts',(-3.02088051200006,2.2,-3.48573025600002));
#321142=CARTESIAN_POINT('Ctrl Pts',(-3.02134168300006,12.2,-3.48813409600002));
#321143=CARTESIAN_POINT('Ctrl Pts',(-3.02134168300006,5.2,-3.48813409600002));
#321144=CARTESIAN_POINT('Ctrl Pts',(-3.02134168300006,2.2,-3.48813409600002));
#321145=CARTESIAN_POINT('Ctrl Pts',(-3.02180097900006,12.2,-3.49054194300002));
#321146=CARTESIAN_POINT('Ctrl Pts',(-3.02180097900006,5.2,-3.49054194300002));
#321147=CARTESIAN_POINT('Ctrl Pts',(-3.02180097900006,2.2,-3.49054194300002));
#321148=CARTESIAN_POINT('Ctrl Pts',(-3.02225839100006,12.2,-3.49295379000001));
#321149=CARTESIAN_POINT('Ctrl Pts',(-3.02225839100006,5.2,-3.49295379000001));
#321150=CARTESIAN_POINT('Ctrl Pts',(-3.02225839100006,2.2,-3.49295379000001));
#321151=CARTESIAN_POINT('Ctrl Pts',(-3.02271391300006,12.2,-3.49536963500002));
#321152=CARTESIAN_POINT('Ctrl Pts',(-3.02271391300006,5.2,-3.49536963500002));
#321153=CARTESIAN_POINT('Ctrl Pts',(-3.02271391300006,2.2,-3.49536963500002));
#321154=CARTESIAN_POINT('Ctrl Pts',(-3.02316753600006,12.2,-3.49778947100001));
#321155=CARTESIAN_POINT('Ctrl Pts',(-3.02316753600006,5.2,-3.49778947100001));
#321156=CARTESIAN_POINT('Ctrl Pts',(-3.02316753600006,2.2,-3.49778947100001));
#321157=CARTESIAN_POINT('Ctrl Pts',(-3.02361925200006,12.2,-3.50021329300001));
#321158=CARTESIAN_POINT('Ctrl Pts',(-3.02361925200006,5.2,-3.50021329300001));
#321159=CARTESIAN_POINT('Ctrl Pts',(-3.02361925200006,2.2,-3.50021329300001));
#321160=CARTESIAN_POINT('Ctrl Pts',(-3.02406905400006,12.2,-3.50264109700001));
#321161=CARTESIAN_POINT('Ctrl Pts',(-3.02406905400006,5.2,-3.50264109700001));
#321162=CARTESIAN_POINT('Ctrl Pts',(-3.02406905400006,2.2,-3.50264109700001));
#321163=CARTESIAN_POINT('Ctrl Pts',(-3.02451693500006,12.2,-3.50507287600001));
#321164=CARTESIAN_POINT('Ctrl Pts',(-3.02451693500006,5.2,-3.50507287600001));
#321165=CARTESIAN_POINT('Ctrl Pts',(-3.02451693500006,2.2,-3.50507287600001));
#321166=CARTESIAN_POINT('Ctrl Pts',(-3.02496288600006,12.2,-3.50750862700002));
#321167=CARTESIAN_POINT('Ctrl Pts',(-3.02496288600006,5.2,-3.50750862700002));
#321168=CARTESIAN_POINT('Ctrl Pts',(-3.02496288600006,2.2,-3.50750862700002));
#321169=CARTESIAN_POINT('Ctrl Pts',(-3.02540690200006,12.2,-3.50994834400002));
#321170=CARTESIAN_POINT('Ctrl Pts',(-3.02540690200006,5.2,-3.50994834400002));
#321171=CARTESIAN_POINT('Ctrl Pts',(-3.02540690200006,2.2,-3.50994834400002));
#321172=CARTESIAN_POINT('Ctrl Pts',(-3.02584897300005,12.2,-3.51239202200002));
#321173=CARTESIAN_POINT('Ctrl Pts',(-3.02584897300005,5.2,-3.51239202200002));
#321174=CARTESIAN_POINT('Ctrl Pts',(-3.02584897300005,2.2,-3.51239202200002));
#321175=CARTESIAN_POINT('Ctrl Pts',(-3.02628909100005,12.2,-3.51483965700002));
#321176=CARTESIAN_POINT('Ctrl Pts',(-3.02628909100005,5.2,-3.51483965700002));
#321177=CARTESIAN_POINT('Ctrl Pts',(-3.02628909100005,2.2,-3.51483965700002));
#321178=CARTESIAN_POINT('Ctrl Pts',(-3.02672725000006,12.2,-3.51729124200002));
#321179=CARTESIAN_POINT('Ctrl Pts',(-3.02672725000006,5.2,-3.51729124200002));
#321180=CARTESIAN_POINT('Ctrl Pts',(-3.02672725000006,2.2,-3.51729124200002));
#321181=CARTESIAN_POINT('Ctrl Pts',(-3.02716344200006,12.2,-3.51974677400001));
#321182=CARTESIAN_POINT('Ctrl Pts',(-3.02716344200006,5.2,-3.51974677400001));
#321183=CARTESIAN_POINT('Ctrl Pts',(-3.02716344200006,2.2,-3.51974677400001));
#321184=CARTESIAN_POINT('Ctrl Pts',(-3.02759765900006,12.2,-3.52220624600001));
#321185=CARTESIAN_POINT('Ctrl Pts',(-3.02759765900006,5.2,-3.52220624600001));
#321186=CARTESIAN_POINT('Ctrl Pts',(-3.02759765900006,2.2,-3.52220624600001));
#321187=CARTESIAN_POINT('Ctrl Pts',(-3.02802989500006,12.2,-3.52466965500001));
#321188=CARTESIAN_POINT('Ctrl Pts',(-3.02802989500006,5.2,-3.52466965500001));
#321189=CARTESIAN_POINT('Ctrl Pts',(-3.02802989500006,2.2,-3.52466965500001));
#321190=CARTESIAN_POINT('Ctrl Pts',(-3.02846014100006,12.2,-3.52713699300002));
#321191=CARTESIAN_POINT('Ctrl Pts',(-3.02846014100006,5.2,-3.52713699300002));
#321192=CARTESIAN_POINT('Ctrl Pts',(-3.02846014100006,2.2,-3.52713699300002));
#321193=CARTESIAN_POINT('Ctrl Pts',(-3.02888839000006,12.2,-3.52960825900002));
#321194=CARTESIAN_POINT('Ctrl Pts',(-3.02888839000006,5.2,-3.52960825900002));
#321195=CARTESIAN_POINT('Ctrl Pts',(-3.02888839000006,2.2,-3.52960825900002));
#321196=CARTESIAN_POINT('Ctrl Pts',(-3.02931463500005,12.2,-3.53208344400001));
#321197=CARTESIAN_POINT('Ctrl Pts',(-3.02931463500005,5.2,-3.53208344400001));
#321198=CARTESIAN_POINT('Ctrl Pts',(-3.02931463500005,2.2,-3.53208344400001));
#321199=CARTESIAN_POINT('Ctrl Pts',(-3.02973886900006,12.2,-3.53456254500002));
#321200=CARTESIAN_POINT('Ctrl Pts',(-3.02973886900006,5.2,-3.53456254500002));
#321201=CARTESIAN_POINT('Ctrl Pts',(-3.02973886900006,2.2,-3.53456254500002));
#321202=CARTESIAN_POINT('Ctrl Pts',(-3.03016108200006,12.2,-3.53704555700002));
#321203=CARTESIAN_POINT('Ctrl Pts',(-3.03016108200006,5.2,-3.53704555700002));
#321204=CARTESIAN_POINT('Ctrl Pts',(-3.03016108200006,2.2,-3.53704555700002));
#321205=CARTESIAN_POINT('Ctrl Pts',(-3.03058126900006,12.2,-3.53953247400002));
#321206=CARTESIAN_POINT('Ctrl Pts',(-3.03058126900006,5.2,-3.53953247400002));
#321207=CARTESIAN_POINT('Ctrl Pts',(-3.03058126900006,2.2,-3.53953247400002));
#321208=CARTESIAN_POINT('Ctrl Pts',(-3.03099942300005,12.2,-3.54202329100001));
#321209=CARTESIAN_POINT('Ctrl Pts',(-3.03099942300005,5.2,-3.54202329100001));
#321210=CARTESIAN_POINT('Ctrl Pts',(-3.03099942300005,2.2,-3.54202329100001));
#321211=CARTESIAN_POINT('Ctrl Pts',(-3.03141553400006,12.2,-3.54451800500001));
#321212=CARTESIAN_POINT('Ctrl Pts',(-3.03141553400006,5.2,-3.54451800500001));
#321213=CARTESIAN_POINT('Ctrl Pts',(-3.03141553400006,2.2,-3.54451800500001));
#321214=CARTESIAN_POINT('Ctrl Pts',(-3.03182959700006,12.2,-3.54701660600002));
#321215=CARTESIAN_POINT('Ctrl Pts',(-3.03182959700006,5.2,-3.54701660600002));
#321216=CARTESIAN_POINT('Ctrl Pts',(-3.03182959700006,2.2,-3.54701660600002));
#321217=CARTESIAN_POINT('Ctrl Pts',(-3.03224160400006,12.2,-3.54951909500001));
#321218=CARTESIAN_POINT('Ctrl Pts',(-3.03224160400006,5.2,-3.54951909500001));
#321219=CARTESIAN_POINT('Ctrl Pts',(-3.03224160400006,2.2,-3.54951909500001));
#321220=CARTESIAN_POINT('Ctrl Pts',(-3.03265154800005,12.2,-3.55202546300001));
#321221=CARTESIAN_POINT('Ctrl Pts',(-3.03265154800005,5.2,-3.55202546300001));
#321222=CARTESIAN_POINT('Ctrl Pts',(-3.03265154800005,2.2,-3.55202546300001));
#321223=CARTESIAN_POINT('Ctrl Pts',(-3.03305942100006,12.2,-3.55453570500002));
#321224=CARTESIAN_POINT('Ctrl Pts',(-3.03305942100006,5.2,-3.55453570500002));
#321225=CARTESIAN_POINT('Ctrl Pts',(-3.03305942100006,2.2,-3.55453570500002));
#321226=CARTESIAN_POINT('Ctrl Pts',(-3.03346521700006,12.2,-3.55704981800002));
#321227=CARTESIAN_POINT('Ctrl Pts',(-3.03346521700006,5.2,-3.55704981800002));
#321228=CARTESIAN_POINT('Ctrl Pts',(-3.03346521700006,2.2,-3.55704981800002));
#321229=CARTESIAN_POINT('Ctrl Pts',(-3.03386892600006,12.2,-3.55956779500001));
#321230=CARTESIAN_POINT('Ctrl Pts',(-3.03386892600006,5.2,-3.55956779500001));
#321231=CARTESIAN_POINT('Ctrl Pts',(-3.03386892600006,2.2,-3.55956779500001));
#321232=CARTESIAN_POINT('Ctrl Pts',(-3.03427054400006,12.2,-3.56208963200002));
#321233=CARTESIAN_POINT('Ctrl Pts',(-3.03427054400006,5.2,-3.56208963200002));
#321234=CARTESIAN_POINT('Ctrl Pts',(-3.03427054400006,2.2,-3.56208963200002));
#321235=CARTESIAN_POINT('Ctrl Pts',(-3.03467006100006,12.2,-3.56461532400001));
#321236=CARTESIAN_POINT('Ctrl Pts',(-3.03467006100006,5.2,-3.56461532400001));
#321237=CARTESIAN_POINT('Ctrl Pts',(-3.03467006100006,2.2,-3.56461532400001));
#321238=CARTESIAN_POINT('Ctrl Pts',(-3.03506747200006,12.2,-3.56714486400001));
#321239=CARTESIAN_POINT('Ctrl Pts',(-3.03506747200006,5.2,-3.56714486400001));
#321240=CARTESIAN_POINT('Ctrl Pts',(-3.03506747200006,2.2,-3.56714486400001));
#321241=CARTESIAN_POINT('Ctrl Pts',(-3.03546276900006,12.2,-3.56967824900002));
#321242=CARTESIAN_POINT('Ctrl Pts',(-3.03546276900006,5.2,-3.56967824900002));
#321243=CARTESIAN_POINT('Ctrl Pts',(-3.03546276900006,2.2,-3.56967824900002));
#321244=CARTESIAN_POINT('Ctrl Pts',(-3.03585594400006,12.2,-3.57221547200002));
#321245=CARTESIAN_POINT('Ctrl Pts',(-3.03585594400006,5.2,-3.57221547200002));
#321246=CARTESIAN_POINT('Ctrl Pts',(-3.03585594400006,2.2,-3.57221547200002));
#321247=CARTESIAN_POINT('Ctrl Pts',(-3.03624699100005,12.2,-3.57475652900002));
#321248=CARTESIAN_POINT('Ctrl Pts',(-3.03624699100005,5.2,-3.57475652900002));
#321249=CARTESIAN_POINT('Ctrl Pts',(-3.03624699100005,2.2,-3.57475652900002));
#321250=CARTESIAN_POINT('Ctrl Pts',(-3.03663590200005,12.2,-3.57730141600001));
#321251=CARTESIAN_POINT('Ctrl Pts',(-3.03663590200005,5.2,-3.57730141600001));
#321252=CARTESIAN_POINT('Ctrl Pts',(-3.03663590200005,2.2,-3.57730141600001));
#321253=CARTESIAN_POINT('Ctrl Pts',(-3.03702267000005,12.2,-3.57985012500002));
#321254=CARTESIAN_POINT('Ctrl Pts',(-3.03702267000005,5.2,-3.57985012500002));
#321255=CARTESIAN_POINT('Ctrl Pts',(-3.03702267000005,2.2,-3.57985012500002));
#321256=CARTESIAN_POINT('Ctrl Pts',(-3.03740728800005,12.2,-3.58240265400001));
#321257=CARTESIAN_POINT('Ctrl Pts',(-3.03740728800005,5.2,-3.58240265400001));
#321258=CARTESIAN_POINT('Ctrl Pts',(-3.03740728800005,2.2,-3.58240265400001));
#321259=CARTESIAN_POINT('Ctrl Pts',(-3.03778975000006,12.2,-3.58495899600001));
#321260=CARTESIAN_POINT('Ctrl Pts',(-3.03778975000006,5.2,-3.58495899600001));
#321261=CARTESIAN_POINT('Ctrl Pts',(-3.03778975000006,2.2,-3.58495899600001));
#321262=CARTESIAN_POINT('Ctrl Pts',(-3.03817004900006,12.2,-3.58751914600001));
#321263=CARTESIAN_POINT('Ctrl Pts',(-3.03817004900006,5.2,-3.58751914600001));
#321264=CARTESIAN_POINT('Ctrl Pts',(-3.03817004900006,2.2,-3.58751914600001));
#321265=CARTESIAN_POINT('Ctrl Pts',(-3.03854817600006,12.2,-3.59008310000001));
#321266=CARTESIAN_POINT('Ctrl Pts',(-3.03854817600006,5.2,-3.59008310000001));
#321267=CARTESIAN_POINT('Ctrl Pts',(-3.03854817600006,2.2,-3.59008310000001));
#321268=CARTESIAN_POINT('Ctrl Pts',(-3.03892412400006,12.2,-3.59265085000001));
#321269=CARTESIAN_POINT('Ctrl Pts',(-3.03892412400006,5.2,-3.59265085000001));
#321270=CARTESIAN_POINT('Ctrl Pts',(-3.03892412400006,2.2,-3.59265085000001));
#321271=CARTESIAN_POINT('Ctrl Pts',(-3.03929788700006,12.2,-3.59522239500001));
#321272=CARTESIAN_POINT('Ctrl Pts',(-3.03929788700006,5.2,-3.59522239500001));
#321273=CARTESIAN_POINT('Ctrl Pts',(-3.03929788700006,2.2,-3.59522239500001));
#321274=CARTESIAN_POINT('Ctrl Pts',(-3.03966945600005,12.2,-3.59779772400001));
#321275=CARTESIAN_POINT('Ctrl Pts',(-3.03966945600005,5.2,-3.59779772400001));
#321276=CARTESIAN_POINT('Ctrl Pts',(-3.03966945600005,2.2,-3.59779772400001));
#321277=CARTESIAN_POINT('Ctrl Pts',(-3.04003882600006,12.2,-3.60037683700002));
#321278=CARTESIAN_POINT('Ctrl Pts',(-3.04003882600006,5.2,-3.60037683700002));
#321279=CARTESIAN_POINT('Ctrl Pts',(-3.04003882600006,2.2,-3.60037683700002));
#321280=CARTESIAN_POINT('Ctrl Pts',(-3.04040598800006,12.2,-3.60295972600001));
#321281=CARTESIAN_POINT('Ctrl Pts',(-3.04040598800006,5.2,-3.60295972600001));
#321282=CARTESIAN_POINT('Ctrl Pts',(-3.04040598800006,2.2,-3.60295972600001));
#321283=CARTESIAN_POINT('Ctrl Pts',(-3.04077093700006,12.2,-3.60554638700001));
#321284=CARTESIAN_POINT('Ctrl Pts',(-3.04077093700006,5.2,-3.60554638700001));
#321285=CARTESIAN_POINT('Ctrl Pts',(-3.04077093700006,2.2,-3.60554638700001));
#321286=CARTESIAN_POINT('Ctrl Pts',(-3.04113366700005,12.2,-3.60813681500002));
#321287=CARTESIAN_POINT('Ctrl Pts',(-3.04113366700005,5.2,-3.60813681500002));
#321288=CARTESIAN_POINT('Ctrl Pts',(-3.04113366700005,2.2,-3.60813681500002));
#321289=CARTESIAN_POINT('Ctrl Pts',(-3.04149417000006,12.2,-3.61073100600001));
#321290=CARTESIAN_POINT('Ctrl Pts',(-3.04149417000006,5.2,-3.61073100600001));
#321291=CARTESIAN_POINT('Ctrl Pts',(-3.04149417000006,2.2,-3.61073100600001));
#321292=CARTESIAN_POINT('Ctrl Pts',(-3.04185244200006,12.2,-3.61332895400002));
#321293=CARTESIAN_POINT('Ctrl Pts',(-3.04185244200006,5.2,-3.61332895400002));
#321294=CARTESIAN_POINT('Ctrl Pts',(-3.04185244200006,2.2,-3.61332895400002));
#321295=CARTESIAN_POINT('Ctrl Pts',(-3.04220847300006,12.2,-3.61593065600001));
#321296=CARTESIAN_POINT('Ctrl Pts',(-3.04220847300006,5.2,-3.61593065600001));
#321297=CARTESIAN_POINT('Ctrl Pts',(-3.04220847300006,2.2,-3.61593065600001));
#321298=CARTESIAN_POINT('Ctrl Pts',(-3.04256225800006,12.2,-3.61853610400001));
#321299=CARTESIAN_POINT('Ctrl Pts',(-3.04256225800006,5.2,-3.61853610400001));
#321300=CARTESIAN_POINT('Ctrl Pts',(-3.04256225800006,2.2,-3.61853610400001));
#321301=CARTESIAN_POINT('Ctrl Pts',(-3.04291378800006,12.2,-3.62114529300001));
#321302=CARTESIAN_POINT('Ctrl Pts',(-3.04291378800006,5.2,-3.62114529300001));
#321303=CARTESIAN_POINT('Ctrl Pts',(-3.04291378800006,2.2,-3.62114529300001));
#321304=CARTESIAN_POINT('Ctrl Pts',(-3.04326305300005,12.2,-3.62375821500001));
#321305=CARTESIAN_POINT('Ctrl Pts',(-3.04326305300005,5.2,-3.62375821500001));
#321306=CARTESIAN_POINT('Ctrl Pts',(-3.04326305300005,2.2,-3.62375821500001));
#321307=CARTESIAN_POINT('Ctrl Pts',(-3.04361004500006,12.2,-3.62637486600002));
#321308=CARTESIAN_POINT('Ctrl Pts',(-3.04361004500006,5.2,-3.62637486600002));
#321309=CARTESIAN_POINT('Ctrl Pts',(-3.04361004500006,2.2,-3.62637486600002));
#321310=CARTESIAN_POINT('Ctrl Pts',(-3.04395475800006,12.2,-3.62899523800001));
#321311=CARTESIAN_POINT('Ctrl Pts',(-3.04395475800006,5.2,-3.62899523800001));
#321312=CARTESIAN_POINT('Ctrl Pts',(-3.04395475800006,2.2,-3.62899523800001));
#321313=CARTESIAN_POINT('Ctrl Pts',(-3.04429718300006,12.2,-3.63161932600002));
#321314=CARTESIAN_POINT('Ctrl Pts',(-3.04429718300006,5.2,-3.63161932600002));
#321315=CARTESIAN_POINT('Ctrl Pts',(-3.04429718300006,2.2,-3.63161932600002));
#321316=CARTESIAN_POINT('Ctrl Pts',(-3.04463731600006,12.2,-3.63424712900001));
#321317=CARTESIAN_POINT('Ctrl Pts',(-3.04463731600006,5.2,-3.63424712900001));
#321318=CARTESIAN_POINT('Ctrl Pts',(-3.04463731600006,2.2,-3.63424712900001));
#321319=CARTESIAN_POINT('Ctrl Pts',(-3.04497515600006,12.2,-3.63687864000001));
#321320=CARTESIAN_POINT('Ctrl Pts',(-3.04497515600006,5.2,-3.63687864000001));
#321321=CARTESIAN_POINT('Ctrl Pts',(-3.04497515600006,2.2,-3.63687864000001));
#321322=CARTESIAN_POINT('Ctrl Pts',(-3.04531069900006,12.2,-3.63951386200001));
#321323=CARTESIAN_POINT('Ctrl Pts',(-3.04531069900006,5.2,-3.63951386200001));
#321324=CARTESIAN_POINT('Ctrl Pts',(-3.04531069900006,2.2,-3.63951386200001));
#321325=CARTESIAN_POINT('Ctrl Pts',(-3.04557729400006,12.2,-3.64162500500001));
#321326=CARTESIAN_POINT('Ctrl Pts',(-3.04557729400006,5.2,-3.64162500500001));
#321327=CARTESIAN_POINT('Ctrl Pts',(-3.04557729400006,2.2,-3.64162500500001));
#321328=CARTESIAN_POINT('Ctrl Pts',(-3.04577620700006,12.2,-3.64321003100001));
#321329=CARTESIAN_POINT('Ctrl Pts',(-3.04577620700006,5.2,-3.64321003100001));
#321330=CARTESIAN_POINT('Ctrl Pts',(-3.04577620700006,2.2,-3.64321003100001));
#321331=CARTESIAN_POINT('Ctrl Pts',(-3.04590835500006,12.2,-3.64426745700001));
#321332=CARTESIAN_POINT('Ctrl Pts',(-3.04590835500006,5.2,-3.64426745700001));
#321333=CARTESIAN_POINT('Ctrl Pts',(-3.04590835500006,2.2,-3.64426745700001));
#321334=CARTESIAN_POINT('Ctrl Pts',(-3.04597431500006,12.2,-3.64479635500001));
#321335=CARTESIAN_POINT('Ctrl Pts',(-3.04597431500006,5.2,-3.64479635500001));
#321336=CARTESIAN_POINT('Ctrl Pts',(-3.04597431500006,2.2,-3.64479635500001));
#321337=CARTESIAN_POINT('',(-3.04597431500006,2.7,-3.64479635500001));
#321338=CARTESIAN_POINT('',(-3.04597431500006,12.2,-3.64479635500001));
#321339=CARTESIAN_POINT('Ctrl Pts',(-2.77432738100006,2.7,-2.87279823800001));
#321340=CARTESIAN_POINT('Ctrl Pts',(-2.7744374764468,2.7,-2.87291314750764));
#321341=CARTESIAN_POINT('Ctrl Pts',(-2.77454645880482,2.69999999999987,
-2.87302912203624));
#321342=CARTESIAN_POINT('Ctrl Pts',(-2.77488192258474,2.69999999999987,
-2.8733877460855));
#321343=CARTESIAN_POINT('Ctrl Pts',(-2.77511779315,2.7,-2.87364373929698));
#321344=CARTESIAN_POINT('Ctrl Pts',(-2.77611559716086,2.7,-2.87473558902309));
#321345=CARTESIAN_POINT('Ctrl Pts',(-2.77693139030848,2.7,-2.87565470358675));
#321346=CARTESIAN_POINT('Ctrl Pts',(-2.7804778170359,2.7,-2.87971816338106));
#321347=CARTESIAN_POINT('Ctrl Pts',(-2.78335042552836,2.7,-2.88320615918335));
#321348=CARTESIAN_POINT('Ctrl Pts',(-2.79571151680306,2.7,-2.89872292454845));
#321349=CARTESIAN_POINT('Ctrl Pts',(-2.80534829486808,2.7,-2.91230134672957));
#321350=CARTESIAN_POINT('Ctrl Pts',(-2.83882810873472,2.7,-2.96274864644993));
#321351=CARTESIAN_POINT('Ctrl Pts',(-2.86724824082749,2.7,-3.01294763423819));
#321352=CARTESIAN_POINT('Ctrl Pts',(-2.9494517880223,2.7,-3.19589938056903));
#321353=CARTESIAN_POINT('Ctrl Pts',(-3.01313420540364,2.7,-3.38146906140652));
#321354=CARTESIAN_POINT('Ctrl Pts',(-3.04597431500006,2.7,-3.64479635500001));
#321355=CARTESIAN_POINT('Origin',(-5.66300478732629E-14,15.2,-1.77635683940025E-14));
#321356=CARTESIAN_POINT('',(-2.77990780000006,2.7,-3.85157274700001));
#321357=CARTESIAN_POINT('',(-2.77990780000006,12.2,-3.85157274700001));
#321358=CARTESIAN_POINT('Origin',(-5.66300478732629E-14,2.7,-1.92943768261394E-14));
#321359=CARTESIAN_POINT('Ctrl Pts',(-2.77990780000006,12.2,-3.85157274700001));
#321360=CARTESIAN_POINT('Ctrl Pts',(-2.77990780000006,5.2,-3.85157274700001));
#321361=CARTESIAN_POINT('Ctrl Pts',(-2.77990780000006,2.2,-3.85157274700001));
#321362=CARTESIAN_POINT('Ctrl Pts',(-2.77941156100006,12.2,-3.85137824500001));
#321363=CARTESIAN_POINT('Ctrl Pts',(-2.77941156100006,5.2,-3.85137824500001));
#321364=CARTESIAN_POINT('Ctrl Pts',(-2.77941156100006,2.2,-3.85137824500001));
#321365=CARTESIAN_POINT('Ctrl Pts',(-2.77841949900006,12.2,-3.85098910900001));
#321366=CARTESIAN_POINT('Ctrl Pts',(-2.77841949900006,5.2,-3.85098910900001));
#321367=CARTESIAN_POINT('Ctrl Pts',(-2.77841949900006,2.2,-3.85098910900001));
#321368=CARTESIAN_POINT('Ctrl Pts',(-2.77693265500006,12.2,-3.85040501300002));
#321369=CARTESIAN_POINT('Ctrl Pts',(-2.77693265500006,5.2,-3.85040501300002));
#321370=CARTESIAN_POINT('Ctrl Pts',(-2.77693265500006,2.2,-3.85040501300002));
#321371=CARTESIAN_POINT('Ctrl Pts',(-2.77495269300006,12.2,-3.84962543000002));
#321372=CARTESIAN_POINT('Ctrl Pts',(-2.77495269300006,5.2,-3.84962543000002));
#321373=CARTESIAN_POINT('Ctrl Pts',(-2.77495269300006,2.2,-3.84962543000002));
#321374=CARTESIAN_POINT('Ctrl Pts',(-2.77248190100006,12.2,-3.84864964100001));
#321375=CARTESIAN_POINT('Ctrl Pts',(-2.77248190100006,5.2,-3.84864964100001));
#321376=CARTESIAN_POINT('Ctrl Pts',(-2.77248190100006,2.2,-3.84864964100001));
#321377=CARTESIAN_POINT('Ctrl Pts',(-2.77001526900006,12.2,-3.84767254100002));
#321378=CARTESIAN_POINT('Ctrl Pts',(-2.77001526900006,5.2,-3.84767254100002));
#321379=CARTESIAN_POINT('Ctrl Pts',(-2.77001526900006,2.2,-3.84767254100002));
#321380=CARTESIAN_POINT('Ctrl Pts',(-2.76755280100006,12.2,-3.84669413500002));
#321381=CARTESIAN_POINT('Ctrl Pts',(-2.76755280100006,5.2,-3.84669413500002));
#321382=CARTESIAN_POINT('Ctrl Pts',(-2.76755280100006,2.2,-3.84669413500002));
#321383=CARTESIAN_POINT('Ctrl Pts',(-2.76509449600006,12.2,-3.84571442400001));
#321384=CARTESIAN_POINT('Ctrl Pts',(-2.76509449600006,5.2,-3.84571442400001));
#321385=CARTESIAN_POINT('Ctrl Pts',(-2.76509449600006,2.2,-3.84571442400001));
#321386=CARTESIAN_POINT('Ctrl Pts',(-2.76264035700006,12.2,-3.84473341500001));
#321387=CARTESIAN_POINT('Ctrl Pts',(-2.76264035700006,5.2,-3.84473341500001));
#321388=CARTESIAN_POINT('Ctrl Pts',(-2.76264035700006,2.2,-3.84473341500001));
#321389=CARTESIAN_POINT('Ctrl Pts',(-2.76019038700006,12.2,-3.84375111500002));
#321390=CARTESIAN_POINT('Ctrl Pts',(-2.76019038700006,5.2,-3.84375111500002));
#321391=CARTESIAN_POINT('Ctrl Pts',(-2.76019038700006,2.2,-3.84375111500002));
#321392=CARTESIAN_POINT('Ctrl Pts',(-2.75774459100006,12.2,-3.84276753400002));
#321393=CARTESIAN_POINT('Ctrl Pts',(-2.75774459100006,5.2,-3.84276753400002));
#321394=CARTESIAN_POINT('Ctrl Pts',(-2.75774459100006,2.2,-3.84276753400002));
#321395=CARTESIAN_POINT('Ctrl Pts',(-2.75530297200006,12.2,-3.84178268000001));
#321396=CARTESIAN_POINT('Ctrl Pts',(-2.75530297200006,5.2,-3.84178268000001));
#321397=CARTESIAN_POINT('Ctrl Pts',(-2.75530297200006,2.2,-3.84178268000001));
#321398=CARTESIAN_POINT('Ctrl Pts',(-2.75286553500006,12.2,-3.84079656400001));
#321399=CARTESIAN_POINT('Ctrl Pts',(-2.75286553500006,5.2,-3.84079656400001));
#321400=CARTESIAN_POINT('Ctrl Pts',(-2.75286553500006,2.2,-3.84079656400001));
#321401=CARTESIAN_POINT('Ctrl Pts',(-2.75043228400006,12.2,-3.83980919600001));
#321402=CARTESIAN_POINT('Ctrl Pts',(-2.75043228400006,5.2,-3.83980919600001));
#321403=CARTESIAN_POINT('Ctrl Pts',(-2.75043228400006,2.2,-3.83980919600001));
#321404=CARTESIAN_POINT('Ctrl Pts',(-2.74800322200006,12.2,-3.83882058400001));
#321405=CARTESIAN_POINT('Ctrl Pts',(-2.74800322200006,5.2,-3.83882058400001));
#321406=CARTESIAN_POINT('Ctrl Pts',(-2.74800322200006,2.2,-3.83882058400001));
#321407=CARTESIAN_POINT('Ctrl Pts',(-2.74557835200006,12.2,-3.83783073700001));
#321408=CARTESIAN_POINT('Ctrl Pts',(-2.74557835200006,5.2,-3.83783073700001));
#321409=CARTESIAN_POINT('Ctrl Pts',(-2.74557835200006,2.2,-3.83783073700001));
#321410=CARTESIAN_POINT('Ctrl Pts',(-2.74315767900006,12.2,-3.83683966200001));
#321411=CARTESIAN_POINT('Ctrl Pts',(-2.74315767900006,5.2,-3.83683966200001));
#321412=CARTESIAN_POINT('Ctrl Pts',(-2.74315767900006,2.2,-3.83683966200001));
#321413=CARTESIAN_POINT('Ctrl Pts',(-2.74074120400006,12.2,-3.83584736600001));
#321414=CARTESIAN_POINT('Ctrl Pts',(-2.74074120400006,5.2,-3.83584736600001));
#321415=CARTESIAN_POINT('Ctrl Pts',(-2.74074120400006,2.2,-3.83584736600001));
#321416=CARTESIAN_POINT('Ctrl Pts',(-2.73832893100006,12.2,-3.83485385600002));
#321417=CARTESIAN_POINT('Ctrl Pts',(-2.73832893100006,5.2,-3.83485385600002));
#321418=CARTESIAN_POINT('Ctrl Pts',(-2.73832893100006,2.2,-3.83485385600002));
#321419=CARTESIAN_POINT('Ctrl Pts',(-2.73592086200006,12.2,-3.83385914000002));
#321420=CARTESIAN_POINT('Ctrl Pts',(-2.73592086200006,5.2,-3.83385914000002));
#321421=CARTESIAN_POINT('Ctrl Pts',(-2.73592086200006,2.2,-3.83385914000002));
#321422=CARTESIAN_POINT('Ctrl Pts',(-2.73351700100006,12.2,-3.83286322600001));
#321423=CARTESIAN_POINT('Ctrl Pts',(-2.73351700100006,5.2,-3.83286322600001));
#321424=CARTESIAN_POINT('Ctrl Pts',(-2.73351700100006,2.2,-3.83286322600001));
#321425=CARTESIAN_POINT('Ctrl Pts',(-2.73111735300006,12.2,-3.83186612200001));
#321426=CARTESIAN_POINT('Ctrl Pts',(-2.73111735300006,5.2,-3.83186612200001));
#321427=CARTESIAN_POINT('Ctrl Pts',(-2.73111735300006,2.2,-3.83186612200001));
#321428=CARTESIAN_POINT('Ctrl Pts',(-2.72872191700006,12.2,-3.83086783600001));
#321429=CARTESIAN_POINT('Ctrl Pts',(-2.72872191700006,5.2,-3.83086783600001));
#321430=CARTESIAN_POINT('Ctrl Pts',(-2.72872191700006,2.2,-3.83086783600001));
#321431=CARTESIAN_POINT('Ctrl Pts',(-2.72633070100006,12.2,-3.82986837600002));
#321432=CARTESIAN_POINT('Ctrl Pts',(-2.72633070100006,5.2,-3.82986837600002));
#321433=CARTESIAN_POINT('Ctrl Pts',(-2.72633070100006,2.2,-3.82986837600002));
#321434=CARTESIAN_POINT('Ctrl Pts',(-2.72394370500006,12.2,-3.82886775100001));
#321435=CARTESIAN_POINT('Ctrl Pts',(-2.72394370500006,5.2,-3.82886775100001));
#321436=CARTESIAN_POINT('Ctrl Pts',(-2.72394370500006,2.2,-3.82886775100001));
#321437=CARTESIAN_POINT('Ctrl Pts',(-2.72156093400006,12.2,-3.82786597100001));
#321438=CARTESIAN_POINT('Ctrl Pts',(-2.72156093400006,5.2,-3.82786597100001));
#321439=CARTESIAN_POINT('Ctrl Pts',(-2.72156093400006,2.2,-3.82786597100001));
#321440=CARTESIAN_POINT('Ctrl Pts',(-2.71918239200006,12.2,-3.82686304200002));
#321441=CARTESIAN_POINT('Ctrl Pts',(-2.71918239200006,5.2,-3.82686304200002));
#321442=CARTESIAN_POINT('Ctrl Pts',(-2.71918239200006,2.2,-3.82686304200002));
#321443=CARTESIAN_POINT('Ctrl Pts',(-2.71680808000006,12.2,-3.82585897200002));
#321444=CARTESIAN_POINT('Ctrl Pts',(-2.71680808000006,5.2,-3.82585897200002));
#321445=CARTESIAN_POINT('Ctrl Pts',(-2.71680808000006,2.2,-3.82585897200002));
#321446=CARTESIAN_POINT('Ctrl Pts',(-2.71443800200006,12.2,-3.82485377000001));
#321447=CARTESIAN_POINT('Ctrl Pts',(-2.71443800200006,5.2,-3.82485377000001));
#321448=CARTESIAN_POINT('Ctrl Pts',(-2.71443800200006,2.2,-3.82485377000001));
#321449=CARTESIAN_POINT('Ctrl Pts',(-2.71207216300006,12.2,-3.82384744400001));
#321450=CARTESIAN_POINT('Ctrl Pts',(-2.71207216300006,5.2,-3.82384744400001));
#321451=CARTESIAN_POINT('Ctrl Pts',(-2.71207216300006,2.2,-3.82384744400001));
#321452=CARTESIAN_POINT('Ctrl Pts',(-2.70971056400006,12.2,-3.82284000200002));
#321453=CARTESIAN_POINT('Ctrl Pts',(-2.70971056400006,5.2,-3.82284000200002));
#321454=CARTESIAN_POINT('Ctrl Pts',(-2.70971056400006,2.2,-3.82284000200002));
#321455=CARTESIAN_POINT('Ctrl Pts',(-2.70735320900005,12.2,-3.82183145200001));
#321456=CARTESIAN_POINT('Ctrl Pts',(-2.70735320900005,5.2,-3.82183145200001));
#321457=CARTESIAN_POINT('Ctrl Pts',(-2.70735320900005,2.2,-3.82183145200001));
#321458=CARTESIAN_POINT('Ctrl Pts',(-2.70500010100006,12.2,-3.82082180200001));
#321459=CARTESIAN_POINT('Ctrl Pts',(-2.70500010100006,5.2,-3.82082180200001));
#321460=CARTESIAN_POINT('Ctrl Pts',(-2.70500010100006,2.2,-3.82082180200001));
#321461=CARTESIAN_POINT('Ctrl Pts',(-2.70265124300006,12.2,-3.81981106100001));
#321462=CARTESIAN_POINT('Ctrl Pts',(-2.70265124300006,5.2,-3.81981106100001));
#321463=CARTESIAN_POINT('Ctrl Pts',(-2.70265124300006,2.2,-3.81981106100001));
#321464=CARTESIAN_POINT('Ctrl Pts',(-2.70030663800005,12.2,-3.81879923700001));
#321465=CARTESIAN_POINT('Ctrl Pts',(-2.70030663800005,5.2,-3.81879923700001));
#321466=CARTESIAN_POINT('Ctrl Pts',(-2.70030663800005,2.2,-3.81879923700001));
#321467=CARTESIAN_POINT('Ctrl Pts',(-2.69796629100005,12.2,-3.81778633700002));
#321468=CARTESIAN_POINT('Ctrl Pts',(-2.69796629100005,5.2,-3.81778633700002));
#321469=CARTESIAN_POINT('Ctrl Pts',(-2.69796629100005,2.2,-3.81778633700002));
#321470=CARTESIAN_POINT('Ctrl Pts',(-2.69563020300006,12.2,-3.81677237200002));
#321471=CARTESIAN_POINT('Ctrl Pts',(-2.69563020300006,5.2,-3.81677237200002));
#321472=CARTESIAN_POINT('Ctrl Pts',(-2.69563020300006,2.2,-3.81677237200002));
#321473=CARTESIAN_POINT('Ctrl Pts',(-2.69329837900006,12.2,-3.81575734800002));
#321474=CARTESIAN_POINT('Ctrl Pts',(-2.69329837900006,5.2,-3.81575734800002));
#321475=CARTESIAN_POINT('Ctrl Pts',(-2.69329837900006,2.2,-3.81575734800002));
#321476=CARTESIAN_POINT('Ctrl Pts',(-2.69097082000005,12.2,-3.81474127600002));
#321477=CARTESIAN_POINT('Ctrl Pts',(-2.69097082000005,5.2,-3.81474127600002));
#321478=CARTESIAN_POINT('Ctrl Pts',(-2.69097082000005,2.2,-3.81474127600002));
#321479=CARTESIAN_POINT('Ctrl Pts',(-2.68864753000006,12.2,-3.81372416000001));
#321480=CARTESIAN_POINT('Ctrl Pts',(-2.68864753000006,5.2,-3.81372416000001));
#321481=CARTESIAN_POINT('Ctrl Pts',(-2.68864753000006,2.2,-3.81372416000001));
#321482=CARTESIAN_POINT('Ctrl Pts',(-2.68632851300006,12.2,-3.81270601300002));
#321483=CARTESIAN_POINT('Ctrl Pts',(-2.68632851300006,5.2,-3.81270601300002));
#321484=CARTESIAN_POINT('Ctrl Pts',(-2.68632851300006,2.2,-3.81270601300002));
#321485=CARTESIAN_POINT('Ctrl Pts',(-2.68401377200005,12.2,-3.81168684000002));
#321486=CARTESIAN_POINT('Ctrl Pts',(-2.68401377200005,5.2,-3.81168684000002));
#321487=CARTESIAN_POINT('Ctrl Pts',(-2.68401377200005,2.2,-3.81168684000002));
#321488=CARTESIAN_POINT('Ctrl Pts',(-2.68170330900006,12.2,-3.81066665100001));
#321489=CARTESIAN_POINT('Ctrl Pts',(-2.68170330900006,5.2,-3.81066665100001));
#321490=CARTESIAN_POINT('Ctrl Pts',(-2.68170330900006,2.2,-3.81066665100001));
#321491=CARTESIAN_POINT('Ctrl Pts',(-2.67939712900006,12.2,-3.80964545400001));
#321492=CARTESIAN_POINT('Ctrl Pts',(-2.67939712900006,5.2,-3.80964545400001));
#321493=CARTESIAN_POINT('Ctrl Pts',(-2.67939712900006,2.2,-3.80964545400001));
#321494=CARTESIAN_POINT('Ctrl Pts',(-2.67709523200006,12.2,-3.80862325700001));
#321495=CARTESIAN_POINT('Ctrl Pts',(-2.67709523200006,5.2,-3.80862325700001));
#321496=CARTESIAN_POINT('Ctrl Pts',(-2.67709523200006,2.2,-3.80862325700001));
#321497=CARTESIAN_POINT('Ctrl Pts',(-2.67479762500006,12.2,-3.80760006800001));
#321498=CARTESIAN_POINT('Ctrl Pts',(-2.67479762500006,5.2,-3.80760006800001));
#321499=CARTESIAN_POINT('Ctrl Pts',(-2.67479762500006,2.2,-3.80760006800001));
#321500=CARTESIAN_POINT('Ctrl Pts',(-2.67250430800006,12.2,-3.80657589700002));
#321501=CARTESIAN_POINT('Ctrl Pts',(-2.67250430800006,5.2,-3.80657589700002));
#321502=CARTESIAN_POINT('Ctrl Pts',(-2.67250430800006,2.2,-3.80657589700002));
#321503=CARTESIAN_POINT('Ctrl Pts',(-2.67021528500006,12.2,-3.80555075200002));
#321504=CARTESIAN_POINT('Ctrl Pts',(-2.67021528500006,5.2,-3.80555075200002));
#321505=CARTESIAN_POINT('Ctrl Pts',(-2.67021528500006,2.2,-3.80555075200002));
#321506=CARTESIAN_POINT('Ctrl Pts',(-2.66793056000005,12.2,-3.80452464100001));
#321507=CARTESIAN_POINT('Ctrl Pts',(-2.66793056000005,5.2,-3.80452464100001));
#321508=CARTESIAN_POINT('Ctrl Pts',(-2.66793056000005,2.2,-3.80452464100001));
#321509=CARTESIAN_POINT('Ctrl Pts',(-2.66565013400006,12.2,-3.80349757300001));
#321510=CARTESIAN_POINT('Ctrl Pts',(-2.66565013400006,5.2,-3.80349757300001));
#321511=CARTESIAN_POINT('Ctrl Pts',(-2.66565013400006,2.2,-3.80349757300001));
#321512=CARTESIAN_POINT('Ctrl Pts',(-2.66337401300006,12.2,-3.80246955600001));
#321513=CARTESIAN_POINT('Ctrl Pts',(-2.66337401300006,5.2,-3.80246955600001));
#321514=CARTESIAN_POINT('Ctrl Pts',(-2.66337401300006,2.2,-3.80246955600001));
#321515=CARTESIAN_POINT('Ctrl Pts',(-2.66110219800006,12.2,-3.80144059800001));
#321516=CARTESIAN_POINT('Ctrl Pts',(-2.66110219800006,5.2,-3.80144059800001));
#321517=CARTESIAN_POINT('Ctrl Pts',(-2.66110219800006,2.2,-3.80144059800001));
#321518=CARTESIAN_POINT('Ctrl Pts',(-2.65883469300006,12.2,-3.80041070900001));
#321519=CARTESIAN_POINT('Ctrl Pts',(-2.65883469300006,5.2,-3.80041070900001));
#321520=CARTESIAN_POINT('Ctrl Pts',(-2.65883469300006,2.2,-3.80041070900001));
#321521=CARTESIAN_POINT('Ctrl Pts',(-2.65657149900006,12.2,-3.79937989600001));
#321522=CARTESIAN_POINT('Ctrl Pts',(-2.65657149900006,5.2,-3.79937989600001));
#321523=CARTESIAN_POINT('Ctrl Pts',(-2.65657149900006,2.2,-3.79937989600001));
#321524=CARTESIAN_POINT('Ctrl Pts',(-2.65431262200006,12.2,-3.79834816800001));
#321525=CARTESIAN_POINT('Ctrl Pts',(-2.65431262200006,5.2,-3.79834816800001));
#321526=CARTESIAN_POINT('Ctrl Pts',(-2.65431262200006,2.2,-3.79834816800001));
#321527=CARTESIAN_POINT('Ctrl Pts',(-2.65205806300005,12.2,-3.79731553500001));
#321528=CARTESIAN_POINT('Ctrl Pts',(-2.65205806300005,5.2,-3.79731553500001));
#321529=CARTESIAN_POINT('Ctrl Pts',(-2.65205806300005,2.2,-3.79731553500001));
#321530=CARTESIAN_POINT('Ctrl Pts',(-2.64980782600006,12.2,-3.79628200300001));
#321531=CARTESIAN_POINT('Ctrl Pts',(-2.64980782600006,5.2,-3.79628200300001));
#321532=CARTESIAN_POINT('Ctrl Pts',(-2.64980782600006,2.2,-3.79628200300001));
#321533=CARTESIAN_POINT('Ctrl Pts',(-2.64756191200005,12.2,-3.79524758300001));
#321534=CARTESIAN_POINT('Ctrl Pts',(-2.64756191200005,5.2,-3.79524758300001));
#321535=CARTESIAN_POINT('Ctrl Pts',(-2.64756191200005,2.2,-3.79524758300001));
#321536=CARTESIAN_POINT('Ctrl Pts',(-2.64532032700005,12.2,-3.79421228300002));
#321537=CARTESIAN_POINT('Ctrl Pts',(-2.64532032700005,5.2,-3.79421228300002));
#321538=CARTESIAN_POINT('Ctrl Pts',(-2.64532032700005,2.2,-3.79421228300002));
#321539=CARTESIAN_POINT('Ctrl Pts',(-2.64308307200006,12.2,-3.79317611000001));
#321540=CARTESIAN_POINT('Ctrl Pts',(-2.64308307200006,5.2,-3.79317611000001));
#321541=CARTESIAN_POINT('Ctrl Pts',(-2.64308307200006,2.2,-3.79317611000001));
#321542=CARTESIAN_POINT('Ctrl Pts',(-2.64085015200005,12.2,-3.79213907500001));
#321543=CARTESIAN_POINT('Ctrl Pts',(-2.64085015200005,5.2,-3.79213907500001));
#321544=CARTESIAN_POINT('Ctrl Pts',(-2.64085015200005,2.2,-3.79213907500001));
#321545=CARTESIAN_POINT('Ctrl Pts',(-2.63862156700006,12.2,-3.79110118500002));
#321546=CARTESIAN_POINT('Ctrl Pts',(-2.63862156700006,5.2,-3.79110118500002));
#321547=CARTESIAN_POINT('Ctrl Pts',(-2.63862156700006,2.2,-3.79110118500002));
#321548=CARTESIAN_POINT('Ctrl Pts',(-2.63639732200006,12.2,-3.79006245000001));
#321549=CARTESIAN_POINT('Ctrl Pts',(-2.63639732200006,5.2,-3.79006245000001));
#321550=CARTESIAN_POINT('Ctrl Pts',(-2.63639732200006,2.2,-3.79006245000001));
#321551=CARTESIAN_POINT('Ctrl Pts',(-2.63417741900006,12.2,-3.78902287700001));
#321552=CARTESIAN_POINT('Ctrl Pts',(-2.63417741900006,5.2,-3.78902287700001));
#321553=CARTESIAN_POINT('Ctrl Pts',(-2.63417741900006,2.2,-3.78902287700001));
#321554=CARTESIAN_POINT('Ctrl Pts',(-2.63196186200005,12.2,-3.78798247500002));
#321555=CARTESIAN_POINT('Ctrl Pts',(-2.63196186200005,5.2,-3.78798247500002));
#321556=CARTESIAN_POINT('Ctrl Pts',(-2.63196186200005,2.2,-3.78798247500002));
#321557=CARTESIAN_POINT('Ctrl Pts',(-2.62975065300005,12.2,-3.78694125500001));
#321558=CARTESIAN_POINT('Ctrl Pts',(-2.62975065300005,5.2,-3.78694125500001));
#321559=CARTESIAN_POINT('Ctrl Pts',(-2.62975065300005,2.2,-3.78694125500001));
#321560=CARTESIAN_POINT('Ctrl Pts',(-2.62754379500006,12.2,-3.78589922300002));
#321561=CARTESIAN_POINT('Ctrl Pts',(-2.62754379500006,5.2,-3.78589922300002));
#321562=CARTESIAN_POINT('Ctrl Pts',(-2.62754379500006,2.2,-3.78589922300002));
#321563=CARTESIAN_POINT('Ctrl Pts',(-2.62534129200006,12.2,-3.78485639000001));
#321564=CARTESIAN_POINT('Ctrl Pts',(-2.62534129200006,5.2,-3.78485639000001));
#321565=CARTESIAN_POINT('Ctrl Pts',(-2.62534129200006,2.2,-3.78485639000001));
#321566=CARTESIAN_POINT('Ctrl Pts',(-2.62314314600005,12.2,-3.78381276300002));
#321567=CARTESIAN_POINT('Ctrl Pts',(-2.62314314600005,5.2,-3.78381276300002));
#321568=CARTESIAN_POINT('Ctrl Pts',(-2.62314314600005,2.2,-3.78381276300002));
#321569=CARTESIAN_POINT('Ctrl Pts',(-2.62094936000006,12.2,-3.78276835100001));
#321570=CARTESIAN_POINT('Ctrl Pts',(-2.62094936000006,5.2,-3.78276835100001));
#321571=CARTESIAN_POINT('Ctrl Pts',(-2.62094936000006,2.2,-3.78276835100001));
#321572=CARTESIAN_POINT('Ctrl Pts',(-2.61875993600006,12.2,-3.78172316300001));
#321573=CARTESIAN_POINT('Ctrl Pts',(-2.61875993600006,5.2,-3.78172316300001));
#321574=CARTESIAN_POINT('Ctrl Pts',(-2.61875993600006,2.2,-3.78172316300001));
#321575=CARTESIAN_POINT('Ctrl Pts',(-2.61657488000006,12.2,-3.78067720900002));
#321576=CARTESIAN_POINT('Ctrl Pts',(-2.61657488000006,5.2,-3.78067720900002));
#321577=CARTESIAN_POINT('Ctrl Pts',(-2.61657488000006,2.2,-3.78067720900002));
#321578=CARTESIAN_POINT('Ctrl Pts',(-2.61439419100005,12.2,-3.77963049600002));
#321579=CARTESIAN_POINT('Ctrl Pts',(-2.61439419100005,5.2,-3.77963049600002));
#321580=CARTESIAN_POINT('Ctrl Pts',(-2.61439419100005,2.2,-3.77963049600002));
#321581=CARTESIAN_POINT('Ctrl Pts',(-2.61221787400005,12.2,-3.77858303400001));
#321582=CARTESIAN_POINT('Ctrl Pts',(-2.61221787400005,5.2,-3.77858303400001));
#321583=CARTESIAN_POINT('Ctrl Pts',(-2.61221787400005,2.2,-3.77858303400001));
#321584=CARTESIAN_POINT('Ctrl Pts',(-2.61004593100005,12.2,-3.77753483200001));
#321585=CARTESIAN_POINT('Ctrl Pts',(-2.61004593100005,5.2,-3.77753483200001));
#321586=CARTESIAN_POINT('Ctrl Pts',(-2.61004593100005,2.2,-3.77753483200001));
#321587=CARTESIAN_POINT('Ctrl Pts',(-2.60787836600006,12.2,-3.77648589700001));
#321588=CARTESIAN_POINT('Ctrl Pts',(-2.60787836600006,5.2,-3.77648589700001));
#321589=CARTESIAN_POINT('Ctrl Pts',(-2.60787836600006,2.2,-3.77648589700001));
#321590=CARTESIAN_POINT('Ctrl Pts',(-2.60571518100006,12.2,-3.77543624000001));
#321591=CARTESIAN_POINT('Ctrl Pts',(-2.60571518100006,5.2,-3.77543624000001));
#321592=CARTESIAN_POINT('Ctrl Pts',(-2.60571518100006,2.2,-3.77543624000001));
#321593=CARTESIAN_POINT('Ctrl Pts',(-2.60355637900005,12.2,-3.77438587000002));
#321594=CARTESIAN_POINT('Ctrl Pts',(-2.60355637900005,5.2,-3.77438587000002));
#321595=CARTESIAN_POINT('Ctrl Pts',(-2.60355637900005,2.2,-3.77438587000002));
#321596=CARTESIAN_POINT('Ctrl Pts',(-2.60140196200005,12.2,-3.77333479500002));
#321597=CARTESIAN_POINT('Ctrl Pts',(-2.60140196200005,5.2,-3.77333479500002));
#321598=CARTESIAN_POINT('Ctrl Pts',(-2.60140196200005,2.2,-3.77333479500002));
#321599=CARTESIAN_POINT('Ctrl Pts',(-2.59925193500006,12.2,-3.77228302300002));
#321600=CARTESIAN_POINT('Ctrl Pts',(-2.59925193500006,5.2,-3.77228302300002));
#321601=CARTESIAN_POINT('Ctrl Pts',(-2.59925193500006,2.2,-3.77228302300002));
#321602=CARTESIAN_POINT('Ctrl Pts',(-2.59710629800006,12.2,-3.77123056500002));
#321603=CARTESIAN_POINT('Ctrl Pts',(-2.59710629800006,5.2,-3.77123056500002));
#321604=CARTESIAN_POINT('Ctrl Pts',(-2.59710629800006,2.2,-3.77123056500002));
#321605=CARTESIAN_POINT('Ctrl Pts',(-2.59496505700006,12.2,-3.77017742800001));
#321606=CARTESIAN_POINT('Ctrl Pts',(-2.59496505700006,5.2,-3.77017742800001));
#321607=CARTESIAN_POINT('Ctrl Pts',(-2.59496505700006,2.2,-3.77017742800001));
#321608=CARTESIAN_POINT('Ctrl Pts',(-2.59282821200005,12.2,-3.76912362300001));
#321609=CARTESIAN_POINT('Ctrl Pts',(-2.59282821200005,5.2,-3.76912362300001));
#321610=CARTESIAN_POINT('Ctrl Pts',(-2.59282821200005,2.2,-3.76912362300001));
#321611=CARTESIAN_POINT('Ctrl Pts',(-2.59069576700006,12.2,-3.76806915700001));
#321612=CARTESIAN_POINT('Ctrl Pts',(-2.59069576700006,5.2,-3.76806915700001));
#321613=CARTESIAN_POINT('Ctrl Pts',(-2.59069576700006,2.2,-3.76806915700001));
#321614=CARTESIAN_POINT('Ctrl Pts',(-2.58856772500006,12.2,-3.76701404000002));
#321615=CARTESIAN_POINT('Ctrl Pts',(-2.58856772500006,5.2,-3.76701404000002));
#321616=CARTESIAN_POINT('Ctrl Pts',(-2.58856772500006,2.2,-3.76701404000002));
#321617=CARTESIAN_POINT('Ctrl Pts',(-2.58644408800006,12.2,-3.76595828200001));
#321618=CARTESIAN_POINT('Ctrl Pts',(-2.58644408800006,5.2,-3.76595828200001));
#321619=CARTESIAN_POINT('Ctrl Pts',(-2.58644408800006,2.2,-3.76595828200001));
#321620=CARTESIAN_POINT('Ctrl Pts',(-2.58432486000005,12.2,-3.76490188900001));
#321621=CARTESIAN_POINT('Ctrl Pts',(-2.58432486000005,5.2,-3.76490188900001));
#321622=CARTESIAN_POINT('Ctrl Pts',(-2.58432486000005,2.2,-3.76490188900001));
#321623=CARTESIAN_POINT('Ctrl Pts',(-2.58221004200006,12.2,-3.76384487400002));
#321624=CARTESIAN_POINT('Ctrl Pts',(-2.58221004200006,5.2,-3.76384487400002));
#321625=CARTESIAN_POINT('Ctrl Pts',(-2.58221004200006,2.2,-3.76384487400002));
#321626=CARTESIAN_POINT('Ctrl Pts',(-2.58009963800006,12.2,-3.76278724400001));
#321627=CARTESIAN_POINT('Ctrl Pts',(-2.58009963800006,5.2,-3.76278724400001));
#321628=CARTESIAN_POINT('Ctrl Pts',(-2.58009963800006,2.2,-3.76278724400001));
#321629=CARTESIAN_POINT('Ctrl Pts',(-2.57799365100006,12.2,-3.76172900700002));
#321630=CARTESIAN_POINT('Ctrl Pts',(-2.57799365100006,5.2,-3.76172900700002));
#321631=CARTESIAN_POINT('Ctrl Pts',(-2.57799365100006,2.2,-3.76172900700002));
#321632=CARTESIAN_POINT('Ctrl Pts',(-2.57589208100006,12.2,-3.76067017500001));
#321633=CARTESIAN_POINT('Ctrl Pts',(-2.57589208100006,5.2,-3.76067017500001));
#321634=CARTESIAN_POINT('Ctrl Pts',(-2.57589208100006,2.2,-3.76067017500001));
#321635=CARTESIAN_POINT('Ctrl Pts',(-2.57379493500005,12.2,-3.75961075500001));
#321636=CARTESIAN_POINT('Ctrl Pts',(-2.57379493500005,5.2,-3.75961075500001));
#321637=CARTESIAN_POINT('Ctrl Pts',(-2.57379493500005,2.2,-3.75961075500001));
#321638=CARTESIAN_POINT('Ctrl Pts',(-2.57170221300006,12.2,-3.75855075600001));
#321639=CARTESIAN_POINT('Ctrl Pts',(-2.57170221300006,5.2,-3.75855075600001));
#321640=CARTESIAN_POINT('Ctrl Pts',(-2.57170221300006,2.2,-3.75855075600001));
#321641=CARTESIAN_POINT('Ctrl Pts',(-2.56961391900006,12.2,-3.75749018800001));
#321642=CARTESIAN_POINT('Ctrl Pts',(-2.56961391900006,5.2,-3.75749018800001));
#321643=CARTESIAN_POINT('Ctrl Pts',(-2.56961391900006,2.2,-3.75749018800001));
#321644=CARTESIAN_POINT('Ctrl Pts',(-2.56753005400005,12.2,-3.75642906000001));
#321645=CARTESIAN_POINT('Ctrl Pts',(-2.56753005400005,5.2,-3.75642906000001));
#321646=CARTESIAN_POINT('Ctrl Pts',(-2.56753005400005,2.2,-3.75642906000001));
#321647=CARTESIAN_POINT('Ctrl Pts',(-2.56545062200006,12.2,-3.75536738200001));
#321648=CARTESIAN_POINT('Ctrl Pts',(-2.56545062200006,5.2,-3.75536738200001));
#321649=CARTESIAN_POINT('Ctrl Pts',(-2.56545062200006,2.2,-3.75536738200001));
#321650=CARTESIAN_POINT('Ctrl Pts',(-2.56337562600006,12.2,-3.75430516100002));
#321651=CARTESIAN_POINT('Ctrl Pts',(-2.56337562600006,5.2,-3.75430516100002));
#321652=CARTESIAN_POINT('Ctrl Pts',(-2.56337562600006,2.2,-3.75430516100002));
#321653=CARTESIAN_POINT('Ctrl Pts',(-2.56130506800006,12.2,-3.75324240800001));
#321654=CARTESIAN_POINT('Ctrl Pts',(-2.56130506800006,5.2,-3.75324240800001));
#321655=CARTESIAN_POINT('Ctrl Pts',(-2.56130506800006,2.2,-3.75324240800001));
#321656=CARTESIAN_POINT('Ctrl Pts',(-2.55923894900006,12.2,-3.75217913300002));
#321657=CARTESIAN_POINT('Ctrl Pts',(-2.55923894900006,5.2,-3.75217913300002));
#321658=CARTESIAN_POINT('Ctrl Pts',(-2.55923894900006,2.2,-3.75217913300002));
#321659=CARTESIAN_POINT('Ctrl Pts',(-2.55717727500006,12.2,-3.75111534300002));
#321660=CARTESIAN_POINT('Ctrl Pts',(-2.55717727500006,5.2,-3.75111534300002));
#321661=CARTESIAN_POINT('Ctrl Pts',(-2.55717727500006,2.2,-3.75111534300002));
#321662=CARTESIAN_POINT('Ctrl Pts',(-2.55512004700006,12.2,-3.75005104800001));
#321663=CARTESIAN_POINT('Ctrl Pts',(-2.55512004700006,5.2,-3.75005104800001));
#321664=CARTESIAN_POINT('Ctrl Pts',(-2.55512004700006,2.2,-3.75005104800001));
#321665=CARTESIAN_POINT('Ctrl Pts',(-2.55306726700006,12.2,-3.74898625800002));
#321666=CARTESIAN_POINT('Ctrl Pts',(-2.55306726700006,5.2,-3.74898625800002));
#321667=CARTESIAN_POINT('Ctrl Pts',(-2.55306726700006,2.2,-3.74898625800002));
#321668=CARTESIAN_POINT('Ctrl Pts',(-2.55101893800005,12.2,-3.74792098200002));
#321669=CARTESIAN_POINT('Ctrl Pts',(-2.55101893800005,5.2,-3.74792098200002));
#321670=CARTESIAN_POINT('Ctrl Pts',(-2.55101893800005,2.2,-3.74792098200002));
#321671=CARTESIAN_POINT('Ctrl Pts',(-2.54897506300006,12.2,-3.74685523000001));
#321672=CARTESIAN_POINT('Ctrl Pts',(-2.54897506300006,5.2,-3.74685523000001));
#321673=CARTESIAN_POINT('Ctrl Pts',(-2.54897506300006,2.2,-3.74685523000001));
#321674=CARTESIAN_POINT('Ctrl Pts',(-2.54693564500006,12.2,-3.74578901000001));
#321675=CARTESIAN_POINT('Ctrl Pts',(-2.54693564500006,5.2,-3.74578901000001));
#321676=CARTESIAN_POINT('Ctrl Pts',(-2.54693564500006,2.2,-3.74578901000001));
#321677=CARTESIAN_POINT('Ctrl Pts',(-2.54490068500006,12.2,-3.74472233100001));
#321678=CARTESIAN_POINT('Ctrl Pts',(-2.54490068500006,5.2,-3.74472233100001));
#321679=CARTESIAN_POINT('Ctrl Pts',(-2.54490068500006,2.2,-3.74472233100001));
#321680=CARTESIAN_POINT('Ctrl Pts',(-2.54287018700006,12.2,-3.74365520400001));
#321681=CARTESIAN_POINT('Ctrl Pts',(-2.54287018700006,5.2,-3.74365520400001));
#321682=CARTESIAN_POINT('Ctrl Pts',(-2.54287018700006,2.2,-3.74365520400001));
#321683=CARTESIAN_POINT('Ctrl Pts',(-2.54084415400006,12.2,-3.74258763800002));
#321684=CARTESIAN_POINT('Ctrl Pts',(-2.54084415400006,5.2,-3.74258763800002));
#321685=CARTESIAN_POINT('Ctrl Pts',(-2.54084415400006,2.2,-3.74258763800002));
#321686=CARTESIAN_POINT('Ctrl Pts',(-2.53882258600005,12.2,-3.74151964200002));
#321687=CARTESIAN_POINT('Ctrl Pts',(-2.53882258600005,5.2,-3.74151964200002));
#321688=CARTESIAN_POINT('Ctrl Pts',(-2.53882258600005,2.2,-3.74151964200002));
#321689=CARTESIAN_POINT('Ctrl Pts',(-2.53680548900005,12.2,-3.74045122600001));
#321690=CARTESIAN_POINT('Ctrl Pts',(-2.53680548900005,5.2,-3.74045122600001));
#321691=CARTESIAN_POINT('Ctrl Pts',(-2.53680548900005,2.2,-3.74045122600001));
#321692=CARTESIAN_POINT('Ctrl Pts',(-2.53479286300006,12.2,-3.73938239800002));
#321693=CARTESIAN_POINT('Ctrl Pts',(-2.53479286300006,5.2,-3.73938239800002));
#321694=CARTESIAN_POINT('Ctrl Pts',(-2.53479286300006,2.2,-3.73938239800002));
#321695=CARTESIAN_POINT('Ctrl Pts',(-2.53278471100006,12.2,-3.73831316800001));
#321696=CARTESIAN_POINT('Ctrl Pts',(-2.53278471100006,5.2,-3.73831316800001));
#321697=CARTESIAN_POINT('Ctrl Pts',(-2.53278471100006,2.2,-3.73831316800001));
#321698=CARTESIAN_POINT('Ctrl Pts',(-2.53078103700005,12.2,-3.73724354700002));
#321699=CARTESIAN_POINT('Ctrl Pts',(-2.53078103700005,5.2,-3.73724354700002));
#321700=CARTESIAN_POINT('Ctrl Pts',(-2.53078103700005,2.2,-3.73724354700002));
#321701=CARTESIAN_POINT('Ctrl Pts',(-2.52878184200005,12.2,-3.73617354300002));
#321702=CARTESIAN_POINT('Ctrl Pts',(-2.52878184200005,5.2,-3.73617354300002));
#321703=CARTESIAN_POINT('Ctrl Pts',(-2.52878184200005,2.2,-3.73617354300002));
#321704=CARTESIAN_POINT('Ctrl Pts',(-2.52678712900006,12.2,-3.73510316700001));
#321705=CARTESIAN_POINT('Ctrl Pts',(-2.52678712900006,5.2,-3.73510316700001));
#321706=CARTESIAN_POINT('Ctrl Pts',(-2.52678712900006,2.2,-3.73510316700001));
#321707=CARTESIAN_POINT('Ctrl Pts',(-2.52479690100006,12.2,-3.73403242600002));
#321708=CARTESIAN_POINT('Ctrl Pts',(-2.52479690100006,5.2,-3.73403242600002));
#321709=CARTESIAN_POINT('Ctrl Pts',(-2.52479690100006,2.2,-3.73403242600002));
#321710=CARTESIAN_POINT('Ctrl Pts',(-2.52281115900006,12.2,-3.73296133000002));
#321711=CARTESIAN_POINT('Ctrl Pts',(-2.52281115900006,5.2,-3.73296133000002));
#321712=CARTESIAN_POINT('Ctrl Pts',(-2.52281115900006,2.2,-3.73296133000002));
#321713=CARTESIAN_POINT('Ctrl Pts',(-2.52082990700006,12.2,-3.73188989100001));
#321714=CARTESIAN_POINT('Ctrl Pts',(-2.52082990700006,5.2,-3.73188989100001));
#321715=CARTESIAN_POINT('Ctrl Pts',(-2.52082990700006,2.2,-3.73188989100001));
#321716=CARTESIAN_POINT('Ctrl Pts',(-2.51885314600006,12.2,-3.73081811600001));
#321717=CARTESIAN_POINT('Ctrl Pts',(-2.51885314600006,5.2,-3.73081811600001));
#321718=CARTESIAN_POINT('Ctrl Pts',(-2.51885314600006,2.2,-3.73081811600001));
#321719=CARTESIAN_POINT('Ctrl Pts',(-2.51688088000006,12.2,-3.72974601700002));
#321720=CARTESIAN_POINT('Ctrl Pts',(-2.51688088000006,5.2,-3.72974601700002));
#321721=CARTESIAN_POINT('Ctrl Pts',(-2.51688088000006,2.2,-3.72974601700002));
#321722=CARTESIAN_POINT('Ctrl Pts',(-2.51491311100006,12.2,-3.72867360100001));
#321723=CARTESIAN_POINT('Ctrl Pts',(-2.51491311100006,5.2,-3.72867360100001));
#321724=CARTESIAN_POINT('Ctrl Pts',(-2.51491311100006,2.2,-3.72867360100001));
#321725=CARTESIAN_POINT('Ctrl Pts',(-2.51294984100006,12.2,-3.72760087900001));
#321726=CARTESIAN_POINT('Ctrl Pts',(-2.51294984100006,5.2,-3.72760087900001));
#321727=CARTESIAN_POINT('Ctrl Pts',(-2.51294984100006,2.2,-3.72760087900001));
#321728=CARTESIAN_POINT('Ctrl Pts',(-2.51099107300006,12.2,-3.72652786100002));
#321729=CARTESIAN_POINT('Ctrl Pts',(-2.51099107300006,5.2,-3.72652786100002));
#321730=CARTESIAN_POINT('Ctrl Pts',(-2.51099107300006,2.2,-3.72652786100002));
#321731=CARTESIAN_POINT('Ctrl Pts',(-2.50903680800006,12.2,-3.72545455600001));
#321732=CARTESIAN_POINT('Ctrl Pts',(-2.50903680800006,5.2,-3.72545455600001));
#321733=CARTESIAN_POINT('Ctrl Pts',(-2.50903680800006,2.2,-3.72545455600001));
#321734=CARTESIAN_POINT('Ctrl Pts',(-2.50708705000006,12.2,-3.72438097300002));
#321735=CARTESIAN_POINT('Ctrl Pts',(-2.50708705000006,5.2,-3.72438097300002));
#321736=CARTESIAN_POINT('Ctrl Pts',(-2.50708705000006,2.2,-3.72438097300002));
#321737=CARTESIAN_POINT('Ctrl Pts',(-2.50514180200006,12.2,-3.72330712300001));
#321738=CARTESIAN_POINT('Ctrl Pts',(-2.50514180200006,5.2,-3.72330712300001));
#321739=CARTESIAN_POINT('Ctrl Pts',(-2.50514180200006,2.2,-3.72330712300001));
#321740=CARTESIAN_POINT('Ctrl Pts',(-2.50320106400005,12.2,-3.72223301500001));
#321741=CARTESIAN_POINT('Ctrl Pts',(-2.50320106400005,5.2,-3.72223301500001));
#321742=CARTESIAN_POINT('Ctrl Pts',(-2.50320106400005,2.2,-3.72223301500001));
#321743=CARTESIAN_POINT('Ctrl Pts',(-2.50126484000006,12.2,-3.72115866000001));
#321744=CARTESIAN_POINT('Ctrl Pts',(-2.50126484000006,5.2,-3.72115866000001));
#321745=CARTESIAN_POINT('Ctrl Pts',(-2.50126484000006,2.2,-3.72115866000001));
#321746=CARTESIAN_POINT('Ctrl Pts',(-2.49933313300006,12.2,-3.72008406500001));
#321747=CARTESIAN_POINT('Ctrl Pts',(-2.49933313300006,5.2,-3.72008406500001));
#321748=CARTESIAN_POINT('Ctrl Pts',(-2.49933313300006,2.2,-3.72008406500001));
#321749=CARTESIAN_POINT('Ctrl Pts',(-2.49740594300006,12.2,-3.71900924300002));
#321750=CARTESIAN_POINT('Ctrl Pts',(-2.49740594300006,5.2,-3.71900924300002));
#321751=CARTESIAN_POINT('Ctrl Pts',(-2.49740594300006,2.2,-3.71900924300002));
#321752=CARTESIAN_POINT('Ctrl Pts',(-2.49548327500006,12.2,-3.71793420100001));
#321753=CARTESIAN_POINT('Ctrl Pts',(-2.49548327500006,5.2,-3.71793420100001));
#321754=CARTESIAN_POINT('Ctrl Pts',(-2.49548327500006,2.2,-3.71793420100001));
#321755=CARTESIAN_POINT('Ctrl Pts',(-2.49356512900006,12.2,-3.71685895000001));
#321756=CARTESIAN_POINT('Ctrl Pts',(-2.49356512900006,5.2,-3.71685895000001));
#321757=CARTESIAN_POINT('Ctrl Pts',(-2.49356512900006,2.2,-3.71685895000001));
#321758=CARTESIAN_POINT('Ctrl Pts',(-2.49165150900006,12.2,-3.71578350000001));
#321759=CARTESIAN_POINT('Ctrl Pts',(-2.49165150900006,5.2,-3.71578350000001));
#321760=CARTESIAN_POINT('Ctrl Pts',(-2.49165150900006,2.2,-3.71578350000001));
#321761=CARTESIAN_POINT('Ctrl Pts',(-2.48974241700005,12.2,-3.71470786100002));
#321762=CARTESIAN_POINT('Ctrl Pts',(-2.48974241700005,5.2,-3.71470786100002));
#321763=CARTESIAN_POINT('Ctrl Pts',(-2.48974241700005,2.2,-3.71470786100002));
#321764=CARTESIAN_POINT('Ctrl Pts',(-2.48783785500006,12.2,-3.71363204200001));
#321765=CARTESIAN_POINT('Ctrl Pts',(-2.48783785500006,5.2,-3.71363204200001));
#321766=CARTESIAN_POINT('Ctrl Pts',(-2.48783785500006,2.2,-3.71363204200001));
#321767=CARTESIAN_POINT('Ctrl Pts',(-2.48593782500006,12.2,-3.71255605200002));
#321768=CARTESIAN_POINT('Ctrl Pts',(-2.48593782500006,5.2,-3.71255605200002));
#321769=CARTESIAN_POINT('Ctrl Pts',(-2.48593782500006,2.2,-3.71255605200002));
#321770=CARTESIAN_POINT('Ctrl Pts',(-2.48404233000006,12.2,-3.71147990400001));
#321771=CARTESIAN_POINT('Ctrl Pts',(-2.48404233000006,5.2,-3.71147990400001));
#321772=CARTESIAN_POINT('Ctrl Pts',(-2.48404233000006,2.2,-3.71147990400001));
#321773=CARTESIAN_POINT('Ctrl Pts',(-2.48215137200006,12.2,-3.71040360600002));
#321774=CARTESIAN_POINT('Ctrl Pts',(-2.48215137200006,5.2,-3.71040360600002));
#321775=CARTESIAN_POINT('Ctrl Pts',(-2.48215137200006,2.2,-3.71040360600002));
#321776=CARTESIAN_POINT('Ctrl Pts',(-2.48026495300006,12.2,-3.70932716700001));
#321777=CARTESIAN_POINT('Ctrl Pts',(-2.48026495300006,5.2,-3.70932716700001));
#321778=CARTESIAN_POINT('Ctrl Pts',(-2.48026495300006,2.2,-3.70932716700001));
#321779=CARTESIAN_POINT('Ctrl Pts',(-2.47838307600006,12.2,-3.70825059800001));
#321780=CARTESIAN_POINT('Ctrl Pts',(-2.47838307600006,5.2,-3.70825059800001));
#321781=CARTESIAN_POINT('Ctrl Pts',(-2.47838307600006,2.2,-3.70825059800001));
#321782=CARTESIAN_POINT('Ctrl Pts',(-2.47650574200006,12.2,-3.70717391000001));
#321783=CARTESIAN_POINT('Ctrl Pts',(-2.47650574200006,5.2,-3.70717391000001));
#321784=CARTESIAN_POINT('Ctrl Pts',(-2.47650574200006,2.2,-3.70717391000001));
#321785=CARTESIAN_POINT('Ctrl Pts',(-2.47463295400005,12.2,-3.70609711100002));
#321786=CARTESIAN_POINT('Ctrl Pts',(-2.47463295400005,5.2,-3.70609711100002));
#321787=CARTESIAN_POINT('Ctrl Pts',(-2.47463295400005,2.2,-3.70609711100002));
#321788=CARTESIAN_POINT('Ctrl Pts',(-2.47276471500005,12.2,-3.70502021200001));
#321789=CARTESIAN_POINT('Ctrl Pts',(-2.47276471500005,5.2,-3.70502021200001));
#321790=CARTESIAN_POINT('Ctrl Pts',(-2.47276471500005,2.2,-3.70502021200001));
#321791=CARTESIAN_POINT('Ctrl Pts',(-2.47090102700006,12.2,-3.70394322200001));
#321792=CARTESIAN_POINT('Ctrl Pts',(-2.47090102700006,5.2,-3.70394322200001));
#321793=CARTESIAN_POINT('Ctrl Pts',(-2.47090102700006,2.2,-3.70394322200001));
#321794=CARTESIAN_POINT('Ctrl Pts',(-2.46904188900006,12.2,-3.70286615300001));
#321795=CARTESIAN_POINT('Ctrl Pts',(-2.46904188900006,5.2,-3.70286615300001));
#321796=CARTESIAN_POINT('Ctrl Pts',(-2.46904188900006,2.2,-3.70286615300001));
#321797=CARTESIAN_POINT('Ctrl Pts',(-2.46718730800006,12.2,-3.70178901300001));
#321798=CARTESIAN_POINT('Ctrl Pts',(-2.46718730800006,5.2,-3.70178901300001));
#321799=CARTESIAN_POINT('Ctrl Pts',(-2.46718730800006,2.2,-3.70178901300001));
#321800=CARTESIAN_POINT('Ctrl Pts',(-2.46533728400005,12.2,-3.70071181300001));
#321801=CARTESIAN_POINT('Ctrl Pts',(-2.46533728400005,5.2,-3.70071181300001));
#321802=CARTESIAN_POINT('Ctrl Pts',(-2.46533728400005,2.2,-3.70071181300001));
#321803=CARTESIAN_POINT('Ctrl Pts',(-2.46349181900006,12.2,-3.69963456400002));
#321804=CARTESIAN_POINT('Ctrl Pts',(-2.46349181900006,5.2,-3.69963456400002));
#321805=CARTESIAN_POINT('Ctrl Pts',(-2.46349181900006,2.2,-3.69963456400002));
#321806=CARTESIAN_POINT('Ctrl Pts',(-2.46165091500006,12.2,-3.69855727400001));
#321807=CARTESIAN_POINT('Ctrl Pts',(-2.46165091500006,5.2,-3.69855727400001));
#321808=CARTESIAN_POINT('Ctrl Pts',(-2.46165091500006,2.2,-3.69855727400001));
#321809=CARTESIAN_POINT('Ctrl Pts',(-2.45981457400006,12.2,-3.69747995500001));
#321810=CARTESIAN_POINT('Ctrl Pts',(-2.45981457400006,5.2,-3.69747995500001));
#321811=CARTESIAN_POINT('Ctrl Pts',(-2.45981457400006,2.2,-3.69747995500001));
#321812=CARTESIAN_POINT('Ctrl Pts',(-2.45798280000006,12.2,-3.69640261500002));
#321813=CARTESIAN_POINT('Ctrl Pts',(-2.45798280000006,5.2,-3.69640261500002));
#321814=CARTESIAN_POINT('Ctrl Pts',(-2.45798280000006,2.2,-3.69640261500002));
#321815=CARTESIAN_POINT('Ctrl Pts',(-2.45615559300006,12.2,-3.69532526700001));
#321816=CARTESIAN_POINT('Ctrl Pts',(-2.45615559300006,5.2,-3.69532526700001));
#321817=CARTESIAN_POINT('Ctrl Pts',(-2.45615559300006,2.2,-3.69532526700001));
#321818=CARTESIAN_POINT('Ctrl Pts',(-2.45433295700006,12.2,-3.69424791900002));
#321819=CARTESIAN_POINT('Ctrl Pts',(-2.45433295700006,5.2,-3.69424791900002));
#321820=CARTESIAN_POINT('Ctrl Pts',(-2.45433295700006,2.2,-3.69424791900002));
#321821=CARTESIAN_POINT('Ctrl Pts',(-2.45251489200006,12.2,-3.69317058200001));
#321822=CARTESIAN_POINT('Ctrl Pts',(-2.45251489200006,5.2,-3.69317058200001));
#321823=CARTESIAN_POINT('Ctrl Pts',(-2.45251489200006,2.2,-3.69317058200001));
#321824=CARTESIAN_POINT('Ctrl Pts',(-2.45070140100006,12.2,-3.69209326600001));
#321825=CARTESIAN_POINT('Ctrl Pts',(-2.45070140100006,5.2,-3.69209326600001));
#321826=CARTESIAN_POINT('Ctrl Pts',(-2.45070140100006,2.2,-3.69209326600001));
#321827=CARTESIAN_POINT('Ctrl Pts',(-2.44889248600006,12.2,-3.69101598000002));
#321828=CARTESIAN_POINT('Ctrl Pts',(-2.44889248600006,5.2,-3.69101598000002));
#321829=CARTESIAN_POINT('Ctrl Pts',(-2.44889248600006,2.2,-3.69101598000002));
#321830=CARTESIAN_POINT('Ctrl Pts',(-2.44708815000005,12.2,-3.68993873700001));
#321831=CARTESIAN_POINT('Ctrl Pts',(-2.44708815000005,5.2,-3.68993873700001));
#321832=CARTESIAN_POINT('Ctrl Pts',(-2.44708815000005,2.2,-3.68993873700001));
#321833=CARTESIAN_POINT('Ctrl Pts',(-2.44528839500005,12.2,-3.68886154500002));
#321834=CARTESIAN_POINT('Ctrl Pts',(-2.44528839500005,5.2,-3.68886154500002));
#321835=CARTESIAN_POINT('Ctrl Pts',(-2.44528839500005,2.2,-3.68886154500002));
#321836=CARTESIAN_POINT('Ctrl Pts',(-2.44349322200006,12.2,-3.68778441500002));
#321837=CARTESIAN_POINT('Ctrl Pts',(-2.44349322200006,5.2,-3.68778441500002));
#321838=CARTESIAN_POINT('Ctrl Pts',(-2.44349322200006,2.2,-3.68778441500002));
#321839=CARTESIAN_POINT('Ctrl Pts',(-2.44170263400005,12.2,-3.68670735800002));
#321840=CARTESIAN_POINT('Ctrl Pts',(-2.44170263400005,5.2,-3.68670735800002));
#321841=CARTESIAN_POINT('Ctrl Pts',(-2.44170263400005,2.2,-3.68670735800002));
#321842=CARTESIAN_POINT('Ctrl Pts',(-2.43991663200006,12.2,-3.68563038300001));
#321843=CARTESIAN_POINT('Ctrl Pts',(-2.43991663200006,5.2,-3.68563038300001));
#321844=CARTESIAN_POINT('Ctrl Pts',(-2.43991663200006,2.2,-3.68563038300001));
#321845=CARTESIAN_POINT('Ctrl Pts',(-2.43813521800006,12.2,-3.68455350000001));
#321846=CARTESIAN_POINT('Ctrl Pts',(-2.43813521800006,5.2,-3.68455350000001));
#321847=CARTESIAN_POINT('Ctrl Pts',(-2.43813521800006,2.2,-3.68455350000001));
#321848=CARTESIAN_POINT('Ctrl Pts',(-2.43635839500006,12.2,-3.68347672200001));
#321849=CARTESIAN_POINT('Ctrl Pts',(-2.43635839500006,5.2,-3.68347672200001));
#321850=CARTESIAN_POINT('Ctrl Pts',(-2.43635839500006,2.2,-3.68347672200001));
#321851=CARTESIAN_POINT('Ctrl Pts',(-2.43458616500006,12.2,-3.68240005700001));
#321852=CARTESIAN_POINT('Ctrl Pts',(-2.43458616500006,5.2,-3.68240005700001));
#321853=CARTESIAN_POINT('Ctrl Pts',(-2.43458616500006,2.2,-3.68240005700001));
#321854=CARTESIAN_POINT('Ctrl Pts',(-2.43281852900005,12.2,-3.68132351600002));
#321855=CARTESIAN_POINT('Ctrl Pts',(-2.43281852900005,5.2,-3.68132351600002));
#321856=CARTESIAN_POINT('Ctrl Pts',(-2.43281852900005,2.2,-3.68132351600002));
#321857=CARTESIAN_POINT('Ctrl Pts',(-2.43105549100005,12.2,-3.68024710900002));
#321858=CARTESIAN_POINT('Ctrl Pts',(-2.43105549100005,5.2,-3.68024710900002));
#321859=CARTESIAN_POINT('Ctrl Pts',(-2.43105549100005,2.2,-3.68024710900002));
#321860=CARTESIAN_POINT('Ctrl Pts',(-2.42929705000006,12.2,-3.67917084700002));
#321861=CARTESIAN_POINT('Ctrl Pts',(-2.42929705000006,5.2,-3.67917084700002));
#321862=CARTESIAN_POINT('Ctrl Pts',(-2.42929705000006,2.2,-3.67917084700002));
#321863=CARTESIAN_POINT('Ctrl Pts',(-2.42754321100006,12.2,-3.67809474100001));
#321864=CARTESIAN_POINT('Ctrl Pts',(-2.42754321100006,5.2,-3.67809474100001));
#321865=CARTESIAN_POINT('Ctrl Pts',(-2.42754321100006,2.2,-3.67809474100001));
#321866=CARTESIAN_POINT('Ctrl Pts',(-2.42579397300006,12.2,-3.67701880000002));
#321867=CARTESIAN_POINT('Ctrl Pts',(-2.42579397300006,5.2,-3.67701880000002));
#321868=CARTESIAN_POINT('Ctrl Pts',(-2.42579397300006,2.2,-3.67701880000002));
#321869=CARTESIAN_POINT('Ctrl Pts',(-2.42404934000006,12.2,-3.67594303600002));
#321870=CARTESIAN_POINT('Ctrl Pts',(-2.42404934000006,5.2,-3.67594303600002));
#321871=CARTESIAN_POINT('Ctrl Pts',(-2.42404934000006,2.2,-3.67594303600002));
#321872=CARTESIAN_POINT('Ctrl Pts',(-2.42230931300006,12.2,-3.67486745700001));
#321873=CARTESIAN_POINT('Ctrl Pts',(-2.42230931300006,5.2,-3.67486745700001));
#321874=CARTESIAN_POINT('Ctrl Pts',(-2.42230931300006,2.2,-3.67486745700001));
#321875=CARTESIAN_POINT('Ctrl Pts',(-2.42057389400005,12.2,-3.67379207700001));
#321876=CARTESIAN_POINT('Ctrl Pts',(-2.42057389400005,5.2,-3.67379207700001));
#321877=CARTESIAN_POINT('Ctrl Pts',(-2.42057389400005,2.2,-3.67379207700001));
#321878=CARTESIAN_POINT('Ctrl Pts',(-2.41884308600006,12.2,-3.67271690500001));
#321879=CARTESIAN_POINT('Ctrl Pts',(-2.41884308600006,5.2,-3.67271690500001));
#321880=CARTESIAN_POINT('Ctrl Pts',(-2.41884308600006,2.2,-3.67271690500001));
#321881=CARTESIAN_POINT('Ctrl Pts',(-2.41711689000006,12.2,-3.67164195000001));
#321882=CARTESIAN_POINT('Ctrl Pts',(-2.41711689000006,5.2,-3.67164195000001));
#321883=CARTESIAN_POINT('Ctrl Pts',(-2.41711689000006,2.2,-3.67164195000001));
#321884=CARTESIAN_POINT('Ctrl Pts',(-2.41539530800006,12.2,-3.67056722400001));
#321885=CARTESIAN_POINT('Ctrl Pts',(-2.41539530800006,5.2,-3.67056722400001));
#321886=CARTESIAN_POINT('Ctrl Pts',(-2.41539530800006,2.2,-3.67056722400001));
#321887=CARTESIAN_POINT('Ctrl Pts',(-2.41367834100005,12.2,-3.66949273900001));
#321888=CARTESIAN_POINT('Ctrl Pts',(-2.41367834100005,5.2,-3.66949273900001));
#321889=CARTESIAN_POINT('Ctrl Pts',(-2.41367834100005,2.2,-3.66949273900001));
#321890=CARTESIAN_POINT('Ctrl Pts',(-2.41196599200005,12.2,-3.66841850200001));
#321891=CARTESIAN_POINT('Ctrl Pts',(-2.41196599200005,5.2,-3.66841850200001));
#321892=CARTESIAN_POINT('Ctrl Pts',(-2.41196599200005,2.2,-3.66841850200001));
#321893=CARTESIAN_POINT('Ctrl Pts',(-2.41025826200006,12.2,-3.66734452800001));
#321894=CARTESIAN_POINT('Ctrl Pts',(-2.41025826200006,5.2,-3.66734452800001));
#321895=CARTESIAN_POINT('Ctrl Pts',(-2.41025826200006,2.2,-3.66734452800001));
#321896=CARTESIAN_POINT('Ctrl Pts',(-2.40855515500006,12.2,-3.66627082400001));
#321897=CARTESIAN_POINT('Ctrl Pts',(-2.40855515500006,5.2,-3.66627082400001));
#321898=CARTESIAN_POINT('Ctrl Pts',(-2.40855515500006,2.2,-3.66627082400001));
#321899=CARTESIAN_POINT('Ctrl Pts',(-2.40685666900006,12.2,-3.66519740200001));
#321900=CARTESIAN_POINT('Ctrl Pts',(-2.40685666900006,5.2,-3.66519740200001));
#321901=CARTESIAN_POINT('Ctrl Pts',(-2.40685666900006,2.2,-3.66519740200001));
#321902=CARTESIAN_POINT('Ctrl Pts',(-2.40516281000006,12.2,-3.66412427300002));
#321903=CARTESIAN_POINT('Ctrl Pts',(-2.40516281000006,5.2,-3.66412427300002));
#321904=CARTESIAN_POINT('Ctrl Pts',(-2.40516281000006,2.2,-3.66412427300002));
#321905=CARTESIAN_POINT('Ctrl Pts',(-2.40347357600006,12.2,-3.66305144800001));
#321906=CARTESIAN_POINT('Ctrl Pts',(-2.40347357600006,5.2,-3.66305144800001));
#321907=CARTESIAN_POINT('Ctrl Pts',(-2.40347357600006,2.2,-3.66305144800001));
#321908=CARTESIAN_POINT('Ctrl Pts',(-2.40178897100006,12.2,-3.66197893700001));
#321909=CARTESIAN_POINT('Ctrl Pts',(-2.40178897100006,5.2,-3.66197893700001));
#321910=CARTESIAN_POINT('Ctrl Pts',(-2.40178897100006,2.2,-3.66197893700001));
#321911=CARTESIAN_POINT('Ctrl Pts',(-2.40010899700006,12.2,-3.66090675000001));
#321912=CARTESIAN_POINT('Ctrl Pts',(-2.40010899700006,5.2,-3.66090675000001));
#321913=CARTESIAN_POINT('Ctrl Pts',(-2.40010899700006,2.2,-3.66090675000001));
#321914=CARTESIAN_POINT('Ctrl Pts',(-2.39843365500006,12.2,-3.65983490000001));
#321915=CARTESIAN_POINT('Ctrl Pts',(-2.39843365500006,5.2,-3.65983490000001));
#321916=CARTESIAN_POINT('Ctrl Pts',(-2.39843365500006,2.2,-3.65983490000001));
#321917=CARTESIAN_POINT('Ctrl Pts',(-2.39676294700006,12.2,-3.65876339700002));
#321918=CARTESIAN_POINT('Ctrl Pts',(-2.39676294700006,5.2,-3.65876339700002));
#321919=CARTESIAN_POINT('Ctrl Pts',(-2.39676294700006,2.2,-3.65876339700002));
#321920=CARTESIAN_POINT('Ctrl Pts',(-2.39509687400006,12.2,-3.65769224900002));
#321921=CARTESIAN_POINT('Ctrl Pts',(-2.39509687400006,5.2,-3.65769224900002));
#321922=CARTESIAN_POINT('Ctrl Pts',(-2.39509687400006,2.2,-3.65769224900002));
#321923=CARTESIAN_POINT('Ctrl Pts',(-2.39343543800006,12.2,-3.65662147100001));
#321924=CARTESIAN_POINT('Ctrl Pts',(-2.39343543800006,5.2,-3.65662147100001));
#321925=CARTESIAN_POINT('Ctrl Pts',(-2.39343543800006,2.2,-3.65662147100001));
#321926=CARTESIAN_POINT('Ctrl Pts',(-2.39177864100005,12.2,-3.65555107100001));
#321927=CARTESIAN_POINT('Ctrl Pts',(-2.39177864100005,5.2,-3.65555107100001));
#321928=CARTESIAN_POINT('Ctrl Pts',(-2.39177864100005,2.2,-3.65555107100001));
#321929=CARTESIAN_POINT('Ctrl Pts',(-2.39012648600006,12.2,-3.65448106200001));
#321930=CARTESIAN_POINT('Ctrl Pts',(-2.39012648600006,5.2,-3.65448106200001));
#321931=CARTESIAN_POINT('Ctrl Pts',(-2.39012648600006,2.2,-3.65448106200001));
#321932=CARTESIAN_POINT('Ctrl Pts',(-2.38847897200006,12.2,-3.65341145300001));
#321933=CARTESIAN_POINT('Ctrl Pts',(-2.38847897200006,5.2,-3.65341145300001));
#321934=CARTESIAN_POINT('Ctrl Pts',(-2.38847897200006,2.2,-3.65341145300001));
#321935=CARTESIAN_POINT('Ctrl Pts',(-2.38683610300006,12.2,-3.65234225600001));
#321936=CARTESIAN_POINT('Ctrl Pts',(-2.38683610300006,5.2,-3.65234225600001));
#321937=CARTESIAN_POINT('Ctrl Pts',(-2.38683610300006,2.2,-3.65234225600001));
#321938=CARTESIAN_POINT('Ctrl Pts',(-2.38519788000006,12.2,-3.65127348100001));
#321939=CARTESIAN_POINT('Ctrl Pts',(-2.38519788000006,5.2,-3.65127348100001));
#321940=CARTESIAN_POINT('Ctrl Pts',(-2.38519788000006,2.2,-3.65127348100001));
#321941=CARTESIAN_POINT('Ctrl Pts',(-2.38356430300006,12.2,-3.65020514000001));
#321942=CARTESIAN_POINT('Ctrl Pts',(-2.38356430300006,5.2,-3.65020514000001));
#321943=CARTESIAN_POINT('Ctrl Pts',(-2.38356430300006,2.2,-3.65020514000001));
#321944=CARTESIAN_POINT('Ctrl Pts',(-2.38193537600006,12.2,-3.64913724300001));
#321945=CARTESIAN_POINT('Ctrl Pts',(-2.38193537600006,5.2,-3.64913724300001));
#321946=CARTESIAN_POINT('Ctrl Pts',(-2.38193537600006,2.2,-3.64913724300001));
#321947=CARTESIAN_POINT('Ctrl Pts',(-2.38031110000006,12.2,-3.64806980200001));
#321948=CARTESIAN_POINT('Ctrl Pts',(-2.38031110000006,5.2,-3.64806980200001));
#321949=CARTESIAN_POINT('Ctrl Pts',(-2.38031110000006,2.2,-3.64806980200001));
#321950=CARTESIAN_POINT('Ctrl Pts',(-2.37869147600006,12.2,-3.64700282800001));
#321951=CARTESIAN_POINT('Ctrl Pts',(-2.37869147600006,5.2,-3.64700282800001));
#321952=CARTESIAN_POINT('Ctrl Pts',(-2.37869147600006,2.2,-3.64700282800001));
#321953=CARTESIAN_POINT('Ctrl Pts',(-2.37707650600006,12.2,-3.64593633100001));
#321954=CARTESIAN_POINT('Ctrl Pts',(-2.37707650600006,5.2,-3.64593633100001));
#321955=CARTESIAN_POINT('Ctrl Pts',(-2.37707650600006,2.2,-3.64593633100001));
#321956=CARTESIAN_POINT('Ctrl Pts',(-2.37546619100006,12.2,-3.64487032100001));
#321957=CARTESIAN_POINT('Ctrl Pts',(-2.37546619100006,5.2,-3.64487032100001));
#321958=CARTESIAN_POINT('Ctrl Pts',(-2.37546619100006,2.2,-3.64487032100001));
#321959=CARTESIAN_POINT('Ctrl Pts',(-2.37386053300006,12.2,-3.64380481300001));
#321960=CARTESIAN_POINT('Ctrl Pts',(-2.37386053300006,5.2,-3.64380481300001));
#321961=CARTESIAN_POINT('Ctrl Pts',(-2.37386053300006,2.2,-3.64380481300001));
#321962=CARTESIAN_POINT('Ctrl Pts',(-2.37225953400006,12.2,-3.64273981500002));
#321963=CARTESIAN_POINT('Ctrl Pts',(-2.37225953400006,5.2,-3.64273981500002));
#321964=CARTESIAN_POINT('Ctrl Pts',(-2.37225953400006,2.2,-3.64273981500002));
#321965=CARTESIAN_POINT('Ctrl Pts',(-2.37066319500005,12.2,-3.64167533800002));
#321966=CARTESIAN_POINT('Ctrl Pts',(-2.37066319500005,5.2,-3.64167533800002));
#321967=CARTESIAN_POINT('Ctrl Pts',(-2.37066319500005,2.2,-3.64167533800002));
#321968=CARTESIAN_POINT('Ctrl Pts',(-2.36907151800006,12.2,-3.64061139500001));
#321969=CARTESIAN_POINT('Ctrl Pts',(-2.36907151800006,5.2,-3.64061139500001));
#321970=CARTESIAN_POINT('Ctrl Pts',(-2.36907151800006,2.2,-3.64061139500001));
#321971=CARTESIAN_POINT('Ctrl Pts',(-2.36748450500006,12.2,-3.63954799500001));
#321972=CARTESIAN_POINT('Ctrl Pts',(-2.36748450500006,5.2,-3.63954799500001));
#321973=CARTESIAN_POINT('Ctrl Pts',(-2.36748450500006,2.2,-3.63954799500001));
#321974=CARTESIAN_POINT('Ctrl Pts',(-2.36590215600006,12.2,-3.63848515200001));
#321975=CARTESIAN_POINT('Ctrl Pts',(-2.36590215600006,5.2,-3.63848515200001));
#321976=CARTESIAN_POINT('Ctrl Pts',(-2.36590215600006,2.2,-3.63848515200001));
#321977=CARTESIAN_POINT('Ctrl Pts',(-2.36432447400006,12.2,-3.63742287500001));
#321978=CARTESIAN_POINT('Ctrl Pts',(-2.36432447400006,5.2,-3.63742287500001));
#321979=CARTESIAN_POINT('Ctrl Pts',(-2.36432447400006,2.2,-3.63742287500001));
#321980=CARTESIAN_POINT('Ctrl Pts',(-2.36275145800006,12.2,-3.63636117400001));
#321981=CARTESIAN_POINT('Ctrl Pts',(-2.36275145800006,5.2,-3.63636117400001));
#321982=CARTESIAN_POINT('Ctrl Pts',(-2.36275145800006,2.2,-3.63636117400001));
#321983=CARTESIAN_POINT('Ctrl Pts',(-2.36118311300006,12.2,-3.63530006400001));
#321984=CARTESIAN_POINT('Ctrl Pts',(-2.36118311300006,5.2,-3.63530006400001));
#321985=CARTESIAN_POINT('Ctrl Pts',(-2.36118311300006,2.2,-3.63530006400001));
#321986=CARTESIAN_POINT('Ctrl Pts',(-2.35961943900006,12.2,-3.63423955300001));
#321987=CARTESIAN_POINT('Ctrl Pts',(-2.35961943900006,5.2,-3.63423955300001));
#321988=CARTESIAN_POINT('Ctrl Pts',(-2.35961943900006,2.2,-3.63423955300001));
#321989=CARTESIAN_POINT('Ctrl Pts',(-2.35806043600005,12.2,-3.63317965400002));
#321990=CARTESIAN_POINT('Ctrl Pts',(-2.35806043600005,5.2,-3.63317965400002));
#321991=CARTESIAN_POINT('Ctrl Pts',(-2.35806043600005,2.2,-3.63317965400002));
#321992=CARTESIAN_POINT('Ctrl Pts',(-2.35650610600006,12.2,-3.63212037800002));
#321993=CARTESIAN_POINT('Ctrl Pts',(-2.35650610600006,5.2,-3.63212037800002));
#321994=CARTESIAN_POINT('Ctrl Pts',(-2.35650610600006,2.2,-3.63212037800002));
#321995=CARTESIAN_POINT('Ctrl Pts',(-2.35495645300006,12.2,-3.63106173500002));
#321996=CARTESIAN_POINT('Ctrl Pts',(-2.35495645300006,5.2,-3.63106173500002));
#321997=CARTESIAN_POINT('Ctrl Pts',(-2.35495645300006,2.2,-3.63106173500002));
#321998=CARTESIAN_POINT('Ctrl Pts',(-2.35341147600006,12.2,-3.63000373800002));
#321999=CARTESIAN_POINT('Ctrl Pts',(-2.35341147600006,5.2,-3.63000373800002));
#322000=CARTESIAN_POINT('Ctrl Pts',(-2.35341147600006,2.2,-3.63000373800002));
#322001=CARTESIAN_POINT('Ctrl Pts',(-2.35187117600006,12.2,-3.62894639800002));
#322002=CARTESIAN_POINT('Ctrl Pts',(-2.35187117600006,5.2,-3.62894639800002));
#322003=CARTESIAN_POINT('Ctrl Pts',(-2.35187117600006,2.2,-3.62894639800002));
#322004=CARTESIAN_POINT('Ctrl Pts',(-2.35033555600006,12.2,-3.62788972600002));
#322005=CARTESIAN_POINT('Ctrl Pts',(-2.35033555600006,5.2,-3.62788972600002));
#322006=CARTESIAN_POINT('Ctrl Pts',(-2.35033555600006,2.2,-3.62788972600002));
#322007=CARTESIAN_POINT('Ctrl Pts',(-2.34880461600006,12.2,-3.62683373300001));
#322008=CARTESIAN_POINT('Ctrl Pts',(-2.34880461600006,5.2,-3.62683373300001));
#322009=CARTESIAN_POINT('Ctrl Pts',(-2.34880461600006,2.2,-3.62683373300001));
#322010=CARTESIAN_POINT('Ctrl Pts',(-2.34727835800005,12.2,-3.62577843200001));
#322011=CARTESIAN_POINT('Ctrl Pts',(-2.34727835800005,5.2,-3.62577843200001));
#322012=CARTESIAN_POINT('Ctrl Pts',(-2.34727835800005,2.2,-3.62577843200001));
#322013=CARTESIAN_POINT('Ctrl Pts',(-2.34575678400006,12.2,-3.62472383300001));
#322014=CARTESIAN_POINT('Ctrl Pts',(-2.34575678400006,5.2,-3.62472383300001));
#322015=CARTESIAN_POINT('Ctrl Pts',(-2.34575678400006,2.2,-3.62472383300001));
#322016=CARTESIAN_POINT('Ctrl Pts',(-2.34423989400006,12.2,-3.62366994800002));
#322017=CARTESIAN_POINT('Ctrl Pts',(-2.34423989400006,5.2,-3.62366994800002));
#322018=CARTESIAN_POINT('Ctrl Pts',(-2.34423989400006,2.2,-3.62366994800002));
#322019=CARTESIAN_POINT('Ctrl Pts',(-2.34272769000006,12.2,-3.62261678700001));
#322020=CARTESIAN_POINT('Ctrl Pts',(-2.34272769000006,5.2,-3.62261678700001));
#322021=CARTESIAN_POINT('Ctrl Pts',(-2.34272769000006,2.2,-3.62261678700001));
#322022=CARTESIAN_POINT('Ctrl Pts',(-2.34122017400006,12.2,-3.62156436400001));
#322023=CARTESIAN_POINT('Ctrl Pts',(-2.34122017400006,5.2,-3.62156436400001));
#322024=CARTESIAN_POINT('Ctrl Pts',(-2.34122017400006,2.2,-3.62156436400001));
#322025=CARTESIAN_POINT('Ctrl Pts',(-2.33971734600006,12.2,-3.62051269000002));
#322026=CARTESIAN_POINT('Ctrl Pts',(-2.33971734600006,5.2,-3.62051269000002));
#322027=CARTESIAN_POINT('Ctrl Pts',(-2.33971734600006,2.2,-3.62051269000002));
#322028=CARTESIAN_POINT('Ctrl Pts',(-2.33821920800006,12.2,-3.61946177600001));
#322029=CARTESIAN_POINT('Ctrl Pts',(-2.33821920800006,5.2,-3.61946177600001));
#322030=CARTESIAN_POINT('Ctrl Pts',(-2.33821920800006,2.2,-3.61946177600001));
#322031=CARTESIAN_POINT('Ctrl Pts',(-2.33672576200005,12.2,-3.61841163300001));
#322032=CARTESIAN_POINT('Ctrl Pts',(-2.33672576200005,5.2,-3.61841163300001));
#322033=CARTESIAN_POINT('Ctrl Pts',(-2.33672576200005,2.2,-3.61841163300001));
#322034=CARTESIAN_POINT('Ctrl Pts',(-2.33523700800006,12.2,-3.61736227300002));
#322035=CARTESIAN_POINT('Ctrl Pts',(-2.33523700800006,5.2,-3.61736227300002));
#322036=CARTESIAN_POINT('Ctrl Pts',(-2.33523700800006,2.2,-3.61736227300002));
#322037=CARTESIAN_POINT('Ctrl Pts',(-2.33375294700005,12.2,-3.61631370800001));
#322038=CARTESIAN_POINT('Ctrl Pts',(-2.33375294700005,5.2,-3.61631370800001));
#322039=CARTESIAN_POINT('Ctrl Pts',(-2.33375294700005,2.2,-3.61631370800001));
#322040=CARTESIAN_POINT('Ctrl Pts',(-2.33227358100006,12.2,-3.61526595000001));
#322041=CARTESIAN_POINT('Ctrl Pts',(-2.33227358100006,5.2,-3.61526595000001));
#322042=CARTESIAN_POINT('Ctrl Pts',(-2.33227358100006,2.2,-3.61526595000001));
#322043=CARTESIAN_POINT('Ctrl Pts',(-2.33079891200005,12.2,-3.61421900900002));
#322044=CARTESIAN_POINT('Ctrl Pts',(-2.33079891200005,5.2,-3.61421900900002));
#322045=CARTESIAN_POINT('Ctrl Pts',(-2.33079891200005,2.2,-3.61421900900002));
#322046=CARTESIAN_POINT('Ctrl Pts',(-2.32932893900006,12.2,-3.61317289800001));
#322047=CARTESIAN_POINT('Ctrl Pts',(-2.32932893900006,5.2,-3.61317289800001));
#322048=CARTESIAN_POINT('Ctrl Pts',(-2.32932893900006,2.2,-3.61317289800001));
#322049=CARTESIAN_POINT('Ctrl Pts',(-2.32786366600005,12.2,-3.61212762900001));
#322050=CARTESIAN_POINT('Ctrl Pts',(-2.32786366600005,5.2,-3.61212762900001));
#322051=CARTESIAN_POINT('Ctrl Pts',(-2.32786366600005,2.2,-3.61212762900001));
#322052=CARTESIAN_POINT('Ctrl Pts',(-2.32640309200006,12.2,-3.61108321200001));
#322053=CARTESIAN_POINT('Ctrl Pts',(-2.32640309200006,5.2,-3.61108321200001));
#322054=CARTESIAN_POINT('Ctrl Pts',(-2.32640309200006,2.2,-3.61108321200001));
#322055=CARTESIAN_POINT('Ctrl Pts',(-2.32494721700006,12.2,-3.61003966100002));
#322056=CARTESIAN_POINT('Ctrl Pts',(-2.32494721700006,5.2,-3.61003966100002));
#322057=CARTESIAN_POINT('Ctrl Pts',(-2.32494721700006,2.2,-3.61003966100002));
#322058=CARTESIAN_POINT('Ctrl Pts',(-2.32349604700006,12.2,-3.60899698600001));
#322059=CARTESIAN_POINT('Ctrl Pts',(-2.32349604700006,5.2,-3.60899698600001));
#322060=CARTESIAN_POINT('Ctrl Pts',(-2.32349604700006,2.2,-3.60899698600001));
#322061=CARTESIAN_POINT('Ctrl Pts',(-2.32204957800006,12.2,-3.60795520000002));
#322062=CARTESIAN_POINT('Ctrl Pts',(-2.32204957800006,5.2,-3.60795520000002));
#322063=CARTESIAN_POINT('Ctrl Pts',(-2.32204957800006,2.2,-3.60795520000002));
#322064=CARTESIAN_POINT('Ctrl Pts',(-2.32060781400006,12.2,-3.60691431500001));
#322065=CARTESIAN_POINT('Ctrl Pts',(-2.32060781400006,5.2,-3.60691431500001));
#322066=CARTESIAN_POINT('Ctrl Pts',(-2.32060781400006,2.2,-3.60691431500001));
#322067=CARTESIAN_POINT('Ctrl Pts',(-2.31917075400006,12.2,-3.60587434100001));
#322068=CARTESIAN_POINT('Ctrl Pts',(-2.31917075400006,5.2,-3.60587434100001));
#322069=CARTESIAN_POINT('Ctrl Pts',(-2.31917075400006,2.2,-3.60587434100001));
#322070=CARTESIAN_POINT('Ctrl Pts',(-2.31773840300006,12.2,-3.60483529100001));
#322071=CARTESIAN_POINT('Ctrl Pts',(-2.31773840300006,5.2,-3.60483529100001));
#322072=CARTESIAN_POINT('Ctrl Pts',(-2.31773840300006,2.2,-3.60483529100001));
#322073=CARTESIAN_POINT('Ctrl Pts',(-2.31631075700005,12.2,-3.60379717800001));
#322074=CARTESIAN_POINT('Ctrl Pts',(-2.31631075700005,5.2,-3.60379717800001));
#322075=CARTESIAN_POINT('Ctrl Pts',(-2.31631075700005,2.2,-3.60379717800001));
#322076=CARTESIAN_POINT('Ctrl Pts',(-2.31488782100006,12.2,-3.60276001200001));
#322077=CARTESIAN_POINT('Ctrl Pts',(-2.31488782100006,5.2,-3.60276001200001));
#322078=CARTESIAN_POINT('Ctrl Pts',(-2.31488782100006,2.2,-3.60276001200001));
#322079=CARTESIAN_POINT('Ctrl Pts',(-2.31346959400006,12.2,-3.60172380500002));
#322080=CARTESIAN_POINT('Ctrl Pts',(-2.31346959400006,5.2,-3.60172380500002));
#322081=CARTESIAN_POINT('Ctrl Pts',(-2.31346959400006,2.2,-3.60172380500002));
#322082=CARTESIAN_POINT('Ctrl Pts',(-2.31205607800006,12.2,-3.60068857100002));
#322083=CARTESIAN_POINT('Ctrl Pts',(-2.31205607800006,5.2,-3.60068857100002));
#322084=CARTESIAN_POINT('Ctrl Pts',(-2.31205607800006,2.2,-3.60068857100002));
#322085=CARTESIAN_POINT('Ctrl Pts',(-2.31064727300006,12.2,-3.59965432000001));
#322086=CARTESIAN_POINT('Ctrl Pts',(-2.31064727300006,5.2,-3.59965432000001));
#322087=CARTESIAN_POINT('Ctrl Pts',(-2.31064727300006,2.2,-3.59965432000001));
#322088=CARTESIAN_POINT('Ctrl Pts',(-2.30924318100006,12.2,-3.59862106400001));
#322089=CARTESIAN_POINT('Ctrl Pts',(-2.30924318100006,5.2,-3.59862106400001));
#322090=CARTESIAN_POINT('Ctrl Pts',(-2.30924318100006,2.2,-3.59862106400001));
#322091=CARTESIAN_POINT('Ctrl Pts',(-2.30784380200005,12.2,-3.59758881800001));
#322092=CARTESIAN_POINT('Ctrl Pts',(-2.30784380200005,5.2,-3.59758881800001));
#322093=CARTESIAN_POINT('Ctrl Pts',(-2.30784380200005,2.2,-3.59758881800001));
#322094=CARTESIAN_POINT('Ctrl Pts',(-2.30644913800006,12.2,-3.59655759000002));
#322095=CARTESIAN_POINT('Ctrl Pts',(-2.30644913800006,5.2,-3.59655759000002));
#322096=CARTESIAN_POINT('Ctrl Pts',(-2.30644913800006,2.2,-3.59655759000002));
#322097=CARTESIAN_POINT('Ctrl Pts',(-2.30505918900006,12.2,-3.59552739400002));
#322098=CARTESIAN_POINT('Ctrl Pts',(-2.30505918900006,5.2,-3.59552739400002));
#322099=CARTESIAN_POINT('Ctrl Pts',(-2.30505918900006,2.2,-3.59552739400002));
#322100=CARTESIAN_POINT('Ctrl Pts',(-2.30367395700006,12.2,-3.59449824100002));
#322101=CARTESIAN_POINT('Ctrl Pts',(-2.30367395700006,5.2,-3.59449824100002));
#322102=CARTESIAN_POINT('Ctrl Pts',(-2.30367395700006,2.2,-3.59449824100002));
#322103=CARTESIAN_POINT('Ctrl Pts',(-2.30229344300006,12.2,-3.59347014600001));
#322104=CARTESIAN_POINT('Ctrl Pts',(-2.30229344300006,5.2,-3.59347014600001));
#322105=CARTESIAN_POINT('Ctrl Pts',(-2.30229344300006,2.2,-3.59347014600001));
#322106=CARTESIAN_POINT('Ctrl Pts',(-2.30091764700005,12.2,-3.59244311700001));
#322107=CARTESIAN_POINT('Ctrl Pts',(-2.30091764700005,5.2,-3.59244311700001));
#322108=CARTESIAN_POINT('Ctrl Pts',(-2.30091764700005,2.2,-3.59244311700001));
#322109=CARTESIAN_POINT('Ctrl Pts',(-2.29954657000006,12.2,-3.59141717000002));
#322110=CARTESIAN_POINT('Ctrl Pts',(-2.29954657000006,5.2,-3.59141717000002));
#322111=CARTESIAN_POINT('Ctrl Pts',(-2.29954657000006,2.2,-3.59141717000002));
#322112=CARTESIAN_POINT('Ctrl Pts',(-2.29818021300006,12.2,-3.59039231400001));
#322113=CARTESIAN_POINT('Ctrl Pts',(-2.29818021300006,5.2,-3.59039231400001));
#322114=CARTESIAN_POINT('Ctrl Pts',(-2.29818021300006,2.2,-3.59039231400001));
#322115=CARTESIAN_POINT('Ctrl Pts',(-2.29681857700006,12.2,-3.58936856400002));
#322116=CARTESIAN_POINT('Ctrl Pts',(-2.29681857700006,5.2,-3.58936856400002));
#322117=CARTESIAN_POINT('Ctrl Pts',(-2.29681857700006,2.2,-3.58936856400002));
#322118=CARTESIAN_POINT('Ctrl Pts',(-2.29546166300006,12.2,-3.58834593000001));
#322119=CARTESIAN_POINT('Ctrl Pts',(-2.29546166300006,5.2,-3.58834593000001));
#322120=CARTESIAN_POINT('Ctrl Pts',(-2.29546166300006,2.2,-3.58834593000001));
#322121=CARTESIAN_POINT('Ctrl Pts',(-2.29410947100006,12.2,-3.58732442600001));
#322122=CARTESIAN_POINT('Ctrl Pts',(-2.29410947100006,5.2,-3.58732442600001));
#322123=CARTESIAN_POINT('Ctrl Pts',(-2.29410947100006,2.2,-3.58732442600001));
#322124=CARTESIAN_POINT('Ctrl Pts',(-2.29276200300006,12.2,-3.58630406300001));
#322125=CARTESIAN_POINT('Ctrl Pts',(-2.29276200300006,5.2,-3.58630406300001));
#322126=CARTESIAN_POINT('Ctrl Pts',(-2.29276200300006,2.2,-3.58630406300001));
#322127=CARTESIAN_POINT('Ctrl Pts',(-2.29141926000006,12.2,-3.58528485300001));
#322128=CARTESIAN_POINT('Ctrl Pts',(-2.29141926000006,5.2,-3.58528485300001));
#322129=CARTESIAN_POINT('Ctrl Pts',(-2.29141926000006,2.2,-3.58528485300001));
#322130=CARTESIAN_POINT('Ctrl Pts',(-2.29008124100006,12.2,-3.58426681000001));
#322131=CARTESIAN_POINT('Ctrl Pts',(-2.29008124100006,5.2,-3.58426681000001));
#322132=CARTESIAN_POINT('Ctrl Pts',(-2.29008124100006,2.2,-3.58426681000001));
#322133=CARTESIAN_POINT('Ctrl Pts',(-2.28874794800006,12.2,-3.58324994600002));
#322134=CARTESIAN_POINT('Ctrl Pts',(-2.28874794800006,5.2,-3.58324994600002));
#322135=CARTESIAN_POINT('Ctrl Pts',(-2.28874794800006,2.2,-3.58324994600002));
#322136=CARTESIAN_POINT('Ctrl Pts',(-2.28741938200006,12.2,-3.58223427200001));
#322137=CARTESIAN_POINT('Ctrl Pts',(-2.28741938200006,5.2,-3.58223427200001));
#322138=CARTESIAN_POINT('Ctrl Pts',(-2.28741938200006,2.2,-3.58223427200001));
#322139=CARTESIAN_POINT('Ctrl Pts',(-2.28609554300006,12.2,-3.58121980100002));
#322140=CARTESIAN_POINT('Ctrl Pts',(-2.28609554300006,5.2,-3.58121980100002));
#322141=CARTESIAN_POINT('Ctrl Pts',(-2.28609554300006,2.2,-3.58121980100002));
#322142=CARTESIAN_POINT('Ctrl Pts',(-2.28477643300006,12.2,-3.58020654600002));
#322143=CARTESIAN_POINT('Ctrl Pts',(-2.28477643300006,5.2,-3.58020654600002));
#322144=CARTESIAN_POINT('Ctrl Pts',(-2.28477643300006,2.2,-3.58020654600002));
#322145=CARTESIAN_POINT('Ctrl Pts',(-2.28346205200006,12.2,-3.57919451900001));
#322146=CARTESIAN_POINT('Ctrl Pts',(-2.28346205200006,5.2,-3.57919451900001));
#322147=CARTESIAN_POINT('Ctrl Pts',(-2.28346205200006,2.2,-3.57919451900001));
#322148=CARTESIAN_POINT('Ctrl Pts',(-2.28215239900006,12.2,-3.57818373200002));
#322149=CARTESIAN_POINT('Ctrl Pts',(-2.28215239900006,5.2,-3.57818373200002));
#322150=CARTESIAN_POINT('Ctrl Pts',(-2.28215239900006,2.2,-3.57818373200002));
#322151=CARTESIAN_POINT('Ctrl Pts',(-2.28084747800006,12.2,-3.57717419900001));
#322152=CARTESIAN_POINT('Ctrl Pts',(-2.28084747800006,5.2,-3.57717419900001));
#322153=CARTESIAN_POINT('Ctrl Pts',(-2.28084747800006,2.2,-3.57717419900001));
#322154=CARTESIAN_POINT('Ctrl Pts',(-2.27954728600006,12.2,-3.57616593100001));
#322155=CARTESIAN_POINT('Ctrl Pts',(-2.27954728600006,5.2,-3.57616593100001));
#322156=CARTESIAN_POINT('Ctrl Pts',(-2.27954728600006,2.2,-3.57616593100001));
#322157=CARTESIAN_POINT('Ctrl Pts',(-2.27825182700006,12.2,-3.57515894100001));
#322158=CARTESIAN_POINT('Ctrl Pts',(-2.27825182700006,5.2,-3.57515894100001));
#322159=CARTESIAN_POINT('Ctrl Pts',(-2.27825182700006,2.2,-3.57515894100001));
#322160=CARTESIAN_POINT('Ctrl Pts',(-2.27696109900006,12.2,-3.57415324200002));
#322161=CARTESIAN_POINT('Ctrl Pts',(-2.27696109900006,5.2,-3.57415324200002));
#322162=CARTESIAN_POINT('Ctrl Pts',(-2.27696109900006,2.2,-3.57415324200002));
#322163=CARTESIAN_POINT('Ctrl Pts',(-2.27567510500006,12.2,-3.57314884700001));
#322164=CARTESIAN_POINT('Ctrl Pts',(-2.27567510500006,5.2,-3.57314884700001));
#322165=CARTESIAN_POINT('Ctrl Pts',(-2.27567510500006,2.2,-3.57314884700001));
#322166=CARTESIAN_POINT('Ctrl Pts',(-2.27439384400005,12.2,-3.57214576600001));
#322167=CARTESIAN_POINT('Ctrl Pts',(-2.27439384400005,5.2,-3.57214576600001));
#322168=CARTESIAN_POINT('Ctrl Pts',(-2.27439384400005,2.2,-3.57214576600001));
#322169=CARTESIAN_POINT('Ctrl Pts',(-2.27311731600006,12.2,-3.57114401400001));
#322170=CARTESIAN_POINT('Ctrl Pts',(-2.27311731600006,5.2,-3.57114401400001));
#322171=CARTESIAN_POINT('Ctrl Pts',(-2.27311731600006,2.2,-3.57114401400001));
#322172=CARTESIAN_POINT('Ctrl Pts',(-2.27184552400006,12.2,-3.57014360500001));
#322173=CARTESIAN_POINT('Ctrl Pts',(-2.27184552400006,5.2,-3.57014360500001));
#322174=CARTESIAN_POINT('Ctrl Pts',(-2.27184552400006,2.2,-3.57014360500001));
#322175=CARTESIAN_POINT('Ctrl Pts',(-2.27057846700006,12.2,-3.56914454800001));
#322176=CARTESIAN_POINT('Ctrl Pts',(-2.27057846700006,5.2,-3.56914454800001));
#322177=CARTESIAN_POINT('Ctrl Pts',(-2.27057846700006,2.2,-3.56914454800001));
#322178=CARTESIAN_POINT('Ctrl Pts',(-2.26931614600006,12.2,-3.56814685800002));
#322179=CARTESIAN_POINT('Ctrl Pts',(-2.26931614600006,5.2,-3.56814685800002));
#322180=CARTESIAN_POINT('Ctrl Pts',(-2.26931614600006,2.2,-3.56814685800002));
#322181=CARTESIAN_POINT('Ctrl Pts',(-2.26805856000006,12.2,-3.56715054700001));
#322182=CARTESIAN_POINT('Ctrl Pts',(-2.26805856000006,5.2,-3.56715054700001));
#322183=CARTESIAN_POINT('Ctrl Pts',(-2.26805856000006,2.2,-3.56715054700001));
#322184=CARTESIAN_POINT('Ctrl Pts',(-2.26680571100006,12.2,-3.56615562900001));
#322185=CARTESIAN_POINT('Ctrl Pts',(-2.26680571100006,5.2,-3.56615562900001));
#322186=CARTESIAN_POINT('Ctrl Pts',(-2.26680571100006,2.2,-3.56615562900001));
#322187=CARTESIAN_POINT('Ctrl Pts',(-2.26555760000006,12.2,-3.56516211500002));
#322188=CARTESIAN_POINT('Ctrl Pts',(-2.26555760000006,5.2,-3.56516211500002));
#322189=CARTESIAN_POINT('Ctrl Pts',(-2.26555760000006,2.2,-3.56516211500002));
#322190=CARTESIAN_POINT('Ctrl Pts',(-2.26431422600006,12.2,-3.56417002000001));
#322191=CARTESIAN_POINT('Ctrl Pts',(-2.26431422600006,5.2,-3.56417002000001));
#322192=CARTESIAN_POINT('Ctrl Pts',(-2.26431422600006,2.2,-3.56417002000001));
#322193=CARTESIAN_POINT('Ctrl Pts',(-2.26307559100006,12.2,-3.56317935400002));
#322194=CARTESIAN_POINT('Ctrl Pts',(-2.26307559100006,5.2,-3.56317935400002));
#322195=CARTESIAN_POINT('Ctrl Pts',(-2.26307559100006,2.2,-3.56317935400002));
#322196=CARTESIAN_POINT('Ctrl Pts',(-2.26184169300006,12.2,-3.56219013200001));
#322197=CARTESIAN_POINT('Ctrl Pts',(-2.26184169300006,5.2,-3.56219013200001));
#322198=CARTESIAN_POINT('Ctrl Pts',(-2.26184169300006,2.2,-3.56219013200001));
#322199=CARTESIAN_POINT('Ctrl Pts',(-2.26061253600006,12.2,-3.56120236700002));
#322200=CARTESIAN_POINT('Ctrl Pts',(-2.26061253600006,5.2,-3.56120236700002));
#322201=CARTESIAN_POINT('Ctrl Pts',(-2.26061253600006,2.2,-3.56120236700002));
#322202=CARTESIAN_POINT('Ctrl Pts',(-2.25938811800006,12.2,-3.56021607000002));
#322203=CARTESIAN_POINT('Ctrl Pts',(-2.25938811800006,5.2,-3.56021607000002));
#322204=CARTESIAN_POINT('Ctrl Pts',(-2.25938811800006,2.2,-3.56021607000002));
#322205=CARTESIAN_POINT('Ctrl Pts',(-2.25816843900006,12.2,-3.55923125600001));
#322206=CARTESIAN_POINT('Ctrl Pts',(-2.25816843900006,5.2,-3.55923125600001));
#322207=CARTESIAN_POINT('Ctrl Pts',(-2.25816843900006,2.2,-3.55923125600001));
#322208=CARTESIAN_POINT('Ctrl Pts',(-2.25695350000006,12.2,-3.55824793700001));
#322209=CARTESIAN_POINT('Ctrl Pts',(-2.25695350000006,5.2,-3.55824793700001));
#322210=CARTESIAN_POINT('Ctrl Pts',(-2.25695350000006,2.2,-3.55824793700001));
#322211=CARTESIAN_POINT('Ctrl Pts',(-2.25574330200006,12.2,-3.55726612600002));
#322212=CARTESIAN_POINT('Ctrl Pts',(-2.25574330200006,5.2,-3.55726612600002));
#322213=CARTESIAN_POINT('Ctrl Pts',(-2.25574330200006,2.2,-3.55726612600002));
#322214=CARTESIAN_POINT('Ctrl Pts',(-2.25453784600006,12.2,-3.55628583600001));
#322215=CARTESIAN_POINT('Ctrl Pts',(-2.25453784600006,5.2,-3.55628583600001));
#322216=CARTESIAN_POINT('Ctrl Pts',(-2.25453784600006,2.2,-3.55628583600001));
#322217=CARTESIAN_POINT('Ctrl Pts',(-2.25333713000006,12.2,-3.55530708100002));
#322218=CARTESIAN_POINT('Ctrl Pts',(-2.25333713000006,5.2,-3.55530708100002));
#322219=CARTESIAN_POINT('Ctrl Pts',(-2.25333713000006,2.2,-3.55530708100002));
#322220=CARTESIAN_POINT('Ctrl Pts',(-2.25214115600005,12.2,-3.55432987300001));
#322221=CARTESIAN_POINT('Ctrl Pts',(-2.25214115600005,5.2,-3.55432987300001));
#322222=CARTESIAN_POINT('Ctrl Pts',(-2.25214115600005,2.2,-3.55432987300001));
#322223=CARTESIAN_POINT('Ctrl Pts',(-2.25094992400006,12.2,-3.55335422500001));
#322224=CARTESIAN_POINT('Ctrl Pts',(-2.25094992400006,5.2,-3.55335422500001));
#322225=CARTESIAN_POINT('Ctrl Pts',(-2.25094992400006,2.2,-3.55335422500001));
#322226=CARTESIAN_POINT('Ctrl Pts',(-2.24976343500006,12.2,-3.55238015100001));
#322227=CARTESIAN_POINT('Ctrl Pts',(-2.24976343500006,5.2,-3.55238015100001));
#322228=CARTESIAN_POINT('Ctrl Pts',(-2.24976343500006,2.2,-3.55238015100001));
#322229=CARTESIAN_POINT('Ctrl Pts',(-2.24858168800006,12.2,-3.55140766300002));
#322230=CARTESIAN_POINT('Ctrl Pts',(-2.24858168800006,5.2,-3.55140766300002));
#322231=CARTESIAN_POINT('Ctrl Pts',(-2.24858168800006,2.2,-3.55140766300002));
#322232=CARTESIAN_POINT('Ctrl Pts',(-2.24740468200006,12.2,-3.55043677600001));
#322233=CARTESIAN_POINT('Ctrl Pts',(-2.24740468200006,5.2,-3.55043677600001));
#322234=CARTESIAN_POINT('Ctrl Pts',(-2.24740468200006,2.2,-3.55043677600001));
#322235=CARTESIAN_POINT('Ctrl Pts',(-2.24623242100006,12.2,-3.54946750100002));
#322236=CARTESIAN_POINT('Ctrl Pts',(-2.24623242100006,5.2,-3.54946750100002));
#322237=CARTESIAN_POINT('Ctrl Pts',(-2.24623242100006,2.2,-3.54946750100002));
#322238=CARTESIAN_POINT('Ctrl Pts',(-2.24506490200006,12.2,-3.54849985200001));
#322239=CARTESIAN_POINT('Ctrl Pts',(-2.24506490200006,5.2,-3.54849985200001));
#322240=CARTESIAN_POINT('Ctrl Pts',(-2.24506490200006,2.2,-3.54849985200001));
#322241=CARTESIAN_POINT('Ctrl Pts',(-2.24390212800006,12.2,-3.54753384500002));
#322242=CARTESIAN_POINT('Ctrl Pts',(-2.24390212800006,5.2,-3.54753384500002));
#322243=CARTESIAN_POINT('Ctrl Pts',(-2.24390212800006,2.2,-3.54753384500002));
#322244=CARTESIAN_POINT('Ctrl Pts',(-2.24274409600006,12.2,-3.54656948900002));
#322245=CARTESIAN_POINT('Ctrl Pts',(-2.24274409600006,5.2,-3.54656948900002));
#322246=CARTESIAN_POINT('Ctrl Pts',(-2.24274409600006,2.2,-3.54656948900002));
#322247=CARTESIAN_POINT('Ctrl Pts',(-2.24159080800006,12.2,-3.54560679900001));
#322248=CARTESIAN_POINT('Ctrl Pts',(-2.24159080800006,5.2,-3.54560679900001));
#322249=CARTESIAN_POINT('Ctrl Pts',(-2.24159080800006,2.2,-3.54560679900001));
#322250=CARTESIAN_POINT('Ctrl Pts',(-2.24044226300005,12.2,-3.54464578800001));
#322251=CARTESIAN_POINT('Ctrl Pts',(-2.24044226300005,5.2,-3.54464578800001));
#322252=CARTESIAN_POINT('Ctrl Pts',(-2.24044226300005,2.2,-3.54464578800001));
#322253=CARTESIAN_POINT('Ctrl Pts',(-2.23929846300006,12.2,-3.54368647200001));
#322254=CARTESIAN_POINT('Ctrl Pts',(-2.23929846300006,5.2,-3.54368647200001));
#322255=CARTESIAN_POINT('Ctrl Pts',(-2.23929846300006,2.2,-3.54368647200001));
#322256=CARTESIAN_POINT('Ctrl Pts',(-2.23815940700006,12.2,-3.54272886000001));
#322257=CARTESIAN_POINT('Ctrl Pts',(-2.23815940700006,5.2,-3.54272886000001));
#322258=CARTESIAN_POINT('Ctrl Pts',(-2.23815940700006,2.2,-3.54272886000001));
#322259=CARTESIAN_POINT('Ctrl Pts',(-2.23702509400006,12.2,-3.54177296900001));
#322260=CARTESIAN_POINT('Ctrl Pts',(-2.23702509400006,5.2,-3.54177296900001));
#322261=CARTESIAN_POINT('Ctrl Pts',(-2.23702509400006,2.2,-3.54177296900001));
#322262=CARTESIAN_POINT('Ctrl Pts',(-2.23589552500005,12.2,-3.54081881000001));
#322263=CARTESIAN_POINT('Ctrl Pts',(-2.23589552500005,5.2,-3.54081881000001));
#322264=CARTESIAN_POINT('Ctrl Pts',(-2.23589552500005,2.2,-3.54081881000001));
#322265=CARTESIAN_POINT('Ctrl Pts',(-2.23477070200006,12.2,-3.53986640000001));
#322266=CARTESIAN_POINT('Ctrl Pts',(-2.23477070200006,5.2,-3.53986640000001));
#322267=CARTESIAN_POINT('Ctrl Pts',(-2.23477070200006,2.2,-3.53986640000001));
#322268=CARTESIAN_POINT('Ctrl Pts',(-2.23365062200005,12.2,-3.53891574700001));
#322269=CARTESIAN_POINT('Ctrl Pts',(-2.23365062200005,5.2,-3.53891574700001));
#322270=CARTESIAN_POINT('Ctrl Pts',(-2.23365062200005,2.2,-3.53891574700001));
#322271=CARTESIAN_POINT('Ctrl Pts',(-2.23253528700006,12.2,-3.53796687000001));
#322272=CARTESIAN_POINT('Ctrl Pts',(-2.23253528700006,5.2,-3.53796687000001));
#322273=CARTESIAN_POINT('Ctrl Pts',(-2.23253528700006,2.2,-3.53796687000001));
#322274=CARTESIAN_POINT('Ctrl Pts',(-2.23142469500006,12.2,-3.53701978000001));
#322275=CARTESIAN_POINT('Ctrl Pts',(-2.23142469500006,5.2,-3.53701978000001));
#322276=CARTESIAN_POINT('Ctrl Pts',(-2.23142469500006,2.2,-3.53701978000001));
#322277=CARTESIAN_POINT('Ctrl Pts',(-2.23031884900006,12.2,-3.53607449000001));
#322278=CARTESIAN_POINT('Ctrl Pts',(-2.23031884900006,5.2,-3.53607449000001));
#322279=CARTESIAN_POINT('Ctrl Pts',(-2.23031884900006,2.2,-3.53607449000001));
#322280=CARTESIAN_POINT('Ctrl Pts',(-2.22921774700006,12.2,-3.53513101400001));
#322281=CARTESIAN_POINT('Ctrl Pts',(-2.22921774700006,5.2,-3.53513101400001));
#322282=CARTESIAN_POINT('Ctrl Pts',(-2.22921774700006,2.2,-3.53513101400001));
#322283=CARTESIAN_POINT('Ctrl Pts',(-2.22812138900006,12.2,-3.53418936800002));
#322284=CARTESIAN_POINT('Ctrl Pts',(-2.22812138900006,5.2,-3.53418936800002));
#322285=CARTESIAN_POINT('Ctrl Pts',(-2.22812138900006,2.2,-3.53418936800002));
#322286=CARTESIAN_POINT('Ctrl Pts',(-2.22702977400006,12.2,-3.53324956200002));
#322287=CARTESIAN_POINT('Ctrl Pts',(-2.22702977400006,5.2,-3.53324956200002));
#322288=CARTESIAN_POINT('Ctrl Pts',(-2.22702977400006,2.2,-3.53324956200002));
#322289=CARTESIAN_POINT('Ctrl Pts',(-2.22594290400006,12.2,-3.53231161200001));
#322290=CARTESIAN_POINT('Ctrl Pts',(-2.22594290400006,5.2,-3.53231161200001));
#322291=CARTESIAN_POINT('Ctrl Pts',(-2.22594290400006,2.2,-3.53231161200001));
#322292=CARTESIAN_POINT('Ctrl Pts',(-2.22486077700006,12.2,-3.53137553200002));
#322293=CARTESIAN_POINT('Ctrl Pts',(-2.22486077700006,5.2,-3.53137553200002));
#322294=CARTESIAN_POINT('Ctrl Pts',(-2.22486077700006,2.2,-3.53137553200002));
#322295=CARTESIAN_POINT('Ctrl Pts',(-2.22378339500006,12.2,-3.53044133300001));
#322296=CARTESIAN_POINT('Ctrl Pts',(-2.22378339500006,5.2,-3.53044133300001));
#322297=CARTESIAN_POINT('Ctrl Pts',(-2.22378339500006,2.2,-3.53044133300001));
#322298=CARTESIAN_POINT('Ctrl Pts',(-2.22271075500006,12.2,-3.52950903200002));
#322299=CARTESIAN_POINT('Ctrl Pts',(-2.22271075500006,5.2,-3.52950903200002));
#322300=CARTESIAN_POINT('Ctrl Pts',(-2.22271075500006,2.2,-3.52950903200002));
#322301=CARTESIAN_POINT('Ctrl Pts',(-2.22164286100006,12.2,-3.52857864200002));
#322302=CARTESIAN_POINT('Ctrl Pts',(-2.22164286100006,5.2,-3.52857864200002));
#322303=CARTESIAN_POINT('Ctrl Pts',(-2.22164286100006,2.2,-3.52857864200002));
#322304=CARTESIAN_POINT('Ctrl Pts',(-2.22057970800006,12.2,-3.52765017500001));
#322305=CARTESIAN_POINT('Ctrl Pts',(-2.22057970800006,5.2,-3.52765017500001));
#322306=CARTESIAN_POINT('Ctrl Pts',(-2.22057970800006,2.2,-3.52765017500001));
#322307=CARTESIAN_POINT('Ctrl Pts',(-2.21952129900005,12.2,-3.52672364800001));
#322308=CARTESIAN_POINT('Ctrl Pts',(-2.21952129900005,5.2,-3.52672364800001));
#322309=CARTESIAN_POINT('Ctrl Pts',(-2.21952129900005,2.2,-3.52672364800001));
#322310=CARTESIAN_POINT('Ctrl Pts',(-2.21846763300006,12.2,-3.52579907200001));
#322311=CARTESIAN_POINT('Ctrl Pts',(-2.21846763300006,5.2,-3.52579907200001));
#322312=CARTESIAN_POINT('Ctrl Pts',(-2.21846763300006,2.2,-3.52579907200001));
#322313=CARTESIAN_POINT('Ctrl Pts',(-2.21741870900006,12.2,-3.52487646300002));
#322314=CARTESIAN_POINT('Ctrl Pts',(-2.21741870900006,5.2,-3.52487646300002));
#322315=CARTESIAN_POINT('Ctrl Pts',(-2.21741870900006,2.2,-3.52487646300002));
#322316=CARTESIAN_POINT('Ctrl Pts',(-2.21637452700006,12.2,-3.52395583300002));
#322317=CARTESIAN_POINT('Ctrl Pts',(-2.21637452700006,5.2,-3.52395583300002));
#322318=CARTESIAN_POINT('Ctrl Pts',(-2.21637452700006,2.2,-3.52395583300002));
#322319=CARTESIAN_POINT('Ctrl Pts',(-2.21533508800006,12.2,-3.52303719700001));
#322320=CARTESIAN_POINT('Ctrl Pts',(-2.21533508800006,5.2,-3.52303719700001));
#322321=CARTESIAN_POINT('Ctrl Pts',(-2.21533508800006,2.2,-3.52303719700001));
#322322=CARTESIAN_POINT('Ctrl Pts',(-2.21430039000006,12.2,-3.52212056900001));
#322323=CARTESIAN_POINT('Ctrl Pts',(-2.21430039000006,5.2,-3.52212056900001));
#322324=CARTESIAN_POINT('Ctrl Pts',(-2.21430039000006,2.2,-3.52212056900001));
#322325=CARTESIAN_POINT('Ctrl Pts',(-2.21327043400006,12.2,-3.52120596400002));
#322326=CARTESIAN_POINT('Ctrl Pts',(-2.21327043400006,5.2,-3.52120596400002));
#322327=CARTESIAN_POINT('Ctrl Pts',(-2.21327043400006,2.2,-3.52120596400002));
#322328=CARTESIAN_POINT('Ctrl Pts',(-2.21224521900006,12.2,-3.52029339500001));
#322329=CARTESIAN_POINT('Ctrl Pts',(-2.21224521900006,5.2,-3.52029339500001));
#322330=CARTESIAN_POINT('Ctrl Pts',(-2.21224521900006,2.2,-3.52029339500001));
#322331=CARTESIAN_POINT('Ctrl Pts',(-2.21122474400006,12.2,-3.51938287600001));
#322332=CARTESIAN_POINT('Ctrl Pts',(-2.21122474400006,5.2,-3.51938287600001));
#322333=CARTESIAN_POINT('Ctrl Pts',(-2.21122474400006,2.2,-3.51938287600001));
#322334=CARTESIAN_POINT('Ctrl Pts',(-2.21020901100006,12.2,-3.51847442100001));
#322335=CARTESIAN_POINT('Ctrl Pts',(-2.21020901100006,5.2,-3.51847442100001));
#322336=CARTESIAN_POINT('Ctrl Pts',(-2.21020901100006,2.2,-3.51847442100001));
#322337=CARTESIAN_POINT('Ctrl Pts',(-2.20919801800005,12.2,-3.51756804500001));
#322338=CARTESIAN_POINT('Ctrl Pts',(-2.20919801800005,5.2,-3.51756804500001));
#322339=CARTESIAN_POINT('Ctrl Pts',(-2.20919801800005,2.2,-3.51756804500001));
#322340=CARTESIAN_POINT('Ctrl Pts',(-2.20819176300005,12.2,-3.51666376200002));
#322341=CARTESIAN_POINT('Ctrl Pts',(-2.20819176300005,5.2,-3.51666376200002));
#322342=CARTESIAN_POINT('Ctrl Pts',(-2.20819176300005,2.2,-3.51666376200002));
#322343=CARTESIAN_POINT('Ctrl Pts',(-2.20719024800006,12.2,-3.51576158700002));
#322344=CARTESIAN_POINT('Ctrl Pts',(-2.20719024800006,5.2,-3.51576158700002));
#322345=CARTESIAN_POINT('Ctrl Pts',(-2.20719024800006,2.2,-3.51576158700002));
#322346=CARTESIAN_POINT('Ctrl Pts',(-2.20619347100006,12.2,-3.51486153100002));
#322347=CARTESIAN_POINT('Ctrl Pts',(-2.20619347100006,5.2,-3.51486153100002));
#322348=CARTESIAN_POINT('Ctrl Pts',(-2.20619347100006,2.2,-3.51486153100002));
#322349=CARTESIAN_POINT('Ctrl Pts',(-2.20520143300006,12.2,-3.51396361200001));
#322350=CARTESIAN_POINT('Ctrl Pts',(-2.20520143300006,5.2,-3.51396361200001));
#322351=CARTESIAN_POINT('Ctrl Pts',(-2.20520143300006,2.2,-3.51396361200001));
#322352=CARTESIAN_POINT('Ctrl Pts',(-2.20421413200006,12.2,-3.51306784200001));
#322353=CARTESIAN_POINT('Ctrl Pts',(-2.20421413200006,5.2,-3.51306784200001));
#322354=CARTESIAN_POINT('Ctrl Pts',(-2.20421413200006,2.2,-3.51306784200001));
#322355=CARTESIAN_POINT('Ctrl Pts',(-2.20323156900006,12.2,-3.51217423700001));
#322356=CARTESIAN_POINT('Ctrl Pts',(-2.20323156900006,5.2,-3.51217423700001));
#322357=CARTESIAN_POINT('Ctrl Pts',(-2.20323156900006,2.2,-3.51217423700001));
#322358=CARTESIAN_POINT('Ctrl Pts',(-2.20225374200006,12.2,-3.51128281000001));
#322359=CARTESIAN_POINT('Ctrl Pts',(-2.20225374200006,5.2,-3.51128281000001));
#322360=CARTESIAN_POINT('Ctrl Pts',(-2.20225374200006,2.2,-3.51128281000001));
#322361=CARTESIAN_POINT('Ctrl Pts',(-2.20128065100006,12.2,-3.51039357700001));
#322362=CARTESIAN_POINT('Ctrl Pts',(-2.20128065100006,5.2,-3.51039357700001));
#322363=CARTESIAN_POINT('Ctrl Pts',(-2.20128065100006,2.2,-3.51039357700001));
#322364=CARTESIAN_POINT('Ctrl Pts',(-2.20031229600006,12.2,-3.50950655100001));
#322365=CARTESIAN_POINT('Ctrl Pts',(-2.20031229600006,5.2,-3.50950655100001));
#322366=CARTESIAN_POINT('Ctrl Pts',(-2.20031229600006,2.2,-3.50950655100001));
#322367=CARTESIAN_POINT('Ctrl Pts',(-2.19934867500006,12.2,-3.50862174600001));
#322368=CARTESIAN_POINT('Ctrl Pts',(-2.19934867500006,5.2,-3.50862174600001));
#322369=CARTESIAN_POINT('Ctrl Pts',(-2.19934867500006,2.2,-3.50862174600001));
#322370=CARTESIAN_POINT('Ctrl Pts',(-2.19838978900006,12.2,-3.50773917800002));
#322371=CARTESIAN_POINT('Ctrl Pts',(-2.19838978900006,5.2,-3.50773917800002));
#322372=CARTESIAN_POINT('Ctrl Pts',(-2.19838978900006,2.2,-3.50773917800002));
#322373=CARTESIAN_POINT('Ctrl Pts',(-2.19743563700006,12.2,-3.50685886100001));
#322374=CARTESIAN_POINT('Ctrl Pts',(-2.19743563700006,5.2,-3.50685886100001));
#322375=CARTESIAN_POINT('Ctrl Pts',(-2.19743563700006,2.2,-3.50685886100001));
#322376=CARTESIAN_POINT('Ctrl Pts',(-2.19648621700005,12.2,-3.50598081000001));
#322377=CARTESIAN_POINT('Ctrl Pts',(-2.19648621700005,5.2,-3.50598081000001));
#322378=CARTESIAN_POINT('Ctrl Pts',(-2.19648621700005,2.2,-3.50598081000001));
#322379=CARTESIAN_POINT('Ctrl Pts',(-2.19554153100006,12.2,-3.50510503800002));
#322380=CARTESIAN_POINT('Ctrl Pts',(-2.19554153100006,5.2,-3.50510503800002));
#322381=CARTESIAN_POINT('Ctrl Pts',(-2.19554153100006,2.2,-3.50510503800002));
#322382=CARTESIAN_POINT('Ctrl Pts',(-2.19460157600006,12.2,-3.50423156200002));
#322383=CARTESIAN_POINT('Ctrl Pts',(-2.19460157600006,5.2,-3.50423156200002));
#322384=CARTESIAN_POINT('Ctrl Pts',(-2.19460157600006,2.2,-3.50423156200002));
#322385=CARTESIAN_POINT('Ctrl Pts',(-2.19366635100006,12.2,-3.50336039400001));
#322386=CARTESIAN_POINT('Ctrl Pts',(-2.19366635100006,5.2,-3.50336039400001));
#322387=CARTESIAN_POINT('Ctrl Pts',(-2.19366635100006,2.2,-3.50336039400001));
#322388=CARTESIAN_POINT('Ctrl Pts',(-2.19273585700006,12.2,-3.50249155100002));
#322389=CARTESIAN_POINT('Ctrl Pts',(-2.19273585700006,5.2,-3.50249155100002));
#322390=CARTESIAN_POINT('Ctrl Pts',(-2.19273585700006,2.2,-3.50249155100002));
#322391=CARTESIAN_POINT('Ctrl Pts',(-2.19181009200006,12.2,-3.50162504600001));
#322392=CARTESIAN_POINT('Ctrl Pts',(-2.19181009200006,5.2,-3.50162504600001));
#322393=CARTESIAN_POINT('Ctrl Pts',(-2.19181009200006,2.2,-3.50162504600001));
#322394=CARTESIAN_POINT('Ctrl Pts',(-2.19088905600006,12.2,-3.50076089500002));
#322395=CARTESIAN_POINT('Ctrl Pts',(-2.19088905600006,5.2,-3.50076089500002));
#322396=CARTESIAN_POINT('Ctrl Pts',(-2.19088905600006,2.2,-3.50076089500002));
#322397=CARTESIAN_POINT('Ctrl Pts',(-2.18997274800006,12.2,-3.49989911300002));
#322398=CARTESIAN_POINT('Ctrl Pts',(-2.18997274800006,5.2,-3.49989911300002));
#322399=CARTESIAN_POINT('Ctrl Pts',(-2.18997274800006,2.2,-3.49989911300002));
#322400=CARTESIAN_POINT('Ctrl Pts',(-2.18906116700006,12.2,-3.49903971300002));
#322401=CARTESIAN_POINT('Ctrl Pts',(-2.18906116700006,5.2,-3.49903971300002));
#322402=CARTESIAN_POINT('Ctrl Pts',(-2.18906116700006,2.2,-3.49903971300002));
#322403=CARTESIAN_POINT('Ctrl Pts',(-2.18815431200006,12.2,-3.49818271100002));
#322404=CARTESIAN_POINT('Ctrl Pts',(-2.18815431200006,5.2,-3.49818271100002));
#322405=CARTESIAN_POINT('Ctrl Pts',(-2.18815431200006,2.2,-3.49818271100002));
#322406=CARTESIAN_POINT('Ctrl Pts',(-2.18725218200006,12.2,-3.49732812300001));
#322407=CARTESIAN_POINT('Ctrl Pts',(-2.18725218200006,5.2,-3.49732812300001));
#322408=CARTESIAN_POINT('Ctrl Pts',(-2.18725218200006,2.2,-3.49732812300001));
#322409=CARTESIAN_POINT('Ctrl Pts',(-2.18635477700006,12.2,-3.49647596200001));
#322410=CARTESIAN_POINT('Ctrl Pts',(-2.18635477700006,5.2,-3.49647596200001));
#322411=CARTESIAN_POINT('Ctrl Pts',(-2.18635477700006,2.2,-3.49647596200001));
#322412=CARTESIAN_POINT('Ctrl Pts',(-2.18546209500006,12.2,-3.49562624400001));
#322413=CARTESIAN_POINT('Ctrl Pts',(-2.18546209500006,5.2,-3.49562624400001));
#322414=CARTESIAN_POINT('Ctrl Pts',(-2.18546209500006,2.2,-3.49562624400001));
#322415=CARTESIAN_POINT('Ctrl Pts',(-2.18457413600006,12.2,-3.49477898400002));
#322416=CARTESIAN_POINT('Ctrl Pts',(-2.18457413600006,5.2,-3.49477898400002));
#322417=CARTESIAN_POINT('Ctrl Pts',(-2.18457413600006,2.2,-3.49477898400002));
#322418=CARTESIAN_POINT('Ctrl Pts',(-2.18369089900006,12.2,-3.49393419600001));
#322419=CARTESIAN_POINT('Ctrl Pts',(-2.18369089900006,5.2,-3.49393419600001));
#322420=CARTESIAN_POINT('Ctrl Pts',(-2.18369089900006,2.2,-3.49393419600001));
#322421=CARTESIAN_POINT('Ctrl Pts',(-2.18281238100006,12.2,-3.49309189600001));
#322422=CARTESIAN_POINT('Ctrl Pts',(-2.18281238100006,5.2,-3.49309189600001));
#322423=CARTESIAN_POINT('Ctrl Pts',(-2.18281238100006,2.2,-3.49309189600001));
#322424=CARTESIAN_POINT('Ctrl Pts',(-2.18193858400006,12.2,-3.49225209900001));
#322425=CARTESIAN_POINT('Ctrl Pts',(-2.18193858400006,5.2,-3.49225209900001));
#322426=CARTESIAN_POINT('Ctrl Pts',(-2.18193858400006,2.2,-3.49225209900001));
#322427=CARTESIAN_POINT('Ctrl Pts',(-2.18106950600006,12.2,-3.49141482000002));
#322428=CARTESIAN_POINT('Ctrl Pts',(-2.18106950600006,5.2,-3.49141482000002));
#322429=CARTESIAN_POINT('Ctrl Pts',(-2.18106950600006,2.2,-3.49141482000002));
#322430=CARTESIAN_POINT('Ctrl Pts',(-2.18020514400005,12.2,-3.49058007400001));
#322431=CARTESIAN_POINT('Ctrl Pts',(-2.18020514400005,5.2,-3.49058007400001));
#322432=CARTESIAN_POINT('Ctrl Pts',(-2.18020514400005,2.2,-3.49058007400001));
#322433=CARTESIAN_POINT('Ctrl Pts',(-2.17934550000006,12.2,-3.48974787600001));
#322434=CARTESIAN_POINT('Ctrl Pts',(-2.17934550000006,5.2,-3.48974787600001));
#322435=CARTESIAN_POINT('Ctrl Pts',(-2.17934550000006,2.2,-3.48974787600001));
#322436=CARTESIAN_POINT('Ctrl Pts',(-2.17849057100006,12.2,-3.48891824200001));
#322437=CARTESIAN_POINT('Ctrl Pts',(-2.17849057100006,5.2,-3.48891824200001));
#322438=CARTESIAN_POINT('Ctrl Pts',(-2.17849057100006,2.2,-3.48891824200001));
#322439=CARTESIAN_POINT('Ctrl Pts',(-2.17764035600006,12.2,-3.48809118700002));
#322440=CARTESIAN_POINT('Ctrl Pts',(-2.17764035600006,5.2,-3.48809118700002));
#322441=CARTESIAN_POINT('Ctrl Pts',(-2.17764035600006,2.2,-3.48809118700002));
#322442=CARTESIAN_POINT('Ctrl Pts',(-2.17679485500006,12.2,-3.48726672600002));
#322443=CARTESIAN_POINT('Ctrl Pts',(-2.17679485500006,5.2,-3.48726672600002));
#322444=CARTESIAN_POINT('Ctrl Pts',(-2.17679485500006,2.2,-3.48726672600002));
#322445=CARTESIAN_POINT('Ctrl Pts',(-2.17595406600006,12.2,-3.48644487300001));
#322446=CARTESIAN_POINT('Ctrl Pts',(-2.17595406600006,5.2,-3.48644487300001));
#322447=CARTESIAN_POINT('Ctrl Pts',(-2.17595406600006,2.2,-3.48644487300001));
#322448=CARTESIAN_POINT('Ctrl Pts',(-2.17511798700006,12.2,-3.48562564600002));
#322449=CARTESIAN_POINT('Ctrl Pts',(-2.17511798700006,5.2,-3.48562564600002));
#322450=CARTESIAN_POINT('Ctrl Pts',(-2.17511798700006,2.2,-3.48562564600002));
#322451=CARTESIAN_POINT('Ctrl Pts',(-2.17428661800006,12.2,-3.48480905900002));
#322452=CARTESIAN_POINT('Ctrl Pts',(-2.17428661800006,5.2,-3.48480905900002));
#322453=CARTESIAN_POINT('Ctrl Pts',(-2.17428661800006,2.2,-3.48480905900002));
#322454=CARTESIAN_POINT('Ctrl Pts',(-2.17345995800006,12.2,-3.48399512700002));
#322455=CARTESIAN_POINT('Ctrl Pts',(-2.17345995800006,5.2,-3.48399512700002));
#322456=CARTESIAN_POINT('Ctrl Pts',(-2.17345995800006,2.2,-3.48399512700002));
#322457=CARTESIAN_POINT('Ctrl Pts',(-2.17263800500006,12.2,-3.48318386600001));
#322458=CARTESIAN_POINT('Ctrl Pts',(-2.17263800500006,5.2,-3.48318386600001));
#322459=CARTESIAN_POINT('Ctrl Pts',(-2.17263800500006,2.2,-3.48318386600001));
#322460=CARTESIAN_POINT('Ctrl Pts',(-2.17182075800006,12.2,-3.48237529200001));
#322461=CARTESIAN_POINT('Ctrl Pts',(-2.17182075800006,5.2,-3.48237529200001));
#322462=CARTESIAN_POINT('Ctrl Pts',(-2.17182075800006,2.2,-3.48237529200001));
#322463=CARTESIAN_POINT('Ctrl Pts',(-2.17100821500006,12.2,-3.48156941900001));
#322464=CARTESIAN_POINT('Ctrl Pts',(-2.17100821500006,5.2,-3.48156941900001));
#322465=CARTESIAN_POINT('Ctrl Pts',(-2.17100821500006,2.2,-3.48156941900001));
#322466=CARTESIAN_POINT('Ctrl Pts',(-2.17020037600005,12.2,-3.48076626400001));
#322467=CARTESIAN_POINT('Ctrl Pts',(-2.17020037600005,5.2,-3.48076626400001));
#322468=CARTESIAN_POINT('Ctrl Pts',(-2.17020037600005,2.2,-3.48076626400001));
#322469=CARTESIAN_POINT('Ctrl Pts',(-2.16939723900006,12.2,-3.47996584200001));
#322470=CARTESIAN_POINT('Ctrl Pts',(-2.16939723900006,5.2,-3.47996584200001));
#322471=CARTESIAN_POINT('Ctrl Pts',(-2.16939723900006,2.2,-3.47996584200001));
#322472=CARTESIAN_POINT('Ctrl Pts',(-2.16859880300006,12.2,-3.47916816900002));
#322473=CARTESIAN_POINT('Ctrl Pts',(-2.16859880300006,5.2,-3.47916816900002));
#322474=CARTESIAN_POINT('Ctrl Pts',(-2.16859880300006,2.2,-3.47916816900002));
#322475=CARTESIAN_POINT('Ctrl Pts',(-2.16780506500006,12.2,-3.47837326000001));
#322476=CARTESIAN_POINT('Ctrl Pts',(-2.16780506500006,5.2,-3.47837326000001));
#322477=CARTESIAN_POINT('Ctrl Pts',(-2.16780506500006,2.2,-3.47837326000001));
#322478=CARTESIAN_POINT('Ctrl Pts',(-2.16701602600006,12.2,-3.47758113100001));
#322479=CARTESIAN_POINT('Ctrl Pts',(-2.16701602600006,5.2,-3.47758113100001));
#322480=CARTESIAN_POINT('Ctrl Pts',(-2.16701602600006,2.2,-3.47758113100001));
#322481=CARTESIAN_POINT('Ctrl Pts',(-2.16623168300006,12.2,-3.47679179900001));
#322482=CARTESIAN_POINT('Ctrl Pts',(-2.16623168300006,5.2,-3.47679179900001));
#322483=CARTESIAN_POINT('Ctrl Pts',(-2.16623168300006,2.2,-3.47679179900001));
#322484=CARTESIAN_POINT('Ctrl Pts',(-2.16545203600006,12.2,-3.47600527800001));
#322485=CARTESIAN_POINT('Ctrl Pts',(-2.16545203600006,5.2,-3.47600527800001));
#322486=CARTESIAN_POINT('Ctrl Pts',(-2.16545203600006,2.2,-3.47600527800001));
#322487=CARTESIAN_POINT('Ctrl Pts',(-2.16467708200006,12.2,-3.47522158300002));
#322488=CARTESIAN_POINT('Ctrl Pts',(-2.16467708200006,5.2,-3.47522158300002));
#322489=CARTESIAN_POINT('Ctrl Pts',(-2.16467708200006,2.2,-3.47522158300002));
#322490=CARTESIAN_POINT('Ctrl Pts',(-2.16390682000006,12.2,-3.47444073300001));
#322491=CARTESIAN_POINT('Ctrl Pts',(-2.16390682000006,5.2,-3.47444073300001));
#322492=CARTESIAN_POINT('Ctrl Pts',(-2.16390682000006,2.2,-3.47444073300001));
#322493=CARTESIAN_POINT('Ctrl Pts',(-2.16314124800005,12.2,-3.47366274100001));
#322494=CARTESIAN_POINT('Ctrl Pts',(-2.16314124800005,5.2,-3.47366274100001));
#322495=CARTESIAN_POINT('Ctrl Pts',(-2.16314124800005,2.2,-3.47366274100001));
#322496=CARTESIAN_POINT('Ctrl Pts',(-2.16238036500005,12.2,-3.47288762500002));
#322497=CARTESIAN_POINT('Ctrl Pts',(-2.16238036500005,5.2,-3.47288762500002));
#322498=CARTESIAN_POINT('Ctrl Pts',(-2.16238036500005,2.2,-3.47288762500002));
#322499=CARTESIAN_POINT('Ctrl Pts',(-2.16162417000006,12.2,-3.47211539900002));
#322500=CARTESIAN_POINT('Ctrl Pts',(-2.16162417000006,5.2,-3.47211539900002));
#322501=CARTESIAN_POINT('Ctrl Pts',(-2.16162417000006,2.2,-3.47211539900002));
#322502=CARTESIAN_POINT('Ctrl Pts',(-2.16087266000006,12.2,-3.47134608100002));
#322503=CARTESIAN_POINT('Ctrl Pts',(-2.16087266000006,5.2,-3.47134608100002));
#322504=CARTESIAN_POINT('Ctrl Pts',(-2.16087266000006,2.2,-3.47134608100002));
#322505=CARTESIAN_POINT('Ctrl Pts',(-2.16012583500006,12.2,-3.47057968500001));
#322506=CARTESIAN_POINT('Ctrl Pts',(-2.16012583500006,5.2,-3.47057968500001));
#322507=CARTESIAN_POINT('Ctrl Pts',(-2.16012583500006,2.2,-3.47057968500001));
#322508=CARTESIAN_POINT('Ctrl Pts',(-2.15938369100006,12.2,-3.46981622800001));
#322509=CARTESIAN_POINT('Ctrl Pts',(-2.15938369100006,5.2,-3.46981622800001));
#322510=CARTESIAN_POINT('Ctrl Pts',(-2.15938369100006,2.2,-3.46981622800001));
#322511=CARTESIAN_POINT('Ctrl Pts',(-2.15864623000006,12.2,-3.46905572800001));
#322512=CARTESIAN_POINT('Ctrl Pts',(-2.15864623000006,5.2,-3.46905572800001));
#322513=CARTESIAN_POINT('Ctrl Pts',(-2.15864623000006,2.2,-3.46905572800001));
#322514=CARTESIAN_POINT('Ctrl Pts',(-2.15791344700006,12.2,-3.46829819800002));
#322515=CARTESIAN_POINT('Ctrl Pts',(-2.15791344700006,5.2,-3.46829819800002));
#322516=CARTESIAN_POINT('Ctrl Pts',(-2.15791344700006,2.2,-3.46829819800002));
#322517=CARTESIAN_POINT('Ctrl Pts',(-2.15718534100006,12.2,-3.46754365400002));
#322518=CARTESIAN_POINT('Ctrl Pts',(-2.15718534100006,5.2,-3.46754365400002));
#322519=CARTESIAN_POINT('Ctrl Pts',(-2.15718534100006,2.2,-3.46754365400002));
#322520=CARTESIAN_POINT('Ctrl Pts',(-2.15646191100006,12.2,-3.46679211500001));
#322521=CARTESIAN_POINT('Ctrl Pts',(-2.15646191100006,5.2,-3.46679211500001));
#322522=CARTESIAN_POINT('Ctrl Pts',(-2.15646191100006,2.2,-3.46679211500001));
#322523=CARTESIAN_POINT('Ctrl Pts',(-2.15574315500006,12.2,-3.46604359700001));
#322524=CARTESIAN_POINT('Ctrl Pts',(-2.15574315500006,5.2,-3.46604359700001));
#322525=CARTESIAN_POINT('Ctrl Pts',(-2.15574315500006,2.2,-3.46604359700001));
#322526=CARTESIAN_POINT('Ctrl Pts',(-2.15502907200006,12.2,-3.46529811400002));
#322527=CARTESIAN_POINT('Ctrl Pts',(-2.15502907200006,5.2,-3.46529811400002));
#322528=CARTESIAN_POINT('Ctrl Pts',(-2.15502907200006,2.2,-3.46529811400002));
#322529=CARTESIAN_POINT('Ctrl Pts',(-2.15431965800006,12.2,-3.46455568300001));
#322530=CARTESIAN_POINT('Ctrl Pts',(-2.15431965800006,5.2,-3.46455568300001));
#322531=CARTESIAN_POINT('Ctrl Pts',(-2.15431965800006,2.2,-3.46455568300001));
#322532=CARTESIAN_POINT('Ctrl Pts',(-2.15361491300006,12.2,-3.46381632200002));
#322533=CARTESIAN_POINT('Ctrl Pts',(-2.15361491300006,5.2,-3.46381632200002));
#322534=CARTESIAN_POINT('Ctrl Pts',(-2.15361491300006,2.2,-3.46381632200002));
#322535=CARTESIAN_POINT('Ctrl Pts',(-2.15291483500006,12.2,-3.46308004600001));
#322536=CARTESIAN_POINT('Ctrl Pts',(-2.15291483500006,5.2,-3.46308004600001));
#322537=CARTESIAN_POINT('Ctrl Pts',(-2.15291483500006,2.2,-3.46308004600001));
#322538=CARTESIAN_POINT('Ctrl Pts',(-2.15221942100006,12.2,-3.46234687200001));
#322539=CARTESIAN_POINT('Ctrl Pts',(-2.15221942100006,5.2,-3.46234687200001));
#322540=CARTESIAN_POINT('Ctrl Pts',(-2.15221942100006,2.2,-3.46234687200001));
#322541=CARTESIAN_POINT('Ctrl Pts',(-2.15152867000006,12.2,-3.46161681600002));
#322542=CARTESIAN_POINT('Ctrl Pts',(-2.15152867000006,5.2,-3.46161681600002));
#322543=CARTESIAN_POINT('Ctrl Pts',(-2.15152867000006,2.2,-3.46161681600002));
#322544=CARTESIAN_POINT('Ctrl Pts',(-2.15084257900005,12.2,-3.46088989500001));
#322545=CARTESIAN_POINT('Ctrl Pts',(-2.15084257900005,5.2,-3.46088989500001));
#322546=CARTESIAN_POINT('Ctrl Pts',(-2.15084257900005,2.2,-3.46088989500001));
#322547=CARTESIAN_POINT('Ctrl Pts',(-2.15016114900005,12.2,-3.46016612500001));
#322548=CARTESIAN_POINT('Ctrl Pts',(-2.15016114900005,5.2,-3.46016612500001));
#322549=CARTESIAN_POINT('Ctrl Pts',(-2.15016114900005,2.2,-3.46016612500001));
#322550=CARTESIAN_POINT('Ctrl Pts',(-2.14948437400006,12.2,-3.45944552300002));
#322551=CARTESIAN_POINT('Ctrl Pts',(-2.14948437400006,5.2,-3.45944552300002));
#322552=CARTESIAN_POINT('Ctrl Pts',(-2.14948437400006,2.2,-3.45944552300002));
#322553=CARTESIAN_POINT('Ctrl Pts',(-2.14881225400006,12.2,-3.45872810500001));
#322554=CARTESIAN_POINT('Ctrl Pts',(-2.14881225400006,5.2,-3.45872810500001));
#322555=CARTESIAN_POINT('Ctrl Pts',(-2.14881225400006,2.2,-3.45872810500001));
#322556=CARTESIAN_POINT('Ctrl Pts',(-2.14814478800006,12.2,-3.45801388900002));
#322557=CARTESIAN_POINT('Ctrl Pts',(-2.14814478800006,5.2,-3.45801388900002));
#322558=CARTESIAN_POINT('Ctrl Pts',(-2.14814478800006,2.2,-3.45801388900002));
#322559=CARTESIAN_POINT('Ctrl Pts',(-2.14748197100006,12.2,-3.45730289000001));
#322560=CARTESIAN_POINT('Ctrl Pts',(-2.14748197100006,5.2,-3.45730289000001));
#322561=CARTESIAN_POINT('Ctrl Pts',(-2.14748197100006,2.2,-3.45730289000001));
#322562=CARTESIAN_POINT('Ctrl Pts',(-2.14682380300005,12.2,-3.45659512600001));
#322563=CARTESIAN_POINT('Ctrl Pts',(-2.14682380300005,5.2,-3.45659512600001));
#322564=CARTESIAN_POINT('Ctrl Pts',(-2.14682380300005,2.2,-3.45659512600001));
#322565=CARTESIAN_POINT('Ctrl Pts',(-2.14617028200006,12.2,-3.45589061500001));
#322566=CARTESIAN_POINT('Ctrl Pts',(-2.14617028200006,5.2,-3.45589061500001));
#322567=CARTESIAN_POINT('Ctrl Pts',(-2.14617028200006,2.2,-3.45589061500001));
#322568=CARTESIAN_POINT('Ctrl Pts',(-2.14552140400006,12.2,-3.45518937000001));
#322569=CARTESIAN_POINT('Ctrl Pts',(-2.14552140400006,5.2,-3.45518937000001));
#322570=CARTESIAN_POINT('Ctrl Pts',(-2.14552140400006,2.2,-3.45518937000001));
#322571=CARTESIAN_POINT('Ctrl Pts',(-2.14487717000006,12.2,-3.45449141200001));
#322572=CARTESIAN_POINT('Ctrl Pts',(-2.14487717000006,5.2,-3.45449141200001));
#322573=CARTESIAN_POINT('Ctrl Pts',(-2.14487717000006,2.2,-3.45449141200001));
#322574=CARTESIAN_POINT('Ctrl Pts',(-2.14423757400006,12.2,-3.45379675600002));
#322575=CARTESIAN_POINT('Ctrl Pts',(-2.14423757400006,5.2,-3.45379675600002));
#322576=CARTESIAN_POINT('Ctrl Pts',(-2.14423757400006,2.2,-3.45379675600002));
#322577=CARTESIAN_POINT('Ctrl Pts',(-2.14360261700006,12.2,-3.45310541800002));
#322578=CARTESIAN_POINT('Ctrl Pts',(-2.14360261700006,5.2,-3.45310541800002));
#322579=CARTESIAN_POINT('Ctrl Pts',(-2.14360261700006,2.2,-3.45310541800002));
#322580=CARTESIAN_POINT('Ctrl Pts',(-2.14297229500006,12.2,-3.45241741600002));
#322581=CARTESIAN_POINT('Ctrl Pts',(-2.14297229500006,5.2,-3.45241741600002));
#322582=CARTESIAN_POINT('Ctrl Pts',(-2.14297229500006,2.2,-3.45241741600002));
#322583=CARTESIAN_POINT('Ctrl Pts',(-2.14234660600006,12.2,-3.45173276800002));
#322584=CARTESIAN_POINT('Ctrl Pts',(-2.14234660600006,5.2,-3.45173276800002));
#322585=CARTESIAN_POINT('Ctrl Pts',(-2.14234660600006,2.2,-3.45173276800002));
#322586=CARTESIAN_POINT('Ctrl Pts',(-2.14172554800005,12.2,-3.45105149000001));
#322587=CARTESIAN_POINT('Ctrl Pts',(-2.14172554800005,5.2,-3.45105149000001));
#322588=CARTESIAN_POINT('Ctrl Pts',(-2.14172554800005,2.2,-3.45105149000001));
#322589=CARTESIAN_POINT('Ctrl Pts',(-2.14110911800006,12.2,-3.45037359900001));
#322590=CARTESIAN_POINT('Ctrl Pts',(-2.14110911800006,5.2,-3.45037359900001));
#322591=CARTESIAN_POINT('Ctrl Pts',(-2.14110911800006,2.2,-3.45037359900001));
#322592=CARTESIAN_POINT('Ctrl Pts',(-2.14049731400006,12.2,-3.44969911300002));
#322593=CARTESIAN_POINT('Ctrl Pts',(-2.14049731400006,5.2,-3.44969911300002));
#322594=CARTESIAN_POINT('Ctrl Pts',(-2.14049731400006,2.2,-3.44969911300002));
#322595=CARTESIAN_POINT('Ctrl Pts',(-2.13989013300006,12.2,-3.44902804800002));
#322596=CARTESIAN_POINT('Ctrl Pts',(-2.13989013300006,5.2,-3.44902804800002));
#322597=CARTESIAN_POINT('Ctrl Pts',(-2.13989013300006,2.2,-3.44902804800002));
#322598=CARTESIAN_POINT('Ctrl Pts',(-2.13928757500006,12.2,-3.44836042300001));
#322599=CARTESIAN_POINT('Ctrl Pts',(-2.13928757500006,5.2,-3.44836042300001));
#322600=CARTESIAN_POINT('Ctrl Pts',(-2.13928757500006,2.2,-3.44836042300001));
#322601=CARTESIAN_POINT('Ctrl Pts',(-2.13868963400006,12.2,-3.44769625300001));
#322602=CARTESIAN_POINT('Ctrl Pts',(-2.13868963400006,5.2,-3.44769625300001));
#322603=CARTESIAN_POINT('Ctrl Pts',(-2.13868963400006,2.2,-3.44769625300001));
#322604=CARTESIAN_POINT('Ctrl Pts',(-2.13809631100006,12.2,-3.44703555800002));
#322605=CARTESIAN_POINT('Ctrl Pts',(-2.13809631100006,5.2,-3.44703555800002));
#322606=CARTESIAN_POINT('Ctrl Pts',(-2.13809631100006,2.2,-3.44703555800002));
#322607=CARTESIAN_POINT('Ctrl Pts',(-2.13750760000006,12.2,-3.44637835300002));
#322608=CARTESIAN_POINT('Ctrl Pts',(-2.13750760000006,5.2,-3.44637835300002));
#322609=CARTESIAN_POINT('Ctrl Pts',(-2.13750760000006,2.2,-3.44637835300002));
#322610=CARTESIAN_POINT('Ctrl Pts',(-2.13692350100006,12.2,-3.44572465600002));
#322611=CARTESIAN_POINT('Ctrl Pts',(-2.13692350100006,5.2,-3.44572465600002));
#322612=CARTESIAN_POINT('Ctrl Pts',(-2.13692350100006,2.2,-3.44572465600002));
#322613=CARTESIAN_POINT('Ctrl Pts',(-2.13634401000005,12.2,-3.44507448500002));
#322614=CARTESIAN_POINT('Ctrl Pts',(-2.13634401000005,5.2,-3.44507448500002));
#322615=CARTESIAN_POINT('Ctrl Pts',(-2.13634401000005,2.2,-3.44507448500002));
#322616=CARTESIAN_POINT('Ctrl Pts',(-2.13576912600006,12.2,-3.44442785800001));
#322617=CARTESIAN_POINT('Ctrl Pts',(-2.13576912600006,5.2,-3.44442785800001));
#322618=CARTESIAN_POINT('Ctrl Pts',(-2.13576912600006,2.2,-3.44442785800001));
#322619=CARTESIAN_POINT('Ctrl Pts',(-2.13519884400006,12.2,-3.44378479200001));
#322620=CARTESIAN_POINT('Ctrl Pts',(-2.13519884400006,5.2,-3.44378479200001));
#322621=CARTESIAN_POINT('Ctrl Pts',(-2.13519884400006,2.2,-3.44378479200001));
#322622=CARTESIAN_POINT('Ctrl Pts',(-2.13463316400006,12.2,-3.44314530400001));
#322623=CARTESIAN_POINT('Ctrl Pts',(-2.13463316400006,5.2,-3.44314530400001));
#322624=CARTESIAN_POINT('Ctrl Pts',(-2.13463316400006,2.2,-3.44314530400001));
#322625=CARTESIAN_POINT('Ctrl Pts',(-2.13407208100006,12.2,-3.44250941200002));
#322626=CARTESIAN_POINT('Ctrl Pts',(-2.13407208100006,5.2,-3.44250941200002));
#322627=CARTESIAN_POINT('Ctrl Pts',(-2.13407208100006,2.2,-3.44250941200002));
#322628=CARTESIAN_POINT('Ctrl Pts',(-2.13351559300006,12.2,-3.44187713400002));
#322629=CARTESIAN_POINT('Ctrl Pts',(-2.13351559300006,5.2,-3.44187713400002));
#322630=CARTESIAN_POINT('Ctrl Pts',(-2.13351559300006,2.2,-3.44187713400002));
#322631=CARTESIAN_POINT('Ctrl Pts',(-2.13296369900006,12.2,-3.44124848800002));
#322632=CARTESIAN_POINT('Ctrl Pts',(-2.13296369900006,5.2,-3.44124848800002));
#322633=CARTESIAN_POINT('Ctrl Pts',(-2.13296369900006,2.2,-3.44124848800002));
#322634=CARTESIAN_POINT('Ctrl Pts',(-2.13241639400006,12.2,-3.44062349100001));
#322635=CARTESIAN_POINT('Ctrl Pts',(-2.13241639400006,5.2,-3.44062349100001));
#322636=CARTESIAN_POINT('Ctrl Pts',(-2.13241639400006,2.2,-3.44062349100001));
#322637=CARTESIAN_POINT('Ctrl Pts',(-2.13187367600006,12.2,-3.44000216100001));
#322638=CARTESIAN_POINT('Ctrl Pts',(-2.13187367600006,5.2,-3.44000216100001));
#322639=CARTESIAN_POINT('Ctrl Pts',(-2.13187367600006,2.2,-3.44000216100001));
#322640=CARTESIAN_POINT('Ctrl Pts',(-2.13133554200006,12.2,-3.43938451500001));
#322641=CARTESIAN_POINT('Ctrl Pts',(-2.13133554200006,5.2,-3.43938451500001));
#322642=CARTESIAN_POINT('Ctrl Pts',(-2.13133554200006,2.2,-3.43938451500001));
#322643=CARTESIAN_POINT('Ctrl Pts',(-2.13080198900006,12.2,-3.43877057300002));
#322644=CARTESIAN_POINT('Ctrl Pts',(-2.13080198900006,5.2,-3.43877057300002));
#322645=CARTESIAN_POINT('Ctrl Pts',(-2.13080198900006,2.2,-3.43877057300002));
#322646=CARTESIAN_POINT('Ctrl Pts',(-2.13027301500006,12.2,-3.43816035200001));
#322647=CARTESIAN_POINT('Ctrl Pts',(-2.13027301500006,5.2,-3.43816035200001));
#322648=CARTESIAN_POINT('Ctrl Pts',(-2.13027301500006,2.2,-3.43816035200001));
#322649=CARTESIAN_POINT('Ctrl Pts',(-2.12974861500005,12.2,-3.43755386900002));
#322650=CARTESIAN_POINT('Ctrl Pts',(-2.12974861500005,5.2,-3.43755386900002));
#322651=CARTESIAN_POINT('Ctrl Pts',(-2.12974861500005,2.2,-3.43755386900002));
#322652=CARTESIAN_POINT('Ctrl Pts',(-2.12922878900006,12.2,-3.43695114400001));
#322653=CARTESIAN_POINT('Ctrl Pts',(-2.12922878900006,5.2,-3.43695114400001));
#322654=CARTESIAN_POINT('Ctrl Pts',(-2.12922878900006,2.2,-3.43695114400001));
#322655=CARTESIAN_POINT('Ctrl Pts',(-2.12871353300006,12.2,-3.43635219300001));
#322656=CARTESIAN_POINT('Ctrl Pts',(-2.12871353300006,5.2,-3.43635219300001));
#322657=CARTESIAN_POINT('Ctrl Pts',(-2.12871353300006,2.2,-3.43635219300001));
#322658=CARTESIAN_POINT('Ctrl Pts',(-2.12820284200005,12.2,-3.43575703600001));
#322659=CARTESIAN_POINT('Ctrl Pts',(-2.12820284200005,5.2,-3.43575703600001));
#322660=CARTESIAN_POINT('Ctrl Pts',(-2.12820284200005,2.2,-3.43575703600001));
#322661=CARTESIAN_POINT('Ctrl Pts',(-2.12769671400005,12.2,-3.43516569000001));
#322662=CARTESIAN_POINT('Ctrl Pts',(-2.12769671400005,5.2,-3.43516569000001));
#322663=CARTESIAN_POINT('Ctrl Pts',(-2.12769671400005,2.2,-3.43516569000001));
#322664=CARTESIAN_POINT('Ctrl Pts',(-2.12719514700006,12.2,-3.43457817300001));
#322665=CARTESIAN_POINT('Ctrl Pts',(-2.12719514700006,5.2,-3.43457817300001));
#322666=CARTESIAN_POINT('Ctrl Pts',(-2.12719514700006,2.2,-3.43457817300001));
#322667=CARTESIAN_POINT('Ctrl Pts',(-2.12669813800006,12.2,-3.43399450400002));
#322668=CARTESIAN_POINT('Ctrl Pts',(-2.12669813800006,5.2,-3.43399450400002));
#322669=CARTESIAN_POINT('Ctrl Pts',(-2.12669813800006,2.2,-3.43399450400002));
#322670=CARTESIAN_POINT('Ctrl Pts',(-2.12620568200005,12.2,-3.43341470100002));
#322671=CARTESIAN_POINT('Ctrl Pts',(-2.12620568200005,5.2,-3.43341470100002));
#322672=CARTESIAN_POINT('Ctrl Pts',(-2.12620568200005,2.2,-3.43341470100002));
#322673=CARTESIAN_POINT('Ctrl Pts',(-2.12571777800005,12.2,-3.43283878300001));
#322674=CARTESIAN_POINT('Ctrl Pts',(-2.12571777800005,5.2,-3.43283878300001));
#322675=CARTESIAN_POINT('Ctrl Pts',(-2.12571777800005,2.2,-3.43283878300001));
#322676=CARTESIAN_POINT('Ctrl Pts',(-2.12523442100006,12.2,-3.43226676700001));
#322677=CARTESIAN_POINT('Ctrl Pts',(-2.12523442100006,5.2,-3.43226676700001));
#322678=CARTESIAN_POINT('Ctrl Pts',(-2.12523442100006,2.2,-3.43226676700001));
#322679=CARTESIAN_POINT('Ctrl Pts',(-2.12475560800006,12.2,-3.43169867300002));
#322680=CARTESIAN_POINT('Ctrl Pts',(-2.12475560800006,5.2,-3.43169867300002));
#322681=CARTESIAN_POINT('Ctrl Pts',(-2.12475560800006,2.2,-3.43169867300002));
#322682=CARTESIAN_POINT('Ctrl Pts',(-2.12428133600006,12.2,-3.43113451900001));
#322683=CARTESIAN_POINT('Ctrl Pts',(-2.12428133600006,5.2,-3.43113451900001));
#322684=CARTESIAN_POINT('Ctrl Pts',(-2.12428133600006,2.2,-3.43113451900001));
#322685=CARTESIAN_POINT('Ctrl Pts',(-2.12381160300006,12.2,-3.43057432300002));
#322686=CARTESIAN_POINT('Ctrl Pts',(-2.12381160300006,5.2,-3.43057432300002));
#322687=CARTESIAN_POINT('Ctrl Pts',(-2.12381160300006,2.2,-3.43057432300002));
#322688=CARTESIAN_POINT('Ctrl Pts',(-2.12334640400006,12.2,-3.43001810500001));
#322689=CARTESIAN_POINT('Ctrl Pts',(-2.12334640400006,5.2,-3.43001810500001));
#322690=CARTESIAN_POINT('Ctrl Pts',(-2.12334640400006,2.2,-3.43001810500001));
#322691=CARTESIAN_POINT('Ctrl Pts',(-2.12288573600006,12.2,-3.42946588200002));
#322692=CARTESIAN_POINT('Ctrl Pts',(-2.12288573600006,5.2,-3.42946588200002));
#322693=CARTESIAN_POINT('Ctrl Pts',(-2.12288573600006,2.2,-3.42946588200002));
#322694=CARTESIAN_POINT('Ctrl Pts',(-2.12242959500006,12.2,-3.42891767300001));
#322695=CARTESIAN_POINT('Ctrl Pts',(-2.12242959500006,5.2,-3.42891767300001));
#322696=CARTESIAN_POINT('Ctrl Pts',(-2.12242959500006,2.2,-3.42891767300001));
#322697=CARTESIAN_POINT('Ctrl Pts',(-2.12197798100005,12.2,-3.42837349800002));
#322698=CARTESIAN_POINT('Ctrl Pts',(-2.12197798100005,5.2,-3.42837349800002));
#322699=CARTESIAN_POINT('Ctrl Pts',(-2.12197798100005,2.2,-3.42837349800002));
#322700=CARTESIAN_POINT('Ctrl Pts',(-2.12153088600005,12.2,-3.42783337400002));
#322701=CARTESIAN_POINT('Ctrl Pts',(-2.12153088600005,5.2,-3.42783337400002));
#322702=CARTESIAN_POINT('Ctrl Pts',(-2.12153088600005,2.2,-3.42783337400002));
#322703=CARTESIAN_POINT('Ctrl Pts',(-2.12108830800006,12.2,-3.42729732200001));
#322704=CARTESIAN_POINT('Ctrl Pts',(-2.12108830800006,5.2,-3.42729732200001));
#322705=CARTESIAN_POINT('Ctrl Pts',(-2.12108830800006,2.2,-3.42729732200001));
#322706=CARTESIAN_POINT('Ctrl Pts',(-2.12065024400005,12.2,-3.42676535900001));
#322707=CARTESIAN_POINT('Ctrl Pts',(-2.12065024400005,5.2,-3.42676535900001));
#322708=CARTESIAN_POINT('Ctrl Pts',(-2.12065024400005,2.2,-3.42676535900001));
#322709=CARTESIAN_POINT('Ctrl Pts',(-2.12021669100006,12.2,-3.42623750400001));
#322710=CARTESIAN_POINT('Ctrl Pts',(-2.12021669100006,5.2,-3.42623750400001));
#322711=CARTESIAN_POINT('Ctrl Pts',(-2.12021669100006,2.2,-3.42623750400001));
#322712=CARTESIAN_POINT('Ctrl Pts',(-2.11978764400006,12.2,-3.42571377800001));
#322713=CARTESIAN_POINT('Ctrl Pts',(-2.11978764400006,5.2,-3.42571377800001));
#322714=CARTESIAN_POINT('Ctrl Pts',(-2.11978764400006,2.2,-3.42571377800001));
#322715=CARTESIAN_POINT('Ctrl Pts',(-2.11936310100006,12.2,-3.42519419800002));
#322716=CARTESIAN_POINT('Ctrl Pts',(-2.11936310100006,5.2,-3.42519419800002));
#322717=CARTESIAN_POINT('Ctrl Pts',(-2.11936310100006,2.2,-3.42519419800002));
#322718=CARTESIAN_POINT('Ctrl Pts',(-2.11894305700006,12.2,-3.42467878500001));
#322719=CARTESIAN_POINT('Ctrl Pts',(-2.11894305700006,5.2,-3.42467878500001));
#322720=CARTESIAN_POINT('Ctrl Pts',(-2.11894305700006,2.2,-3.42467878500001));
#322721=CARTESIAN_POINT('Ctrl Pts',(-2.11852750900006,12.2,-3.42416755600001));
#322722=CARTESIAN_POINT('Ctrl Pts',(-2.11852750900006,5.2,-3.42416755600001));
#322723=CARTESIAN_POINT('Ctrl Pts',(-2.11852750900006,2.2,-3.42416755600001));
#322724=CARTESIAN_POINT('Ctrl Pts',(-2.11811645100005,12.2,-3.42366053200001));
#322725=CARTESIAN_POINT('Ctrl Pts',(-2.11811645100005,5.2,-3.42366053200001));
#322726=CARTESIAN_POINT('Ctrl Pts',(-2.11811645100005,2.2,-3.42366053200001));
#322727=CARTESIAN_POINT('Ctrl Pts',(-2.11770988300006,12.2,-3.42315773100001));
#322728=CARTESIAN_POINT('Ctrl Pts',(-2.11770988300006,5.2,-3.42315773100001));
#322729=CARTESIAN_POINT('Ctrl Pts',(-2.11770988300006,2.2,-3.42315773100001));
#322730=CARTESIAN_POINT('Ctrl Pts',(-2.11730780000006,12.2,-3.42265917200002));
#322731=CARTESIAN_POINT('Ctrl Pts',(-2.11730780000006,5.2,-3.42265917200002));
#322732=CARTESIAN_POINT('Ctrl Pts',(-2.11730780000006,2.2,-3.42265917200002));
#322733=CARTESIAN_POINT('Ctrl Pts',(-2.11691019700006,12.2,-3.42216487600002));
#322734=CARTESIAN_POINT('Ctrl Pts',(-2.11691019700006,5.2,-3.42216487600002));
#322735=CARTESIAN_POINT('Ctrl Pts',(-2.11691019700006,2.2,-3.42216487600002));
#322736=CARTESIAN_POINT('Ctrl Pts',(-2.11651707000006,12.2,-3.42167486200001));
#322737=CARTESIAN_POINT('Ctrl Pts',(-2.11651707000006,5.2,-3.42167486200001));
#322738=CARTESIAN_POINT('Ctrl Pts',(-2.11651707000006,2.2,-3.42167486200001));
#322739=CARTESIAN_POINT('Ctrl Pts',(-2.11612841600005,12.2,-3.42118914800002));
#322740=CARTESIAN_POINT('Ctrl Pts',(-2.11612841600005,5.2,-3.42118914800002));
#322741=CARTESIAN_POINT('Ctrl Pts',(-2.11612841600005,2.2,-3.42118914800002));
#322742=CARTESIAN_POINT('Ctrl Pts',(-2.11574423200006,12.2,-3.42070775600002));
#322743=CARTESIAN_POINT('Ctrl Pts',(-2.11574423200006,5.2,-3.42070775600002));
#322744=CARTESIAN_POINT('Ctrl Pts',(-2.11574423200006,2.2,-3.42070775600002));
#322745=CARTESIAN_POINT('Ctrl Pts',(-2.11536451200006,12.2,-3.42023070300002));
#322746=CARTESIAN_POINT('Ctrl Pts',(-2.11536451200006,5.2,-3.42023070300002));
#322747=CARTESIAN_POINT('Ctrl Pts',(-2.11536451200006,2.2,-3.42023070300002));
#322748=CARTESIAN_POINT('Ctrl Pts',(-2.11498925300006,12.2,-3.41975801000002));
#322749=CARTESIAN_POINT('Ctrl Pts',(-2.11498925300006,5.2,-3.41975801000002));
#322750=CARTESIAN_POINT('Ctrl Pts',(-2.11498925300006,2.2,-3.41975801000002));
#322751=CARTESIAN_POINT('Ctrl Pts',(-2.11461845100006,12.2,-3.41928969700001));
#322752=CARTESIAN_POINT('Ctrl Pts',(-2.11461845100006,5.2,-3.41928969700001));
#322753=CARTESIAN_POINT('Ctrl Pts',(-2.11461845100006,2.2,-3.41928969700001));
#322754=CARTESIAN_POINT('Ctrl Pts',(-2.11425210100006,12.2,-3.41882578300002));
#322755=CARTESIAN_POINT('Ctrl Pts',(-2.11425210100006,5.2,-3.41882578300002));
#322756=CARTESIAN_POINT('Ctrl Pts',(-2.11425210100006,2.2,-3.41882578300002));
#322757=CARTESIAN_POINT('Ctrl Pts',(-2.11389020000006,12.2,-3.41836628800001));
#322758=CARTESIAN_POINT('Ctrl Pts',(-2.11389020000006,5.2,-3.41836628800001));
#322759=CARTESIAN_POINT('Ctrl Pts',(-2.11389020000006,2.2,-3.41836628800001));
#322760=CARTESIAN_POINT('Ctrl Pts',(-2.11353274400006,12.2,-3.41791123100001));
#322761=CARTESIAN_POINT('Ctrl Pts',(-2.11353274400006,5.2,-3.41791123100001));
#322762=CARTESIAN_POINT('Ctrl Pts',(-2.11353274400006,2.2,-3.41791123100001));
#322763=CARTESIAN_POINT('Ctrl Pts',(-2.11317972800006,12.2,-3.41746063500001));
#322764=CARTESIAN_POINT('Ctrl Pts',(-2.11317972800006,5.2,-3.41746063500001));
#322765=CARTESIAN_POINT('Ctrl Pts',(-2.11317972800006,2.2,-3.41746063500001));
#322766=CARTESIAN_POINT('Ctrl Pts',(-2.11283114900006,12.2,-3.41701451600001));
#322767=CARTESIAN_POINT('Ctrl Pts',(-2.11283114900006,5.2,-3.41701451600001));
#322768=CARTESIAN_POINT('Ctrl Pts',(-2.11283114900006,2.2,-3.41701451600001));
#322769=CARTESIAN_POINT('Ctrl Pts',(-2.11248700100006,12.2,-3.41657289700001));
#322770=CARTESIAN_POINT('Ctrl Pts',(-2.11248700100006,5.2,-3.41657289700001));
#322771=CARTESIAN_POINT('Ctrl Pts',(-2.11248700100006,2.2,-3.41657289700001));
#322772=CARTESIAN_POINT('Ctrl Pts',(-2.11214728000006,12.2,-3.41613579500001));
#322773=CARTESIAN_POINT('Ctrl Pts',(-2.11214728000006,5.2,-3.41613579500001));
#322774=CARTESIAN_POINT('Ctrl Pts',(-2.11214728000006,2.2,-3.41613579500001));
#322775=CARTESIAN_POINT('Ctrl Pts',(-2.11181198300006,12.2,-3.41570323300001));
#322776=CARTESIAN_POINT('Ctrl Pts',(-2.11181198300006,5.2,-3.41570323300001));
#322777=CARTESIAN_POINT('Ctrl Pts',(-2.11181198300006,2.2,-3.41570323300001));
#322778=CARTESIAN_POINT('Ctrl Pts',(-2.11148110500006,12.2,-3.41527523000002));
#322779=CARTESIAN_POINT('Ctrl Pts',(-2.11148110500006,5.2,-3.41527523000002));
#322780=CARTESIAN_POINT('Ctrl Pts',(-2.11148110500006,2.2,-3.41527523000002));
#322781=CARTESIAN_POINT('Ctrl Pts',(-2.11115464100006,12.2,-3.41485180600001));
#322782=CARTESIAN_POINT('Ctrl Pts',(-2.11115464100006,5.2,-3.41485180600001));
#322783=CARTESIAN_POINT('Ctrl Pts',(-2.11115464100006,2.2,-3.41485180600001));
#322784=CARTESIAN_POINT('Ctrl Pts',(-2.11083258700006,12.2,-3.41443298300002));
#322785=CARTESIAN_POINT('Ctrl Pts',(-2.11083258700006,5.2,-3.41443298300002));
#322786=CARTESIAN_POINT('Ctrl Pts',(-2.11083258700006,2.2,-3.41443298300002));
#322787=CARTESIAN_POINT('Ctrl Pts',(-2.11051493900006,12.2,-3.41401877900001));
#322788=CARTESIAN_POINT('Ctrl Pts',(-2.11051493900006,5.2,-3.41401877900001));
#322789=CARTESIAN_POINT('Ctrl Pts',(-2.11051493900006,2.2,-3.41401877900001));
#322790=CARTESIAN_POINT('Ctrl Pts',(-2.11020169000005,12.2,-3.41360921600002));
#322791=CARTESIAN_POINT('Ctrl Pts',(-2.11020169000005,5.2,-3.41360921600002));
#322792=CARTESIAN_POINT('Ctrl Pts',(-2.11020169000005,2.2,-3.41360921600002));
#322793=CARTESIAN_POINT('Ctrl Pts',(-2.10989284000005,12.2,-3.41320431400002));
#322794=CARTESIAN_POINT('Ctrl Pts',(-2.10989284000005,5.2,-3.41320431400002));
#322795=CARTESIAN_POINT('Ctrl Pts',(-2.10989284000005,2.2,-3.41320431400002));
#322796=CARTESIAN_POINT('Ctrl Pts',(-2.10958838100006,12.2,-3.41280409200001));
#322797=CARTESIAN_POINT('Ctrl Pts',(-2.10958838100006,5.2,-3.41280409200001));
#322798=CARTESIAN_POINT('Ctrl Pts',(-2.10958838100006,2.2,-3.41280409200001));
#322799=CARTESIAN_POINT('Ctrl Pts',(-2.10928830800006,12.2,-3.41240857400001));
#322800=CARTESIAN_POINT('Ctrl Pts',(-2.10928830800006,5.2,-3.41240857400001));
#322801=CARTESIAN_POINT('Ctrl Pts',(-2.10928830800006,2.2,-3.41240857400001));
#322802=CARTESIAN_POINT('Ctrl Pts',(-2.10899261900006,12.2,-3.41201777800002));
#322803=CARTESIAN_POINT('Ctrl Pts',(-2.10899261900006,5.2,-3.41201777800002));
#322804=CARTESIAN_POINT('Ctrl Pts',(-2.10899261900006,2.2,-3.41201777800002));
#322805=CARTESIAN_POINT('Ctrl Pts',(-2.10870130700005,12.2,-3.41163172500002));
#322806=CARTESIAN_POINT('Ctrl Pts',(-2.10870130700005,5.2,-3.41163172500002));
#322807=CARTESIAN_POINT('Ctrl Pts',(-2.10870130700005,2.2,-3.41163172500002));
#322808=CARTESIAN_POINT('Ctrl Pts',(-2.10841436900005,12.2,-3.41125043600002));
#322809=CARTESIAN_POINT('Ctrl Pts',(-2.10841436900005,5.2,-3.41125043600002));
#322810=CARTESIAN_POINT('Ctrl Pts',(-2.10841436900005,2.2,-3.41125043600002));
#322811=CARTESIAN_POINT('Ctrl Pts',(-2.10813179800006,12.2,-3.41087393300001));
#322812=CARTESIAN_POINT('Ctrl Pts',(-2.10813179800006,5.2,-3.41087393300001));
#322813=CARTESIAN_POINT('Ctrl Pts',(-2.10813179800006,2.2,-3.41087393300001));
#322814=CARTESIAN_POINT('Ctrl Pts',(-2.10785359100006,12.2,-3.41050223400002));
#322815=CARTESIAN_POINT('Ctrl Pts',(-2.10785359100006,5.2,-3.41050223400002));
#322816=CARTESIAN_POINT('Ctrl Pts',(-2.10785359100006,2.2,-3.41050223400002));
#322817=CARTESIAN_POINT('Ctrl Pts',(-2.10757974300006,12.2,-3.41013536400002));
#322818=CARTESIAN_POINT('Ctrl Pts',(-2.10757974300006,5.2,-3.41013536400002));
#322819=CARTESIAN_POINT('Ctrl Pts',(-2.10757974300006,2.2,-3.41013536400002));
#322820=CARTESIAN_POINT('Ctrl Pts',(-2.10731024700006,12.2,-3.40977334100002));
#322821=CARTESIAN_POINT('Ctrl Pts',(-2.10731024700006,5.2,-3.40977334100002));
#322822=CARTESIAN_POINT('Ctrl Pts',(-2.10731024700006,2.2,-3.40977334100002));
#322823=CARTESIAN_POINT('Ctrl Pts',(-2.10704510100005,12.2,-3.40941618700001));
#322824=CARTESIAN_POINT('Ctrl Pts',(-2.10704510100005,5.2,-3.40941618700001));
#322825=CARTESIAN_POINT('Ctrl Pts',(-2.10704510100005,2.2,-3.40941618700001));
#322826=CARTESIAN_POINT('Ctrl Pts',(-2.10678429900006,12.2,-3.40906392200001));
#322827=CARTESIAN_POINT('Ctrl Pts',(-2.10678429900006,5.2,-3.40906392200001));
#322828=CARTESIAN_POINT('Ctrl Pts',(-2.10678429900006,2.2,-3.40906392200001));
#322829=CARTESIAN_POINT('Ctrl Pts',(-2.10652783500006,12.2,-3.40871657000001));
#322830=CARTESIAN_POINT('Ctrl Pts',(-2.10652783500006,5.2,-3.40871657000001));
#322831=CARTESIAN_POINT('Ctrl Pts',(-2.10652783500006,2.2,-3.40871657000001));
#322832=CARTESIAN_POINT('Ctrl Pts',(-2.10627570600006,12.2,-3.40837415000002));
#322833=CARTESIAN_POINT('Ctrl Pts',(-2.10627570600006,5.2,-3.40837415000002));
#322834=CARTESIAN_POINT('Ctrl Pts',(-2.10627570600006,2.2,-3.40837415000002));
#322835=CARTESIAN_POINT('Ctrl Pts',(-2.10602790400006,12.2,-3.40803668300001));
#322836=CARTESIAN_POINT('Ctrl Pts',(-2.10602790400006,5.2,-3.40803668300001));
#322837=CARTESIAN_POINT('Ctrl Pts',(-2.10602790400006,2.2,-3.40803668300001));
#322838=CARTESIAN_POINT('Ctrl Pts',(-2.10578442500006,12.2,-3.40770419100001));
#322839=CARTESIAN_POINT('Ctrl Pts',(-2.10578442500006,5.2,-3.40770419100001));
#322840=CARTESIAN_POINT('Ctrl Pts',(-2.10578442500006,2.2,-3.40770419100001));
#322841=CARTESIAN_POINT('Ctrl Pts',(-2.10554526400006,12.2,-3.40737669700002));
#322842=CARTESIAN_POINT('Ctrl Pts',(-2.10554526400006,5.2,-3.40737669700002));
#322843=CARTESIAN_POINT('Ctrl Pts',(-2.10554526400006,2.2,-3.40737669700002));
#322844=CARTESIAN_POINT('Ctrl Pts',(-2.10531041800006,12.2,-3.40705422000001));
#322845=CARTESIAN_POINT('Ctrl Pts',(-2.10531041800006,5.2,-3.40705422000001));
#322846=CARTESIAN_POINT('Ctrl Pts',(-2.10531041800006,2.2,-3.40705422000001));
#322847=CARTESIAN_POINT('Ctrl Pts',(-2.10507987800006,12.2,-3.40673678300002));
#322848=CARTESIAN_POINT('Ctrl Pts',(-2.10507987800006,5.2,-3.40673678300002));
#322849=CARTESIAN_POINT('Ctrl Pts',(-2.10507987800006,2.2,-3.40673678300002));
#322850=CARTESIAN_POINT('Ctrl Pts',(-2.10485364100006,12.2,-3.40642440800002));
#322851=CARTESIAN_POINT('Ctrl Pts',(-2.10485364100006,5.2,-3.40642440800002));
#322852=CARTESIAN_POINT('Ctrl Pts',(-2.10485364100006,2.2,-3.40642440800002));
#322853=CARTESIAN_POINT('Ctrl Pts',(-2.10463170000006,12.2,-3.40611711600001));
#322854=CARTESIAN_POINT('Ctrl Pts',(-2.10463170000006,5.2,-3.40611711600001));
#322855=CARTESIAN_POINT('Ctrl Pts',(-2.10463170000006,2.2,-3.40611711600001));
#322856=CARTESIAN_POINT('Ctrl Pts',(-2.10441405000005,12.2,-3.40581492800001));
#322857=CARTESIAN_POINT('Ctrl Pts',(-2.10441405000005,5.2,-3.40581492800001));
#322858=CARTESIAN_POINT('Ctrl Pts',(-2.10441405000005,2.2,-3.40581492800001));
#322859=CARTESIAN_POINT('Ctrl Pts',(-2.10420068800006,12.2,-3.40551786700001));
#322860=CARTESIAN_POINT('Ctrl Pts',(-2.10420068800006,5.2,-3.40551786700001));
#322861=CARTESIAN_POINT('Ctrl Pts',(-2.10420068800006,2.2,-3.40551786700001));
#322862=CARTESIAN_POINT('Ctrl Pts',(-2.10399160500006,12.2,-3.40522595500001));
#322863=CARTESIAN_POINT('Ctrl Pts',(-2.10399160500006,5.2,-3.40522595500001));
#322864=CARTESIAN_POINT('Ctrl Pts',(-2.10399160500006,2.2,-3.40522595500001));
#322865=CARTESIAN_POINT('Ctrl Pts',(-2.10378679800006,12.2,-3.40493921300002));
#322866=CARTESIAN_POINT('Ctrl Pts',(-2.10378679800006,5.2,-3.40493921300002));
#322867=CARTESIAN_POINT('Ctrl Pts',(-2.10378679800006,2.2,-3.40493921300002));
#322868=CARTESIAN_POINT('Ctrl Pts',(-2.10358626000006,12.2,-3.40465766400001));
#322869=CARTESIAN_POINT('Ctrl Pts',(-2.10358626000006,5.2,-3.40465766400001));
#322870=CARTESIAN_POINT('Ctrl Pts',(-2.10358626000006,2.2,-3.40465766400001));
#322871=CARTESIAN_POINT('Ctrl Pts',(-2.10338998700006,12.2,-3.40438132900001));
#322872=CARTESIAN_POINT('Ctrl Pts',(-2.10338998700006,5.2,-3.40438132900001));
#322873=CARTESIAN_POINT('Ctrl Pts',(-2.10338998700006,2.2,-3.40438132900001));
#322874=CARTESIAN_POINT('Ctrl Pts',(-2.10319797000006,12.2,-3.40411023100001));
#322875=CARTESIAN_POINT('Ctrl Pts',(-2.10319797000006,5.2,-3.40411023100001));
#322876=CARTESIAN_POINT('Ctrl Pts',(-2.10319797000006,2.2,-3.40411023100001));
#322877=CARTESIAN_POINT('Ctrl Pts',(-2.10301020700005,12.2,-3.40384439300002));
#322878=CARTESIAN_POINT('Ctrl Pts',(-2.10301020700005,5.2,-3.40384439300002));
#322879=CARTESIAN_POINT('Ctrl Pts',(-2.10301020700005,2.2,-3.40384439300002));
#322880=CARTESIAN_POINT('Ctrl Pts',(-2.10282669100006,12.2,-3.40358383500002));
#322881=CARTESIAN_POINT('Ctrl Pts',(-2.10282669100006,5.2,-3.40358383500002));
#322882=CARTESIAN_POINT('Ctrl Pts',(-2.10282669100006,2.2,-3.40358383500002));
#322883=CARTESIAN_POINT('Ctrl Pts',(-2.10264741500006,12.2,-3.40332858100002));
#322884=CARTESIAN_POINT('Ctrl Pts',(-2.10264741500006,5.2,-3.40332858100002));
#322885=CARTESIAN_POINT('Ctrl Pts',(-2.10264741500006,2.2,-3.40332858100002));
#322886=CARTESIAN_POINT('Ctrl Pts',(-2.10247237400006,12.2,-3.40307865400002));
#322887=CARTESIAN_POINT('Ctrl Pts',(-2.10247237400006,5.2,-3.40307865400002));
#322888=CARTESIAN_POINT('Ctrl Pts',(-2.10247237400006,2.2,-3.40307865400002));
#322889=CARTESIAN_POINT('Ctrl Pts',(-2.10230156200006,12.2,-3.40283407500001));
#322890=CARTESIAN_POINT('Ctrl Pts',(-2.10230156200006,5.2,-3.40283407500001));
#322891=CARTESIAN_POINT('Ctrl Pts',(-2.10230156200006,2.2,-3.40283407500001));
#322892=CARTESIAN_POINT('Ctrl Pts',(-2.10213497400006,12.2,-3.40259486800001));
#322893=CARTESIAN_POINT('Ctrl Pts',(-2.10213497400006,5.2,-3.40259486800001));
#322894=CARTESIAN_POINT('Ctrl Pts',(-2.10213497400006,2.2,-3.40259486800001));
#322895=CARTESIAN_POINT('Ctrl Pts',(-2.10197260400005,12.2,-3.40236105400002));
#322896=CARTESIAN_POINT('Ctrl Pts',(-2.10197260400005,5.2,-3.40236105400002));
#322897=CARTESIAN_POINT('Ctrl Pts',(-2.10197260400005,2.2,-3.40236105400002));
#322898=CARTESIAN_POINT('Ctrl Pts',(-2.10181444400006,12.2,-3.40213265700001));
#322899=CARTESIAN_POINT('Ctrl Pts',(-2.10181444400006,5.2,-3.40213265700001));
#322900=CARTESIAN_POINT('Ctrl Pts',(-2.10181444400006,2.2,-3.40213265700001));
#322901=CARTESIAN_POINT('Ctrl Pts',(-2.10166048900006,12.2,-3.40190970000001));
#322902=CARTESIAN_POINT('Ctrl Pts',(-2.10166048900006,5.2,-3.40190970000001));
#322903=CARTESIAN_POINT('Ctrl Pts',(-2.10166048900006,2.2,-3.40190970000001));
#322904=CARTESIAN_POINT('Ctrl Pts',(-2.10151073300006,12.2,-3.40169220500002));
#322905=CARTESIAN_POINT('Ctrl Pts',(-2.10151073300006,5.2,-3.40169220500002));
#322906=CARTESIAN_POINT('Ctrl Pts',(-2.10151073300006,2.2,-3.40169220500002));
#322907=CARTESIAN_POINT('Ctrl Pts',(-2.10136517100006,12.2,-3.40148019400001));
#322908=CARTESIAN_POINT('Ctrl Pts',(-2.10136517100006,5.2,-3.40148019400001));
#322909=CARTESIAN_POINT('Ctrl Pts',(-2.10136517100006,2.2,-3.40148019400001));
#322910=CARTESIAN_POINT('Ctrl Pts',(-2.10122379400006,12.2,-3.40127369300002));
#322911=CARTESIAN_POINT('Ctrl Pts',(-2.10122379400006,5.2,-3.40127369300002));
#322912=CARTESIAN_POINT('Ctrl Pts',(-2.10122379400006,2.2,-3.40127369300002));
#322913=CARTESIAN_POINT('Ctrl Pts',(-2.10108659900006,12.2,-3.40107272300001));
#322914=CARTESIAN_POINT('Ctrl Pts',(-2.10108659900006,5.2,-3.40107272300001));
#322915=CARTESIAN_POINT('Ctrl Pts',(-2.10108659900006,2.2,-3.40107272300001));
#322916=CARTESIAN_POINT('Ctrl Pts',(-2.10095357700005,12.2,-3.40087730700001));
#322917=CARTESIAN_POINT('Ctrl Pts',(-2.10095357700005,5.2,-3.40087730700001));
#322918=CARTESIAN_POINT('Ctrl Pts',(-2.10095357700005,2.2,-3.40087730700001));
#322919=CARTESIAN_POINT('Ctrl Pts',(-2.10082472400006,12.2,-3.40068746900001));
#322920=CARTESIAN_POINT('Ctrl Pts',(-2.10082472400006,5.2,-3.40068746900001));
#322921=CARTESIAN_POINT('Ctrl Pts',(-2.10082472400006,2.2,-3.40068746900001));
#322922=CARTESIAN_POINT('Ctrl Pts',(-2.10070003200005,12.2,-3.40050323100002));
#322923=CARTESIAN_POINT('Ctrl Pts',(-2.10070003200005,5.2,-3.40050323100002));
#322924=CARTESIAN_POINT('Ctrl Pts',(-2.10070003200005,2.2,-3.40050323100002));
#322925=CARTESIAN_POINT('Ctrl Pts',(-2.10057949400006,12.2,-3.40032461800002));
#322926=CARTESIAN_POINT('Ctrl Pts',(-2.10057949400006,5.2,-3.40032461800002));
#322927=CARTESIAN_POINT('Ctrl Pts',(-2.10057949400006,2.2,-3.40032461800002));
#322928=CARTESIAN_POINT('Ctrl Pts',(-2.10046310500006,12.2,-3.40015165400001));
#322929=CARTESIAN_POINT('Ctrl Pts',(-2.10046310500006,5.2,-3.40015165400001));
#322930=CARTESIAN_POINT('Ctrl Pts',(-2.10046310500006,2.2,-3.40015165400001));
#322931=CARTESIAN_POINT('Ctrl Pts',(-2.10035085800006,12.2,-3.39998436000001));
#322932=CARTESIAN_POINT('Ctrl Pts',(-2.10035085800006,5.2,-3.39998436000001));
#322933=CARTESIAN_POINT('Ctrl Pts',(-2.10035085800006,2.2,-3.39998436000001));
#322934=CARTESIAN_POINT('Ctrl Pts',(-2.10024274500006,12.2,-3.39982276200002));
#322935=CARTESIAN_POINT('Ctrl Pts',(-2.10024274500006,5.2,-3.39982276200002));
#322936=CARTESIAN_POINT('Ctrl Pts',(-2.10024274500006,2.2,-3.39982276200002));
#322937=CARTESIAN_POINT('Ctrl Pts',(-2.10013876200006,12.2,-3.39966688300001));
#322938=CARTESIAN_POINT('Ctrl Pts',(-2.10013876200006,5.2,-3.39966688300001));
#322939=CARTESIAN_POINT('Ctrl Pts',(-2.10013876200006,2.2,-3.39966688300001));
#322940=CARTESIAN_POINT('Ctrl Pts',(-2.10003890000006,12.2,-3.39951674700002));
#322941=CARTESIAN_POINT('Ctrl Pts',(-2.10003890000006,5.2,-3.39951674700002));
#322942=CARTESIAN_POINT('Ctrl Pts',(-2.10003890000006,2.2,-3.39951674700002));
#322943=CARTESIAN_POINT('Ctrl Pts',(-2.09994315400006,12.2,-3.39937237600001));
#322944=CARTESIAN_POINT('Ctrl Pts',(-2.09994315400006,5.2,-3.39937237600001));
#322945=CARTESIAN_POINT('Ctrl Pts',(-2.09994315400006,2.2,-3.39937237600001));
#322946=CARTESIAN_POINT('Ctrl Pts',(-2.09985151600006,12.2,-3.39923379500001));
#322947=CARTESIAN_POINT('Ctrl Pts',(-2.09985151600006,5.2,-3.39923379500001));
#322948=CARTESIAN_POINT('Ctrl Pts',(-2.09985151600006,2.2,-3.39923379500001));
#322949=CARTESIAN_POINT('Ctrl Pts',(-2.09976398000005,12.2,-3.39910102700001));
#322950=CARTESIAN_POINT('Ctrl Pts',(-2.09976398000005,5.2,-3.39910102700001));
#322951=CARTESIAN_POINT('Ctrl Pts',(-2.09976398000005,2.2,-3.39910102700001));
#322952=CARTESIAN_POINT('Ctrl Pts',(-2.09968053900006,12.2,-3.39897409600002));
#322953=CARTESIAN_POINT('Ctrl Pts',(-2.09968053900006,5.2,-3.39897409600002));
#322954=CARTESIAN_POINT('Ctrl Pts',(-2.09968053900006,2.2,-3.39897409600002));
#322955=CARTESIAN_POINT('Ctrl Pts',(-2.09960118500006,12.2,-3.39885302900001));
#322956=CARTESIAN_POINT('Ctrl Pts',(-2.09960118500006,5.2,-3.39885302900001));
#322957=CARTESIAN_POINT('Ctrl Pts',(-2.09960118500006,2.2,-3.39885302900001));
#322958=CARTESIAN_POINT('Ctrl Pts',(-2.09952591200006,12.2,-3.39873785000002));
#322959=CARTESIAN_POINT('Ctrl Pts',(-2.09952591200006,5.2,-3.39873785000002));
#322960=CARTESIAN_POINT('Ctrl Pts',(-2.09952591200006,2.2,-3.39873785000002));
#322961=CARTESIAN_POINT('Ctrl Pts',(-2.09945471100006,12.2,-3.39862858500001));
#322962=CARTESIAN_POINT('Ctrl Pts',(-2.09945471100006,5.2,-3.39862858500001));
#322963=CARTESIAN_POINT('Ctrl Pts',(-2.09945471100006,2.2,-3.39862858500001));
#322964=CARTESIAN_POINT('Ctrl Pts',(-2.09938757500006,12.2,-3.39852525600001));
#322965=CARTESIAN_POINT('Ctrl Pts',(-2.09938757500006,5.2,-3.39852525600001));
#322966=CARTESIAN_POINT('Ctrl Pts',(-2.09938757500006,2.2,-3.39852525600001));
#322967=CARTESIAN_POINT('Ctrl Pts',(-2.09932450100006,12.2,-3.39842788700001));
#322968=CARTESIAN_POINT('Ctrl Pts',(-2.09932450100006,5.2,-3.39842788700001));
#322969=CARTESIAN_POINT('Ctrl Pts',(-2.09932450100006,2.2,-3.39842788700001));
#322970=CARTESIAN_POINT('Ctrl Pts',(-2.09926547900006,12.2,-3.39833649900001));
#322971=CARTESIAN_POINT('Ctrl Pts',(-2.09926547900006,5.2,-3.39833649900001));
#322972=CARTESIAN_POINT('Ctrl Pts',(-2.09926547900006,2.2,-3.39833649900001));
#322973=CARTESIAN_POINT('Ctrl Pts',(-2.09921050200006,12.2,-3.39825111500001));
#322974=CARTESIAN_POINT('Ctrl Pts',(-2.09921050200006,5.2,-3.39825111500001));
#322975=CARTESIAN_POINT('Ctrl Pts',(-2.09921050200006,2.2,-3.39825111500001));
#322976=CARTESIAN_POINT('Ctrl Pts',(-2.09915956600006,12.2,-3.39817176000001));
#322977=CARTESIAN_POINT('Ctrl Pts',(-2.09915956600006,5.2,-3.39817176000001));
#322978=CARTESIAN_POINT('Ctrl Pts',(-2.09915956600006,2.2,-3.39817176000001));
#322979=CARTESIAN_POINT('Ctrl Pts',(-2.09911266000006,12.2,-3.39809846200001));
#322980=CARTESIAN_POINT('Ctrl Pts',(-2.09911266000006,5.2,-3.39809846200001));
#322981=CARTESIAN_POINT('Ctrl Pts',(-2.09911266000006,2.2,-3.39809846200001));
#322982=CARTESIAN_POINT('Ctrl Pts',(-2.09906977500005,12.2,-3.39803125200001));
#322983=CARTESIAN_POINT('Ctrl Pts',(-2.09906977500005,5.2,-3.39803125200001));
#322984=CARTESIAN_POINT('Ctrl Pts',(-2.09906977500005,2.2,-3.39803125200001));
#322985=CARTESIAN_POINT('Ctrl Pts',(-2.09903090200006,12.2,-3.39797016400002));
#322986=CARTESIAN_POINT('Ctrl Pts',(-2.09903090200006,5.2,-3.39797016400002));
#322987=CARTESIAN_POINT('Ctrl Pts',(-2.09903090200006,2.2,-3.39797016400002));
#322988=CARTESIAN_POINT('Ctrl Pts',(-2.09899603200005,12.2,-3.39791522200001));
#322989=CARTESIAN_POINT('Ctrl Pts',(-2.09899603200005,5.2,-3.39791522200001));
#322990=CARTESIAN_POINT('Ctrl Pts',(-2.09899603200005,2.2,-3.39791522200001));
#322991=CARTESIAN_POINT('Ctrl Pts',(-2.09896516000006,12.2,-3.39786644800002));
#322992=CARTESIAN_POINT('Ctrl Pts',(-2.09896516000006,5.2,-3.39786644800002));
#322993=CARTESIAN_POINT('Ctrl Pts',(-2.09896516000006,2.2,-3.39786644800002));
#322994=CARTESIAN_POINT('Ctrl Pts',(-2.0989354047251,12.2,-3.39781929544304));
#322995=CARTESIAN_POINT('Ctrl Pts',(-2.0989354047251,5.2,-3.39781929544304));
#322996=CARTESIAN_POINT('Ctrl Pts',(-2.0989354047251,2.2,-3.39781929544304));
#322997=CARTESIAN_POINT('Ctrl Pts',(-2.0989151302594,12.2,-3.39778702279926));
#322998=CARTESIAN_POINT('Ctrl Pts',(-2.0989151302594,5.2,-3.39778702279926));
#322999=CARTESIAN_POINT('Ctrl Pts',(-2.0989151302594,2.2,-3.39778702279926));
#323000=CARTESIAN_POINT('Ctrl Pts',(-2.09890181977372,12.2,-3.39776573310334));
#323001=CARTESIAN_POINT('Ctrl Pts',(-2.09890181977372,5.2,-3.39776573310334));
#323002=CARTESIAN_POINT('Ctrl Pts',(-2.09890181977372,2.2,-3.39776573310334));
#323003=CARTESIAN_POINT('Ctrl Pts',(-2.09889355742141,12.2,-3.39775245437597));
#323004=CARTESIAN_POINT('Ctrl Pts',(-2.09889355742141,5.2,-3.39775245437597));
#323005=CARTESIAN_POINT('Ctrl Pts',(-2.09889355742141,2.2,-3.39775245437597));
#323006=CARTESIAN_POINT('Ctrl Pts',(-2.09888845200005,12.2,-3.39774425600002));
#323007=CARTESIAN_POINT('Ctrl Pts',(-2.09888845200005,5.2,-3.39774425600002));
#323008=CARTESIAN_POINT('Ctrl Pts',(-2.09888845200005,2.2,-3.39774425600002));
#323009=CARTESIAN_POINT('',(-2.09888828100006,2.7,-3.39774436300001));
#323010=CARTESIAN_POINT('',(-2.09888828100006,12.2,-3.39774436300001));
#323011=CARTESIAN_POINT('Ctrl Pts',(-2.77990780000006,2.7,-3.85157274700001));
#323012=CARTESIAN_POINT('Ctrl Pts',(-2.5607296334765,2.7,-3.76566536820642));
#323013=CARTESIAN_POINT('Ctrl Pts',(-2.39555995610288,2.6999999999955,-3.66650574172274));
#323014=CARTESIAN_POINT('Ctrl Pts',(-2.15514138129518,2.6999999999955,-3.47929284706468));
#323015=CARTESIAN_POINT('Ctrl Pts',(-2.10572616940241,2.7,-3.40841675459135));
#323016=CARTESIAN_POINT('Ctrl Pts',(-2.09906882271441,2.7,-3.39803012695728));
#323017=CARTESIAN_POINT('Ctrl Pts',(-2.09897779197314,2.7,-3.39788771970969));
#323018=CARTESIAN_POINT('Ctrl Pts',(-2.09888845200005,2.7,-3.39774425600002));
#323019=CARTESIAN_POINT('Origin',(-2.09886131100005,15.2,-3.39770070400002));
#323020=CARTESIAN_POINT('',(-1.90509662000005,2.7,-3.08402851200002));
#323021=CARTESIAN_POINT('',(-1.90509662000005,2.2,-3.08402851200002));
#323022=CARTESIAN_POINT('',(-1.04943065555809,2.7,-1.69885035196417));
#323023=CARTESIAN_POINT('Origin',(-5.66300478732629E-14,15.2,-1.77635683940025E-14));
#323024=CARTESIAN_POINT('',(-1.40617553900006,2.7,-3.34115180000001));
#323025=CARTESIAN_POINT('',(-1.40617553900006,12.2,-3.34115180000001));
#323026=CARTESIAN_POINT('Origin',(-5.66300478732629E-14,2.7,-1.92943768261394E-14));
#323027=CARTESIAN_POINT('Origin',(-5.66300478732629E-14,15.2,-1.77635683940025E-14));
#323028=CARTESIAN_POINT('',(-1.54920894300006,2.7,-3.68100717000001));
#323029=CARTESIAN_POINT('',(-1.54920894300006,12.2,-3.68100717000001));
#323030=CARTESIAN_POINT('',(-5.63454419629576E-14,2.7,-1.86181372517296E-14));
#323031=CARTESIAN_POINT('Ctrl Pts',(-1.54920881500006,12.2,-3.68100722400001));
#323032=CARTESIAN_POINT('Ctrl Pts',(-1.54920881500006,5.2,-3.68100722400001));
#323033=CARTESIAN_POINT('Ctrl Pts',(-1.54920881500006,2.2,-3.68100722400001));
#323034=CARTESIAN_POINT('Ctrl Pts',(-1.54921144480716,12.2,-3.68101354053696));
#323035=CARTESIAN_POINT('Ctrl Pts',(-1.54921144480716,5.2,-3.68101354053696));
#323036=CARTESIAN_POINT('Ctrl Pts',(-1.54921144480716,2.2,-3.68101354053696));
#323037=CARTESIAN_POINT('Ctrl Pts',(-1.54921653367158,12.2,-3.6810257569059));
#323038=CARTESIAN_POINT('Ctrl Pts',(-1.54921653367158,5.2,-3.6810257569059));
#323039=CARTESIAN_POINT('Ctrl Pts',(-1.54921653367158,2.2,-3.6810257569059));
#323040=CARTESIAN_POINT('Ctrl Pts',(-1.54922407480527,12.2,-3.68104387907971));
#323041=CARTESIAN_POINT('Ctrl Pts',(-1.54922407480527,5.2,-3.68104387907971));
#323042=CARTESIAN_POINT('Ctrl Pts',(-1.54922407480527,2.2,-3.68104387907971));
#323043=CARTESIAN_POINT('Ctrl Pts',(-1.54923408213771,12.2,-3.68106787202714));
#323044=CARTESIAN_POINT('Ctrl Pts',(-1.54923408213771,5.19999999999999,
-3.68106787202714));
#323045=CARTESIAN_POINT('Ctrl Pts',(-1.54923408213771,2.2,-3.68106787202714));
#323046=CARTESIAN_POINT('Ctrl Pts',(-1.54925130100006,12.2,-3.68110978700001));
#323047=CARTESIAN_POINT('Ctrl Pts',(-1.54925130100006,5.2,-3.68110978700001));
#323048=CARTESIAN_POINT('Ctrl Pts',(-1.54925130100006,2.2,-3.68110978700001));
#323049=CARTESIAN_POINT('Ctrl Pts',(-1.54927039300006,12.2,-3.68115639400001));
#323050=CARTESIAN_POINT('Ctrl Pts',(-1.54927039300006,5.2,-3.68115639400001));
#323051=CARTESIAN_POINT('Ctrl Pts',(-1.54927039300006,2.2,-3.68115639400001));
#323052=CARTESIAN_POINT('Ctrl Pts',(-1.54929219900006,12.2,-3.68120983900001));
#323053=CARTESIAN_POINT('Ctrl Pts',(-1.54929219900006,5.2,-3.68120983900001));
#323054=CARTESIAN_POINT('Ctrl Pts',(-1.54929219900006,2.2,-3.68120983900001));
#323055=CARTESIAN_POINT('Ctrl Pts',(-1.54931671100006,12.2,-3.68127011900001));
#323056=CARTESIAN_POINT('Ctrl Pts',(-1.54931671100006,5.2,-3.68127011900001));
#323057=CARTESIAN_POINT('Ctrl Pts',(-1.54931671100006,2.2,-3.68127011900001));
#323058=CARTESIAN_POINT('Ctrl Pts',(-1.54934390400005,12.2,-3.68133722700001));
#323059=CARTESIAN_POINT('Ctrl Pts',(-1.54934390400005,5.2,-3.68133722700001));
#323060=CARTESIAN_POINT('Ctrl Pts',(-1.54934390400005,2.2,-3.68133722700001));
#323061=CARTESIAN_POINT('Ctrl Pts',(-1.54937375600006,12.2,-3.68141115300002));
#323062=CARTESIAN_POINT('Ctrl Pts',(-1.54937375600006,5.2,-3.68141115300002));
#323063=CARTESIAN_POINT('Ctrl Pts',(-1.54937375600006,2.2,-3.68141115300002));
#323064=CARTESIAN_POINT('Ctrl Pts',(-1.54940623200006,12.2,-3.68149188800002));
#323065=CARTESIAN_POINT('Ctrl Pts',(-1.54940623200006,5.2,-3.68149188800002));
#323066=CARTESIAN_POINT('Ctrl Pts',(-1.54940623200006,2.2,-3.68149188800002));
#323067=CARTESIAN_POINT('Ctrl Pts',(-1.54944130200006,12.2,-3.68157942000002));
#323068=CARTESIAN_POINT('Ctrl Pts',(-1.54944130200006,5.2,-3.68157942000002));
#323069=CARTESIAN_POINT('Ctrl Pts',(-1.54944130200006,2.2,-3.68157942000002));
#323070=CARTESIAN_POINT('Ctrl Pts',(-1.54947893900005,12.2,-3.68167374100001));
#323071=CARTESIAN_POINT('Ctrl Pts',(-1.54947893900005,5.2,-3.68167374100001));
#323072=CARTESIAN_POINT('Ctrl Pts',(-1.54947893900005,2.2,-3.68167374100001));
#323073=CARTESIAN_POINT('Ctrl Pts',(-1.54951911600006,12.2,-3.68177484000002));
#323074=CARTESIAN_POINT('Ctrl Pts',(-1.54951911600006,5.2,-3.68177484000002));
#323075=CARTESIAN_POINT('Ctrl Pts',(-1.54951911600006,2.2,-3.68177484000002));
#323076=CARTESIAN_POINT('Ctrl Pts',(-1.54956181300005,12.2,-3.68188271100002));
#323077=CARTESIAN_POINT('Ctrl Pts',(-1.54956181300005,5.2,-3.68188271100002));
#323078=CARTESIAN_POINT('Ctrl Pts',(-1.54956181300005,2.2,-3.68188271100002));
#323079=CARTESIAN_POINT('Ctrl Pts',(-1.54960700900005,12.2,-3.68199734600001));
#323080=CARTESIAN_POINT('Ctrl Pts',(-1.54960700900005,5.2,-3.68199734600001));
#323081=CARTESIAN_POINT('Ctrl Pts',(-1.54960700900005,2.2,-3.68199734600001));
#323082=CARTESIAN_POINT('Ctrl Pts',(-1.54965467900006,12.2,-3.68211873800002));
#323083=CARTESIAN_POINT('Ctrl Pts',(-1.54965467900006,5.2,-3.68211873800002));
#323084=CARTESIAN_POINT('Ctrl Pts',(-1.54965467900006,2.2,-3.68211873800002));
#323085=CARTESIAN_POINT('Ctrl Pts',(-1.54970480200005,12.2,-3.68224687900002));
#323086=CARTESIAN_POINT('Ctrl Pts',(-1.54970480200005,5.2,-3.68224687900002));
#323087=CARTESIAN_POINT('Ctrl Pts',(-1.54970480200005,2.2,-3.68224687900002));
#323088=CARTESIAN_POINT('Ctrl Pts',(-1.54975735300006,12.2,-3.68238175900002));
#323089=CARTESIAN_POINT('Ctrl Pts',(-1.54975735300006,5.2,-3.68238175900002));
#323090=CARTESIAN_POINT('Ctrl Pts',(-1.54975735300006,2.2,-3.68238175900002));
#323091=CARTESIAN_POINT('Ctrl Pts',(-1.54981230700006,12.2,-3.68252337000001));
#323092=CARTESIAN_POINT('Ctrl Pts',(-1.54981230700006,5.2,-3.68252337000001));
#323093=CARTESIAN_POINT('Ctrl Pts',(-1.54981230700006,2.2,-3.68252337000001));
#323094=CARTESIAN_POINT('Ctrl Pts',(-1.54986963900006,12.2,-3.68267170500001));
#323095=CARTESIAN_POINT('Ctrl Pts',(-1.54986963900006,5.2,-3.68267170500001));
#323096=CARTESIAN_POINT('Ctrl Pts',(-1.54986963900006,2.2,-3.68267170500001));
#323097=CARTESIAN_POINT('Ctrl Pts',(-1.54992932600006,12.2,-3.68282675200001));
#323098=CARTESIAN_POINT('Ctrl Pts',(-1.54992932600006,5.2,-3.68282675200001));
#323099=CARTESIAN_POINT('Ctrl Pts',(-1.54992932600006,2.2,-3.68282675200001));
#323100=CARTESIAN_POINT('Ctrl Pts',(-1.54999134300006,12.2,-3.68298850500001));
#323101=CARTESIAN_POINT('Ctrl Pts',(-1.54999134300006,5.2,-3.68298850500001));
#323102=CARTESIAN_POINT('Ctrl Pts',(-1.54999134300006,2.2,-3.68298850500001));
#323103=CARTESIAN_POINT('Ctrl Pts',(-1.55005566800006,12.2,-3.68315695700002));
#323104=CARTESIAN_POINT('Ctrl Pts',(-1.55005566800006,5.2,-3.68315695700002));
#323105=CARTESIAN_POINT('Ctrl Pts',(-1.55005566800006,2.2,-3.68315695700002));
#323106=CARTESIAN_POINT('Ctrl Pts',(-1.55012227800006,12.2,-3.68333209600001));
#323107=CARTESIAN_POINT('Ctrl Pts',(-1.55012227800006,5.2,-3.68333209600001));
#323108=CARTESIAN_POINT('Ctrl Pts',(-1.55012227800006,2.2,-3.68333209600001));
#323109=CARTESIAN_POINT('Ctrl Pts',(-1.55019114900006,12.2,-3.68351391700001));
#323110=CARTESIAN_POINT('Ctrl Pts',(-1.55019114900006,5.2,-3.68351391700001));
#323111=CARTESIAN_POINT('Ctrl Pts',(-1.55019114900006,2.2,-3.68351391700001));
#323112=CARTESIAN_POINT('Ctrl Pts',(-1.55026226000006,12.2,-3.68370241000001));
#323113=CARTESIAN_POINT('Ctrl Pts',(-1.55026226000006,5.2,-3.68370241000001));
#323114=CARTESIAN_POINT('Ctrl Pts',(-1.55026226000006,2.2,-3.68370241000001));
#323115=CARTESIAN_POINT('Ctrl Pts',(-1.55033558600006,12.2,-3.68389756800001));
#323116=CARTESIAN_POINT('Ctrl Pts',(-1.55033558600006,5.2,-3.68389756800001));
#323117=CARTESIAN_POINT('Ctrl Pts',(-1.55033558600006,2.2,-3.68389756800001));
#323118=CARTESIAN_POINT('Ctrl Pts',(-1.55041110500005,12.2,-3.68409938100001));
#323119=CARTESIAN_POINT('Ctrl Pts',(-1.55041110500005,5.2,-3.68409938100001));
#323120=CARTESIAN_POINT('Ctrl Pts',(-1.55041110500005,2.2,-3.68409938100001));
#323121=CARTESIAN_POINT('Ctrl Pts',(-1.55048879300006,12.2,-3.68430784300001));
#323122=CARTESIAN_POINT('Ctrl Pts',(-1.55048879300006,5.2,-3.68430784300001));
#323123=CARTESIAN_POINT('Ctrl Pts',(-1.55048879300006,2.2,-3.68430784300001));
#323124=CARTESIAN_POINT('Ctrl Pts',(-1.55056862800006,12.2,-3.68452294300001));
#323125=CARTESIAN_POINT('Ctrl Pts',(-1.55056862800006,5.2,-3.68452294300001));
#323126=CARTESIAN_POINT('Ctrl Pts',(-1.55056862800006,2.2,-3.68452294300001));
#323127=CARTESIAN_POINT('Ctrl Pts',(-1.55065058700006,12.2,-3.68474467500001));
#323128=CARTESIAN_POINT('Ctrl Pts',(-1.55065058700006,5.2,-3.68474467500001));
#323129=CARTESIAN_POINT('Ctrl Pts',(-1.55065058700006,2.2,-3.68474467500001));
#323130=CARTESIAN_POINT('Ctrl Pts',(-1.55073464700005,12.2,-3.68497302900002));
#323131=CARTESIAN_POINT('Ctrl Pts',(-1.55073464700005,5.2,-3.68497302900002));
#323132=CARTESIAN_POINT('Ctrl Pts',(-1.55073464700005,2.2,-3.68497302900002));
#323133=CARTESIAN_POINT('Ctrl Pts',(-1.55082078700006,12.2,-3.68520799800002));
#323134=CARTESIAN_POINT('Ctrl Pts',(-1.55082078700006,5.2,-3.68520799800002));
#323135=CARTESIAN_POINT('Ctrl Pts',(-1.55082078700006,2.2,-3.68520799800002));
#323136=CARTESIAN_POINT('Ctrl Pts',(-1.55090898200006,12.2,-3.68544957200001));
#323137=CARTESIAN_POINT('Ctrl Pts',(-1.55090898200006,5.2,-3.68544957200001));
#323138=CARTESIAN_POINT('Ctrl Pts',(-1.55090898200006,2.2,-3.68544957200001));
#323139=CARTESIAN_POINT('Ctrl Pts',(-1.55099921200006,12.2,-3.68569774400001));
#323140=CARTESIAN_POINT('Ctrl Pts',(-1.55099921200006,5.2,-3.68569774400001));
#323141=CARTESIAN_POINT('Ctrl Pts',(-1.55099921200006,2.2,-3.68569774400001));
#323142=CARTESIAN_POINT('Ctrl Pts',(-1.55109145400006,12.2,-3.68595250600002));
#323143=CARTESIAN_POINT('Ctrl Pts',(-1.55109145400006,5.2,-3.68595250600002));
#323144=CARTESIAN_POINT('Ctrl Pts',(-1.55109145400006,2.2,-3.68595250600002));
#323145=CARTESIAN_POINT('Ctrl Pts',(-1.55118568700006,12.2,-3.68621384800001));
#323146=CARTESIAN_POINT('Ctrl Pts',(-1.55118568700006,5.2,-3.68621384800001));
#323147=CARTESIAN_POINT('Ctrl Pts',(-1.55118568700006,2.2,-3.68621384800001));
#323148=CARTESIAN_POINT('Ctrl Pts',(-1.55128188600006,12.2,-3.68648176300002));
#323149=CARTESIAN_POINT('Ctrl Pts',(-1.55128188600006,5.2,-3.68648176300002));
#323150=CARTESIAN_POINT('Ctrl Pts',(-1.55128188600006,2.2,-3.68648176300002));
#323151=CARTESIAN_POINT('Ctrl Pts',(-1.55138003100005,12.2,-3.68675624400002));
#323152=CARTESIAN_POINT('Ctrl Pts',(-1.55138003100005,5.2,-3.68675624400002));
#323153=CARTESIAN_POINT('Ctrl Pts',(-1.55138003100005,2.2,-3.68675624400002));
#323154=CARTESIAN_POINT('Ctrl Pts',(-1.55148010000006,12.2,-3.68703728000002));
#323155=CARTESIAN_POINT('Ctrl Pts',(-1.55148010000006,5.2,-3.68703728000002));
#323156=CARTESIAN_POINT('Ctrl Pts',(-1.55148010000006,2.2,-3.68703728000002));
#323157=CARTESIAN_POINT('Ctrl Pts',(-1.55158207100006,12.2,-3.68732486500001));
#323158=CARTESIAN_POINT('Ctrl Pts',(-1.55158207100006,5.2,-3.68732486500001));
#323159=CARTESIAN_POINT('Ctrl Pts',(-1.55158207100006,2.2,-3.68732486500001));
#323160=CARTESIAN_POINT('Ctrl Pts',(-1.55168592200006,12.2,-3.68761899000001));
#323161=CARTESIAN_POINT('Ctrl Pts',(-1.55168592200006,5.2,-3.68761899000001));
#323162=CARTESIAN_POINT('Ctrl Pts',(-1.55168592200006,2.2,-3.68761899000001));
#323163=CARTESIAN_POINT('Ctrl Pts',(-1.55179163200006,12.2,-3.68791964500002));
#323164=CARTESIAN_POINT('Ctrl Pts',(-1.55179163200006,5.2,-3.68791964500002));
#323165=CARTESIAN_POINT('Ctrl Pts',(-1.55179163200006,2.2,-3.68791964500002));
#323166=CARTESIAN_POINT('Ctrl Pts',(-1.55189917800006,12.2,-3.68822682500001));
#323167=CARTESIAN_POINT('Ctrl Pts',(-1.55189917800006,5.2,-3.68822682500001));
#323168=CARTESIAN_POINT('Ctrl Pts',(-1.55189917800006,2.2,-3.68822682500001));
#323169=CARTESIAN_POINT('Ctrl Pts',(-1.55200854000005,12.2,-3.68854051900001));
#323170=CARTESIAN_POINT('Ctrl Pts',(-1.55200854000005,5.2,-3.68854051900001));
#323171=CARTESIAN_POINT('Ctrl Pts',(-1.55200854000005,2.2,-3.68854051900001));
#323172=CARTESIAN_POINT('Ctrl Pts',(-1.55211969500006,12.2,-3.68886072000001));
#323173=CARTESIAN_POINT('Ctrl Pts',(-1.55211969500006,5.2,-3.68886072000001));
#323174=CARTESIAN_POINT('Ctrl Pts',(-1.55211969500006,2.2,-3.68886072000001));
#323175=CARTESIAN_POINT('Ctrl Pts',(-1.55223262400006,12.2,-3.68918742000002));
#323176=CARTESIAN_POINT('Ctrl Pts',(-1.55223262400006,5.2,-3.68918742000002));
#323177=CARTESIAN_POINT('Ctrl Pts',(-1.55223262400006,2.2,-3.68918742000002));
#323178=CARTESIAN_POINT('Ctrl Pts',(-1.55234730400006,12.2,-3.68952060900002));
#323179=CARTESIAN_POINT('Ctrl Pts',(-1.55234730400006,5.2,-3.68952060900002));
#323180=CARTESIAN_POINT('Ctrl Pts',(-1.55234730400006,2.2,-3.68952060900002));
#323181=CARTESIAN_POINT('Ctrl Pts',(-1.55246371400006,12.2,-3.68986028200001));
#323182=CARTESIAN_POINT('Ctrl Pts',(-1.55246371400006,5.2,-3.68986028200001));
#323183=CARTESIAN_POINT('Ctrl Pts',(-1.55246371400006,2.2,-3.68986028200001));
#323184=CARTESIAN_POINT('Ctrl Pts',(-1.55258183200006,12.2,-3.69020642700002));
#323185=CARTESIAN_POINT('Ctrl Pts',(-1.55258183200006,5.2,-3.69020642700002));
#323186=CARTESIAN_POINT('Ctrl Pts',(-1.55258183200006,2.2,-3.69020642700002));
#323187=CARTESIAN_POINT('Ctrl Pts',(-1.55270163900005,12.2,-3.69055903800001));
#323188=CARTESIAN_POINT('Ctrl Pts',(-1.55270163900005,5.2,-3.69055903800001));
#323189=CARTESIAN_POINT('Ctrl Pts',(-1.55270163900005,2.2,-3.69055903800001));
#323190=CARTESIAN_POINT('Ctrl Pts',(-1.55282311500006,12.2,-3.69091810700001));
#323191=CARTESIAN_POINT('Ctrl Pts',(-1.55282311500006,5.2,-3.69091810700001));
#323192=CARTESIAN_POINT('Ctrl Pts',(-1.55282311500006,2.2,-3.69091810700001));
#323193=CARTESIAN_POINT('Ctrl Pts',(-1.55294623500006,12.2,-3.69128362500001));
#323194=CARTESIAN_POINT('Ctrl Pts',(-1.55294623500006,5.2,-3.69128362500001));
#323195=CARTESIAN_POINT('Ctrl Pts',(-1.55294623500006,2.2,-3.69128362500001));
#323196=CARTESIAN_POINT('Ctrl Pts',(-1.55307098100006,12.2,-3.69165558300002));
#323197=CARTESIAN_POINT('Ctrl Pts',(-1.55307098100006,5.2,-3.69165558300002));
#323198=CARTESIAN_POINT('Ctrl Pts',(-1.55307098100006,2.2,-3.69165558300002));
#323199=CARTESIAN_POINT('Ctrl Pts',(-1.55319733200006,12.2,-3.69203397300002));
#323200=CARTESIAN_POINT('Ctrl Pts',(-1.55319733200006,5.2,-3.69203397300002));
#323201=CARTESIAN_POINT('Ctrl Pts',(-1.55319733200006,2.2,-3.69203397300002));
#323202=CARTESIAN_POINT('Ctrl Pts',(-1.55332526700006,12.2,-3.69241878900001));
#323203=CARTESIAN_POINT('Ctrl Pts',(-1.55332526700006,5.2,-3.69241878900001));
#323204=CARTESIAN_POINT('Ctrl Pts',(-1.55332526700006,2.2,-3.69241878900001));
#323205=CARTESIAN_POINT('Ctrl Pts',(-1.55345476600006,12.2,-3.69281002200001));
#323206=CARTESIAN_POINT('Ctrl Pts',(-1.55345476600006,5.2,-3.69281002200001));
#323207=CARTESIAN_POINT('Ctrl Pts',(-1.55345476600006,2.2,-3.69281002200001));
#323208=CARTESIAN_POINT('Ctrl Pts',(-1.55358580700006,12.2,-3.69320766100001));
#323209=CARTESIAN_POINT('Ctrl Pts',(-1.55358580700006,5.2,-3.69320766100001));
#323210=CARTESIAN_POINT('Ctrl Pts',(-1.55358580700006,2.2,-3.69320766100001));
#323211=CARTESIAN_POINT('Ctrl Pts',(-1.55371837200006,12.2,-3.69361170100001));
#323212=CARTESIAN_POINT('Ctrl Pts',(-1.55371837200006,5.2,-3.69361170100001));
#323213=CARTESIAN_POINT('Ctrl Pts',(-1.55371837200006,2.2,-3.69361170100001));
#323214=CARTESIAN_POINT('Ctrl Pts',(-1.55385243800006,12.2,-3.69402213200001));
#323215=CARTESIAN_POINT('Ctrl Pts',(-1.55385243800006,5.2,-3.69402213200001));
#323216=CARTESIAN_POINT('Ctrl Pts',(-1.55385243800006,2.2,-3.69402213200001));
#323217=CARTESIAN_POINT('Ctrl Pts',(-1.55398798700006,12.2,-3.69443894600002));
#323218=CARTESIAN_POINT('Ctrl Pts',(-1.55398798700006,5.2,-3.69443894600002));
#323219=CARTESIAN_POINT('Ctrl Pts',(-1.55398798700006,2.2,-3.69443894600002));
#323220=CARTESIAN_POINT('Ctrl Pts',(-1.55412499800006,12.2,-3.69486213600001));
#323221=CARTESIAN_POINT('Ctrl Pts',(-1.55412499800006,5.2,-3.69486213600001));
#323222=CARTESIAN_POINT('Ctrl Pts',(-1.55412499800006,2.2,-3.69486213600001));
#323223=CARTESIAN_POINT('Ctrl Pts',(-1.55426345100006,12.2,-3.69529169300002));
#323224=CARTESIAN_POINT('Ctrl Pts',(-1.55426345100006,5.2,-3.69529169300002));
#323225=CARTESIAN_POINT('Ctrl Pts',(-1.55426345100006,2.2,-3.69529169300002));
#323226=CARTESIAN_POINT('Ctrl Pts',(-1.55440332500006,12.2,-3.69572760900001));
#323227=CARTESIAN_POINT('Ctrl Pts',(-1.55440332500006,5.2,-3.69572760900001));
#323228=CARTESIAN_POINT('Ctrl Pts',(-1.55440332500006,2.2,-3.69572760900001));
#323229=CARTESIAN_POINT('Ctrl Pts',(-1.55454460100006,12.2,-3.69616987500001));
#323230=CARTESIAN_POINT('Ctrl Pts',(-1.55454460100006,5.2,-3.69616987500001));
#323231=CARTESIAN_POINT('Ctrl Pts',(-1.55454460100006,2.2,-3.69616987500001));
#323232=CARTESIAN_POINT('Ctrl Pts',(-1.55468726000006,12.2,-3.69661848400002));
#323233=CARTESIAN_POINT('Ctrl Pts',(-1.55468726000006,5.2,-3.69661848400002));
#323234=CARTESIAN_POINT('Ctrl Pts',(-1.55468726000006,2.2,-3.69661848400002));
#323235=CARTESIAN_POINT('Ctrl Pts',(-1.55483128000005,12.2,-3.69707342600002));
#323236=CARTESIAN_POINT('Ctrl Pts',(-1.55483128000005,5.2,-3.69707342600002));
#323237=CARTESIAN_POINT('Ctrl Pts',(-1.55483128000005,2.2,-3.69707342600002));
#323238=CARTESIAN_POINT('Ctrl Pts',(-1.55497664300006,12.2,-3.69753469500001));
#323239=CARTESIAN_POINT('Ctrl Pts',(-1.55497664300006,5.2,-3.69753469500001));
#323240=CARTESIAN_POINT('Ctrl Pts',(-1.55497664300006,2.2,-3.69753469500001));
#323241=CARTESIAN_POINT('Ctrl Pts',(-1.55512332800006,12.2,-3.69800228200001));
#323242=CARTESIAN_POINT('Ctrl Pts',(-1.55512332800006,5.2,-3.69800228200001));
#323243=CARTESIAN_POINT('Ctrl Pts',(-1.55512332800006,2.2,-3.69800228200001));
#323244=CARTESIAN_POINT('Ctrl Pts',(-1.55527131700006,12.2,-3.69847617800001));
#323245=CARTESIAN_POINT('Ctrl Pts',(-1.55527131700006,5.2,-3.69847617800001));
#323246=CARTESIAN_POINT('Ctrl Pts',(-1.55527131700006,2.2,-3.69847617800001));
#323247=CARTESIAN_POINT('Ctrl Pts',(-1.55542058900005,12.2,-3.69895637600001));
#323248=CARTESIAN_POINT('Ctrl Pts',(-1.55542058900005,5.2,-3.69895637600001));
#323249=CARTESIAN_POINT('Ctrl Pts',(-1.55542058900005,2.2,-3.69895637600001));
#323250=CARTESIAN_POINT('Ctrl Pts',(-1.55557112500006,12.2,-3.69944286800001));
#323251=CARTESIAN_POINT('Ctrl Pts',(-1.55557112500006,5.2,-3.69944286800001));
#323252=CARTESIAN_POINT('Ctrl Pts',(-1.55557112500006,2.2,-3.69944286800001));
#323253=CARTESIAN_POINT('Ctrl Pts',(-1.55572290600006,12.2,-3.69993564400001));
#323254=CARTESIAN_POINT('Ctrl Pts',(-1.55572290600006,5.2,-3.69993564400001));
#323255=CARTESIAN_POINT('Ctrl Pts',(-1.55572290600006,2.2,-3.69993564400001));
#323256=CARTESIAN_POINT('Ctrl Pts',(-1.55587591300006,12.2,-3.70043469700001));
#323257=CARTESIAN_POINT('Ctrl Pts',(-1.55587591300006,5.2,-3.70043469700001));
#323258=CARTESIAN_POINT('Ctrl Pts',(-1.55587591300006,2.2,-3.70043469700001));
#323259=CARTESIAN_POINT('Ctrl Pts',(-1.55603012600006,12.2,-3.70094001900001));
#323260=CARTESIAN_POINT('Ctrl Pts',(-1.55603012600006,5.2,-3.70094001900001));
#323261=CARTESIAN_POINT('Ctrl Pts',(-1.55603012600006,2.2,-3.70094001900001));
#323262=CARTESIAN_POINT('Ctrl Pts',(-1.55618552500006,12.2,-3.70145160200002));
#323263=CARTESIAN_POINT('Ctrl Pts',(-1.55618552500006,5.2,-3.70145160200002));
#323264=CARTESIAN_POINT('Ctrl Pts',(-1.55618552500006,2.2,-3.70145160200002));
#323265=CARTESIAN_POINT('Ctrl Pts',(-1.55634209300006,12.2,-3.70196943800002));
#323266=CARTESIAN_POINT('Ctrl Pts',(-1.55634209300006,5.2,-3.70196943800002));
#323267=CARTESIAN_POINT('Ctrl Pts',(-1.55634209300006,2.2,-3.70196943800002));
#323268=CARTESIAN_POINT('Ctrl Pts',(-1.55649981000006,12.2,-3.70249351700001));
#323269=CARTESIAN_POINT('Ctrl Pts',(-1.55649981000006,5.2,-3.70249351700001));
#323270=CARTESIAN_POINT('Ctrl Pts',(-1.55649981000006,2.2,-3.70249351700001));
#323271=CARTESIAN_POINT('Ctrl Pts',(-1.55665865600006,12.2,-3.70302383400002));
#323272=CARTESIAN_POINT('Ctrl Pts',(-1.55665865600006,5.2,-3.70302383400002));
#323273=CARTESIAN_POINT('Ctrl Pts',(-1.55665865600006,2.2,-3.70302383400002));
#323274=CARTESIAN_POINT('Ctrl Pts',(-1.55681861300006,12.2,-3.70356037800001));
#323275=CARTESIAN_POINT('Ctrl Pts',(-1.55681861300006,5.2,-3.70356037800001));
#323276=CARTESIAN_POINT('Ctrl Pts',(-1.55681861300006,2.2,-3.70356037800001));
#323277=CARTESIAN_POINT('Ctrl Pts',(-1.55697966300006,12.2,-3.70410314200001));
#323278=CARTESIAN_POINT('Ctrl Pts',(-1.55697966300006,5.2,-3.70410314200001));
#323279=CARTESIAN_POINT('Ctrl Pts',(-1.55697966300006,2.2,-3.70410314200001));
#323280=CARTESIAN_POINT('Ctrl Pts',(-1.55714178500005,12.2,-3.70465211700001));
#323281=CARTESIAN_POINT('Ctrl Pts',(-1.55714178500005,5.2,-3.70465211700001));
#323282=CARTESIAN_POINT('Ctrl Pts',(-1.55714178500005,2.2,-3.70465211700001));
#323283=CARTESIAN_POINT('Ctrl Pts',(-1.55730496200006,12.2,-3.70520729600001));
#323284=CARTESIAN_POINT('Ctrl Pts',(-1.55730496200006,5.2,-3.70520729600001));
#323285=CARTESIAN_POINT('Ctrl Pts',(-1.55730496200006,2.2,-3.70520729600001));
#323286=CARTESIAN_POINT('Ctrl Pts',(-1.55746917600006,12.2,-3.70576867200001));
#323287=CARTESIAN_POINT('Ctrl Pts',(-1.55746917600006,5.2,-3.70576867200001));
#323288=CARTESIAN_POINT('Ctrl Pts',(-1.55746917600006,2.2,-3.70576867200001));
#323289=CARTESIAN_POINT('Ctrl Pts',(-1.55763440700006,12.2,-3.70633623300002));
#323290=CARTESIAN_POINT('Ctrl Pts',(-1.55763440700006,5.2,-3.70633623300002));
#323291=CARTESIAN_POINT('Ctrl Pts',(-1.55763440700006,2.2,-3.70633623300002));
#323292=CARTESIAN_POINT('Ctrl Pts',(-1.55780063700006,12.2,-3.70690997500001));
#323293=CARTESIAN_POINT('Ctrl Pts',(-1.55780063700006,5.2,-3.70690997500001));
#323294=CARTESIAN_POINT('Ctrl Pts',(-1.55780063700006,2.2,-3.70690997500001));
#323295=CARTESIAN_POINT('Ctrl Pts',(-1.55796784700006,12.2,-3.70748988700001));
#323296=CARTESIAN_POINT('Ctrl Pts',(-1.55796784700006,5.2,-3.70748988700001));
#323297=CARTESIAN_POINT('Ctrl Pts',(-1.55796784700006,2.2,-3.70748988700001));
#323298=CARTESIAN_POINT('Ctrl Pts',(-1.55813601900005,12.2,-3.70807596300001));
#323299=CARTESIAN_POINT('Ctrl Pts',(-1.55813601900005,5.2,-3.70807596300001));
#323300=CARTESIAN_POINT('Ctrl Pts',(-1.55813601900005,2.2,-3.70807596300001));
#323301=CARTESIAN_POINT('Ctrl Pts',(-1.55830513500006,12.2,-3.70866819300002));
#323302=CARTESIAN_POINT('Ctrl Pts',(-1.55830513500006,5.2,-3.70866819300002));
#323303=CARTESIAN_POINT('Ctrl Pts',(-1.55830513500006,2.2,-3.70866819300002));
#323304=CARTESIAN_POINT('Ctrl Pts',(-1.55847517600006,12.2,-3.70926657000001));
#323305=CARTESIAN_POINT('Ctrl Pts',(-1.55847517600006,5.2,-3.70926657000001));
#323306=CARTESIAN_POINT('Ctrl Pts',(-1.55847517600006,2.2,-3.70926657000001));
#323307=CARTESIAN_POINT('Ctrl Pts',(-1.55864612500005,12.2,-3.70987108600001));
#323308=CARTESIAN_POINT('Ctrl Pts',(-1.55864612500005,5.2,-3.70987108600001));
#323309=CARTESIAN_POINT('Ctrl Pts',(-1.55864612500005,2.2,-3.70987108600001));
#323310=CARTESIAN_POINT('Ctrl Pts',(-1.55881796400006,12.2,-3.71048173200001));
#323311=CARTESIAN_POINT('Ctrl Pts',(-1.55881796400006,5.2,-3.71048173200001));
#323312=CARTESIAN_POINT('Ctrl Pts',(-1.55881796400006,2.2,-3.71048173200001));
#323313=CARTESIAN_POINT('Ctrl Pts',(-1.55899067400005,12.2,-3.71109850100002));
#323314=CARTESIAN_POINT('Ctrl Pts',(-1.55899067400005,5.2,-3.71109850100002));
#323315=CARTESIAN_POINT('Ctrl Pts',(-1.55899067400005,2.2,-3.71109850100002));
#323316=CARTESIAN_POINT('Ctrl Pts',(-1.55916423600006,12.2,-3.71172138300001));
#323317=CARTESIAN_POINT('Ctrl Pts',(-1.55916423600006,5.2,-3.71172138300001));
#323318=CARTESIAN_POINT('Ctrl Pts',(-1.55916423600006,2.2,-3.71172138300001));
#323319=CARTESIAN_POINT('Ctrl Pts',(-1.55933863300006,12.2,-3.71235037100002));
#323320=CARTESIAN_POINT('Ctrl Pts',(-1.55933863300006,5.2,-3.71235037100002));
#323321=CARTESIAN_POINT('Ctrl Pts',(-1.55933863300006,2.2,-3.71235037100002));
#323322=CARTESIAN_POINT('Ctrl Pts',(-1.55951384900006,12.2,-3.71298545800002));
#323323=CARTESIAN_POINT('Ctrl Pts',(-1.55951384900006,5.2,-3.71298545800002));
#323324=CARTESIAN_POINT('Ctrl Pts',(-1.55951384900006,2.2,-3.71298545800002));
#323325=CARTESIAN_POINT('Ctrl Pts',(-1.55968986300006,12.2,-3.71362663500001));
#323326=CARTESIAN_POINT('Ctrl Pts',(-1.55968986300006,5.2,-3.71362663500001));
#323327=CARTESIAN_POINT('Ctrl Pts',(-1.55968986300006,2.2,-3.71362663500001));
#323328=CARTESIAN_POINT('Ctrl Pts',(-1.55986666000006,12.2,-3.71427389300001));
#323329=CARTESIAN_POINT('Ctrl Pts',(-1.55986666000006,5.2,-3.71427389300001));
#323330=CARTESIAN_POINT('Ctrl Pts',(-1.55986666000006,2.2,-3.71427389300001));
#323331=CARTESIAN_POINT('Ctrl Pts',(-1.56004422000006,12.2,-3.71492722500002));
#323332=CARTESIAN_POINT('Ctrl Pts',(-1.56004422000006,5.2,-3.71492722500002));
#323333=CARTESIAN_POINT('Ctrl Pts',(-1.56004422000006,2.2,-3.71492722500002));
#323334=CARTESIAN_POINT('Ctrl Pts',(-1.56022252800006,12.2,-3.71558662200002));
#323335=CARTESIAN_POINT('Ctrl Pts',(-1.56022252800006,5.2,-3.71558662200002));
#323336=CARTESIAN_POINT('Ctrl Pts',(-1.56022252800006,2.2,-3.71558662200002));
#323337=CARTESIAN_POINT('Ctrl Pts',(-1.56040156400006,12.2,-3.71625207700002));
#323338=CARTESIAN_POINT('Ctrl Pts',(-1.56040156400006,5.2,-3.71625207700002));
#323339=CARTESIAN_POINT('Ctrl Pts',(-1.56040156400006,2.2,-3.71625207700002));
#323340=CARTESIAN_POINT('Ctrl Pts',(-1.56058131100006,12.2,-3.71692358100002));
#323341=CARTESIAN_POINT('Ctrl Pts',(-1.56058131100006,5.2,-3.71692358100002));
#323342=CARTESIAN_POINT('Ctrl Pts',(-1.56058131100006,2.2,-3.71692358100002));
#323343=CARTESIAN_POINT('Ctrl Pts',(-1.56076175300006,12.2,-3.71760112700001));
#323344=CARTESIAN_POINT('Ctrl Pts',(-1.56076175300006,5.2,-3.71760112700001));
#323345=CARTESIAN_POINT('Ctrl Pts',(-1.56076175300006,2.2,-3.71760112700001));
#323346=CARTESIAN_POINT('Ctrl Pts',(-1.56094287100006,12.2,-3.71828470600001));
#323347=CARTESIAN_POINT('Ctrl Pts',(-1.56094287100006,5.2,-3.71828470600001));
#323348=CARTESIAN_POINT('Ctrl Pts',(-1.56094287100006,2.2,-3.71828470600001));
#323349=CARTESIAN_POINT('Ctrl Pts',(-1.56112464800006,12.2,-3.71897431000002));
#323350=CARTESIAN_POINT('Ctrl Pts',(-1.56112464800006,5.2,-3.71897431000002));
#323351=CARTESIAN_POINT('Ctrl Pts',(-1.56112464800006,2.2,-3.71897431000002));
#323352=CARTESIAN_POINT('Ctrl Pts',(-1.56130706700006,12.2,-3.71966993000001));
#323353=CARTESIAN_POINT('Ctrl Pts',(-1.56130706700006,5.2,-3.71966993000001));
#323354=CARTESIAN_POINT('Ctrl Pts',(-1.56130706700006,2.2,-3.71966993000001));
#323355=CARTESIAN_POINT('Ctrl Pts',(-1.56149011100006,12.2,-3.72037156100001));
#323356=CARTESIAN_POINT('Ctrl Pts',(-1.56149011100006,5.2,-3.72037156100001));
#323357=CARTESIAN_POINT('Ctrl Pts',(-1.56149011100006,2.2,-3.72037156100001));
#323358=CARTESIAN_POINT('Ctrl Pts',(-1.56167376300006,12.2,-3.72107919100001));
#323359=CARTESIAN_POINT('Ctrl Pts',(-1.56167376300006,5.2,-3.72107919100001));
#323360=CARTESIAN_POINT('Ctrl Pts',(-1.56167376300006,2.2,-3.72107919100001));
#323361=CARTESIAN_POINT('Ctrl Pts',(-1.56185800400006,12.2,-3.72179281400001));
#323362=CARTESIAN_POINT('Ctrl Pts',(-1.56185800400006,5.2,-3.72179281400001));
#323363=CARTESIAN_POINT('Ctrl Pts',(-1.56185800400006,2.2,-3.72179281400001));
#323364=CARTESIAN_POINT('Ctrl Pts',(-1.56204282100005,12.2,-3.72251242200001));
#323365=CARTESIAN_POINT('Ctrl Pts',(-1.56204282100005,5.2,-3.72251242200001));
#323366=CARTESIAN_POINT('Ctrl Pts',(-1.56204282100005,2.2,-3.72251242200001));
#323367=CARTESIAN_POINT('Ctrl Pts',(-1.56222819300006,12.2,-3.72323800600002));
#323368=CARTESIAN_POINT('Ctrl Pts',(-1.56222819300006,5.2,-3.72323800600002));
#323369=CARTESIAN_POINT('Ctrl Pts',(-1.56222819300006,2.2,-3.72323800600002));
#323370=CARTESIAN_POINT('Ctrl Pts',(-1.56241410500006,12.2,-3.72396955900001));
#323371=CARTESIAN_POINT('Ctrl Pts',(-1.56241410500006,5.2,-3.72396955900001));
#323372=CARTESIAN_POINT('Ctrl Pts',(-1.56241410500006,2.2,-3.72396955900001));
#323373=CARTESIAN_POINT('Ctrl Pts',(-1.56260053900006,12.2,-3.72470707300002));
#323374=CARTESIAN_POINT('Ctrl Pts',(-1.56260053900006,5.2,-3.72470707300002));
#323375=CARTESIAN_POINT('Ctrl Pts',(-1.56260053900006,2.2,-3.72470707300002));
#323376=CARTESIAN_POINT('Ctrl Pts',(-1.56278748000006,12.2,-3.72545053900001));
#323377=CARTESIAN_POINT('Ctrl Pts',(-1.56278748000006,5.2,-3.72545053900001));
#323378=CARTESIAN_POINT('Ctrl Pts',(-1.56278748000006,2.2,-3.72545053900001));
#323379=CARTESIAN_POINT('Ctrl Pts',(-1.56297490900006,12.2,-3.72619994800001));
#323380=CARTESIAN_POINT('Ctrl Pts',(-1.56297490900006,5.2,-3.72619994800001));
#323381=CARTESIAN_POINT('Ctrl Pts',(-1.56297490900006,2.2,-3.72619994800001));
#323382=CARTESIAN_POINT('Ctrl Pts',(-1.56316281100006,12.2,-3.72695529500001));
#323383=CARTESIAN_POINT('Ctrl Pts',(-1.56316281100006,5.2,-3.72695529500001));
#323384=CARTESIAN_POINT('Ctrl Pts',(-1.56316281100006,2.2,-3.72695529500001));
#323385=CARTESIAN_POINT('Ctrl Pts',(-1.56335117000005,12.2,-3.72771656800001));
#323386=CARTESIAN_POINT('Ctrl Pts',(-1.56335117000005,5.2,-3.72771656800001));
#323387=CARTESIAN_POINT('Ctrl Pts',(-1.56335117000005,2.2,-3.72771656800001));
#323388=CARTESIAN_POINT('Ctrl Pts',(-1.56353996800006,12.2,-3.72848376400002));
#323389=CARTESIAN_POINT('Ctrl Pts',(-1.56353996800006,5.2,-3.72848376400002));
#323390=CARTESIAN_POINT('Ctrl Pts',(-1.56353996800006,2.2,-3.72848376400002));
#323391=CARTESIAN_POINT('Ctrl Pts',(-1.56372918800006,12.2,-3.72925687000001));
#323392=CARTESIAN_POINT('Ctrl Pts',(-1.56372918800006,5.2,-3.72925687000001));
#323393=CARTESIAN_POINT('Ctrl Pts',(-1.56372918800006,2.2,-3.72925687000001));
#323394=CARTESIAN_POINT('Ctrl Pts',(-1.56391881500005,12.2,-3.73003588000001));
#323395=CARTESIAN_POINT('Ctrl Pts',(-1.56391881500005,5.2,-3.73003588000001));
#323396=CARTESIAN_POINT('Ctrl Pts',(-1.56391881500005,2.2,-3.73003588000001));
#323397=CARTESIAN_POINT('Ctrl Pts',(-1.56410883100006,12.2,-3.73082078600001));
#323398=CARTESIAN_POINT('Ctrl Pts',(-1.56410883100006,5.2,-3.73082078600001));
#323399=CARTESIAN_POINT('Ctrl Pts',(-1.56410883100006,2.2,-3.73082078600001));
#323400=CARTESIAN_POINT('Ctrl Pts',(-1.56429922100006,12.2,-3.73161158000002));
#323401=CARTESIAN_POINT('Ctrl Pts',(-1.56429922100006,5.2,-3.73161158000002));
#323402=CARTESIAN_POINT('Ctrl Pts',(-1.56429922100006,2.2,-3.73161158000002));
#323403=CARTESIAN_POINT('Ctrl Pts',(-1.56448996900005,12.2,-3.73240825400002));
#323404=CARTESIAN_POINT('Ctrl Pts',(-1.56448996900005,5.2,-3.73240825400002));
#323405=CARTESIAN_POINT('Ctrl Pts',(-1.56448996900005,2.2,-3.73240825400002));
#323406=CARTESIAN_POINT('Ctrl Pts',(-1.56468105700006,12.2,-3.73321079900002));
#323407=CARTESIAN_POINT('Ctrl Pts',(-1.56468105700006,5.2,-3.73321079900002));
#323408=CARTESIAN_POINT('Ctrl Pts',(-1.56468105700006,2.2,-3.73321079900002));
#323409=CARTESIAN_POINT('Ctrl Pts',(-1.56487247100005,12.2,-3.73401920800001));
#323410=CARTESIAN_POINT('Ctrl Pts',(-1.56487247100005,5.2,-3.73401920800001));
#323411=CARTESIAN_POINT('Ctrl Pts',(-1.56487247100005,2.2,-3.73401920800001));
#323412=CARTESIAN_POINT('Ctrl Pts',(-1.56506419200006,12.2,-3.73483347200001));
#323413=CARTESIAN_POINT('Ctrl Pts',(-1.56506419200006,5.2,-3.73483347200001));
#323414=CARTESIAN_POINT('Ctrl Pts',(-1.56506419200006,2.2,-3.73483347200001));
#323415=CARTESIAN_POINT('Ctrl Pts',(-1.56525620700006,12.2,-3.73565358500001));
#323416=CARTESIAN_POINT('Ctrl Pts',(-1.56525620700006,5.2,-3.73565358500001));
#323417=CARTESIAN_POINT('Ctrl Pts',(-1.56525620700006,2.2,-3.73565358500001));
#323418=CARTESIAN_POINT('Ctrl Pts',(-1.56544849800006,12.2,-3.73647953600001));
#323419=CARTESIAN_POINT('Ctrl Pts',(-1.56544849800006,5.2,-3.73647953600001));
#323420=CARTESIAN_POINT('Ctrl Pts',(-1.56544849800006,2.2,-3.73647953600001));
#323421=CARTESIAN_POINT('Ctrl Pts',(-1.56564104900006,12.2,-3.73731132000001));
#323422=CARTESIAN_POINT('Ctrl Pts',(-1.56564104900006,5.2,-3.73731132000001));
#323423=CARTESIAN_POINT('Ctrl Pts',(-1.56564104900006,2.2,-3.73731132000001));
#323424=CARTESIAN_POINT('Ctrl Pts',(-1.56583384600005,12.2,-3.73814892600001));
#323425=CARTESIAN_POINT('Ctrl Pts',(-1.56583384600005,5.2,-3.73814892600001));
#323426=CARTESIAN_POINT('Ctrl Pts',(-1.56583384600005,2.2,-3.73814892600001));
#323427=CARTESIAN_POINT('Ctrl Pts',(-1.56602687100006,12.2,-3.73899234800001));
#323428=CARTESIAN_POINT('Ctrl Pts',(-1.56602687100006,5.2,-3.73899234800001));
#323429=CARTESIAN_POINT('Ctrl Pts',(-1.56602687100006,2.2,-3.73899234800001));
#323430=CARTESIAN_POINT('Ctrl Pts',(-1.56622010900006,12.2,-3.73984157700002));
#323431=CARTESIAN_POINT('Ctrl Pts',(-1.56622010900006,5.2,-3.73984157700002));
#323432=CARTESIAN_POINT('Ctrl Pts',(-1.56622010900006,2.2,-3.73984157700002));
#323433=CARTESIAN_POINT('Ctrl Pts',(-1.56641354400006,12.2,-3.74069660600002));
#323434=CARTESIAN_POINT('Ctrl Pts',(-1.56641354400006,5.2,-3.74069660600002));
#323435=CARTESIAN_POINT('Ctrl Pts',(-1.56641354400006,2.2,-3.74069660600002));
#323436=CARTESIAN_POINT('Ctrl Pts',(-1.56660716100005,12.2,-3.74155742600002));
#323437=CARTESIAN_POINT('Ctrl Pts',(-1.56660716100005,5.2,-3.74155742600002));
#323438=CARTESIAN_POINT('Ctrl Pts',(-1.56660716100005,2.2,-3.74155742600002));
#323439=CARTESIAN_POINT('Ctrl Pts',(-1.56680094400006,12.2,-3.74242402900002));
#323440=CARTESIAN_POINT('Ctrl Pts',(-1.56680094400006,5.2,-3.74242402900002));
#323441=CARTESIAN_POINT('Ctrl Pts',(-1.56680094400006,2.2,-3.74242402900002));
#323442=CARTESIAN_POINT('Ctrl Pts',(-1.56699487700006,12.2,-3.74329640700001));
#323443=CARTESIAN_POINT('Ctrl Pts',(-1.56699487700006,5.2,-3.74329640700001));
#323444=CARTESIAN_POINT('Ctrl Pts',(-1.56699487700006,2.2,-3.74329640700001));
#323445=CARTESIAN_POINT('Ctrl Pts',(-1.56718894400006,12.2,-3.74417455200001));
#323446=CARTESIAN_POINT('Ctrl Pts',(-1.56718894400006,5.2,-3.74417455200001));
#323447=CARTESIAN_POINT('Ctrl Pts',(-1.56718894400006,2.2,-3.74417455200001));
#323448=CARTESIAN_POINT('Ctrl Pts',(-1.56738313100006,12.2,-3.74505845700002));
#323449=CARTESIAN_POINT('Ctrl Pts',(-1.56738313100006,5.2,-3.74505845700002));
#323450=CARTESIAN_POINT('Ctrl Pts',(-1.56738313100006,2.2,-3.74505845700002));
#323451=CARTESIAN_POINT('Ctrl Pts',(-1.56757742100006,12.2,-3.74594811200001));
#323452=CARTESIAN_POINT('Ctrl Pts',(-1.56757742100006,5.2,-3.74594811200001));
#323453=CARTESIAN_POINT('Ctrl Pts',(-1.56757742100006,2.2,-3.74594811200001));
#323454=CARTESIAN_POINT('Ctrl Pts',(-1.56777179900006,12.2,-3.74684351100001));
#323455=CARTESIAN_POINT('Ctrl Pts',(-1.56777179900006,5.2,-3.74684351100001));
#323456=CARTESIAN_POINT('Ctrl Pts',(-1.56777179900006,2.2,-3.74684351100001));
#323457=CARTESIAN_POINT('Ctrl Pts',(-1.56796625000006,12.2,-3.74774464500002));
#323458=CARTESIAN_POINT('Ctrl Pts',(-1.56796625000006,5.2,-3.74774464500002));
#323459=CARTESIAN_POINT('Ctrl Pts',(-1.56796625000006,2.2,-3.74774464500002));
#323460=CARTESIAN_POINT('Ctrl Pts',(-1.56816076000006,12.2,-3.74865150500002));
#323461=CARTESIAN_POINT('Ctrl Pts',(-1.56816076000006,5.2,-3.74865150500002));
#323462=CARTESIAN_POINT('Ctrl Pts',(-1.56816076000006,2.2,-3.74865150500002));
#323463=CARTESIAN_POINT('Ctrl Pts',(-1.56835531100006,12.2,-3.74956408500001));
#323464=CARTESIAN_POINT('Ctrl Pts',(-1.56835531100006,5.2,-3.74956408500001));
#323465=CARTESIAN_POINT('Ctrl Pts',(-1.56835531100006,2.2,-3.74956408500001));
#323466=CARTESIAN_POINT('Ctrl Pts',(-1.56854988800006,12.2,-3.75048237600001));
#323467=CARTESIAN_POINT('Ctrl Pts',(-1.56854988800006,5.2,-3.75048237600001));
#323468=CARTESIAN_POINT('Ctrl Pts',(-1.56854988800006,2.2,-3.75048237600001));
#323469=CARTESIAN_POINT('Ctrl Pts',(-1.56874447900006,12.2,-3.75140637000001));
#323470=CARTESIAN_POINT('Ctrl Pts',(-1.56874447900006,5.2,-3.75140637000001));
#323471=CARTESIAN_POINT('Ctrl Pts',(-1.56874447900006,2.2,-3.75140637000001));
#323472=CARTESIAN_POINT('Ctrl Pts',(-1.56893906600006,12.2,-3.75233605800001));
#323473=CARTESIAN_POINT('Ctrl Pts',(-1.56893906600006,5.2,-3.75233605800001));
#323474=CARTESIAN_POINT('Ctrl Pts',(-1.56893906600006,2.2,-3.75233605800001));
#323475=CARTESIAN_POINT('Ctrl Pts',(-1.56913363400006,12.2,-3.75327143400002));
#323476=CARTESIAN_POINT('Ctrl Pts',(-1.56913363400006,5.2,-3.75327143400002));
#323477=CARTESIAN_POINT('Ctrl Pts',(-1.56913363400006,2.2,-3.75327143400002));
#323478=CARTESIAN_POINT('Ctrl Pts',(-1.56932817100006,12.2,-3.75421248800002));
#323479=CARTESIAN_POINT('Ctrl Pts',(-1.56932817100006,5.2,-3.75421248800002));
#323480=CARTESIAN_POINT('Ctrl Pts',(-1.56932817100006,2.2,-3.75421248800002));
#323481=CARTESIAN_POINT('Ctrl Pts',(-1.56952265800005,12.2,-3.75515921400002));
#323482=CARTESIAN_POINT('Ctrl Pts',(-1.56952265800005,5.2,-3.75515921400002));
#323483=CARTESIAN_POINT('Ctrl Pts',(-1.56952265800005,2.2,-3.75515921400002));
#323484=CARTESIAN_POINT('Ctrl Pts',(-1.56971708200006,12.2,-3.75611160200001));
#323485=CARTESIAN_POINT('Ctrl Pts',(-1.56971708200006,5.2,-3.75611160200001));
#323486=CARTESIAN_POINT('Ctrl Pts',(-1.56971708200006,2.2,-3.75611160200001));
#323487=CARTESIAN_POINT('Ctrl Pts',(-1.56991142900006,12.2,-3.75706964400001));
#323488=CARTESIAN_POINT('Ctrl Pts',(-1.56991142900006,5.2,-3.75706964400001));
#323489=CARTESIAN_POINT('Ctrl Pts',(-1.56991142900006,2.2,-3.75706964400001));
#323490=CARTESIAN_POINT('Ctrl Pts',(-1.57010568200006,12.2,-3.75803333400002));
#323491=CARTESIAN_POINT('Ctrl Pts',(-1.57010568200006,5.2,-3.75803333400002));
#323492=CARTESIAN_POINT('Ctrl Pts',(-1.57010568200006,2.2,-3.75803333400002));
#323493=CARTESIAN_POINT('Ctrl Pts',(-1.57029982900006,12.2,-3.75900266300001));
#323494=CARTESIAN_POINT('Ctrl Pts',(-1.57029982900006,5.2,-3.75900266300001));
#323495=CARTESIAN_POINT('Ctrl Pts',(-1.57029982900006,2.2,-3.75900266300001));
#323496=CARTESIAN_POINT('Ctrl Pts',(-1.57049385200006,12.2,-3.75997762300001));
#323497=CARTESIAN_POINT('Ctrl Pts',(-1.57049385200006,5.2,-3.75997762300001));
#323498=CARTESIAN_POINT('Ctrl Pts',(-1.57049385200006,2.2,-3.75997762300001));
#323499=CARTESIAN_POINT('Ctrl Pts',(-1.57068773900006,12.2,-3.76095820600002));
#323500=CARTESIAN_POINT('Ctrl Pts',(-1.57068773900006,5.2,-3.76095820600002));
#323501=CARTESIAN_POINT('Ctrl Pts',(-1.57068773900006,2.2,-3.76095820600002));
#323502=CARTESIAN_POINT('Ctrl Pts',(-1.57088147400006,12.2,-3.76194440300001));
#323503=CARTESIAN_POINT('Ctrl Pts',(-1.57088147400006,5.2,-3.76194440300001));
#323504=CARTESIAN_POINT('Ctrl Pts',(-1.57088147400006,2.2,-3.76194440300001));
#323505=CARTESIAN_POINT('Ctrl Pts',(-1.57107504200006,12.2,-3.76293620800002));
#323506=CARTESIAN_POINT('Ctrl Pts',(-1.57107504200006,5.2,-3.76293620800002));
#323507=CARTESIAN_POINT('Ctrl Pts',(-1.57107504200006,2.2,-3.76293620800002));
#323508=CARTESIAN_POINT('Ctrl Pts',(-1.57126843100006,12.2,-3.76393361100002));
#323509=CARTESIAN_POINT('Ctrl Pts',(-1.57126843100006,5.2,-3.76393361100002));
#323510=CARTESIAN_POINT('Ctrl Pts',(-1.57126843100006,2.2,-3.76393361100002));
#323511=CARTESIAN_POINT('Ctrl Pts',(-1.57146162400006,12.2,-3.76493660500001));
#323512=CARTESIAN_POINT('Ctrl Pts',(-1.57146162400006,5.2,-3.76493660500001));
#323513=CARTESIAN_POINT('Ctrl Pts',(-1.57146162400006,2.2,-3.76493660500001));
#323514=CARTESIAN_POINT('Ctrl Pts',(-1.57165460600006,12.2,-3.76594518200001));
#323515=CARTESIAN_POINT('Ctrl Pts',(-1.57165460600006,5.2,-3.76594518200001));
#323516=CARTESIAN_POINT('Ctrl Pts',(-1.57165460600006,2.2,-3.76594518200001));
#323517=CARTESIAN_POINT('Ctrl Pts',(-1.57184736600006,12.2,-3.76695933400002));
#323518=CARTESIAN_POINT('Ctrl Pts',(-1.57184736600006,5.2,-3.76695933400002));
#323519=CARTESIAN_POINT('Ctrl Pts',(-1.57184736600006,2.2,-3.76695933400002));
#323520=CARTESIAN_POINT('Ctrl Pts',(-1.57203988700006,12.2,-3.76797905300001));
#323521=CARTESIAN_POINT('Ctrl Pts',(-1.57203988700006,5.2,-3.76797905300001));
#323522=CARTESIAN_POINT('Ctrl Pts',(-1.57203988700006,2.2,-3.76797905300001));
#323523=CARTESIAN_POINT('Ctrl Pts',(-1.57223215400006,12.2,-3.76900433100001));
#323524=CARTESIAN_POINT('Ctrl Pts',(-1.57223215400006,5.2,-3.76900433100001));
#323525=CARTESIAN_POINT('Ctrl Pts',(-1.57223215400006,2.2,-3.76900433100001));
#323526=CARTESIAN_POINT('Ctrl Pts',(-1.57242415500006,12.2,-3.77003516000002));
#323527=CARTESIAN_POINT('Ctrl Pts',(-1.57242415500006,5.2,-3.77003516000002));
#323528=CARTESIAN_POINT('Ctrl Pts',(-1.57242415500006,2.2,-3.77003516000002));
#323529=CARTESIAN_POINT('Ctrl Pts',(-1.57261587600006,12.2,-3.77107153100001));
#323530=CARTESIAN_POINT('Ctrl Pts',(-1.57261587600006,5.2,-3.77107153100001));
#323531=CARTESIAN_POINT('Ctrl Pts',(-1.57261587600006,2.2,-3.77107153100001));
#323532=CARTESIAN_POINT('Ctrl Pts',(-1.57280730000006,12.2,-3.77211343700001));
#323533=CARTESIAN_POINT('Ctrl Pts',(-1.57280730000006,5.2,-3.77211343700001));
#323534=CARTESIAN_POINT('Ctrl Pts',(-1.57280730000006,2.2,-3.77211343700001));
#323535=CARTESIAN_POINT('Ctrl Pts',(-1.57299841500006,12.2,-3.77316087100001));
#323536=CARTESIAN_POINT('Ctrl Pts',(-1.57299841500006,5.2,-3.77316087100001));
#323537=CARTESIAN_POINT('Ctrl Pts',(-1.57299841500006,2.2,-3.77316087100001));
#323538=CARTESIAN_POINT('Ctrl Pts',(-1.57318920600006,12.2,-3.77421382400001));
#323539=CARTESIAN_POINT('Ctrl Pts',(-1.57318920600006,5.2,-3.77421382400001));
#323540=CARTESIAN_POINT('Ctrl Pts',(-1.57318920600006,2.2,-3.77421382400001));
#323541=CARTESIAN_POINT('Ctrl Pts',(-1.57337966000005,12.2,-3.77527228700002));
#323542=CARTESIAN_POINT('Ctrl Pts',(-1.57337966000005,5.2,-3.77527228700002));
#323543=CARTESIAN_POINT('Ctrl Pts',(-1.57337966000005,2.2,-3.77527228700002));
#323544=CARTESIAN_POINT('Ctrl Pts',(-1.57356976200006,12.2,-3.77633625300001));
#323545=CARTESIAN_POINT('Ctrl Pts',(-1.57356976200006,5.2,-3.77633625300001));
#323546=CARTESIAN_POINT('Ctrl Pts',(-1.57356976200006,2.2,-3.77633625300001));
#323547=CARTESIAN_POINT('Ctrl Pts',(-1.57375949900006,12.2,-3.77740571600001));
#323548=CARTESIAN_POINT('Ctrl Pts',(-1.57375949900006,5.2,-3.77740571600001));
#323549=CARTESIAN_POINT('Ctrl Pts',(-1.57375949900006,2.2,-3.77740571600001));
#323550=CARTESIAN_POINT('Ctrl Pts',(-1.57394885500006,12.2,-3.77848066400002));
#323551=CARTESIAN_POINT('Ctrl Pts',(-1.57394885500006,5.2,-3.77848066400002));
#323552=CARTESIAN_POINT('Ctrl Pts',(-1.57394885500006,2.2,-3.77848066400002));
#323553=CARTESIAN_POINT('Ctrl Pts',(-1.57413781900006,12.2,-3.77956109200001));
#323554=CARTESIAN_POINT('Ctrl Pts',(-1.57413781900006,5.2,-3.77956109200001));
#323555=CARTESIAN_POINT('Ctrl Pts',(-1.57413781900006,2.2,-3.77956109200001));
#323556=CARTESIAN_POINT('Ctrl Pts',(-1.57432637600006,12.2,-3.78064699100001));
#323557=CARTESIAN_POINT('Ctrl Pts',(-1.57432637600006,5.2,-3.78064699100001));
#323558=CARTESIAN_POINT('Ctrl Pts',(-1.57432637600006,2.2,-3.78064699100001));
#323559=CARTESIAN_POINT('Ctrl Pts',(-1.57451451100005,12.2,-3.78173835300001));
#323560=CARTESIAN_POINT('Ctrl Pts',(-1.57451451100005,5.2,-3.78173835300001));
#323561=CARTESIAN_POINT('Ctrl Pts',(-1.57451451100005,2.2,-3.78173835300001));
#323562=CARTESIAN_POINT('Ctrl Pts',(-1.57470221200006,12.2,-3.78283517000002));
#323563=CARTESIAN_POINT('Ctrl Pts',(-1.57470221200006,5.2,-3.78283517000002));
#323564=CARTESIAN_POINT('Ctrl Pts',(-1.57470221200006,2.2,-3.78283517000002));
#323565=CARTESIAN_POINT('Ctrl Pts',(-1.57488946500006,12.2,-3.78393743500002));
#323566=CARTESIAN_POINT('Ctrl Pts',(-1.57488946500006,5.2,-3.78393743500002));
#323567=CARTESIAN_POINT('Ctrl Pts',(-1.57488946500006,2.2,-3.78393743500002));
#323568=CARTESIAN_POINT('Ctrl Pts',(-1.57507625600006,12.2,-3.78504513900001));
#323569=CARTESIAN_POINT('Ctrl Pts',(-1.57507625600006,5.2,-3.78504513900001));
#323570=CARTESIAN_POINT('Ctrl Pts',(-1.57507625600006,2.2,-3.78504513900001));
#323571=CARTESIAN_POINT('Ctrl Pts',(-1.57526257100006,12.2,-3.78615827400001));
#323572=CARTESIAN_POINT('Ctrl Pts',(-1.57526257100006,5.2,-3.78615827400001));
#323573=CARTESIAN_POINT('Ctrl Pts',(-1.57526257100006,2.2,-3.78615827400001));
#323574=CARTESIAN_POINT('Ctrl Pts',(-1.57544839700006,12.2,-3.78727683200001));
#323575=CARTESIAN_POINT('Ctrl Pts',(-1.57544839700006,5.2,-3.78727683200001));
#323576=CARTESIAN_POINT('Ctrl Pts',(-1.57544839700006,2.2,-3.78727683200001));
#323577=CARTESIAN_POINT('Ctrl Pts',(-1.57563372100005,12.2,-3.78840080700002));
#323578=CARTESIAN_POINT('Ctrl Pts',(-1.57563372100005,5.2,-3.78840080700002));
#323579=CARTESIAN_POINT('Ctrl Pts',(-1.57563372100005,2.2,-3.78840080700002));
#323580=CARTESIAN_POINT('Ctrl Pts',(-1.57581852800006,12.2,-3.78953018700001));
#323581=CARTESIAN_POINT('Ctrl Pts',(-1.57581852800006,5.2,-3.78953018700001));
#323582=CARTESIAN_POINT('Ctrl Pts',(-1.57581852800006,2.2,-3.78953018700001));
#323583=CARTESIAN_POINT('Ctrl Pts',(-1.57600280500006,12.2,-3.79066496800001));
#323584=CARTESIAN_POINT('Ctrl Pts',(-1.57600280500006,5.2,-3.79066496800001));
#323585=CARTESIAN_POINT('Ctrl Pts',(-1.57600280500006,2.2,-3.79066496800001));
#323586=CARTESIAN_POINT('Ctrl Pts',(-1.57618654000005,12.2,-3.79180514000002));
#323587=CARTESIAN_POINT('Ctrl Pts',(-1.57618654000005,5.2,-3.79180514000002));
#323588=CARTESIAN_POINT('Ctrl Pts',(-1.57618654000005,2.2,-3.79180514000002));
#323589=CARTESIAN_POINT('Ctrl Pts',(-1.57636971900006,12.2,-3.79295069600001));
#323590=CARTESIAN_POINT('Ctrl Pts',(-1.57636971900006,5.2,-3.79295069600001));
#323591=CARTESIAN_POINT('Ctrl Pts',(-1.57636971900006,2.2,-3.79295069600001));
#323592=CARTESIAN_POINT('Ctrl Pts',(-1.57655232800006,12.2,-3.79410162700001));
#323593=CARTESIAN_POINT('Ctrl Pts',(-1.57655232800006,5.2,-3.79410162700001));
#323594=CARTESIAN_POINT('Ctrl Pts',(-1.57655232800006,2.2,-3.79410162700001));
#323595=CARTESIAN_POINT('Ctrl Pts',(-1.57673435400006,12.2,-3.79525792600001));
#323596=CARTESIAN_POINT('Ctrl Pts',(-1.57673435400006,5.2,-3.79525792600001));
#323597=CARTESIAN_POINT('Ctrl Pts',(-1.57673435400006,2.2,-3.79525792600001));
#323598=CARTESIAN_POINT('Ctrl Pts',(-1.57691578400006,12.2,-3.79641958400001));
#323599=CARTESIAN_POINT('Ctrl Pts',(-1.57691578400006,5.2,-3.79641958400001));
#323600=CARTESIAN_POINT('Ctrl Pts',(-1.57691578400006,2.2,-3.79641958400001));
#323601=CARTESIAN_POINT('Ctrl Pts',(-1.57709660400006,12.2,-3.79758659500002));
#323602=CARTESIAN_POINT('Ctrl Pts',(-1.57709660400006,5.2,-3.79758659500002));
#323603=CARTESIAN_POINT('Ctrl Pts',(-1.57709660400006,2.2,-3.79758659500002));
#323604=CARTESIAN_POINT('Ctrl Pts',(-1.57727680300006,12.2,-3.79875894900001));
#323605=CARTESIAN_POINT('Ctrl Pts',(-1.57727680300006,5.2,-3.79875894900001));
#323606=CARTESIAN_POINT('Ctrl Pts',(-1.57727680300006,2.2,-3.79875894900001));
#323607=CARTESIAN_POINT('Ctrl Pts',(-1.57745636500006,12.2,-3.79993664000001));
#323608=CARTESIAN_POINT('Ctrl Pts',(-1.57745636500006,5.2,-3.79993664000001));
#323609=CARTESIAN_POINT('Ctrl Pts',(-1.57745636500006,2.2,-3.79993664000001));
#323610=CARTESIAN_POINT('Ctrl Pts',(-1.57763528000005,12.2,-3.80111965800001));
#323611=CARTESIAN_POINT('Ctrl Pts',(-1.57763528000005,5.2,-3.80111965800001));
#323612=CARTESIAN_POINT('Ctrl Pts',(-1.57763528000005,2.2,-3.80111965800001));
#323613=CARTESIAN_POINT('Ctrl Pts',(-1.57781353300006,12.2,-3.80230799500001));
#323614=CARTESIAN_POINT('Ctrl Pts',(-1.57781353300006,5.2,-3.80230799500001));
#323615=CARTESIAN_POINT('Ctrl Pts',(-1.57781353300006,2.2,-3.80230799500001));
#323616=CARTESIAN_POINT('Ctrl Pts',(-1.57799111000006,12.2,-3.80350164500001));
#323617=CARTESIAN_POINT('Ctrl Pts',(-1.57799111000006,5.2,-3.80350164500001));
#323618=CARTESIAN_POINT('Ctrl Pts',(-1.57799111000006,2.2,-3.80350164500001));
#323619=CARTESIAN_POINT('Ctrl Pts',(-1.57816800100006,12.2,-3.80470059800002));
#323620=CARTESIAN_POINT('Ctrl Pts',(-1.57816800100006,5.2,-3.80470059800002));
#323621=CARTESIAN_POINT('Ctrl Pts',(-1.57816800100006,2.2,-3.80470059800002));
#323622=CARTESIAN_POINT('Ctrl Pts',(-1.57834419200006,12.2,-3.80590484900001));
#323623=CARTESIAN_POINT('Ctrl Pts',(-1.57834419200006,5.2,-3.80590484900001));
#323624=CARTESIAN_POINT('Ctrl Pts',(-1.57834419200006,2.2,-3.80590484900001));
#323625=CARTESIAN_POINT('Ctrl Pts',(-1.57851966900005,12.2,-3.80711438700001));
#323626=CARTESIAN_POINT('Ctrl Pts',(-1.57851966900005,5.2,-3.80711438700001));
#323627=CARTESIAN_POINT('Ctrl Pts',(-1.57851966900005,2.2,-3.80711438700001));
#323628=CARTESIAN_POINT('Ctrl Pts',(-1.57869441900006,12.2,-3.80832920600001));
#323629=CARTESIAN_POINT('Ctrl Pts',(-1.57869441900006,5.2,-3.80832920600001));
#323630=CARTESIAN_POINT('Ctrl Pts',(-1.57869441900006,2.2,-3.80832920600001));
#323631=CARTESIAN_POINT('Ctrl Pts',(-1.57886843200005,12.2,-3.80954929600001));
#323632=CARTESIAN_POINT('Ctrl Pts',(-1.57886843200005,5.2,-3.80954929600001));
#323633=CARTESIAN_POINT('Ctrl Pts',(-1.57886843200005,2.2,-3.80954929600001));
#323634=CARTESIAN_POINT('Ctrl Pts',(-1.57904169200005,12.2,-3.81077465100002));
#323635=CARTESIAN_POINT('Ctrl Pts',(-1.57904169200005,5.2,-3.81077465100002));
#323636=CARTESIAN_POINT('Ctrl Pts',(-1.57904169200005,2.2,-3.81077465100002));
#323637=CARTESIAN_POINT('Ctrl Pts',(-1.57921418900006,12.2,-3.81200526300002));
#323638=CARTESIAN_POINT('Ctrl Pts',(-1.57921418900006,5.2,-3.81200526300002));
#323639=CARTESIAN_POINT('Ctrl Pts',(-1.57921418900006,2.2,-3.81200526300002));
#323640=CARTESIAN_POINT('Ctrl Pts',(-1.57938590800006,12.2,-3.81324112200002));
#323641=CARTESIAN_POINT('Ctrl Pts',(-1.57938590800006,5.2,-3.81324112200002));
#323642=CARTESIAN_POINT('Ctrl Pts',(-1.57938590800006,2.2,-3.81324112200002));
#323643=CARTESIAN_POINT('Ctrl Pts',(-1.57955683700005,12.2,-3.81448222300001));
#323644=CARTESIAN_POINT('Ctrl Pts',(-1.57955683700005,5.2,-3.81448222300001));
#323645=CARTESIAN_POINT('Ctrl Pts',(-1.57955683700005,2.2,-3.81448222300001));
#323646=CARTESIAN_POINT('Ctrl Pts',(-1.57972696400006,12.2,-3.81572855600002));
#323647=CARTESIAN_POINT('Ctrl Pts',(-1.57972696400006,5.2,-3.81572855600002));
#323648=CARTESIAN_POINT('Ctrl Pts',(-1.57972696400006,2.2,-3.81572855600002));
#323649=CARTESIAN_POINT('Ctrl Pts',(-1.57989627800006,12.2,-3.81698011500001));
#323650=CARTESIAN_POINT('Ctrl Pts',(-1.57989627800006,5.2,-3.81698011500001));
#323651=CARTESIAN_POINT('Ctrl Pts',(-1.57989627800006,2.2,-3.81698011500001));
#323652=CARTESIAN_POINT('Ctrl Pts',(-1.58006476400006,12.2,-3.81823689000001));
#323653=CARTESIAN_POINT('Ctrl Pts',(-1.58006476400006,5.2,-3.81823689000001));
#323654=CARTESIAN_POINT('Ctrl Pts',(-1.58006476400006,2.2,-3.81823689000001));
#323655=CARTESIAN_POINT('Ctrl Pts',(-1.58023240900006,12.2,-3.81949887400001));
#323656=CARTESIAN_POINT('Ctrl Pts',(-1.58023240900006,5.2,-3.81949887400001));
#323657=CARTESIAN_POINT('Ctrl Pts',(-1.58023240900006,2.2,-3.81949887400001));
#323658=CARTESIAN_POINT('Ctrl Pts',(-1.58039920300005,12.2,-3.82076605800002));
#323659=CARTESIAN_POINT('Ctrl Pts',(-1.58039920300005,5.2,-3.82076605800002));
#323660=CARTESIAN_POINT('Ctrl Pts',(-1.58039920300005,2.2,-3.82076605800002));
#323661=CARTESIAN_POINT('Ctrl Pts',(-1.58056513200005,12.2,-3.82203843600001));
#323662=CARTESIAN_POINT('Ctrl Pts',(-1.58056513200005,5.2,-3.82203843600001));
#323663=CARTESIAN_POINT('Ctrl Pts',(-1.58056513200005,2.2,-3.82203843600001));
#323664=CARTESIAN_POINT('Ctrl Pts',(-1.58073018500006,12.2,-3.82331599900001));
#323665=CARTESIAN_POINT('Ctrl Pts',(-1.58073018500006,5.2,-3.82331599900001));
#323666=CARTESIAN_POINT('Ctrl Pts',(-1.58073018500006,2.2,-3.82331599900001));
#323667=CARTESIAN_POINT('Ctrl Pts',(-1.58089434800006,12.2,-3.82459873900002));
#323668=CARTESIAN_POINT('Ctrl Pts',(-1.58089434800006,5.2,-3.82459873900002));
#323669=CARTESIAN_POINT('Ctrl Pts',(-1.58089434800006,2.2,-3.82459873900002));
#323670=CARTESIAN_POINT('Ctrl Pts',(-1.58105761000006,12.2,-3.82588664800001));
#323671=CARTESIAN_POINT('Ctrl Pts',(-1.58105761000006,5.2,-3.82588664800001));
#323672=CARTESIAN_POINT('Ctrl Pts',(-1.58105761000006,2.2,-3.82588664800001));
#323673=CARTESIAN_POINT('Ctrl Pts',(-1.58121995800005,12.2,-3.82717971800002));
#323674=CARTESIAN_POINT('Ctrl Pts',(-1.58121995800005,5.2,-3.82717971800002));
#323675=CARTESIAN_POINT('Ctrl Pts',(-1.58121995800005,2.2,-3.82717971800002));
#323676=CARTESIAN_POINT('Ctrl Pts',(-1.58138138000006,12.2,-3.82847794200002));
#323677=CARTESIAN_POINT('Ctrl Pts',(-1.58138138000006,5.2,-3.82847794200002));
#323678=CARTESIAN_POINT('Ctrl Pts',(-1.58138138000006,2.2,-3.82847794200002));
#323679=CARTESIAN_POINT('Ctrl Pts',(-1.58154186500005,12.2,-3.82978131200002));
#323680=CARTESIAN_POINT('Ctrl Pts',(-1.58154186500005,5.2,-3.82978131200002));
#323681=CARTESIAN_POINT('Ctrl Pts',(-1.58154186500005,2.2,-3.82978131200002));
#323682=CARTESIAN_POINT('Ctrl Pts',(-1.58170139800006,12.2,-3.83108981900001));
#323683=CARTESIAN_POINT('Ctrl Pts',(-1.58170139800006,5.2,-3.83108981900001));
#323684=CARTESIAN_POINT('Ctrl Pts',(-1.58170139800006,2.2,-3.83108981900001));
#323685=CARTESIAN_POINT('Ctrl Pts',(-1.58185997000006,12.2,-3.83240345600001));
#323686=CARTESIAN_POINT('Ctrl Pts',(-1.58185997000006,5.2,-3.83240345600001));
#323687=CARTESIAN_POINT('Ctrl Pts',(-1.58185997000006,2.2,-3.83240345600001));
#323688=CARTESIAN_POINT('Ctrl Pts',(-1.58201756800006,12.2,-3.83372221400001));
#323689=CARTESIAN_POINT('Ctrl Pts',(-1.58201756800006,5.2,-3.83372221400001));
#323690=CARTESIAN_POINT('Ctrl Pts',(-1.58201756800006,2.2,-3.83372221400001));
#323691=CARTESIAN_POINT('Ctrl Pts',(-1.58217417900006,12.2,-3.83504608800001));
#323692=CARTESIAN_POINT('Ctrl Pts',(-1.58217417900006,5.2,-3.83504608800001));
#323693=CARTESIAN_POINT('Ctrl Pts',(-1.58217417900006,2.2,-3.83504608800001));
#323694=CARTESIAN_POINT('Ctrl Pts',(-1.58232979100006,12.2,-3.83637506500001));
#323695=CARTESIAN_POINT('Ctrl Pts',(-1.58232979100006,5.2,-3.83637506500001));
#323696=CARTESIAN_POINT('Ctrl Pts',(-1.58232979100006,2.2,-3.83637506500001));
#323697=CARTESIAN_POINT('Ctrl Pts',(-1.58248439400006,12.2,-3.83770914200001));
#323698=CARTESIAN_POINT('Ctrl Pts',(-1.58248439400006,5.2,-3.83770914200001));
#323699=CARTESIAN_POINT('Ctrl Pts',(-1.58248439400006,2.2,-3.83770914200001));
#323700=CARTESIAN_POINT('Ctrl Pts',(-1.58263797400006,12.2,-3.83904831000002));
#323701=CARTESIAN_POINT('Ctrl Pts',(-1.58263797400006,5.2,-3.83904831000002));
#323702=CARTESIAN_POINT('Ctrl Pts',(-1.58263797400006,2.2,-3.83904831000002));
#323703=CARTESIAN_POINT('Ctrl Pts',(-1.58279052000006,12.2,-3.84039255800001));
#323704=CARTESIAN_POINT('Ctrl Pts',(-1.58279052000006,5.2,-3.84039255800001));
#323705=CARTESIAN_POINT('Ctrl Pts',(-1.58279052000006,2.2,-3.84039255800001));
#323706=CARTESIAN_POINT('Ctrl Pts',(-1.58294202100006,12.2,-3.84174188200001));
#323707=CARTESIAN_POINT('Ctrl Pts',(-1.58294202100006,5.2,-3.84174188200001));
#323708=CARTESIAN_POINT('Ctrl Pts',(-1.58294202100006,2.2,-3.84174188200001));
#323709=CARTESIAN_POINT('Ctrl Pts',(-1.58309246300006,12.2,-3.84309627200001));
#323710=CARTESIAN_POINT('Ctrl Pts',(-1.58309246300006,5.2,-3.84309627200001));
#323711=CARTESIAN_POINT('Ctrl Pts',(-1.58309246300006,2.2,-3.84309627200001));
#323712=CARTESIAN_POINT('Ctrl Pts',(-1.58324183600006,12.2,-3.84445572000002));
#323713=CARTESIAN_POINT('Ctrl Pts',(-1.58324183600006,5.2,-3.84445572000002));
#323714=CARTESIAN_POINT('Ctrl Pts',(-1.58324183600006,2.2,-3.84445572000002));
#323715=CARTESIAN_POINT('Ctrl Pts',(-1.58339012800006,12.2,-3.84582022000002));
#323716=CARTESIAN_POINT('Ctrl Pts',(-1.58339012800006,5.2,-3.84582022000002));
#323717=CARTESIAN_POINT('Ctrl Pts',(-1.58339012800006,2.2,-3.84582022000002));
#323718=CARTESIAN_POINT('Ctrl Pts',(-1.58353732700005,12.2,-3.84718976100002));
#323719=CARTESIAN_POINT('Ctrl Pts',(-1.58353732700005,5.2,-3.84718976100002));
#323720=CARTESIAN_POINT('Ctrl Pts',(-1.58353732700005,2.2,-3.84718976100002));
#323721=CARTESIAN_POINT('Ctrl Pts',(-1.58368342100006,12.2,-3.84856433800001));
#323722=CARTESIAN_POINT('Ctrl Pts',(-1.58368342100006,5.2,-3.84856433800001));
#323723=CARTESIAN_POINT('Ctrl Pts',(-1.58368342100006,2.2,-3.84856433800001));
#323724=CARTESIAN_POINT('Ctrl Pts',(-1.58382839900006,12.2,-3.84994394200001));
#323725=CARTESIAN_POINT('Ctrl Pts',(-1.58382839900006,5.2,-3.84994394200001));
#323726=CARTESIAN_POINT('Ctrl Pts',(-1.58382839900006,2.2,-3.84994394200001));
#323727=CARTESIAN_POINT('Ctrl Pts',(-1.58397225000006,12.2,-3.85132856500002));
#323728=CARTESIAN_POINT('Ctrl Pts',(-1.58397225000006,5.2,-3.85132856500002));
#323729=CARTESIAN_POINT('Ctrl Pts',(-1.58397225000006,2.2,-3.85132856500002));
#323730=CARTESIAN_POINT('Ctrl Pts',(-1.58411496100005,12.2,-3.85271819900002));
#323731=CARTESIAN_POINT('Ctrl Pts',(-1.58411496100005,5.2,-3.85271819900002));
#323732=CARTESIAN_POINT('Ctrl Pts',(-1.58411496100005,2.2,-3.85271819900002));
#323733=CARTESIAN_POINT('Ctrl Pts',(-1.58425652100005,12.2,-3.85411283600002));
#323734=CARTESIAN_POINT('Ctrl Pts',(-1.58425652100005,5.2,-3.85411283600002));
#323735=CARTESIAN_POINT('Ctrl Pts',(-1.58425652100005,2.2,-3.85411283600002));
#323736=CARTESIAN_POINT('Ctrl Pts',(-1.58439691900006,12.2,-3.85551247000001));
#323737=CARTESIAN_POINT('Ctrl Pts',(-1.58439691900006,5.2,-3.85551247000001));
#323738=CARTESIAN_POINT('Ctrl Pts',(-1.58439691900006,2.2,-3.85551247000001));
#323739=CARTESIAN_POINT('Ctrl Pts',(-1.58453614300006,12.2,-3.85691709000001));
#323740=CARTESIAN_POINT('Ctrl Pts',(-1.58453614300006,5.2,-3.85691709000001));
#323741=CARTESIAN_POINT('Ctrl Pts',(-1.58453614300006,2.2,-3.85691709000001));
#323742=CARTESIAN_POINT('Ctrl Pts',(-1.58467418200006,12.2,-3.85832669000001));
#323743=CARTESIAN_POINT('Ctrl Pts',(-1.58467418200006,5.2,-3.85832669000001));
#323744=CARTESIAN_POINT('Ctrl Pts',(-1.58467418200006,2.2,-3.85832669000001));
#323745=CARTESIAN_POINT('Ctrl Pts',(-1.58481102500006,12.2,-3.85974126200002));
#323746=CARTESIAN_POINT('Ctrl Pts',(-1.58481102500006,5.2,-3.85974126200002));
#323747=CARTESIAN_POINT('Ctrl Pts',(-1.58481102500006,2.2,-3.85974126200002));
#323748=CARTESIAN_POINT('Ctrl Pts',(-1.58494665900006,12.2,-3.86116079800002));
#323749=CARTESIAN_POINT('Ctrl Pts',(-1.58494665900006,5.2,-3.86116079800002));
#323750=CARTESIAN_POINT('Ctrl Pts',(-1.58494665900006,2.2,-3.86116079800002));
#323751=CARTESIAN_POINT('Ctrl Pts',(-1.58508107400006,12.2,-3.86258529000001));
#323752=CARTESIAN_POINT('Ctrl Pts',(-1.58508107400006,5.2,-3.86258529000001));
#323753=CARTESIAN_POINT('Ctrl Pts',(-1.58508107400006,2.2,-3.86258529000001));
#323754=CARTESIAN_POINT('Ctrl Pts',(-1.58521425900006,12.2,-3.86401473000001));
#323755=CARTESIAN_POINT('Ctrl Pts',(-1.58521425900006,5.2,-3.86401473000001));
#323756=CARTESIAN_POINT('Ctrl Pts',(-1.58521425900006,2.2,-3.86401473000001));
#323757=CARTESIAN_POINT('Ctrl Pts',(-1.58534620200005,12.2,-3.86544911100001));
#323758=CARTESIAN_POINT('Ctrl Pts',(-1.58534620200005,5.2,-3.86544911100001));
#323759=CARTESIAN_POINT('Ctrl Pts',(-1.58534620200005,2.2,-3.86544911100001));
#323760=CARTESIAN_POINT('Ctrl Pts',(-1.58547689100006,12.2,-3.86688842400002));
#323761=CARTESIAN_POINT('Ctrl Pts',(-1.58547689100006,5.2,-3.86688842400002));
#323762=CARTESIAN_POINT('Ctrl Pts',(-1.58547689100006,2.2,-3.86688842400002));
#323763=CARTESIAN_POINT('Ctrl Pts',(-1.58560631700006,12.2,-3.86833266100002));
#323764=CARTESIAN_POINT('Ctrl Pts',(-1.58560631700006,5.2,-3.86833266100002));
#323765=CARTESIAN_POINT('Ctrl Pts',(-1.58560631700006,2.2,-3.86833266100002));
#323766=CARTESIAN_POINT('Ctrl Pts',(-1.58573446800006,12.2,-3.86978181500002));
#323767=CARTESIAN_POINT('Ctrl Pts',(-1.58573446800006,5.2,-3.86978181500002));
#323768=CARTESIAN_POINT('Ctrl Pts',(-1.58573446800006,2.2,-3.86978181500002));
#323769=CARTESIAN_POINT('Ctrl Pts',(-1.58586133200005,12.2,-3.87123587800001));
#323770=CARTESIAN_POINT('Ctrl Pts',(-1.58586133200005,5.2,-3.87123587800001));
#323771=CARTESIAN_POINT('Ctrl Pts',(-1.58586133200005,2.2,-3.87123587800001));
#323772=CARTESIAN_POINT('Ctrl Pts',(-1.58598689800006,12.2,-3.87269484100001));
#323773=CARTESIAN_POINT('Ctrl Pts',(-1.58598689800006,5.2,-3.87269484100001));
#323774=CARTESIAN_POINT('Ctrl Pts',(-1.58598689800006,2.2,-3.87269484100001));
#323775=CARTESIAN_POINT('Ctrl Pts',(-1.58611115600006,12.2,-3.87415869700002));
#323776=CARTESIAN_POINT('Ctrl Pts',(-1.58611115600006,5.2,-3.87415869700002));
#323777=CARTESIAN_POINT('Ctrl Pts',(-1.58611115600006,2.2,-3.87415869700002));
#323778=CARTESIAN_POINT('Ctrl Pts',(-1.58623409500006,12.2,-3.87562744000002));
#323779=CARTESIAN_POINT('Ctrl Pts',(-1.58623409500006,5.2,-3.87562744000002));
#323780=CARTESIAN_POINT('Ctrl Pts',(-1.58623409500006,2.2,-3.87562744000002));
#323781=CARTESIAN_POINT('Ctrl Pts',(-1.58635570200006,12.2,-3.87710105900001));
#323782=CARTESIAN_POINT('Ctrl Pts',(-1.58635570200006,5.2,-3.87710105900001));
#323783=CARTESIAN_POINT('Ctrl Pts',(-1.58635570200006,2.2,-3.87710105900001));
#323784=CARTESIAN_POINT('Ctrl Pts',(-1.58647596900006,12.2,-3.87857954800001));
#323785=CARTESIAN_POINT('Ctrl Pts',(-1.58647596900006,5.2,-3.87857954800001));
#323786=CARTESIAN_POINT('Ctrl Pts',(-1.58647596900006,2.2,-3.87857954800001));
#323787=CARTESIAN_POINT('Ctrl Pts',(-1.58659488300006,12.2,-3.88006289700002));
#323788=CARTESIAN_POINT('Ctrl Pts',(-1.58659488300006,5.2,-3.88006289700002));
#323789=CARTESIAN_POINT('Ctrl Pts',(-1.58659488300006,2.2,-3.88006289700002));
#323790=CARTESIAN_POINT('Ctrl Pts',(-1.58671243300006,12.2,-3.88155110200001));
#323791=CARTESIAN_POINT('Ctrl Pts',(-1.58671243300006,5.2,-3.88155110200001));
#323792=CARTESIAN_POINT('Ctrl Pts',(-1.58671243300006,2.2,-3.88155110200001));
#323793=CARTESIAN_POINT('Ctrl Pts',(-1.58682861100006,12.2,-3.88304415200002));
#323794=CARTESIAN_POINT('Ctrl Pts',(-1.58682861100006,5.2,-3.88304415200002));
#323795=CARTESIAN_POINT('Ctrl Pts',(-1.58682861100006,2.2,-3.88304415200002));
#323796=CARTESIAN_POINT('Ctrl Pts',(-1.58694340200006,12.2,-3.88454203900002));
#323797=CARTESIAN_POINT('Ctrl Pts',(-1.58694340200006,5.2,-3.88454203900002));
#323798=CARTESIAN_POINT('Ctrl Pts',(-1.58694340200006,2.2,-3.88454203900002));
#323799=CARTESIAN_POINT('Ctrl Pts',(-1.58705679800006,12.2,-3.88604475700001));
#323800=CARTESIAN_POINT('Ctrl Pts',(-1.58705679800006,5.2,-3.88604475700001));
#323801=CARTESIAN_POINT('Ctrl Pts',(-1.58705679800006,2.2,-3.88604475700001));
#323802=CARTESIAN_POINT('Ctrl Pts',(-1.58716878700006,12.2,-3.88755229700001));
#323803=CARTESIAN_POINT('Ctrl Pts',(-1.58716878700006,5.2,-3.88755229700001));
#323804=CARTESIAN_POINT('Ctrl Pts',(-1.58716878700006,2.2,-3.88755229700001));
#323805=CARTESIAN_POINT('Ctrl Pts',(-1.58727936000005,12.2,-3.88906465100002));
#323806=CARTESIAN_POINT('Ctrl Pts',(-1.58727936000005,5.2,-3.88906465100002));
#323807=CARTESIAN_POINT('Ctrl Pts',(-1.58727936000005,2.2,-3.88906465100002));
#323808=CARTESIAN_POINT('Ctrl Pts',(-1.58738850400006,12.2,-3.89058181300001));
#323809=CARTESIAN_POINT('Ctrl Pts',(-1.58738850400006,5.2,-3.89058181300001));
#323810=CARTESIAN_POINT('Ctrl Pts',(-1.58738850400006,2.2,-3.89058181300001));
#323811=CARTESIAN_POINT('Ctrl Pts',(-1.58749621100006,12.2,-3.89210377300001));
#323812=CARTESIAN_POINT('Ctrl Pts',(-1.58749621100006,5.2,-3.89210377300001));
#323813=CARTESIAN_POINT('Ctrl Pts',(-1.58749621100006,2.2,-3.89210377300001));
#323814=CARTESIAN_POINT('Ctrl Pts',(-1.58760246700006,12.2,-3.89363052400002));
#323815=CARTESIAN_POINT('Ctrl Pts',(-1.58760246700006,5.2,-3.89363052400002));
#323816=CARTESIAN_POINT('Ctrl Pts',(-1.58760246700006,2.2,-3.89363052400002));
#323817=CARTESIAN_POINT('Ctrl Pts',(-1.58770726400005,12.2,-3.89516205800001));
#323818=CARTESIAN_POINT('Ctrl Pts',(-1.58770726400005,5.2,-3.89516205800001));
#323819=CARTESIAN_POINT('Ctrl Pts',(-1.58770726400005,2.2,-3.89516205800001));
#323820=CARTESIAN_POINT('Ctrl Pts',(-1.58781059000005,12.2,-3.89669836700001));
#323821=CARTESIAN_POINT('Ctrl Pts',(-1.58781059000005,5.2,-3.89669836700001));
#323822=CARTESIAN_POINT('Ctrl Pts',(-1.58781059000005,2.2,-3.89669836700001));
#323823=CARTESIAN_POINT('Ctrl Pts',(-1.58791243700006,12.2,-3.89823944300002));
#323824=CARTESIAN_POINT('Ctrl Pts',(-1.58791243700006,5.2,-3.89823944300002));
#323825=CARTESIAN_POINT('Ctrl Pts',(-1.58791243700006,2.2,-3.89823944300002));
#323826=CARTESIAN_POINT('Ctrl Pts',(-1.58801279100006,12.2,-3.89978528000002));
#323827=CARTESIAN_POINT('Ctrl Pts',(-1.58801279100006,5.2,-3.89978528000002));
#323828=CARTESIAN_POINT('Ctrl Pts',(-1.58801279100006,2.2,-3.89978528000002));
#323829=CARTESIAN_POINT('Ctrl Pts',(-1.58811164400006,12.2,-3.90133586700002));
#323830=CARTESIAN_POINT('Ctrl Pts',(-1.58811164400006,5.2,-3.90133586700002));
#323831=CARTESIAN_POINT('Ctrl Pts',(-1.58811164400006,2.2,-3.90133586700002));
#323832=CARTESIAN_POINT('Ctrl Pts',(-1.58820898400006,12.2,-3.90289119900002));
#323833=CARTESIAN_POINT('Ctrl Pts',(-1.58820898400006,5.2,-3.90289119900002));
#323834=CARTESIAN_POINT('Ctrl Pts',(-1.58820898400006,2.2,-3.90289119900002));
#323835=CARTESIAN_POINT('Ctrl Pts',(-1.58830480300006,12.2,-3.90445126600001));
#323836=CARTESIAN_POINT('Ctrl Pts',(-1.58830480300006,5.2,-3.90445126600001));
#323837=CARTESIAN_POINT('Ctrl Pts',(-1.58830480300006,2.2,-3.90445126600001));
#323838=CARTESIAN_POINT('Ctrl Pts',(-1.58839908700006,12.2,-3.90601606200002));
#323839=CARTESIAN_POINT('Ctrl Pts',(-1.58839908700006,5.2,-3.90601606200002));
#323840=CARTESIAN_POINT('Ctrl Pts',(-1.58839908700006,2.2,-3.90601606200002));
#323841=CARTESIAN_POINT('Ctrl Pts',(-1.58849182800005,12.2,-3.90758557700002));
#323842=CARTESIAN_POINT('Ctrl Pts',(-1.58849182800005,5.2,-3.90758557700002));
#323843=CARTESIAN_POINT('Ctrl Pts',(-1.58849182800005,2.2,-3.90758557700002));
#323844=CARTESIAN_POINT('Ctrl Pts',(-1.58858301700006,12.2,-3.90915980500001));
#323845=CARTESIAN_POINT('Ctrl Pts',(-1.58858301700006,5.2,-3.90915980500001));
#323846=CARTESIAN_POINT('Ctrl Pts',(-1.58858301700006,2.2,-3.90915980500001));
#323847=CARTESIAN_POINT('Ctrl Pts',(-1.58867264000006,12.2,-3.91073873900002));
#323848=CARTESIAN_POINT('Ctrl Pts',(-1.58867264000006,5.2,-3.91073873900002));
#323849=CARTESIAN_POINT('Ctrl Pts',(-1.58867264000006,2.2,-3.91073873900002));
#323850=CARTESIAN_POINT('Ctrl Pts',(-1.58876068900006,12.2,-3.91232236800001));
#323851=CARTESIAN_POINT('Ctrl Pts',(-1.58876068900006,5.2,-3.91232236800001));
#323852=CARTESIAN_POINT('Ctrl Pts',(-1.58876068900006,2.2,-3.91232236800001));
#323853=CARTESIAN_POINT('Ctrl Pts',(-1.58884715500006,12.2,-3.91391068700001));
#323854=CARTESIAN_POINT('Ctrl Pts',(-1.58884715500006,5.2,-3.91391068700001));
#323855=CARTESIAN_POINT('Ctrl Pts',(-1.58884715500006,2.2,-3.91391068700001));
#323856=CARTESIAN_POINT('Ctrl Pts',(-1.58893202500006,12.2,-3.91550368600001));
#323857=CARTESIAN_POINT('Ctrl Pts',(-1.58893202500006,5.2,-3.91550368600001));
#323858=CARTESIAN_POINT('Ctrl Pts',(-1.58893202500006,2.2,-3.91550368600001));
#323859=CARTESIAN_POINT('Ctrl Pts',(-1.58901529100006,12.2,-3.91710135900002));
#323860=CARTESIAN_POINT('Ctrl Pts',(-1.58901529100006,5.2,-3.91710135900002));
#323861=CARTESIAN_POINT('Ctrl Pts',(-1.58901529100006,2.2,-3.91710135900002));
#323862=CARTESIAN_POINT('Ctrl Pts',(-1.58909694200006,12.2,-3.91870369900001));
#323863=CARTESIAN_POINT('Ctrl Pts',(-1.58909694200006,5.2,-3.91870369900001));
#323864=CARTESIAN_POINT('Ctrl Pts',(-1.58909694200006,2.2,-3.91870369900001));
#323865=CARTESIAN_POINT('Ctrl Pts',(-1.58917696700006,12.2,-3.92031069400002));
#323866=CARTESIAN_POINT('Ctrl Pts',(-1.58917696700006,5.2,-3.92031069400002));
#323867=CARTESIAN_POINT('Ctrl Pts',(-1.58917696700006,2.2,-3.92031069400002));
#323868=CARTESIAN_POINT('Ctrl Pts',(-1.58925535800006,12.2,-3.92192234100001));
#323869=CARTESIAN_POINT('Ctrl Pts',(-1.58925535800006,5.2,-3.92192234100001));
#323870=CARTESIAN_POINT('Ctrl Pts',(-1.58925535800006,2.2,-3.92192234100001));
#323871=CARTESIAN_POINT('Ctrl Pts',(-1.58933210400006,12.2,-3.92353862800002));
#323872=CARTESIAN_POINT('Ctrl Pts',(-1.58933210400006,5.2,-3.92353862800002));
#323873=CARTESIAN_POINT('Ctrl Pts',(-1.58933210400006,2.2,-3.92353862800002));
#323874=CARTESIAN_POINT('Ctrl Pts',(-1.58940719400006,12.2,-3.92515955000002));
#323875=CARTESIAN_POINT('Ctrl Pts',(-1.58940719400006,5.2,-3.92515955000002));
#323876=CARTESIAN_POINT('Ctrl Pts',(-1.58940719400006,2.2,-3.92515955000002));
#323877=CARTESIAN_POINT('Ctrl Pts',(-1.58948062000006,12.2,-3.92678509900001));
#323878=CARTESIAN_POINT('Ctrl Pts',(-1.58948062000006,5.2,-3.92678509900001));
#323879=CARTESIAN_POINT('Ctrl Pts',(-1.58948062000006,2.2,-3.92678509900001));
#323880=CARTESIAN_POINT('Ctrl Pts',(-1.58955237000006,12.2,-3.92841526600002));
#323881=CARTESIAN_POINT('Ctrl Pts',(-1.58955237000006,5.2,-3.92841526600002));
#323882=CARTESIAN_POINT('Ctrl Pts',(-1.58955237000006,2.2,-3.92841526600002));
#323883=CARTESIAN_POINT('Ctrl Pts',(-1.58962243600006,12.2,-3.93005004400001));
#323884=CARTESIAN_POINT('Ctrl Pts',(-1.58962243600006,5.2,-3.93005004400001));
#323885=CARTESIAN_POINT('Ctrl Pts',(-1.58962243600006,2.2,-3.93005004400001));
#323886=CARTESIAN_POINT('Ctrl Pts',(-1.58969080700006,12.2,-3.93168942500001));
#323887=CARTESIAN_POINT('Ctrl Pts',(-1.58969080700006,5.2,-3.93168942500001));
#323888=CARTESIAN_POINT('Ctrl Pts',(-1.58969080700006,2.2,-3.93168942500001));
#323889=CARTESIAN_POINT('Ctrl Pts',(-1.58975747200006,12.2,-3.93333340100002));
#323890=CARTESIAN_POINT('Ctrl Pts',(-1.58975747200006,5.2,-3.93333340100002));
#323891=CARTESIAN_POINT('Ctrl Pts',(-1.58975747200006,2.2,-3.93333340100002));
#323892=CARTESIAN_POINT('Ctrl Pts',(-1.58982242300006,12.2,-3.93498196400001));
#323893=CARTESIAN_POINT('Ctrl Pts',(-1.58982242300006,5.2,-3.93498196400001));
#323894=CARTESIAN_POINT('Ctrl Pts',(-1.58982242300006,2.2,-3.93498196400001));
#323895=CARTESIAN_POINT('Ctrl Pts',(-1.58988565000006,12.2,-3.93663510600001));
#323896=CARTESIAN_POINT('Ctrl Pts',(-1.58988565000006,5.2,-3.93663510600001));
#323897=CARTESIAN_POINT('Ctrl Pts',(-1.58988565000006,2.2,-3.93663510600001));
#323898=CARTESIAN_POINT('Ctrl Pts',(-1.58994714200006,12.2,-3.93829282200001));
#323899=CARTESIAN_POINT('Ctrl Pts',(-1.58994714200006,5.2,-3.93829282200001));
#323900=CARTESIAN_POINT('Ctrl Pts',(-1.58994714200006,2.2,-3.93829282200001));
#323901=CARTESIAN_POINT('Ctrl Pts',(-1.59000689100006,12.2,-3.93995509900002));
#323902=CARTESIAN_POINT('Ctrl Pts',(-1.59000689100006,5.2,-3.93995509900002));
#323903=CARTESIAN_POINT('Ctrl Pts',(-1.59000689100006,2.2,-3.93995509900002));
#323904=CARTESIAN_POINT('Ctrl Pts',(-1.59006488600005,12.2,-3.94162193300001));
#323905=CARTESIAN_POINT('Ctrl Pts',(-1.59006488600005,5.2,-3.94162193300001));
#323906=CARTESIAN_POINT('Ctrl Pts',(-1.59006488600005,2.2,-3.94162193300001));
#323907=CARTESIAN_POINT('Ctrl Pts',(-1.59012111700006,12.2,-3.94329331600002));
#323908=CARTESIAN_POINT('Ctrl Pts',(-1.59012111700006,5.2,-3.94329331600002));
#323909=CARTESIAN_POINT('Ctrl Pts',(-1.59012111700006,2.2,-3.94329331600002));
#323910=CARTESIAN_POINT('Ctrl Pts',(-1.59017557600006,12.2,-3.94496923900002));
#323911=CARTESIAN_POINT('Ctrl Pts',(-1.59017557600006,5.2,-3.94496923900002));
#323912=CARTESIAN_POINT('Ctrl Pts',(-1.59017557600006,2.2,-3.94496923900002));
#323913=CARTESIAN_POINT('Ctrl Pts',(-1.59022825200006,12.2,-3.94664969400001));
#323914=CARTESIAN_POINT('Ctrl Pts',(-1.59022825200006,5.2,-3.94664969400001));
#323915=CARTESIAN_POINT('Ctrl Pts',(-1.59022825200006,2.2,-3.94664969400001));
#323916=CARTESIAN_POINT('Ctrl Pts',(-1.59027913600006,12.2,-3.94833467500002));
#323917=CARTESIAN_POINT('Ctrl Pts',(-1.59027913600006,5.2,-3.94833467500002));
#323918=CARTESIAN_POINT('Ctrl Pts',(-1.59027913600006,2.2,-3.94833467500002));
#323919=CARTESIAN_POINT('Ctrl Pts',(-1.59032821800006,12.2,-3.95002417200002));
#323920=CARTESIAN_POINT('Ctrl Pts',(-1.59032821800006,5.2,-3.95002417200002));
#323921=CARTESIAN_POINT('Ctrl Pts',(-1.59032821800006,2.2,-3.95002417200002));
#323922=CARTESIAN_POINT('Ctrl Pts',(-1.59037548900006,12.2,-3.95171817900001));
#323923=CARTESIAN_POINT('Ctrl Pts',(-1.59037548900006,5.2,-3.95171817900001));
#323924=CARTESIAN_POINT('Ctrl Pts',(-1.59037548900006,2.2,-3.95171817900001));
#323925=CARTESIAN_POINT('Ctrl Pts',(-1.59042093900006,12.2,-3.95341668700001));
#323926=CARTESIAN_POINT('Ctrl Pts',(-1.59042093900006,5.2,-3.95341668700001));
#323927=CARTESIAN_POINT('Ctrl Pts',(-1.59042093900006,2.2,-3.95341668700001));
#323928=CARTESIAN_POINT('Ctrl Pts',(-1.59046455800006,12.2,-3.95511968800002));
#323929=CARTESIAN_POINT('Ctrl Pts',(-1.59046455800006,5.2,-3.95511968800002));
#323930=CARTESIAN_POINT('Ctrl Pts',(-1.59046455800006,2.2,-3.95511968800002));
#323931=CARTESIAN_POINT('Ctrl Pts',(-1.59050633700006,12.2,-3.95682717600002));
#323932=CARTESIAN_POINT('Ctrl Pts',(-1.59050633700006,5.2,-3.95682717600002));
#323933=CARTESIAN_POINT('Ctrl Pts',(-1.59050633700006,2.2,-3.95682717600002));
#323934=CARTESIAN_POINT('Ctrl Pts',(-1.59054626700006,12.2,-3.95853914200002));
#323935=CARTESIAN_POINT('Ctrl Pts',(-1.59054626700006,5.2,-3.95853914200002));
#323936=CARTESIAN_POINT('Ctrl Pts',(-1.59054626700006,2.2,-3.95853914200002));
#323937=CARTESIAN_POINT('Ctrl Pts',(-1.59058434000006,12.2,-3.96025557800002));
#323938=CARTESIAN_POINT('Ctrl Pts',(-1.59058434000006,5.2,-3.96025557800002));
#323939=CARTESIAN_POINT('Ctrl Pts',(-1.59058434000006,2.2,-3.96025557800002));
#323940=CARTESIAN_POINT('Ctrl Pts',(-1.59062054300006,12.2,-3.96197647600002));
#323941=CARTESIAN_POINT('Ctrl Pts',(-1.59062054300006,5.2,-3.96197647600002));
#323942=CARTESIAN_POINT('Ctrl Pts',(-1.59062054300006,2.2,-3.96197647600002));
#323943=CARTESIAN_POINT('Ctrl Pts',(-1.59065486900006,12.2,-3.96370182900001));
#323944=CARTESIAN_POINT('Ctrl Pts',(-1.59065486900006,5.2,-3.96370182900001));
#323945=CARTESIAN_POINT('Ctrl Pts',(-1.59065486900006,2.2,-3.96370182900001));
#323946=CARTESIAN_POINT('Ctrl Pts',(-1.59068730800006,12.2,-3.96543163000001));
#323947=CARTESIAN_POINT('Ctrl Pts',(-1.59068730800006,5.2,-3.96543163000001));
#323948=CARTESIAN_POINT('Ctrl Pts',(-1.59068730800006,2.2,-3.96543163000001));
#323949=CARTESIAN_POINT('Ctrl Pts',(-1.59071785200006,12.2,-3.96716586900002));
#323950=CARTESIAN_POINT('Ctrl Pts',(-1.59071785200006,5.2,-3.96716586900002));
#323951=CARTESIAN_POINT('Ctrl Pts',(-1.59071785200006,2.2,-3.96716586900002));
#323952=CARTESIAN_POINT('Ctrl Pts',(-1.59074649000006,12.2,-3.96890453900001));
#323953=CARTESIAN_POINT('Ctrl Pts',(-1.59074649000006,5.2,-3.96890453900001));
#323954=CARTESIAN_POINT('Ctrl Pts',(-1.59074649000006,2.2,-3.96890453900001));
#323955=CARTESIAN_POINT('Ctrl Pts',(-1.59077321300006,12.2,-3.97064763300001));
#323956=CARTESIAN_POINT('Ctrl Pts',(-1.59077321300006,5.2,-3.97064763300001));
#323957=CARTESIAN_POINT('Ctrl Pts',(-1.59077321300006,2.2,-3.97064763300001));
#323958=CARTESIAN_POINT('Ctrl Pts',(-1.59079801300006,12.2,-3.97239514300002));
#323959=CARTESIAN_POINT('Ctrl Pts',(-1.59079801300006,5.2,-3.97239514300002));
#323960=CARTESIAN_POINT('Ctrl Pts',(-1.59079801300006,2.2,-3.97239514300002));
#323961=CARTESIAN_POINT('Ctrl Pts',(-1.59082087900006,12.2,-3.97414706000002));
#323962=CARTESIAN_POINT('Ctrl Pts',(-1.59082087900006,5.2,-3.97414706000002));
#323963=CARTESIAN_POINT('Ctrl Pts',(-1.59082087900006,2.2,-3.97414706000002));
#323964=CARTESIAN_POINT('Ctrl Pts',(-1.59084180300006,12.2,-3.97590337900001));
#323965=CARTESIAN_POINT('Ctrl Pts',(-1.59084180300006,5.2,-3.97590337900001));
#323966=CARTESIAN_POINT('Ctrl Pts',(-1.59084180300006,2.2,-3.97590337900001));
#323967=CARTESIAN_POINT('Ctrl Pts',(-1.59086077700006,12.2,-3.97766408900001));
#323968=CARTESIAN_POINT('Ctrl Pts',(-1.59086077700006,5.2,-3.97766408900001));
#323969=CARTESIAN_POINT('Ctrl Pts',(-1.59086077700006,2.2,-3.97766408900001));
#323970=CARTESIAN_POINT('Ctrl Pts',(-1.59087779000005,12.2,-3.97942918500001));
#323971=CARTESIAN_POINT('Ctrl Pts',(-1.59087779000005,5.2,-3.97942918500001));
#323972=CARTESIAN_POINT('Ctrl Pts',(-1.59087779000005,2.2,-3.97942918500001));
#323973=CARTESIAN_POINT('Ctrl Pts',(-1.59089283300006,12.2,-3.98119865700002));
#323974=CARTESIAN_POINT('Ctrl Pts',(-1.59089283300006,5.2,-3.98119865700002));
#323975=CARTESIAN_POINT('Ctrl Pts',(-1.59089283300006,2.2,-3.98119865700002));
#323976=CARTESIAN_POINT('Ctrl Pts',(-1.59090589800006,12.2,-3.98297249800001));
#323977=CARTESIAN_POINT('Ctrl Pts',(-1.59090589800006,5.2,-3.98297249800001));
#323978=CARTESIAN_POINT('Ctrl Pts',(-1.59090589800006,2.2,-3.98297249800001));
#323979=CARTESIAN_POINT('Ctrl Pts',(-1.59091697500006,12.2,-3.98475070100002));
#323980=CARTESIAN_POINT('Ctrl Pts',(-1.59091697500006,5.2,-3.98475070100002));
#323981=CARTESIAN_POINT('Ctrl Pts',(-1.59091697500006,2.2,-3.98475070100002));
#323982=CARTESIAN_POINT('Ctrl Pts',(-1.59092605600006,12.2,-3.98653325700002));
#323983=CARTESIAN_POINT('Ctrl Pts',(-1.59092605600006,5.2,-3.98653325700002));
#323984=CARTESIAN_POINT('Ctrl Pts',(-1.59092605600006,2.2,-3.98653325700002));
#323985=CARTESIAN_POINT('Ctrl Pts',(-1.59093313200006,12.2,-3.98832015800001));
#323986=CARTESIAN_POINT('Ctrl Pts',(-1.59093313200006,5.2,-3.98832015800001));
#323987=CARTESIAN_POINT('Ctrl Pts',(-1.59093313200006,2.2,-3.98832015800001));
#323988=CARTESIAN_POINT('Ctrl Pts',(-1.59093819200006,12.2,-3.99011139900002));
#323989=CARTESIAN_POINT('Ctrl Pts',(-1.59093819200006,5.2,-3.99011139900002));
#323990=CARTESIAN_POINT('Ctrl Pts',(-1.59093819200006,2.2,-3.99011139900002));
#323991=CARTESIAN_POINT('Ctrl Pts',(-1.59094123000005,12.2,-3.99190697000002));
#323992=CARTESIAN_POINT('Ctrl Pts',(-1.59094123000005,5.2,-3.99190697000002));
#323993=CARTESIAN_POINT('Ctrl Pts',(-1.59094123000005,2.2,-3.99190697000002));
#323994=CARTESIAN_POINT('Ctrl Pts',(-1.59094223500006,12.2,-3.99370686200001));
#323995=CARTESIAN_POINT('Ctrl Pts',(-1.59094223500006,5.2,-3.99370686200001));
#323996=CARTESIAN_POINT('Ctrl Pts',(-1.59094223500006,2.2,-3.99370686200001));
#323997=CARTESIAN_POINT('Ctrl Pts',(-1.59094120000006,12.2,-3.99551107000002));
#323998=CARTESIAN_POINT('Ctrl Pts',(-1.59094120000006,5.2,-3.99551107000002));
#323999=CARTESIAN_POINT('Ctrl Pts',(-1.59094120000006,2.2,-3.99551107000002));
#324000=CARTESIAN_POINT('Ctrl Pts',(-1.59093811300006,12.2,-3.99731958500002));
#324001=CARTESIAN_POINT('Ctrl Pts',(-1.59093811300006,5.2,-3.99731958500002));
#324002=CARTESIAN_POINT('Ctrl Pts',(-1.59093811300006,2.2,-3.99731958500002));
#324003=CARTESIAN_POINT('Ctrl Pts',(-1.59093296700005,12.2,-3.99913239900001));
#324004=CARTESIAN_POINT('Ctrl Pts',(-1.59093296700005,5.2,-3.99913239900001));
#324005=CARTESIAN_POINT('Ctrl Pts',(-1.59093296700005,2.2,-3.99913239900001));
#324006=CARTESIAN_POINT('Ctrl Pts',(-1.59092575600006,12.2,-4.00094950500002));
#324007=CARTESIAN_POINT('Ctrl Pts',(-1.59092575600006,5.2,-4.00094950500002));
#324008=CARTESIAN_POINT('Ctrl Pts',(-1.59092575600006,2.2,-4.00094950500002));
#324009=CARTESIAN_POINT('Ctrl Pts',(-1.59091646700006,12.2,-4.00277089400001));
#324010=CARTESIAN_POINT('Ctrl Pts',(-1.59091646700006,5.2,-4.00277089400001));
#324011=CARTESIAN_POINT('Ctrl Pts',(-1.59091646700006,2.2,-4.00277089400001));
#324012=CARTESIAN_POINT('Ctrl Pts',(-1.59090509200006,12.2,-4.00459656000002));
#324013=CARTESIAN_POINT('Ctrl Pts',(-1.59090509200006,5.2,-4.00459656000002));
#324014=CARTESIAN_POINT('Ctrl Pts',(-1.59090509200006,2.2,-4.00459656000002));
#324015=CARTESIAN_POINT('Ctrl Pts',(-1.59089162400006,12.2,-4.00642649300002));
#324016=CARTESIAN_POINT('Ctrl Pts',(-1.59089162400006,5.2,-4.00642649300002));
#324017=CARTESIAN_POINT('Ctrl Pts',(-1.59089162400006,2.2,-4.00642649300002));
#324018=CARTESIAN_POINT('Ctrl Pts',(-1.59087605400006,12.2,-4.00826068700002));
#324019=CARTESIAN_POINT('Ctrl Pts',(-1.59087605400006,5.2,-4.00826068700002));
#324020=CARTESIAN_POINT('Ctrl Pts',(-1.59087605400006,2.2,-4.00826068700002));
#324021=CARTESIAN_POINT('Ctrl Pts',(-1.59085837300006,12.2,-4.01009913300001));
#324022=CARTESIAN_POINT('Ctrl Pts',(-1.59085837300006,5.2,-4.01009913300001));
#324023=CARTESIAN_POINT('Ctrl Pts',(-1.59085837300006,2.2,-4.01009913300001));
#324024=CARTESIAN_POINT('Ctrl Pts',(-1.59083857100006,12.2,-4.01194182600001));
#324025=CARTESIAN_POINT('Ctrl Pts',(-1.59083857100006,5.2,-4.01194182600001));
#324026=CARTESIAN_POINT('Ctrl Pts',(-1.59083857100006,2.2,-4.01194182600001));
#324027=CARTESIAN_POINT('Ctrl Pts',(-1.59081664100006,12.2,-4.01378875500002));
#324028=CARTESIAN_POINT('Ctrl Pts',(-1.59081664100006,5.2,-4.01378875500002));
#324029=CARTESIAN_POINT('Ctrl Pts',(-1.59081664100006,2.2,-4.01378875500002));
#324030=CARTESIAN_POINT('Ctrl Pts',(-1.59079257400006,12.2,-4.01563991400002));
#324031=CARTESIAN_POINT('Ctrl Pts',(-1.59079257400006,5.2,-4.01563991400002));
#324032=CARTESIAN_POINT('Ctrl Pts',(-1.59079257400006,2.2,-4.01563991400002));
#324033=CARTESIAN_POINT('Ctrl Pts',(-1.59076636100006,12.2,-4.01749529400002));
#324034=CARTESIAN_POINT('Ctrl Pts',(-1.59076636100006,5.2,-4.01749529400002));
#324035=CARTESIAN_POINT('Ctrl Pts',(-1.59076636100006,2.2,-4.01749529400002));
#324036=CARTESIAN_POINT('Ctrl Pts',(-1.59073799500006,12.2,-4.01935488800001));
#324037=CARTESIAN_POINT('Ctrl Pts',(-1.59073799500006,5.2,-4.01935488800001));
#324038=CARTESIAN_POINT('Ctrl Pts',(-1.59073799500006,2.2,-4.01935488800001));
#324039=CARTESIAN_POINT('Ctrl Pts',(-1.59070746500006,12.2,-4.02121868900001));
#324040=CARTESIAN_POINT('Ctrl Pts',(-1.59070746500006,5.2,-4.02121868900001));
#324041=CARTESIAN_POINT('Ctrl Pts',(-1.59070746500006,2.2,-4.02121868900001));
#324042=CARTESIAN_POINT('Ctrl Pts',(-1.59067476500006,12.2,-4.02308668800002));
#324043=CARTESIAN_POINT('Ctrl Pts',(-1.59067476500006,5.2,-4.02308668800002));
#324044=CARTESIAN_POINT('Ctrl Pts',(-1.59067476500006,2.2,-4.02308668800002));
#324045=CARTESIAN_POINT('Ctrl Pts',(-1.59063988400006,12.2,-4.02495887800002));
#324046=CARTESIAN_POINT('Ctrl Pts',(-1.59063988400006,5.2,-4.02495887800002));
#324047=CARTESIAN_POINT('Ctrl Pts',(-1.59063988400006,2.2,-4.02495887800002));
#324048=CARTESIAN_POINT('Ctrl Pts',(-1.59060281600006,12.2,-4.02683525200001));
#324049=CARTESIAN_POINT('Ctrl Pts',(-1.59060281600006,5.2,-4.02683525200001));
#324050=CARTESIAN_POINT('Ctrl Pts',(-1.59060281600006,2.2,-4.02683525200001));
#324051=CARTESIAN_POINT('Ctrl Pts',(-1.59056355200006,12.2,-4.02871580100001));
#324052=CARTESIAN_POINT('Ctrl Pts',(-1.59056355200006,5.2,-4.02871580100001));
#324053=CARTESIAN_POINT('Ctrl Pts',(-1.59056355200006,2.2,-4.02871580100001));
#324054=CARTESIAN_POINT('Ctrl Pts',(-1.59052208200006,12.2,-4.03060051700002));
#324055=CARTESIAN_POINT('Ctrl Pts',(-1.59052208200006,5.2,-4.03060051700002));
#324056=CARTESIAN_POINT('Ctrl Pts',(-1.59052208200006,2.2,-4.03060051700002));
#324057=CARTESIAN_POINT('Ctrl Pts',(-1.59047840000006,12.2,-4.03248939400001));
#324058=CARTESIAN_POINT('Ctrl Pts',(-1.59047840000006,5.2,-4.03248939400001));
#324059=CARTESIAN_POINT('Ctrl Pts',(-1.59047840000006,2.2,-4.03248939400001));
#324060=CARTESIAN_POINT('Ctrl Pts',(-1.59043249400006,12.2,-4.03438242200002));
#324061=CARTESIAN_POINT('Ctrl Pts',(-1.59043249400006,5.2,-4.03438242200002));
#324062=CARTESIAN_POINT('Ctrl Pts',(-1.59043249400006,2.2,-4.03438242200002));
#324063=CARTESIAN_POINT('Ctrl Pts',(-1.59038436000006,12.2,-4.03627959500001));
#324064=CARTESIAN_POINT('Ctrl Pts',(-1.59038436000006,5.2,-4.03627959500001));
#324065=CARTESIAN_POINT('Ctrl Pts',(-1.59038436000006,2.2,-4.03627959500001));
#324066=CARTESIAN_POINT('Ctrl Pts',(-1.59033398800006,12.2,-4.03818090400001));
#324067=CARTESIAN_POINT('Ctrl Pts',(-1.59033398800006,5.2,-4.03818090400001));
#324068=CARTESIAN_POINT('Ctrl Pts',(-1.59033398800006,2.2,-4.03818090400001));
#324069=CARTESIAN_POINT('Ctrl Pts',(-1.59028137000006,12.2,-4.04008634300002));
#324070=CARTESIAN_POINT('Ctrl Pts',(-1.59028137000006,5.2,-4.04008634300002));
#324071=CARTESIAN_POINT('Ctrl Pts',(-1.59028137000006,2.2,-4.04008634300002));
#324072=CARTESIAN_POINT('Ctrl Pts',(-1.59022649600006,12.2,-4.04199590300002));
#324073=CARTESIAN_POINT('Ctrl Pts',(-1.59022649600006,5.2,-4.04199590300002));
#324074=CARTESIAN_POINT('Ctrl Pts',(-1.59022649600006,2.2,-4.04199590300002));
#324075=CARTESIAN_POINT('Ctrl Pts',(-1.59016936000006,12.2,-4.04390957600001));
#324076=CARTESIAN_POINT('Ctrl Pts',(-1.59016936000006,5.2,-4.04390957600001));
#324077=CARTESIAN_POINT('Ctrl Pts',(-1.59016936000006,2.2,-4.04390957600001));
#324078=CARTESIAN_POINT('Ctrl Pts',(-1.59010995200006,12.2,-4.04582735600002));
#324079=CARTESIAN_POINT('Ctrl Pts',(-1.59010995200006,5.2,-4.04582735600002));
#324080=CARTESIAN_POINT('Ctrl Pts',(-1.59010995200006,2.2,-4.04582735600002));
#324081=CARTESIAN_POINT('Ctrl Pts',(-1.59004826600006,12.2,-4.04774923300002));
#324082=CARTESIAN_POINT('Ctrl Pts',(-1.59004826600006,5.2,-4.04774923300002));
#324083=CARTESIAN_POINT('Ctrl Pts',(-1.59004826600006,2.2,-4.04774923300002));
#324084=CARTESIAN_POINT('Ctrl Pts',(-1.58998429200006,12.2,-4.04967520200001));
#324085=CARTESIAN_POINT('Ctrl Pts',(-1.58998429200006,5.2,-4.04967520200001));
#324086=CARTESIAN_POINT('Ctrl Pts',(-1.58998429200006,2.2,-4.04967520200001));
#324087=CARTESIAN_POINT('Ctrl Pts',(-1.58991802200006,12.2,-4.05160525300001));
#324088=CARTESIAN_POINT('Ctrl Pts',(-1.58991802200006,5.2,-4.05160525300001));
#324089=CARTESIAN_POINT('Ctrl Pts',(-1.58991802200006,2.2,-4.05160525300001));
#324090=CARTESIAN_POINT('Ctrl Pts',(-1.58984944900005,12.2,-4.05353937800002));
#324091=CARTESIAN_POINT('Ctrl Pts',(-1.58984944900005,5.2,-4.05353937800002));
#324092=CARTESIAN_POINT('Ctrl Pts',(-1.58984944900005,2.2,-4.05353937800002));
#324093=CARTESIAN_POINT('Ctrl Pts',(-1.58977856400006,12.2,-4.05547757100001));
#324094=CARTESIAN_POINT('Ctrl Pts',(-1.58977856400006,5.2,-4.05547757100001));
#324095=CARTESIAN_POINT('Ctrl Pts',(-1.58977856400006,2.2,-4.05547757100001));
#324096=CARTESIAN_POINT('Ctrl Pts',(-1.58970535900006,12.2,-4.05741982400002));
#324097=CARTESIAN_POINT('Ctrl Pts',(-1.58970535900006,5.2,-4.05741982400002));
#324098=CARTESIAN_POINT('Ctrl Pts',(-1.58970535900006,2.2,-4.05741982400002));
#324099=CARTESIAN_POINT('Ctrl Pts',(-1.58962982700006,12.2,-4.05936612800001));
#324100=CARTESIAN_POINT('Ctrl Pts',(-1.58962982700006,5.2,-4.05936612800001));
#324101=CARTESIAN_POINT('Ctrl Pts',(-1.58962982700006,2.2,-4.05936612800001));
#324102=CARTESIAN_POINT('Ctrl Pts',(-1.58955195800006,12.2,-4.06131647700001));
#324103=CARTESIAN_POINT('Ctrl Pts',(-1.58955195800006,5.2,-4.06131647700001));
#324104=CARTESIAN_POINT('Ctrl Pts',(-1.58955195800006,2.2,-4.06131647700001));
#324105=CARTESIAN_POINT('Ctrl Pts',(-1.58947174700006,12.2,-4.06327086300001));
#324106=CARTESIAN_POINT('Ctrl Pts',(-1.58947174700006,5.2,-4.06327086300001));
#324107=CARTESIAN_POINT('Ctrl Pts',(-1.58947174700006,2.2,-4.06327086300001));
#324108=CARTESIAN_POINT('Ctrl Pts',(-1.58938918300006,12.2,-4.06522927600002));
#324109=CARTESIAN_POINT('Ctrl Pts',(-1.58938918300006,5.2,-4.06522927600002));
#324110=CARTESIAN_POINT('Ctrl Pts',(-1.58938918300006,2.2,-4.06522927600002));
#324111=CARTESIAN_POINT('Ctrl Pts',(-1.58930425900006,12.2,-4.06719171200002));
#324112=CARTESIAN_POINT('Ctrl Pts',(-1.58930425900006,5.2,-4.06719171200002));
#324113=CARTESIAN_POINT('Ctrl Pts',(-1.58930425900006,2.2,-4.06719171200002));
#324114=CARTESIAN_POINT('Ctrl Pts',(-1.58921696800005,12.2,-4.06915816000001));
#324115=CARTESIAN_POINT('Ctrl Pts',(-1.58921696800005,5.2,-4.06915816000001));
#324116=CARTESIAN_POINT('Ctrl Pts',(-1.58921696800005,2.2,-4.06915816000001));
#324117=CARTESIAN_POINT('Ctrl Pts',(-1.58912730200006,12.2,-4.07112861400002));
#324118=CARTESIAN_POINT('Ctrl Pts',(-1.58912730200006,5.2,-4.07112861400002));
#324119=CARTESIAN_POINT('Ctrl Pts',(-1.58912730200006,2.2,-4.07112861400002));
#324120=CARTESIAN_POINT('Ctrl Pts',(-1.58903525200006,12.2,-4.07310306600001));
#324121=CARTESIAN_POINT('Ctrl Pts',(-1.58903525200006,5.2,-4.07310306600001));
#324122=CARTESIAN_POINT('Ctrl Pts',(-1.58903525200006,2.2,-4.07310306600001));
#324123=CARTESIAN_POINT('Ctrl Pts',(-1.58894081100006,12.2,-4.07508150900001));
#324124=CARTESIAN_POINT('Ctrl Pts',(-1.58894081100006,5.2,-4.07508150900001));
#324125=CARTESIAN_POINT('Ctrl Pts',(-1.58894081100006,2.2,-4.07508150900001));
#324126=CARTESIAN_POINT('Ctrl Pts',(-1.58884397200006,12.2,-4.07706393400002));
#324127=CARTESIAN_POINT('Ctrl Pts',(-1.58884397200006,5.2,-4.07706393400002));
#324128=CARTESIAN_POINT('Ctrl Pts',(-1.58884397200006,2.2,-4.07706393400002));
#324129=CARTESIAN_POINT('Ctrl Pts',(-1.58874472600006,12.2,-4.07905033500001));
#324130=CARTESIAN_POINT('Ctrl Pts',(-1.58874472600006,5.2,-4.07905033500001));
#324131=CARTESIAN_POINT('Ctrl Pts',(-1.58874472600006,2.2,-4.07905033500001));
#324132=CARTESIAN_POINT('Ctrl Pts',(-1.58864306500006,12.2,-4.08104070300002));
#324133=CARTESIAN_POINT('Ctrl Pts',(-1.58864306500006,5.2,-4.08104070300002));
#324134=CARTESIAN_POINT('Ctrl Pts',(-1.58864306500006,2.2,-4.08104070300002));
#324135=CARTESIAN_POINT('Ctrl Pts',(-1.58853898100005,12.2,-4.08303502800001));
#324136=CARTESIAN_POINT('Ctrl Pts',(-1.58853898100005,5.2,-4.08303502800001));
#324137=CARTESIAN_POINT('Ctrl Pts',(-1.58853898100005,2.2,-4.08303502800001));
#324138=CARTESIAN_POINT('Ctrl Pts',(-1.58843246800005,12.2,-4.08503330800002));
#324139=CARTESIAN_POINT('Ctrl Pts',(-1.58843246800005,5.2,-4.08503330800002));
#324140=CARTESIAN_POINT('Ctrl Pts',(-1.58843246800005,2.2,-4.08503330800002));
#324141=CARTESIAN_POINT('Ctrl Pts',(-1.58832351800006,12.2,-4.08703553000001));
#324142=CARTESIAN_POINT('Ctrl Pts',(-1.58832351800006,5.2,-4.08703553000001));
#324143=CARTESIAN_POINT('Ctrl Pts',(-1.58832351800006,2.2,-4.08703553000001));
#324144=CARTESIAN_POINT('Ctrl Pts',(-1.58821212100006,12.2,-4.08904169000001));
#324145=CARTESIAN_POINT('Ctrl Pts',(-1.58821212100006,5.2,-4.08904169000001));
#324146=CARTESIAN_POINT('Ctrl Pts',(-1.58821212100006,2.2,-4.08904169000001));
#324147=CARTESIAN_POINT('Ctrl Pts',(-1.58809827200006,12.2,-4.09105177800001));
#324148=CARTESIAN_POINT('Ctrl Pts',(-1.58809827200006,5.2,-4.09105177800001));
#324149=CARTESIAN_POINT('Ctrl Pts',(-1.58809827200006,2.2,-4.09105177800001));
#324150=CARTESIAN_POINT('Ctrl Pts',(-1.58798196200005,12.2,-4.09306578800001));
#324151=CARTESIAN_POINT('Ctrl Pts',(-1.58798196200005,5.2,-4.09306578800001));
#324152=CARTESIAN_POINT('Ctrl Pts',(-1.58798196200005,2.2,-4.09306578800001));
#324153=CARTESIAN_POINT('Ctrl Pts',(-1.58786318400006,12.2,-4.09508371000001));
#324154=CARTESIAN_POINT('Ctrl Pts',(-1.58786318400006,5.2,-4.09508371000001));
#324155=CARTESIAN_POINT('Ctrl Pts',(-1.58786318400006,2.2,-4.09508371000001));
#324156=CARTESIAN_POINT('Ctrl Pts',(-1.58774193000006,12.2,-4.09710553900001));
#324157=CARTESIAN_POINT('Ctrl Pts',(-1.58774193000006,5.2,-4.09710553900001));
#324158=CARTESIAN_POINT('Ctrl Pts',(-1.58774193000006,2.2,-4.09710553900001));
#324159=CARTESIAN_POINT('Ctrl Pts',(-1.58761819200006,12.2,-4.09913126700001));
#324160=CARTESIAN_POINT('Ctrl Pts',(-1.58761819200006,5.2,-4.09913126700001));
#324161=CARTESIAN_POINT('Ctrl Pts',(-1.58761819200006,2.2,-4.09913126700001));
#324162=CARTESIAN_POINT('Ctrl Pts',(-1.58749196400006,12.2,-4.10116088400001));
#324163=CARTESIAN_POINT('Ctrl Pts',(-1.58749196400006,5.2,-4.10116088400001));
#324164=CARTESIAN_POINT('Ctrl Pts',(-1.58749196400006,2.2,-4.10116088400001));
#324165=CARTESIAN_POINT('Ctrl Pts',(-1.58736323700006,12.2,-4.10319438400002));
#324166=CARTESIAN_POINT('Ctrl Pts',(-1.58736323700006,5.2,-4.10319438400002));
#324167=CARTESIAN_POINT('Ctrl Pts',(-1.58736323700006,2.2,-4.10319438400002));
#324168=CARTESIAN_POINT('Ctrl Pts',(-1.58723200500006,12.2,-4.10523176000002));
#324169=CARTESIAN_POINT('Ctrl Pts',(-1.58723200500006,5.2,-4.10523176000002));
#324170=CARTESIAN_POINT('Ctrl Pts',(-1.58723200500006,2.2,-4.10523176000002));
#324171=CARTESIAN_POINT('Ctrl Pts',(-1.58709825800006,12.2,-4.10727300300001));
#324172=CARTESIAN_POINT('Ctrl Pts',(-1.58709825800006,5.2,-4.10727300300001));
#324173=CARTESIAN_POINT('Ctrl Pts',(-1.58709825800006,2.2,-4.10727300300001));
#324174=CARTESIAN_POINT('Ctrl Pts',(-1.58696199100006,12.2,-4.10931810600002));
#324175=CARTESIAN_POINT('Ctrl Pts',(-1.58696199100006,5.2,-4.10931810600002));
#324176=CARTESIAN_POINT('Ctrl Pts',(-1.58696199100006,2.2,-4.10931810600002));
#324177=CARTESIAN_POINT('Ctrl Pts',(-1.58682319500006,12.2,-4.11136706100002));
#324178=CARTESIAN_POINT('Ctrl Pts',(-1.58682319500006,5.2,-4.11136706100002));
#324179=CARTESIAN_POINT('Ctrl Pts',(-1.58682319500006,2.2,-4.11136706100002));
#324180=CARTESIAN_POINT('Ctrl Pts',(-1.58668186400006,12.2,-4.11341985900001));
#324181=CARTESIAN_POINT('Ctrl Pts',(-1.58668186400006,5.2,-4.11341985900001));
#324182=CARTESIAN_POINT('Ctrl Pts',(-1.58668186400006,2.2,-4.11341985900001));
#324183=CARTESIAN_POINT('Ctrl Pts',(-1.58653799000006,12.2,-4.11547649600001));
#324184=CARTESIAN_POINT('Ctrl Pts',(-1.58653799000006,5.2,-4.11547649600001));
#324185=CARTESIAN_POINT('Ctrl Pts',(-1.58653799000006,2.2,-4.11547649600001));
#324186=CARTESIAN_POINT('Ctrl Pts',(-1.58639156500006,12.2,-4.11753696100002));
#324187=CARTESIAN_POINT('Ctrl Pts',(-1.58639156500006,5.2,-4.11753696100002));
#324188=CARTESIAN_POINT('Ctrl Pts',(-1.58639156500006,2.2,-4.11753696100002));
#324189=CARTESIAN_POINT('Ctrl Pts',(-1.58624258200006,12.2,-4.11960124800002));
#324190=CARTESIAN_POINT('Ctrl Pts',(-1.58624258200006,5.2,-4.11960124800002));
#324191=CARTESIAN_POINT('Ctrl Pts',(-1.58624258200006,2.2,-4.11960124800002));
#324192=CARTESIAN_POINT('Ctrl Pts',(-1.58609103400006,12.2,-4.12166934900001));
#324193=CARTESIAN_POINT('Ctrl Pts',(-1.58609103400006,5.2,-4.12166934900001));
#324194=CARTESIAN_POINT('Ctrl Pts',(-1.58609103400006,2.2,-4.12166934900001));
#324195=CARTESIAN_POINT('Ctrl Pts',(-1.58593691400006,12.2,-4.12374125600001));
#324196=CARTESIAN_POINT('Ctrl Pts',(-1.58593691400006,5.2,-4.12374125600001));
#324197=CARTESIAN_POINT('Ctrl Pts',(-1.58593691400006,2.2,-4.12374125600001));
#324198=CARTESIAN_POINT('Ctrl Pts',(-1.58578021300006,12.2,-4.12581696100002));
#324199=CARTESIAN_POINT('Ctrl Pts',(-1.58578021300006,5.2,-4.12581696100002));
#324200=CARTESIAN_POINT('Ctrl Pts',(-1.58578021300006,2.2,-4.12581696100002));
#324201=CARTESIAN_POINT('Ctrl Pts',(-1.58562092600006,12.2,-4.12789645800002));
#324202=CARTESIAN_POINT('Ctrl Pts',(-1.58562092600006,5.2,-4.12789645800002));
#324203=CARTESIAN_POINT('Ctrl Pts',(-1.58562092600006,2.2,-4.12789645800002));
#324204=CARTESIAN_POINT('Ctrl Pts',(-1.58545904500006,12.2,-4.12997973800001));
#324205=CARTESIAN_POINT('Ctrl Pts',(-1.58545904500006,5.2,-4.12997973800001));
#324206=CARTESIAN_POINT('Ctrl Pts',(-1.58545904500006,2.2,-4.12997973800001));
#324207=CARTESIAN_POINT('Ctrl Pts',(-1.58529456300006,12.2,-4.13206679300002));
#324208=CARTESIAN_POINT('Ctrl Pts',(-1.58529456300006,5.2,-4.13206679300002));
#324209=CARTESIAN_POINT('Ctrl Pts',(-1.58529456300006,2.2,-4.13206679300002));
#324210=CARTESIAN_POINT('Ctrl Pts',(-1.58512747100006,12.2,-4.13415761600001));
#324211=CARTESIAN_POINT('Ctrl Pts',(-1.58512747100006,5.2,-4.13415761600001));
#324212=CARTESIAN_POINT('Ctrl Pts',(-1.58512747100006,2.2,-4.13415761600001));
#324213=CARTESIAN_POINT('Ctrl Pts',(-1.58495776300006,12.2,-4.13625220100001));
#324214=CARTESIAN_POINT('Ctrl Pts',(-1.58495776300006,5.2,-4.13625220100001));
#324215=CARTESIAN_POINT('Ctrl Pts',(-1.58495776300006,2.2,-4.13625220100001));
#324216=CARTESIAN_POINT('Ctrl Pts',(-1.58478543300005,12.2,-4.13835053800002));
#324217=CARTESIAN_POINT('Ctrl Pts',(-1.58478543300005,5.2,-4.13835053800002));
#324218=CARTESIAN_POINT('Ctrl Pts',(-1.58478543300005,2.2,-4.13835053800002));
#324219=CARTESIAN_POINT('Ctrl Pts',(-1.58461047300006,12.2,-4.14045261900001));
#324220=CARTESIAN_POINT('Ctrl Pts',(-1.58461047300006,5.2,-4.14045261900001));
#324221=CARTESIAN_POINT('Ctrl Pts',(-1.58461047300006,2.2,-4.14045261900001));
#324222=CARTESIAN_POINT('Ctrl Pts',(-1.58443287500006,12.2,-4.14255843800001));
#324223=CARTESIAN_POINT('Ctrl Pts',(-1.58443287500006,5.2,-4.14255843800001));
#324224=CARTESIAN_POINT('Ctrl Pts',(-1.58443287500006,2.2,-4.14255843800001));
#324225=CARTESIAN_POINT('Ctrl Pts',(-1.58425263200005,12.2,-4.14466798700001));
#324226=CARTESIAN_POINT('Ctrl Pts',(-1.58425263200005,5.2,-4.14466798700001));
#324227=CARTESIAN_POINT('Ctrl Pts',(-1.58425263200005,2.2,-4.14466798700001));
#324228=CARTESIAN_POINT('Ctrl Pts',(-1.58406973900005,12.2,-4.14678125800001));
#324229=CARTESIAN_POINT('Ctrl Pts',(-1.58406973900005,5.2,-4.14678125800001));
#324230=CARTESIAN_POINT('Ctrl Pts',(-1.58406973900005,2.2,-4.14678125800001));
#324231=CARTESIAN_POINT('Ctrl Pts',(-1.58388418800006,12.2,-4.14889824300001));
#324232=CARTESIAN_POINT('Ctrl Pts',(-1.58388418800006,5.2,-4.14889824300001));
#324233=CARTESIAN_POINT('Ctrl Pts',(-1.58388418800006,2.2,-4.14889824300001));
#324234=CARTESIAN_POINT('Ctrl Pts',(-1.58369597100006,12.2,-4.15101893700002));
#324235=CARTESIAN_POINT('Ctrl Pts',(-1.58369597100006,5.2,-4.15101893700002));
#324236=CARTESIAN_POINT('Ctrl Pts',(-1.58369597100006,2.2,-4.15101893700002));
#324237=CARTESIAN_POINT('Ctrl Pts',(-1.58350508100006,12.2,-4.15314332800001));
#324238=CARTESIAN_POINT('Ctrl Pts',(-1.58350508100006,5.2,-4.15314332800001));
#324239=CARTESIAN_POINT('Ctrl Pts',(-1.58350508100006,2.2,-4.15314332800001));
#324240=CARTESIAN_POINT('Ctrl Pts',(-1.58331151200006,12.2,-4.15527141200001));
#324241=CARTESIAN_POINT('Ctrl Pts',(-1.58331151200006,5.2,-4.15527141200001));
#324242=CARTESIAN_POINT('Ctrl Pts',(-1.58331151200006,2.2,-4.15527141200001));
#324243=CARTESIAN_POINT('Ctrl Pts',(-1.58311525700006,12.2,-4.15740318000001));
#324244=CARTESIAN_POINT('Ctrl Pts',(-1.58311525700006,5.2,-4.15740318000001));
#324245=CARTESIAN_POINT('Ctrl Pts',(-1.58311525700006,2.2,-4.15740318000001));
#324246=CARTESIAN_POINT('Ctrl Pts',(-1.58291630800006,12.2,-4.15953862300002));
#324247=CARTESIAN_POINT('Ctrl Pts',(-1.58291630800006,5.2,-4.15953862300002));
#324248=CARTESIAN_POINT('Ctrl Pts',(-1.58291630800006,2.2,-4.15953862300002));
#324249=CARTESIAN_POINT('Ctrl Pts',(-1.58271465900006,12.2,-4.16167773700002));
#324250=CARTESIAN_POINT('Ctrl Pts',(-1.58271465900006,5.2,-4.16167773700002));
#324251=CARTESIAN_POINT('Ctrl Pts',(-1.58271465900006,2.2,-4.16167773700002));
#324252=CARTESIAN_POINT('Ctrl Pts',(-1.58251030300006,12.2,-4.16382051100001));
#324253=CARTESIAN_POINT('Ctrl Pts',(-1.58251030300006,5.2,-4.16382051100001));
#324254=CARTESIAN_POINT('Ctrl Pts',(-1.58251030300006,2.2,-4.16382051100001));
#324255=CARTESIAN_POINT('Ctrl Pts',(-1.58230323300006,12.2,-4.16596693800001));
#324256=CARTESIAN_POINT('Ctrl Pts',(-1.58230323300006,5.2,-4.16596693800001));
#324257=CARTESIAN_POINT('Ctrl Pts',(-1.58230323300006,2.2,-4.16596693800001));
#324258=CARTESIAN_POINT('Ctrl Pts',(-1.58209344200006,12.2,-4.16811701200002));
#324259=CARTESIAN_POINT('Ctrl Pts',(-1.58209344200006,5.2,-4.16811701200002));
#324260=CARTESIAN_POINT('Ctrl Pts',(-1.58209344200006,2.2,-4.16811701200002));
#324261=CARTESIAN_POINT('Ctrl Pts',(-1.58188092400006,12.2,-4.17027072500002));
#324262=CARTESIAN_POINT('Ctrl Pts',(-1.58188092400006,5.2,-4.17027072500002));
#324263=CARTESIAN_POINT('Ctrl Pts',(-1.58188092400006,2.2,-4.17027072500002));
#324264=CARTESIAN_POINT('Ctrl Pts',(-1.58166567100006,12.2,-4.17242806800001));
#324265=CARTESIAN_POINT('Ctrl Pts',(-1.58166567100006,5.2,-4.17242806800001));
#324266=CARTESIAN_POINT('Ctrl Pts',(-1.58166567100006,2.2,-4.17242806800001));
#324267=CARTESIAN_POINT('Ctrl Pts',(-1.58144767600006,12.2,-4.17458903300002));
#324268=CARTESIAN_POINT('Ctrl Pts',(-1.58144767600006,5.2,-4.17458903300002));
#324269=CARTESIAN_POINT('Ctrl Pts',(-1.58144767600006,2.2,-4.17458903300002));
#324270=CARTESIAN_POINT('Ctrl Pts',(-1.58122693300006,12.2,-4.17675361500002));
#324271=CARTESIAN_POINT('Ctrl Pts',(-1.58122693300006,5.2,-4.17675361500002));
#324272=CARTESIAN_POINT('Ctrl Pts',(-1.58122693300006,2.2,-4.17675361500002));
#324273=CARTESIAN_POINT('Ctrl Pts',(-1.58100343600006,12.2,-4.17892180400001));
#324274=CARTESIAN_POINT('Ctrl Pts',(-1.58100343600006,5.2,-4.17892180400001));
#324275=CARTESIAN_POINT('Ctrl Pts',(-1.58100343600006,2.2,-4.17892180400001));
#324276=CARTESIAN_POINT('Ctrl Pts',(-1.58077717700006,12.2,-4.18109359400002));
#324277=CARTESIAN_POINT('Ctrl Pts',(-1.58077717700006,5.2,-4.18109359400002));
#324278=CARTESIAN_POINT('Ctrl Pts',(-1.58077717700006,2.2,-4.18109359400002));
#324279=CARTESIAN_POINT('Ctrl Pts',(-1.58054815100006,12.2,-4.18326897700001));
#324280=CARTESIAN_POINT('Ctrl Pts',(-1.58054815100006,5.2,-4.18326897700001));
#324281=CARTESIAN_POINT('Ctrl Pts',(-1.58054815100006,2.2,-4.18326897700001));
#324282=CARTESIAN_POINT('Ctrl Pts',(-1.58031634800006,12.2,-4.18544794600002));
#324283=CARTESIAN_POINT('Ctrl Pts',(-1.58031634800006,5.2,-4.18544794600002));
#324284=CARTESIAN_POINT('Ctrl Pts',(-1.58031634800006,2.2,-4.18544794600002));
#324285=CARTESIAN_POINT('Ctrl Pts',(-1.58008176400006,12.2,-4.18763049100002));
#324286=CARTESIAN_POINT('Ctrl Pts',(-1.58008176400006,5.2,-4.18763049100002));
#324287=CARTESIAN_POINT('Ctrl Pts',(-1.58008176400006,2.2,-4.18763049100002));
#324288=CARTESIAN_POINT('Ctrl Pts',(-1.57984439200006,12.2,-4.18981660600001));
#324289=CARTESIAN_POINT('Ctrl Pts',(-1.57984439200006,5.2,-4.18981660600001));
#324290=CARTESIAN_POINT('Ctrl Pts',(-1.57984439200006,2.2,-4.18981660600001));
#324291=CARTESIAN_POINT('Ctrl Pts',(-1.57960422500006,12.2,-4.19200628400001));
#324292=CARTESIAN_POINT('Ctrl Pts',(-1.57960422500006,5.2,-4.19200628400001));
#324293=CARTESIAN_POINT('Ctrl Pts',(-1.57960422500006,2.2,-4.19200628400001));
#324294=CARTESIAN_POINT('Ctrl Pts',(-1.57936125600005,12.2,-4.19419951600001));
#324295=CARTESIAN_POINT('Ctrl Pts',(-1.57936125600005,5.2,-4.19419951600001));
#324296=CARTESIAN_POINT('Ctrl Pts',(-1.57936125600005,2.2,-4.19419951600001));
#324297=CARTESIAN_POINT('Ctrl Pts',(-1.57911547900006,12.2,-4.19639629700002));
#324298=CARTESIAN_POINT('Ctrl Pts',(-1.57911547900006,5.2,-4.19639629700002));
#324299=CARTESIAN_POINT('Ctrl Pts',(-1.57911547900006,2.2,-4.19639629700002));
#324300=CARTESIAN_POINT('Ctrl Pts',(-1.57886688700006,12.2,-4.19859661600002));
#324301=CARTESIAN_POINT('Ctrl Pts',(-1.57886688700006,5.2,-4.19859661600002));
#324302=CARTESIAN_POINT('Ctrl Pts',(-1.57886688700006,2.2,-4.19859661600002));
#324303=CARTESIAN_POINT('Ctrl Pts',(-1.57861547400006,12.2,-4.20080046700001));
#324304=CARTESIAN_POINT('Ctrl Pts',(-1.57861547400006,5.2,-4.20080046700001));
#324305=CARTESIAN_POINT('Ctrl Pts',(-1.57861547400006,2.2,-4.20080046700001));
#324306=CARTESIAN_POINT('Ctrl Pts',(-1.57836123400006,12.2,-4.20300784300002));
#324307=CARTESIAN_POINT('Ctrl Pts',(-1.57836123400006,5.2,-4.20300784300002));
#324308=CARTESIAN_POINT('Ctrl Pts',(-1.57836123400006,2.2,-4.20300784300002));
#324309=CARTESIAN_POINT('Ctrl Pts',(-1.57810415800005,12.2,-4.20521873600002));
#324310=CARTESIAN_POINT('Ctrl Pts',(-1.57810415800005,5.2,-4.20521873600002));
#324311=CARTESIAN_POINT('Ctrl Pts',(-1.57810415800005,2.2,-4.20521873600002));
#324312=CARTESIAN_POINT('Ctrl Pts',(-1.57784424200006,12.2,-4.20743313800001));
#324313=CARTESIAN_POINT('Ctrl Pts',(-1.57784424200006,5.2,-4.20743313800001));
#324314=CARTESIAN_POINT('Ctrl Pts',(-1.57784424200006,2.2,-4.20743313800001));
#324315=CARTESIAN_POINT('Ctrl Pts',(-1.57758148000006,12.2,-4.20965104200001));
#324316=CARTESIAN_POINT('Ctrl Pts',(-1.57758148000006,5.2,-4.20965104200001));
#324317=CARTESIAN_POINT('Ctrl Pts',(-1.57758148000006,2.2,-4.20965104200001));
#324318=CARTESIAN_POINT('Ctrl Pts',(-1.57731586300006,12.2,-4.21187243900001));
#324319=CARTESIAN_POINT('Ctrl Pts',(-1.57731586300006,5.2,-4.21187243900001));
#324320=CARTESIAN_POINT('Ctrl Pts',(-1.57731586300006,2.2,-4.21187243900001));
#324321=CARTESIAN_POINT('Ctrl Pts',(-1.57704738600006,12.2,-4.21409732500001));
#324322=CARTESIAN_POINT('Ctrl Pts',(-1.57704738600006,5.2,-4.21409732500001));
#324323=CARTESIAN_POINT('Ctrl Pts',(-1.57704738600006,2.2,-4.21409732500001));
#324324=CARTESIAN_POINT('Ctrl Pts',(-1.57677604200006,12.2,-4.21632568700002));
#324325=CARTESIAN_POINT('Ctrl Pts',(-1.57677604200006,5.2,-4.21632568700002));
#324326=CARTESIAN_POINT('Ctrl Pts',(-1.57677604200006,2.2,-4.21632568700002));
#324327=CARTESIAN_POINT('Ctrl Pts',(-1.57650182500006,12.2,-4.21855752300001));
#324328=CARTESIAN_POINT('Ctrl Pts',(-1.57650182500006,5.2,-4.21855752300001));
#324329=CARTESIAN_POINT('Ctrl Pts',(-1.57650182500006,2.2,-4.21855752300001));
#324330=CARTESIAN_POINT('Ctrl Pts',(-1.57622472900006,12.2,-4.22079282100002));
#324331=CARTESIAN_POINT('Ctrl Pts',(-1.57622472900006,5.2,-4.22079282100002));
#324332=CARTESIAN_POINT('Ctrl Pts',(-1.57622472900006,2.2,-4.22079282100002));
#324333=CARTESIAN_POINT('Ctrl Pts',(-1.57594474700006,12.2,-4.22303157600001));
#324334=CARTESIAN_POINT('Ctrl Pts',(-1.57594474700006,5.2,-4.22303157600001));
#324335=CARTESIAN_POINT('Ctrl Pts',(-1.57594474700006,2.2,-4.22303157600001));
#324336=CARTESIAN_POINT('Ctrl Pts',(-1.57566187300006,12.2,-4.22527378000002));
#324337=CARTESIAN_POINT('Ctrl Pts',(-1.57566187300006,5.2,-4.22527378000002));
#324338=CARTESIAN_POINT('Ctrl Pts',(-1.57566187300006,2.2,-4.22527378000002));
#324339=CARTESIAN_POINT('Ctrl Pts',(-1.57537610000006,12.2,-4.22751942500001));
#324340=CARTESIAN_POINT('Ctrl Pts',(-1.57537610000006,5.2,-4.22751942500001));
#324341=CARTESIAN_POINT('Ctrl Pts',(-1.57537610000006,2.2,-4.22751942500001));
#324342=CARTESIAN_POINT('Ctrl Pts',(-1.57508742400006,12.2,-4.22976850400001));
#324343=CARTESIAN_POINT('Ctrl Pts',(-1.57508742400006,5.2,-4.22976850400001));
#324344=CARTESIAN_POINT('Ctrl Pts',(-1.57508742400006,2.2,-4.22976850400001));
#324345=CARTESIAN_POINT('Ctrl Pts',(-1.57479583600006,12.2,-4.23202100900001));
#324346=CARTESIAN_POINT('Ctrl Pts',(-1.57479583600006,5.2,-4.23202100900001));
#324347=CARTESIAN_POINT('Ctrl Pts',(-1.57479583600006,2.2,-4.23202100900001));
#324348=CARTESIAN_POINT('Ctrl Pts',(-1.57450132900005,12.2,-4.23427693300002));
#324349=CARTESIAN_POINT('Ctrl Pts',(-1.57450132900005,5.2,-4.23427693300002));
#324350=CARTESIAN_POINT('Ctrl Pts',(-1.57450132900005,2.2,-4.23427693300002));
#324351=CARTESIAN_POINT('Ctrl Pts',(-1.57420390100006,12.2,-4.23653626600001));
#324352=CARTESIAN_POINT('Ctrl Pts',(-1.57420390100006,5.2,-4.23653626600001));
#324353=CARTESIAN_POINT('Ctrl Pts',(-1.57420390100006,2.2,-4.23653626600001));
#324354=CARTESIAN_POINT('Ctrl Pts',(-1.57390354300006,12.2,-4.23879900400001));
#324355=CARTESIAN_POINT('Ctrl Pts',(-1.57390354300006,5.2,-4.23879900400001));
#324356=CARTESIAN_POINT('Ctrl Pts',(-1.57390354300006,2.2,-4.23879900400001));
#324357=CARTESIAN_POINT('Ctrl Pts',(-1.57360024800006,12.2,-4.24106513700002));
#324358=CARTESIAN_POINT('Ctrl Pts',(-1.57360024800006,5.2,-4.24106513700002));
#324359=CARTESIAN_POINT('Ctrl Pts',(-1.57360024800006,2.2,-4.24106513700002));
#324360=CARTESIAN_POINT('Ctrl Pts',(-1.57329401100006,12.2,-4.24333465900002));
#324361=CARTESIAN_POINT('Ctrl Pts',(-1.57329401100006,5.2,-4.24333465900002));
#324362=CARTESIAN_POINT('Ctrl Pts',(-1.57329401100006,2.2,-4.24333465900002));
#324363=CARTESIAN_POINT('Ctrl Pts',(-1.57298482700006,12.2,-4.24560756200002));
#324364=CARTESIAN_POINT('Ctrl Pts',(-1.57298482700006,5.2,-4.24560756200002));
#324365=CARTESIAN_POINT('Ctrl Pts',(-1.57298482700006,2.2,-4.24560756200002));
#324366=CARTESIAN_POINT('Ctrl Pts',(-1.57267268700006,12.2,-4.24788383800002));
#324367=CARTESIAN_POINT('Ctrl Pts',(-1.57267268700006,5.2,-4.24788383800002));
#324368=CARTESIAN_POINT('Ctrl Pts',(-1.57267268700006,2.2,-4.24788383800002));
#324369=CARTESIAN_POINT('Ctrl Pts',(-1.57235758700006,12.2,-4.25016347900002));
#324370=CARTESIAN_POINT('Ctrl Pts',(-1.57235758700006,5.2,-4.25016347900002));
#324371=CARTESIAN_POINT('Ctrl Pts',(-1.57235758700006,2.2,-4.25016347900002));
#324372=CARTESIAN_POINT('Ctrl Pts',(-1.57203952100006,12.2,-4.25244647900001));
#324373=CARTESIAN_POINT('Ctrl Pts',(-1.57203952100006,5.2,-4.25244647900001));
#324374=CARTESIAN_POINT('Ctrl Pts',(-1.57203952100006,2.2,-4.25244647900001));
#324375=CARTESIAN_POINT('Ctrl Pts',(-1.57171848200006,12.2,-4.25473282900001));
#324376=CARTESIAN_POINT('Ctrl Pts',(-1.57171848200006,5.2,-4.25473282900001));
#324377=CARTESIAN_POINT('Ctrl Pts',(-1.57171848200006,2.2,-4.25473282900001));
#324378=CARTESIAN_POINT('Ctrl Pts',(-1.57139446300006,12.2,-4.25702252300002));
#324379=CARTESIAN_POINT('Ctrl Pts',(-1.57139446300006,5.2,-4.25702252300002));
#324380=CARTESIAN_POINT('Ctrl Pts',(-1.57139446300006,2.2,-4.25702252300002));
#324381=CARTESIAN_POINT('Ctrl Pts',(-1.57106746100005,12.2,-4.25931555100002));
#324382=CARTESIAN_POINT('Ctrl Pts',(-1.57106746100005,5.2,-4.25931555100002));
#324383=CARTESIAN_POINT('Ctrl Pts',(-1.57106746100005,2.2,-4.25931555100002));
#324384=CARTESIAN_POINT('Ctrl Pts',(-1.57073746600006,12.2,-4.26161190800002));
#324385=CARTESIAN_POINT('Ctrl Pts',(-1.57073746600006,5.2,-4.26161190800002));
#324386=CARTESIAN_POINT('Ctrl Pts',(-1.57073746600006,2.2,-4.26161190800002));
#324387=CARTESIAN_POINT('Ctrl Pts',(-1.57040447600005,12.2,-4.26391158500001));
#324388=CARTESIAN_POINT('Ctrl Pts',(-1.57040447600005,5.2,-4.26391158500001));
#324389=CARTESIAN_POINT('Ctrl Pts',(-1.57040447600005,2.2,-4.26391158500001));
#324390=CARTESIAN_POINT('Ctrl Pts',(-1.57006848200006,12.2,-4.26621457600001));
#324391=CARTESIAN_POINT('Ctrl Pts',(-1.57006848200006,5.2,-4.26621457600001));
#324392=CARTESIAN_POINT('Ctrl Pts',(-1.57006848200006,2.2,-4.26621457600001));
#324393=CARTESIAN_POINT('Ctrl Pts',(-1.56972947900006,12.2,-4.26852087100002));
#324394=CARTESIAN_POINT('Ctrl Pts',(-1.56972947900006,5.2,-4.26852087100002));
#324395=CARTESIAN_POINT('Ctrl Pts',(-1.56972947900006,2.2,-4.26852087100002));
#324396=CARTESIAN_POINT('Ctrl Pts',(-1.56938746200006,12.2,-4.27083046500002));
#324397=CARTESIAN_POINT('Ctrl Pts',(-1.56938746200006,5.2,-4.27083046500002));
#324398=CARTESIAN_POINT('Ctrl Pts',(-1.56938746200006,2.2,-4.27083046500002));
#324399=CARTESIAN_POINT('Ctrl Pts',(-1.56904242300006,12.2,-4.27314334800001));
#324400=CARTESIAN_POINT('Ctrl Pts',(-1.56904242300006,5.2,-4.27314334800001));
#324401=CARTESIAN_POINT('Ctrl Pts',(-1.56904242300006,2.2,-4.27314334800001));
#324402=CARTESIAN_POINT('Ctrl Pts',(-1.56869435800005,12.2,-4.27545951600001));
#324403=CARTESIAN_POINT('Ctrl Pts',(-1.56869435800005,5.2,-4.27545951600001));
#324404=CARTESIAN_POINT('Ctrl Pts',(-1.56869435800005,2.2,-4.27545951600001));
#324405=CARTESIAN_POINT('Ctrl Pts',(-1.56834326000005,12.2,-4.27777895800002));
#324406=CARTESIAN_POINT('Ctrl Pts',(-1.56834326000005,5.2,-4.27777895800002));
#324407=CARTESIAN_POINT('Ctrl Pts',(-1.56834326000005,2.2,-4.27777895800002));
#324408=CARTESIAN_POINT('Ctrl Pts',(-1.56798912400005,12.2,-4.28010166800001));
#324409=CARTESIAN_POINT('Ctrl Pts',(-1.56798912400005,5.2,-4.28010166800001));
#324410=CARTESIAN_POINT('Ctrl Pts',(-1.56798912400005,2.2,-4.28010166800001));
#324411=CARTESIAN_POINT('Ctrl Pts',(-1.56763194300006,12.2,-4.28242763800001));
#324412=CARTESIAN_POINT('Ctrl Pts',(-1.56763194300006,5.2,-4.28242763800001));
#324413=CARTESIAN_POINT('Ctrl Pts',(-1.56763194300006,2.2,-4.28242763800001));
#324414=CARTESIAN_POINT('Ctrl Pts',(-1.56727171100006,12.2,-4.28475686200001));
#324415=CARTESIAN_POINT('Ctrl Pts',(-1.56727171100006,5.2,-4.28475686200001));
#324416=CARTESIAN_POINT('Ctrl Pts',(-1.56727171100006,2.2,-4.28475686200001));
#324417=CARTESIAN_POINT('Ctrl Pts',(-1.56690842400006,12.2,-4.28708933000001));
#324418=CARTESIAN_POINT('Ctrl Pts',(-1.56690842400006,5.2,-4.28708933000001));
#324419=CARTESIAN_POINT('Ctrl Pts',(-1.56690842400006,2.2,-4.28708933000001));
#324420=CARTESIAN_POINT('Ctrl Pts',(-1.56654207500006,12.2,-4.28942503600001));
#324421=CARTESIAN_POINT('Ctrl Pts',(-1.56654207500006,5.2,-4.28942503600001));
#324422=CARTESIAN_POINT('Ctrl Pts',(-1.56654207500006,2.2,-4.28942503600001));
#324423=CARTESIAN_POINT('Ctrl Pts',(-1.56617265800006,12.2,-4.29176397300001));
#324424=CARTESIAN_POINT('Ctrl Pts',(-1.56617265800006,5.2,-4.29176397300001));
#324425=CARTESIAN_POINT('Ctrl Pts',(-1.56617265800006,2.2,-4.29176397300001));
#324426=CARTESIAN_POINT('Ctrl Pts',(-1.56580016900006,12.2,-4.29410613300002));
#324427=CARTESIAN_POINT('Ctrl Pts',(-1.56580016900006,5.2,-4.29410613300002));
#324428=CARTESIAN_POINT('Ctrl Pts',(-1.56580016900006,2.2,-4.29410613300002));
#324429=CARTESIAN_POINT('Ctrl Pts',(-1.56542459900006,12.2,-4.29645150700001));
#324430=CARTESIAN_POINT('Ctrl Pts',(-1.56542459900006,5.2,-4.29645150700001));
#324431=CARTESIAN_POINT('Ctrl Pts',(-1.56542459900006,2.2,-4.29645150700001));
#324432=CARTESIAN_POINT('Ctrl Pts',(-1.56504594300006,12.2,-4.29880009000001));
#324433=CARTESIAN_POINT('Ctrl Pts',(-1.56504594300006,5.2,-4.29880009000001));
#324434=CARTESIAN_POINT('Ctrl Pts',(-1.56504594300006,2.2,-4.29880009000001));
#324435=CARTESIAN_POINT('Ctrl Pts',(-1.56466419900006,12.2,-4.30115187200002));
#324436=CARTESIAN_POINT('Ctrl Pts',(-1.56466419900006,5.2,-4.30115187200002));
#324437=CARTESIAN_POINT('Ctrl Pts',(-1.56466419900006,2.2,-4.30115187200002));
#324438=CARTESIAN_POINT('Ctrl Pts',(-1.56427935700005,12.2,-4.30350684800001));
#324439=CARTESIAN_POINT('Ctrl Pts',(-1.56427935700005,5.2,-4.30350684800001));
#324440=CARTESIAN_POINT('Ctrl Pts',(-1.56427935700005,2.2,-4.30350684800001));
#324441=CARTESIAN_POINT('Ctrl Pts',(-1.56389141300005,12.2,-4.30586500900001));
#324442=CARTESIAN_POINT('Ctrl Pts',(-1.56389141300005,5.2,-4.30586500900001));
#324443=CARTESIAN_POINT('Ctrl Pts',(-1.56389141300005,2.2,-4.30586500900001));
#324444=CARTESIAN_POINT('Ctrl Pts',(-1.56350036100006,12.2,-4.30822634700001));
#324445=CARTESIAN_POINT('Ctrl Pts',(-1.56350036100006,5.2,-4.30822634700001));
#324446=CARTESIAN_POINT('Ctrl Pts',(-1.56350036100006,2.2,-4.30822634700001));
#324447=CARTESIAN_POINT('Ctrl Pts',(-1.56310619600006,12.2,-4.31059085600001));
#324448=CARTESIAN_POINT('Ctrl Pts',(-1.56310619600006,5.2,-4.31059085600001));
#324449=CARTESIAN_POINT('Ctrl Pts',(-1.56310619600006,2.2,-4.31059085600001));
#324450=CARTESIAN_POINT('Ctrl Pts',(-1.56270891100006,12.2,-4.31295852800002));
#324451=CARTESIAN_POINT('Ctrl Pts',(-1.56270891100006,5.2,-4.31295852800002));
#324452=CARTESIAN_POINT('Ctrl Pts',(-1.56270891100006,2.2,-4.31295852800002));
#324453=CARTESIAN_POINT('Ctrl Pts',(-1.56230850300005,12.2,-4.31532935500002));
#324454=CARTESIAN_POINT('Ctrl Pts',(-1.56230850300005,5.2,-4.31532935500002));
#324455=CARTESIAN_POINT('Ctrl Pts',(-1.56230850300005,2.2,-4.31532935500002));
#324456=CARTESIAN_POINT('Ctrl Pts',(-1.56190496300006,12.2,-4.31770333100001));
#324457=CARTESIAN_POINT('Ctrl Pts',(-1.56190496300006,5.2,-4.31770333100001));
#324458=CARTESIAN_POINT('Ctrl Pts',(-1.56190496300006,2.2,-4.31770333100001));
#324459=CARTESIAN_POINT('Ctrl Pts',(-1.56149828800005,12.2,-4.32008044700002));
#324460=CARTESIAN_POINT('Ctrl Pts',(-1.56149828800005,5.2,-4.32008044700002));
#324461=CARTESIAN_POINT('Ctrl Pts',(-1.56149828800005,2.2,-4.32008044700002));
#324462=CARTESIAN_POINT('Ctrl Pts',(-1.56108847100006,12.2,-4.32246069400001));
#324463=CARTESIAN_POINT('Ctrl Pts',(-1.56108847100006,5.2,-4.32246069400001));
#324464=CARTESIAN_POINT('Ctrl Pts',(-1.56108847100006,2.2,-4.32246069400001));
#324465=CARTESIAN_POINT('Ctrl Pts',(-1.56067550700006,12.2,-4.32484406800001));
#324466=CARTESIAN_POINT('Ctrl Pts',(-1.56067550700006,5.2,-4.32484406800001));
#324467=CARTESIAN_POINT('Ctrl Pts',(-1.56067550700006,2.2,-4.32484406800001));
#324468=CARTESIAN_POINT('Ctrl Pts',(-1.56025939000005,12.2,-4.32723056000002));
#324469=CARTESIAN_POINT('Ctrl Pts',(-1.56025939000005,5.2,-4.32723056000002));
#324470=CARTESIAN_POINT('Ctrl Pts',(-1.56025939000005,2.2,-4.32723056000002));
#324471=CARTESIAN_POINT('Ctrl Pts',(-1.55984011600005,12.2,-4.32962016300001));
#324472=CARTESIAN_POINT('Ctrl Pts',(-1.55984011600005,5.2,-4.32962016300001));
#324473=CARTESIAN_POINT('Ctrl Pts',(-1.55984011600005,2.2,-4.32962016300001));
#324474=CARTESIAN_POINT('Ctrl Pts',(-1.55941767800006,12.2,-4.33201286900001));
#324475=CARTESIAN_POINT('Ctrl Pts',(-1.55941767800006,5.2,-4.33201286900001));
#324476=CARTESIAN_POINT('Ctrl Pts',(-1.55941767800006,2.2,-4.33201286900001));
#324477=CARTESIAN_POINT('Ctrl Pts',(-1.55899207100005,12.2,-4.33440866900002));
#324478=CARTESIAN_POINT('Ctrl Pts',(-1.55899207100005,5.2,-4.33440866900002));
#324479=CARTESIAN_POINT('Ctrl Pts',(-1.55899207100005,2.2,-4.33440866900002));
#324480=CARTESIAN_POINT('Ctrl Pts',(-1.55856328800006,12.2,-4.33680755900001));
#324481=CARTESIAN_POINT('Ctrl Pts',(-1.55856328800006,5.2,-4.33680755900001));
#324482=CARTESIAN_POINT('Ctrl Pts',(-1.55856328800006,2.2,-4.33680755900001));
#324483=CARTESIAN_POINT('Ctrl Pts',(-1.55813132700006,12.2,-4.33920952900001));
#324484=CARTESIAN_POINT('Ctrl Pts',(-1.55813132700006,5.2,-4.33920952900001));
#324485=CARTESIAN_POINT('Ctrl Pts',(-1.55813132700006,2.2,-4.33920952900001));
#324486=CARTESIAN_POINT('Ctrl Pts',(-1.55769618000006,12.2,-4.34161457200001));
#324487=CARTESIAN_POINT('Ctrl Pts',(-1.55769618000006,5.2,-4.34161457200001));
#324488=CARTESIAN_POINT('Ctrl Pts',(-1.55769618000006,2.2,-4.34161457200001));
#324489=CARTESIAN_POINT('Ctrl Pts',(-1.55725784300006,12.2,-4.34402268000001));
#324490=CARTESIAN_POINT('Ctrl Pts',(-1.55725784300006,5.2,-4.34402268000001));
#324491=CARTESIAN_POINT('Ctrl Pts',(-1.55725784300006,2.2,-4.34402268000001));
#324492=CARTESIAN_POINT('Ctrl Pts',(-1.55681630800005,12.2,-4.34643384800002));
#324493=CARTESIAN_POINT('Ctrl Pts',(-1.55681630800005,5.2,-4.34643384800002));
#324494=CARTESIAN_POINT('Ctrl Pts',(-1.55681630800005,2.2,-4.34643384800002));
#324495=CARTESIAN_POINT('Ctrl Pts',(-1.55637157300006,12.2,-4.34884806500001));
#324496=CARTESIAN_POINT('Ctrl Pts',(-1.55637157300006,5.2,-4.34884806500001));
#324497=CARTESIAN_POINT('Ctrl Pts',(-1.55637157300006,2.2,-4.34884806500001));
#324498=CARTESIAN_POINT('Ctrl Pts',(-1.55592363000005,12.2,-4.35126532700002));
#324499=CARTESIAN_POINT('Ctrl Pts',(-1.55592363000005,5.2,-4.35126532700002));
#324500=CARTESIAN_POINT('Ctrl Pts',(-1.55592363000005,2.2,-4.35126532700002));
#324501=CARTESIAN_POINT('Ctrl Pts',(-1.55547247600006,12.2,-4.35368562300001));
#324502=CARTESIAN_POINT('Ctrl Pts',(-1.55547247600006,5.2,-4.35368562300001));
#324503=CARTESIAN_POINT('Ctrl Pts',(-1.55547247600006,2.2,-4.35368562300001));
#324504=CARTESIAN_POINT('Ctrl Pts',(-1.55501810200006,12.2,-4.35610894900002));
#324505=CARTESIAN_POINT('Ctrl Pts',(-1.55501810200006,5.2,-4.35610894900002));
#324506=CARTESIAN_POINT('Ctrl Pts',(-1.55501810200006,2.2,-4.35610894900002));
#324507=CARTESIAN_POINT('Ctrl Pts',(-1.55456050700006,12.2,-4.35853529600001));
#324508=CARTESIAN_POINT('Ctrl Pts',(-1.55456050700006,5.2,-4.35853529600001));
#324509=CARTESIAN_POINT('Ctrl Pts',(-1.55456050700006,2.2,-4.35853529600001));
#324510=CARTESIAN_POINT('Ctrl Pts',(-1.55409968300006,12.2,-4.36096465600002));
#324511=CARTESIAN_POINT('Ctrl Pts',(-1.55409968300006,5.2,-4.36096465600002));
#324512=CARTESIAN_POINT('Ctrl Pts',(-1.55409968300006,2.2,-4.36096465600002));
#324513=CARTESIAN_POINT('Ctrl Pts',(-1.55363562600006,12.2,-4.36339702300002));
#324514=CARTESIAN_POINT('Ctrl Pts',(-1.55363562600006,5.2,-4.36339702300002));
#324515=CARTESIAN_POINT('Ctrl Pts',(-1.55363562600006,2.2,-4.36339702300002));
#324516=CARTESIAN_POINT('Ctrl Pts',(-1.55316833000006,12.2,-4.36583238800001));
#324517=CARTESIAN_POINT('Ctrl Pts',(-1.55316833000006,5.2,-4.36583238800001));
#324518=CARTESIAN_POINT('Ctrl Pts',(-1.55316833000006,2.2,-4.36583238800001));
#324519=CARTESIAN_POINT('Ctrl Pts',(-1.55269779000006,12.2,-4.36827074500002));
#324520=CARTESIAN_POINT('Ctrl Pts',(-1.55269779000006,5.2,-4.36827074500002));
#324521=CARTESIAN_POINT('Ctrl Pts',(-1.55269779000006,2.2,-4.36827074500002));
#324522=CARTESIAN_POINT('Ctrl Pts',(-1.55222400100006,12.2,-4.37071208400001));
#324523=CARTESIAN_POINT('Ctrl Pts',(-1.55222400100006,5.2,-4.37071208400001));
#324524=CARTESIAN_POINT('Ctrl Pts',(-1.55222400100006,2.2,-4.37071208400001));
#324525=CARTESIAN_POINT('Ctrl Pts',(-1.55174695700006,12.2,-4.37315640100001));
#324526=CARTESIAN_POINT('Ctrl Pts',(-1.55174695700006,5.2,-4.37315640100001));
#324527=CARTESIAN_POINT('Ctrl Pts',(-1.55174695700006,2.2,-4.37315640100001));
#324528=CARTESIAN_POINT('Ctrl Pts',(-1.55126665400006,12.2,-4.37560368700002));
#324529=CARTESIAN_POINT('Ctrl Pts',(-1.55126665400006,5.2,-4.37560368700002));
#324530=CARTESIAN_POINT('Ctrl Pts',(-1.55126665400006,2.2,-4.37560368700002));
#324531=CARTESIAN_POINT('Ctrl Pts',(-1.55078308600005,12.2,-4.37805393400001));
#324532=CARTESIAN_POINT('Ctrl Pts',(-1.55078308600005,5.2,-4.37805393400001));
#324533=CARTESIAN_POINT('Ctrl Pts',(-1.55078308600005,2.2,-4.37805393400001));
#324534=CARTESIAN_POINT('Ctrl Pts',(-1.55029624800005,12.2,-4.38050713600001));
#324535=CARTESIAN_POINT('Ctrl Pts',(-1.55029624800005,5.2,-4.38050713600001));
#324536=CARTESIAN_POINT('Ctrl Pts',(-1.55029624800005,2.2,-4.38050713600001));
#324537=CARTESIAN_POINT('Ctrl Pts',(-1.54980613500005,12.2,-4.38296328300002));
#324538=CARTESIAN_POINT('Ctrl Pts',(-1.54980613500005,5.2,-4.38296328300002));
#324539=CARTESIAN_POINT('Ctrl Pts',(-1.54980613500005,2.2,-4.38296328300002));
#324540=CARTESIAN_POINT('Ctrl Pts',(-1.54931274100006,12.2,-4.38542237000001));
#324541=CARTESIAN_POINT('Ctrl Pts',(-1.54931274100006,5.2,-4.38542237000001));
#324542=CARTESIAN_POINT('Ctrl Pts',(-1.54931274100006,2.2,-4.38542237000001));
#324543=CARTESIAN_POINT('Ctrl Pts',(-1.54881606300005,12.2,-4.38788438900001));
#324544=CARTESIAN_POINT('Ctrl Pts',(-1.54881606300005,5.2,-4.38788438900001));
#324545=CARTESIAN_POINT('Ctrl Pts',(-1.54881606300005,2.2,-4.38788438900001));
#324546=CARTESIAN_POINT('Ctrl Pts',(-1.54831609400006,12.2,-4.39034933300002));
#324547=CARTESIAN_POINT('Ctrl Pts',(-1.54831609400006,5.2,-4.39034933300002));
#324548=CARTESIAN_POINT('Ctrl Pts',(-1.54831609400006,2.2,-4.39034933300002));
#324549=CARTESIAN_POINT('Ctrl Pts',(-1.54781282900006,12.2,-4.39281719400002));
#324550=CARTESIAN_POINT('Ctrl Pts',(-1.54781282900006,5.2,-4.39281719400002));
#324551=CARTESIAN_POINT('Ctrl Pts',(-1.54781282900006,2.2,-4.39281719400002));
#324552=CARTESIAN_POINT('Ctrl Pts',(-1.54730626400006,12.2,-4.39528796400001));
#324553=CARTESIAN_POINT('Ctrl Pts',(-1.54730626400006,5.2,-4.39528796400001));
#324554=CARTESIAN_POINT('Ctrl Pts',(-1.54730626400006,2.2,-4.39528796400001));
#324555=CARTESIAN_POINT('Ctrl Pts',(-1.54679639400006,12.2,-4.39776163600001));
#324556=CARTESIAN_POINT('Ctrl Pts',(-1.54679639400006,5.2,-4.39776163600001));
#324557=CARTESIAN_POINT('Ctrl Pts',(-1.54679639400006,2.2,-4.39776163600001));
#324558=CARTESIAN_POINT('Ctrl Pts',(-1.54628321200006,12.2,-4.40023820300001));
#324559=CARTESIAN_POINT('Ctrl Pts',(-1.54628321200006,5.2,-4.40023820300001));
#324560=CARTESIAN_POINT('Ctrl Pts',(-1.54628321200006,2.2,-4.40023820300001));
#324561=CARTESIAN_POINT('Ctrl Pts',(-1.54576671500006,12.2,-4.40271765800002));
#324562=CARTESIAN_POINT('Ctrl Pts',(-1.54576671500006,5.2,-4.40271765800002));
#324563=CARTESIAN_POINT('Ctrl Pts',(-1.54576671500006,2.2,-4.40271765800002));
#324564=CARTESIAN_POINT('Ctrl Pts',(-1.54524689700006,12.2,-4.40519999300002));
#324565=CARTESIAN_POINT('Ctrl Pts',(-1.54524689700006,5.2,-4.40519999300002));
#324566=CARTESIAN_POINT('Ctrl Pts',(-1.54524689700006,2.2,-4.40519999300002));
#324567=CARTESIAN_POINT('Ctrl Pts',(-1.54472375300006,12.2,-4.40768520000002));
#324568=CARTESIAN_POINT('Ctrl Pts',(-1.54472375300006,5.2,-4.40768520000002));
#324569=CARTESIAN_POINT('Ctrl Pts',(-1.54472375300006,2.2,-4.40768520000002));
#324570=CARTESIAN_POINT('Ctrl Pts',(-1.54419727900006,12.2,-4.41017327200001));
#324571=CARTESIAN_POINT('Ctrl Pts',(-1.54419727900006,5.2,-4.41017327200001));
#324572=CARTESIAN_POINT('Ctrl Pts',(-1.54419727900006,2.2,-4.41017327200001));
#324573=CARTESIAN_POINT('Ctrl Pts',(-1.54366747000006,12.2,-4.41266420300002));
#324574=CARTESIAN_POINT('Ctrl Pts',(-1.54366747000006,5.2,-4.41266420300002));
#324575=CARTESIAN_POINT('Ctrl Pts',(-1.54366747000006,2.2,-4.41266420300002));
#324576=CARTESIAN_POINT('Ctrl Pts',(-1.54313432000006,12.2,-4.41515798400001));
#324577=CARTESIAN_POINT('Ctrl Pts',(-1.54313432000006,5.2,-4.41515798400001));
#324578=CARTESIAN_POINT('Ctrl Pts',(-1.54313432000006,2.2,-4.41515798400001));
#324579=CARTESIAN_POINT('Ctrl Pts',(-1.54259782500006,12.2,-4.41765460700001));
#324580=CARTESIAN_POINT('Ctrl Pts',(-1.54259782500006,5.2,-4.41765460700001));
#324581=CARTESIAN_POINT('Ctrl Pts',(-1.54259782500006,2.2,-4.41765460700001));
#324582=CARTESIAN_POINT('Ctrl Pts',(-1.54205797900006,12.2,-4.42015406700001));
#324583=CARTESIAN_POINT('Ctrl Pts',(-1.54205797900006,5.2,-4.42015406700001));
#324584=CARTESIAN_POINT('Ctrl Pts',(-1.54205797900006,2.2,-4.42015406700001));
#324585=CARTESIAN_POINT('Ctrl Pts',(-1.54151477800006,12.2,-4.42265635500001));
#324586=CARTESIAN_POINT('Ctrl Pts',(-1.54151477800006,5.2,-4.42265635500001));
#324587=CARTESIAN_POINT('Ctrl Pts',(-1.54151477800006,2.2,-4.42265635500001));
#324588=CARTESIAN_POINT('Ctrl Pts',(-1.54096821700006,12.2,-4.42516146300001));
#324589=CARTESIAN_POINT('Ctrl Pts',(-1.54096821700006,5.2,-4.42516146300001));
#324590=CARTESIAN_POINT('Ctrl Pts',(-1.54096821700006,2.2,-4.42516146300001));
#324591=CARTESIAN_POINT('Ctrl Pts',(-1.54041829100006,12.2,-4.42766938500001));
#324592=CARTESIAN_POINT('Ctrl Pts',(-1.54041829100006,5.2,-4.42766938500001));
#324593=CARTESIAN_POINT('Ctrl Pts',(-1.54041829100006,2.2,-4.42766938500001));
#324594=CARTESIAN_POINT('Ctrl Pts',(-1.53986499500005,12.2,-4.43018011200001));
#324595=CARTESIAN_POINT('Ctrl Pts',(-1.53986499500005,5.2,-4.43018011200001));
#324596=CARTESIAN_POINT('Ctrl Pts',(-1.53986499500005,2.2,-4.43018011200001));
#324597=CARTESIAN_POINT('Ctrl Pts',(-1.53930832500006,12.2,-4.43269363900002));
#324598=CARTESIAN_POINT('Ctrl Pts',(-1.53930832500006,5.2,-4.43269363900002));
#324599=CARTESIAN_POINT('Ctrl Pts',(-1.53930832500006,2.2,-4.43269363900002));
#324600=CARTESIAN_POINT('Ctrl Pts',(-1.53874827600006,12.2,-4.43520995700001));
#324601=CARTESIAN_POINT('Ctrl Pts',(-1.53874827600006,5.2,-4.43520995700001));
#324602=CARTESIAN_POINT('Ctrl Pts',(-1.53874827600006,2.2,-4.43520995700001));
#324603=CARTESIAN_POINT('Ctrl Pts',(-1.53818484200006,12.2,-4.43772905900001));
#324604=CARTESIAN_POINT('Ctrl Pts',(-1.53818484200006,5.2,-4.43772905900001));
#324605=CARTESIAN_POINT('Ctrl Pts',(-1.53818484200006,2.2,-4.43772905900001));
#324606=CARTESIAN_POINT('Ctrl Pts',(-1.53761802000006,12.2,-4.44025093800001));
#324607=CARTESIAN_POINT('Ctrl Pts',(-1.53761802000006,5.2,-4.44025093800001));
#324608=CARTESIAN_POINT('Ctrl Pts',(-1.53761802000006,2.2,-4.44025093800001));
#324609=CARTESIAN_POINT('Ctrl Pts',(-1.53704780500005,12.2,-4.44277558600001));
#324610=CARTESIAN_POINT('Ctrl Pts',(-1.53704780500005,5.2,-4.44277558600001));
#324611=CARTESIAN_POINT('Ctrl Pts',(-1.53704780500005,2.2,-4.44277558600001));
#324612=CARTESIAN_POINT('Ctrl Pts',(-1.53647419100006,12.2,-4.44530299700002));
#324613=CARTESIAN_POINT('Ctrl Pts',(-1.53647419100006,5.2,-4.44530299700002));
#324614=CARTESIAN_POINT('Ctrl Pts',(-1.53647419100006,2.2,-4.44530299700002));
#324615=CARTESIAN_POINT('Ctrl Pts',(-1.53589717400005,12.2,-4.44783316200001));
#324616=CARTESIAN_POINT('Ctrl Pts',(-1.53589717400005,5.2,-4.44783316200001));
#324617=CARTESIAN_POINT('Ctrl Pts',(-1.53589717400005,2.2,-4.44783316200001));
#324618=CARTESIAN_POINT('Ctrl Pts',(-1.53531674800006,12.2,-4.45036607300001));
#324619=CARTESIAN_POINT('Ctrl Pts',(-1.53531674800006,5.2,-4.45036607300001));
#324620=CARTESIAN_POINT('Ctrl Pts',(-1.53531674800006,2.2,-4.45036607300001));
#324621=CARTESIAN_POINT('Ctrl Pts',(-1.53473291000006,12.2,-4.45290172400002));
#324622=CARTESIAN_POINT('Ctrl Pts',(-1.53473291000006,5.2,-4.45290172400002));
#324623=CARTESIAN_POINT('Ctrl Pts',(-1.53473291000006,2.2,-4.45290172400002));
#324624=CARTESIAN_POINT('Ctrl Pts',(-1.53414565400006,12.2,-4.45544010600001));
#324625=CARTESIAN_POINT('Ctrl Pts',(-1.53414565400006,5.2,-4.45544010600001));
#324626=CARTESIAN_POINT('Ctrl Pts',(-1.53414565400006,2.2,-4.45544010600001));
#324627=CARTESIAN_POINT('Ctrl Pts',(-1.53355497600006,12.2,-4.45798121300002));
#324628=CARTESIAN_POINT('Ctrl Pts',(-1.53355497600006,5.2,-4.45798121300002));
#324629=CARTESIAN_POINT('Ctrl Pts',(-1.53355497600006,2.2,-4.45798121300002));
#324630=CARTESIAN_POINT('Ctrl Pts',(-1.53296087100005,12.2,-4.46052503700002));
#324631=CARTESIAN_POINT('Ctrl Pts',(-1.53296087100005,5.2,-4.46052503700002));
#324632=CARTESIAN_POINT('Ctrl Pts',(-1.53296087100005,2.2,-4.46052503700002));
#324633=CARTESIAN_POINT('Ctrl Pts',(-1.53236333600006,12.2,-4.46307157300001));
#324634=CARTESIAN_POINT('Ctrl Pts',(-1.53236333600006,5.2,-4.46307157300001));
#324635=CARTESIAN_POINT('Ctrl Pts',(-1.53236333600006,2.2,-4.46307157300001));
#324636=CARTESIAN_POINT('Ctrl Pts',(-1.53176236500005,12.2,-4.46562081300002));
#324637=CARTESIAN_POINT('Ctrl Pts',(-1.53176236500005,5.2,-4.46562081300002));
#324638=CARTESIAN_POINT('Ctrl Pts',(-1.53176236500005,2.2,-4.46562081300002));
#324639=CARTESIAN_POINT('Ctrl Pts',(-1.53115795500006,12.2,-4.46817275000001));
#324640=CARTESIAN_POINT('Ctrl Pts',(-1.53115795500006,5.2,-4.46817275000001));
#324641=CARTESIAN_POINT('Ctrl Pts',(-1.53115795500006,2.2,-4.46817275000001));
#324642=CARTESIAN_POINT('Ctrl Pts',(-1.53055010200006,12.2,-4.47072737700001));
#324643=CARTESIAN_POINT('Ctrl Pts',(-1.53055010200006,5.2,-4.47072737700001));
#324644=CARTESIAN_POINT('Ctrl Pts',(-1.53055010200006,2.2,-4.47072737700001));
#324645=CARTESIAN_POINT('Ctrl Pts',(-1.52993880100006,12.2,-4.47328468700002));
#324646=CARTESIAN_POINT('Ctrl Pts',(-1.52993880100006,5.2,-4.47328468700002));
#324647=CARTESIAN_POINT('Ctrl Pts',(-1.52993880100006,2.2,-4.47328468700002));
#324648=CARTESIAN_POINT('Ctrl Pts',(-1.52932404500006,12.2,-4.47584467000001));
#324649=CARTESIAN_POINT('Ctrl Pts',(-1.52932404500006,5.2,-4.47584467000001));
#324650=CARTESIAN_POINT('Ctrl Pts',(-1.52932404500006,2.2,-4.47584467000001));
#324651=CARTESIAN_POINT('Ctrl Pts',(-1.52870582800006,12.2,-4.47840731700001));
#324652=CARTESIAN_POINT('Ctrl Pts',(-1.52870582800006,5.2,-4.47840731700001));
#324653=CARTESIAN_POINT('Ctrl Pts',(-1.52870582800006,2.2,-4.47840731700001));
#324654=CARTESIAN_POINT('Ctrl Pts',(-1.52808414600006,12.2,-4.48097261900001));
#324655=CARTESIAN_POINT('Ctrl Pts',(-1.52808414600006,5.2,-4.48097261900001));
#324656=CARTESIAN_POINT('Ctrl Pts',(-1.52808414600006,2.2,-4.48097261900001));
#324657=CARTESIAN_POINT('Ctrl Pts',(-1.52745899300006,12.2,-4.48354056900001));
#324658=CARTESIAN_POINT('Ctrl Pts',(-1.52745899300006,5.2,-4.48354056900001));
#324659=CARTESIAN_POINT('Ctrl Pts',(-1.52745899300006,2.2,-4.48354056900001));
#324660=CARTESIAN_POINT('Ctrl Pts',(-1.52683036500005,12.2,-4.48611115700002));
#324661=CARTESIAN_POINT('Ctrl Pts',(-1.52683036500005,5.2,-4.48611115700002));
#324662=CARTESIAN_POINT('Ctrl Pts',(-1.52683036500005,2.2,-4.48611115700002));
#324663=CARTESIAN_POINT('Ctrl Pts',(-1.52619825900006,12.2,-4.48868437900002));
#324664=CARTESIAN_POINT('Ctrl Pts',(-1.52619825900006,5.2,-4.48868437900002));
#324665=CARTESIAN_POINT('Ctrl Pts',(-1.52619825900006,2.2,-4.48868437900002));
#324666=CARTESIAN_POINT('Ctrl Pts',(-1.52556267200006,12.2,-4.49126023200002));
#324667=CARTESIAN_POINT('Ctrl Pts',(-1.52556267200006,5.2,-4.49126023200002));
#324668=CARTESIAN_POINT('Ctrl Pts',(-1.52556267200006,2.2,-4.49126023200002));
#324669=CARTESIAN_POINT('Ctrl Pts',(-1.52492360500006,12.2,-4.49383871500002));
#324670=CARTESIAN_POINT('Ctrl Pts',(-1.52492360500006,5.2,-4.49383871500002));
#324671=CARTESIAN_POINT('Ctrl Pts',(-1.52492360500006,2.2,-4.49383871500002));
#324672=CARTESIAN_POINT('Ctrl Pts',(-1.52440956500006,12.2,-4.49590360400002));
#324673=CARTESIAN_POINT('Ctrl Pts',(-1.52440956500006,5.2,-4.49590360400002));
#324674=CARTESIAN_POINT('Ctrl Pts',(-1.52440956500006,2.2,-4.49590360400002));
#324675=CARTESIAN_POINT('Ctrl Pts',(-1.52402246800006,12.2,-4.49745345200002));
#324676=CARTESIAN_POINT('Ctrl Pts',(-1.52402246800006,5.2,-4.49745345200002));
#324677=CARTESIAN_POINT('Ctrl Pts',(-1.52402246800006,2.2,-4.49745345200002));
#324678=CARTESIAN_POINT('Ctrl Pts',(-1.52376370700006,12.2,-4.49848720900001));
#324679=CARTESIAN_POINT('Ctrl Pts',(-1.52376370700006,5.2,-4.49848720900001));
#324680=CARTESIAN_POINT('Ctrl Pts',(-1.52376370700006,2.2,-4.49848720900001));
#324681=CARTESIAN_POINT('Ctrl Pts',(-1.52363415300006,12.2,-4.49900422000002));
#324682=CARTESIAN_POINT('Ctrl Pts',(-1.52363415300006,5.2,-4.49900422000002));
#324683=CARTESIAN_POINT('Ctrl Pts',(-1.52363415300006,2.2,-4.49900422000002));
#324684=CARTESIAN_POINT('',(-1.52363415200006,2.7,-4.49900422000002));
#324685=CARTESIAN_POINT('',(-1.52363415200006,12.2,-4.49900422000002));
#324686=CARTESIAN_POINT('Ctrl Pts',(-1.54920881500006,2.7,-3.68100722400001));
#324687=CARTESIAN_POINT('Ctrl Pts',(-1.5492699808608,2.7,-3.68115413835674));
#324688=CARTESIAN_POINT('Ctrl Pts',(-1.54932969519839,2.70000000000379,
-3.6813016557513));
#324689=CARTESIAN_POINT('Ctrl Pts',(-1.54951244654765,2.70000000000379,
-3.68175597959113));
#324690=CARTESIAN_POINT('Ctrl Pts',(-1.549639932611,2.70000000000408,-3.68207990099521));
#324691=CARTESIAN_POINT('Ctrl Pts',(-1.55017632519208,2.70000000000408,
-3.68345945901149));
#324692=CARTESIAN_POINT('Ctrl Pts',(-1.55060466855355,2.70000000000408,
-3.68461026767503));
#324693=CARTESIAN_POINT('Ctrl Pts',(-1.55244518831997,2.70000000000408,
-3.68968448235393));
#324694=CARTESIAN_POINT('Ctrl Pts',(-1.55386348666925,2.70000000000408,
-3.69397409267706));
#324695=CARTESIAN_POINT('Ctrl Pts',(-1.55978529038518,2.70000000000408,
-3.71291067441931));
#324696=CARTESIAN_POINT('Ctrl Pts',(-1.56386617840707,2.70000000000408,
-3.72905519462682));
#324697=CARTESIAN_POINT('Ctrl Pts',(-1.57685980730779,2.70000000000408,
-3.78818228384373));
#324698=CARTESIAN_POINT('Ctrl Pts',(-1.58522695273552,2.7,-3.8452561404863));
#324699=CARTESIAN_POINT('Ctrl Pts',(-1.59579187190059,2.7,-4.04559018005418));
#324700=CARTESIAN_POINT('Ctrl Pts',(-1.58808709236768,2.7,-4.24179194839253));
#324701=CARTESIAN_POINT('Ctrl Pts',(-1.52363415300006,2.7,-4.49900422000002));
#324702=CARTESIAN_POINT('Origin',(-5.66300478732629E-14,15.2,-1.77635683940025E-14));
#324703=CARTESIAN_POINT('',(-1.20083826600006,2.7,-4.59570315100002));
#324704=CARTESIAN_POINT('',(-1.20083826600006,12.2,-4.59570315100001));
#324705=CARTESIAN_POINT('Origin',(-5.66300478732629E-14,2.7,-1.92943768261394E-14));
#324706=CARTESIAN_POINT('Ctrl Pts',(-1.20083826600006,12.2,-4.59570315100001));
#324707=CARTESIAN_POINT('Ctrl Pts',(-1.20083826600006,5.2,-4.59570315100001));
#324708=CARTESIAN_POINT('Ctrl Pts',(-1.20083826600006,2.2,-4.59570315100001));
#324709=CARTESIAN_POINT('Ctrl Pts',(-1.20044580000006,12.2,-4.59534252100001));
#324710=CARTESIAN_POINT('Ctrl Pts',(-1.20044580000006,5.2,-4.59534252100001));
#324711=CARTESIAN_POINT('Ctrl Pts',(-1.20044580000006,2.2,-4.59534252100001));
#324712=CARTESIAN_POINT('Ctrl Pts',(-1.19966130200006,12.2,-4.59462129000002));
#324713=CARTESIAN_POINT('Ctrl Pts',(-1.19966130200006,5.2,-4.59462129000002));
#324714=CARTESIAN_POINT('Ctrl Pts',(-1.19966130200006,2.2,-4.59462129000002));
#324715=CARTESIAN_POINT('Ctrl Pts',(-1.19848586200006,12.2,-4.59353952500001));
#324716=CARTESIAN_POINT('Ctrl Pts',(-1.19848586200006,5.2,-4.59353952500001));
#324717=CARTESIAN_POINT('Ctrl Pts',(-1.19848586200006,2.2,-4.59353952500001));
#324718=CARTESIAN_POINT('Ctrl Pts',(-1.19692122000005,12.2,-4.59209734200002));
#324719=CARTESIAN_POINT('Ctrl Pts',(-1.19692122000005,5.2,-4.59209734200002));
#324720=CARTESIAN_POINT('Ctrl Pts',(-1.19692122000005,2.2,-4.59209734200002));
#324721=CARTESIAN_POINT('Ctrl Pts',(-1.19496977000005,12.2,-4.59029489100002));
#324722=CARTESIAN_POINT('Ctrl Pts',(-1.19496977000005,5.2,-4.59029489100002));
#324723=CARTESIAN_POINT('Ctrl Pts',(-1.19496977000005,2.2,-4.59029489100002));
#324724=CARTESIAN_POINT('Ctrl Pts',(-1.19302267400006,12.2,-4.58849272400002));
#324725=CARTESIAN_POINT('Ctrl Pts',(-1.19302267400006,5.2,-4.58849272400002));
#324726=CARTESIAN_POINT('Ctrl Pts',(-1.19302267400006,2.2,-4.58849272400002));
#324727=CARTESIAN_POINT('Ctrl Pts',(-1.19107993200006,12.2,-4.58669084000002));
#324728=CARTESIAN_POINT('Ctrl Pts',(-1.19107993200006,5.2,-4.58669084000002));
#324729=CARTESIAN_POINT('Ctrl Pts',(-1.19107993200006,2.2,-4.58669084000002));
#324730=CARTESIAN_POINT('Ctrl Pts',(-1.18914154200006,12.2,-4.58488924600001));
#324731=CARTESIAN_POINT('Ctrl Pts',(-1.18914154200006,5.2,-4.58488924600001));
#324732=CARTESIAN_POINT('Ctrl Pts',(-1.18914154200006,2.2,-4.58488924600001));
#324733=CARTESIAN_POINT('Ctrl Pts',(-1.18720750800006,12.2,-4.58308794500002));
#324734=CARTESIAN_POINT('Ctrl Pts',(-1.18720750800006,5.2,-4.58308794500002));
#324735=CARTESIAN_POINT('Ctrl Pts',(-1.18720750800006,2.2,-4.58308794500002));
#324736=CARTESIAN_POINT('Ctrl Pts',(-1.18527782700006,12.2,-4.58128694600001));
#324737=CARTESIAN_POINT('Ctrl Pts',(-1.18527782700006,5.2,-4.58128694600001));
#324738=CARTESIAN_POINT('Ctrl Pts',(-1.18527782700006,2.2,-4.58128694600001));
#324739=CARTESIAN_POINT('Ctrl Pts',(-1.18335250000006,12.2,-4.57948626000002));
#324740=CARTESIAN_POINT('Ctrl Pts',(-1.18335250000006,5.2,-4.57948626000002));
#324741=CARTESIAN_POINT('Ctrl Pts',(-1.18335250000006,2.2,-4.57948626000002));
#324742=CARTESIAN_POINT('Ctrl Pts',(-1.18143152900006,12.2,-4.57768589700001));
#324743=CARTESIAN_POINT('Ctrl Pts',(-1.18143152900006,5.2,-4.57768589700001));
#324744=CARTESIAN_POINT('Ctrl Pts',(-1.18143152900006,2.2,-4.57768589700001));
#324745=CARTESIAN_POINT('Ctrl Pts',(-1.17951491300005,12.2,-4.57588586700002));
#324746=CARTESIAN_POINT('Ctrl Pts',(-1.17951491300005,5.2,-4.57588586700002));
#324747=CARTESIAN_POINT('Ctrl Pts',(-1.17951491300005,2.2,-4.57588586700002));
#324748=CARTESIAN_POINT('Ctrl Pts',(-1.17760265200006,12.2,-4.57408618200001));
#324749=CARTESIAN_POINT('Ctrl Pts',(-1.17760265200006,5.2,-4.57408618200001));
#324750=CARTESIAN_POINT('Ctrl Pts',(-1.17760265200006,2.2,-4.57408618200001));
#324751=CARTESIAN_POINT('Ctrl Pts',(-1.17569474700006,12.2,-4.57228685000001));
#324752=CARTESIAN_POINT('Ctrl Pts',(-1.17569474700006,5.2,-4.57228685000001));
#324753=CARTESIAN_POINT('Ctrl Pts',(-1.17569474700006,2.2,-4.57228685000001));
#324754=CARTESIAN_POINT('Ctrl Pts',(-1.17379119700006,12.2,-4.57048788200002));
#324755=CARTESIAN_POINT('Ctrl Pts',(-1.17379119700006,5.2,-4.57048788200002));
#324756=CARTESIAN_POINT('Ctrl Pts',(-1.17379119700006,2.2,-4.57048788200002));
#324757=CARTESIAN_POINT('Ctrl Pts',(-1.17189200400006,12.2,-4.56868928400001));
#324758=CARTESIAN_POINT('Ctrl Pts',(-1.17189200400006,5.2,-4.56868928400001));
#324759=CARTESIAN_POINT('Ctrl Pts',(-1.17189200400006,2.2,-4.56868928400001));
#324760=CARTESIAN_POINT('Ctrl Pts',(-1.16999716800006,12.2,-4.56689106400002));
#324761=CARTESIAN_POINT('Ctrl Pts',(-1.16999716800006,5.2,-4.56689106400002));
#324762=CARTESIAN_POINT('Ctrl Pts',(-1.16999716800006,2.2,-4.56689106400002));
#324763=CARTESIAN_POINT('Ctrl Pts',(-1.16810668600006,12.2,-4.56509323000001));
#324764=CARTESIAN_POINT('Ctrl Pts',(-1.16810668600006,5.2,-4.56509323000001));
#324765=CARTESIAN_POINT('Ctrl Pts',(-1.16810668600006,2.2,-4.56509323000001));
#324766=CARTESIAN_POINT('Ctrl Pts',(-1.16622056200006,12.2,-4.56329579100001));
#324767=CARTESIAN_POINT('Ctrl Pts',(-1.16622056200006,5.2,-4.56329579100001));
#324768=CARTESIAN_POINT('Ctrl Pts',(-1.16622056200006,2.2,-4.56329579100001));
#324769=CARTESIAN_POINT('Ctrl Pts',(-1.16433879500006,12.2,-4.56149875400001));
#324770=CARTESIAN_POINT('Ctrl Pts',(-1.16433879500006,5.2,-4.56149875400001));
#324771=CARTESIAN_POINT('Ctrl Pts',(-1.16433879500006,2.2,-4.56149875400001));
#324772=CARTESIAN_POINT('Ctrl Pts',(-1.16246138400006,12.2,-4.55970212800001));
#324773=CARTESIAN_POINT('Ctrl Pts',(-1.16246138400006,5.2,-4.55970212800001));
#324774=CARTESIAN_POINT('Ctrl Pts',(-1.16246138400006,2.2,-4.55970212800001));
#324775=CARTESIAN_POINT('Ctrl Pts',(-1.16058832900006,12.2,-4.55790592300001));
#324776=CARTESIAN_POINT('Ctrl Pts',(-1.16058832900006,5.2,-4.55790592300001));
#324777=CARTESIAN_POINT('Ctrl Pts',(-1.16058832900006,2.2,-4.55790592300001));
#324778=CARTESIAN_POINT('Ctrl Pts',(-1.15871963300005,12.2,-4.55611014800001));
#324779=CARTESIAN_POINT('Ctrl Pts',(-1.15871963300005,5.2,-4.55611014800001));
#324780=CARTESIAN_POINT('Ctrl Pts',(-1.15871963300005,2.2,-4.55611014800001));
#324781=CARTESIAN_POINT('Ctrl Pts',(-1.15685529300006,12.2,-4.55431481100002));
#324782=CARTESIAN_POINT('Ctrl Pts',(-1.15685529300006,5.2,-4.55431481100002));
#324783=CARTESIAN_POINT('Ctrl Pts',(-1.15685529300006,2.2,-4.55431481100002));
#324784=CARTESIAN_POINT('Ctrl Pts',(-1.15499531100006,12.2,-4.55251992200001));
#324785=CARTESIAN_POINT('Ctrl Pts',(-1.15499531100006,5.2,-4.55251992200001));
#324786=CARTESIAN_POINT('Ctrl Pts',(-1.15499531100006,2.2,-4.55251992200001));
#324787=CARTESIAN_POINT('Ctrl Pts',(-1.15313968500006,12.2,-4.55072549000001));
#324788=CARTESIAN_POINT('Ctrl Pts',(-1.15313968500006,5.2,-4.55072549000001));
#324789=CARTESIAN_POINT('Ctrl Pts',(-1.15313968500006,2.2,-4.55072549000001));
#324790=CARTESIAN_POINT('Ctrl Pts',(-1.15128841800006,12.2,-4.54893152300002));
#324791=CARTESIAN_POINT('Ctrl Pts',(-1.15128841800006,5.2,-4.54893152300002));
#324792=CARTESIAN_POINT('Ctrl Pts',(-1.15128841800006,2.2,-4.54893152300002));
#324793=CARTESIAN_POINT('Ctrl Pts',(-1.14944150700006,12.2,-4.54713802900002));
#324794=CARTESIAN_POINT('Ctrl Pts',(-1.14944150700006,5.2,-4.54713802900002));
#324795=CARTESIAN_POINT('Ctrl Pts',(-1.14944150700006,2.2,-4.54713802900002));
#324796=CARTESIAN_POINT('Ctrl Pts',(-1.14759895400006,12.2,-4.54534501800001));
#324797=CARTESIAN_POINT('Ctrl Pts',(-1.14759895400006,5.2,-4.54534501800001));
#324798=CARTESIAN_POINT('Ctrl Pts',(-1.14759895400006,2.2,-4.54534501800001));
#324799=CARTESIAN_POINT('Ctrl Pts',(-1.14576075900006,12.2,-4.54355249800001));
#324800=CARTESIAN_POINT('Ctrl Pts',(-1.14576075900006,5.2,-4.54355249800001));
#324801=CARTESIAN_POINT('Ctrl Pts',(-1.14576075900006,2.2,-4.54355249800001));
#324802=CARTESIAN_POINT('Ctrl Pts',(-1.14392692100005,12.2,-4.54176047800001));
#324803=CARTESIAN_POINT('Ctrl Pts',(-1.14392692100005,5.2,-4.54176047800001));
#324804=CARTESIAN_POINT('Ctrl Pts',(-1.14392692100005,2.2,-4.54176047800001));
#324805=CARTESIAN_POINT('Ctrl Pts',(-1.14209744100006,12.2,-4.53996896700001));
#324806=CARTESIAN_POINT('Ctrl Pts',(-1.14209744100006,5.2,-4.53996896700001));
#324807=CARTESIAN_POINT('Ctrl Pts',(-1.14209744100006,2.2,-4.53996896700001));
#324808=CARTESIAN_POINT('Ctrl Pts',(-1.14027231800006,12.2,-4.53817797400001));
#324809=CARTESIAN_POINT('Ctrl Pts',(-1.14027231800006,5.2,-4.53817797400001));
#324810=CARTESIAN_POINT('Ctrl Pts',(-1.14027231800006,2.2,-4.53817797400001));
#324811=CARTESIAN_POINT('Ctrl Pts',(-1.13845155200006,12.2,-4.53638750700001));
#324812=CARTESIAN_POINT('Ctrl Pts',(-1.13845155200006,5.2,-4.53638750700001));
#324813=CARTESIAN_POINT('Ctrl Pts',(-1.13845155200006,2.2,-4.53638750700001));
#324814=CARTESIAN_POINT('Ctrl Pts',(-1.13663514400006,12.2,-4.53459757600001));
#324815=CARTESIAN_POINT('Ctrl Pts',(-1.13663514400006,5.2,-4.53459757600001));
#324816=CARTESIAN_POINT('Ctrl Pts',(-1.13663514400006,2.2,-4.53459757600001));
#324817=CARTESIAN_POINT('Ctrl Pts',(-1.13482309400006,12.2,-4.53280818900001));
#324818=CARTESIAN_POINT('Ctrl Pts',(-1.13482309400006,5.2,-4.53280818900001));
#324819=CARTESIAN_POINT('Ctrl Pts',(-1.13482309400006,2.2,-4.53280818900001));
#324820=CARTESIAN_POINT('Ctrl Pts',(-1.13301540100006,12.2,-4.53101935600001));
#324821=CARTESIAN_POINT('Ctrl Pts',(-1.13301540100006,5.2,-4.53101935600001));
#324822=CARTESIAN_POINT('Ctrl Pts',(-1.13301540100006,2.2,-4.53101935600001));
#324823=CARTESIAN_POINT('Ctrl Pts',(-1.13121206600006,12.2,-4.52923108400002));
#324824=CARTESIAN_POINT('Ctrl Pts',(-1.13121206600006,5.2,-4.52923108400002));
#324825=CARTESIAN_POINT('Ctrl Pts',(-1.13121206600006,2.2,-4.52923108400002));
#324826=CARTESIAN_POINT('Ctrl Pts',(-1.12941308600006,12.2,-4.52744338400001));
#324827=CARTESIAN_POINT('Ctrl Pts',(-1.12941308600006,5.2,-4.52744338400001));
#324828=CARTESIAN_POINT('Ctrl Pts',(-1.12941308600006,2.2,-4.52744338400001));
#324829=CARTESIAN_POINT('Ctrl Pts',(-1.12761846500006,12.2,-4.52565626400002));
#324830=CARTESIAN_POINT('Ctrl Pts',(-1.12761846500006,5.2,-4.52565626400002));
#324831=CARTESIAN_POINT('Ctrl Pts',(-1.12761846500006,2.2,-4.52565626400002));
#324832=CARTESIAN_POINT('Ctrl Pts',(-1.12582820100006,12.2,-4.52386973300001));
#324833=CARTESIAN_POINT('Ctrl Pts',(-1.12582820100006,5.2,-4.52386973300001));
#324834=CARTESIAN_POINT('Ctrl Pts',(-1.12582820100006,2.2,-4.52386973300001));
#324835=CARTESIAN_POINT('Ctrl Pts',(-1.12404229400005,12.2,-4.52208379900001));
#324836=CARTESIAN_POINT('Ctrl Pts',(-1.12404229400005,5.2,-4.52208379900001));
#324837=CARTESIAN_POINT('Ctrl Pts',(-1.12404229400005,2.2,-4.52208379900001));
#324838=CARTESIAN_POINT('Ctrl Pts',(-1.12226074300006,12.2,-4.52029847200001));
#324839=CARTESIAN_POINT('Ctrl Pts',(-1.12226074300006,5.2,-4.52029847200001));
#324840=CARTESIAN_POINT('Ctrl Pts',(-1.12226074300006,2.2,-4.52029847200001));
#324841=CARTESIAN_POINT('Ctrl Pts',(-1.12048354900006,12.2,-4.51851376100001));
#324842=CARTESIAN_POINT('Ctrl Pts',(-1.12048354900006,5.2,-4.51851376100001));
#324843=CARTESIAN_POINT('Ctrl Pts',(-1.12048354900006,2.2,-4.51851376100001));
#324844=CARTESIAN_POINT('Ctrl Pts',(-1.11871071100005,12.2,-4.51672967500001));
#324845=CARTESIAN_POINT('Ctrl Pts',(-1.11871071100005,5.2,-4.51672967500001));
#324846=CARTESIAN_POINT('Ctrl Pts',(-1.11871071100005,2.2,-4.51672967500001));
#324847=CARTESIAN_POINT('Ctrl Pts',(-1.11694223100006,12.2,-4.51494622200002));
#324848=CARTESIAN_POINT('Ctrl Pts',(-1.11694223100006,5.2,-4.51494622200002));
#324849=CARTESIAN_POINT('Ctrl Pts',(-1.11694223100006,2.2,-4.51494622200002));
#324850=CARTESIAN_POINT('Ctrl Pts',(-1.11517810600006,12.2,-4.51316341200001));
#324851=CARTESIAN_POINT('Ctrl Pts',(-1.11517810600006,5.2,-4.51316341200001));
#324852=CARTESIAN_POINT('Ctrl Pts',(-1.11517810600006,2.2,-4.51316341200001));
#324853=CARTESIAN_POINT('Ctrl Pts',(-1.11341833700005,12.2,-4.51138125500002));
#324854=CARTESIAN_POINT('Ctrl Pts',(-1.11341833700005,5.2,-4.51138125500002));
#324855=CARTESIAN_POINT('Ctrl Pts',(-1.11341833700005,2.2,-4.51138125500002));
#324856=CARTESIAN_POINT('Ctrl Pts',(-1.11166292300006,12.2,-4.50959975800002));
#324857=CARTESIAN_POINT('Ctrl Pts',(-1.11166292300006,5.2,-4.50959975800002));
#324858=CARTESIAN_POINT('Ctrl Pts',(-1.11166292300006,2.2,-4.50959975800002));
#324859=CARTESIAN_POINT('Ctrl Pts',(-1.10991186600006,12.2,-4.50781893000002));
#324860=CARTESIAN_POINT('Ctrl Pts',(-1.10991186600006,5.2,-4.50781893000002));
#324861=CARTESIAN_POINT('Ctrl Pts',(-1.10991186600006,2.2,-4.50781893000002));
#324862=CARTESIAN_POINT('Ctrl Pts',(-1.10816516400006,12.2,-4.50603878100001));
#324863=CARTESIAN_POINT('Ctrl Pts',(-1.10816516400006,5.2,-4.50603878100001));
#324864=CARTESIAN_POINT('Ctrl Pts',(-1.10816516400006,2.2,-4.50603878100001));
#324865=CARTESIAN_POINT('Ctrl Pts',(-1.10642281700006,12.2,-4.50425932100002));
#324866=CARTESIAN_POINT('Ctrl Pts',(-1.10642281700006,5.2,-4.50425932100002));
#324867=CARTESIAN_POINT('Ctrl Pts',(-1.10642281700006,2.2,-4.50425932100002));
#324868=CARTESIAN_POINT('Ctrl Pts',(-1.10468482400006,12.2,-4.50248055700001));
#324869=CARTESIAN_POINT('Ctrl Pts',(-1.10468482400006,5.2,-4.50248055700001));
#324870=CARTESIAN_POINT('Ctrl Pts',(-1.10468482400006,2.2,-4.50248055700001));
#324871=CARTESIAN_POINT('Ctrl Pts',(-1.10295118700006,12.2,-4.50070249900001));
#324872=CARTESIAN_POINT('Ctrl Pts',(-1.10295118700006,5.2,-4.50070249900001));
#324873=CARTESIAN_POINT('Ctrl Pts',(-1.10295118700006,2.2,-4.50070249900001));
#324874=CARTESIAN_POINT('Ctrl Pts',(-1.10122190400006,12.2,-4.49892515500002));
#324875=CARTESIAN_POINT('Ctrl Pts',(-1.10122190400006,5.2,-4.49892515500002));
#324876=CARTESIAN_POINT('Ctrl Pts',(-1.10122190400006,2.2,-4.49892515500002));
#324877=CARTESIAN_POINT('Ctrl Pts',(-1.09949697400006,12.2,-4.49714853700002));
#324878=CARTESIAN_POINT('Ctrl Pts',(-1.09949697400006,5.2,-4.49714853700002));
#324879=CARTESIAN_POINT('Ctrl Pts',(-1.09949697400006,2.2,-4.49714853700002));
#324880=CARTESIAN_POINT('Ctrl Pts',(-1.09777639800006,12.2,-4.49537265200001));
#324881=CARTESIAN_POINT('Ctrl Pts',(-1.09777639800006,5.2,-4.49537265200001));
#324882=CARTESIAN_POINT('Ctrl Pts',(-1.09777639800006,2.2,-4.49537265200001));
#324883=CARTESIAN_POINT('Ctrl Pts',(-1.09606017600006,12.2,-4.49359750800001));
#324884=CARTESIAN_POINT('Ctrl Pts',(-1.09606017600006,5.2,-4.49359750800001));
#324885=CARTESIAN_POINT('Ctrl Pts',(-1.09606017600006,2.2,-4.49359750800001));
#324886=CARTESIAN_POINT('Ctrl Pts',(-1.09434830700006,12.2,-4.49182311700001));
#324887=CARTESIAN_POINT('Ctrl Pts',(-1.09434830700006,5.2,-4.49182311700001));
#324888=CARTESIAN_POINT('Ctrl Pts',(-1.09434830700006,2.2,-4.49182311700001));
#324889=CARTESIAN_POINT('Ctrl Pts',(-1.09264079000006,12.2,-4.49004948600002));
#324890=CARTESIAN_POINT('Ctrl Pts',(-1.09264079000006,5.2,-4.49004948600002));
#324891=CARTESIAN_POINT('Ctrl Pts',(-1.09264079000006,2.2,-4.49004948600002));
#324892=CARTESIAN_POINT('Ctrl Pts',(-1.09093762600006,12.2,-4.48827662500001));
#324893=CARTESIAN_POINT('Ctrl Pts',(-1.09093762600006,5.2,-4.48827662500001));
#324894=CARTESIAN_POINT('Ctrl Pts',(-1.09093762600006,2.2,-4.48827662500001));
#324895=CARTESIAN_POINT('Ctrl Pts',(-1.08923881400006,12.2,-4.48650454200001));
#324896=CARTESIAN_POINT('Ctrl Pts',(-1.08923881400006,5.2,-4.48650454200001));
#324897=CARTESIAN_POINT('Ctrl Pts',(-1.08923881400006,2.2,-4.48650454200001));
#324898=CARTESIAN_POINT('Ctrl Pts',(-1.08754435300006,12.2,-4.48473324900001));
#324899=CARTESIAN_POINT('Ctrl Pts',(-1.08754435300006,5.2,-4.48473324900001));
#324900=CARTESIAN_POINT('Ctrl Pts',(-1.08754435300006,2.2,-4.48473324900001));
#324901=CARTESIAN_POINT('Ctrl Pts',(-1.08585424400006,12.2,-4.48296275200001));
#324902=CARTESIAN_POINT('Ctrl Pts',(-1.08585424400006,5.2,-4.48296275200001));
#324903=CARTESIAN_POINT('Ctrl Pts',(-1.08585424400006,2.2,-4.48296275200001));
#324904=CARTESIAN_POINT('Ctrl Pts',(-1.08416848500006,12.2,-4.48119306300002));
#324905=CARTESIAN_POINT('Ctrl Pts',(-1.08416848500006,5.2,-4.48119306300002));
#324906=CARTESIAN_POINT('Ctrl Pts',(-1.08416848500006,2.2,-4.48119306300002));
#324907=CARTESIAN_POINT('Ctrl Pts',(-1.08248707700006,12.2,-4.47942418800002));
#324908=CARTESIAN_POINT('Ctrl Pts',(-1.08248707700006,5.2,-4.47942418800002));
#324909=CARTESIAN_POINT('Ctrl Pts',(-1.08248707700006,2.2,-4.47942418800002));
#324910=CARTESIAN_POINT('Ctrl Pts',(-1.08081001900006,12.2,-4.47765613900001));
#324911=CARTESIAN_POINT('Ctrl Pts',(-1.08081001900006,5.2,-4.47765613900001));
#324912=CARTESIAN_POINT('Ctrl Pts',(-1.08081001900006,2.2,-4.47765613900001));
#324913=CARTESIAN_POINT('Ctrl Pts',(-1.07913731000005,12.2,-4.47588892300002));
#324914=CARTESIAN_POINT('Ctrl Pts',(-1.07913731000005,5.2,-4.47588892300002));
#324915=CARTESIAN_POINT('Ctrl Pts',(-1.07913731000005,2.2,-4.47588892300002));
#324916=CARTESIAN_POINT('Ctrl Pts',(-1.07746895100005,12.2,-4.47412255100001));
#324917=CARTESIAN_POINT('Ctrl Pts',(-1.07746895100005,5.2,-4.47412255100001));
#324918=CARTESIAN_POINT('Ctrl Pts',(-1.07746895100005,2.2,-4.47412255100001));
#324919=CARTESIAN_POINT('Ctrl Pts',(-1.07580494000006,12.2,-4.47235703200001));
#324920=CARTESIAN_POINT('Ctrl Pts',(-1.07580494000006,5.2,-4.47235703200001));
#324921=CARTESIAN_POINT('Ctrl Pts',(-1.07580494000006,2.2,-4.47235703200001));
#324922=CARTESIAN_POINT('Ctrl Pts',(-1.07414527700006,12.2,-4.47059237500001));
#324923=CARTESIAN_POINT('Ctrl Pts',(-1.07414527700006,5.2,-4.47059237500001));
#324924=CARTESIAN_POINT('Ctrl Pts',(-1.07414527700006,2.2,-4.47059237500001));
#324925=CARTESIAN_POINT('Ctrl Pts',(-1.07248996200005,12.2,-4.46882858800001));
#324926=CARTESIAN_POINT('Ctrl Pts',(-1.07248996200005,5.2,-4.46882858800001));
#324927=CARTESIAN_POINT('Ctrl Pts',(-1.07248996200005,2.2,-4.46882858800001));
#324928=CARTESIAN_POINT('Ctrl Pts',(-1.07083899300006,12.2,-4.46706568300002));
#324929=CARTESIAN_POINT('Ctrl Pts',(-1.07083899300006,5.2,-4.46706568300002));
#324930=CARTESIAN_POINT('Ctrl Pts',(-1.07083899300006,2.2,-4.46706568300002));
#324931=CARTESIAN_POINT('Ctrl Pts',(-1.06919237200006,12.2,-4.46530366700001));
#324932=CARTESIAN_POINT('Ctrl Pts',(-1.06919237200006,5.2,-4.46530366700001));
#324933=CARTESIAN_POINT('Ctrl Pts',(-1.06919237200006,2.2,-4.46530366700001));
#324934=CARTESIAN_POINT('Ctrl Pts',(-1.06755009600006,12.2,-4.46354255000001));
#324935=CARTESIAN_POINT('Ctrl Pts',(-1.06755009600006,5.2,-4.46354255000001));
#324936=CARTESIAN_POINT('Ctrl Pts',(-1.06755009600006,2.2,-4.46354255000001));
#324937=CARTESIAN_POINT('Ctrl Pts',(-1.06591216500005,12.2,-4.46178234200001));
#324938=CARTESIAN_POINT('Ctrl Pts',(-1.06591216500005,5.2,-4.46178234200001));
#324939=CARTESIAN_POINT('Ctrl Pts',(-1.06591216500005,2.2,-4.46178234200001));
#324940=CARTESIAN_POINT('Ctrl Pts',(-1.06427858000006,12.2,-4.46002305000002));
#324941=CARTESIAN_POINT('Ctrl Pts',(-1.06427858000006,5.2,-4.46002305000002));
#324942=CARTESIAN_POINT('Ctrl Pts',(-1.06427858000006,2.2,-4.46002305000002));
#324943=CARTESIAN_POINT('Ctrl Pts',(-1.06264933900006,12.2,-4.45826468700002));
#324944=CARTESIAN_POINT('Ctrl Pts',(-1.06264933900006,5.2,-4.45826468700002));
#324945=CARTESIAN_POINT('Ctrl Pts',(-1.06264933900006,2.2,-4.45826468700002));
#324946=CARTESIAN_POINT('Ctrl Pts',(-1.06102444200006,12.2,-4.45650725900002));
#324947=CARTESIAN_POINT('Ctrl Pts',(-1.06102444200006,5.2,-4.45650725900002));
#324948=CARTESIAN_POINT('Ctrl Pts',(-1.06102444200006,2.2,-4.45650725900002));
#324949=CARTESIAN_POINT('Ctrl Pts',(-1.05940388700006,12.2,-4.45475077800001));
#324950=CARTESIAN_POINT('Ctrl Pts',(-1.05940388700006,5.2,-4.45475077800001));
#324951=CARTESIAN_POINT('Ctrl Pts',(-1.05940388700006,2.2,-4.45475077800001));
#324952=CARTESIAN_POINT('Ctrl Pts',(-1.05778767600005,12.2,-4.45299525200001));
#324953=CARTESIAN_POINT('Ctrl Pts',(-1.05778767600005,5.2,-4.45299525200001));
#324954=CARTESIAN_POINT('Ctrl Pts',(-1.05778767600005,2.2,-4.45299525200001));
#324955=CARTESIAN_POINT('Ctrl Pts',(-1.05617580600006,12.2,-4.45124069000002));
#324956=CARTESIAN_POINT('Ctrl Pts',(-1.05617580600006,5.2,-4.45124069000002));
#324957=CARTESIAN_POINT('Ctrl Pts',(-1.05617580600006,2.2,-4.45124069000002));
#324958=CARTESIAN_POINT('Ctrl Pts',(-1.05456827700006,12.2,-4.44948710300002));
#324959=CARTESIAN_POINT('Ctrl Pts',(-1.05456827700006,5.2,-4.44948710300002));
#324960=CARTESIAN_POINT('Ctrl Pts',(-1.05456827700006,2.2,-4.44948710300002));
#324961=CARTESIAN_POINT('Ctrl Pts',(-1.05296508800006,12.2,-4.44773449800001));
#324962=CARTESIAN_POINT('Ctrl Pts',(-1.05296508800006,5.2,-4.44773449800001));
#324963=CARTESIAN_POINT('Ctrl Pts',(-1.05296508800006,2.2,-4.44773449800001));
#324964=CARTESIAN_POINT('Ctrl Pts',(-1.05136624100005,12.2,-4.44598288600002));
#324965=CARTESIAN_POINT('Ctrl Pts',(-1.05136624100005,5.2,-4.44598288600002));
#324966=CARTESIAN_POINT('Ctrl Pts',(-1.05136624100005,2.2,-4.44598288600002));
#324967=CARTESIAN_POINT('Ctrl Pts',(-1.04977173200006,12.2,-4.44423227700002));
#324968=CARTESIAN_POINT('Ctrl Pts',(-1.04977173200006,5.2,-4.44423227700002));
#324969=CARTESIAN_POINT('Ctrl Pts',(-1.04977173200006,2.2,-4.44423227700002));
#324970=CARTESIAN_POINT('Ctrl Pts',(-1.04818156000006,12.2,-4.44248267900001));
#324971=CARTESIAN_POINT('Ctrl Pts',(-1.04818156000006,5.2,-4.44248267900001));
#324972=CARTESIAN_POINT('Ctrl Pts',(-1.04818156000006,2.2,-4.44248267900001));
#324973=CARTESIAN_POINT('Ctrl Pts',(-1.04659572800006,12.2,-4.44073410200001));
#324974=CARTESIAN_POINT('Ctrl Pts',(-1.04659572800006,5.2,-4.44073410200001));
#324975=CARTESIAN_POINT('Ctrl Pts',(-1.04659572800006,2.2,-4.44073410200001));
#324976=CARTESIAN_POINT('Ctrl Pts',(-1.04501423200006,12.2,-4.43898655500002));
#324977=CARTESIAN_POINT('Ctrl Pts',(-1.04501423200006,5.2,-4.43898655500002));
#324978=CARTESIAN_POINT('Ctrl Pts',(-1.04501423200006,2.2,-4.43898655500002));
#324979=CARTESIAN_POINT('Ctrl Pts',(-1.04343707300006,12.2,-4.43724004900002));
#324980=CARTESIAN_POINT('Ctrl Pts',(-1.04343707300006,5.2,-4.43724004900002));
#324981=CARTESIAN_POINT('Ctrl Pts',(-1.04343707300006,2.2,-4.43724004900002));
#324982=CARTESIAN_POINT('Ctrl Pts',(-1.04186424800006,12.2,-4.43549459200002));
#324983=CARTESIAN_POINT('Ctrl Pts',(-1.04186424800006,5.2,-4.43549459200002));
#324984=CARTESIAN_POINT('Ctrl Pts',(-1.04186424800006,2.2,-4.43549459200002));
#324985=CARTESIAN_POINT('Ctrl Pts',(-1.04029575900006,12.2,-4.43375019500001));
#324986=CARTESIAN_POINT('Ctrl Pts',(-1.04029575900006,5.2,-4.43375019500001));
#324987=CARTESIAN_POINT('Ctrl Pts',(-1.04029575900006,2.2,-4.43375019500001));
#324988=CARTESIAN_POINT('Ctrl Pts',(-1.03873160300005,12.2,-4.43200686600001));
#324989=CARTESIAN_POINT('Ctrl Pts',(-1.03873160300005,5.2,-4.43200686600001));
#324990=CARTESIAN_POINT('Ctrl Pts',(-1.03873160300005,2.2,-4.43200686600001));
#324991=CARTESIAN_POINT('Ctrl Pts',(-1.03717178100006,12.2,-4.43026461500001));
#324992=CARTESIAN_POINT('Ctrl Pts',(-1.03717178100006,5.2,-4.43026461500001));
#324993=CARTESIAN_POINT('Ctrl Pts',(-1.03717178100006,2.2,-4.43026461500001));
#324994=CARTESIAN_POINT('Ctrl Pts',(-1.03561629200006,12.2,-4.42852345200002));
#324995=CARTESIAN_POINT('Ctrl Pts',(-1.03561629200006,5.2,-4.42852345200002));
#324996=CARTESIAN_POINT('Ctrl Pts',(-1.03561629200006,2.2,-4.42852345200002));
#324997=CARTESIAN_POINT('Ctrl Pts',(-1.03406513300005,12.2,-4.42678338600001));
#324998=CARTESIAN_POINT('Ctrl Pts',(-1.03406513300005,5.2,-4.42678338600001));
#324999=CARTESIAN_POINT('Ctrl Pts',(-1.03406513300005,2.2,-4.42678338600001));
#325000=CARTESIAN_POINT('Ctrl Pts',(-1.03251830500006,12.2,-4.42504442600002));
#325001=CARTESIAN_POINT('Ctrl Pts',(-1.03251830500006,5.2,-4.42504442600002));
#325002=CARTESIAN_POINT('Ctrl Pts',(-1.03251830500006,2.2,-4.42504442600002));
#325003=CARTESIAN_POINT('Ctrl Pts',(-1.03097580700006,12.2,-4.42330658300001));
#325004=CARTESIAN_POINT('Ctrl Pts',(-1.03097580700006,5.2,-4.42330658300001));
#325005=CARTESIAN_POINT('Ctrl Pts',(-1.03097580700006,2.2,-4.42330658300001));
#325006=CARTESIAN_POINT('Ctrl Pts',(-1.02943763800006,12.2,-4.42156986600001));
#325007=CARTESIAN_POINT('Ctrl Pts',(-1.02943763800006,5.2,-4.42156986600001));
#325008=CARTESIAN_POINT('Ctrl Pts',(-1.02943763800006,2.2,-4.42156986600001));
#325009=CARTESIAN_POINT('Ctrl Pts',(-1.02790379700005,12.2,-4.41983428400002));
#325010=CARTESIAN_POINT('Ctrl Pts',(-1.02790379700005,5.2,-4.41983428400002));
#325011=CARTESIAN_POINT('Ctrl Pts',(-1.02790379700005,2.2,-4.41983428400002));
#325012=CARTESIAN_POINT('Ctrl Pts',(-1.02637428300006,12.2,-4.41809984700001));
#325013=CARTESIAN_POINT('Ctrl Pts',(-1.02637428300006,5.2,-4.41809984700001));
#325014=CARTESIAN_POINT('Ctrl Pts',(-1.02637428300006,2.2,-4.41809984700001));
#325015=CARTESIAN_POINT('Ctrl Pts',(-1.02484909500006,12.2,-4.41636656500001));
#325016=CARTESIAN_POINT('Ctrl Pts',(-1.02484909500006,5.2,-4.41636656500001));
#325017=CARTESIAN_POINT('Ctrl Pts',(-1.02484909500006,2.2,-4.41636656500001));
#325018=CARTESIAN_POINT('Ctrl Pts',(-1.02332823300006,12.2,-4.41463444800001));
#325019=CARTESIAN_POINT('Ctrl Pts',(-1.02332823300006,5.2,-4.41463444800001));
#325020=CARTESIAN_POINT('Ctrl Pts',(-1.02332823300006,2.2,-4.41463444800001));
#325021=CARTESIAN_POINT('Ctrl Pts',(-1.02181169500006,12.2,-4.41290350400001));
#325022=CARTESIAN_POINT('Ctrl Pts',(-1.02181169500006,5.2,-4.41290350400001));
#325023=CARTESIAN_POINT('Ctrl Pts',(-1.02181169500006,2.2,-4.41290350400001));
#325024=CARTESIAN_POINT('Ctrl Pts',(-1.02029948100006,12.2,-4.41117374400001));
#325025=CARTESIAN_POINT('Ctrl Pts',(-1.02029948100006,5.2,-4.41117374400001));
#325026=CARTESIAN_POINT('Ctrl Pts',(-1.02029948100006,2.2,-4.41117374400001));
#325027=CARTESIAN_POINT('Ctrl Pts',(-1.01879158900006,12.2,-4.40944517800002));
#325028=CARTESIAN_POINT('Ctrl Pts',(-1.01879158900006,5.2,-4.40944517800002));
#325029=CARTESIAN_POINT('Ctrl Pts',(-1.01879158900006,2.2,-4.40944517800002));
#325030=CARTESIAN_POINT('Ctrl Pts',(-1.01728801800006,12.2,-4.40771781400001));
#325031=CARTESIAN_POINT('Ctrl Pts',(-1.01728801800006,5.2,-4.40771781400001));
#325032=CARTESIAN_POINT('Ctrl Pts',(-1.01728801800006,2.2,-4.40771781400001));
#325033=CARTESIAN_POINT('Ctrl Pts',(-1.01578876700006,12.2,-4.40599166300002));
#325034=CARTESIAN_POINT('Ctrl Pts',(-1.01578876700006,5.2,-4.40599166300002));
#325035=CARTESIAN_POINT('Ctrl Pts',(-1.01578876700006,2.2,-4.40599166300002));
#325036=CARTESIAN_POINT('Ctrl Pts',(-1.01429383600006,12.2,-4.40426673500002));
#325037=CARTESIAN_POINT('Ctrl Pts',(-1.01429383600006,5.2,-4.40426673500002));
#325038=CARTESIAN_POINT('Ctrl Pts',(-1.01429383600006,2.2,-4.40426673500002));
#325039=CARTESIAN_POINT('Ctrl Pts',(-1.01280322400006,12.2,-4.40254303900002));
#325040=CARTESIAN_POINT('Ctrl Pts',(-1.01280322400006,5.2,-4.40254303900002));
#325041=CARTESIAN_POINT('Ctrl Pts',(-1.01280322400006,2.2,-4.40254303900002));
#325042=CARTESIAN_POINT('Ctrl Pts',(-1.01131692900006,12.2,-4.40082058400002));
#325043=CARTESIAN_POINT('Ctrl Pts',(-1.01131692900006,5.2,-4.40082058400002));
#325044=CARTESIAN_POINT('Ctrl Pts',(-1.01131692900006,2.2,-4.40082058400002));
#325045=CARTESIAN_POINT('Ctrl Pts',(-1.00983494900006,12.2,-4.39909938100001));
#325046=CARTESIAN_POINT('Ctrl Pts',(-1.00983494900006,5.2,-4.39909938100001));
#325047=CARTESIAN_POINT('Ctrl Pts',(-1.00983494900006,2.2,-4.39909938100001));
#325048=CARTESIAN_POINT('Ctrl Pts',(-1.00835728600006,12.2,-4.39737943900001));
#325049=CARTESIAN_POINT('Ctrl Pts',(-1.00835728600006,5.2,-4.39737943900001));
#325050=CARTESIAN_POINT('Ctrl Pts',(-1.00835728600006,2.2,-4.39737943900001));
#325051=CARTESIAN_POINT('Ctrl Pts',(-1.00688393600006,12.2,-4.39566076900002));
#325052=CARTESIAN_POINT('Ctrl Pts',(-1.00688393600006,5.2,-4.39566076900002));
#325053=CARTESIAN_POINT('Ctrl Pts',(-1.00688393600006,2.2,-4.39566076900002));
#325054=CARTESIAN_POINT('Ctrl Pts',(-1.00541489900006,12.2,-4.39394337900001));
#325055=CARTESIAN_POINT('Ctrl Pts',(-1.00541489900006,5.2,-4.39394337900001));
#325056=CARTESIAN_POINT('Ctrl Pts',(-1.00541489900006,2.2,-4.39394337900001));
#325057=CARTESIAN_POINT('Ctrl Pts',(-1.00395017500006,12.2,-4.39222728000002));
#325058=CARTESIAN_POINT('Ctrl Pts',(-1.00395017500006,5.2,-4.39222728000002));
#325059=CARTESIAN_POINT('Ctrl Pts',(-1.00395017500006,2.2,-4.39222728000002));
#325060=CARTESIAN_POINT('Ctrl Pts',(-1.00248976100006,12.2,-4.39051248200002));
#325061=CARTESIAN_POINT('Ctrl Pts',(-1.00248976100006,5.2,-4.39051248200002));
#325062=CARTESIAN_POINT('Ctrl Pts',(-1.00248976100006,2.2,-4.39051248200002));
#325063=CARTESIAN_POINT('Ctrl Pts',(-1.00103365600006,12.2,-4.38879899400002));
#325064=CARTESIAN_POINT('Ctrl Pts',(-1.00103365600006,5.2,-4.38879899400002));
#325065=CARTESIAN_POINT('Ctrl Pts',(-1.00103365600006,2.2,-4.38879899400002));
#325066=CARTESIAN_POINT('Ctrl Pts',(-0.999581859000056,12.2,-4.38708682600002));
#325067=CARTESIAN_POINT('Ctrl Pts',(-0.999581859000056,5.2,-4.38708682600002));
#325068=CARTESIAN_POINT('Ctrl Pts',(-0.999581859000056,2.2,-4.38708682600002));
#325069=CARTESIAN_POINT('Ctrl Pts',(-0.998134371000056,12.2,-4.38537598800002));
#325070=CARTESIAN_POINT('Ctrl Pts',(-0.998134371000056,5.2,-4.38537598800002));
#325071=CARTESIAN_POINT('Ctrl Pts',(-0.998134371000056,2.2,-4.38537598800002));
#325072=CARTESIAN_POINT('Ctrl Pts',(-0.996691187000056,12.2,-4.38366649000002));
#325073=CARTESIAN_POINT('Ctrl Pts',(-0.996691187000056,5.2,-4.38366649000002));
#325074=CARTESIAN_POINT('Ctrl Pts',(-0.996691187000056,2.2,-4.38366649000002));
#325075=CARTESIAN_POINT('Ctrl Pts',(-0.995252310000057,12.2,-4.38195834100001));
#325076=CARTESIAN_POINT('Ctrl Pts',(-0.995252310000057,5.2,-4.38195834100001));
#325077=CARTESIAN_POINT('Ctrl Pts',(-0.995252310000057,2.2,-4.38195834100001));
#325078=CARTESIAN_POINT('Ctrl Pts',(-0.993817735000055,12.2,-4.38025155200001));
#325079=CARTESIAN_POINT('Ctrl Pts',(-0.993817735000055,5.2,-4.38025155200001));
#325080=CARTESIAN_POINT('Ctrl Pts',(-0.993817735000055,2.2,-4.38025155200001));
#325081=CARTESIAN_POINT('Ctrl Pts',(-0.992387463000056,12.2,-4.37854613300001));
#325082=CARTESIAN_POINT('Ctrl Pts',(-0.992387463000056,5.2,-4.37854613300001));
#325083=CARTESIAN_POINT('Ctrl Pts',(-0.992387463000056,2.2,-4.37854613300001));
#325084=CARTESIAN_POINT('Ctrl Pts',(-0.990961492000055,12.2,-4.37684209300001));
#325085=CARTESIAN_POINT('Ctrl Pts',(-0.990961492000055,5.2,-4.37684209300001));
#325086=CARTESIAN_POINT('Ctrl Pts',(-0.990961492000055,2.2,-4.37684209300001));
#325087=CARTESIAN_POINT('Ctrl Pts',(-0.989539821000056,12.2,-4.37513944100001));
#325088=CARTESIAN_POINT('Ctrl Pts',(-0.989539821000056,5.2,-4.37513944100001));
#325089=CARTESIAN_POINT('Ctrl Pts',(-0.989539821000056,2.2,-4.37513944100001));
#325090=CARTESIAN_POINT('Ctrl Pts',(-0.988122448000055,12.2,-4.37343819000001));
#325091=CARTESIAN_POINT('Ctrl Pts',(-0.988122448000055,5.2,-4.37343819000001));
#325092=CARTESIAN_POINT('Ctrl Pts',(-0.988122448000055,2.2,-4.37343819000001));
#325093=CARTESIAN_POINT('Ctrl Pts',(-0.986709372000056,12.2,-4.37173834700001));
#325094=CARTESIAN_POINT('Ctrl Pts',(-0.986709372000056,5.2,-4.37173834700001));
#325095=CARTESIAN_POINT('Ctrl Pts',(-0.986709372000056,2.2,-4.37173834700001));
#325096=CARTESIAN_POINT('Ctrl Pts',(-0.985300593000057,12.2,-4.37003992300002));
#325097=CARTESIAN_POINT('Ctrl Pts',(-0.985300593000057,5.2,-4.37003992300002));
#325098=CARTESIAN_POINT('Ctrl Pts',(-0.985300593000057,2.2,-4.37003992300002));
#325099=CARTESIAN_POINT('Ctrl Pts',(-0.983896107000056,12.2,-4.36834292900001));
#325100=CARTESIAN_POINT('Ctrl Pts',(-0.983896107000056,5.2,-4.36834292900001));
#325101=CARTESIAN_POINT('Ctrl Pts',(-0.983896107000056,2.2,-4.36834292900001));
#325102=CARTESIAN_POINT('Ctrl Pts',(-0.982495915000056,12.2,-4.36664737300001));
#325103=CARTESIAN_POINT('Ctrl Pts',(-0.982495915000056,5.2,-4.36664737300001));
#325104=CARTESIAN_POINT('Ctrl Pts',(-0.982495915000056,2.2,-4.36664737300001));
#325105=CARTESIAN_POINT('Ctrl Pts',(-0.981100015000056,12.2,-4.36495326700001));
#325106=CARTESIAN_POINT('Ctrl Pts',(-0.981100015000056,5.2,-4.36495326700001));
#325107=CARTESIAN_POINT('Ctrl Pts',(-0.981100015000056,2.2,-4.36495326700001));
#325108=CARTESIAN_POINT('Ctrl Pts',(-0.979708405000055,12.2,-4.36326061900001));
#325109=CARTESIAN_POINT('Ctrl Pts',(-0.979708405000055,5.2,-4.36326061900001));
#325110=CARTESIAN_POINT('Ctrl Pts',(-0.979708405000055,2.2,-4.36326061900001));
#325111=CARTESIAN_POINT('Ctrl Pts',(-0.978321085000056,12.2,-4.36156944000002));
#325112=CARTESIAN_POINT('Ctrl Pts',(-0.978321085000056,5.2,-4.36156944000002));
#325113=CARTESIAN_POINT('Ctrl Pts',(-0.978321085000056,2.2,-4.36156944000002));
#325114=CARTESIAN_POINT('Ctrl Pts',(-0.976938052000056,12.2,-4.35987974100001));
#325115=CARTESIAN_POINT('Ctrl Pts',(-0.976938052000056,5.2,-4.35987974100001));
#325116=CARTESIAN_POINT('Ctrl Pts',(-0.976938052000056,2.2,-4.35987974100001));
#325117=CARTESIAN_POINT('Ctrl Pts',(-0.975559305000055,12.2,-4.35819153100002));
#325118=CARTESIAN_POINT('Ctrl Pts',(-0.975559305000055,5.2,-4.35819153100002));
#325119=CARTESIAN_POINT('Ctrl Pts',(-0.975559305000055,2.2,-4.35819153100002));
#325120=CARTESIAN_POINT('Ctrl Pts',(-0.974184843000057,12.2,-4.35650481900002));
#325121=CARTESIAN_POINT('Ctrl Pts',(-0.974184843000057,5.2,-4.35650481900002));
#325122=CARTESIAN_POINT('Ctrl Pts',(-0.974184843000057,2.2,-4.35650481900002));
#325123=CARTESIAN_POINT('Ctrl Pts',(-0.972814664000056,12.2,-4.35481961700001));
#325124=CARTESIAN_POINT('Ctrl Pts',(-0.972814664000056,5.2,-4.35481961700001));
#325125=CARTESIAN_POINT('Ctrl Pts',(-0.972814664000056,2.2,-4.35481961700001));
#325126=CARTESIAN_POINT('Ctrl Pts',(-0.971448767000057,12.2,-4.35313593500001));
#325127=CARTESIAN_POINT('Ctrl Pts',(-0.971448767000057,5.2,-4.35313593500001));
#325128=CARTESIAN_POINT('Ctrl Pts',(-0.971448767000057,2.2,-4.35313593500001));
#325129=CARTESIAN_POINT('Ctrl Pts',(-0.970087150000056,12.2,-4.35145378100001));
#325130=CARTESIAN_POINT('Ctrl Pts',(-0.970087150000056,5.2,-4.35145378100001));
#325131=CARTESIAN_POINT('Ctrl Pts',(-0.970087150000056,2.2,-4.35145378100001));
#325132=CARTESIAN_POINT('Ctrl Pts',(-0.968729812000056,12.2,-4.34977316700001));
#325133=CARTESIAN_POINT('Ctrl Pts',(-0.968729812000056,5.2,-4.34977316700001));
#325134=CARTESIAN_POINT('Ctrl Pts',(-0.968729812000056,2.2,-4.34977316700001));
#325135=CARTESIAN_POINT('Ctrl Pts',(-0.967376751000056,12.2,-4.34809410300002));
#325136=CARTESIAN_POINT('Ctrl Pts',(-0.967376751000056,5.2,-4.34809410300002));
#325137=CARTESIAN_POINT('Ctrl Pts',(-0.967376751000056,2.2,-4.34809410300002));
#325138=CARTESIAN_POINT('Ctrl Pts',(-0.966027967000055,12.2,-4.34641659700001));
#325139=CARTESIAN_POINT('Ctrl Pts',(-0.966027967000055,5.2,-4.34641659700001));
#325140=CARTESIAN_POINT('Ctrl Pts',(-0.966027967000055,2.2,-4.34641659700001));
#325141=CARTESIAN_POINT('Ctrl Pts',(-0.964683457000056,12.2,-4.34474066300002));
#325142=CARTESIAN_POINT('Ctrl Pts',(-0.964683457000056,5.2,-4.34474066300002));
#325143=CARTESIAN_POINT('Ctrl Pts',(-0.964683457000056,2.2,-4.34474066300002));
#325144=CARTESIAN_POINT('Ctrl Pts',(-0.963343219000056,12.2,-4.34306630800001));
#325145=CARTESIAN_POINT('Ctrl Pts',(-0.963343219000056,5.2,-4.34306630800001));
#325146=CARTESIAN_POINT('Ctrl Pts',(-0.963343219000056,2.2,-4.34306630800001));
#325147=CARTESIAN_POINT('Ctrl Pts',(-0.962007251000055,12.2,-4.34139354300001));
#325148=CARTESIAN_POINT('Ctrl Pts',(-0.962007251000055,5.2,-4.34139354300001));
#325149=CARTESIAN_POINT('Ctrl Pts',(-0.962007251000055,2.2,-4.34139354300001));
#325150=CARTESIAN_POINT('Ctrl Pts',(-0.960675554000057,12.2,-4.33972237800001));
#325151=CARTESIAN_POINT('Ctrl Pts',(-0.960675554000057,5.2,-4.33972237800001));
#325152=CARTESIAN_POINT('Ctrl Pts',(-0.960675554000057,2.2,-4.33972237800001));
#325153=CARTESIAN_POINT('Ctrl Pts',(-0.959348124000057,12.2,-4.33805282500002));
#325154=CARTESIAN_POINT('Ctrl Pts',(-0.959348124000057,5.2,-4.33805282500002));
#325155=CARTESIAN_POINT('Ctrl Pts',(-0.959348124000057,2.2,-4.33805282500002));
#325156=CARTESIAN_POINT('Ctrl Pts',(-0.958024960000056,12.2,-4.33638489200002));
#325157=CARTESIAN_POINT('Ctrl Pts',(-0.958024960000056,5.2,-4.33638489200002));
#325158=CARTESIAN_POINT('Ctrl Pts',(-0.958024960000056,2.2,-4.33638489200002));
#325159=CARTESIAN_POINT('Ctrl Pts',(-0.956706062000056,12.2,-4.33471859000001));
#325160=CARTESIAN_POINT('Ctrl Pts',(-0.956706062000056,5.2,-4.33471859000001));
#325161=CARTESIAN_POINT('Ctrl Pts',(-0.956706062000056,2.2,-4.33471859000001));
#325162=CARTESIAN_POINT('Ctrl Pts',(-0.955391425000055,12.2,-4.33305392900001));
#325163=CARTESIAN_POINT('Ctrl Pts',(-0.955391425000055,5.2,-4.33305392900001));
#325164=CARTESIAN_POINT('Ctrl Pts',(-0.955391425000055,2.2,-4.33305392900001));
#325165=CARTESIAN_POINT('Ctrl Pts',(-0.954081050000056,12.2,-4.33139092000001));
#325166=CARTESIAN_POINT('Ctrl Pts',(-0.954081050000056,5.2,-4.33139092000001));
#325167=CARTESIAN_POINT('Ctrl Pts',(-0.954081050000056,2.2,-4.33139092000001));
#325168=CARTESIAN_POINT('Ctrl Pts',(-0.952774934000056,12.2,-4.32972957100001));
#325169=CARTESIAN_POINT('Ctrl Pts',(-0.952774934000056,5.2,-4.32972957100001));
#325170=CARTESIAN_POINT('Ctrl Pts',(-0.952774934000056,2.2,-4.32972957100001));
#325171=CARTESIAN_POINT('Ctrl Pts',(-0.951473076000056,12.2,-4.32806989600001));
#325172=CARTESIAN_POINT('Ctrl Pts',(-0.951473076000056,5.2,-4.32806989600001));
#325173=CARTESIAN_POINT('Ctrl Pts',(-0.951473076000056,2.2,-4.32806989600001));
#325174=CARTESIAN_POINT('Ctrl Pts',(-0.950175474000057,12.2,-4.32641190200002));
#325175=CARTESIAN_POINT('Ctrl Pts',(-0.950175474000057,5.2,-4.32641190200002));
#325176=CARTESIAN_POINT('Ctrl Pts',(-0.950175474000057,2.2,-4.32641190200002));
#325177=CARTESIAN_POINT('Ctrl Pts',(-0.948882126000056,12.2,-4.32475560100002));
#325178=CARTESIAN_POINT('Ctrl Pts',(-0.948882126000056,5.2,-4.32475560100002));
#325179=CARTESIAN_POINT('Ctrl Pts',(-0.948882126000056,2.2,-4.32475560100002));
#325180=CARTESIAN_POINT('Ctrl Pts',(-0.947593031000055,12.2,-4.32310100300001));
#325181=CARTESIAN_POINT('Ctrl Pts',(-0.947593031000055,5.2,-4.32310100300001));
#325182=CARTESIAN_POINT('Ctrl Pts',(-0.947593031000055,2.2,-4.32310100300001));
#325183=CARTESIAN_POINT('Ctrl Pts',(-0.946308186000057,12.2,-4.32144811800002));
#325184=CARTESIAN_POINT('Ctrl Pts',(-0.946308186000057,5.2,-4.32144811800002));
#325185=CARTESIAN_POINT('Ctrl Pts',(-0.946308186000057,2.2,-4.32144811800002));
#325186=CARTESIAN_POINT('Ctrl Pts',(-0.945027590000055,12.2,-4.31979695700001));
#325187=CARTESIAN_POINT('Ctrl Pts',(-0.945027590000055,5.2,-4.31979695700001));
#325188=CARTESIAN_POINT('Ctrl Pts',(-0.945027590000055,2.2,-4.31979695700001));
#325189=CARTESIAN_POINT('Ctrl Pts',(-0.943751240000056,12.2,-4.31814752900001));
#325190=CARTESIAN_POINT('Ctrl Pts',(-0.943751240000056,5.2,-4.31814752900001));
#325191=CARTESIAN_POINT('Ctrl Pts',(-0.943751240000056,2.2,-4.31814752900001));
#325192=CARTESIAN_POINT('Ctrl Pts',(-0.942479137000056,12.2,-4.31649984600002));
#325193=CARTESIAN_POINT('Ctrl Pts',(-0.942479137000056,5.2,-4.31649984600002));
#325194=CARTESIAN_POINT('Ctrl Pts',(-0.942479137000056,2.2,-4.31649984600002));
#325195=CARTESIAN_POINT('Ctrl Pts',(-0.941211276000056,12.2,-4.31485391700001));
#325196=CARTESIAN_POINT('Ctrl Pts',(-0.941211276000056,5.2,-4.31485391700001));
#325197=CARTESIAN_POINT('Ctrl Pts',(-0.941211276000056,2.2,-4.31485391700001));
#325198=CARTESIAN_POINT('Ctrl Pts',(-0.939947657000056,12.2,-4.31320975300002));
#325199=CARTESIAN_POINT('Ctrl Pts',(-0.939947657000056,5.2,-4.31320975300002));
#325200=CARTESIAN_POINT('Ctrl Pts',(-0.939947657000056,2.2,-4.31320975300002));
#325201=CARTESIAN_POINT('Ctrl Pts',(-0.938688278000056,12.2,-4.31156736500002));
#325202=CARTESIAN_POINT('Ctrl Pts',(-0.938688278000056,5.2,-4.31156736500002));
#325203=CARTESIAN_POINT('Ctrl Pts',(-0.938688278000056,2.2,-4.31156736500002));
#325204=CARTESIAN_POINT('Ctrl Pts',(-0.937433136000055,12.2,-4.30992676300002));
#325205=CARTESIAN_POINT('Ctrl Pts',(-0.937433136000055,5.2,-4.30992676300002));
#325206=CARTESIAN_POINT('Ctrl Pts',(-0.937433136000055,2.2,-4.30992676300002));
#325207=CARTESIAN_POINT('Ctrl Pts',(-0.936182229000057,12.2,-4.30828795600001));
#325208=CARTESIAN_POINT('Ctrl Pts',(-0.936182229000057,5.2,-4.30828795600001));
#325209=CARTESIAN_POINT('Ctrl Pts',(-0.936182229000057,2.2,-4.30828795600001));
#325210=CARTESIAN_POINT('Ctrl Pts',(-0.934935557000056,12.2,-4.30665095700002));
#325211=CARTESIAN_POINT('Ctrl Pts',(-0.934935557000056,5.2,-4.30665095700002));
#325212=CARTESIAN_POINT('Ctrl Pts',(-0.934935557000056,2.2,-4.30665095700002));
#325213=CARTESIAN_POINT('Ctrl Pts',(-0.933693116000055,12.2,-4.30501577500001));
#325214=CARTESIAN_POINT('Ctrl Pts',(-0.933693116000055,5.2,-4.30501577500001));
#325215=CARTESIAN_POINT('Ctrl Pts',(-0.933693116000055,2.2,-4.30501577500001));
#325216=CARTESIAN_POINT('Ctrl Pts',(-0.932454904000056,12.2,-4.30338242000001));
#325217=CARTESIAN_POINT('Ctrl Pts',(-0.932454904000056,5.2,-4.30338242000001));
#325218=CARTESIAN_POINT('Ctrl Pts',(-0.932454904000056,2.2,-4.30338242000001));
#325219=CARTESIAN_POINT('Ctrl Pts',(-0.931220922000057,12.2,-4.30175090400001));
#325220=CARTESIAN_POINT('Ctrl Pts',(-0.931220922000057,5.2,-4.30175090400001));
#325221=CARTESIAN_POINT('Ctrl Pts',(-0.931220922000057,2.2,-4.30175090400001));
#325222=CARTESIAN_POINT('Ctrl Pts',(-0.929991165000056,12.2,-4.30012123500001));
#325223=CARTESIAN_POINT('Ctrl Pts',(-0.929991165000056,5.2,-4.30012123500001));
#325224=CARTESIAN_POINT('Ctrl Pts',(-0.929991165000056,2.2,-4.30012123500001));
#325225=CARTESIAN_POINT('Ctrl Pts',(-0.928765631000056,12.2,-4.29849342700001));
#325226=CARTESIAN_POINT('Ctrl Pts',(-0.928765631000056,5.2,-4.29849342700001));
#325227=CARTESIAN_POINT('Ctrl Pts',(-0.928765631000056,2.2,-4.29849342700001));
#325228=CARTESIAN_POINT('Ctrl Pts',(-0.927544319000055,12.2,-4.29686748800002));
#325229=CARTESIAN_POINT('Ctrl Pts',(-0.927544319000055,5.2,-4.29686748800002));
#325230=CARTESIAN_POINT('Ctrl Pts',(-0.927544319000055,2.2,-4.29686748800002));
#325231=CARTESIAN_POINT('Ctrl Pts',(-0.926327227000057,12.2,-4.29524342900002));
#325232=CARTESIAN_POINT('Ctrl Pts',(-0.926327227000057,5.2,-4.29524342900002));
#325233=CARTESIAN_POINT('Ctrl Pts',(-0.926327227000057,2.2,-4.29524342900002));
#325234=CARTESIAN_POINT('Ctrl Pts',(-0.925114352000056,12.2,-4.29362126000001));
#325235=CARTESIAN_POINT('Ctrl Pts',(-0.925114352000056,5.2,-4.29362126000001));
#325236=CARTESIAN_POINT('Ctrl Pts',(-0.925114352000056,2.2,-4.29362126000001));
#325237=CARTESIAN_POINT('Ctrl Pts',(-0.923905693000057,12.2,-4.29200099300001));
#325238=CARTESIAN_POINT('Ctrl Pts',(-0.923905693000057,5.2,-4.29200099300001));
#325239=CARTESIAN_POINT('Ctrl Pts',(-0.923905693000057,2.2,-4.29200099300001));
#325240=CARTESIAN_POINT('Ctrl Pts',(-0.922701248000056,12.2,-4.29038263800001));
#325241=CARTESIAN_POINT('Ctrl Pts',(-0.922701248000056,5.2,-4.29038263800001));
#325242=CARTESIAN_POINT('Ctrl Pts',(-0.922701248000056,2.2,-4.29038263800001));
#325243=CARTESIAN_POINT('Ctrl Pts',(-0.921501014000056,12.2,-4.28876620600001));
#325244=CARTESIAN_POINT('Ctrl Pts',(-0.921501014000056,5.2,-4.28876620600001));
#325245=CARTESIAN_POINT('Ctrl Pts',(-0.921501014000056,2.2,-4.28876620600001));
#325246=CARTESIAN_POINT('Ctrl Pts',(-0.920304988000057,12.2,-4.28715170600002));
#325247=CARTESIAN_POINT('Ctrl Pts',(-0.920304988000057,5.2,-4.28715170600002));
#325248=CARTESIAN_POINT('Ctrl Pts',(-0.920304988000057,2.2,-4.28715170600002));
#325249=CARTESIAN_POINT('Ctrl Pts',(-0.919113169000055,12.2,-4.28553915100002));
#325250=CARTESIAN_POINT('Ctrl Pts',(-0.919113169000055,5.2,-4.28553915100002));
#325251=CARTESIAN_POINT('Ctrl Pts',(-0.919113169000055,2.2,-4.28553915100002));
#325252=CARTESIAN_POINT('Ctrl Pts',(-0.917925555000056,12.2,-4.28392854900002));
#325253=CARTESIAN_POINT('Ctrl Pts',(-0.917925555000056,5.2,-4.28392854900002));
#325254=CARTESIAN_POINT('Ctrl Pts',(-0.917925555000056,2.2,-4.28392854900002));
#325255=CARTESIAN_POINT('Ctrl Pts',(-0.916742144000056,12.2,-4.28231991300001));
#325256=CARTESIAN_POINT('Ctrl Pts',(-0.916742144000056,5.2,-4.28231991300001));
#325257=CARTESIAN_POINT('Ctrl Pts',(-0.916742144000056,2.2,-4.28231991300001));
#325258=CARTESIAN_POINT('Ctrl Pts',(-0.915562933000055,12.2,-4.28071325300001));
#325259=CARTESIAN_POINT('Ctrl Pts',(-0.915562933000055,5.2,-4.28071325300001));
#325260=CARTESIAN_POINT('Ctrl Pts',(-0.915562933000055,2.2,-4.28071325300001));
#325261=CARTESIAN_POINT('Ctrl Pts',(-0.914387920000056,12.2,-4.27910857900001));
#325262=CARTESIAN_POINT('Ctrl Pts',(-0.914387920000056,5.2,-4.27910857900001));
#325263=CARTESIAN_POINT('Ctrl Pts',(-0.914387920000056,2.2,-4.27910857900001));
#325264=CARTESIAN_POINT('Ctrl Pts',(-0.913217103000056,12.2,-4.27750590100001));
#325265=CARTESIAN_POINT('Ctrl Pts',(-0.913217103000056,5.2,-4.27750590100001));
#325266=CARTESIAN_POINT('Ctrl Pts',(-0.913217103000056,2.2,-4.27750590100001));
#325267=CARTESIAN_POINT('Ctrl Pts',(-0.912050479000056,12.2,-4.27590523100001));
#325268=CARTESIAN_POINT('Ctrl Pts',(-0.912050479000056,5.2,-4.27590523100001));
#325269=CARTESIAN_POINT('Ctrl Pts',(-0.912050479000056,2.2,-4.27590523100001));
#325270=CARTESIAN_POINT('Ctrl Pts',(-0.910888047000055,12.2,-4.27430658100001));
#325271=CARTESIAN_POINT('Ctrl Pts',(-0.910888047000055,5.2,-4.27430658100001));
#325272=CARTESIAN_POINT('Ctrl Pts',(-0.910888047000055,2.2,-4.27430658100001));
#325273=CARTESIAN_POINT('Ctrl Pts',(-0.909729802000055,12.2,-4.27270995800002));
#325274=CARTESIAN_POINT('Ctrl Pts',(-0.909729802000055,5.2,-4.27270995800002));
#325275=CARTESIAN_POINT('Ctrl Pts',(-0.909729802000055,2.2,-4.27270995800002));
#325276=CARTESIAN_POINT('Ctrl Pts',(-0.908575745000055,12.2,-4.27111537700001));
#325277=CARTESIAN_POINT('Ctrl Pts',(-0.908575745000055,5.2,-4.27111537700001));
#325278=CARTESIAN_POINT('Ctrl Pts',(-0.908575745000055,2.2,-4.27111537700001));
#325279=CARTESIAN_POINT('Ctrl Pts',(-0.907425872000056,12.2,-4.26952284600001));
#325280=CARTESIAN_POINT('Ctrl Pts',(-0.907425872000056,5.2,-4.26952284600001));
#325281=CARTESIAN_POINT('Ctrl Pts',(-0.907425872000056,2.2,-4.26952284600001));
#325282=CARTESIAN_POINT('Ctrl Pts',(-0.906280181000056,12.2,-4.26793237600001));
#325283=CARTESIAN_POINT('Ctrl Pts',(-0.906280181000056,5.2,-4.26793237600001));
#325284=CARTESIAN_POINT('Ctrl Pts',(-0.906280181000056,2.2,-4.26793237600001));
#325285=CARTESIAN_POINT('Ctrl Pts',(-0.905138668000056,12.2,-4.26634397900001));
#325286=CARTESIAN_POINT('Ctrl Pts',(-0.905138668000056,5.2,-4.26634397900001));
#325287=CARTESIAN_POINT('Ctrl Pts',(-0.905138668000056,2.2,-4.26634397900001));
#325288=CARTESIAN_POINT('Ctrl Pts',(-0.904001333000056,12.2,-4.26475766500001));
#325289=CARTESIAN_POINT('Ctrl Pts',(-0.904001333000056,5.2,-4.26475766500001));
#325290=CARTESIAN_POINT('Ctrl Pts',(-0.904001333000056,2.2,-4.26475766500001));
#325291=CARTESIAN_POINT('Ctrl Pts',(-0.902868173000057,12.2,-4.26317344500001));
#325292=CARTESIAN_POINT('Ctrl Pts',(-0.902868173000057,5.2,-4.26317344500001));
#325293=CARTESIAN_POINT('Ctrl Pts',(-0.902868173000057,2.2,-4.26317344500001));
#325294=CARTESIAN_POINT('Ctrl Pts',(-0.901739184000055,12.2,-4.26159132900001));
#325295=CARTESIAN_POINT('Ctrl Pts',(-0.901739184000055,5.2,-4.26159132900001));
#325296=CARTESIAN_POINT('Ctrl Pts',(-0.901739184000055,2.2,-4.26159132900001));
#325297=CARTESIAN_POINT('Ctrl Pts',(-0.900614366000055,12.2,-4.26001133000002));
#325298=CARTESIAN_POINT('Ctrl Pts',(-0.900614366000055,5.2,-4.26001133000002));
#325299=CARTESIAN_POINT('Ctrl Pts',(-0.900614366000055,2.2,-4.26001133000002));
#325300=CARTESIAN_POINT('Ctrl Pts',(-0.899493714000055,12.2,-4.25843345600001));
#325301=CARTESIAN_POINT('Ctrl Pts',(-0.899493714000055,5.2,-4.25843345600001));
#325302=CARTESIAN_POINT('Ctrl Pts',(-0.899493714000055,2.2,-4.25843345600001));
#325303=CARTESIAN_POINT('Ctrl Pts',(-0.898377227000056,12.2,-4.25685771900001));
#325304=CARTESIAN_POINT('Ctrl Pts',(-0.898377227000056,5.2,-4.25685771900001));
#325305=CARTESIAN_POINT('Ctrl Pts',(-0.898377227000056,2.2,-4.25685771900001));
#325306=CARTESIAN_POINT('Ctrl Pts',(-0.897264902000057,12.2,-4.25528413200002));
#325307=CARTESIAN_POINT('Ctrl Pts',(-0.897264902000057,5.2,-4.25528413200002));
#325308=CARTESIAN_POINT('Ctrl Pts',(-0.897264902000057,2.2,-4.25528413200002));
#325309=CARTESIAN_POINT('Ctrl Pts',(-0.896156737000057,12.2,-4.25371270300001));
#325310=CARTESIAN_POINT('Ctrl Pts',(-0.896156737000057,5.2,-4.25371270300001));
#325311=CARTESIAN_POINT('Ctrl Pts',(-0.896156737000057,2.2,-4.25371270300001));
#325312=CARTESIAN_POINT('Ctrl Pts',(-0.895052728000056,12.2,-4.25214344400001));
#325313=CARTESIAN_POINT('Ctrl Pts',(-0.895052728000056,5.2,-4.25214344400001));
#325314=CARTESIAN_POINT('Ctrl Pts',(-0.895052728000056,2.2,-4.25214344400001));
#325315=CARTESIAN_POINT('Ctrl Pts',(-0.893952874000057,12.2,-4.25057636600001));
#325316=CARTESIAN_POINT('Ctrl Pts',(-0.893952874000057,5.2,-4.25057636600001));
#325317=CARTESIAN_POINT('Ctrl Pts',(-0.893952874000057,2.2,-4.25057636600001));
#325318=CARTESIAN_POINT('Ctrl Pts',(-0.892857172000056,12.2,-4.24901148100002));
#325319=CARTESIAN_POINT('Ctrl Pts',(-0.892857172000056,5.2,-4.24901148100002));
#325320=CARTESIAN_POINT('Ctrl Pts',(-0.892857172000056,2.2,-4.24901148100002));
#325321=CARTESIAN_POINT('Ctrl Pts',(-0.891765620000056,12.2,-4.24744879800001));
#325322=CARTESIAN_POINT('Ctrl Pts',(-0.891765620000056,5.2,-4.24744879800001));
#325323=CARTESIAN_POINT('Ctrl Pts',(-0.891765620000056,2.2,-4.24744879800001));
#325324=CARTESIAN_POINT('Ctrl Pts',(-0.890678213000056,12.2,-4.24588832900001));
#325325=CARTESIAN_POINT('Ctrl Pts',(-0.890678213000056,5.2,-4.24588832900001));
#325326=CARTESIAN_POINT('Ctrl Pts',(-0.890678213000056,2.2,-4.24588832900001));
#325327=CARTESIAN_POINT('Ctrl Pts',(-0.889594950000056,12.2,-4.24433008500001));
#325328=CARTESIAN_POINT('Ctrl Pts',(-0.889594950000056,5.2,-4.24433008500001));
#325329=CARTESIAN_POINT('Ctrl Pts',(-0.889594950000056,2.2,-4.24433008500001));
#325330=CARTESIAN_POINT('Ctrl Pts',(-0.888515829000056,12.2,-4.24277407700002));
#325331=CARTESIAN_POINT('Ctrl Pts',(-0.888515829000056,5.2,-4.24277407700002));
#325332=CARTESIAN_POINT('Ctrl Pts',(-0.888515829000056,2.2,-4.24277407700002));
#325333=CARTESIAN_POINT('Ctrl Pts',(-0.887440846000055,12.2,-4.24122031600001));
#325334=CARTESIAN_POINT('Ctrl Pts',(-0.887440846000055,5.2,-4.24122031600001));
#325335=CARTESIAN_POINT('Ctrl Pts',(-0.887440846000055,2.2,-4.24122031600001));
#325336=CARTESIAN_POINT('Ctrl Pts',(-0.886370000000056,12.2,-4.23966881300001));
#325337=CARTESIAN_POINT('Ctrl Pts',(-0.886370000000056,5.2,-4.23966881300001));
#325338=CARTESIAN_POINT('Ctrl Pts',(-0.886370000000056,2.2,-4.23966881300001));
#325339=CARTESIAN_POINT('Ctrl Pts',(-0.885303286000055,12.2,-4.23811957800002));
#325340=CARTESIAN_POINT('Ctrl Pts',(-0.885303286000055,5.2,-4.23811957800002));
#325341=CARTESIAN_POINT('Ctrl Pts',(-0.885303286000055,2.2,-4.23811957800002));
#325342=CARTESIAN_POINT('Ctrl Pts',(-0.884240702000056,12.2,-4.23657262400001));
#325343=CARTESIAN_POINT('Ctrl Pts',(-0.884240702000056,5.2,-4.23657262400001));
#325344=CARTESIAN_POINT('Ctrl Pts',(-0.884240702000056,2.2,-4.23657262400001));
#325345=CARTESIAN_POINT('Ctrl Pts',(-0.883182246000055,12.2,-4.23502796100002));
#325346=CARTESIAN_POINT('Ctrl Pts',(-0.883182246000055,5.2,-4.23502796100002));
#325347=CARTESIAN_POINT('Ctrl Pts',(-0.883182246000055,2.2,-4.23502796100002));
#325348=CARTESIAN_POINT('Ctrl Pts',(-0.882127915000056,12.2,-4.23348560000001));
#325349=CARTESIAN_POINT('Ctrl Pts',(-0.882127915000056,5.2,-4.23348560000001));
#325350=CARTESIAN_POINT('Ctrl Pts',(-0.882127915000056,2.2,-4.23348560000001));
#325351=CARTESIAN_POINT('Ctrl Pts',(-0.881077706000056,12.2,-4.23194555300002));
#325352=CARTESIAN_POINT('Ctrl Pts',(-0.881077706000056,5.2,-4.23194555300002));
#325353=CARTESIAN_POINT('Ctrl Pts',(-0.881077706000056,2.2,-4.23194555300002));
#325354=CARTESIAN_POINT('Ctrl Pts',(-0.880031616000055,12.2,-4.23040783000001));
#325355=CARTESIAN_POINT('Ctrl Pts',(-0.880031616000055,5.2,-4.23040783000001));
#325356=CARTESIAN_POINT('Ctrl Pts',(-0.880031616000055,2.2,-4.23040783000001));
#325357=CARTESIAN_POINT('Ctrl Pts',(-0.878989642000055,12.2,-4.22887244300002));
#325358=CARTESIAN_POINT('Ctrl Pts',(-0.878989642000055,5.2,-4.22887244300002));
#325359=CARTESIAN_POINT('Ctrl Pts',(-0.878989642000055,2.2,-4.22887244300002));
#325360=CARTESIAN_POINT('Ctrl Pts',(-0.877951781000055,12.2,-4.22733940200001));
#325361=CARTESIAN_POINT('Ctrl Pts',(-0.877951781000055,5.2,-4.22733940200001));
#325362=CARTESIAN_POINT('Ctrl Pts',(-0.877951781000055,2.2,-4.22733940200001));
#325363=CARTESIAN_POINT('Ctrl Pts',(-0.876918030000056,12.2,-4.22580872000001));
#325364=CARTESIAN_POINT('Ctrl Pts',(-0.876918030000056,5.2,-4.22580872000001));
#325365=CARTESIAN_POINT('Ctrl Pts',(-0.876918030000056,2.2,-4.22580872000001));
#325366=CARTESIAN_POINT('Ctrl Pts',(-0.875888388000057,12.2,-4.22428040700002));
#325367=CARTESIAN_POINT('Ctrl Pts',(-0.875888388000057,5.2,-4.22428040700002));
#325368=CARTESIAN_POINT('Ctrl Pts',(-0.875888388000057,2.2,-4.22428040700002));
#325369=CARTESIAN_POINT('Ctrl Pts',(-0.874862850000057,12.2,-4.22275447400001));
#325370=CARTESIAN_POINT('Ctrl Pts',(-0.874862850000057,5.2,-4.22275447400001));
#325371=CARTESIAN_POINT('Ctrl Pts',(-0.874862850000057,2.2,-4.22275447400001));
#325372=CARTESIAN_POINT('Ctrl Pts',(-0.873841413000056,12.2,-4.22123093200002));
#325373=CARTESIAN_POINT('Ctrl Pts',(-0.873841413000056,5.2,-4.22123093200002));
#325374=CARTESIAN_POINT('Ctrl Pts',(-0.873841413000056,2.2,-4.22123093200002));
#325375=CARTESIAN_POINT('Ctrl Pts',(-0.872824076000055,12.2,-4.21970979500002));
#325376=CARTESIAN_POINT('Ctrl Pts',(-0.872824076000055,5.2,-4.21970979500002));
#325377=CARTESIAN_POINT('Ctrl Pts',(-0.872824076000055,2.2,-4.21970979500002));
#325378=CARTESIAN_POINT('Ctrl Pts',(-0.871810833000056,12.2,-4.21819107000001));
#325379=CARTESIAN_POINT('Ctrl Pts',(-0.871810833000056,5.2,-4.21819107000001));
#325380=CARTESIAN_POINT('Ctrl Pts',(-0.871810833000056,2.2,-4.21819107000001));
#325381=CARTESIAN_POINT('Ctrl Pts',(-0.870801684000057,12.2,-4.21667477100002));
#325382=CARTESIAN_POINT('Ctrl Pts',(-0.870801684000057,5.2,-4.21667477100002));
#325383=CARTESIAN_POINT('Ctrl Pts',(-0.870801684000057,2.2,-4.21667477100002));
#325384=CARTESIAN_POINT('Ctrl Pts',(-0.869796624000055,12.2,-4.21516090900001));
#325385=CARTESIAN_POINT('Ctrl Pts',(-0.869796624000055,5.2,-4.21516090900001));
#325386=CARTESIAN_POINT('Ctrl Pts',(-0.869796624000055,2.2,-4.21516090900001));
#325387=CARTESIAN_POINT('Ctrl Pts',(-0.868795651000056,12.2,-4.21364949400001));
#325388=CARTESIAN_POINT('Ctrl Pts',(-0.868795651000056,5.2,-4.21364949400001));
#325389=CARTESIAN_POINT('Ctrl Pts',(-0.868795651000056,2.2,-4.21364949400001));
#325390=CARTESIAN_POINT('Ctrl Pts',(-0.867798761000056,12.2,-4.21214053900002));
#325391=CARTESIAN_POINT('Ctrl Pts',(-0.867798761000056,5.2,-4.21214053900002));
#325392=CARTESIAN_POINT('Ctrl Pts',(-0.867798761000056,2.2,-4.21214053900002));
#325393=CARTESIAN_POINT('Ctrl Pts',(-0.866805951000057,12.2,-4.21063405500002));
#325394=CARTESIAN_POINT('Ctrl Pts',(-0.866805951000057,5.2,-4.21063405500002));
#325395=CARTESIAN_POINT('Ctrl Pts',(-0.866805951000057,2.2,-4.21063405500002));
#325396=CARTESIAN_POINT('Ctrl Pts',(-0.865817219000055,12.2,-4.20913005200001));
#325397=CARTESIAN_POINT('Ctrl Pts',(-0.865817219000055,5.2,-4.20913005200001));
#325398=CARTESIAN_POINT('Ctrl Pts',(-0.865817219000055,2.2,-4.20913005200001));
#325399=CARTESIAN_POINT('Ctrl Pts',(-0.864832560000056,12.2,-4.20762854200001));
#325400=CARTESIAN_POINT('Ctrl Pts',(-0.864832560000056,5.2,-4.20762854200001));
#325401=CARTESIAN_POINT('Ctrl Pts',(-0.864832560000056,2.2,-4.20762854200001));
#325402=CARTESIAN_POINT('Ctrl Pts',(-0.863851973000056,12.2,-4.20612953700001));
#325403=CARTESIAN_POINT('Ctrl Pts',(-0.863851973000056,5.2,-4.20612953700001));
#325404=CARTESIAN_POINT('Ctrl Pts',(-0.863851973000056,2.2,-4.20612953700001));
#325405=CARTESIAN_POINT('Ctrl Pts',(-0.862875453000056,12.2,-4.20463304800001));
#325406=CARTESIAN_POINT('Ctrl Pts',(-0.862875453000056,5.2,-4.20463304800001));
#325407=CARTESIAN_POINT('Ctrl Pts',(-0.862875453000056,2.2,-4.20463304800001));
#325408=CARTESIAN_POINT('Ctrl Pts',(-0.861902999000056,12.2,-4.20313908800001));
#325409=CARTESIAN_POINT('Ctrl Pts',(-0.861902999000056,5.2,-4.20313908800001));
#325410=CARTESIAN_POINT('Ctrl Pts',(-0.861902999000056,2.2,-4.20313908800001));
#325411=CARTESIAN_POINT('Ctrl Pts',(-0.860934605000055,12.2,-4.20164766600001));
#325412=CARTESIAN_POINT('Ctrl Pts',(-0.860934605000055,5.2,-4.20164766600001));
#325413=CARTESIAN_POINT('Ctrl Pts',(-0.860934605000055,2.2,-4.20164766600001));
#325414=CARTESIAN_POINT('Ctrl Pts',(-0.859970269000057,12.2,-4.20015879300002));
#325415=CARTESIAN_POINT('Ctrl Pts',(-0.859970269000057,5.2,-4.20015879300002));
#325416=CARTESIAN_POINT('Ctrl Pts',(-0.859970269000057,2.2,-4.20015879300002));
#325417=CARTESIAN_POINT('Ctrl Pts',(-0.859009988000056,12.2,-4.19867248200001));
#325418=CARTESIAN_POINT('Ctrl Pts',(-0.859009988000056,5.2,-4.19867248200001));
#325419=CARTESIAN_POINT('Ctrl Pts',(-0.859009988000056,2.2,-4.19867248200001));
#325420=CARTESIAN_POINT('Ctrl Pts',(-0.858053759000056,12.2,-4.19718874600001));
#325421=CARTESIAN_POINT('Ctrl Pts',(-0.858053759000056,5.2,-4.19718874600001));
#325422=CARTESIAN_POINT('Ctrl Pts',(-0.858053759000056,2.2,-4.19718874600001));
#325423=CARTESIAN_POINT('Ctrl Pts',(-0.857101578000057,12.2,-4.19570759300001));
#325424=CARTESIAN_POINT('Ctrl Pts',(-0.857101578000057,5.2,-4.19570759300001));
#325425=CARTESIAN_POINT('Ctrl Pts',(-0.857101578000057,2.2,-4.19570759300001));
#325426=CARTESIAN_POINT('Ctrl Pts',(-0.856153441000057,12.2,-4.19422903700001));
#325427=CARTESIAN_POINT('Ctrl Pts',(-0.856153441000057,5.2,-4.19422903700001));
#325428=CARTESIAN_POINT('Ctrl Pts',(-0.856153441000057,2.2,-4.19422903700001));
#325429=CARTESIAN_POINT('Ctrl Pts',(-0.855209346000055,12.2,-4.19275308800001));
#325430=CARTESIAN_POINT('Ctrl Pts',(-0.855209346000055,5.2,-4.19275308800001));
#325431=CARTESIAN_POINT('Ctrl Pts',(-0.855209346000055,2.2,-4.19275308800001));
#325432=CARTESIAN_POINT('Ctrl Pts',(-0.854269289000056,12.2,-4.19127975900001));
#325433=CARTESIAN_POINT('Ctrl Pts',(-0.854269289000056,5.2,-4.19127975900001));
#325434=CARTESIAN_POINT('Ctrl Pts',(-0.854269289000056,2.2,-4.19127975900001));
#325435=CARTESIAN_POINT('Ctrl Pts',(-0.853333268000057,12.2,-4.18980906100002));
#325436=CARTESIAN_POINT('Ctrl Pts',(-0.853333268000057,5.2,-4.18980906100002));
#325437=CARTESIAN_POINT('Ctrl Pts',(-0.853333268000057,2.2,-4.18980906100002));
#325438=CARTESIAN_POINT('Ctrl Pts',(-0.852401276000055,12.2,-4.18834100500002));
#325439=CARTESIAN_POINT('Ctrl Pts',(-0.852401276000055,5.2,-4.18834100500002));
#325440=CARTESIAN_POINT('Ctrl Pts',(-0.852401276000055,2.2,-4.18834100500002));
#325441=CARTESIAN_POINT('Ctrl Pts',(-0.851473313000056,12.2,-4.18687560300001));
#325442=CARTESIAN_POINT('Ctrl Pts',(-0.851473313000056,5.2,-4.18687560300001));
#325443=CARTESIAN_POINT('Ctrl Pts',(-0.851473313000056,2.2,-4.18687560300001));
#325444=CARTESIAN_POINT('Ctrl Pts',(-0.850549375000057,12.2,-4.18541286700002));
#325445=CARTESIAN_POINT('Ctrl Pts',(-0.850549375000057,5.2,-4.18541286700002));
#325446=CARTESIAN_POINT('Ctrl Pts',(-0.850549375000057,2.2,-4.18541286700002));
#325447=CARTESIAN_POINT('Ctrl Pts',(-0.849629457000055,12.2,-4.18395280800001));
#325448=CARTESIAN_POINT('Ctrl Pts',(-0.849629457000055,5.2,-4.18395280800001));
#325449=CARTESIAN_POINT('Ctrl Pts',(-0.849629457000055,2.2,-4.18395280800001));
#325450=CARTESIAN_POINT('Ctrl Pts',(-0.848713556000057,12.2,-4.18249543700002));
#325451=CARTESIAN_POINT('Ctrl Pts',(-0.848713556000057,5.2,-4.18249543700002));
#325452=CARTESIAN_POINT('Ctrl Pts',(-0.848713556000057,2.2,-4.18249543700002));
#325453=CARTESIAN_POINT('Ctrl Pts',(-0.847801670000056,12.2,-4.18104076700001));
#325454=CARTESIAN_POINT('Ctrl Pts',(-0.847801670000056,5.2,-4.18104076700001));
#325455=CARTESIAN_POINT('Ctrl Pts',(-0.847801670000056,2.2,-4.18104076700001));
#325456=CARTESIAN_POINT('Ctrl Pts',(-0.846893794000056,12.2,-4.17958880900001));
#325457=CARTESIAN_POINT('Ctrl Pts',(-0.846893794000056,5.2,-4.17958880900001));
#325458=CARTESIAN_POINT('Ctrl Pts',(-0.846893794000056,2.2,-4.17958880900001));
#325459=CARTESIAN_POINT('Ctrl Pts',(-0.845989925000056,12.2,-4.17813957500002));
#325460=CARTESIAN_POINT('Ctrl Pts',(-0.845989925000056,5.2,-4.17813957500002));
#325461=CARTESIAN_POINT('Ctrl Pts',(-0.845989925000056,2.2,-4.17813957500002));
#325462=CARTESIAN_POINT('Ctrl Pts',(-0.845090058000055,12.2,-4.17669307700002));
#325463=CARTESIAN_POINT('Ctrl Pts',(-0.845090058000055,5.2,-4.17669307700002));
#325464=CARTESIAN_POINT('Ctrl Pts',(-0.845090058000055,2.2,-4.17669307700002));
#325465=CARTESIAN_POINT('Ctrl Pts',(-0.844194192000056,12.2,-4.17524932500001));
#325466=CARTESIAN_POINT('Ctrl Pts',(-0.844194192000056,5.2,-4.17524932500001));
#325467=CARTESIAN_POINT('Ctrl Pts',(-0.844194192000056,2.2,-4.17524932500001));
#325468=CARTESIAN_POINT('Ctrl Pts',(-0.843302321000056,12.2,-4.17380833300002));
#325469=CARTESIAN_POINT('Ctrl Pts',(-0.843302321000056,5.2,-4.17380833300002));
#325470=CARTESIAN_POINT('Ctrl Pts',(-0.843302321000056,2.2,-4.17380833300002));
#325471=CARTESIAN_POINT('Ctrl Pts',(-0.842414442000056,12.2,-4.17237011100001));
#325472=CARTESIAN_POINT('Ctrl Pts',(-0.842414442000056,5.2,-4.17237011100001));
#325473=CARTESIAN_POINT('Ctrl Pts',(-0.842414442000056,2.2,-4.17237011100001));
#325474=CARTESIAN_POINT('Ctrl Pts',(-0.841530551000057,12.2,-4.17093467200001));
#325475=CARTESIAN_POINT('Ctrl Pts',(-0.841530551000057,5.2,-4.17093467200001));
#325476=CARTESIAN_POINT('Ctrl Pts',(-0.841530551000057,2.2,-4.17093467200001));
#325477=CARTESIAN_POINT('Ctrl Pts',(-0.840650646000055,12.2,-4.16950202700002));
#325478=CARTESIAN_POINT('Ctrl Pts',(-0.840650646000055,5.2,-4.16950202700002));
#325479=CARTESIAN_POINT('Ctrl Pts',(-0.840650646000055,2.2,-4.16950202700002));
#325480=CARTESIAN_POINT('Ctrl Pts',(-0.839774721000056,12.2,-4.16807218800002));
#325481=CARTESIAN_POINT('Ctrl Pts',(-0.839774721000056,5.2,-4.16807218800002));
#325482=CARTESIAN_POINT('Ctrl Pts',(-0.839774721000056,2.2,-4.16807218800002));
#325483=CARTESIAN_POINT('Ctrl Pts',(-0.838902774000055,12.2,-4.16664516700001));
#325484=CARTESIAN_POINT('Ctrl Pts',(-0.838902774000055,5.2,-4.16664516700001));
#325485=CARTESIAN_POINT('Ctrl Pts',(-0.838902774000055,2.2,-4.16664516700001));
#325486=CARTESIAN_POINT('Ctrl Pts',(-0.838034801000056,12.2,-4.16522097500001));
#325487=CARTESIAN_POINT('Ctrl Pts',(-0.838034801000056,5.2,-4.16522097500001));
#325488=CARTESIAN_POINT('Ctrl Pts',(-0.838034801000056,2.2,-4.16522097500001));
#325489=CARTESIAN_POINT('Ctrl Pts',(-0.837170796000055,12.2,-4.16379962500002));
#325490=CARTESIAN_POINT('Ctrl Pts',(-0.837170796000055,5.2,-4.16379962500002));
#325491=CARTESIAN_POINT('Ctrl Pts',(-0.837170796000055,2.2,-4.16379962500002));
#325492=CARTESIAN_POINT('Ctrl Pts',(-0.836310758000056,12.2,-4.16238112900002));
#325493=CARTESIAN_POINT('Ctrl Pts',(-0.836310758000056,5.2,-4.16238112900002));
#325494=CARTESIAN_POINT('Ctrl Pts',(-0.836310758000056,2.2,-4.16238112900002));
#325495=CARTESIAN_POINT('Ctrl Pts',(-0.835454681000056,12.2,-4.16096549800002));
#325496=CARTESIAN_POINT('Ctrl Pts',(-0.835454681000056,5.2,-4.16096549800002));
#325497=CARTESIAN_POINT('Ctrl Pts',(-0.835454681000056,2.2,-4.16096549800002));
#325498=CARTESIAN_POINT('Ctrl Pts',(-0.834602564000055,12.2,-4.15955274300002));
#325499=CARTESIAN_POINT('Ctrl Pts',(-0.834602564000055,5.2,-4.15955274300002));
#325500=CARTESIAN_POINT('Ctrl Pts',(-0.834602564000055,2.2,-4.15955274300002));
#325501=CARTESIAN_POINT('Ctrl Pts',(-0.833754401000055,12.2,-4.15814287900002));
#325502=CARTESIAN_POINT('Ctrl Pts',(-0.833754401000055,5.2,-4.15814287900002));
#325503=CARTESIAN_POINT('Ctrl Pts',(-0.833754401000055,2.2,-4.15814287900002));
#325504=CARTESIAN_POINT('Ctrl Pts',(-0.832910187000057,12.2,-4.15673591400001));
#325505=CARTESIAN_POINT('Ctrl Pts',(-0.832910187000057,5.2,-4.15673591400001));
#325506=CARTESIAN_POINT('Ctrl Pts',(-0.832910187000057,2.2,-4.15673591400001));
#325507=CARTESIAN_POINT('Ctrl Pts',(-0.832069920000055,12.2,-4.15533186300001));
#325508=CARTESIAN_POINT('Ctrl Pts',(-0.832069920000055,5.2,-4.15533186300001));
#325509=CARTESIAN_POINT('Ctrl Pts',(-0.832069920000055,2.2,-4.15533186300001));
#325510=CARTESIAN_POINT('Ctrl Pts',(-0.831233596000055,12.2,-4.15393073700002));
#325511=CARTESIAN_POINT('Ctrl Pts',(-0.831233596000055,5.2,-4.15393073700002));
#325512=CARTESIAN_POINT('Ctrl Pts',(-0.831233596000055,2.2,-4.15393073700002));
#325513=CARTESIAN_POINT('Ctrl Pts',(-0.830401209000057,12.2,-4.15253254800001));
#325514=CARTESIAN_POINT('Ctrl Pts',(-0.830401209000057,5.2,-4.15253254800001));
#325515=CARTESIAN_POINT('Ctrl Pts',(-0.830401209000057,2.2,-4.15253254800001));
#325516=CARTESIAN_POINT('Ctrl Pts',(-0.829572758000056,12.2,-4.15113730800002));
#325517=CARTESIAN_POINT('Ctrl Pts',(-0.829572758000056,5.2,-4.15113730800002));
#325518=CARTESIAN_POINT('Ctrl Pts',(-0.829572758000056,2.2,-4.15113730800002));
#325519=CARTESIAN_POINT('Ctrl Pts',(-0.828748237000055,12.2,-4.14974502800002));
#325520=CARTESIAN_POINT('Ctrl Pts',(-0.828748237000055,5.2,-4.14974502800002));
#325521=CARTESIAN_POINT('Ctrl Pts',(-0.828748237000055,2.2,-4.14974502800002));
#325522=CARTESIAN_POINT('Ctrl Pts',(-0.827927642000056,12.2,-4.14835572200001));
#325523=CARTESIAN_POINT('Ctrl Pts',(-0.827927642000056,5.2,-4.14835572200001));
#325524=CARTESIAN_POINT('Ctrl Pts',(-0.827927642000056,2.2,-4.14835572200001));
#325525=CARTESIAN_POINT('Ctrl Pts',(-0.827110969000057,12.2,-4.14696940100002));
#325526=CARTESIAN_POINT('Ctrl Pts',(-0.827110969000057,5.2,-4.14696940100002));
#325527=CARTESIAN_POINT('Ctrl Pts',(-0.827110969000057,2.2,-4.14696940100002));
#325528=CARTESIAN_POINT('Ctrl Pts',(-0.826298215000056,12.2,-4.14558607700001));
#325529=CARTESIAN_POINT('Ctrl Pts',(-0.826298215000056,5.2,-4.14558607700001));
#325530=CARTESIAN_POINT('Ctrl Pts',(-0.826298215000056,2.2,-4.14558607700001));
#325531=CARTESIAN_POINT('Ctrl Pts',(-0.825489374000057,12.2,-4.14420576200001));
#325532=CARTESIAN_POINT('Ctrl Pts',(-0.825489374000057,5.2,-4.14420576200001));
#325533=CARTESIAN_POINT('Ctrl Pts',(-0.825489374000057,2.2,-4.14420576200001));
#325534=CARTESIAN_POINT('Ctrl Pts',(-0.824684443000056,12.2,-4.14282846700001));
#325535=CARTESIAN_POINT('Ctrl Pts',(-0.824684443000056,5.2,-4.14282846700001));
#325536=CARTESIAN_POINT('Ctrl Pts',(-0.824684443000056,2.2,-4.14282846700001));
#325537=CARTESIAN_POINT('Ctrl Pts',(-0.823883418000056,12.2,-4.14145420800001));
#325538=CARTESIAN_POINT('Ctrl Pts',(-0.823883418000056,5.2,-4.14145420800001));
#325539=CARTESIAN_POINT('Ctrl Pts',(-0.823883418000056,2.2,-4.14145420800001));
#325540=CARTESIAN_POINT('Ctrl Pts',(-0.823086295000056,12.2,-4.14008299300002));
#325541=CARTESIAN_POINT('Ctrl Pts',(-0.823086295000056,5.2,-4.14008299300002));
#325542=CARTESIAN_POINT('Ctrl Pts',(-0.823086295000056,2.2,-4.14008299300002));
#325543=CARTESIAN_POINT('Ctrl Pts',(-0.822293068000055,12.2,-4.13871483500001));
#325544=CARTESIAN_POINT('Ctrl Pts',(-0.822293068000055,5.2,-4.13871483500001));
#325545=CARTESIAN_POINT('Ctrl Pts',(-0.822293068000055,2.2,-4.13871483500001));
#325546=CARTESIAN_POINT('Ctrl Pts',(-0.821503734000055,12.2,-4.13734974900001));
#325547=CARTESIAN_POINT('Ctrl Pts',(-0.821503734000055,5.2,-4.13734974900001));
#325548=CARTESIAN_POINT('Ctrl Pts',(-0.821503734000055,2.2,-4.13734974900001));
#325549=CARTESIAN_POINT('Ctrl Pts',(-0.820718289000055,12.2,-4.13598774400001));
#325550=CARTESIAN_POINT('Ctrl Pts',(-0.820718289000055,5.2,-4.13598774400001));
#325551=CARTESIAN_POINT('Ctrl Pts',(-0.820718289000055,2.2,-4.13598774400001));
#325552=CARTESIAN_POINT('Ctrl Pts',(-0.819936729000055,12.2,-4.13462883300001));
#325553=CARTESIAN_POINT('Ctrl Pts',(-0.819936729000055,5.2,-4.13462883300001));
#325554=CARTESIAN_POINT('Ctrl Pts',(-0.819936729000055,2.2,-4.13462883300001));
#325555=CARTESIAN_POINT('Ctrl Pts',(-0.819159048000057,12.2,-4.13327303000001));
#325556=CARTESIAN_POINT('Ctrl Pts',(-0.819159048000057,5.2,-4.13327303000001));
#325557=CARTESIAN_POINT('Ctrl Pts',(-0.819159048000057,2.2,-4.13327303000001));
#325558=CARTESIAN_POINT('Ctrl Pts',(-0.818385244000056,12.2,-4.13192034400002));
#325559=CARTESIAN_POINT('Ctrl Pts',(-0.818385244000056,5.2,-4.13192034400002));
#325560=CARTESIAN_POINT('Ctrl Pts',(-0.818385244000056,2.2,-4.13192034400002));
#325561=CARTESIAN_POINT('Ctrl Pts',(-0.817615311000056,12.2,-4.13057079000001));
#325562=CARTESIAN_POINT('Ctrl Pts',(-0.817615311000056,5.2,-4.13057079000001));
#325563=CARTESIAN_POINT('Ctrl Pts',(-0.817615311000056,2.2,-4.13057079000001));
#325564=CARTESIAN_POINT('Ctrl Pts',(-0.816849244000055,12.2,-4.12922438000002));
#325565=CARTESIAN_POINT('Ctrl Pts',(-0.816849244000055,5.2,-4.12922438000002));
#325566=CARTESIAN_POINT('Ctrl Pts',(-0.816849244000055,2.2,-4.12922438000002));
#325567=CARTESIAN_POINT('Ctrl Pts',(-0.816087040000056,12.2,-4.12788112400001));
#325568=CARTESIAN_POINT('Ctrl Pts',(-0.816087040000056,5.2,-4.12788112400001));
#325569=CARTESIAN_POINT('Ctrl Pts',(-0.816087040000056,2.2,-4.12788112400001));
#325570=CARTESIAN_POINT('Ctrl Pts',(-0.815328694000056,12.2,-4.12654103700001));
#325571=CARTESIAN_POINT('Ctrl Pts',(-0.815328694000056,5.2,-4.12654103700001));
#325572=CARTESIAN_POINT('Ctrl Pts',(-0.815328694000056,2.2,-4.12654103700001));
#325573=CARTESIAN_POINT('Ctrl Pts',(-0.814574201000056,12.2,-4.12520413000002));
#325574=CARTESIAN_POINT('Ctrl Pts',(-0.814574201000056,5.2,-4.12520413000002));
#325575=CARTESIAN_POINT('Ctrl Pts',(-0.814574201000056,2.2,-4.12520413000002));
#325576=CARTESIAN_POINT('Ctrl Pts',(-0.813823558000056,12.2,-4.12387041700002));
#325577=CARTESIAN_POINT('Ctrl Pts',(-0.813823558000056,5.2,-4.12387041700002));
#325578=CARTESIAN_POINT('Ctrl Pts',(-0.813823558000056,2.2,-4.12387041700002));
#325579=CARTESIAN_POINT('Ctrl Pts',(-0.813076758000056,12.2,-4.12253990800002));
#325580=CARTESIAN_POINT('Ctrl Pts',(-0.813076758000056,5.2,-4.12253990800002));
#325581=CARTESIAN_POINT('Ctrl Pts',(-0.813076758000056,2.2,-4.12253990800002));
#325582=CARTESIAN_POINT('Ctrl Pts',(-0.812333800000056,12.2,-4.12121261600001));
#325583=CARTESIAN_POINT('Ctrl Pts',(-0.812333800000056,5.2,-4.12121261600001));
#325584=CARTESIAN_POINT('Ctrl Pts',(-0.812333800000056,2.2,-4.12121261600001));
#325585=CARTESIAN_POINT('Ctrl Pts',(-0.811594676000055,12.2,-4.11988855500002));
#325586=CARTESIAN_POINT('Ctrl Pts',(-0.811594676000055,5.2,-4.11988855500002));
#325587=CARTESIAN_POINT('Ctrl Pts',(-0.811594676000055,2.2,-4.11988855500002));
#325588=CARTESIAN_POINT('Ctrl Pts',(-0.810859382000055,12.2,-4.11856773600002));
#325589=CARTESIAN_POINT('Ctrl Pts',(-0.810859382000055,5.2,-4.11856773600002));
#325590=CARTESIAN_POINT('Ctrl Pts',(-0.810859382000055,2.2,-4.11856773600002));
#325591=CARTESIAN_POINT('Ctrl Pts',(-0.810127916000055,12.2,-4.11725017200002));
#325592=CARTESIAN_POINT('Ctrl Pts',(-0.810127916000055,5.2,-4.11725017200002));
#325593=CARTESIAN_POINT('Ctrl Pts',(-0.810127916000055,2.2,-4.11725017200002));
#325594=CARTESIAN_POINT('Ctrl Pts',(-0.809400270000056,12.2,-4.11593587500001));
#325595=CARTESIAN_POINT('Ctrl Pts',(-0.809400270000056,5.2,-4.11593587500001));
#325596=CARTESIAN_POINT('Ctrl Pts',(-0.809400270000056,2.2,-4.11593587500001));
#325597=CARTESIAN_POINT('Ctrl Pts',(-0.808676442000056,12.2,-4.11462485700001));
#325598=CARTESIAN_POINT('Ctrl Pts',(-0.808676442000056,5.2,-4.11462485700001));
#325599=CARTESIAN_POINT('Ctrl Pts',(-0.808676442000056,2.2,-4.11462485700001));
#325600=CARTESIAN_POINT('Ctrl Pts',(-0.807956425000055,12.2,-4.11331713200001));
#325601=CARTESIAN_POINT('Ctrl Pts',(-0.807956425000055,5.2,-4.11331713200001));
#325602=CARTESIAN_POINT('Ctrl Pts',(-0.807956425000055,2.2,-4.11331713200001));
#325603=CARTESIAN_POINT('Ctrl Pts',(-0.807240215000055,12.2,-4.11201271100001));
#325604=CARTESIAN_POINT('Ctrl Pts',(-0.807240215000055,5.2,-4.11201271100001));
#325605=CARTESIAN_POINT('Ctrl Pts',(-0.807240215000055,2.2,-4.11201271100001));
#325606=CARTESIAN_POINT('Ctrl Pts',(-0.806527808000055,12.2,-4.11071160900002));
#325607=CARTESIAN_POINT('Ctrl Pts',(-0.806527808000055,5.2,-4.11071160900002));
#325608=CARTESIAN_POINT('Ctrl Pts',(-0.806527808000055,2.2,-4.11071160900002));
#325609=CARTESIAN_POINT('Ctrl Pts',(-0.805819199000056,12.2,-4.10941383600001));
#325610=CARTESIAN_POINT('Ctrl Pts',(-0.805819199000056,5.2,-4.10941383600001));
#325611=CARTESIAN_POINT('Ctrl Pts',(-0.805819199000056,2.2,-4.10941383600001));
#325612=CARTESIAN_POINT('Ctrl Pts',(-0.805114383000056,12.2,-4.10811940500002));
#325613=CARTESIAN_POINT('Ctrl Pts',(-0.805114383000056,5.2,-4.10811940500002));
#325614=CARTESIAN_POINT('Ctrl Pts',(-0.805114383000056,2.2,-4.10811940500002));
#325615=CARTESIAN_POINT('Ctrl Pts',(-0.804413354000056,12.2,-4.10682833000001));
#325616=CARTESIAN_POINT('Ctrl Pts',(-0.804413354000056,5.2,-4.10682833000001));
#325617=CARTESIAN_POINT('Ctrl Pts',(-0.804413354000056,2.2,-4.10682833000001));
#325618=CARTESIAN_POINT('Ctrl Pts',(-0.803716109000057,12.2,-4.10554062200001));
#325619=CARTESIAN_POINT('Ctrl Pts',(-0.803716109000057,5.2,-4.10554062200001));
#325620=CARTESIAN_POINT('Ctrl Pts',(-0.803716109000057,2.2,-4.10554062200001));
#325621=CARTESIAN_POINT('Ctrl Pts',(-0.803022642000055,12.2,-4.10425629400001));
#325622=CARTESIAN_POINT('Ctrl Pts',(-0.803022642000055,5.2,-4.10425629400001));
#325623=CARTESIAN_POINT('Ctrl Pts',(-0.803022642000055,2.2,-4.10425629400001));
#325624=CARTESIAN_POINT('Ctrl Pts',(-0.802332949000055,12.2,-4.10297536000002));
#325625=CARTESIAN_POINT('Ctrl Pts',(-0.802332949000055,5.2,-4.10297536000002));
#325626=CARTESIAN_POINT('Ctrl Pts',(-0.802332949000055,2.2,-4.10297536000002));
#325627=CARTESIAN_POINT('Ctrl Pts',(-0.801647024000056,12.2,-4.10169783100002));
#325628=CARTESIAN_POINT('Ctrl Pts',(-0.801647024000056,5.2,-4.10169783100002));
#325629=CARTESIAN_POINT('Ctrl Pts',(-0.801647024000056,2.2,-4.10169783100002));
#325630=CARTESIAN_POINT('Ctrl Pts',(-0.800964863000055,12.2,-4.10042372100001));
#325631=CARTESIAN_POINT('Ctrl Pts',(-0.800964863000055,5.2,-4.10042372100001));
#325632=CARTESIAN_POINT('Ctrl Pts',(-0.800964863000055,2.2,-4.10042372100001));
#325633=CARTESIAN_POINT('Ctrl Pts',(-0.800286459000056,12.2,-4.09915304200001));
#325634=CARTESIAN_POINT('Ctrl Pts',(-0.800286459000056,5.2,-4.09915304200001));
#325635=CARTESIAN_POINT('Ctrl Pts',(-0.800286459000056,2.2,-4.09915304200001));
#325636=CARTESIAN_POINT('Ctrl Pts',(-0.799611809000057,12.2,-4.09788580800001));
#325637=CARTESIAN_POINT('Ctrl Pts',(-0.799611809000057,5.2,-4.09788580800001));
#325638=CARTESIAN_POINT('Ctrl Pts',(-0.799611809000057,2.2,-4.09788580800001));
#325639=CARTESIAN_POINT('Ctrl Pts',(-0.798940908000055,12.2,-4.09662202900002));
#325640=CARTESIAN_POINT('Ctrl Pts',(-0.798940908000055,5.2,-4.09662202900002));
#325641=CARTESIAN_POINT('Ctrl Pts',(-0.798940908000055,2.2,-4.09662202900002));
#325642=CARTESIAN_POINT('Ctrl Pts',(-0.798273750000057,12.2,-4.09536172000001));
#325643=CARTESIAN_POINT('Ctrl Pts',(-0.798273750000057,5.2,-4.09536172000001));
#325644=CARTESIAN_POINT('Ctrl Pts',(-0.798273750000057,2.2,-4.09536172000001));
#325645=CARTESIAN_POINT('Ctrl Pts',(-0.797610330000056,12.2,-4.09410489300001));
#325646=CARTESIAN_POINT('Ctrl Pts',(-0.797610330000056,5.2,-4.09410489300001));
#325647=CARTESIAN_POINT('Ctrl Pts',(-0.797610330000056,2.2,-4.09410489300001));
#325648=CARTESIAN_POINT('Ctrl Pts',(-0.796950643000055,12.2,-4.09285156100001));
#325649=CARTESIAN_POINT('Ctrl Pts',(-0.796950643000055,5.2,-4.09285156100001));
#325650=CARTESIAN_POINT('Ctrl Pts',(-0.796950643000055,2.2,-4.09285156100001));
#325651=CARTESIAN_POINT('Ctrl Pts',(-0.796294684000056,12.2,-4.09160173700001));
#325652=CARTESIAN_POINT('Ctrl Pts',(-0.796294684000056,5.2,-4.09160173700001));
#325653=CARTESIAN_POINT('Ctrl Pts',(-0.796294684000056,2.2,-4.09160173700001));
#325654=CARTESIAN_POINT('Ctrl Pts',(-0.795642447000056,12.2,-4.09035543500002));
#325655=CARTESIAN_POINT('Ctrl Pts',(-0.795642447000056,5.2,-4.09035543500002));
#325656=CARTESIAN_POINT('Ctrl Pts',(-0.795642447000056,2.2,-4.09035543500002));
#325657=CARTESIAN_POINT('Ctrl Pts',(-0.794993928000055,12.2,-4.08911266500001));
#325658=CARTESIAN_POINT('Ctrl Pts',(-0.794993928000055,5.2,-4.08911266500001));
#325659=CARTESIAN_POINT('Ctrl Pts',(-0.794993928000055,2.2,-4.08911266500001));
#325660=CARTESIAN_POINT('Ctrl Pts',(-0.794349120000056,12.2,-4.08787344200002));
#325661=CARTESIAN_POINT('Ctrl Pts',(-0.794349120000056,5.2,-4.08787344200002));
#325662=CARTESIAN_POINT('Ctrl Pts',(-0.794349120000056,2.2,-4.08787344200002));
#325663=CARTESIAN_POINT('Ctrl Pts',(-0.793708020000056,12.2,-4.08663777800002));
#325664=CARTESIAN_POINT('Ctrl Pts',(-0.793708020000056,5.2,-4.08663777800002));
#325665=CARTESIAN_POINT('Ctrl Pts',(-0.793708020000056,2.2,-4.08663777800002));
#325666=CARTESIAN_POINT('Ctrl Pts',(-0.793070621000057,12.2,-4.08540568800001));
#325667=CARTESIAN_POINT('Ctrl Pts',(-0.793070621000057,5.2,-4.08540568800001));
#325668=CARTESIAN_POINT('Ctrl Pts',(-0.793070621000057,2.2,-4.08540568800001));
#325669=CARTESIAN_POINT('Ctrl Pts',(-0.792436919000057,12.2,-4.08417718200001));
#325670=CARTESIAN_POINT('Ctrl Pts',(-0.792436919000057,5.2,-4.08417718200001));
#325671=CARTESIAN_POINT('Ctrl Pts',(-0.792436919000057,2.2,-4.08417718200001));
#325672=CARTESIAN_POINT('Ctrl Pts',(-0.791806906000057,12.2,-4.08295227500002));
#325673=CARTESIAN_POINT('Ctrl Pts',(-0.791806906000057,5.2,-4.08295227500002));
#325674=CARTESIAN_POINT('Ctrl Pts',(-0.791806906000057,2.2,-4.08295227500002));
#325675=CARTESIAN_POINT('Ctrl Pts',(-0.791180580000056,12.2,-4.08173097900002));
#325676=CARTESIAN_POINT('Ctrl Pts',(-0.791180580000056,5.2,-4.08173097900002));
#325677=CARTESIAN_POINT('Ctrl Pts',(-0.791180580000056,2.2,-4.08173097900002));
#325678=CARTESIAN_POINT('Ctrl Pts',(-0.790557934000056,12.2,-4.08051330800001));
#325679=CARTESIAN_POINT('Ctrl Pts',(-0.790557934000056,5.2,-4.08051330800001));
#325680=CARTESIAN_POINT('Ctrl Pts',(-0.790557934000056,2.2,-4.08051330800001));
#325681=CARTESIAN_POINT('Ctrl Pts',(-0.789938961000055,12.2,-4.07929927400001));
#325682=CARTESIAN_POINT('Ctrl Pts',(-0.789938961000055,5.2,-4.07929927400001));
#325683=CARTESIAN_POINT('Ctrl Pts',(-0.789938961000055,2.2,-4.07929927400001));
#325684=CARTESIAN_POINT('Ctrl Pts',(-0.789323659000055,12.2,-4.07808889000002));
#325685=CARTESIAN_POINT('Ctrl Pts',(-0.789323659000055,5.2,-4.07808889000002));
#325686=CARTESIAN_POINT('Ctrl Pts',(-0.789323659000055,2.2,-4.07808889000002));
#325687=CARTESIAN_POINT('Ctrl Pts',(-0.788712019000056,12.2,-4.07688217000001));
#325688=CARTESIAN_POINT('Ctrl Pts',(-0.788712019000056,5.2,-4.07688217000001));
#325689=CARTESIAN_POINT('Ctrl Pts',(-0.788712019000056,2.2,-4.07688217000001));
#325690=CARTESIAN_POINT('Ctrl Pts',(-0.788104037000057,12.2,-4.07567912700001));
#325691=CARTESIAN_POINT('Ctrl Pts',(-0.788104037000057,5.2,-4.07567912700001));
#325692=CARTESIAN_POINT('Ctrl Pts',(-0.788104037000057,2.2,-4.07567912700001));
#325693=CARTESIAN_POINT('Ctrl Pts',(-0.787499708000056,12.2,-4.07447977400002));
#325694=CARTESIAN_POINT('Ctrl Pts',(-0.787499708000056,5.2,-4.07447977400002));
#325695=CARTESIAN_POINT('Ctrl Pts',(-0.787499708000056,2.2,-4.07447977400002));
#325696=CARTESIAN_POINT('Ctrl Pts',(-0.786899026000055,12.2,-4.07328412200001));
#325697=CARTESIAN_POINT('Ctrl Pts',(-0.786899026000055,5.2,-4.07328412200001));
#325698=CARTESIAN_POINT('Ctrl Pts',(-0.786899026000055,2.2,-4.07328412200001));
#325699=CARTESIAN_POINT('Ctrl Pts',(-0.786301985000056,12.2,-4.07209218900002));
#325700=CARTESIAN_POINT('Ctrl Pts',(-0.786301985000056,5.2,-4.07209218900002));
#325701=CARTESIAN_POINT('Ctrl Pts',(-0.786301985000056,2.2,-4.07209218900002));
#325702=CARTESIAN_POINT('Ctrl Pts',(-0.785708579000056,12.2,-4.07090398400001));
#325703=CARTESIAN_POINT('Ctrl Pts',(-0.785708579000056,5.2,-4.07090398400001));
#325704=CARTESIAN_POINT('Ctrl Pts',(-0.785708579000056,2.2,-4.07090398400001));
#325705=CARTESIAN_POINT('Ctrl Pts',(-0.785118804000057,12.2,-4.06971952100001));
#325706=CARTESIAN_POINT('Ctrl Pts',(-0.785118804000057,5.2,-4.06971952100001));
#325707=CARTESIAN_POINT('Ctrl Pts',(-0.785118804000057,2.2,-4.06971952100001));
#325708=CARTESIAN_POINT('Ctrl Pts',(-0.784532652000056,12.2,-4.06853881500002));
#325709=CARTESIAN_POINT('Ctrl Pts',(-0.784532652000056,5.2,-4.06853881500002));
#325710=CARTESIAN_POINT('Ctrl Pts',(-0.784532652000056,2.2,-4.06853881500002));
#325711=CARTESIAN_POINT('Ctrl Pts',(-0.783950118000056,12.2,-4.06736187600002));
#325712=CARTESIAN_POINT('Ctrl Pts',(-0.783950118000056,5.2,-4.06736187600002));
#325713=CARTESIAN_POINT('Ctrl Pts',(-0.783950118000056,2.2,-4.06736187600002));
#325714=CARTESIAN_POINT('Ctrl Pts',(-0.783371197000056,12.2,-4.06618872200001));
#325715=CARTESIAN_POINT('Ctrl Pts',(-0.783371197000056,5.2,-4.06618872200001));
#325716=CARTESIAN_POINT('Ctrl Pts',(-0.783371197000056,2.2,-4.06618872200001));
#325717=CARTESIAN_POINT('Ctrl Pts',(-0.782795883000055,12.2,-4.06501936200002));
#325718=CARTESIAN_POINT('Ctrl Pts',(-0.782795883000055,5.2,-4.06501936200002));
#325719=CARTESIAN_POINT('Ctrl Pts',(-0.782795883000055,2.2,-4.06501936200002));
#325720=CARTESIAN_POINT('Ctrl Pts',(-0.782224170000055,12.2,-4.06385381100002));
#325721=CARTESIAN_POINT('Ctrl Pts',(-0.782224170000055,5.2,-4.06385381100002));
#325722=CARTESIAN_POINT('Ctrl Pts',(-0.782224170000055,2.2,-4.06385381100002));
#325723=CARTESIAN_POINT('Ctrl Pts',(-0.781656052000056,12.2,-4.06269208200001));
#325724=CARTESIAN_POINT('Ctrl Pts',(-0.781656052000056,5.2,-4.06269208200001));
#325725=CARTESIAN_POINT('Ctrl Pts',(-0.781656052000056,2.2,-4.06269208200001));
#325726=CARTESIAN_POINT('Ctrl Pts',(-0.781091522000056,12.2,-4.06153418900002));
#325727=CARTESIAN_POINT('Ctrl Pts',(-0.781091522000056,5.2,-4.06153418900002));
#325728=CARTESIAN_POINT('Ctrl Pts',(-0.781091522000056,2.2,-4.06153418900002));
#325729=CARTESIAN_POINT('Ctrl Pts',(-0.780530576000055,12.2,-4.06038014600002));
#325730=CARTESIAN_POINT('Ctrl Pts',(-0.780530576000055,5.2,-4.06038014600002));
#325731=CARTESIAN_POINT('Ctrl Pts',(-0.780530576000055,2.2,-4.06038014600002));
#325732=CARTESIAN_POINT('Ctrl Pts',(-0.779973208000057,12.2,-4.05922996500002));
#325733=CARTESIAN_POINT('Ctrl Pts',(-0.779973208000057,5.2,-4.05922996500002));
#325734=CARTESIAN_POINT('Ctrl Pts',(-0.779973208000057,2.2,-4.05922996500002));
#325735=CARTESIAN_POINT('Ctrl Pts',(-0.779419410000056,12.2,-4.05808365900001));
#325736=CARTESIAN_POINT('Ctrl Pts',(-0.779419410000056,5.2,-4.05808365900001));
#325737=CARTESIAN_POINT('Ctrl Pts',(-0.779419410000056,2.2,-4.05808365900001));
#325738=CARTESIAN_POINT('Ctrl Pts',(-0.778869177000056,12.2,-4.05694124300001));
#325739=CARTESIAN_POINT('Ctrl Pts',(-0.778869177000056,5.2,-4.05694124300001));
#325740=CARTESIAN_POINT('Ctrl Pts',(-0.778869177000056,2.2,-4.05694124300001));
#325741=CARTESIAN_POINT('Ctrl Pts',(-0.778322505000055,12.2,-4.05580272900002));
#325742=CARTESIAN_POINT('Ctrl Pts',(-0.778322505000055,5.2,-4.05580272900002));
#325743=CARTESIAN_POINT('Ctrl Pts',(-0.778322505000055,2.2,-4.05580272900002));
#325744=CARTESIAN_POINT('Ctrl Pts',(-0.777779384000056,12.2,-4.05466813200002));
#325745=CARTESIAN_POINT('Ctrl Pts',(-0.777779384000056,5.2,-4.05466813200002));
#325746=CARTESIAN_POINT('Ctrl Pts',(-0.777779384000056,2.2,-4.05466813200002));
#325747=CARTESIAN_POINT('Ctrl Pts',(-0.777239810000055,12.2,-4.05353746500001));
#325748=CARTESIAN_POINT('Ctrl Pts',(-0.777239810000055,5.2,-4.05353746500001));
#325749=CARTESIAN_POINT('Ctrl Pts',(-0.777239810000055,2.2,-4.05353746500001));
#325750=CARTESIAN_POINT('Ctrl Pts',(-0.776703778000056,12.2,-4.05241074100001));
#325751=CARTESIAN_POINT('Ctrl Pts',(-0.776703778000056,5.2,-4.05241074100001));
#325752=CARTESIAN_POINT('Ctrl Pts',(-0.776703778000056,2.2,-4.05241074100001));
#325753=CARTESIAN_POINT('Ctrl Pts',(-0.776171280000056,12.2,-4.05128797400002));
#325754=CARTESIAN_POINT('Ctrl Pts',(-0.776171280000056,5.2,-4.05128797400002));
#325755=CARTESIAN_POINT('Ctrl Pts',(-0.776171280000056,2.2,-4.05128797400002));
#325756=CARTESIAN_POINT('Ctrl Pts',(-0.775642310000055,12.2,-4.05016917800001));
#325757=CARTESIAN_POINT('Ctrl Pts',(-0.775642310000055,5.2,-4.05016917800001));
#325758=CARTESIAN_POINT('Ctrl Pts',(-0.775642310000055,2.2,-4.05016917800001));
#325759=CARTESIAN_POINT('Ctrl Pts',(-0.775116863000056,12.2,-4.04905436500002));
#325760=CARTESIAN_POINT('Ctrl Pts',(-0.775116863000056,5.2,-4.04905436500002));
#325761=CARTESIAN_POINT('Ctrl Pts',(-0.775116863000056,2.2,-4.04905436500002));
#325762=CARTESIAN_POINT('Ctrl Pts',(-0.774594932000056,12.2,-4.04794355100002));
#325763=CARTESIAN_POINT('Ctrl Pts',(-0.774594932000056,5.2,-4.04794355100002));
#325764=CARTESIAN_POINT('Ctrl Pts',(-0.774594932000056,2.2,-4.04794355100002));
#325765=CARTESIAN_POINT('Ctrl Pts',(-0.774076510000056,12.2,-4.04683674800001));
#325766=CARTESIAN_POINT('Ctrl Pts',(-0.774076510000056,5.2,-4.04683674800001));
#325767=CARTESIAN_POINT('Ctrl Pts',(-0.774076510000056,2.2,-4.04683674800001));
#325768=CARTESIAN_POINT('Ctrl Pts',(-0.773561591000057,12.2,-4.04573397000001));
#325769=CARTESIAN_POINT('Ctrl Pts',(-0.773561591000057,5.2,-4.04573397000001));
#325770=CARTESIAN_POINT('Ctrl Pts',(-0.773561591000057,2.2,-4.04573397000001));
#325771=CARTESIAN_POINT('Ctrl Pts',(-0.773050169000056,12.2,-4.04463523000001));
#325772=CARTESIAN_POINT('Ctrl Pts',(-0.773050169000056,5.2,-4.04463523000001));
#325773=CARTESIAN_POINT('Ctrl Pts',(-0.773050169000056,2.2,-4.04463523000001));
#325774=CARTESIAN_POINT('Ctrl Pts',(-0.772542238000057,12.2,-4.04354054300001));
#325775=CARTESIAN_POINT('Ctrl Pts',(-0.772542238000057,5.2,-4.04354054300001));
#325776=CARTESIAN_POINT('Ctrl Pts',(-0.772542238000057,2.2,-4.04354054300001));
#325777=CARTESIAN_POINT('Ctrl Pts',(-0.772037790000055,12.2,-4.04244992300002));
#325778=CARTESIAN_POINT('Ctrl Pts',(-0.772037790000055,5.2,-4.04244992300002));
#325779=CARTESIAN_POINT('Ctrl Pts',(-0.772037790000055,2.2,-4.04244992300002));
#325780=CARTESIAN_POINT('Ctrl Pts',(-0.771536819000056,12.2,-4.04136338200002));
#325781=CARTESIAN_POINT('Ctrl Pts',(-0.771536819000056,5.2,-4.04136338200002));
#325782=CARTESIAN_POINT('Ctrl Pts',(-0.771536819000056,2.2,-4.04136338200002));
#325783=CARTESIAN_POINT('Ctrl Pts',(-0.771039320000056,12.2,-4.04028093500001));
#325784=CARTESIAN_POINT('Ctrl Pts',(-0.771039320000056,5.2,-4.04028093500001));
#325785=CARTESIAN_POINT('Ctrl Pts',(-0.771039320000056,2.2,-4.04028093500001));
#325786=CARTESIAN_POINT('Ctrl Pts',(-0.770545286000056,12.2,-4.03920259600001));
#325787=CARTESIAN_POINT('Ctrl Pts',(-0.770545286000056,5.2,-4.03920259600001));
#325788=CARTESIAN_POINT('Ctrl Pts',(-0.770545286000056,2.2,-4.03920259600001));
#325789=CARTESIAN_POINT('Ctrl Pts',(-0.770054709000056,12.2,-4.03812837800002));
#325790=CARTESIAN_POINT('Ctrl Pts',(-0.770054709000056,5.2,-4.03812837800002));
#325791=CARTESIAN_POINT('Ctrl Pts',(-0.770054709000056,2.2,-4.03812837800002));
#325792=CARTESIAN_POINT('Ctrl Pts',(-0.769567583000056,12.2,-4.03705829600002));
#325793=CARTESIAN_POINT('Ctrl Pts',(-0.769567583000056,5.2,-4.03705829600002));
#325794=CARTESIAN_POINT('Ctrl Pts',(-0.769567583000056,2.2,-4.03705829600002));
#325795=CARTESIAN_POINT('Ctrl Pts',(-0.769083902000055,12.2,-4.03599236300002));
#325796=CARTESIAN_POINT('Ctrl Pts',(-0.769083902000055,5.2,-4.03599236300002));
#325797=CARTESIAN_POINT('Ctrl Pts',(-0.769083902000055,2.2,-4.03599236300002));
#325798=CARTESIAN_POINT('Ctrl Pts',(-0.768603660000055,12.2,-4.03493059300001));
#325799=CARTESIAN_POINT('Ctrl Pts',(-0.768603660000055,5.2,-4.03493059300001));
#325800=CARTESIAN_POINT('Ctrl Pts',(-0.768603660000055,2.2,-4.03493059300001));
#325801=CARTESIAN_POINT('Ctrl Pts',(-0.768126848000056,12.2,-4.03387300000002));
#325802=CARTESIAN_POINT('Ctrl Pts',(-0.768126848000056,5.2,-4.03387300000002));
#325803=CARTESIAN_POINT('Ctrl Pts',(-0.768126848000056,2.2,-4.03387300000002));
#325804=CARTESIAN_POINT('Ctrl Pts',(-0.767653461000056,12.2,-4.03281959800001));
#325805=CARTESIAN_POINT('Ctrl Pts',(-0.767653461000056,5.2,-4.03281959800001));
#325806=CARTESIAN_POINT('Ctrl Pts',(-0.767653461000056,2.2,-4.03281959800001));
#325807=CARTESIAN_POINT('Ctrl Pts',(-0.767183491000055,12.2,-4.03177040100001));
#325808=CARTESIAN_POINT('Ctrl Pts',(-0.767183491000055,5.2,-4.03177040100001));
#325809=CARTESIAN_POINT('Ctrl Pts',(-0.767183491000055,2.2,-4.03177040100001));
#325810=CARTESIAN_POINT('Ctrl Pts',(-0.766716933000057,12.2,-4.03072542300002));
#325811=CARTESIAN_POINT('Ctrl Pts',(-0.766716933000057,5.2,-4.03072542300002));
#325812=CARTESIAN_POINT('Ctrl Pts',(-0.766716933000057,2.2,-4.03072542300002));
#325813=CARTESIAN_POINT('Ctrl Pts',(-0.766253778000056,12.2,-4.02968467800001));
#325814=CARTESIAN_POINT('Ctrl Pts',(-0.766253778000056,5.2,-4.02968467800001));
#325815=CARTESIAN_POINT('Ctrl Pts',(-0.766253778000056,2.2,-4.02968467800001));
#325816=CARTESIAN_POINT('Ctrl Pts',(-0.765794021000056,12.2,-4.02864818000001));
#325817=CARTESIAN_POINT('Ctrl Pts',(-0.765794021000056,5.2,-4.02864818000001));
#325818=CARTESIAN_POINT('Ctrl Pts',(-0.765794021000056,2.2,-4.02864818000001));
#325819=CARTESIAN_POINT('Ctrl Pts',(-0.765337654000057,12.2,-4.02761594400001));
#325820=CARTESIAN_POINT('Ctrl Pts',(-0.765337654000057,5.2,-4.02761594400001));
#325821=CARTESIAN_POINT('Ctrl Pts',(-0.765337654000057,2.2,-4.02761594400001));
#325822=CARTESIAN_POINT('Ctrl Pts',(-0.764884670000056,12.2,-4.02658798200001));
#325823=CARTESIAN_POINT('Ctrl Pts',(-0.764884670000056,5.2,-4.02658798200001));
#325824=CARTESIAN_POINT('Ctrl Pts',(-0.764884670000056,2.2,-4.02658798200001));
#325825=CARTESIAN_POINT('Ctrl Pts',(-0.764435063000055,12.2,-4.02556431100002));
#325826=CARTESIAN_POINT('Ctrl Pts',(-0.764435063000055,5.2,-4.02556431100002));
#325827=CARTESIAN_POINT('Ctrl Pts',(-0.764435063000055,2.2,-4.02556431100002));
#325828=CARTESIAN_POINT('Ctrl Pts',(-0.763988825000055,12.2,-4.02454494200001));
#325829=CARTESIAN_POINT('Ctrl Pts',(-0.763988825000055,5.2,-4.02454494200001));
#325830=CARTESIAN_POINT('Ctrl Pts',(-0.763988825000055,2.2,-4.02454494200001));
#325831=CARTESIAN_POINT('Ctrl Pts',(-0.763545950000056,12.2,-4.02352989200002));
#325832=CARTESIAN_POINT('Ctrl Pts',(-0.763545950000056,5.2,-4.02352989200002));
#325833=CARTESIAN_POINT('Ctrl Pts',(-0.763545950000056,2.2,-4.02352989200002));
#325834=CARTESIAN_POINT('Ctrl Pts',(-0.763106429000056,12.2,-4.02251917300001));
#325835=CARTESIAN_POINT('Ctrl Pts',(-0.763106429000056,5.2,-4.02251917300001));
#325836=CARTESIAN_POINT('Ctrl Pts',(-0.763106429000056,2.2,-4.02251917300001));
#325837=CARTESIAN_POINT('Ctrl Pts',(-0.762670257000057,12.2,-4.02151280100002));
#325838=CARTESIAN_POINT('Ctrl Pts',(-0.762670257000057,5.2,-4.02151280100002));
#325839=CARTESIAN_POINT('Ctrl Pts',(-0.762670257000057,2.2,-4.02151280100002));
#325840=CARTESIAN_POINT('Ctrl Pts',(-0.762237425000055,12.2,-4.02051078900001));
#325841=CARTESIAN_POINT('Ctrl Pts',(-0.762237425000055,5.2,-4.02051078900001));
#325842=CARTESIAN_POINT('Ctrl Pts',(-0.762237425000055,2.2,-4.02051078900001));
#325843=CARTESIAN_POINT('Ctrl Pts',(-0.761807927000057,12.2,-4.01951315200002));
#325844=CARTESIAN_POINT('Ctrl Pts',(-0.761807927000057,5.2,-4.01951315200002));
#325845=CARTESIAN_POINT('Ctrl Pts',(-0.761807927000057,2.2,-4.01951315200002));
#325846=CARTESIAN_POINT('Ctrl Pts',(-0.761381757000056,12.2,-4.01851990400001));
#325847=CARTESIAN_POINT('Ctrl Pts',(-0.761381757000056,5.2,-4.01851990400001));
#325848=CARTESIAN_POINT('Ctrl Pts',(-0.761381757000056,2.2,-4.01851990400001));
#325849=CARTESIAN_POINT('Ctrl Pts',(-0.760958905000055,12.2,-4.01753105900001));
#325850=CARTESIAN_POINT('Ctrl Pts',(-0.760958905000055,5.2,-4.01753105900001));
#325851=CARTESIAN_POINT('Ctrl Pts',(-0.760958905000055,2.2,-4.01753105900001));
#325852=CARTESIAN_POINT('Ctrl Pts',(-0.760539364000056,12.2,-4.01654663200001));
#325853=CARTESIAN_POINT('Ctrl Pts',(-0.760539364000056,5.2,-4.01654663200001));
#325854=CARTESIAN_POINT('Ctrl Pts',(-0.760539364000056,2.2,-4.01654663200001));
#325855=CARTESIAN_POINT('Ctrl Pts',(-0.760123129000055,12.2,-4.01556663700001));
#325856=CARTESIAN_POINT('Ctrl Pts',(-0.760123129000055,5.2,-4.01556663700001));
#325857=CARTESIAN_POINT('Ctrl Pts',(-0.760123129000055,2.2,-4.01556663700001));
#325858=CARTESIAN_POINT('Ctrl Pts',(-0.759710191000057,12.2,-4.01459108800001));
#325859=CARTESIAN_POINT('Ctrl Pts',(-0.759710191000057,5.2,-4.01459108800001));
#325860=CARTESIAN_POINT('Ctrl Pts',(-0.759710191000057,2.2,-4.01459108800001));
#325861=CARTESIAN_POINT('Ctrl Pts',(-0.759300543000055,12.2,-4.01362000100002));
#325862=CARTESIAN_POINT('Ctrl Pts',(-0.759300543000055,5.2,-4.01362000100002));
#325863=CARTESIAN_POINT('Ctrl Pts',(-0.759300543000055,2.2,-4.01362000100002));
#325864=CARTESIAN_POINT('Ctrl Pts',(-0.758894177000055,12.2,-4.01265338900001));
#325865=CARTESIAN_POINT('Ctrl Pts',(-0.758894177000055,5.2,-4.01265338900001));
#325866=CARTESIAN_POINT('Ctrl Pts',(-0.758894177000055,2.2,-4.01265338900001));
#325867=CARTESIAN_POINT('Ctrl Pts',(-0.758491086000056,12.2,-4.01169126700001));
#325868=CARTESIAN_POINT('Ctrl Pts',(-0.758491086000056,5.2,-4.01169126700001));
#325869=CARTESIAN_POINT('Ctrl Pts',(-0.758491086000056,2.2,-4.01169126700001));
#325870=CARTESIAN_POINT('Ctrl Pts',(-0.758091263000056,12.2,-4.01073364900002));
#325871=CARTESIAN_POINT('Ctrl Pts',(-0.758091263000056,5.2,-4.01073364900002));
#325872=CARTESIAN_POINT('Ctrl Pts',(-0.758091263000056,2.2,-4.01073364900002));
#325873=CARTESIAN_POINT('Ctrl Pts',(-0.757694698000057,12.2,-4.00978055000001));
#325874=CARTESIAN_POINT('Ctrl Pts',(-0.757694698000057,5.2,-4.00978055000001));
#325875=CARTESIAN_POINT('Ctrl Pts',(-0.757694698000057,2.2,-4.00978055000001));
#325876=CARTESIAN_POINT('Ctrl Pts',(-0.757301387000057,12.2,-4.00883198500001));
#325877=CARTESIAN_POINT('Ctrl Pts',(-0.757301387000057,5.2,-4.00883198500001));
#325878=CARTESIAN_POINT('Ctrl Pts',(-0.757301387000057,2.2,-4.00883198500001));
#325879=CARTESIAN_POINT('Ctrl Pts',(-0.756911320000055,12.2,-4.00788796800001));
#325880=CARTESIAN_POINT('Ctrl Pts',(-0.756911320000055,5.2,-4.00788796800001));
#325881=CARTESIAN_POINT('Ctrl Pts',(-0.756911320000055,2.2,-4.00788796800001));
#325882=CARTESIAN_POINT('Ctrl Pts',(-0.756524489000056,12.2,-4.00694851300001));
#325883=CARTESIAN_POINT('Ctrl Pts',(-0.756524489000056,5.2,-4.00694851300001));
#325884=CARTESIAN_POINT('Ctrl Pts',(-0.756524489000056,2.2,-4.00694851300001));
#325885=CARTESIAN_POINT('Ctrl Pts',(-0.756140888000055,12.2,-4.00601363600002));
#325886=CARTESIAN_POINT('Ctrl Pts',(-0.756140888000055,5.2,-4.00601363600002));
#325887=CARTESIAN_POINT('Ctrl Pts',(-0.756140888000055,2.2,-4.00601363600002));
#325888=CARTESIAN_POINT('Ctrl Pts',(-0.755760509000056,12.2,-4.00508335200001));
#325889=CARTESIAN_POINT('Ctrl Pts',(-0.755760509000056,5.2,-4.00508335200001));
#325890=CARTESIAN_POINT('Ctrl Pts',(-0.755760509000056,2.2,-4.00508335200001));
#325891=CARTESIAN_POINT('Ctrl Pts',(-0.755383344000055,12.2,-4.00415767300002));
#325892=CARTESIAN_POINT('Ctrl Pts',(-0.755383344000055,5.2,-4.00415767300002));
#325893=CARTESIAN_POINT('Ctrl Pts',(-0.755383344000055,2.2,-4.00415767300002));
#325894=CARTESIAN_POINT('Ctrl Pts',(-0.755009383000056,12.2,-4.00323661600002));
#325895=CARTESIAN_POINT('Ctrl Pts',(-0.755009383000056,5.2,-4.00323661600002));
#325896=CARTESIAN_POINT('Ctrl Pts',(-0.755009383000056,2.2,-4.00323661600002));
#325897=CARTESIAN_POINT('Ctrl Pts',(-0.754638622000057,12.2,-4.00232019600002));
#325898=CARTESIAN_POINT('Ctrl Pts',(-0.754638622000057,5.2,-4.00232019600002));
#325899=CARTESIAN_POINT('Ctrl Pts',(-0.754638622000057,2.2,-4.00232019600002));
#325900=CARTESIAN_POINT('Ctrl Pts',(-0.754271050000056,12.2,-4.00140842600001));
#325901=CARTESIAN_POINT('Ctrl Pts',(-0.754271050000056,5.2,-4.00140842600001));
#325902=CARTESIAN_POINT('Ctrl Pts',(-0.754271050000056,2.2,-4.00140842600001));
#325903=CARTESIAN_POINT('Ctrl Pts',(-0.753906660000055,12.2,-4.00050132300001));
#325904=CARTESIAN_POINT('Ctrl Pts',(-0.753906660000055,5.2,-4.00050132300001));
#325905=CARTESIAN_POINT('Ctrl Pts',(-0.753906660000055,2.2,-4.00050132300001));
#325906=CARTESIAN_POINT('Ctrl Pts',(-0.753545444000056,12.2,-3.99959889900002));
#325907=CARTESIAN_POINT('Ctrl Pts',(-0.753545444000056,5.2,-3.99959889900002));
#325908=CARTESIAN_POINT('Ctrl Pts',(-0.753545444000056,2.2,-3.99959889900002));
#325909=CARTESIAN_POINT('Ctrl Pts',(-0.753187395000056,12.2,-3.99870117100001));
#325910=CARTESIAN_POINT('Ctrl Pts',(-0.753187395000056,5.2,-3.99870117100001));
#325911=CARTESIAN_POINT('Ctrl Pts',(-0.753187395000056,2.2,-3.99870117100001));
#325912=CARTESIAN_POINT('Ctrl Pts',(-0.752832503000055,12.2,-3.99780815500002));
#325913=CARTESIAN_POINT('Ctrl Pts',(-0.752832503000055,5.2,-3.99780815500002));
#325914=CARTESIAN_POINT('Ctrl Pts',(-0.752832503000055,2.2,-3.99780815500002));
#325915=CARTESIAN_POINT('Ctrl Pts',(-0.752480762000056,12.2,-3.99691986300001));
#325916=CARTESIAN_POINT('Ctrl Pts',(-0.752480762000056,5.2,-3.99691986300001));
#325917=CARTESIAN_POINT('Ctrl Pts',(-0.752480762000056,2.2,-3.99691986300001));
#325918=CARTESIAN_POINT('Ctrl Pts',(-0.752132163000055,12.2,-3.99603631100002));
#325919=CARTESIAN_POINT('Ctrl Pts',(-0.752132163000055,5.2,-3.99603631100002));
#325920=CARTESIAN_POINT('Ctrl Pts',(-0.752132163000055,2.2,-3.99603631100002));
#325921=CARTESIAN_POINT('Ctrl Pts',(-0.751786697000056,12.2,-3.99515751500001));
#325922=CARTESIAN_POINT('Ctrl Pts',(-0.751786697000056,5.2,-3.99515751500001));
#325923=CARTESIAN_POINT('Ctrl Pts',(-0.751786697000056,2.2,-3.99515751500001));
#325924=CARTESIAN_POINT('Ctrl Pts',(-0.751444357000055,12.2,-3.99428348800001));
#325925=CARTESIAN_POINT('Ctrl Pts',(-0.751444357000055,5.2,-3.99428348800001));
#325926=CARTESIAN_POINT('Ctrl Pts',(-0.751444357000055,2.2,-3.99428348800001));
#325927=CARTESIAN_POINT('Ctrl Pts',(-0.751105134000056,12.2,-3.99341424700001));
#325928=CARTESIAN_POINT('Ctrl Pts',(-0.751105134000056,5.2,-3.99341424700001));
#325929=CARTESIAN_POINT('Ctrl Pts',(-0.751105134000056,2.2,-3.99341424700001));
#325930=CARTESIAN_POINT('Ctrl Pts',(-0.750769020000056,12.2,-3.99254980800002));
#325931=CARTESIAN_POINT('Ctrl Pts',(-0.750769020000056,5.2,-3.99254980800002));
#325932=CARTESIAN_POINT('Ctrl Pts',(-0.750769020000056,2.2,-3.99254980800002));
#325933=CARTESIAN_POINT('Ctrl Pts',(-0.750436006000056,12.2,-3.99169018200002));
#325934=CARTESIAN_POINT('Ctrl Pts',(-0.750436006000056,5.2,-3.99169018200002));
#325935=CARTESIAN_POINT('Ctrl Pts',(-0.750436006000056,2.2,-3.99169018200002));
#325936=CARTESIAN_POINT('Ctrl Pts',(-0.750106085000055,12.2,-3.99083538700001));
#325937=CARTESIAN_POINT('Ctrl Pts',(-0.750106085000055,5.2,-3.99083538700001));
#325938=CARTESIAN_POINT('Ctrl Pts',(-0.750106085000055,2.2,-3.99083538700001));
#325939=CARTESIAN_POINT('Ctrl Pts',(-0.749779247000056,12.2,-3.98998543900001));
#325940=CARTESIAN_POINT('Ctrl Pts',(-0.749779247000056,5.2,-3.98998543900001));
#325941=CARTESIAN_POINT('Ctrl Pts',(-0.749779247000056,2.2,-3.98998543900001));
#325942=CARTESIAN_POINT('Ctrl Pts',(-0.749455485000056,12.2,-3.98914035100002));
#325943=CARTESIAN_POINT('Ctrl Pts',(-0.749455485000056,5.2,-3.98914035100002));
#325944=CARTESIAN_POINT('Ctrl Pts',(-0.749455485000056,2.2,-3.98914035100002));
#325945=CARTESIAN_POINT('Ctrl Pts',(-0.749134790000056,12.2,-3.98830014000001));
#325946=CARTESIAN_POINT('Ctrl Pts',(-0.749134790000056,5.2,-3.98830014000001));
#325947=CARTESIAN_POINT('Ctrl Pts',(-0.749134790000056,2.2,-3.98830014000001));
#325948=CARTESIAN_POINT('Ctrl Pts',(-0.748817152000055,12.2,-3.98746481800002));
#325949=CARTESIAN_POINT('Ctrl Pts',(-0.748817152000055,5.2,-3.98746481800002));
#325950=CARTESIAN_POINT('Ctrl Pts',(-0.748817152000055,2.2,-3.98746481800002));
#325951=CARTESIAN_POINT('Ctrl Pts',(-0.748502565000055,12.2,-3.98663440500002));
#325952=CARTESIAN_POINT('Ctrl Pts',(-0.748502565000055,5.2,-3.98663440500002));
#325953=CARTESIAN_POINT('Ctrl Pts',(-0.748502565000055,2.2,-3.98663440500002));
#325954=CARTESIAN_POINT('Ctrl Pts',(-0.748191019000056,12.2,-3.98580891300002));
#325955=CARTESIAN_POINT('Ctrl Pts',(-0.748191019000056,5.2,-3.98580891300002));
#325956=CARTESIAN_POINT('Ctrl Pts',(-0.748191019000056,2.2,-3.98580891300002));
#325957=CARTESIAN_POINT('Ctrl Pts',(-0.747882505000056,12.2,-3.98498835800002));
#325958=CARTESIAN_POINT('Ctrl Pts',(-0.747882505000056,5.2,-3.98498835800002));
#325959=CARTESIAN_POINT('Ctrl Pts',(-0.747882505000056,2.2,-3.98498835800002));
#325960=CARTESIAN_POINT('Ctrl Pts',(-0.747577015000056,12.2,-3.98417275500002));
#325961=CARTESIAN_POINT('Ctrl Pts',(-0.747577015000056,5.2,-3.98417275500002));
#325962=CARTESIAN_POINT('Ctrl Pts',(-0.747577015000056,2.2,-3.98417275500002));
#325963=CARTESIAN_POINT('Ctrl Pts',(-0.747274539000056,12.2,-3.98336212200002));
#325964=CARTESIAN_POINT('Ctrl Pts',(-0.747274539000056,5.2,-3.98336212200002));
#325965=CARTESIAN_POINT('Ctrl Pts',(-0.747274539000056,2.2,-3.98336212200002));
#325966=CARTESIAN_POINT('Ctrl Pts',(-0.746975070000057,12.2,-3.98255647000001));
#325967=CARTESIAN_POINT('Ctrl Pts',(-0.746975070000057,5.2,-3.98255647000001));
#325968=CARTESIAN_POINT('Ctrl Pts',(-0.746975070000057,2.2,-3.98255647000001));
#325969=CARTESIAN_POINT('Ctrl Pts',(-0.746678599000056,12.2,-3.98175581800002));
#325970=CARTESIAN_POINT('Ctrl Pts',(-0.746678599000056,5.2,-3.98175581800002));
#325971=CARTESIAN_POINT('Ctrl Pts',(-0.746678599000056,2.2,-3.98175581800002));
#325972=CARTESIAN_POINT('Ctrl Pts',(-0.746385115000056,12.2,-3.98096018100001));
#325973=CARTESIAN_POINT('Ctrl Pts',(-0.746385115000056,5.2,-3.98096018100001));
#325974=CARTESIAN_POINT('Ctrl Pts',(-0.746385115000056,2.2,-3.98096018100001));
#325975=CARTESIAN_POINT('Ctrl Pts',(-0.746094611000055,12.2,-3.98016957200001));
#325976=CARTESIAN_POINT('Ctrl Pts',(-0.746094611000055,5.2,-3.98016957200001));
#325977=CARTESIAN_POINT('Ctrl Pts',(-0.746094611000055,2.2,-3.98016957200001));
#325978=CARTESIAN_POINT('Ctrl Pts',(-0.745807078000055,12.2,-3.97938401000001));
#325979=CARTESIAN_POINT('Ctrl Pts',(-0.745807078000055,5.2,-3.97938401000001));
#325980=CARTESIAN_POINT('Ctrl Pts',(-0.745807078000055,2.2,-3.97938401000001));
#325981=CARTESIAN_POINT('Ctrl Pts',(-0.745522507000055,12.2,-3.97860350800002));
#325982=CARTESIAN_POINT('Ctrl Pts',(-0.745522507000055,5.2,-3.97860350800002));
#325983=CARTESIAN_POINT('Ctrl Pts',(-0.745522507000055,2.2,-3.97860350800002));
#325984=CARTESIAN_POINT('Ctrl Pts',(-0.745240887000056,12.2,-3.97782808200001));
#325985=CARTESIAN_POINT('Ctrl Pts',(-0.745240887000056,5.2,-3.97782808200001));
#325986=CARTESIAN_POINT('Ctrl Pts',(-0.745240887000056,2.2,-3.97782808200001));
#325987=CARTESIAN_POINT('Ctrl Pts',(-0.744962211000055,12.2,-3.97705774900002));
#325988=CARTESIAN_POINT('Ctrl Pts',(-0.744962211000055,5.2,-3.97705774900002));
#325989=CARTESIAN_POINT('Ctrl Pts',(-0.744962211000055,2.2,-3.97705774900002));
#325990=CARTESIAN_POINT('Ctrl Pts',(-0.744686470000057,12.2,-3.97629252400002));
#325991=CARTESIAN_POINT('Ctrl Pts',(-0.744686470000057,5.2,-3.97629252400002));
#325992=CARTESIAN_POINT('Ctrl Pts',(-0.744686470000057,2.2,-3.97629252400002));
#325993=CARTESIAN_POINT('Ctrl Pts',(-0.744413653000056,12.2,-3.97553242100001));
#325994=CARTESIAN_POINT('Ctrl Pts',(-0.744413653000056,5.2,-3.97553242100001));
#325995=CARTESIAN_POINT('Ctrl Pts',(-0.744413653000056,2.2,-3.97553242100001));
#325996=CARTESIAN_POINT('Ctrl Pts',(-0.744143752000056,12.2,-3.97477745900002));
#325997=CARTESIAN_POINT('Ctrl Pts',(-0.744143752000056,5.2,-3.97477745900002));
#325998=CARTESIAN_POINT('Ctrl Pts',(-0.744143752000056,2.2,-3.97477745900002));
#325999=CARTESIAN_POINT('Ctrl Pts',(-0.743876758000056,12.2,-3.97402765100002));
#326000=CARTESIAN_POINT('Ctrl Pts',(-0.743876758000056,5.2,-3.97402765100002));
#326001=CARTESIAN_POINT('Ctrl Pts',(-0.743876758000056,2.2,-3.97402765100002));
#326002=CARTESIAN_POINT('Ctrl Pts',(-0.743612661000055,12.2,-3.97328301400002));
#326003=CARTESIAN_POINT('Ctrl Pts',(-0.743612661000055,5.2,-3.97328301400002));
#326004=CARTESIAN_POINT('Ctrl Pts',(-0.743612661000055,2.2,-3.97328301400002));
#326005=CARTESIAN_POINT('Ctrl Pts',(-0.743351452000055,12.2,-3.97254356300001));
#326006=CARTESIAN_POINT('Ctrl Pts',(-0.743351452000055,5.2,-3.97254356300001));
#326007=CARTESIAN_POINT('Ctrl Pts',(-0.743351452000055,2.2,-3.97254356300001));
#326008=CARTESIAN_POINT('Ctrl Pts',(-0.743093122000056,12.2,-3.97180931500001));
#326009=CARTESIAN_POINT('Ctrl Pts',(-0.743093122000056,5.2,-3.97180931500001));
#326010=CARTESIAN_POINT('Ctrl Pts',(-0.743093122000056,2.2,-3.97180931500001));
#326011=CARTESIAN_POINT('Ctrl Pts',(-0.742837660000056,12.2,-3.97108028500002));
#326012=CARTESIAN_POINT('Ctrl Pts',(-0.742837660000056,5.2,-3.97108028500002));
#326013=CARTESIAN_POINT('Ctrl Pts',(-0.742837660000056,2.2,-3.97108028500002));
#326014=CARTESIAN_POINT('Ctrl Pts',(-0.742585058000056,12.2,-3.97035649000001));
#326015=CARTESIAN_POINT('Ctrl Pts',(-0.742585058000056,5.2,-3.97035649000001));
#326016=CARTESIAN_POINT('Ctrl Pts',(-0.742585058000056,2.2,-3.97035649000001));
#326017=CARTESIAN_POINT('Ctrl Pts',(-0.742335305000056,12.2,-3.96963794400001));
#326018=CARTESIAN_POINT('Ctrl Pts',(-0.742335305000056,5.2,-3.96963794400001));
#326019=CARTESIAN_POINT('Ctrl Pts',(-0.742335305000056,2.2,-3.96963794400001));
#326020=CARTESIAN_POINT('Ctrl Pts',(-0.742088393000057,12.2,-3.96892466500002));
#326021=CARTESIAN_POINT('Ctrl Pts',(-0.742088393000057,5.2,-3.96892466500002));
#326022=CARTESIAN_POINT('Ctrl Pts',(-0.742088393000057,2.2,-3.96892466500002));
#326023=CARTESIAN_POINT('Ctrl Pts',(-0.741844312000056,12.2,-3.96821666800002));
#326024=CARTESIAN_POINT('Ctrl Pts',(-0.741844312000056,5.2,-3.96821666800002));
#326025=CARTESIAN_POINT('Ctrl Pts',(-0.741844312000056,2.2,-3.96821666800002));
#326026=CARTESIAN_POINT('Ctrl Pts',(-0.741603052000055,12.2,-3.96751396800001));
#326027=CARTESIAN_POINT('Ctrl Pts',(-0.741603052000055,5.2,-3.96751396800001));
#326028=CARTESIAN_POINT('Ctrl Pts',(-0.741603052000055,2.2,-3.96751396800001));
#326029=CARTESIAN_POINT('Ctrl Pts',(-0.741364603000055,12.2,-3.96681658300002));
#326030=CARTESIAN_POINT('Ctrl Pts',(-0.741364603000055,5.2,-3.96681658300002));
#326031=CARTESIAN_POINT('Ctrl Pts',(-0.741364603000055,2.2,-3.96681658300002));
#326032=CARTESIAN_POINT('Ctrl Pts',(-0.741128956000056,12.2,-3.96612452900001));
#326033=CARTESIAN_POINT('Ctrl Pts',(-0.741128956000056,5.2,-3.96612452900001));
#326034=CARTESIAN_POINT('Ctrl Pts',(-0.741128956000056,2.2,-3.96612452900001));
#326035=CARTESIAN_POINT('Ctrl Pts',(-0.740896100000056,12.2,-3.96543782100002));
#326036=CARTESIAN_POINT('Ctrl Pts',(-0.740896100000056,5.2,-3.96543782100002));
#326037=CARTESIAN_POINT('Ctrl Pts',(-0.740896100000056,2.2,-3.96543782100002));
#326038=CARTESIAN_POINT('Ctrl Pts',(-0.740666025000056,12.2,-3.96475647700001));
#326039=CARTESIAN_POINT('Ctrl Pts',(-0.740666025000056,5.2,-3.96475647700001));
#326040=CARTESIAN_POINT('Ctrl Pts',(-0.740666025000056,2.2,-3.96475647700001));
#326041=CARTESIAN_POINT('Ctrl Pts',(-0.740438724000055,12.2,-3.96408051000002));
#326042=CARTESIAN_POINT('Ctrl Pts',(-0.740438724000055,5.2,-3.96408051000002));
#326043=CARTESIAN_POINT('Ctrl Pts',(-0.740438724000055,2.2,-3.96408051000002));
#326044=CARTESIAN_POINT('Ctrl Pts',(-0.740214183000055,12.2,-3.96340994000001));
#326045=CARTESIAN_POINT('Ctrl Pts',(-0.740214183000055,5.2,-3.96340994000001));
#326046=CARTESIAN_POINT('Ctrl Pts',(-0.740214183000055,2.2,-3.96340994000001));
#326047=CARTESIAN_POINT('Ctrl Pts',(-0.739992395000056,12.2,-3.96274478100001));
#326048=CARTESIAN_POINT('Ctrl Pts',(-0.739992395000056,5.2,-3.96274478100001));
#326049=CARTESIAN_POINT('Ctrl Pts',(-0.739992395000056,2.2,-3.96274478100001));
#326050=CARTESIAN_POINT('Ctrl Pts',(-0.739773349000057,12.2,-3.96208504900001));
#326051=CARTESIAN_POINT('Ctrl Pts',(-0.739773349000057,5.2,-3.96208504900001));
#326052=CARTESIAN_POINT('Ctrl Pts',(-0.739773349000057,2.2,-3.96208504900001));
#326053=CARTESIAN_POINT('Ctrl Pts',(-0.739557033000056,12.2,-3.96143076100001));
#326054=CARTESIAN_POINT('Ctrl Pts',(-0.739557033000056,5.2,-3.96143076100001));
#326055=CARTESIAN_POINT('Ctrl Pts',(-0.739557033000056,2.2,-3.96143076100001));
#326056=CARTESIAN_POINT('Ctrl Pts',(-0.739343439000055,12.2,-3.96078193500002));
#326057=CARTESIAN_POINT('Ctrl Pts',(-0.739343439000055,5.2,-3.96078193500002));
#326058=CARTESIAN_POINT('Ctrl Pts',(-0.739343439000055,2.2,-3.96078193500002));
#326059=CARTESIAN_POINT('Ctrl Pts',(-0.739132557000056,12.2,-3.96013858500002));
#326060=CARTESIAN_POINT('Ctrl Pts',(-0.739132557000056,5.2,-3.96013858500002));
#326061=CARTESIAN_POINT('Ctrl Pts',(-0.739132557000056,2.2,-3.96013858500002));
#326062=CARTESIAN_POINT('Ctrl Pts',(-0.738924376000056,12.2,-3.95950072800002));
#326063=CARTESIAN_POINT('Ctrl Pts',(-0.738924376000056,5.2,-3.95950072800002));
#326064=CARTESIAN_POINT('Ctrl Pts',(-0.738924376000056,2.2,-3.95950072800002));
#326065=CARTESIAN_POINT('Ctrl Pts',(-0.738718886000056,12.2,-3.95886838100001));
#326066=CARTESIAN_POINT('Ctrl Pts',(-0.738718886000056,5.2,-3.95886838100001));
#326067=CARTESIAN_POINT('Ctrl Pts',(-0.738718886000056,2.2,-3.95886838100001));
#326068=CARTESIAN_POINT('Ctrl Pts',(-0.738516076000056,12.2,-3.95824156200002));
#326069=CARTESIAN_POINT('Ctrl Pts',(-0.738516076000056,5.2,-3.95824156200002));
#326070=CARTESIAN_POINT('Ctrl Pts',(-0.738516076000056,2.2,-3.95824156200002));
#326071=CARTESIAN_POINT('Ctrl Pts',(-0.738315935000056,12.2,-3.95762028500001));
#326072=CARTESIAN_POINT('Ctrl Pts',(-0.738315935000056,5.2,-3.95762028500001));
#326073=CARTESIAN_POINT('Ctrl Pts',(-0.738315935000056,2.2,-3.95762028500001));
#326074=CARTESIAN_POINT('Ctrl Pts',(-0.738118454000055,12.2,-3.95700456700002));
#326075=CARTESIAN_POINT('Ctrl Pts',(-0.738118454000055,5.2,-3.95700456700002));
#326076=CARTESIAN_POINT('Ctrl Pts',(-0.738118454000055,2.2,-3.95700456700002));
#326077=CARTESIAN_POINT('Ctrl Pts',(-0.737923622000055,12.2,-3.95639442600002));
#326078=CARTESIAN_POINT('Ctrl Pts',(-0.737923622000055,5.2,-3.95639442600002));
#326079=CARTESIAN_POINT('Ctrl Pts',(-0.737923622000055,2.2,-3.95639442600002));
#326080=CARTESIAN_POINT('Ctrl Pts',(-0.737731429000055,12.2,-3.95578987800001));
#326081=CARTESIAN_POINT('Ctrl Pts',(-0.737731429000055,5.2,-3.95578987800001));
#326082=CARTESIAN_POINT('Ctrl Pts',(-0.737731429000055,2.2,-3.95578987800001));
#326083=CARTESIAN_POINT('Ctrl Pts',(-0.737541863000055,12.2,-3.95519093900001));
#326084=CARTESIAN_POINT('Ctrl Pts',(-0.737541863000055,5.2,-3.95519093900001));
#326085=CARTESIAN_POINT('Ctrl Pts',(-0.737541863000055,2.2,-3.95519093900001));
#326086=CARTESIAN_POINT('Ctrl Pts',(-0.737354914000056,12.2,-3.95459762800002));
#326087=CARTESIAN_POINT('Ctrl Pts',(-0.737354914000056,5.2,-3.95459762800002));
#326088=CARTESIAN_POINT('Ctrl Pts',(-0.737354914000056,2.2,-3.95459762800002));
#326089=CARTESIAN_POINT('Ctrl Pts',(-0.737170572000055,12.2,-3.95400995800001));
#326090=CARTESIAN_POINT('Ctrl Pts',(-0.737170572000055,5.2,-3.95400995800001));
#326091=CARTESIAN_POINT('Ctrl Pts',(-0.737170572000055,2.2,-3.95400995800001));
#326092=CARTESIAN_POINT('Ctrl Pts',(-0.736988825000056,12.2,-3.95342795000001));
#326093=CARTESIAN_POINT('Ctrl Pts',(-0.736988825000056,5.2,-3.95342795000001));
#326094=CARTESIAN_POINT('Ctrl Pts',(-0.736988825000056,2.2,-3.95342795000001));
#326095=CARTESIAN_POINT('Ctrl Pts',(-0.736809662000055,12.2,-3.95285161700001));
#326096=CARTESIAN_POINT('Ctrl Pts',(-0.736809662000055,5.2,-3.95285161700001));
#326097=CARTESIAN_POINT('Ctrl Pts',(-0.736809662000055,2.2,-3.95285161700001));
#326098=CARTESIAN_POINT('Ctrl Pts',(-0.736633073000055,12.2,-3.95228097900001));
#326099=CARTESIAN_POINT('Ctrl Pts',(-0.736633073000055,5.2,-3.95228097900001));
#326100=CARTESIAN_POINT('Ctrl Pts',(-0.736633073000055,2.2,-3.95228097900001));
#326101=CARTESIAN_POINT('Ctrl Pts',(-0.736459048000055,12.2,-3.95171605100002));
#326102=CARTESIAN_POINT('Ctrl Pts',(-0.736459048000055,5.2,-3.95171605100002));
#326103=CARTESIAN_POINT('Ctrl Pts',(-0.736459048000055,2.2,-3.95171605100002));
#326104=CARTESIAN_POINT('Ctrl Pts',(-0.736287574000055,12.2,-3.95115685200001));
#326105=CARTESIAN_POINT('Ctrl Pts',(-0.736287574000055,5.2,-3.95115685200001));
#326106=CARTESIAN_POINT('Ctrl Pts',(-0.736287574000055,2.2,-3.95115685200001));
#326107=CARTESIAN_POINT('Ctrl Pts',(-0.736118641000055,12.2,-3.95060339600001));
#326108=CARTESIAN_POINT('Ctrl Pts',(-0.736118641000055,5.2,-3.95060339600001));
#326109=CARTESIAN_POINT('Ctrl Pts',(-0.736118641000055,2.2,-3.95060339600001));
#326110=CARTESIAN_POINT('Ctrl Pts',(-0.735952238000056,12.2,-3.95005570300001));
#326111=CARTESIAN_POINT('Ctrl Pts',(-0.735952238000056,5.2,-3.95005570300001));
#326112=CARTESIAN_POINT('Ctrl Pts',(-0.735952238000056,2.2,-3.95005570300001));
#326113=CARTESIAN_POINT('Ctrl Pts',(-0.735788355000055,12.2,-3.94951378800001));
#326114=CARTESIAN_POINT('Ctrl Pts',(-0.735788355000055,5.2,-3.94951378800001));
#326115=CARTESIAN_POINT('Ctrl Pts',(-0.735788355000055,2.2,-3.94951378800001));
#326116=CARTESIAN_POINT('Ctrl Pts',(-0.735626978000056,12.2,-3.94897766900002));
#326117=CARTESIAN_POINT('Ctrl Pts',(-0.735626978000056,5.2,-3.94897766900002));
#326118=CARTESIAN_POINT('Ctrl Pts',(-0.735626978000056,2.2,-3.94897766900002));
#326119=CARTESIAN_POINT('Ctrl Pts',(-0.735468096000057,12.2,-3.94844736400001));
#326120=CARTESIAN_POINT('Ctrl Pts',(-0.735468096000057,5.2,-3.94844736400001));
#326121=CARTESIAN_POINT('Ctrl Pts',(-0.735468096000057,2.2,-3.94844736400001));
#326122=CARTESIAN_POINT('Ctrl Pts',(-0.735311701000055,12.2,-3.94792288800002));
#326123=CARTESIAN_POINT('Ctrl Pts',(-0.735311701000055,5.2,-3.94792288800002));
#326124=CARTESIAN_POINT('Ctrl Pts',(-0.735311701000055,2.2,-3.94792288800002));
#326125=CARTESIAN_POINT('Ctrl Pts',(-0.735157778000056,12.2,-3.94740426000002));
#326126=CARTESIAN_POINT('Ctrl Pts',(-0.735157778000056,5.2,-3.94740426000002));
#326127=CARTESIAN_POINT('Ctrl Pts',(-0.735157778000056,2.2,-3.94740426000002));
#326128=CARTESIAN_POINT('Ctrl Pts',(-0.735006318000057,12.2,-3.94689149700001));
#326129=CARTESIAN_POINT('Ctrl Pts',(-0.735006318000057,5.2,-3.94689149700001));
#326130=CARTESIAN_POINT('Ctrl Pts',(-0.735006318000057,2.2,-3.94689149700001));
#326131=CARTESIAN_POINT('Ctrl Pts',(-0.734857308000055,12.2,-3.94638461600001));
#326132=CARTESIAN_POINT('Ctrl Pts',(-0.734857308000055,5.2,-3.94638461600001));
#326133=CARTESIAN_POINT('Ctrl Pts',(-0.734857308000055,2.2,-3.94638461600001));
#326134=CARTESIAN_POINT('Ctrl Pts',(-0.734710738000055,12.2,-3.94588363500001));
#326135=CARTESIAN_POINT('Ctrl Pts',(-0.734710738000055,5.2,-3.94588363500001));
#326136=CARTESIAN_POINT('Ctrl Pts',(-0.734710738000055,2.2,-3.94588363500001));
#326137=CARTESIAN_POINT('Ctrl Pts',(-0.734566594000056,12.2,-3.94538857000001));
#326138=CARTESIAN_POINT('Ctrl Pts',(-0.734566594000056,5.2,-3.94538857000001));
#326139=CARTESIAN_POINT('Ctrl Pts',(-0.734566594000056,2.2,-3.94538857000001));
#326140=CARTESIAN_POINT('Ctrl Pts',(-0.734424867000056,12.2,-3.94489944000001));
#326141=CARTESIAN_POINT('Ctrl Pts',(-0.734424867000056,5.2,-3.94489944000001));
#326142=CARTESIAN_POINT('Ctrl Pts',(-0.734424867000056,2.2,-3.94489944000001));
#326143=CARTESIAN_POINT('Ctrl Pts',(-0.734285544000055,12.2,-3.94441626200001));
#326144=CARTESIAN_POINT('Ctrl Pts',(-0.734285544000055,5.2,-3.94441626200001));
#326145=CARTESIAN_POINT('Ctrl Pts',(-0.734285544000055,2.2,-3.94441626200001));
#326146=CARTESIAN_POINT('Ctrl Pts',(-0.734148613000055,12.2,-3.94393905300001));
#326147=CARTESIAN_POINT('Ctrl Pts',(-0.734148613000055,5.2,-3.94393905300001));
#326148=CARTESIAN_POINT('Ctrl Pts',(-0.734148613000055,2.2,-3.94393905300001));
#326149=CARTESIAN_POINT('Ctrl Pts',(-0.734014063000057,12.2,-3.94346783100001));
#326150=CARTESIAN_POINT('Ctrl Pts',(-0.734014063000057,5.2,-3.94346783100001));
#326151=CARTESIAN_POINT('Ctrl Pts',(-0.734014063000057,2.2,-3.94346783100001));
#326152=CARTESIAN_POINT('Ctrl Pts',(-0.733881881000055,12.2,-3.94300261400002));
#326153=CARTESIAN_POINT('Ctrl Pts',(-0.733881881000055,5.2,-3.94300261400002));
#326154=CARTESIAN_POINT('Ctrl Pts',(-0.733881881000055,2.2,-3.94300261400002));
#326155=CARTESIAN_POINT('Ctrl Pts',(-0.733752055000056,12.2,-3.94254341900002));
#326156=CARTESIAN_POINT('Ctrl Pts',(-0.733752055000056,5.2,-3.94254341900002));
#326157=CARTESIAN_POINT('Ctrl Pts',(-0.733752055000056,2.2,-3.94254341900002));
#326158=CARTESIAN_POINT('Ctrl Pts',(-0.733624575000055,12.2,-3.94209026300001));
#326159=CARTESIAN_POINT('Ctrl Pts',(-0.733624575000055,5.2,-3.94209026300001));
#326160=CARTESIAN_POINT('Ctrl Pts',(-0.733624575000055,2.2,-3.94209026300001));
#326161=CARTESIAN_POINT('Ctrl Pts',(-0.733499428000056,12.2,-3.94164316600001));
#326162=CARTESIAN_POINT('Ctrl Pts',(-0.733499428000056,5.2,-3.94164316600001));
#326163=CARTESIAN_POINT('Ctrl Pts',(-0.733499428000056,2.2,-3.94164316600001));
#326164=CARTESIAN_POINT('Ctrl Pts',(-0.733376600000056,12.2,-3.94120214300001));
#326165=CARTESIAN_POINT('Ctrl Pts',(-0.733376600000056,5.2,-3.94120214300001));
#326166=CARTESIAN_POINT('Ctrl Pts',(-0.733376600000056,2.2,-3.94120214300001));
#326167=CARTESIAN_POINT('Ctrl Pts',(-0.733256082000056,12.2,-3.94076721300001));
#326168=CARTESIAN_POINT('Ctrl Pts',(-0.733256082000056,5.2,-3.94076721300001));
#326169=CARTESIAN_POINT('Ctrl Pts',(-0.733256082000056,2.2,-3.94076721300001));
#326170=CARTESIAN_POINT('Ctrl Pts',(-0.733137859000056,12.2,-3.94033839600001));
#326171=CARTESIAN_POINT('Ctrl Pts',(-0.733137859000056,5.2,-3.94033839600001));
#326172=CARTESIAN_POINT('Ctrl Pts',(-0.733137859000056,2.2,-3.94033839600001));
#326173=CARTESIAN_POINT('Ctrl Pts',(-0.733021920000055,12.2,-3.93991570600001));
#326174=CARTESIAN_POINT('Ctrl Pts',(-0.733021920000055,5.2,-3.93991570600001));
#326175=CARTESIAN_POINT('Ctrl Pts',(-0.733021920000055,2.2,-3.93991570600001));
#326176=CARTESIAN_POINT('Ctrl Pts',(-0.732908254000056,12.2,-3.93949916500001));
#326177=CARTESIAN_POINT('Ctrl Pts',(-0.732908254000056,5.2,-3.93949916500001));
#326178=CARTESIAN_POINT('Ctrl Pts',(-0.732908254000056,2.2,-3.93949916500001));
#326179=CARTESIAN_POINT('Ctrl Pts',(-0.732796846000056,12.2,-3.93908878700001));
#326180=CARTESIAN_POINT('Ctrl Pts',(-0.732796846000056,5.2,-3.93908878700001));
#326181=CARTESIAN_POINT('Ctrl Pts',(-0.732796846000056,2.2,-3.93908878700001));
#326182=CARTESIAN_POINT('Ctrl Pts',(-0.732687684000056,12.2,-3.93868459300001));
#326183=CARTESIAN_POINT('Ctrl Pts',(-0.732687684000056,5.2,-3.93868459300001));
#326184=CARTESIAN_POINT('Ctrl Pts',(-0.732687684000056,2.2,-3.93868459300001));
#326185=CARTESIAN_POINT('Ctrl Pts',(-0.732580758000055,12.2,-3.93828659900001));
#326186=CARTESIAN_POINT('Ctrl Pts',(-0.732580758000055,5.2,-3.93828659900001));
#326187=CARTESIAN_POINT('Ctrl Pts',(-0.732580758000055,2.2,-3.93828659900001));
#326188=CARTESIAN_POINT('Ctrl Pts',(-0.732476052000056,12.2,-3.93789482400001));
#326189=CARTESIAN_POINT('Ctrl Pts',(-0.732476052000056,5.2,-3.93789482400001));
#326190=CARTESIAN_POINT('Ctrl Pts',(-0.732476052000056,2.2,-3.93789482400001));
#326191=CARTESIAN_POINT('Ctrl Pts',(-0.732373555000055,12.2,-3.93750928800001));
#326192=CARTESIAN_POINT('Ctrl Pts',(-0.732373555000055,5.2,-3.93750928800001));
#326193=CARTESIAN_POINT('Ctrl Pts',(-0.732373555000055,2.2,-3.93750928800001));
#326194=CARTESIAN_POINT('Ctrl Pts',(-0.732273255000055,12.2,-3.93713000600002));
#326195=CARTESIAN_POINT('Ctrl Pts',(-0.732273255000055,5.2,-3.93713000600002));
#326196=CARTESIAN_POINT('Ctrl Pts',(-0.732273255000055,2.2,-3.93713000600002));
#326197=CARTESIAN_POINT('Ctrl Pts',(-0.732175138000055,12.2,-3.93675699800001));
#326198=CARTESIAN_POINT('Ctrl Pts',(-0.732175138000055,5.2,-3.93675699800001));
#326199=CARTESIAN_POINT('Ctrl Pts',(-0.732175138000055,2.2,-3.93675699800001));
#326200=CARTESIAN_POINT('Ctrl Pts',(-0.732079191000056,12.2,-3.93639028200001));
#326201=CARTESIAN_POINT('Ctrl Pts',(-0.732079191000056,5.2,-3.93639028200001));
#326202=CARTESIAN_POINT('Ctrl Pts',(-0.732079191000056,2.2,-3.93639028200001));
#326203=CARTESIAN_POINT('Ctrl Pts',(-0.731985402000056,12.2,-3.93602987700001));
#326204=CARTESIAN_POINT('Ctrl Pts',(-0.731985402000056,5.2,-3.93602987700001));
#326205=CARTESIAN_POINT('Ctrl Pts',(-0.731985402000056,2.2,-3.93602987700001));
#326206=CARTESIAN_POINT('Ctrl Pts',(-0.731893758000056,12.2,-3.93567580100001));
#326207=CARTESIAN_POINT('Ctrl Pts',(-0.731893758000056,5.2,-3.93567580100001));
#326208=CARTESIAN_POINT('Ctrl Pts',(-0.731893758000056,2.2,-3.93567580100001));
#326209=CARTESIAN_POINT('Ctrl Pts',(-0.731804245000056,12.2,-3.93532807100001));
#326210=CARTESIAN_POINT('Ctrl Pts',(-0.731804245000056,5.2,-3.93532807100001));
#326211=CARTESIAN_POINT('Ctrl Pts',(-0.731804245000056,2.2,-3.93532807100001));
#326212=CARTESIAN_POINT('Ctrl Pts',(-0.731716851000056,12.2,-3.93498670700001));
#326213=CARTESIAN_POINT('Ctrl Pts',(-0.731716851000056,5.2,-3.93498670700001));
#326214=CARTESIAN_POINT('Ctrl Pts',(-0.731716851000056,2.2,-3.93498670700001));
#326215=CARTESIAN_POINT('Ctrl Pts',(-0.731631562000056,12.2,-3.93465172700001));
#326216=CARTESIAN_POINT('Ctrl Pts',(-0.731631562000056,5.2,-3.93465172700001));
#326217=CARTESIAN_POINT('Ctrl Pts',(-0.731631562000056,2.2,-3.93465172700001));
#326218=CARTESIAN_POINT('Ctrl Pts',(-0.731548366000055,12.2,-3.93432315100001));
#326219=CARTESIAN_POINT('Ctrl Pts',(-0.731548366000055,5.2,-3.93432315100001));
#326220=CARTESIAN_POINT('Ctrl Pts',(-0.731548366000055,2.2,-3.93432315100001));
#326221=CARTESIAN_POINT('Ctrl Pts',(-0.731467248000056,12.2,-3.93400099600001));
#326222=CARTESIAN_POINT('Ctrl Pts',(-0.731467248000056,5.2,-3.93400099600001));
#326223=CARTESIAN_POINT('Ctrl Pts',(-0.731467248000056,2.2,-3.93400099600001));
#326224=CARTESIAN_POINT('Ctrl Pts',(-0.731388196000056,12.2,-3.93368528000002));
#326225=CARTESIAN_POINT('Ctrl Pts',(-0.731388196000056,5.2,-3.93368528000002));
#326226=CARTESIAN_POINT('Ctrl Pts',(-0.731388196000056,2.2,-3.93368528000002));
#326227=CARTESIAN_POINT('Ctrl Pts',(-0.731311196000056,12.2,-3.93337602400001));
#326228=CARTESIAN_POINT('Ctrl Pts',(-0.731311196000056,5.2,-3.93337602400001));
#326229=CARTESIAN_POINT('Ctrl Pts',(-0.731311196000056,2.2,-3.93337602400001));
#326230=CARTESIAN_POINT('Ctrl Pts',(-0.731236235000056,12.2,-3.93307324500002));
#326231=CARTESIAN_POINT('Ctrl Pts',(-0.731236235000056,5.2,-3.93307324500002));
#326232=CARTESIAN_POINT('Ctrl Pts',(-0.731236235000056,2.2,-3.93307324500002));
#326233=CARTESIAN_POINT('Ctrl Pts',(-0.731163299000055,12.2,-3.93277696300002));
#326234=CARTESIAN_POINT('Ctrl Pts',(-0.731163299000055,5.2,-3.93277696300002));
#326235=CARTESIAN_POINT('Ctrl Pts',(-0.731163299000055,2.2,-3.93277696300002));
#326236=CARTESIAN_POINT('Ctrl Pts',(-0.731092374000056,12.2,-3.93248719600002));
#326237=CARTESIAN_POINT('Ctrl Pts',(-0.731092374000056,5.2,-3.93248719600002));
#326238=CARTESIAN_POINT('Ctrl Pts',(-0.731092374000056,2.2,-3.93248719600002));
#326239=CARTESIAN_POINT('Ctrl Pts',(-0.731023446000056,12.2,-3.93220396300002));
#326240=CARTESIAN_POINT('Ctrl Pts',(-0.731023446000056,5.2,-3.93220396300002));
#326241=CARTESIAN_POINT('Ctrl Pts',(-0.731023446000056,2.2,-3.93220396300002));
#326242=CARTESIAN_POINT('Ctrl Pts',(-0.730956503000056,12.2,-3.93192728300002));
#326243=CARTESIAN_POINT('Ctrl Pts',(-0.730956503000056,5.2,-3.93192728300002));
#326244=CARTESIAN_POINT('Ctrl Pts',(-0.730956503000056,2.2,-3.93192728300002));
#326245=CARTESIAN_POINT('Ctrl Pts',(-0.730891530000056,12.2,-3.93165717500001));
#326246=CARTESIAN_POINT('Ctrl Pts',(-0.730891530000056,5.2,-3.93165717500001));
#326247=CARTESIAN_POINT('Ctrl Pts',(-0.730891530000056,2.2,-3.93165717500001));
#326248=CARTESIAN_POINT('Ctrl Pts',(-0.730828514000056,12.2,-3.93139365900002));
#326249=CARTESIAN_POINT('Ctrl Pts',(-0.730828514000056,5.2,-3.93139365900002));
#326250=CARTESIAN_POINT('Ctrl Pts',(-0.730828514000056,2.2,-3.93139365900002));
#326251=CARTESIAN_POINT('Ctrl Pts',(-0.730767439000056,12.2,-3.93113675200001));
#326252=CARTESIAN_POINT('Ctrl Pts',(-0.730767439000056,5.2,-3.93113675200001));
#326253=CARTESIAN_POINT('Ctrl Pts',(-0.730767439000056,2.2,-3.93113675200001));
#326254=CARTESIAN_POINT('Ctrl Pts',(-0.730708292000056,12.2,-3.93088647600001));
#326255=CARTESIAN_POINT('Ctrl Pts',(-0.730708292000056,5.2,-3.93088647600001));
#326256=CARTESIAN_POINT('Ctrl Pts',(-0.730708292000056,2.2,-3.93088647600001));
#326257=CARTESIAN_POINT('Ctrl Pts',(-0.730651060000056,12.2,-3.93064284800001));
#326258=CARTESIAN_POINT('Ctrl Pts',(-0.730651060000056,5.2,-3.93064284800001));
#326259=CARTESIAN_POINT('Ctrl Pts',(-0.730651060000056,2.2,-3.93064284800001));
#326260=CARTESIAN_POINT('Ctrl Pts',(-0.730595727000055,12.2,-3.93040588800002));
#326261=CARTESIAN_POINT('Ctrl Pts',(-0.730595727000055,5.2,-3.93040588800002));
#326262=CARTESIAN_POINT('Ctrl Pts',(-0.730595727000055,2.2,-3.93040588800002));
#326263=CARTESIAN_POINT('Ctrl Pts',(-0.730542281000056,12.2,-3.93017561500002));
#326264=CARTESIAN_POINT('Ctrl Pts',(-0.730542281000056,5.2,-3.93017561500002));
#326265=CARTESIAN_POINT('Ctrl Pts',(-0.730542281000056,2.2,-3.93017561500002));
#326266=CARTESIAN_POINT('Ctrl Pts',(-0.730490706000057,12.2,-3.92995204900001));
#326267=CARTESIAN_POINT('Ctrl Pts',(-0.730490706000057,5.2,-3.92995204900001));
#326268=CARTESIAN_POINT('Ctrl Pts',(-0.730490706000057,2.2,-3.92995204900001));
#326269=CARTESIAN_POINT('Ctrl Pts',(-0.730440988000056,12.2,-3.92973520900001));
#326270=CARTESIAN_POINT('Ctrl Pts',(-0.730440988000056,5.2,-3.92973520900001));
#326271=CARTESIAN_POINT('Ctrl Pts',(-0.730440988000056,2.2,-3.92973520900001));
#326272=CARTESIAN_POINT('Ctrl Pts',(-0.730393113000056,12.2,-3.92952511400001));
#326273=CARTESIAN_POINT('Ctrl Pts',(-0.730393113000056,5.2,-3.92952511400001));
#326274=CARTESIAN_POINT('Ctrl Pts',(-0.730393113000056,2.2,-3.92952511400001));
#326275=CARTESIAN_POINT('Ctrl Pts',(-0.730347066000056,12.2,-3.92932178500002));
#326276=CARTESIAN_POINT('Ctrl Pts',(-0.730347066000056,5.2,-3.92932178500002));
#326277=CARTESIAN_POINT('Ctrl Pts',(-0.730347066000056,2.2,-3.92932178500002));
#326278=CARTESIAN_POINT('Ctrl Pts',(-0.730302831000056,12.2,-3.92912523900002));
#326279=CARTESIAN_POINT('Ctrl Pts',(-0.730302831000056,5.2,-3.92912523900002));
#326280=CARTESIAN_POINT('Ctrl Pts',(-0.730302831000056,2.2,-3.92912523900002));
#326281=CARTESIAN_POINT('Ctrl Pts',(-0.730260396000055,12.2,-3.92893549900001));
#326282=CARTESIAN_POINT('Ctrl Pts',(-0.730260396000055,5.2,-3.92893549900001));
#326283=CARTESIAN_POINT('Ctrl Pts',(-0.730260396000055,2.2,-3.92893549900001));
#326284=CARTESIAN_POINT('Ctrl Pts',(-0.730219745000056,12.2,-3.92875258300001));
#326285=CARTESIAN_POINT('Ctrl Pts',(-0.730219745000056,5.2,-3.92875258300001));
#326286=CARTESIAN_POINT('Ctrl Pts',(-0.730219745000056,2.2,-3.92875258300001));
#326287=CARTESIAN_POINT('Ctrl Pts',(-0.730180862000056,12.2,-3.92857651100002));
#326288=CARTESIAN_POINT('Ctrl Pts',(-0.730180862000056,5.2,-3.92857651100002));
#326289=CARTESIAN_POINT('Ctrl Pts',(-0.730180862000056,2.2,-3.92857651100002));
#326290=CARTESIAN_POINT('Ctrl Pts',(-0.730143733000055,12.2,-3.92840730200001));
#326291=CARTESIAN_POINT('Ctrl Pts',(-0.730143733000055,5.2,-3.92840730200001));
#326292=CARTESIAN_POINT('Ctrl Pts',(-0.730143733000055,2.2,-3.92840730200001));
#326293=CARTESIAN_POINT('Ctrl Pts',(-0.730108344000057,12.2,-3.92824497500001));
#326294=CARTESIAN_POINT('Ctrl Pts',(-0.730108344000057,5.2,-3.92824497500001));
#326295=CARTESIAN_POINT('Ctrl Pts',(-0.730108344000057,2.2,-3.92824497500001));
#326296=CARTESIAN_POINT('Ctrl Pts',(-0.730074682000056,12.2,-3.92808955100001));
#326297=CARTESIAN_POINT('Ctrl Pts',(-0.730074682000056,5.2,-3.92808955100001));
#326298=CARTESIAN_POINT('Ctrl Pts',(-0.730074682000056,2.2,-3.92808955100001));
#326299=CARTESIAN_POINT('Ctrl Pts',(-0.730042727000055,12.2,-3.92794104900001));
#326300=CARTESIAN_POINT('Ctrl Pts',(-0.730042727000055,5.2,-3.92794104900001));
#326301=CARTESIAN_POINT('Ctrl Pts',(-0.730042727000055,2.2,-3.92794104900001));
#326302=CARTESIAN_POINT('Ctrl Pts',(-0.730012467000056,12.2,-3.92779949100001));
#326303=CARTESIAN_POINT('Ctrl Pts',(-0.730012467000056,5.2,-3.92779949100001));
#326304=CARTESIAN_POINT('Ctrl Pts',(-0.730012467000056,2.2,-3.92779949100001));
#326305=CARTESIAN_POINT('Ctrl Pts',(-0.729983883000056,12.2,-3.92766489800001));
#326306=CARTESIAN_POINT('Ctrl Pts',(-0.729983883000056,5.2,-3.92766489800001));
#326307=CARTESIAN_POINT('Ctrl Pts',(-0.729983883000056,2.2,-3.92766489800001));
#326308=CARTESIAN_POINT('Ctrl Pts',(-0.729956962000056,12.2,-3.92753729100002));
#326309=CARTESIAN_POINT('Ctrl Pts',(-0.729956962000056,5.2,-3.92753729100002));
#326310=CARTESIAN_POINT('Ctrl Pts',(-0.729956962000056,2.2,-3.92753729100002));
#326311=CARTESIAN_POINT('Ctrl Pts',(-0.729931687000055,12.2,-3.92741668800001));
#326312=CARTESIAN_POINT('Ctrl Pts',(-0.729931687000055,5.2,-3.92741668800001));
#326313=CARTESIAN_POINT('Ctrl Pts',(-0.729931687000055,2.2,-3.92741668800001));
#326314=CARTESIAN_POINT('Ctrl Pts',(-0.729908045000055,12.2,-3.92730311000001));
#326315=CARTESIAN_POINT('Ctrl Pts',(-0.729908045000055,5.2,-3.92730311000001));
#326316=CARTESIAN_POINT('Ctrl Pts',(-0.729908045000055,2.2,-3.92730311000001));
#326317=CARTESIAN_POINT('Ctrl Pts',(-0.729886021000056,12.2,-3.92719657100002));
#326318=CARTESIAN_POINT('Ctrl Pts',(-0.729886021000056,5.2,-3.92719657100002));
#326319=CARTESIAN_POINT('Ctrl Pts',(-0.729886021000056,2.2,-3.92719657100002));
#326320=CARTESIAN_POINT('Ctrl Pts',(-0.729865602000055,12.2,-3.92709709300001));
#326321=CARTESIAN_POINT('Ctrl Pts',(-0.729865602000055,5.2,-3.92709709300001));
#326322=CARTESIAN_POINT('Ctrl Pts',(-0.729865602000055,2.2,-3.92709709300001));
#326323=CARTESIAN_POINT('Ctrl Pts',(-0.729846772000055,12.2,-3.92700469600001));
#326324=CARTESIAN_POINT('Ctrl Pts',(-0.729846772000055,5.2,-3.92700469600001));
#326325=CARTESIAN_POINT('Ctrl Pts',(-0.729846772000055,2.2,-3.92700469600001));
#326326=CARTESIAN_POINT('Ctrl Pts',(-0.729829512000055,12.2,-3.92691940300002));
#326327=CARTESIAN_POINT('Ctrl Pts',(-0.729829512000055,5.2,-3.92691940300002));
#326328=CARTESIAN_POINT('Ctrl Pts',(-0.729829512000055,2.2,-3.92691940300002));
#326329=CARTESIAN_POINT('Ctrl Pts',(-0.729813802000056,12.2,-3.92684124000001));
#326330=CARTESIAN_POINT('Ctrl Pts',(-0.729813802000056,5.2,-3.92684124000001));
#326331=CARTESIAN_POINT('Ctrl Pts',(-0.729813802000056,2.2,-3.92684124000001));
#326332=CARTESIAN_POINT('Ctrl Pts',(-0.729799621000057,12.2,-3.92677023400001));
#326333=CARTESIAN_POINT('Ctrl Pts',(-0.729799621000057,5.2,-3.92677023400001));
#326334=CARTESIAN_POINT('Ctrl Pts',(-0.729799621000057,2.2,-3.92677023400001));
#326335=CARTESIAN_POINT('Ctrl Pts',(-0.729786954000057,12.2,-3.92670640600001));
#326336=CARTESIAN_POINT('Ctrl Pts',(-0.729786954000057,5.2,-3.92670640600001));
#326337=CARTESIAN_POINT('Ctrl Pts',(-0.729786954000057,2.2,-3.92670640600001));
#326338=CARTESIAN_POINT('Ctrl Pts',(-0.729775786000056,12.2,-3.92664977400001));
#326339=CARTESIAN_POINT('Ctrl Pts',(-0.729775786000056,5.2,-3.92664977400001));
#326340=CARTESIAN_POINT('Ctrl Pts',(-0.729775786000056,2.2,-3.92664977400001));
#326341=CARTESIAN_POINT('Ctrl Pts',(-0.729765073038284,12.2,-3.92659505674791));
#326342=CARTESIAN_POINT('Ctrl Pts',(-0.729765073038284,5.2,-3.92659505674791));
#326343=CARTESIAN_POINT('Ctrl Pts',(-0.729765073038284,2.2,-3.92659505674791));
#326344=CARTESIAN_POINT('Ctrl Pts',(-0.729757824757594,12.2,-3.92655763816102));
#326345=CARTESIAN_POINT('Ctrl Pts',(-0.729757824757594,5.2,-3.92655763816102));
#326346=CARTESIAN_POINT('Ctrl Pts',(-0.729757824757594,2.2,-3.92655763816102));
#326347=CARTESIAN_POINT('Ctrl Pts',(-0.729753103670104,12.2,-3.92653297916544));
#326348=CARTESIAN_POINT('Ctrl Pts',(-0.729753103670104,5.2,-3.92653297916544));
#326349=CARTESIAN_POINT('Ctrl Pts',(-0.729753103670104,2.2,-3.92653297916544));
#326350=CARTESIAN_POINT('Ctrl Pts',(-0.729750197519061,12.2,-3.92651761063945));
#326351=CARTESIAN_POINT('Ctrl Pts',(-0.729750197519061,5.2,-3.92651761063945));
#326352=CARTESIAN_POINT('Ctrl Pts',(-0.729750197519061,2.2,-3.92651761063945));
#326353=CARTESIAN_POINT('Ctrl Pts',(-0.729748397000056,12.2,-3.92650812200001));
#326354=CARTESIAN_POINT('Ctrl Pts',(-0.729748397000056,5.2,-3.92650812200001));
#326355=CARTESIAN_POINT('Ctrl Pts',(-0.729748397000056,2.2,-3.92650812200001));
#326356=CARTESIAN_POINT('',(-0.729748200000057,2.7,-3.92650816000002));
#326357=CARTESIAN_POINT('',(-0.729748200000057,12.2,-3.92650816000002));
#326358=CARTESIAN_POINT('Ctrl Pts',(-1.20083826600006,2.7,-4.59570315100001));
#326359=CARTESIAN_POINT('Ctrl Pts',(-0.99159571956929,2.7,-4.40343391106789));
#326360=CARTESIAN_POINT('Ctrl Pts',(-0.884170970210799,2.69999999999769,
-4.24256418392735));
#326361=CARTESIAN_POINT('Ctrl Pts',(-0.752547076732114,2.69999999999769,
-4.02218548569631));
#326362=CARTESIAN_POINT('Ctrl Pts',(-0.732215363126463,2.69999999999824,
-3.93874877259718));
#326363=CARTESIAN_POINT('Ctrl Pts',(-0.729801785768923,2.69999999999824,
-3.92678179258076));
#326364=CARTESIAN_POINT('Ctrl Pts',(-0.729774387723865,2.7,-3.92664509173279));
#326365=CARTESIAN_POINT('Ctrl Pts',(-0.729748397000056,2.7,-3.92650812200001));
#326366=CARTESIAN_POINT('Origin',(-0.729738823000057,15.2,-3.92645770700002));
#326367=CARTESIAN_POINT('',(-0.662370095000057,2.7,-3.56397122000002));
#326368=CARTESIAN_POINT('',(-0.662370095000057,2.2,-3.56397122000002));
#326369=CARTESIAN_POINT('',(-0.364869411202236,2.7,-1.96322885355537));
#326370=CARTESIAN_POINT('Origin',(-5.66300478732629E-14,15.2,-1.77635683940025E-14));
#326371=CARTESIAN_POINT('',(-0.104256396000055,2.7,-3.62350046200001));
#326372=CARTESIAN_POINT('',(-0.104256396000055,12.2,-3.62350046200001));
#326373=CARTESIAN_POINT('Origin',(-5.66300478732629E-14,2.7,-1.92943768261394E-14));
#326374=CARTESIAN_POINT('Origin',(-5.66300478732629E-14,15.2,-1.77635683940025E-14));
#326375=CARTESIAN_POINT('',(-0.114861152000056,2.7,-3.99207578300001));
#326376=CARTESIAN_POINT('',(-0.114861152000056,12.2,-3.99207578300001));
#326377=CARTESIAN_POINT('',(-5.66071634909361E-14,2.7,-1.84990148774464E-14));
#326378=CARTESIAN_POINT('Ctrl Pts',(-0.114861015000055,12.2,-3.99207578600001));
#326379=CARTESIAN_POINT('Ctrl Pts',(-0.114861015000055,5.2,-3.99207578600001));
#326380=CARTESIAN_POINT('Ctrl Pts',(-0.114861015000055,2.2,-3.99207578600001));
#326381=CARTESIAN_POINT('Ctrl Pts',(-0.114861185985858,12.2,-3.99208262642898));
#326382=CARTESIAN_POINT('Ctrl Pts',(-0.114861185985858,5.2,-3.99208262642898));
#326383=CARTESIAN_POINT('Ctrl Pts',(-0.114861185985858,2.2,-3.99208262642898));
#326384=CARTESIAN_POINT('Ctrl Pts',(-0.114861514799149,12.2,-3.99209585439877));
#326385=CARTESIAN_POINT('Ctrl Pts',(-0.114861514799149,5.2,-3.99209585439877));
#326386=CARTESIAN_POINT('Ctrl Pts',(-0.114861514799149,2.2,-3.99209585439877));
#326387=CARTESIAN_POINT('Ctrl Pts',(-0.11486200797077,12.2,-3.99211547674708));
#326388=CARTESIAN_POINT('Ctrl Pts',(-0.11486200797077,5.2,-3.99211547674708));
#326389=CARTESIAN_POINT('Ctrl Pts',(-0.11486200797077,2.2,-3.99211547674708));
#326390=CARTESIAN_POINT('Ctrl Pts',(-0.114862630472375,12.2,-3.99214150063735));
#326391=CARTESIAN_POINT('Ctrl Pts',(-0.114862630472375,5.2,-3.99214150063735));
#326392=CARTESIAN_POINT('Ctrl Pts',(-0.114862630472375,2.2,-3.99214150063735));
#326393=CARTESIAN_POINT('Ctrl Pts',(-0.114863582000057,12.2,-3.99218677200002));
#326394=CARTESIAN_POINT('Ctrl Pts',(-0.114863582000057,5.2,-3.99218677200002));
#326395=CARTESIAN_POINT('Ctrl Pts',(-0.114863582000057,2.2,-3.99218677200002));
#326396=CARTESIAN_POINT('Ctrl Pts',(-0.114864547000056,12.2,-3.99223712800001));
#326397=CARTESIAN_POINT('Ctrl Pts',(-0.114864547000056,5.2,-3.99223712800001));
#326398=CARTESIAN_POINT('Ctrl Pts',(-0.114864547000056,2.2,-3.99223712800001));
#326399=CARTESIAN_POINT('Ctrl Pts',(-0.114865575000056,12.2,-3.99229484100001));
#326400=CARTESIAN_POINT('Ctrl Pts',(-0.114865575000056,5.2,-3.99229484100001));
#326401=CARTESIAN_POINT('Ctrl Pts',(-0.114865575000056,2.2,-3.99229484100001));
#326402=CARTESIAN_POINT('Ctrl Pts',(-0.114866656000056,12.2,-3.99235990500001));
#326403=CARTESIAN_POINT('Ctrl Pts',(-0.114866656000056,5.2,-3.99235990500001));
#326404=CARTESIAN_POINT('Ctrl Pts',(-0.114866656000056,2.2,-3.99235990500001));
#326405=CARTESIAN_POINT('Ctrl Pts',(-0.114867771000055,12.2,-3.99243230500002));
#326406=CARTESIAN_POINT('Ctrl Pts',(-0.114867771000055,5.2,-3.99243230500002));
#326407=CARTESIAN_POINT('Ctrl Pts',(-0.114867771000055,2.2,-3.99243230500002));
#326408=CARTESIAN_POINT('Ctrl Pts',(-0.114868901000056,12.2,-3.99251202200002));
#326409=CARTESIAN_POINT('Ctrl Pts',(-0.114868901000056,5.2,-3.99251202200002));
#326410=CARTESIAN_POINT('Ctrl Pts',(-0.114868901000056,2.2,-3.99251202200002));
#326411=CARTESIAN_POINT('Ctrl Pts',(-0.114870019000056,12.2,-3.99259903700001));
#326412=CARTESIAN_POINT('Ctrl Pts',(-0.114870019000056,5.2,-3.99259903700001));
#326413=CARTESIAN_POINT('Ctrl Pts',(-0.114870019000056,2.2,-3.99259903700001));
#326414=CARTESIAN_POINT('Ctrl Pts',(-0.114871102000055,12.2,-3.99269332800001));
#326415=CARTESIAN_POINT('Ctrl Pts',(-0.114871102000055,5.2,-3.99269332800001));
#326416=CARTESIAN_POINT('Ctrl Pts',(-0.114871102000055,2.2,-3.99269332800001));
#326417=CARTESIAN_POINT('Ctrl Pts',(-0.114872125000056,12.2,-3.99279487500001));
#326418=CARTESIAN_POINT('Ctrl Pts',(-0.114872125000056,5.2,-3.99279487500001));
#326419=CARTESIAN_POINT('Ctrl Pts',(-0.114872125000056,2.2,-3.99279487500001));
#326420=CARTESIAN_POINT('Ctrl Pts',(-0.114873067000056,12.2,-3.99290366100002));
#326421=CARTESIAN_POINT('Ctrl Pts',(-0.114873067000056,5.2,-3.99290366100002));
#326422=CARTESIAN_POINT('Ctrl Pts',(-0.114873067000056,2.2,-3.99290366100002));
#326423=CARTESIAN_POINT('Ctrl Pts',(-0.114873913000055,12.2,-3.99301967100001));
#326424=CARTESIAN_POINT('Ctrl Pts',(-0.114873913000055,5.2,-3.99301967100001));
#326425=CARTESIAN_POINT('Ctrl Pts',(-0.114873913000055,2.2,-3.99301967100001));
#326426=CARTESIAN_POINT('Ctrl Pts',(-0.114874646000055,12.2,-3.99314289200001));
#326427=CARTESIAN_POINT('Ctrl Pts',(-0.114874646000055,5.2,-3.99314289200001));
#326428=CARTESIAN_POINT('Ctrl Pts',(-0.114874646000055,2.2,-3.99314289200001));
#326429=CARTESIAN_POINT('Ctrl Pts',(-0.114875245000056,12.2,-3.99327330700002));
#326430=CARTESIAN_POINT('Ctrl Pts',(-0.114875245000056,5.2,-3.99327330700002));
#326431=CARTESIAN_POINT('Ctrl Pts',(-0.114875245000056,2.2,-3.99327330700002));
#326432=CARTESIAN_POINT('Ctrl Pts',(-0.114875694000055,12.2,-3.99341090000001));
#326433=CARTESIAN_POINT('Ctrl Pts',(-0.114875694000055,5.2,-3.99341090000001));
#326434=CARTESIAN_POINT('Ctrl Pts',(-0.114875694000055,2.2,-3.99341090000001));
#326435=CARTESIAN_POINT('Ctrl Pts',(-0.114875972000055,12.2,-3.99355565600001));
#326436=CARTESIAN_POINT('Ctrl Pts',(-0.114875972000055,5.2,-3.99355565600001));
#326437=CARTESIAN_POINT('Ctrl Pts',(-0.114875972000055,2.2,-3.99355565600001));
#326438=CARTESIAN_POINT('Ctrl Pts',(-0.114876059000055,12.2,-3.99370755700001));
#326439=CARTESIAN_POINT('Ctrl Pts',(-0.114876059000055,5.2,-3.99370755700001));
#326440=CARTESIAN_POINT('Ctrl Pts',(-0.114876059000055,2.2,-3.99370755700001));
#326441=CARTESIAN_POINT('Ctrl Pts',(-0.114875936000055,12.2,-3.99386658500001));
#326442=CARTESIAN_POINT('Ctrl Pts',(-0.114875936000055,5.2,-3.99386658500001));
#326443=CARTESIAN_POINT('Ctrl Pts',(-0.114875936000055,2.2,-3.99386658500001));
#326444=CARTESIAN_POINT('Ctrl Pts',(-0.114875582000057,12.2,-3.99403272400002));
#326445=CARTESIAN_POINT('Ctrl Pts',(-0.114875582000057,5.2,-3.99403272400002));
#326446=CARTESIAN_POINT('Ctrl Pts',(-0.114875582000057,2.2,-3.99403272400002));
#326447=CARTESIAN_POINT('Ctrl Pts',(-0.114874979000056,12.2,-3.99420595800001));
#326448=CARTESIAN_POINT('Ctrl Pts',(-0.114874979000056,5.2,-3.99420595800001));
#326449=CARTESIAN_POINT('Ctrl Pts',(-0.114874979000056,2.2,-3.99420595800001));
#326450=CARTESIAN_POINT('Ctrl Pts',(-0.114874109000055,12.2,-3.99438627000002));
#326451=CARTESIAN_POINT('Ctrl Pts',(-0.114874109000055,5.2,-3.99438627000002));
#326452=CARTESIAN_POINT('Ctrl Pts',(-0.114874109000055,2.2,-3.99438627000002));
#326453=CARTESIAN_POINT('Ctrl Pts',(-0.114872952000056,12.2,-3.99457364500002));
#326454=CARTESIAN_POINT('Ctrl Pts',(-0.114872952000056,5.2,-3.99457364500002));
#326455=CARTESIAN_POINT('Ctrl Pts',(-0.114872952000056,2.2,-3.99457364500002));
#326456=CARTESIAN_POINT('Ctrl Pts',(-0.114871493000056,12.2,-3.99476806800001));
#326457=CARTESIAN_POINT('Ctrl Pts',(-0.114871493000056,5.2,-3.99476806800001));
#326458=CARTESIAN_POINT('Ctrl Pts',(-0.114871493000056,2.2,-3.99476806800001));
#326459=CARTESIAN_POINT('Ctrl Pts',(-0.114869709000055,12.2,-3.99496952100002));
#326460=CARTESIAN_POINT('Ctrl Pts',(-0.114869709000055,5.2,-3.99496952100002));
#326461=CARTESIAN_POINT('Ctrl Pts',(-0.114869709000055,2.2,-3.99496952100002));
#326462=CARTESIAN_POINT('Ctrl Pts',(-0.114867585000056,12.2,-3.99517798800002));
#326463=CARTESIAN_POINT('Ctrl Pts',(-0.114867585000056,5.2,-3.99517798800002));
#326464=CARTESIAN_POINT('Ctrl Pts',(-0.114867585000056,2.2,-3.99517798800002));
#326465=CARTESIAN_POINT('Ctrl Pts',(-0.114865100000056,12.2,-3.99539345500001));
#326466=CARTESIAN_POINT('Ctrl Pts',(-0.114865100000056,5.2,-3.99539345500001));
#326467=CARTESIAN_POINT('Ctrl Pts',(-0.114865100000056,2.2,-3.99539345500001));
#326468=CARTESIAN_POINT('Ctrl Pts',(-0.114862238000055,12.2,-3.99561590300001));
#326469=CARTESIAN_POINT('Ctrl Pts',(-0.114862238000055,5.2,-3.99561590300001));
#326470=CARTESIAN_POINT('Ctrl Pts',(-0.114862238000055,2.2,-3.99561590300001));
#326471=CARTESIAN_POINT('Ctrl Pts',(-0.114858978000055,12.2,-3.99584531900001));
#326472=CARTESIAN_POINT('Ctrl Pts',(-0.114858978000055,5.2,-3.99584531900001));
#326473=CARTESIAN_POINT('Ctrl Pts',(-0.114858978000055,2.2,-3.99584531900001));
#326474=CARTESIAN_POINT('Ctrl Pts',(-0.114855304000056,12.2,-3.99608168400002));
#326475=CARTESIAN_POINT('Ctrl Pts',(-0.114855304000056,5.2,-3.99608168400002));
#326476=CARTESIAN_POINT('Ctrl Pts',(-0.114855304000056,2.2,-3.99608168400002));
#326477=CARTESIAN_POINT('Ctrl Pts',(-0.114851197000055,12.2,-3.99632498400001));
#326478=CARTESIAN_POINT('Ctrl Pts',(-0.114851197000055,5.2,-3.99632498400001));
#326479=CARTESIAN_POINT('Ctrl Pts',(-0.114851197000055,2.2,-3.99632498400001));
#326480=CARTESIAN_POINT('Ctrl Pts',(-0.114846640000056,12.2,-3.99657520200002));
#326481=CARTESIAN_POINT('Ctrl Pts',(-0.114846640000056,5.2,-3.99657520200002));
#326482=CARTESIAN_POINT('Ctrl Pts',(-0.114846640000056,2.2,-3.99657520200002));
#326483=CARTESIAN_POINT('Ctrl Pts',(-0.114841613000056,12.2,-3.99683232300001));
#326484=CARTESIAN_POINT('Ctrl Pts',(-0.114841613000056,5.2,-3.99683232300001));
#326485=CARTESIAN_POINT('Ctrl Pts',(-0.114841613000056,2.2,-3.99683232300001));
#326486=CARTESIAN_POINT('Ctrl Pts',(-0.114836100000056,12.2,-3.99709633200001));
#326487=CARTESIAN_POINT('Ctrl Pts',(-0.114836100000056,5.2,-3.99709633200001));
#326488=CARTESIAN_POINT('Ctrl Pts',(-0.114836100000056,2.2,-3.99709633200001));
#326489=CARTESIAN_POINT('Ctrl Pts',(-0.114830082000056,12.2,-3.99736721100002));
#326490=CARTESIAN_POINT('Ctrl Pts',(-0.114830082000056,5.2,-3.99736721100002));
#326491=CARTESIAN_POINT('Ctrl Pts',(-0.114830082000056,2.2,-3.99736721100002));
#326492=CARTESIAN_POINT('Ctrl Pts',(-0.114823543000057,12.2,-3.99764494700001));
#326493=CARTESIAN_POINT('Ctrl Pts',(-0.114823543000057,5.2,-3.99764494700001));
#326494=CARTESIAN_POINT('Ctrl Pts',(-0.114823543000057,2.2,-3.99764494700001));
#326495=CARTESIAN_POINT('Ctrl Pts',(-0.114816464000055,12.2,-3.99792952200002));
#326496=CARTESIAN_POINT('Ctrl Pts',(-0.114816464000055,5.2,-3.99792952200002));
#326497=CARTESIAN_POINT('Ctrl Pts',(-0.114816464000055,2.2,-3.99792952200002));
#326498=CARTESIAN_POINT('Ctrl Pts',(-0.114808828000056,12.2,-3.99822092200001));
#326499=CARTESIAN_POINT('Ctrl Pts',(-0.114808828000056,5.2,-3.99822092200001));
#326500=CARTESIAN_POINT('Ctrl Pts',(-0.114808828000056,2.2,-3.99822092200001));
#326501=CARTESIAN_POINT('Ctrl Pts',(-0.114800617000055,12.2,-3.99851912900001));
#326502=CARTESIAN_POINT('Ctrl Pts',(-0.114800617000055,5.2,-3.99851912900001));
#326503=CARTESIAN_POINT('Ctrl Pts',(-0.114800617000055,2.2,-3.99851912900001));
#326504=CARTESIAN_POINT('Ctrl Pts',(-0.114791815000055,12.2,-3.99882413000002));
#326505=CARTESIAN_POINT('Ctrl Pts',(-0.114791815000055,5.2,-3.99882413000002));
#326506=CARTESIAN_POINT('Ctrl Pts',(-0.114791815000055,2.2,-3.99882413000002));
#326507=CARTESIAN_POINT('Ctrl Pts',(-0.114782402000057,12.2,-3.99913590800002));
#326508=CARTESIAN_POINT('Ctrl Pts',(-0.114782402000057,5.2,-3.99913590800002));
#326509=CARTESIAN_POINT('Ctrl Pts',(-0.114782402000057,2.2,-3.99913590800002));
#326510=CARTESIAN_POINT('Ctrl Pts',(-0.114772364000055,12.2,-3.99945444800001));
#326511=CARTESIAN_POINT('Ctrl Pts',(-0.114772364000055,5.2,-3.99945444800001));
#326512=CARTESIAN_POINT('Ctrl Pts',(-0.114772364000055,2.2,-3.99945444800001));
#326513=CARTESIAN_POINT('Ctrl Pts',(-0.114761683000056,12.2,-3.99977973400001));
#326514=CARTESIAN_POINT('Ctrl Pts',(-0.114761683000056,5.2,-3.99977973400001));
#326515=CARTESIAN_POINT('Ctrl Pts',(-0.114761683000056,2.2,-3.99977973400001));
#326516=CARTESIAN_POINT('Ctrl Pts',(-0.114750340000055,12.2,-4.00011175100001));
#326517=CARTESIAN_POINT('Ctrl Pts',(-0.114750340000055,5.2,-4.00011175100001));
#326518=CARTESIAN_POINT('Ctrl Pts',(-0.114750340000055,2.2,-4.00011175100001));
#326519=CARTESIAN_POINT('Ctrl Pts',(-0.114738319000055,12.2,-4.00045048400001));
#326520=CARTESIAN_POINT('Ctrl Pts',(-0.114738319000055,5.2,-4.00045048400001));
#326521=CARTESIAN_POINT('Ctrl Pts',(-0.114738319000055,2.2,-4.00045048400001));
#326522=CARTESIAN_POINT('Ctrl Pts',(-0.114725605000056,12.2,-4.00079591700001));
#326523=CARTESIAN_POINT('Ctrl Pts',(-0.114725605000056,5.2,-4.00079591700001));
#326524=CARTESIAN_POINT('Ctrl Pts',(-0.114725605000056,2.2,-4.00079591700001));
#326525=CARTESIAN_POINT('Ctrl Pts',(-0.114712179000056,12.2,-4.00114803400001));
#326526=CARTESIAN_POINT('Ctrl Pts',(-0.114712179000056,5.2,-4.00114803400001));
#326527=CARTESIAN_POINT('Ctrl Pts',(-0.114712179000056,2.2,-4.00114803400001));
#326528=CARTESIAN_POINT('Ctrl Pts',(-0.114698024000056,12.2,-4.00150682100001));
#326529=CARTESIAN_POINT('Ctrl Pts',(-0.114698024000056,5.2,-4.00150682100001));
#326530=CARTESIAN_POINT('Ctrl Pts',(-0.114698024000056,2.2,-4.00150682100001));
#326531=CARTESIAN_POINT('Ctrl Pts',(-0.114683124000056,12.2,-4.00187226200002));
#326532=CARTESIAN_POINT('Ctrl Pts',(-0.114683124000056,5.2,-4.00187226200002));
#326533=CARTESIAN_POINT('Ctrl Pts',(-0.114683124000056,2.2,-4.00187226200002));
#326534=CARTESIAN_POINT('Ctrl Pts',(-0.114667464000057,12.2,-4.00224434100001));
#326535=CARTESIAN_POINT('Ctrl Pts',(-0.114667464000057,5.2,-4.00224434100001));
#326536=CARTESIAN_POINT('Ctrl Pts',(-0.114667464000057,2.2,-4.00224434100001));
#326537=CARTESIAN_POINT('Ctrl Pts',(-0.114651025000055,12.2,-4.00262304400002));
#326538=CARTESIAN_POINT('Ctrl Pts',(-0.114651025000055,5.2,-4.00262304400002));
#326539=CARTESIAN_POINT('Ctrl Pts',(-0.114651025000055,2.2,-4.00262304400002));
#326540=CARTESIAN_POINT('Ctrl Pts',(-0.114633791000056,12.2,-4.00300835600001));
#326541=CARTESIAN_POINT('Ctrl Pts',(-0.114633791000056,5.2,-4.00300835600001));
#326542=CARTESIAN_POINT('Ctrl Pts',(-0.114633791000056,2.2,-4.00300835600001));
#326543=CARTESIAN_POINT('Ctrl Pts',(-0.114615747000055,12.2,-4.00340026000002));
#326544=CARTESIAN_POINT('Ctrl Pts',(-0.114615747000055,5.2,-4.00340026000002));
#326545=CARTESIAN_POINT('Ctrl Pts',(-0.114615747000055,2.2,-4.00340026000002));
#326546=CARTESIAN_POINT('Ctrl Pts',(-0.114596874000057,12.2,-4.00379874300001));
#326547=CARTESIAN_POINT('Ctrl Pts',(-0.114596874000057,5.2,-4.00379874300001));
#326548=CARTESIAN_POINT('Ctrl Pts',(-0.114596874000057,2.2,-4.00379874300001));
#326549=CARTESIAN_POINT('Ctrl Pts',(-0.114577159000057,12.2,-4.00420378800002));
#326550=CARTESIAN_POINT('Ctrl Pts',(-0.114577159000057,5.2,-4.00420378800002));
#326551=CARTESIAN_POINT('Ctrl Pts',(-0.114577159000057,2.2,-4.00420378800002));
#326552=CARTESIAN_POINT('Ctrl Pts',(-0.114556584000055,12.2,-4.00461538100001));
#326553=CARTESIAN_POINT('Ctrl Pts',(-0.114556584000055,5.2,-4.00461538100001));
#326554=CARTESIAN_POINT('Ctrl Pts',(-0.114556584000055,2.2,-4.00461538100001));
#326555=CARTESIAN_POINT('Ctrl Pts',(-0.114535132000055,12.2,-4.00503350700002));
#326556=CARTESIAN_POINT('Ctrl Pts',(-0.114535132000055,5.2,-4.00503350700002));
#326557=CARTESIAN_POINT('Ctrl Pts',(-0.114535132000055,2.2,-4.00503350700002));
#326558=CARTESIAN_POINT('Ctrl Pts',(-0.114512789000055,12.2,-4.00545815000001));
#326559=CARTESIAN_POINT('Ctrl Pts',(-0.114512789000055,5.2,-4.00545815000001));
#326560=CARTESIAN_POINT('Ctrl Pts',(-0.114512789000055,2.2,-4.00545815000001));
#326561=CARTESIAN_POINT('Ctrl Pts',(-0.114489538000055,12.2,-4.00588929700001));
#326562=CARTESIAN_POINT('Ctrl Pts',(-0.114489538000055,5.2,-4.00588929700001));
#326563=CARTESIAN_POINT('Ctrl Pts',(-0.114489538000055,2.2,-4.00588929700001));
#326564=CARTESIAN_POINT('Ctrl Pts',(-0.114465362000056,12.2,-4.00632693100002));
#326565=CARTESIAN_POINT('Ctrl Pts',(-0.114465362000056,5.2,-4.00632693100002));
#326566=CARTESIAN_POINT('Ctrl Pts',(-0.114465362000056,2.2,-4.00632693100002));
#326567=CARTESIAN_POINT('Ctrl Pts',(-0.114440247000056,12.2,-4.00677103800001));
#326568=CARTESIAN_POINT('Ctrl Pts',(-0.114440247000056,5.2,-4.00677103800001));
#326569=CARTESIAN_POINT('Ctrl Pts',(-0.114440247000056,2.2,-4.00677103800001));
#326570=CARTESIAN_POINT('Ctrl Pts',(-0.114414176000055,12.2,-4.00722160200001));
#326571=CARTESIAN_POINT('Ctrl Pts',(-0.114414176000055,5.2,-4.00722160200001));
#326572=CARTESIAN_POINT('Ctrl Pts',(-0.114414176000055,2.2,-4.00722160200001));
#326573=CARTESIAN_POINT('Ctrl Pts',(-0.114387135000056,12.2,-4.00767861000002));
#326574=CARTESIAN_POINT('Ctrl Pts',(-0.114387135000056,5.2,-4.00767861000002));
#326575=CARTESIAN_POINT('Ctrl Pts',(-0.114387135000056,2.2,-4.00767861000002));
#326576=CARTESIAN_POINT('Ctrl Pts',(-0.114359106000055,12.2,-4.00814204600001));
#326577=CARTESIAN_POINT('Ctrl Pts',(-0.114359106000055,5.2,-4.00814204600001));
#326578=CARTESIAN_POINT('Ctrl Pts',(-0.114359106000055,2.2,-4.00814204600001));
#326579=CARTESIAN_POINT('Ctrl Pts',(-0.114330074000056,12.2,-4.00861189500001));
#326580=CARTESIAN_POINT('Ctrl Pts',(-0.114330074000056,5.2,-4.00861189500001));
#326581=CARTESIAN_POINT('Ctrl Pts',(-0.114330074000056,2.2,-4.00861189500001));
#326582=CARTESIAN_POINT('Ctrl Pts',(-0.114300025000055,12.2,-4.00908814200001));
#326583=CARTESIAN_POINT('Ctrl Pts',(-0.114300025000055,5.2,-4.00908814200001));
#326584=CARTESIAN_POINT('Ctrl Pts',(-0.114300025000055,2.2,-4.00908814200001));
#326585=CARTESIAN_POINT('Ctrl Pts',(-0.114268943000055,12.2,-4.00957077400002));
#326586=CARTESIAN_POINT('Ctrl Pts',(-0.114268943000055,5.2,-4.00957077400002));
#326587=CARTESIAN_POINT('Ctrl Pts',(-0.114268943000055,2.2,-4.00957077400002));
#326588=CARTESIAN_POINT('Ctrl Pts',(-0.114236811000056,12.2,-4.01005977400001));
#326589=CARTESIAN_POINT('Ctrl Pts',(-0.114236811000056,5.2,-4.01005977400001));
#326590=CARTESIAN_POINT('Ctrl Pts',(-0.114236811000056,2.2,-4.01005977400001));
#326591=CARTESIAN_POINT('Ctrl Pts',(-0.114203615000056,12.2,-4.01055512900002));
#326592=CARTESIAN_POINT('Ctrl Pts',(-0.114203615000056,5.2,-4.01055512900002));
#326593=CARTESIAN_POINT('Ctrl Pts',(-0.114203615000056,2.2,-4.01055512900002));
#326594=CARTESIAN_POINT('Ctrl Pts',(-0.114169340000055,12.2,-4.01105682400001));
#326595=CARTESIAN_POINT('Ctrl Pts',(-0.114169340000055,5.2,-4.01105682400001));
#326596=CARTESIAN_POINT('Ctrl Pts',(-0.114169340000055,2.2,-4.01105682400001));
#326597=CARTESIAN_POINT('Ctrl Pts',(-0.114133970000055,12.2,-4.01156484400001));
#326598=CARTESIAN_POINT('Ctrl Pts',(-0.114133970000055,5.2,-4.01156484400001));
#326599=CARTESIAN_POINT('Ctrl Pts',(-0.114133970000055,2.2,-4.01156484400001));
#326600=CARTESIAN_POINT('Ctrl Pts',(-0.114097490000056,12.2,-4.01207917300002));
#326601=CARTESIAN_POINT('Ctrl Pts',(-0.114097490000056,5.2,-4.01207917300002));
#326602=CARTESIAN_POINT('Ctrl Pts',(-0.114097490000056,2.2,-4.01207917300002));
#326603=CARTESIAN_POINT('Ctrl Pts',(-0.114059886000056,12.2,-4.01259979900002));
#326604=CARTESIAN_POINT('Ctrl Pts',(-0.114059886000056,5.2,-4.01259979900002));
#326605=CARTESIAN_POINT('Ctrl Pts',(-0.114059886000056,2.2,-4.01259979900002));
#326606=CARTESIAN_POINT('Ctrl Pts',(-0.114021141000055,12.2,-4.01312670600001));
#326607=CARTESIAN_POINT('Ctrl Pts',(-0.114021141000055,5.2,-4.01312670600001));
#326608=CARTESIAN_POINT('Ctrl Pts',(-0.114021141000055,2.2,-4.01312670600001));
#326609=CARTESIAN_POINT('Ctrl Pts',(-0.113981242000056,12.2,-4.01365988000002));
#326610=CARTESIAN_POINT('Ctrl Pts',(-0.113981242000056,5.2,-4.01365988000002));
#326611=CARTESIAN_POINT('Ctrl Pts',(-0.113981242000056,2.2,-4.01365988000002));
#326612=CARTESIAN_POINT('Ctrl Pts',(-0.113940173000057,12.2,-4.01419930600001));
#326613=CARTESIAN_POINT('Ctrl Pts',(-0.113940173000057,5.2,-4.01419930600001));
#326614=CARTESIAN_POINT('Ctrl Pts',(-0.113940173000057,2.2,-4.01419930600001));
#326615=CARTESIAN_POINT('Ctrl Pts',(-0.113897920000056,12.2,-4.01474496900001));
#326616=CARTESIAN_POINT('Ctrl Pts',(-0.113897920000056,5.2,-4.01474496900001));
#326617=CARTESIAN_POINT('Ctrl Pts',(-0.113897920000056,2.2,-4.01474496900001));
#326618=CARTESIAN_POINT('Ctrl Pts',(-0.113854467000056,12.2,-4.01529685600002));
#326619=CARTESIAN_POINT('Ctrl Pts',(-0.113854467000056,5.2,-4.01529685600002));
#326620=CARTESIAN_POINT('Ctrl Pts',(-0.113854467000056,2.2,-4.01529685600002));
#326621=CARTESIAN_POINT('Ctrl Pts',(-0.113809801000055,12.2,-4.01585495100001));
#326622=CARTESIAN_POINT('Ctrl Pts',(-0.113809801000055,5.2,-4.01585495100001));
#326623=CARTESIAN_POINT('Ctrl Pts',(-0.113809801000055,2.2,-4.01585495100001));
#326624=CARTESIAN_POINT('Ctrl Pts',(-0.113763907000056,12.2,-4.01641924100002));
#326625=CARTESIAN_POINT('Ctrl Pts',(-0.113763907000056,5.2,-4.01641924100002));
#326626=CARTESIAN_POINT('Ctrl Pts',(-0.113763907000056,2.2,-4.01641924100002));
#326627=CARTESIAN_POINT('Ctrl Pts',(-0.113716768000056,12.2,-4.01698971200001));
#326628=CARTESIAN_POINT('Ctrl Pts',(-0.113716768000056,5.2,-4.01698971200001));
#326629=CARTESIAN_POINT('Ctrl Pts',(-0.113716768000056,2.2,-4.01698971200001));
#326630=CARTESIAN_POINT('Ctrl Pts',(-0.113668373000056,12.2,-4.01756634800002));
#326631=CARTESIAN_POINT('Ctrl Pts',(-0.113668373000056,5.2,-4.01756634800002));
#326632=CARTESIAN_POINT('Ctrl Pts',(-0.113668373000056,2.2,-4.01756634800002));
#326633=CARTESIAN_POINT('Ctrl Pts',(-0.113618705000055,12.2,-4.01814913500001));
#326634=CARTESIAN_POINT('Ctrl Pts',(-0.113618705000055,5.2,-4.01814913500001));
#326635=CARTESIAN_POINT('Ctrl Pts',(-0.113618705000055,2.2,-4.01814913500001));
#326636=CARTESIAN_POINT('Ctrl Pts',(-0.113567751000057,12.2,-4.01873805900001));
#326637=CARTESIAN_POINT('Ctrl Pts',(-0.113567751000057,5.2,-4.01873805900001));
#326638=CARTESIAN_POINT('Ctrl Pts',(-0.113567751000057,2.2,-4.01873805900001));
#326639=CARTESIAN_POINT('Ctrl Pts',(-0.113515496000056,12.2,-4.01933310600001));
#326640=CARTESIAN_POINT('Ctrl Pts',(-0.113515496000056,5.2,-4.01933310600001));
#326641=CARTESIAN_POINT('Ctrl Pts',(-0.113515496000056,2.2,-4.01933310600001));
#326642=CARTESIAN_POINT('Ctrl Pts',(-0.113461927000056,12.2,-4.01993426200002));
#326643=CARTESIAN_POINT('Ctrl Pts',(-0.113461927000056,5.2,-4.01993426200002));
#326644=CARTESIAN_POINT('Ctrl Pts',(-0.113461927000056,2.2,-4.01993426200002));
#326645=CARTESIAN_POINT('Ctrl Pts',(-0.113407028000055,12.2,-4.02054151200002));
#326646=CARTESIAN_POINT('Ctrl Pts',(-0.113407028000055,5.2,-4.02054151200002));
#326647=CARTESIAN_POINT('Ctrl Pts',(-0.113407028000055,2.2,-4.02054151200002));
#326648=CARTESIAN_POINT('Ctrl Pts',(-0.113350786000056,12.2,-4.02115484100001));
#326649=CARTESIAN_POINT('Ctrl Pts',(-0.113350786000056,5.2,-4.02115484100001));
#326650=CARTESIAN_POINT('Ctrl Pts',(-0.113350786000056,2.2,-4.02115484100001));
#326651=CARTESIAN_POINT('Ctrl Pts',(-0.113293186000056,12.2,-4.02177423700001));
#326652=CARTESIAN_POINT('Ctrl Pts',(-0.113293186000056,5.2,-4.02177423700001));
#326653=CARTESIAN_POINT('Ctrl Pts',(-0.113293186000056,2.2,-4.02177423700001));
#326654=CARTESIAN_POINT('Ctrl Pts',(-0.113234215000055,12.2,-4.02239968500002));
#326655=CARTESIAN_POINT('Ctrl Pts',(-0.113234215000055,5.2,-4.02239968500002));
#326656=CARTESIAN_POINT('Ctrl Pts',(-0.113234215000055,2.2,-4.02239968500002));
#326657=CARTESIAN_POINT('Ctrl Pts',(-0.113173859000056,12.2,-4.02303117100002));
#326658=CARTESIAN_POINT('Ctrl Pts',(-0.113173859000056,5.2,-4.02303117100002));
#326659=CARTESIAN_POINT('Ctrl Pts',(-0.113173859000056,2.2,-4.02303117100002));
#326660=CARTESIAN_POINT('Ctrl Pts',(-0.113112103000056,12.2,-4.02366868000001));
#326661=CARTESIAN_POINT('Ctrl Pts',(-0.113112103000056,5.2,-4.02366868000001));
#326662=CARTESIAN_POINT('Ctrl Pts',(-0.113112103000056,2.2,-4.02366868000001));
#326663=CARTESIAN_POINT('Ctrl Pts',(-0.113048934000056,12.2,-4.02431219900001));
#326664=CARTESIAN_POINT('Ctrl Pts',(-0.113048934000056,5.2,-4.02431219900001));
#326665=CARTESIAN_POINT('Ctrl Pts',(-0.113048934000056,2.2,-4.02431219900001));
#326666=CARTESIAN_POINT('Ctrl Pts',(-0.112984338000055,12.2,-4.02496171300001));
#326667=CARTESIAN_POINT('Ctrl Pts',(-0.112984338000055,5.2,-4.02496171300001));
#326668=CARTESIAN_POINT('Ctrl Pts',(-0.112984338000055,2.2,-4.02496171300001));
#326669=CARTESIAN_POINT('Ctrl Pts',(-0.112918302000056,12.2,-4.02561720900001));
#326670=CARTESIAN_POINT('Ctrl Pts',(-0.112918302000056,5.2,-4.02561720900001));
#326671=CARTESIAN_POINT('Ctrl Pts',(-0.112918302000056,2.2,-4.02561720900001));
#326672=CARTESIAN_POINT('Ctrl Pts',(-0.112850811000056,12.2,-4.02627867200001));
#326673=CARTESIAN_POINT('Ctrl Pts',(-0.112850811000056,5.2,-4.02627867200001));
#326674=CARTESIAN_POINT('Ctrl Pts',(-0.112850811000056,2.2,-4.02627867200001));
#326675=CARTESIAN_POINT('Ctrl Pts',(-0.112781853000056,12.2,-4.02694608900001));
#326676=CARTESIAN_POINT('Ctrl Pts',(-0.112781853000056,5.2,-4.02694608900001));
#326677=CARTESIAN_POINT('Ctrl Pts',(-0.112781853000056,2.2,-4.02694608900001));
#326678=CARTESIAN_POINT('Ctrl Pts',(-0.112711412000056,12.2,-4.02761944500002));
#326679=CARTESIAN_POINT('Ctrl Pts',(-0.112711412000056,5.2,-4.02761944500002));
#326680=CARTESIAN_POINT('Ctrl Pts',(-0.112711412000056,2.2,-4.02761944500002));
#326681=CARTESIAN_POINT('Ctrl Pts',(-0.112639476000057,12.2,-4.02829872600002));
#326682=CARTESIAN_POINT('Ctrl Pts',(-0.112639476000057,5.2,-4.02829872600002));
#326683=CARTESIAN_POINT('Ctrl Pts',(-0.112639476000057,2.2,-4.02829872600002));
#326684=CARTESIAN_POINT('Ctrl Pts',(-0.112566033000056,12.2,-4.02898392000001));
#326685=CARTESIAN_POINT('Ctrl Pts',(-0.112566033000056,5.2,-4.02898392000001));
#326686=CARTESIAN_POINT('Ctrl Pts',(-0.112566033000056,2.2,-4.02898392000001));
#326687=CARTESIAN_POINT('Ctrl Pts',(-0.112491067000056,12.2,-4.02967501100001));
#326688=CARTESIAN_POINT('Ctrl Pts',(-0.112491067000056,5.2,-4.02967501100001));
#326689=CARTESIAN_POINT('Ctrl Pts',(-0.112491067000056,2.2,-4.02967501100001));
#326690=CARTESIAN_POINT('Ctrl Pts',(-0.112414565000056,12.2,-4.03037198700002));
#326691=CARTESIAN_POINT('Ctrl Pts',(-0.112414565000056,5.2,-4.03037198700002));
#326692=CARTESIAN_POINT('Ctrl Pts',(-0.112414565000056,2.2,-4.03037198700002));
#326693=CARTESIAN_POINT('Ctrl Pts',(-0.112336516000056,12.2,-4.03107483200001));
#326694=CARTESIAN_POINT('Ctrl Pts',(-0.112336516000056,5.2,-4.03107483200001));
#326695=CARTESIAN_POINT('Ctrl Pts',(-0.112336516000056,2.2,-4.03107483200001));
#326696=CARTESIAN_POINT('Ctrl Pts',(-0.112256904000055,12.2,-4.03178353500001));
#326697=CARTESIAN_POINT('Ctrl Pts',(-0.112256904000055,5.2,-4.03178353500001));
#326698=CARTESIAN_POINT('Ctrl Pts',(-0.112256904000055,2.2,-4.03178353500001));
#326699=CARTESIAN_POINT('Ctrl Pts',(-0.112175718000056,12.2,-4.03249807800002));
#326700=CARTESIAN_POINT('Ctrl Pts',(-0.112175718000056,5.2,-4.03249807800002));
#326701=CARTESIAN_POINT('Ctrl Pts',(-0.112175718000056,2.2,-4.03249807800002));
#326702=CARTESIAN_POINT('Ctrl Pts',(-0.112092944000055,12.2,-4.03321845200002));
#326703=CARTESIAN_POINT('Ctrl Pts',(-0.112092944000055,5.2,-4.03321845200002));
#326704=CARTESIAN_POINT('Ctrl Pts',(-0.112092944000055,2.2,-4.03321845200002));
#326705=CARTESIAN_POINT('Ctrl Pts',(-0.112008568000055,12.2,-4.03394464100002));
#326706=CARTESIAN_POINT('Ctrl Pts',(-0.112008568000055,5.2,-4.03394464100002));
#326707=CARTESIAN_POINT('Ctrl Pts',(-0.112008568000055,2.2,-4.03394464100002));
#326708=CARTESIAN_POINT('Ctrl Pts',(-0.111922578000057,12.2,-4.03467663000002));
#326709=CARTESIAN_POINT('Ctrl Pts',(-0.111922578000057,5.2,-4.03467663000002));
#326710=CARTESIAN_POINT('Ctrl Pts',(-0.111922578000057,2.2,-4.03467663000002));
#326711=CARTESIAN_POINT('Ctrl Pts',(-0.111834961000056,12.2,-4.03541440800002));
#326712=CARTESIAN_POINT('Ctrl Pts',(-0.111834961000056,5.2,-4.03541440800002));
#326713=CARTESIAN_POINT('Ctrl Pts',(-0.111834961000056,2.2,-4.03541440800002));
#326714=CARTESIAN_POINT('Ctrl Pts',(-0.111745705000056,12.2,-4.03615796000001));
#326715=CARTESIAN_POINT('Ctrl Pts',(-0.111745705000056,5.2,-4.03615796000001));
#326716=CARTESIAN_POINT('Ctrl Pts',(-0.111745705000056,2.2,-4.03615796000001));
#326717=CARTESIAN_POINT('Ctrl Pts',(-0.111654795000057,12.2,-4.03690727100001));
#326718=CARTESIAN_POINT('Ctrl Pts',(-0.111654795000057,5.2,-4.03690727100001));
#326719=CARTESIAN_POINT('Ctrl Pts',(-0.111654795000057,2.2,-4.03690727100001));
#326720=CARTESIAN_POINT('Ctrl Pts',(-0.111562219000056,12.2,-4.03766233000002));
#326721=CARTESIAN_POINT('Ctrl Pts',(-0.111562219000056,5.2,-4.03766233000002));
#326722=CARTESIAN_POINT('Ctrl Pts',(-0.111562219000056,2.2,-4.03766233000002));
#326723=CARTESIAN_POINT('Ctrl Pts',(-0.111467966000056,12.2,-4.03842312200001));
#326724=CARTESIAN_POINT('Ctrl Pts',(-0.111467966000056,5.2,-4.03842312200001));
#326725=CARTESIAN_POINT('Ctrl Pts',(-0.111467966000056,2.2,-4.03842312200001));
#326726=CARTESIAN_POINT('Ctrl Pts',(-0.111372020000056,12.2,-4.03918963400002));
#326727=CARTESIAN_POINT('Ctrl Pts',(-0.111372020000056,5.2,-4.03918963400002));
#326728=CARTESIAN_POINT('Ctrl Pts',(-0.111372020000056,2.2,-4.03918963400002));
#326729=CARTESIAN_POINT('Ctrl Pts',(-0.111274372000055,12.2,-4.03996185000001));
#326730=CARTESIAN_POINT('Ctrl Pts',(-0.111274372000055,5.2,-4.03996185000001));
#326731=CARTESIAN_POINT('Ctrl Pts',(-0.111274372000055,2.2,-4.03996185000001));
#326732=CARTESIAN_POINT('Ctrl Pts',(-0.111175006000056,12.2,-4.04073976100001));
#326733=CARTESIAN_POINT('Ctrl Pts',(-0.111175006000056,5.2,-4.04073976100001));
#326734=CARTESIAN_POINT('Ctrl Pts',(-0.111175006000056,2.2,-4.04073976100001));
#326735=CARTESIAN_POINT('Ctrl Pts',(-0.111073912000055,12.2,-4.04152335000001));
#326736=CARTESIAN_POINT('Ctrl Pts',(-0.111073912000055,5.2,-4.04152335000001));
#326737=CARTESIAN_POINT('Ctrl Pts',(-0.111073912000055,2.2,-4.04152335000001));
#326738=CARTESIAN_POINT('Ctrl Pts',(-0.110971077000055,12.2,-4.04231260400001));
#326739=CARTESIAN_POINT('Ctrl Pts',(-0.110971077000055,5.2,-4.04231260400001));
#326740=CARTESIAN_POINT('Ctrl Pts',(-0.110971077000055,2.2,-4.04231260400001));
#326741=CARTESIAN_POINT('Ctrl Pts',(-0.110866488000055,12.2,-4.04310751100001));
#326742=CARTESIAN_POINT('Ctrl Pts',(-0.110866488000055,5.2,-4.04310751100001));
#326743=CARTESIAN_POINT('Ctrl Pts',(-0.110866488000055,2.2,-4.04310751100001));
#326744=CARTESIAN_POINT('Ctrl Pts',(-0.110760133000056,12.2,-4.04390805600002));
#326745=CARTESIAN_POINT('Ctrl Pts',(-0.110760133000056,5.2,-4.04390805600002));
#326746=CARTESIAN_POINT('Ctrl Pts',(-0.110760133000056,2.2,-4.04390805600002));
#326747=CARTESIAN_POINT('Ctrl Pts',(-0.110651998000056,12.2,-4.04471422600002));
#326748=CARTESIAN_POINT('Ctrl Pts',(-0.110651998000056,5.2,-4.04471422600002));
#326749=CARTESIAN_POINT('Ctrl Pts',(-0.110651998000056,2.2,-4.04471422600002));
#326750=CARTESIAN_POINT('Ctrl Pts',(-0.110542073000056,12.2,-4.04552600800002));
#326751=CARTESIAN_POINT('Ctrl Pts',(-0.110542073000056,5.2,-4.04552600800002));
#326752=CARTESIAN_POINT('Ctrl Pts',(-0.110542073000056,2.2,-4.04552600800002));
#326753=CARTESIAN_POINT('Ctrl Pts',(-0.110430344000055,12.2,-4.04634338900001));
#326754=CARTESIAN_POINT('Ctrl Pts',(-0.110430344000055,5.2,-4.04634338900001));
#326755=CARTESIAN_POINT('Ctrl Pts',(-0.110430344000055,2.2,-4.04634338900001));
#326756=CARTESIAN_POINT('Ctrl Pts',(-0.110316801000057,12.2,-4.04716635400002));
#326757=CARTESIAN_POINT('Ctrl Pts',(-0.110316801000057,5.2,-4.04716635400002));
#326758=CARTESIAN_POINT('Ctrl Pts',(-0.110316801000057,2.2,-4.04716635400002));
#326759=CARTESIAN_POINT('Ctrl Pts',(-0.110201430000056,12.2,-4.04799489100002));
#326760=CARTESIAN_POINT('Ctrl Pts',(-0.110201430000056,5.2,-4.04799489100002));
#326761=CARTESIAN_POINT('Ctrl Pts',(-0.110201430000056,2.2,-4.04799489100002));
#326762=CARTESIAN_POINT('Ctrl Pts',(-0.110084220000056,12.2,-4.04882898600002));
#326763=CARTESIAN_POINT('Ctrl Pts',(-0.110084220000056,5.2,-4.04882898600002));
#326764=CARTESIAN_POINT('Ctrl Pts',(-0.110084220000056,2.2,-4.04882898600002));
#326765=CARTESIAN_POINT('Ctrl Pts',(-0.109965157000056,12.2,-4.04966862700002));
#326766=CARTESIAN_POINT('Ctrl Pts',(-0.109965157000056,5.2,-4.04966862700002));
#326767=CARTESIAN_POINT('Ctrl Pts',(-0.109965157000056,2.2,-4.04966862700002));
#326768=CARTESIAN_POINT('Ctrl Pts',(-0.109844232000055,12.2,-4.05051379900002));
#326769=CARTESIAN_POINT('Ctrl Pts',(-0.109844232000055,5.2,-4.05051379900002));
#326770=CARTESIAN_POINT('Ctrl Pts',(-0.109844232000055,2.2,-4.05051379900002));
#326771=CARTESIAN_POINT('Ctrl Pts',(-0.109721430000055,12.2,-4.05136449100001));
#326772=CARTESIAN_POINT('Ctrl Pts',(-0.109721430000055,5.2,-4.05136449100001));
#326773=CARTESIAN_POINT('Ctrl Pts',(-0.109721430000055,2.2,-4.05136449100001));
#326774=CARTESIAN_POINT('Ctrl Pts',(-0.109596742000055,12.2,-4.05222068700001));
#326775=CARTESIAN_POINT('Ctrl Pts',(-0.109596742000055,5.2,-4.05222068700001));
#326776=CARTESIAN_POINT('Ctrl Pts',(-0.109596742000055,2.2,-4.05222068700001));
#326777=CARTESIAN_POINT('Ctrl Pts',(-0.109470154000055,12.2,-4.05308237500002));
#326778=CARTESIAN_POINT('Ctrl Pts',(-0.109470154000055,5.2,-4.05308237500002));
#326779=CARTESIAN_POINT('Ctrl Pts',(-0.109470154000055,2.2,-4.05308237500002));
#326780=CARTESIAN_POINT('Ctrl Pts',(-0.109341655000056,12.2,-4.05394954200001));
#326781=CARTESIAN_POINT('Ctrl Pts',(-0.109341655000056,5.2,-4.05394954200001));
#326782=CARTESIAN_POINT('Ctrl Pts',(-0.109341655000056,2.2,-4.05394954200001));
#326783=CARTESIAN_POINT('Ctrl Pts',(-0.109211234000056,12.2,-4.05482217500001));
#326784=CARTESIAN_POINT('Ctrl Pts',(-0.109211234000056,5.2,-4.05482217500001));
#326785=CARTESIAN_POINT('Ctrl Pts',(-0.109211234000056,2.2,-4.05482217500001));
#326786=CARTESIAN_POINT('Ctrl Pts',(-0.109078877000056,12.2,-4.05570026000001));
#326787=CARTESIAN_POINT('Ctrl Pts',(-0.109078877000056,5.2,-4.05570026000001));
#326788=CARTESIAN_POINT('Ctrl Pts',(-0.109078877000056,2.2,-4.05570026000001));
#326789=CARTESIAN_POINT('Ctrl Pts',(-0.108944575000055,12.2,-4.05658378600001));
#326790=CARTESIAN_POINT('Ctrl Pts',(-0.108944575000055,5.2,-4.05658378600001));
#326791=CARTESIAN_POINT('Ctrl Pts',(-0.108944575000055,2.2,-4.05658378600001));
#326792=CARTESIAN_POINT('Ctrl Pts',(-0.108808314000056,12.2,-4.05747273700001));
#326793=CARTESIAN_POINT('Ctrl Pts',(-0.108808314000056,5.2,-4.05747273700001));
#326794=CARTESIAN_POINT('Ctrl Pts',(-0.108808314000056,2.2,-4.05747273700001));
#326795=CARTESIAN_POINT('Ctrl Pts',(-0.108670085000057,12.2,-4.05836710200001));
#326796=CARTESIAN_POINT('Ctrl Pts',(-0.108670085000057,5.2,-4.05836710200001));
#326797=CARTESIAN_POINT('Ctrl Pts',(-0.108670085000057,2.2,-4.05836710200001));
#326798=CARTESIAN_POINT('Ctrl Pts',(-0.108529875000055,12.2,-4.05926686700001));
#326799=CARTESIAN_POINT('Ctrl Pts',(-0.108529875000055,5.2,-4.05926686700001));
#326800=CARTESIAN_POINT('Ctrl Pts',(-0.108529875000055,2.2,-4.05926686700001));
#326801=CARTESIAN_POINT('Ctrl Pts',(-0.108387672000055,12.2,-4.06017201800001));
#326802=CARTESIAN_POINT('Ctrl Pts',(-0.108387672000055,5.2,-4.06017201800001));
#326803=CARTESIAN_POINT('Ctrl Pts',(-0.108387672000055,2.2,-4.06017201800001));
#326804=CARTESIAN_POINT('Ctrl Pts',(-0.108243465000056,12.2,-4.06108254500001));
#326805=CARTESIAN_POINT('Ctrl Pts',(-0.108243465000056,5.2,-4.06108254500001));
#326806=CARTESIAN_POINT('Ctrl Pts',(-0.108243465000056,2.2,-4.06108254500001));
#326807=CARTESIAN_POINT('Ctrl Pts',(-0.108097244000056,12.2,-4.06199843200001));
#326808=CARTESIAN_POINT('Ctrl Pts',(-0.108097244000056,5.2,-4.06199843200001));
#326809=CARTESIAN_POINT('Ctrl Pts',(-0.108097244000056,2.2,-4.06199843200001));
#326810=CARTESIAN_POINT('Ctrl Pts',(-0.107948995000056,12.2,-4.06291966700001));
#326811=CARTESIAN_POINT('Ctrl Pts',(-0.107948995000056,5.2,-4.06291966700001));
#326812=CARTESIAN_POINT('Ctrl Pts',(-0.107948995000056,2.2,-4.06291966700001));
#326813=CARTESIAN_POINT('Ctrl Pts',(-0.107798709000055,12.2,-4.06384623800002));
#326814=CARTESIAN_POINT('Ctrl Pts',(-0.107798709000055,5.2,-4.06384623800002));
#326815=CARTESIAN_POINT('Ctrl Pts',(-0.107798709000055,2.2,-4.06384623800002));
#326816=CARTESIAN_POINT('Ctrl Pts',(-0.107646374000057,12.2,-4.06477813000001));
#326817=CARTESIAN_POINT('Ctrl Pts',(-0.107646374000057,5.2,-4.06477813000001));
#326818=CARTESIAN_POINT('Ctrl Pts',(-0.107646374000057,2.2,-4.06477813000001));
#326819=CARTESIAN_POINT('Ctrl Pts',(-0.107491979000055,12.2,-4.06571533200002));
#326820=CARTESIAN_POINT('Ctrl Pts',(-0.107491979000055,5.2,-4.06571533200002));
#326821=CARTESIAN_POINT('Ctrl Pts',(-0.107491979000055,2.2,-4.06571533200002));
#326822=CARTESIAN_POINT('Ctrl Pts',(-0.107335513000055,12.2,-4.06665783000001));
#326823=CARTESIAN_POINT('Ctrl Pts',(-0.107335513000055,5.2,-4.06665783000001));
#326824=CARTESIAN_POINT('Ctrl Pts',(-0.107335513000055,2.2,-4.06665783000001));
#326825=CARTESIAN_POINT('Ctrl Pts',(-0.107176964000055,12.2,-4.06760561100001));
#326826=CARTESIAN_POINT('Ctrl Pts',(-0.107176964000055,5.2,-4.06760561100001));
#326827=CARTESIAN_POINT('Ctrl Pts',(-0.107176964000055,2.2,-4.06760561100001));
#326828=CARTESIAN_POINT('Ctrl Pts',(-0.107016321000056,12.2,-4.06855866300001));
#326829=CARTESIAN_POINT('Ctrl Pts',(-0.107016321000056,5.2,-4.06855866300001));
#326830=CARTESIAN_POINT('Ctrl Pts',(-0.107016321000056,2.2,-4.06855866300001));
#326831=CARTESIAN_POINT('Ctrl Pts',(-0.106853574000055,12.2,-4.06951697300002));
#326832=CARTESIAN_POINT('Ctrl Pts',(-0.106853574000055,5.2,-4.06951697300002));
#326833=CARTESIAN_POINT('Ctrl Pts',(-0.106853574000055,2.2,-4.06951697300002));
#326834=CARTESIAN_POINT('Ctrl Pts',(-0.106688711000055,12.2,-4.07048052800001));
#326835=CARTESIAN_POINT('Ctrl Pts',(-0.106688711000055,5.2,-4.07048052800001));
#326836=CARTESIAN_POINT('Ctrl Pts',(-0.106688711000055,2.2,-4.07048052800001));
#326837=CARTESIAN_POINT('Ctrl Pts',(-0.106521723000055,12.2,-4.07144931400001));
#326838=CARTESIAN_POINT('Ctrl Pts',(-0.106521723000055,5.2,-4.07144931400001));
#326839=CARTESIAN_POINT('Ctrl Pts',(-0.106521723000055,2.2,-4.07144931400001));
#326840=CARTESIAN_POINT('Ctrl Pts',(-0.106352597000056,12.2,-4.07242332000001));
#326841=CARTESIAN_POINT('Ctrl Pts',(-0.106352597000056,5.2,-4.07242332000001));
#326842=CARTESIAN_POINT('Ctrl Pts',(-0.106352597000056,2.2,-4.07242332000001));
#326843=CARTESIAN_POINT('Ctrl Pts',(-0.106181322000056,12.2,-4.07340253300001));
#326844=CARTESIAN_POINT('Ctrl Pts',(-0.106181322000056,5.2,-4.07340253300001));
#326845=CARTESIAN_POINT('Ctrl Pts',(-0.106181322000056,2.2,-4.07340253300001));
#326846=CARTESIAN_POINT('Ctrl Pts',(-0.106007888000056,12.2,-4.07438693900001));
#326847=CARTESIAN_POINT('Ctrl Pts',(-0.106007888000056,5.2,-4.07438693900001));
#326848=CARTESIAN_POINT('Ctrl Pts',(-0.106007888000056,2.2,-4.07438693900001));
#326849=CARTESIAN_POINT('Ctrl Pts',(-0.105832285000057,12.2,-4.07537652600002));
#326850=CARTESIAN_POINT('Ctrl Pts',(-0.105832285000057,5.2,-4.07537652600002));
#326851=CARTESIAN_POINT('Ctrl Pts',(-0.105832285000057,2.2,-4.07537652600002));
#326852=CARTESIAN_POINT('Ctrl Pts',(-0.105654502000055,12.2,-4.07637128100002));
#326853=CARTESIAN_POINT('Ctrl Pts',(-0.105654502000055,5.2,-4.07637128100002));
#326854=CARTESIAN_POINT('Ctrl Pts',(-0.105654502000055,2.2,-4.07637128100002));
#326855=CARTESIAN_POINT('Ctrl Pts',(-0.105474527000055,12.2,-4.07737119100001));
#326856=CARTESIAN_POINT('Ctrl Pts',(-0.105474527000055,5.2,-4.07737119100001));
#326857=CARTESIAN_POINT('Ctrl Pts',(-0.105474527000055,2.2,-4.07737119100001));
#326858=CARTESIAN_POINT('Ctrl Pts',(-0.105292351000056,12.2,-4.07837624500001));
#326859=CARTESIAN_POINT('Ctrl Pts',(-0.105292351000056,5.2,-4.07837624500001));
#326860=CARTESIAN_POINT('Ctrl Pts',(-0.105292351000056,2.2,-4.07837624500001));
#326861=CARTESIAN_POINT('Ctrl Pts',(-0.105107963000056,12.2,-4.07938642800001));
#326862=CARTESIAN_POINT('Ctrl Pts',(-0.105107963000056,5.2,-4.07938642800001));
#326863=CARTESIAN_POINT('Ctrl Pts',(-0.105107963000056,2.2,-4.07938642800001));
#326864=CARTESIAN_POINT('Ctrl Pts',(-0.104921351000057,12.2,-4.08040173000002));
#326865=CARTESIAN_POINT('Ctrl Pts',(-0.104921351000057,5.2,-4.08040173000002));
#326866=CARTESIAN_POINT('Ctrl Pts',(-0.104921351000057,2.2,-4.08040173000002));
#326867=CARTESIAN_POINT('Ctrl Pts',(-0.104732506000056,12.2,-4.08142213600001));
#326868=CARTESIAN_POINT('Ctrl Pts',(-0.104732506000056,5.2,-4.08142213600001));
#326869=CARTESIAN_POINT('Ctrl Pts',(-0.104732506000056,2.2,-4.08142213600001));
#326870=CARTESIAN_POINT('Ctrl Pts',(-0.104541418000055,12.2,-4.08244763400001));
#326871=CARTESIAN_POINT('Ctrl Pts',(-0.104541418000055,5.2,-4.08244763400001));
#326872=CARTESIAN_POINT('Ctrl Pts',(-0.104541418000055,2.2,-4.08244763400001));
#326873=CARTESIAN_POINT('Ctrl Pts',(-0.104348076000056,12.2,-4.08347821100001));
#326874=CARTESIAN_POINT('Ctrl Pts',(-0.104348076000056,5.2,-4.08347821100001));
#326875=CARTESIAN_POINT('Ctrl Pts',(-0.104348076000056,2.2,-4.08347821100001));
#326876=CARTESIAN_POINT('Ctrl Pts',(-0.104152469000055,12.2,-4.08451385700001));
#326877=CARTESIAN_POINT('Ctrl Pts',(-0.104152469000055,5.2,-4.08451385700001));
#326878=CARTESIAN_POINT('Ctrl Pts',(-0.104152469000055,2.2,-4.08451385700001));
#326879=CARTESIAN_POINT('Ctrl Pts',(-0.103954586000056,12.2,-4.08555455600002));
#326880=CARTESIAN_POINT('Ctrl Pts',(-0.103954586000056,5.2,-4.08555455600002));
#326881=CARTESIAN_POINT('Ctrl Pts',(-0.103954586000056,2.2,-4.08555455600002));
#326882=CARTESIAN_POINT('Ctrl Pts',(-0.103754419000056,12.2,-4.08660029800001));
#326883=CARTESIAN_POINT('Ctrl Pts',(-0.103754419000056,5.2,-4.08660029800001));
#326884=CARTESIAN_POINT('Ctrl Pts',(-0.103754419000056,2.2,-4.08660029800001));
#326885=CARTESIAN_POINT('Ctrl Pts',(-0.103551956000055,12.2,-4.08765106800002));
#326886=CARTESIAN_POINT('Ctrl Pts',(-0.103551956000055,5.2,-4.08765106800002));
#326887=CARTESIAN_POINT('Ctrl Pts',(-0.103551956000055,2.2,-4.08765106800002));
#326888=CARTESIAN_POINT('Ctrl Pts',(-0.103347188000056,12.2,-4.08870685700002));
#326889=CARTESIAN_POINT('Ctrl Pts',(-0.103347188000056,5.2,-4.08870685700002));
#326890=CARTESIAN_POINT('Ctrl Pts',(-0.103347188000056,2.2,-4.08870685700002));
#326891=CARTESIAN_POINT('Ctrl Pts',(-0.103140103000056,12.2,-4.08976764800002));
#326892=CARTESIAN_POINT('Ctrl Pts',(-0.103140103000056,5.2,-4.08976764800002));
#326893=CARTESIAN_POINT('Ctrl Pts',(-0.103140103000056,2.2,-4.08976764800002));
#326894=CARTESIAN_POINT('Ctrl Pts',(-0.102930694000056,12.2,-4.09083343200002));
#326895=CARTESIAN_POINT('Ctrl Pts',(-0.102930694000056,5.2,-4.09083343200002));
#326896=CARTESIAN_POINT('Ctrl Pts',(-0.102930694000056,2.2,-4.09083343200002));
#326897=CARTESIAN_POINT('Ctrl Pts',(-0.102718947000057,12.2,-4.09190419600002));
#326898=CARTESIAN_POINT('Ctrl Pts',(-0.102718947000057,5.2,-4.09190419600002));
#326899=CARTESIAN_POINT('Ctrl Pts',(-0.102718947000057,2.2,-4.09190419600002));
#326900=CARTESIAN_POINT('Ctrl Pts',(-0.102504855000056,12.2,-4.09297992600001));
#326901=CARTESIAN_POINT('Ctrl Pts',(-0.102504855000056,5.2,-4.09297992600001));
#326902=CARTESIAN_POINT('Ctrl Pts',(-0.102504855000056,2.2,-4.09297992600001));
#326903=CARTESIAN_POINT('Ctrl Pts',(-0.102288407000056,12.2,-4.09406061100002));
#326904=CARTESIAN_POINT('Ctrl Pts',(-0.102288407000056,5.2,-4.09406061100002));
#326905=CARTESIAN_POINT('Ctrl Pts',(-0.102288407000056,2.2,-4.09406061100002));
#326906=CARTESIAN_POINT('Ctrl Pts',(-0.102069593000056,12.2,-4.09514623900002));
#326907=CARTESIAN_POINT('Ctrl Pts',(-0.102069593000056,5.2,-4.09514623900002));
#326908=CARTESIAN_POINT('Ctrl Pts',(-0.102069593000056,2.2,-4.09514623900002));
#326909=CARTESIAN_POINT('Ctrl Pts',(-0.101848403000057,12.2,-4.09623679600001));
#326910=CARTESIAN_POINT('Ctrl Pts',(-0.101848403000057,5.2,-4.09623679600001));
#326911=CARTESIAN_POINT('Ctrl Pts',(-0.101848403000057,2.2,-4.09623679600001));
#326912=CARTESIAN_POINT('Ctrl Pts',(-0.101624827000055,12.2,-4.09733227000002));
#326913=CARTESIAN_POINT('Ctrl Pts',(-0.101624827000055,5.2,-4.09733227000002));
#326914=CARTESIAN_POINT('Ctrl Pts',(-0.101624827000055,2.2,-4.09733227000002));
#326915=CARTESIAN_POINT('Ctrl Pts',(-0.101398855000056,12.2,-4.09843264900001));
#326916=CARTESIAN_POINT('Ctrl Pts',(-0.101398855000056,5.2,-4.09843264900001));
#326917=CARTESIAN_POINT('Ctrl Pts',(-0.101398855000056,2.2,-4.09843264900001));
#326918=CARTESIAN_POINT('Ctrl Pts',(-0.101170479000056,12.2,-4.09953792200001));
#326919=CARTESIAN_POINT('Ctrl Pts',(-0.101170479000056,5.2,-4.09953792200001));
#326920=CARTESIAN_POINT('Ctrl Pts',(-0.101170479000056,2.2,-4.09953792200001));
#326921=CARTESIAN_POINT('Ctrl Pts',(-0.100939686000056,12.2,-4.10064807500001));
#326922=CARTESIAN_POINT('Ctrl Pts',(-0.100939686000056,5.2,-4.10064807500001));
#326923=CARTESIAN_POINT('Ctrl Pts',(-0.100939686000056,2.2,-4.10064807500001));
#326924=CARTESIAN_POINT('Ctrl Pts',(-0.100706469000055,12.2,-4.10176309600002));
#326925=CARTESIAN_POINT('Ctrl Pts',(-0.100706469000055,5.2,-4.10176309600002));
#326926=CARTESIAN_POINT('Ctrl Pts',(-0.100706469000055,2.2,-4.10176309600002));
#326927=CARTESIAN_POINT('Ctrl Pts',(-0.100470817000057,12.2,-4.10288297300001));
#326928=CARTESIAN_POINT('Ctrl Pts',(-0.100470817000057,5.2,-4.10288297300001));
#326929=CARTESIAN_POINT('Ctrl Pts',(-0.100470817000057,2.2,-4.10288297300001));
#326930=CARTESIAN_POINT('Ctrl Pts',(-0.100232720000056,12.2,-4.10400769300002));
#326931=CARTESIAN_POINT('Ctrl Pts',(-0.100232720000056,5.2,-4.10400769300002));
#326932=CARTESIAN_POINT('Ctrl Pts',(-0.100232720000056,2.2,-4.10400769300002));
#326933=CARTESIAN_POINT('Ctrl Pts',(-0.0999921710000551,12.2,-4.10513724500001));
#326934=CARTESIAN_POINT('Ctrl Pts',(-0.0999921710000551,5.2,-4.10513724500001));
#326935=CARTESIAN_POINT('Ctrl Pts',(-0.0999921710000551,2.2,-4.10513724500001));
#326936=CARTESIAN_POINT('Ctrl Pts',(-0.0997491570000564,12.2,-4.10627161500001));
#326937=CARTESIAN_POINT('Ctrl Pts',(-0.0997491570000564,5.2,-4.10627161500001));
#326938=CARTESIAN_POINT('Ctrl Pts',(-0.0997491570000564,2.2,-4.10627161500001));
#326939=CARTESIAN_POINT('Ctrl Pts',(-0.0995036710000552,12.2,-4.10741079300001));
#326940=CARTESIAN_POINT('Ctrl Pts',(-0.0995036710000552,5.2,-4.10741079300001));
#326941=CARTESIAN_POINT('Ctrl Pts',(-0.0995036710000552,2.2,-4.10741079300001));
#326942=CARTESIAN_POINT('Ctrl Pts',(-0.099255701000055,12.2,-4.10855476500001));
#326943=CARTESIAN_POINT('Ctrl Pts',(-0.099255701000055,5.2,-4.10855476500001));
#326944=CARTESIAN_POINT('Ctrl Pts',(-0.099255701000055,2.2,-4.10855476500001));
#326945=CARTESIAN_POINT('Ctrl Pts',(-0.0990052400000552,12.2,-4.10970351900001));
#326946=CARTESIAN_POINT('Ctrl Pts',(-0.0990052400000552,5.2,-4.10970351900001));
#326947=CARTESIAN_POINT('Ctrl Pts',(-0.0990052400000552,2.2,-4.10970351900001));
#326948=CARTESIAN_POINT('Ctrl Pts',(-0.098752278000056,12.2,-4.11085704400001));
#326949=CARTESIAN_POINT('Ctrl Pts',(-0.098752278000056,5.2,-4.11085704400001));
#326950=CARTESIAN_POINT('Ctrl Pts',(-0.098752278000056,2.2,-4.11085704400001));
#326951=CARTESIAN_POINT('Ctrl Pts',(-0.0984968050000568,12.2,-4.11201532700002));
#326952=CARTESIAN_POINT('Ctrl Pts',(-0.0984968050000568,5.2,-4.11201532700002));
#326953=CARTESIAN_POINT('Ctrl Pts',(-0.0984968050000568,2.2,-4.11201532700002));
#326954=CARTESIAN_POINT('Ctrl Pts',(-0.0982388110000565,12.2,-4.11317835500002));
#326955=CARTESIAN_POINT('Ctrl Pts',(-0.0982388110000565,5.2,-4.11317835500002));
#326956=CARTESIAN_POINT('Ctrl Pts',(-0.0982388110000565,2.2,-4.11317835500002));
#326957=CARTESIAN_POINT('Ctrl Pts',(-0.0979782880000546,12.2,-4.11434611800002));
#326958=CARTESIAN_POINT('Ctrl Pts',(-0.0979782880000546,5.2,-4.11434611800002));
#326959=CARTESIAN_POINT('Ctrl Pts',(-0.0979782880000546,2.2,-4.11434611800002));
#326960=CARTESIAN_POINT('Ctrl Pts',(-0.0977152270000547,12.2,-4.11551860300001));
#326961=CARTESIAN_POINT('Ctrl Pts',(-0.0977152270000547,5.2,-4.11551860300001));
#326962=CARTESIAN_POINT('Ctrl Pts',(-0.0977152270000547,2.2,-4.11551860300001));
#326963=CARTESIAN_POINT('Ctrl Pts',(-0.097449618000055,12.2,-4.11669579600002));
#326964=CARTESIAN_POINT('Ctrl Pts',(-0.097449618000055,5.2,-4.11669579600002));
#326965=CARTESIAN_POINT('Ctrl Pts',(-0.097449618000055,2.2,-4.11669579600002));
#326966=CARTESIAN_POINT('Ctrl Pts',(-0.0971814510000557,12.2,-4.11787768800002));
#326967=CARTESIAN_POINT('Ctrl Pts',(-0.0971814510000557,5.2,-4.11787768800002));
#326968=CARTESIAN_POINT('Ctrl Pts',(-0.0971814510000557,2.2,-4.11787768800002));
#326969=CARTESIAN_POINT('Ctrl Pts',(-0.096910718000055,12.2,-4.11906426500002));
#326970=CARTESIAN_POINT('Ctrl Pts',(-0.096910718000055,5.2,-4.11906426500002));
#326971=CARTESIAN_POINT('Ctrl Pts',(-0.096910718000055,2.2,-4.11906426500002));
#326972=CARTESIAN_POINT('Ctrl Pts',(-0.0966374100000567,12.2,-4.12025551500002));
#326973=CARTESIAN_POINT('Ctrl Pts',(-0.0966374100000567,5.2,-4.12025551500002));
#326974=CARTESIAN_POINT('Ctrl Pts',(-0.0966374100000567,2.2,-4.12025551500002));
#326975=CARTESIAN_POINT('Ctrl Pts',(-0.0963615180000554,12.2,-4.12145142700002));
#326976=CARTESIAN_POINT('Ctrl Pts',(-0.0963615180000554,5.2,-4.12145142700002));
#326977=CARTESIAN_POINT('Ctrl Pts',(-0.0963615180000554,2.2,-4.12145142700002));
#326978=CARTESIAN_POINT('Ctrl Pts',(-0.096083031000056,12.2,-4.12265198800001));
#326979=CARTESIAN_POINT('Ctrl Pts',(-0.096083031000056,5.2,-4.12265198800001));
#326980=CARTESIAN_POINT('Ctrl Pts',(-0.096083031000056,2.2,-4.12265198800001));
#326981=CARTESIAN_POINT('Ctrl Pts',(-0.0958019420000567,12.2,-4.12385718700001));
#326982=CARTESIAN_POINT('Ctrl Pts',(-0.0958019420000567,5.2,-4.12385718700001));
#326983=CARTESIAN_POINT('Ctrl Pts',(-0.0958019420000567,2.2,-4.12385718700001));
#326984=CARTESIAN_POINT('Ctrl Pts',(-0.0955182420000555,12.2,-4.12506701100002));
#326985=CARTESIAN_POINT('Ctrl Pts',(-0.0955182420000555,5.2,-4.12506701100002));
#326986=CARTESIAN_POINT('Ctrl Pts',(-0.0955182420000555,2.2,-4.12506701100002));
#326987=CARTESIAN_POINT('Ctrl Pts',(-0.0952319210000563,12.2,-4.12628144800002));
#326988=CARTESIAN_POINT('Ctrl Pts',(-0.0952319210000563,5.2,-4.12628144800002));
#326989=CARTESIAN_POINT('Ctrl Pts',(-0.0952319210000563,2.2,-4.12628144800002));
#326990=CARTESIAN_POINT('Ctrl Pts',(-0.094942972000055,12.2,-4.12750048600001));
#326991=CARTESIAN_POINT('Ctrl Pts',(-0.094942972000055,5.2,-4.12750048600001));
#326992=CARTESIAN_POINT('Ctrl Pts',(-0.094942972000055,2.2,-4.12750048600001));
#326993=CARTESIAN_POINT('Ctrl Pts',(-0.094651383000055,12.2,-4.12872411500001));
#326994=CARTESIAN_POINT('Ctrl Pts',(-0.094651383000055,5.2,-4.12872411500001));
#326995=CARTESIAN_POINT('Ctrl Pts',(-0.094651383000055,2.2,-4.12872411500001));
#326996=CARTESIAN_POINT('Ctrl Pts',(-0.0943571480000549,12.2,-4.12995232000001));
#326997=CARTESIAN_POINT('Ctrl Pts',(-0.0943571480000549,5.2,-4.12995232000001));
#326998=CARTESIAN_POINT('Ctrl Pts',(-0.0943571480000549,2.2,-4.12995232000001));
#326999=CARTESIAN_POINT('Ctrl Pts',(-0.0940602560000559,12.2,-4.13118509300002));
#327000=CARTESIAN_POINT('Ctrl Pts',(-0.0940602560000559,5.2,-4.13118509300002));
#327001=CARTESIAN_POINT('Ctrl Pts',(-0.0940602560000559,2.2,-4.13118509300002));
#327002=CARTESIAN_POINT('Ctrl Pts',(-0.0937607010000552,12.2,-4.13242241800001));
#327003=CARTESIAN_POINT('Ctrl Pts',(-0.0937607010000552,5.2,-4.13242241800001));
#327004=CARTESIAN_POINT('Ctrl Pts',(-0.0937607010000552,2.2,-4.13242241800001));
#327005=CARTESIAN_POINT('Ctrl Pts',(-0.0934584710000563,12.2,-4.13366428600002));
#327006=CARTESIAN_POINT('Ctrl Pts',(-0.0934584710000563,5.2,-4.13366428600002));
#327007=CARTESIAN_POINT('Ctrl Pts',(-0.0934584710000563,2.2,-4.13366428600002));
#327008=CARTESIAN_POINT('Ctrl Pts',(-0.0931535600000555,12.2,-4.13491068300001));
#327009=CARTESIAN_POINT('Ctrl Pts',(-0.0931535600000555,5.2,-4.13491068300001));
#327010=CARTESIAN_POINT('Ctrl Pts',(-0.0931535600000555,2.2,-4.13491068300001));
#327011=CARTESIAN_POINT('Ctrl Pts',(-0.0928459580000562,12.2,-4.13616159800001));
#327012=CARTESIAN_POINT('Ctrl Pts',(-0.0928459580000562,5.2,-4.13616159800001));
#327013=CARTESIAN_POINT('Ctrl Pts',(-0.0928459580000562,2.2,-4.13616159800001));
#327014=CARTESIAN_POINT('Ctrl Pts',(-0.0925356570000557,12.2,-4.13741702000001));
#327015=CARTESIAN_POINT('Ctrl Pts',(-0.0925356570000557,5.2,-4.13741702000001));
#327016=CARTESIAN_POINT('Ctrl Pts',(-0.0925356570000557,2.2,-4.13741702000001));
#327017=CARTESIAN_POINT('Ctrl Pts',(-0.0922226470000564,12.2,-4.13867693700002));
#327018=CARTESIAN_POINT('Ctrl Pts',(-0.0922226470000564,5.2,-4.13867693700002));
#327019=CARTESIAN_POINT('Ctrl Pts',(-0.0922226470000564,2.2,-4.13867693700002));
#327020=CARTESIAN_POINT('Ctrl Pts',(-0.0919069210000567,12.2,-4.13994133600001));
#327021=CARTESIAN_POINT('Ctrl Pts',(-0.0919069210000567,5.2,-4.13994133600001));
#327022=CARTESIAN_POINT('Ctrl Pts',(-0.0919069210000567,2.2,-4.13994133600001));
#327023=CARTESIAN_POINT('Ctrl Pts',(-0.0915884700000558,12.2,-4.14121020700001));
#327024=CARTESIAN_POINT('Ctrl Pts',(-0.0915884700000558,5.2,-4.14121020700001));
#327025=CARTESIAN_POINT('Ctrl Pts',(-0.0915884700000558,2.2,-4.14121020700001));
#327026=CARTESIAN_POINT('Ctrl Pts',(-0.0912672860000552,12.2,-4.14248353600001));
#327027=CARTESIAN_POINT('Ctrl Pts',(-0.0912672860000552,5.2,-4.14248353600001));
#327028=CARTESIAN_POINT('Ctrl Pts',(-0.0912672860000552,2.2,-4.14248353600001));
#327029=CARTESIAN_POINT('Ctrl Pts',(-0.0909433590000552,12.2,-4.14376131300001));
#327030=CARTESIAN_POINT('Ctrl Pts',(-0.0909433590000552,5.2,-4.14376131300001));
#327031=CARTESIAN_POINT('Ctrl Pts',(-0.0909433590000552,2.2,-4.14376131300001));
#327032=CARTESIAN_POINT('Ctrl Pts',(-0.0906166830000554,12.2,-4.14504352500002));
#327033=CARTESIAN_POINT('Ctrl Pts',(-0.0906166830000554,5.2,-4.14504352500002));
#327034=CARTESIAN_POINT('Ctrl Pts',(-0.0906166830000554,2.2,-4.14504352500002));
#327035=CARTESIAN_POINT('Ctrl Pts',(-0.0902872480000561,12.2,-4.14633016200002));
#327036=CARTESIAN_POINT('Ctrl Pts',(-0.0902872480000561,5.2,-4.14633016200002));
#327037=CARTESIAN_POINT('Ctrl Pts',(-0.0902872480000561,2.2,-4.14633016200002));
#327038=CARTESIAN_POINT('Ctrl Pts',(-0.0899550450000564,12.2,-4.14762121100001));
#327039=CARTESIAN_POINT('Ctrl Pts',(-0.0899550450000564,5.2,-4.14762121100001));
#327040=CARTESIAN_POINT('Ctrl Pts',(-0.0899550450000564,2.2,-4.14762121100001));
#327041=CARTESIAN_POINT('Ctrl Pts',(-0.0896200680000547,12.2,-4.14891666000001));
#327042=CARTESIAN_POINT('Ctrl Pts',(-0.0896200680000547,5.2,-4.14891666000001));
#327043=CARTESIAN_POINT('Ctrl Pts',(-0.0896200680000547,2.2,-4.14891666000001));
#327044=CARTESIAN_POINT('Ctrl Pts',(-0.0892823060000558,12.2,-4.15021649900002));
#327045=CARTESIAN_POINT('Ctrl Pts',(-0.0892823060000558,5.2,-4.15021649900002));
#327046=CARTESIAN_POINT('Ctrl Pts',(-0.0892823060000558,2.2,-4.15021649900002));
#327047=CARTESIAN_POINT('Ctrl Pts',(-0.0889417520000546,12.2,-4.15152071400001));
#327048=CARTESIAN_POINT('Ctrl Pts',(-0.0889417520000546,5.2,-4.15152071400001));
#327049=CARTESIAN_POINT('Ctrl Pts',(-0.0889417520000546,2.2,-4.15152071400001));
#327050=CARTESIAN_POINT('Ctrl Pts',(-0.0885983980000549,12.2,-4.15282929600002));
#327051=CARTESIAN_POINT('Ctrl Pts',(-0.0885983980000549,5.2,-4.15282929600002));
#327052=CARTESIAN_POINT('Ctrl Pts',(-0.0885983980000549,2.2,-4.15282929600002));
#327053=CARTESIAN_POINT('Ctrl Pts',(-0.0882522360000559,12.2,-4.15414223000001));
#327054=CARTESIAN_POINT('Ctrl Pts',(-0.0882522360000559,5.2,-4.15414223000001));
#327055=CARTESIAN_POINT('Ctrl Pts',(-0.0882522360000559,2.2,-4.15414223000001));
#327056=CARTESIAN_POINT('Ctrl Pts',(-0.0879032580000561,12.2,-4.15545950800002));
#327057=CARTESIAN_POINT('Ctrl Pts',(-0.0879032580000561,5.2,-4.15545950800002));
#327058=CARTESIAN_POINT('Ctrl Pts',(-0.0879032580000561,2.2,-4.15545950800002));
#327059=CARTESIAN_POINT('Ctrl Pts',(-0.0875514550000567,12.2,-4.15678111500001));
#327060=CARTESIAN_POINT('Ctrl Pts',(-0.0875514550000567,5.2,-4.15678111500001));
#327061=CARTESIAN_POINT('Ctrl Pts',(-0.0875514550000567,2.2,-4.15678111500001));
#327062=CARTESIAN_POINT('Ctrl Pts',(-0.087196818000056,12.2,-4.15810704200001));
#327063=CARTESIAN_POINT('Ctrl Pts',(-0.087196818000056,5.2,-4.15810704200001));
#327064=CARTESIAN_POINT('Ctrl Pts',(-0.087196818000056,2.2,-4.15810704200001));
#327065=CARTESIAN_POINT('Ctrl Pts',(-0.0868393420000557,12.2,-4.15943727600002));
#327066=CARTESIAN_POINT('Ctrl Pts',(-0.0868393420000557,5.2,-4.15943727600002));
#327067=CARTESIAN_POINT('Ctrl Pts',(-0.0868393420000557,2.2,-4.15943727600002));
#327068=CARTESIAN_POINT('Ctrl Pts',(-0.086479016000055,12.2,-4.16077180600002));
#327069=CARTESIAN_POINT('Ctrl Pts',(-0.086479016000055,5.2,-4.16077180600002));
#327070=CARTESIAN_POINT('Ctrl Pts',(-0.086479016000055,2.2,-4.16077180600002));
#327071=CARTESIAN_POINT('Ctrl Pts',(-0.0861158340000556,12.2,-4.16211062100002));
#327072=CARTESIAN_POINT('Ctrl Pts',(-0.0861158340000556,5.2,-4.16211062100002));
#327073=CARTESIAN_POINT('Ctrl Pts',(-0.0861158340000556,2.2,-4.16211062100002));
#327074=CARTESIAN_POINT('Ctrl Pts',(-0.0857497870000556,12.2,-4.16345370800002));
#327075=CARTESIAN_POINT('Ctrl Pts',(-0.0857497870000556,5.2,-4.16345370800002));
#327076=CARTESIAN_POINT('Ctrl Pts',(-0.0857497870000556,2.2,-4.16345370800002));
#327077=CARTESIAN_POINT('Ctrl Pts',(-0.0853808670000566,12.2,-4.16480105700002));
#327078=CARTESIAN_POINT('Ctrl Pts',(-0.0853808670000566,5.2,-4.16480105700002));
#327079=CARTESIAN_POINT('Ctrl Pts',(-0.0853808670000566,2.2,-4.16480105700002));
#327080=CARTESIAN_POINT('Ctrl Pts',(-0.0850090670000558,12.2,-4.16615265500001));
#327081=CARTESIAN_POINT('Ctrl Pts',(-0.0850090670000558,5.2,-4.16615265500001));
#327082=CARTESIAN_POINT('Ctrl Pts',(-0.0850090670000558,2.2,-4.16615265500001));
#327083=CARTESIAN_POINT('Ctrl Pts',(-0.0846343790000559,12.2,-4.16750849100001));
#327084=CARTESIAN_POINT('Ctrl Pts',(-0.0846343790000559,5.2,-4.16750849100001));
#327085=CARTESIAN_POINT('Ctrl Pts',(-0.0846343790000559,2.2,-4.16750849100001));
#327086=CARTESIAN_POINT('Ctrl Pts',(-0.084256794000056,12.2,-4.16886855400001));
#327087=CARTESIAN_POINT('Ctrl Pts',(-0.084256794000056,5.2,-4.16886855400001));
#327088=CARTESIAN_POINT('Ctrl Pts',(-0.084256794000056,2.2,-4.16886855400001));
#327089=CARTESIAN_POINT('Ctrl Pts',(-0.0838763050000557,12.2,-4.17023283200002));
#327090=CARTESIAN_POINT('Ctrl Pts',(-0.0838763050000557,5.2,-4.17023283200002));
#327091=CARTESIAN_POINT('Ctrl Pts',(-0.0838763050000557,2.2,-4.17023283200002));
#327092=CARTESIAN_POINT('Ctrl Pts',(-0.0834929050000566,12.2,-4.17160131500002));
#327093=CARTESIAN_POINT('Ctrl Pts',(-0.0834929050000566,5.2,-4.17160131500002));
#327094=CARTESIAN_POINT('Ctrl Pts',(-0.0834929050000566,2.2,-4.17160131500002));
#327095=CARTESIAN_POINT('Ctrl Pts',(-0.0831065840000556,12.2,-4.17297398900002));
#327096=CARTESIAN_POINT('Ctrl Pts',(-0.0831065840000556,5.2,-4.17297398900002));
#327097=CARTESIAN_POINT('Ctrl Pts',(-0.0831065840000556,2.2,-4.17297398900002));
#327098=CARTESIAN_POINT('Ctrl Pts',(-0.0827173360000566,12.2,-4.17435084500001));
#327099=CARTESIAN_POINT('Ctrl Pts',(-0.0827173360000566,5.2,-4.17435084500001));
#327100=CARTESIAN_POINT('Ctrl Pts',(-0.0827173360000566,2.2,-4.17435084500001));
#327101=CARTESIAN_POINT('Ctrl Pts',(-0.0823251550000559,12.2,-4.17573187000002));
#327102=CARTESIAN_POINT('Ctrl Pts',(-0.0823251550000559,5.2,-4.17573187000002));
#327103=CARTESIAN_POINT('Ctrl Pts',(-0.0823251550000559,2.2,-4.17573187000002));
#327104=CARTESIAN_POINT('Ctrl Pts',(-0.0819300290000557,12.2,-4.17711705300002));
#327105=CARTESIAN_POINT('Ctrl Pts',(-0.0819300290000557,5.2,-4.17711705300002));
#327106=CARTESIAN_POINT('Ctrl Pts',(-0.0819300290000557,2.2,-4.17711705300002));
#327107=CARTESIAN_POINT('Ctrl Pts',(-0.0815319540000559,12.2,-4.17850638300001));
#327108=CARTESIAN_POINT('Ctrl Pts',(-0.0815319540000559,5.2,-4.17850638300001));
#327109=CARTESIAN_POINT('Ctrl Pts',(-0.0815319540000559,2.2,-4.17850638300001));
#327110=CARTESIAN_POINT('Ctrl Pts',(-0.0811309220000567,12.2,-4.17989984800001));
#327111=CARTESIAN_POINT('Ctrl Pts',(-0.0811309220000567,5.2,-4.17989984800001));
#327112=CARTESIAN_POINT('Ctrl Pts',(-0.0811309220000567,2.2,-4.17989984800001));
#327113=CARTESIAN_POINT('Ctrl Pts',(-0.0807269240000552,12.2,-4.18129743700002));
#327114=CARTESIAN_POINT('Ctrl Pts',(-0.0807269240000552,5.2,-4.18129743700002));
#327115=CARTESIAN_POINT('Ctrl Pts',(-0.0807269240000552,2.2,-4.18129743700002));
#327116=CARTESIAN_POINT('Ctrl Pts',(-0.0803199530000565,12.2,-4.18269913800001));
#327117=CARTESIAN_POINT('Ctrl Pts',(-0.0803199530000565,5.2,-4.18269913800001));
#327118=CARTESIAN_POINT('Ctrl Pts',(-0.0803199530000565,2.2,-4.18269913800001));
#327119=CARTESIAN_POINT('Ctrl Pts',(-0.0799100020000565,12.2,-4.18410494100002));
#327120=CARTESIAN_POINT('Ctrl Pts',(-0.0799100020000565,5.2,-4.18410494100002));
#327121=CARTESIAN_POINT('Ctrl Pts',(-0.0799100020000565,2.2,-4.18410494100002));
#327122=CARTESIAN_POINT('Ctrl Pts',(-0.0794970630000569,12.2,-4.18551483500002));
#327123=CARTESIAN_POINT('Ctrl Pts',(-0.0794970630000569,5.2,-4.18551483500002));
#327124=CARTESIAN_POINT('Ctrl Pts',(-0.0794970630000569,2.2,-4.18551483500002));
#327125=CARTESIAN_POINT('Ctrl Pts',(-0.0790811280000547,12.2,-4.18692880600001));
#327126=CARTESIAN_POINT('Ctrl Pts',(-0.0790811280000547,5.2,-4.18692880600001));
#327127=CARTESIAN_POINT('Ctrl Pts',(-0.0790811280000547,2.2,-4.18692880600001));
#327128=CARTESIAN_POINT('Ctrl Pts',(-0.0786621920000563,12.2,-4.18834684500001));
#327129=CARTESIAN_POINT('Ctrl Pts',(-0.0786621920000563,5.2,-4.18834684500001));
#327130=CARTESIAN_POINT('Ctrl Pts',(-0.0786621920000563,2.2,-4.18834684500001));
#327131=CARTESIAN_POINT('Ctrl Pts',(-0.0782402460000564,12.2,-4.18976894000001));
#327132=CARTESIAN_POINT('Ctrl Pts',(-0.0782402460000564,5.2,-4.18976894000001));
#327133=CARTESIAN_POINT('Ctrl Pts',(-0.0782402460000564,2.2,-4.18976894000001));
#327134=CARTESIAN_POINT('Ctrl Pts',(-0.0778152820000566,12.2,-4.19119507900001));
#327135=CARTESIAN_POINT('Ctrl Pts',(-0.0778152820000566,5.2,-4.19119507900001));
#327136=CARTESIAN_POINT('Ctrl Pts',(-0.0778152820000566,2.2,-4.19119507900001));
#327137=CARTESIAN_POINT('Ctrl Pts',(-0.0773872930000563,12.2,-4.19262525300002));
#327138=CARTESIAN_POINT('Ctrl Pts',(-0.0773872930000563,5.2,-4.19262525300002));
#327139=CARTESIAN_POINT('Ctrl Pts',(-0.0773872930000563,2.2,-4.19262525300002));
#327140=CARTESIAN_POINT('Ctrl Pts',(-0.076956273000055,12.2,-4.19405944800001));
#327141=CARTESIAN_POINT('Ctrl Pts',(-0.076956273000055,5.2,-4.19405944800001));
#327142=CARTESIAN_POINT('Ctrl Pts',(-0.076956273000055,2.2,-4.19405944800001));
#327143=CARTESIAN_POINT('Ctrl Pts',(-0.0765222130000554,12.2,-4.19549765400001));
#327144=CARTESIAN_POINT('Ctrl Pts',(-0.0765222130000554,5.2,-4.19549765400001));
#327145=CARTESIAN_POINT('Ctrl Pts',(-0.0765222130000554,2.2,-4.19549765400001));
#327146=CARTESIAN_POINT('Ctrl Pts',(-0.0760851080000558,12.2,-4.19693986000001));
#327147=CARTESIAN_POINT('Ctrl Pts',(-0.0760851080000558,5.2,-4.19693986000001));
#327148=CARTESIAN_POINT('Ctrl Pts',(-0.0760851080000558,2.2,-4.19693986000001));
#327149=CARTESIAN_POINT('Ctrl Pts',(-0.0756449490000555,12.2,-4.19838605500002));
#327150=CARTESIAN_POINT('Ctrl Pts',(-0.0756449490000555,5.2,-4.19838605500002));
#327151=CARTESIAN_POINT('Ctrl Pts',(-0.0756449490000555,2.2,-4.19838605500002));
#327152=CARTESIAN_POINT('Ctrl Pts',(-0.0752017290000562,12.2,-4.19983622700002));
#327153=CARTESIAN_POINT('Ctrl Pts',(-0.0752017290000562,5.2,-4.19983622700002));
#327154=CARTESIAN_POINT('Ctrl Pts',(-0.0752017290000562,2.2,-4.19983622700002));
#327155=CARTESIAN_POINT('Ctrl Pts',(-0.0747554410000551,12.2,-4.20129036500001));
#327156=CARTESIAN_POINT('Ctrl Pts',(-0.0747554410000551,5.2,-4.20129036500001));
#327157=CARTESIAN_POINT('Ctrl Pts',(-0.0747554410000551,2.2,-4.20129036500001));
#327158=CARTESIAN_POINT('Ctrl Pts',(-0.074306079000056,12.2,-4.20274845800002));
#327159=CARTESIAN_POINT('Ctrl Pts',(-0.074306079000056,5.2,-4.20274845800002));
#327160=CARTESIAN_POINT('Ctrl Pts',(-0.074306079000056,2.2,-4.20274845800002));
#327161=CARTESIAN_POINT('Ctrl Pts',(-0.0738536340000551,12.2,-4.20421049600002));
#327162=CARTESIAN_POINT('Ctrl Pts',(-0.0738536340000551,5.2,-4.20421049600002));
#327163=CARTESIAN_POINT('Ctrl Pts',(-0.0738536340000551,2.2,-4.20421049600002));
#327164=CARTESIAN_POINT('Ctrl Pts',(-0.0733981010000551,12.2,-4.20567646600002));
#327165=CARTESIAN_POINT('Ctrl Pts',(-0.0733981010000551,5.2,-4.20567646600002));
#327166=CARTESIAN_POINT('Ctrl Pts',(-0.0733981010000551,2.2,-4.20567646600002));
#327167=CARTESIAN_POINT('Ctrl Pts',(-0.0729394710000564,12.2,-4.20714635600001));
#327168=CARTESIAN_POINT('Ctrl Pts',(-0.0729394710000564,5.2,-4.20714635600001));
#327169=CARTESIAN_POINT('Ctrl Pts',(-0.0729394710000564,2.2,-4.20714635600001));
#327170=CARTESIAN_POINT('Ctrl Pts',(-0.0724777380000563,12.2,-4.20862015900001));
#327171=CARTESIAN_POINT('Ctrl Pts',(-0.0724777380000563,5.2,-4.20862015900001));
#327172=CARTESIAN_POINT('Ctrl Pts',(-0.0724777380000563,2.2,-4.20862015900001));
#327173=CARTESIAN_POINT('Ctrl Pts',(-0.0720128950000554,12.2,-4.21009786100001));
#327174=CARTESIAN_POINT('Ctrl Pts',(-0.0720128950000554,5.2,-4.21009786100001));
#327175=CARTESIAN_POINT('Ctrl Pts',(-0.0720128950000554,2.2,-4.21009786100001));
#327176=CARTESIAN_POINT('Ctrl Pts',(-0.0715449360000553,12.2,-4.21157945000001));
#327177=CARTESIAN_POINT('Ctrl Pts',(-0.0715449360000553,5.2,-4.21157945000001));
#327178=CARTESIAN_POINT('Ctrl Pts',(-0.0715449360000553,2.2,-4.21157945000001));
#327179=CARTESIAN_POINT('Ctrl Pts',(-0.0710738530000565,12.2,-4.21306491700001));
#327180=CARTESIAN_POINT('Ctrl Pts',(-0.0710738530000565,5.2,-4.21306491700001));
#327181=CARTESIAN_POINT('Ctrl Pts',(-0.0710738530000565,2.2,-4.21306491700001));
#327182=CARTESIAN_POINT('Ctrl Pts',(-0.0705996390000563,12.2,-4.21455424900001));
#327183=CARTESIAN_POINT('Ctrl Pts',(-0.0705996390000563,5.2,-4.21455424900001));
#327184=CARTESIAN_POINT('Ctrl Pts',(-0.0705996390000563,2.2,-4.21455424900001));
#327185=CARTESIAN_POINT('Ctrl Pts',(-0.0701222880000552,12.2,-4.21604743700001));
#327186=CARTESIAN_POINT('Ctrl Pts',(-0.0701222880000552,5.2,-4.21604743700001));
#327187=CARTESIAN_POINT('Ctrl Pts',(-0.0701222880000552,2.2,-4.21604743700001));
#327188=CARTESIAN_POINT('Ctrl Pts',(-0.0696417920000558,12.2,-4.21754447000001));
#327189=CARTESIAN_POINT('Ctrl Pts',(-0.0696417920000558,5.2,-4.21754447000001));
#327190=CARTESIAN_POINT('Ctrl Pts',(-0.0696417920000558,2.2,-4.21754447000001));
#327191=CARTESIAN_POINT('Ctrl Pts',(-0.0691581460000557,12.2,-4.21904533400001));
#327192=CARTESIAN_POINT('Ctrl Pts',(-0.0691581460000557,5.2,-4.21904533400001));
#327193=CARTESIAN_POINT('Ctrl Pts',(-0.0691581460000557,2.2,-4.21904533400001));
#327194=CARTESIAN_POINT('Ctrl Pts',(-0.0686713410000561,12.2,-4.22055002100001));
#327195=CARTESIAN_POINT('Ctrl Pts',(-0.0686713410000561,5.2,-4.22055002100001));
#327196=CARTESIAN_POINT('Ctrl Pts',(-0.0686713410000561,2.2,-4.22055002100001));
#327197=CARTESIAN_POINT('Ctrl Pts',(-0.0681813710000567,12.2,-4.22205851900001));
#327198=CARTESIAN_POINT('Ctrl Pts',(-0.0681813710000567,5.2,-4.22205851900001));
#327199=CARTESIAN_POINT('Ctrl Pts',(-0.0681813710000567,2.2,-4.22205851900001));
#327200=CARTESIAN_POINT('Ctrl Pts',(-0.0676882310000571,12.2,-4.22357081700001));
#327201=CARTESIAN_POINT('Ctrl Pts',(-0.0676882310000571,5.2,-4.22357081700001));
#327202=CARTESIAN_POINT('Ctrl Pts',(-0.0676882310000571,2.2,-4.22357081700001));
#327203=CARTESIAN_POINT('Ctrl Pts',(-0.0671919130000554,12.2,-4.22508690400001));
#327204=CARTESIAN_POINT('Ctrl Pts',(-0.0671919130000554,5.2,-4.22508690400001));
#327205=CARTESIAN_POINT('Ctrl Pts',(-0.0671919130000554,2.2,-4.22508690400001));
#327206=CARTESIAN_POINT('Ctrl Pts',(-0.0666924100000566,12.2,-4.22660676900001));
#327207=CARTESIAN_POINT('Ctrl Pts',(-0.0666924100000566,5.2,-4.22660676900001));
#327208=CARTESIAN_POINT('Ctrl Pts',(-0.0666924100000566,2.2,-4.22660676900001));
#327209=CARTESIAN_POINT('Ctrl Pts',(-0.0661897150000546,12.2,-4.22813040100001));
#327210=CARTESIAN_POINT('Ctrl Pts',(-0.0661897150000546,5.2,-4.22813040100001));
#327211=CARTESIAN_POINT('Ctrl Pts',(-0.0661897150000546,2.2,-4.22813040100001));
#327212=CARTESIAN_POINT('Ctrl Pts',(-0.0656838230000556,12.2,-4.22965778900001));
#327213=CARTESIAN_POINT('Ctrl Pts',(-0.0656838230000556,5.2,-4.22965778900001));
#327214=CARTESIAN_POINT('Ctrl Pts',(-0.0656838230000556,2.2,-4.22965778900001));
#327215=CARTESIAN_POINT('Ctrl Pts',(-0.0651747270000558,12.2,-4.23118892200002));
#327216=CARTESIAN_POINT('Ctrl Pts',(-0.0651747270000558,5.2,-4.23118892200002));
#327217=CARTESIAN_POINT('Ctrl Pts',(-0.0651747270000558,2.2,-4.23118892200002));
#327218=CARTESIAN_POINT('Ctrl Pts',(-0.0646624190000556,12.2,-4.23272378900001));
#327219=CARTESIAN_POINT('Ctrl Pts',(-0.0646624190000556,5.2,-4.23272378900001));
#327220=CARTESIAN_POINT('Ctrl Pts',(-0.0646624190000556,2.2,-4.23272378900001));
#327221=CARTESIAN_POINT('Ctrl Pts',(-0.0641468940000556,12.2,-4.23426238000001));
#327222=CARTESIAN_POINT('Ctrl Pts',(-0.0641468940000556,5.2,-4.23426238000001));
#327223=CARTESIAN_POINT('Ctrl Pts',(-0.0641468940000556,2.2,-4.23426238000001));
#327224=CARTESIAN_POINT('Ctrl Pts',(-0.0636281460000554,12.2,-4.23580468300001));
#327225=CARTESIAN_POINT('Ctrl Pts',(-0.0636281460000554,5.2,-4.23580468300001));
#327226=CARTESIAN_POINT('Ctrl Pts',(-0.0636281460000554,2.2,-4.23580468300001));
#327227=CARTESIAN_POINT('Ctrl Pts',(-0.0631061670000555,12.2,-4.23735068900001));
#327228=CARTESIAN_POINT('Ctrl Pts',(-0.0631061670000555,5.2,-4.23735068900001));
#327229=CARTESIAN_POINT('Ctrl Pts',(-0.0631061670000555,2.2,-4.23735068900001));
#327230=CARTESIAN_POINT('Ctrl Pts',(-0.0625809500000563,12.2,-4.23890038400002));
#327231=CARTESIAN_POINT('Ctrl Pts',(-0.0625809500000563,5.2,-4.23890038400002));
#327232=CARTESIAN_POINT('Ctrl Pts',(-0.0625809500000563,2.2,-4.23890038400002));
#327233=CARTESIAN_POINT('Ctrl Pts',(-0.0620524920000565,12.2,-4.24045376000001));
#327234=CARTESIAN_POINT('Ctrl Pts',(-0.0620524920000565,5.2,-4.24045376000001));
#327235=CARTESIAN_POINT('Ctrl Pts',(-0.0620524920000565,2.2,-4.24045376000001));
#327236=CARTESIAN_POINT('Ctrl Pts',(-0.0615207820000552,12.2,-4.24201080300001));
#327237=CARTESIAN_POINT('Ctrl Pts',(-0.0615207820000552,5.2,-4.24201080300001));
#327238=CARTESIAN_POINT('Ctrl Pts',(-0.0615207820000552,2.2,-4.24201080300001));
#327239=CARTESIAN_POINT('Ctrl Pts',(-0.0609858180000555,12.2,-4.24357150600001));
#327240=CARTESIAN_POINT('Ctrl Pts',(-0.0609858180000555,5.2,-4.24357150600001));
#327241=CARTESIAN_POINT('Ctrl Pts',(-0.0609858180000555,2.2,-4.24357150600001));
#327242=CARTESIAN_POINT('Ctrl Pts',(-0.0604475910000557,12.2,-4.24513585500002));
#327243=CARTESIAN_POINT('Ctrl Pts',(-0.0604475910000557,5.2,-4.24513585500002));
#327244=CARTESIAN_POINT('Ctrl Pts',(-0.0604475910000557,2.2,-4.24513585500002));
#327245=CARTESIAN_POINT('Ctrl Pts',(-0.0599060960000553,12.2,-4.24670384200001));
#327246=CARTESIAN_POINT('Ctrl Pts',(-0.0599060960000553,5.2,-4.24670384200001));
#327247=CARTESIAN_POINT('Ctrl Pts',(-0.0599060960000553,2.2,-4.24670384200001));
#327248=CARTESIAN_POINT('Ctrl Pts',(-0.0593613260000558,12.2,-4.24827545300001));
#327249=CARTESIAN_POINT('Ctrl Pts',(-0.0593613260000558,5.2,-4.24827545300001));
#327250=CARTESIAN_POINT('Ctrl Pts',(-0.0593613260000558,2.2,-4.24827545300001));
#327251=CARTESIAN_POINT('Ctrl Pts',(-0.0588132750000547,12.2,-4.24985068100002));
#327252=CARTESIAN_POINT('Ctrl Pts',(-0.0588132750000547,5.2,-4.24985068100002));
#327253=CARTESIAN_POINT('Ctrl Pts',(-0.0588132750000547,2.2,-4.24985068100002));
#327254=CARTESIAN_POINT('Ctrl Pts',(-0.0582619360000558,12.2,-4.25142951200002));
#327255=CARTESIAN_POINT('Ctrl Pts',(-0.0582619360000558,5.2,-4.25142951200002));
#327256=CARTESIAN_POINT('Ctrl Pts',(-0.0582619360000558,2.2,-4.25142951200002));
#327257=CARTESIAN_POINT('Ctrl Pts',(-0.0577073040000553,12.2,-4.25301193500002));
#327258=CARTESIAN_POINT('Ctrl Pts',(-0.0577073040000553,5.2,-4.25301193500002));
#327259=CARTESIAN_POINT('Ctrl Pts',(-0.0577073040000553,2.2,-4.25301193500002));
#327260=CARTESIAN_POINT('Ctrl Pts',(-0.057149372000056,12.2,-4.25459794200002));
#327261=CARTESIAN_POINT('Ctrl Pts',(-0.057149372000056,5.2,-4.25459794200002));
#327262=CARTESIAN_POINT('Ctrl Pts',(-0.057149372000056,2.2,-4.25459794200002));
#327263=CARTESIAN_POINT('Ctrl Pts',(-0.0565881350000552,12.2,-4.25618752100001));
#327264=CARTESIAN_POINT('Ctrl Pts',(-0.0565881350000552,5.2,-4.25618752100001));
#327265=CARTESIAN_POINT('Ctrl Pts',(-0.0565881350000552,2.2,-4.25618752100001));
#327266=CARTESIAN_POINT('Ctrl Pts',(-0.0560235860000546,12.2,-4.25778066100001));
#327267=CARTESIAN_POINT('Ctrl Pts',(-0.0560235860000546,5.2,-4.25778066100001));
#327268=CARTESIAN_POINT('Ctrl Pts',(-0.0560235860000546,2.2,-4.25778066100001));
#327269=CARTESIAN_POINT('Ctrl Pts',(-0.0554557180000559,12.2,-4.25937735100002));
#327270=CARTESIAN_POINT('Ctrl Pts',(-0.0554557180000559,5.2,-4.25937735100002));
#327271=CARTESIAN_POINT('Ctrl Pts',(-0.0554557180000559,2.2,-4.25937735100002));
#327272=CARTESIAN_POINT('Ctrl Pts',(-0.0548845270000553,12.2,-4.26097758100001));
#327273=CARTESIAN_POINT('Ctrl Pts',(-0.0548845270000553,5.2,-4.26097758100001));
#327274=CARTESIAN_POINT('Ctrl Pts',(-0.0548845270000553,2.2,-4.26097758100001));
#327275=CARTESIAN_POINT('Ctrl Pts',(-0.0543100050000567,12.2,-4.26258134100001));
#327276=CARTESIAN_POINT('Ctrl Pts',(-0.0543100050000567,5.2,-4.26258134100001));
#327277=CARTESIAN_POINT('Ctrl Pts',(-0.0543100050000567,2.2,-4.26258134100001));
#327278=CARTESIAN_POINT('Ctrl Pts',(-0.0537321480000563,12.2,-4.26418861700002));
#327279=CARTESIAN_POINT('Ctrl Pts',(-0.0537321480000563,5.2,-4.26418861700002));
#327280=CARTESIAN_POINT('Ctrl Pts',(-0.0537321480000563,2.2,-4.26418861700002));
#327281=CARTESIAN_POINT('Ctrl Pts',(-0.0531509480000558,12.2,-4.26579940300002));
#327282=CARTESIAN_POINT('Ctrl Pts',(-0.0531509480000558,5.2,-4.26579940300002));
#327283=CARTESIAN_POINT('Ctrl Pts',(-0.0531509480000558,2.2,-4.26579940300002));
#327284=CARTESIAN_POINT('Ctrl Pts',(-0.0525664010000571,12.2,-4.26741368500001));
#327285=CARTESIAN_POINT('Ctrl Pts',(-0.0525664010000571,5.2,-4.26741368500001));
#327286=CARTESIAN_POINT('Ctrl Pts',(-0.0525664010000571,2.2,-4.26741368500001));
#327287=CARTESIAN_POINT('Ctrl Pts',(-0.051978500000055,12.2,-4.26903145300002));
#327288=CARTESIAN_POINT('Ctrl Pts',(-0.051978500000055,5.2,-4.26903145300002));
#327289=CARTESIAN_POINT('Ctrl Pts',(-0.051978500000055,2.2,-4.26903145300002));
#327290=CARTESIAN_POINT('Ctrl Pts',(-0.0513872380000546,12.2,-4.27065269700002));
#327291=CARTESIAN_POINT('Ctrl Pts',(-0.0513872380000546,5.2,-4.27065269700002));
#327292=CARTESIAN_POINT('Ctrl Pts',(-0.0513872380000546,2.2,-4.27065269700002));
#327293=CARTESIAN_POINT('Ctrl Pts',(-0.0507926120000557,12.2,-4.27227740600001));
#327294=CARTESIAN_POINT('Ctrl Pts',(-0.0507926120000557,5.2,-4.27227740600001));
#327295=CARTESIAN_POINT('Ctrl Pts',(-0.0507926120000557,2.2,-4.27227740600001));
#327296=CARTESIAN_POINT('Ctrl Pts',(-0.0501946120000552,12.2,-4.27390556900002));
#327297=CARTESIAN_POINT('Ctrl Pts',(-0.0501946120000552,5.2,-4.27390556900002));
#327298=CARTESIAN_POINT('Ctrl Pts',(-0.0501946120000552,2.2,-4.27390556900002));
#327299=CARTESIAN_POINT('Ctrl Pts',(-0.0495932360000562,12.2,-4.27553717600002));
#327300=CARTESIAN_POINT('Ctrl Pts',(-0.0495932360000562,5.2,-4.27553717600002));
#327301=CARTESIAN_POINT('Ctrl Pts',(-0.0495932360000562,2.2,-4.27553717600002));
#327302=CARTESIAN_POINT('Ctrl Pts',(-0.048988477000057,12.2,-4.27717221600002));
#327303=CARTESIAN_POINT('Ctrl Pts',(-0.048988477000057,5.2,-4.27717221600002));
#327304=CARTESIAN_POINT('Ctrl Pts',(-0.048988477000057,2.2,-4.27717221600002));
#327305=CARTESIAN_POINT('Ctrl Pts',(-0.0483803290000551,12.2,-4.27881068000001));
#327306=CARTESIAN_POINT('Ctrl Pts',(-0.0483803290000551,5.2,-4.27881068000001));
#327307=CARTESIAN_POINT('Ctrl Pts',(-0.0483803290000551,2.2,-4.27881068000001));
#327308=CARTESIAN_POINT('Ctrl Pts',(-0.0477687860000553,12.2,-4.28045255500002));
#327309=CARTESIAN_POINT('Ctrl Pts',(-0.0477687860000553,5.2,-4.28045255500002));
#327310=CARTESIAN_POINT('Ctrl Pts',(-0.0477687860000553,2.2,-4.28045255500002));
#327311=CARTESIAN_POINT('Ctrl Pts',(-0.047153842000055,12.2,-4.28209783100002));
#327312=CARTESIAN_POINT('Ctrl Pts',(-0.047153842000055,5.2,-4.28209783100002));
#327313=CARTESIAN_POINT('Ctrl Pts',(-0.047153842000055,2.2,-4.28209783100002));
#327314=CARTESIAN_POINT('Ctrl Pts',(-0.0465354920000549,12.2,-4.28374649900002));
#327315=CARTESIAN_POINT('Ctrl Pts',(-0.0465354920000549,5.2,-4.28374649900002));
#327316=CARTESIAN_POINT('Ctrl Pts',(-0.0465354920000549,2.2,-4.28374649900002));
#327317=CARTESIAN_POINT('Ctrl Pts',(-0.0459137300000556,12.2,-4.28539854700002));
#327318=CARTESIAN_POINT('Ctrl Pts',(-0.0459137300000556,5.2,-4.28539854700002));
#327319=CARTESIAN_POINT('Ctrl Pts',(-0.0459137300000556,2.2,-4.28539854700002));
#327320=CARTESIAN_POINT('Ctrl Pts',(-0.0452885500000555,12.2,-4.28705396500002));
#327321=CARTESIAN_POINT('Ctrl Pts',(-0.0452885500000555,5.2,-4.28705396500002));
#327322=CARTESIAN_POINT('Ctrl Pts',(-0.0452885500000555,2.2,-4.28705396500002));
#327323=CARTESIAN_POINT('Ctrl Pts',(-0.0446599480000565,12.2,-4.28871274200001));
#327324=CARTESIAN_POINT('Ctrl Pts',(-0.0446599480000565,5.2,-4.28871274200001));
#327325=CARTESIAN_POINT('Ctrl Pts',(-0.0446599480000565,2.2,-4.28871274200001));
#327326=CARTESIAN_POINT('Ctrl Pts',(-0.0440279170000557,12.2,-4.29037486800001));
#327327=CARTESIAN_POINT('Ctrl Pts',(-0.0440279170000557,5.2,-4.29037486800001));
#327328=CARTESIAN_POINT('Ctrl Pts',(-0.0440279170000557,2.2,-4.29037486800001));
#327329=CARTESIAN_POINT('Ctrl Pts',(-0.043392450000056,12.2,-4.29204033300001));
#327330=CARTESIAN_POINT('Ctrl Pts',(-0.043392450000056,5.2,-4.29204033300001));
#327331=CARTESIAN_POINT('Ctrl Pts',(-0.043392450000056,2.2,-4.29204033300001));
#327332=CARTESIAN_POINT('Ctrl Pts',(-0.0427535450000571,12.2,-4.29370912600001));
#327333=CARTESIAN_POINT('Ctrl Pts',(-0.0427535450000571,5.2,-4.29370912600001));
#327334=CARTESIAN_POINT('Ctrl Pts',(-0.0427535450000571,2.2,-4.29370912600001));
#327335=CARTESIAN_POINT('Ctrl Pts',(-0.0421111930000551,12.2,-4.29538123500001));
#327336=CARTESIAN_POINT('Ctrl Pts',(-0.0421111930000551,5.2,-4.29538123500001));
#327337=CARTESIAN_POINT('Ctrl Pts',(-0.0421111930000551,2.2,-4.29538123500001));
#327338=CARTESIAN_POINT('Ctrl Pts',(-0.0414653900000561,12.2,-4.29705665200002));
#327339=CARTESIAN_POINT('Ctrl Pts',(-0.0414653900000561,5.2,-4.29705665200002));
#327340=CARTESIAN_POINT('Ctrl Pts',(-0.0414653900000561,2.2,-4.29705665200002));
#327341=CARTESIAN_POINT('Ctrl Pts',(-0.0408161310000566,12.2,-4.29873536500001));
#327342=CARTESIAN_POINT('Ctrl Pts',(-0.0408161310000566,5.2,-4.29873536500001));
#327343=CARTESIAN_POINT('Ctrl Pts',(-0.0408161310000566,2.2,-4.29873536500001));
#327344=CARTESIAN_POINT('Ctrl Pts',(-0.0401634110000571,12.2,-4.30041736500002));
#327345=CARTESIAN_POINT('Ctrl Pts',(-0.0401634110000571,5.2,-4.30041736500002));
#327346=CARTESIAN_POINT('Ctrl Pts',(-0.0401634110000571,2.2,-4.30041736500002));
#327347=CARTESIAN_POINT('Ctrl Pts',(-0.0395072220000559,12.2,-4.30210263900001));
#327348=CARTESIAN_POINT('Ctrl Pts',(-0.0395072220000559,5.2,-4.30210263900001));
#327349=CARTESIAN_POINT('Ctrl Pts',(-0.0395072220000559,2.2,-4.30210263900001));
#327350=CARTESIAN_POINT('Ctrl Pts',(-0.038847561000056,12.2,-4.30379117900001));
#327351=CARTESIAN_POINT('Ctrl Pts',(-0.038847561000056,5.2,-4.30379117900001));
#327352=CARTESIAN_POINT('Ctrl Pts',(-0.038847561000056,2.2,-4.30379117900001));
#327353=CARTESIAN_POINT('Ctrl Pts',(-0.0381844200000547,12.2,-4.30548297500001));
#327354=CARTESIAN_POINT('Ctrl Pts',(-0.0381844200000547,5.2,-4.30548297500001));
#327355=CARTESIAN_POINT('Ctrl Pts',(-0.0381844200000547,2.2,-4.30548297500001));
#327356=CARTESIAN_POINT('Ctrl Pts',(-0.0375177970000562,12.2,-4.30717801400001));
#327357=CARTESIAN_POINT('Ctrl Pts',(-0.0375177970000562,5.2,-4.30717801400001));
#327358=CARTESIAN_POINT('Ctrl Pts',(-0.0375177970000562,2.2,-4.30717801400001));
#327359=CARTESIAN_POINT('Ctrl Pts',(-0.0368476850000565,12.2,-4.30887628700001));
#327360=CARTESIAN_POINT('Ctrl Pts',(-0.0368476850000565,5.2,-4.30887628700001));
#327361=CARTESIAN_POINT('Ctrl Pts',(-0.0368476850000565,2.2,-4.30887628700001));
#327362=CARTESIAN_POINT('Ctrl Pts',(-0.0361740780000552,12.2,-4.31057778500001));
#327363=CARTESIAN_POINT('Ctrl Pts',(-0.0361740780000552,5.2,-4.31057778500001));
#327364=CARTESIAN_POINT('Ctrl Pts',(-0.0361740780000552,2.2,-4.31057778500001));
#327365=CARTESIAN_POINT('Ctrl Pts',(-0.0354969720000553,12.2,-4.31228249500001));
#327366=CARTESIAN_POINT('Ctrl Pts',(-0.0354969720000553,5.2,-4.31228249500001));
#327367=CARTESIAN_POINT('Ctrl Pts',(-0.0354969720000553,2.2,-4.31228249500001));
#327368=CARTESIAN_POINT('Ctrl Pts',(-0.0348163610000551,12.2,-4.31399040900001));
#327369=CARTESIAN_POINT('Ctrl Pts',(-0.0348163610000551,5.2,-4.31399040900001));
#327370=CARTESIAN_POINT('Ctrl Pts',(-0.0348163610000551,2.2,-4.31399040900001));
#327371=CARTESIAN_POINT('Ctrl Pts',(-0.0341322390000565,12.2,-4.31570151500001));
#327372=CARTESIAN_POINT('Ctrl Pts',(-0.0341322390000565,5.2,-4.31570151500001));
#327373=CARTESIAN_POINT('Ctrl Pts',(-0.0341322390000565,2.2,-4.31570151500001));
#327374=CARTESIAN_POINT('Ctrl Pts',(-0.0334446030000557,12.2,-4.31741580200002));
#327375=CARTESIAN_POINT('Ctrl Pts',(-0.0334446030000557,5.2,-4.31741580200002));
#327376=CARTESIAN_POINT('Ctrl Pts',(-0.0334446030000557,2.2,-4.31741580200002));
#327377=CARTESIAN_POINT('Ctrl Pts',(-0.0327534450000555,12.2,-4.31913326200001));
#327378=CARTESIAN_POINT('Ctrl Pts',(-0.0327534450000555,5.2,-4.31913326200001));
#327379=CARTESIAN_POINT('Ctrl Pts',(-0.0327534450000555,2.2,-4.31913326200001));
#327380=CARTESIAN_POINT('Ctrl Pts',(-0.0320587610000567,12.2,-4.32085388300001));
#327381=CARTESIAN_POINT('Ctrl Pts',(-0.0320587610000567,5.2,-4.32085388300001));
#327382=CARTESIAN_POINT('Ctrl Pts',(-0.0320587610000567,2.2,-4.32085388300001));
#327383=CARTESIAN_POINT('Ctrl Pts',(-0.0313605480000556,12.2,-4.32257765700002));
#327384=CARTESIAN_POINT('Ctrl Pts',(-0.0313605480000556,5.2,-4.32257765700002));
#327385=CARTESIAN_POINT('Ctrl Pts',(-0.0313605480000556,2.2,-4.32257765700002));
#327386=CARTESIAN_POINT('Ctrl Pts',(-0.030658797000056,12.2,-4.32430457100001));
#327387=CARTESIAN_POINT('Ctrl Pts',(-0.030658797000056,5.2,-4.32430457100001));
#327388=CARTESIAN_POINT('Ctrl Pts',(-0.030658797000056,2.2,-4.32430457100001));
#327389=CARTESIAN_POINT('Ctrl Pts',(-0.0299535050000566,12.2,-4.32603461600001));
#327390=CARTESIAN_POINT('Ctrl Pts',(-0.0299535050000566,5.2,-4.32603461600001));
#327391=CARTESIAN_POINT('Ctrl Pts',(-0.0299535050000566,2.2,-4.32603461600001));
#327392=CARTESIAN_POINT('Ctrl Pts',(-0.0292446680000558,12.2,-4.32776778100001));
#327393=CARTESIAN_POINT('Ctrl Pts',(-0.0292446680000558,5.2,-4.32776778100001));
#327394=CARTESIAN_POINT('Ctrl Pts',(-0.0292446680000558,2.2,-4.32776778100001));
#327395=CARTESIAN_POINT('Ctrl Pts',(-0.0285322780000552,12.2,-4.32950405600002));
#327396=CARTESIAN_POINT('Ctrl Pts',(-0.0285322780000552,5.2,-4.32950405600002));
#327397=CARTESIAN_POINT('Ctrl Pts',(-0.0285322780000552,2.2,-4.32950405600002));
#327398=CARTESIAN_POINT('Ctrl Pts',(-0.0278163330000558,12.2,-4.33124343200001));
#327399=CARTESIAN_POINT('Ctrl Pts',(-0.0278163330000558,5.2,-4.33124343200001));
#327400=CARTESIAN_POINT('Ctrl Pts',(-0.0278163330000558,2.2,-4.33124343200001));
#327401=CARTESIAN_POINT('Ctrl Pts',(-0.0270968250000558,12.2,-4.33298589700001));
#327402=CARTESIAN_POINT('Ctrl Pts',(-0.0270968250000558,5.2,-4.33298589700001));
#327403=CARTESIAN_POINT('Ctrl Pts',(-0.0270968250000558,2.2,-4.33298589700001));
#327404=CARTESIAN_POINT('Ctrl Pts',(-0.0263737510000561,12.2,-4.33473144100001));
#327405=CARTESIAN_POINT('Ctrl Pts',(-0.0263737510000561,5.2,-4.33473144100001));
#327406=CARTESIAN_POINT('Ctrl Pts',(-0.0263737510000561,2.2,-4.33473144100001));
#327407=CARTESIAN_POINT('Ctrl Pts',(-0.0256471060000563,12.2,-4.33648005500002));
#327408=CARTESIAN_POINT('Ctrl Pts',(-0.0256471060000563,5.2,-4.33648005500002));
#327409=CARTESIAN_POINT('Ctrl Pts',(-0.0256471060000563,2.2,-4.33648005500002));
#327410=CARTESIAN_POINT('Ctrl Pts',(-0.0249168840000558,12.2,-4.33823172900001));
#327411=CARTESIAN_POINT('Ctrl Pts',(-0.0249168840000558,5.2,-4.33823172900001));
#327412=CARTESIAN_POINT('Ctrl Pts',(-0.0249168840000558,2.2,-4.33823172900001));
#327413=CARTESIAN_POINT('Ctrl Pts',(-0.0241830820000555,12.2,-4.33998645000001));
#327414=CARTESIAN_POINT('Ctrl Pts',(-0.0241830820000555,5.2,-4.33998645000001));
#327415=CARTESIAN_POINT('Ctrl Pts',(-0.0241830820000555,2.2,-4.33998645000001));
#327416=CARTESIAN_POINT('Ctrl Pts',(-0.0234456920000559,12.2,-4.34174421100002));
#327417=CARTESIAN_POINT('Ctrl Pts',(-0.0234456920000559,5.2,-4.34174421100002));
#327418=CARTESIAN_POINT('Ctrl Pts',(-0.0234456920000559,2.2,-4.34174421100002));
#327419=CARTESIAN_POINT('Ctrl Pts',(-0.0227047110000556,12.2,-4.34350500000001));
#327420=CARTESIAN_POINT('Ctrl Pts',(-0.0227047110000556,5.2,-4.34350500000001));
#327421=CARTESIAN_POINT('Ctrl Pts',(-0.0227047110000556,2.2,-4.34350500000001));
#327422=CARTESIAN_POINT('Ctrl Pts',(-0.0219601350000553,12.2,-4.34526880800002));
#327423=CARTESIAN_POINT('Ctrl Pts',(-0.0219601350000553,5.2,-4.34526880800002));
#327424=CARTESIAN_POINT('Ctrl Pts',(-0.0219601350000553,2.2,-4.34526880800002));
#327425=CARTESIAN_POINT('Ctrl Pts',(-0.0212119570000546,12.2,-4.34703562300002));
#327426=CARTESIAN_POINT('Ctrl Pts',(-0.0212119570000546,5.2,-4.34703562300002));
#327427=CARTESIAN_POINT('Ctrl Pts',(-0.0212119570000546,2.2,-4.34703562300002));
#327428=CARTESIAN_POINT('Ctrl Pts',(-0.0204601740000554,12.2,-4.34880543700002));
#327429=CARTESIAN_POINT('Ctrl Pts',(-0.0204601740000554,5.2,-4.34880543700002));
#327430=CARTESIAN_POINT('Ctrl Pts',(-0.0204601740000554,2.2,-4.34880543700002));
#327431=CARTESIAN_POINT('Ctrl Pts',(-0.019704779000056,12.2,-4.35057823800001));
#327432=CARTESIAN_POINT('Ctrl Pts',(-0.019704779000056,5.2,-4.35057823800001));
#327433=CARTESIAN_POINT('Ctrl Pts',(-0.019704779000056,2.2,-4.35057823800001));
#327434=CARTESIAN_POINT('Ctrl Pts',(-0.018945770000055,12.2,-4.35235401800002));
#327435=CARTESIAN_POINT('Ctrl Pts',(-0.018945770000055,5.2,-4.35235401800002));
#327436=CARTESIAN_POINT('Ctrl Pts',(-0.018945770000055,2.2,-4.35235401800002));
#327437=CARTESIAN_POINT('Ctrl Pts',(-0.0181831400000565,12.2,-4.35413276500002));
#327438=CARTESIAN_POINT('Ctrl Pts',(-0.0181831400000565,5.2,-4.35413276500002));
#327439=CARTESIAN_POINT('Ctrl Pts',(-0.0181831400000565,2.2,-4.35413276500002));
#327440=CARTESIAN_POINT('Ctrl Pts',(-0.0174168870000557,12.2,-4.35591446900002));
#327441=CARTESIAN_POINT('Ctrl Pts',(-0.0174168870000557,5.2,-4.35591446900002));
#327442=CARTESIAN_POINT('Ctrl Pts',(-0.0174168870000557,2.2,-4.35591446900002));
#327443=CARTESIAN_POINT('Ctrl Pts',(-0.0166470020000553,12.2,-4.35769912100001));
#327444=CARTESIAN_POINT('Ctrl Pts',(-0.0166470020000553,5.2,-4.35769912100001));
#327445=CARTESIAN_POINT('Ctrl Pts',(-0.0166470020000553,2.2,-4.35769912100001));
#327446=CARTESIAN_POINT('Ctrl Pts',(-0.0158734840000552,12.2,-4.35948671100002));
#327447=CARTESIAN_POINT('Ctrl Pts',(-0.0158734840000552,5.2,-4.35948671100002));
#327448=CARTESIAN_POINT('Ctrl Pts',(-0.0158734840000552,2.2,-4.35948671100002));
#327449=CARTESIAN_POINT('Ctrl Pts',(-0.0150963270000548,12.2,-4.36127722800002));
#327450=CARTESIAN_POINT('Ctrl Pts',(-0.0150963270000548,5.2,-4.36127722800002));
#327451=CARTESIAN_POINT('Ctrl Pts',(-0.0150963270000548,2.2,-4.36127722800002));
#327452=CARTESIAN_POINT('Ctrl Pts',(-0.014315526000056,12.2,-4.36307066200001));
#327453=CARTESIAN_POINT('Ctrl Pts',(-0.014315526000056,5.2,-4.36307066200001));
#327454=CARTESIAN_POINT('Ctrl Pts',(-0.014315526000056,2.2,-4.36307066200001));
#327455=CARTESIAN_POINT('Ctrl Pts',(-0.0135310770000563,12.2,-4.36486700300001));
#327456=CARTESIAN_POINT('Ctrl Pts',(-0.0135310770000563,5.2,-4.36486700300001));
#327457=CARTESIAN_POINT('Ctrl Pts',(-0.0135310770000563,2.2,-4.36486700300001));
#327458=CARTESIAN_POINT('Ctrl Pts',(-0.0127429750000552,12.2,-4.36666624200001));
#327459=CARTESIAN_POINT('Ctrl Pts',(-0.0127429750000552,5.2,-4.36666624200001));
#327460=CARTESIAN_POINT('Ctrl Pts',(-0.0127429750000552,2.2,-4.36666624200001));
#327461=CARTESIAN_POINT('Ctrl Pts',(-0.0119512150000567,12.2,-4.36846836700001));
#327462=CARTESIAN_POINT('Ctrl Pts',(-0.0119512150000567,5.2,-4.36846836700001));
#327463=CARTESIAN_POINT('Ctrl Pts',(-0.0119512150000567,2.2,-4.36846836700001));
#327464=CARTESIAN_POINT('Ctrl Pts',(-0.0111557950000552,12.2,-4.37027336900002));
#327465=CARTESIAN_POINT('Ctrl Pts',(-0.0111557950000552,5.2,-4.37027336900002));
#327466=CARTESIAN_POINT('Ctrl Pts',(-0.0111557950000552,2.2,-4.37027336900002));
#327467=CARTESIAN_POINT('Ctrl Pts',(-0.0103567060000565,12.2,-4.37208123900001));
#327468=CARTESIAN_POINT('Ctrl Pts',(-0.0103567060000565,5.2,-4.37208123900001));
#327469=CARTESIAN_POINT('Ctrl Pts',(-0.0103567060000565,2.2,-4.37208123900001));
#327470=CARTESIAN_POINT('Ctrl Pts',(-0.00955394600005489,12.2,-4.37389196600002));
#327471=CARTESIAN_POINT('Ctrl Pts',(-0.00955394600005489,5.2,-4.37389196600002));
#327472=CARTESIAN_POINT('Ctrl Pts',(-0.00955394600005489,2.2,-4.37389196600002));
#327473=CARTESIAN_POINT('Ctrl Pts',(-0.00874751200005575,12.2,-4.37570554000001));
#327474=CARTESIAN_POINT('Ctrl Pts',(-0.00874751200005575,5.2,-4.37570554000001));
#327475=CARTESIAN_POINT('Ctrl Pts',(-0.00874751200005575,2.2,-4.37570554000001));
#327476=CARTESIAN_POINT('Ctrl Pts',(-0.00793739600005617,12.2,-4.37752195100002));
#327477=CARTESIAN_POINT('Ctrl Pts',(-0.00793739600005617,5.2,-4.37752195100002));
#327478=CARTESIAN_POINT('Ctrl Pts',(-0.00793739600005617,2.2,-4.37752195100002));
#327479=CARTESIAN_POINT('Ctrl Pts',(-0.00712359700005606,12.2,-4.37934118900001));
#327480=CARTESIAN_POINT('Ctrl Pts',(-0.00712359700005606,5.2,-4.37934118900001));
#327481=CARTESIAN_POINT('Ctrl Pts',(-0.00712359700005606,2.2,-4.37934118900001));
#327482=CARTESIAN_POINT('Ctrl Pts',(-0.00630610800005483,12.2,-4.38116324500001));
#327483=CARTESIAN_POINT('Ctrl Pts',(-0.00630610800005483,5.2,-4.38116324500001));
#327484=CARTESIAN_POINT('Ctrl Pts',(-0.00630610800005483,2.2,-4.38116324500001));
#327485=CARTESIAN_POINT('Ctrl Pts',(-0.00548492600005558,12.2,-4.38298810700001));
#327486=CARTESIAN_POINT('Ctrl Pts',(-0.00548492600005558,5.2,-4.38298810700001));
#327487=CARTESIAN_POINT('Ctrl Pts',(-0.00548492600005558,2.2,-4.38298810700001));
#327488=CARTESIAN_POINT('Ctrl Pts',(-0.00466004600005677,12.2,-4.38481576600001));
#327489=CARTESIAN_POINT('Ctrl Pts',(-0.00466004600005677,5.2,-4.38481576600001));
#327490=CARTESIAN_POINT('Ctrl Pts',(-0.00466004600005677,2.2,-4.38481576600001));
#327491=CARTESIAN_POINT('Ctrl Pts',(-0.00383146400005586,12.2,-4.38664621400001));
#327492=CARTESIAN_POINT('Ctrl Pts',(-0.00383146400005586,5.2,-4.38664621400001));
#327493=CARTESIAN_POINT('Ctrl Pts',(-0.00383146400005586,2.2,-4.38664621400001));
#327494=CARTESIAN_POINT('Ctrl Pts',(-0.00299917500005576,12.2,-4.38847943800001));
#327495=CARTESIAN_POINT('Ctrl Pts',(-0.00299917500005576,5.2,-4.38847943800001));
#327496=CARTESIAN_POINT('Ctrl Pts',(-0.00299917500005576,2.2,-4.38847943800001));
#327497=CARTESIAN_POINT('Ctrl Pts',(-0.00216317600005623,12.2,-4.39031543100001));
#327498=CARTESIAN_POINT('Ctrl Pts',(-0.00216317600005623,5.2,-4.39031543100001));
#327499=CARTESIAN_POINT('Ctrl Pts',(-0.00216317600005623,2.2,-4.39031543100001));
#327500=CARTESIAN_POINT('Ctrl Pts',(-0.00132346000005668,12.2,-4.39215418000002));
#327501=CARTESIAN_POINT('Ctrl Pts',(-0.00132346000005668,5.2,-4.39215418000002));
#327502=CARTESIAN_POINT('Ctrl Pts',(-0.00132346000005668,2.2,-4.39215418000002));
#327503=CARTESIAN_POINT('Ctrl Pts',(-0.000480025000056958,12.2,-4.39399567700002));
#327504=CARTESIAN_POINT('Ctrl Pts',(-0.000480025000056958,5.2,-4.39399567700002));
#327505=CARTESIAN_POINT('Ctrl Pts',(-0.000480025000056958,2.2,-4.39399567700002));
#327506=CARTESIAN_POINT('Ctrl Pts',(0.000367133999944471,12.2,-4.39583991200001));
#327507=CARTESIAN_POINT('Ctrl Pts',(0.000367133999944471,5.2,-4.39583991200001));
#327508=CARTESIAN_POINT('Ctrl Pts',(0.000367133999944471,2.2,-4.39583991200001));
#327509=CARTESIAN_POINT('Ctrl Pts',(0.00121801999994452,12.2,-4.39768687500001));
#327510=CARTESIAN_POINT('Ctrl Pts',(0.00121801999994452,5.2,-4.39768687500001));
#327511=CARTESIAN_POINT('Ctrl Pts',(0.00121801999994452,2.2,-4.39768687500001));
#327512=CARTESIAN_POINT('Ctrl Pts',(0.00207263999994488,12.2,-4.39953655500001));
#327513=CARTESIAN_POINT('Ctrl Pts',(0.00207263999994488,5.2,-4.39953655500001));
#327514=CARTESIAN_POINT('Ctrl Pts',(0.00207263999994488,2.2,-4.39953655500001));
#327515=CARTESIAN_POINT('Ctrl Pts',(0.00293099499994453,12.2,-4.40138894500001));
#327516=CARTESIAN_POINT('Ctrl Pts',(0.00293099499994453,5.2,-4.40138894500001));
#327517=CARTESIAN_POINT('Ctrl Pts',(0.00293099499994453,2.2,-4.40138894500001));
#327518=CARTESIAN_POINT('Ctrl Pts',(0.00379309099994395,12.2,-4.40324403300002));
#327519=CARTESIAN_POINT('Ctrl Pts',(0.00379309099994395,5.2,-4.40324403300002));
#327520=CARTESIAN_POINT('Ctrl Pts',(0.00379309099994395,2.2,-4.40324403300002));
#327521=CARTESIAN_POINT('Ctrl Pts',(0.00465893399994365,12.2,-4.40510180900001));
#327522=CARTESIAN_POINT('Ctrl Pts',(0.00465893399994365,5.2,-4.40510180900001));
#327523=CARTESIAN_POINT('Ctrl Pts',(0.00465893399994365,2.2,-4.40510180900001));
#327524=CARTESIAN_POINT('Ctrl Pts',(0.00552852499994371,12.2,-4.40696226300001));
#327525=CARTESIAN_POINT('Ctrl Pts',(0.00552852499994371,5.2,-4.40696226300001));
#327526=CARTESIAN_POINT('Ctrl Pts',(0.00552852499994371,2.2,-4.40696226300001));
#327527=CARTESIAN_POINT('Ctrl Pts',(0.00640186899994454,12.2,-4.40882538700002));
#327528=CARTESIAN_POINT('Ctrl Pts',(0.00640186899994454,5.2,-4.40882538700002));
#327529=CARTESIAN_POINT('Ctrl Pts',(0.00640186899994454,2.2,-4.40882538700002));
#327530=CARTESIAN_POINT('Ctrl Pts',(0.00727896999994536,12.2,-4.41069117000001));
#327531=CARTESIAN_POINT('Ctrl Pts',(0.00727896999994536,5.2,-4.41069117000001));
#327532=CARTESIAN_POINT('Ctrl Pts',(0.00727896999994536,2.2,-4.41069117000001));
#327533=CARTESIAN_POINT('Ctrl Pts',(0.00815983399994446,12.2,-4.41255960200001));
#327534=CARTESIAN_POINT('Ctrl Pts',(0.00815983399994446,5.2,-4.41255960200001));
#327535=CARTESIAN_POINT('Ctrl Pts',(0.00815983399994446,2.2,-4.41255960200001));
#327536=CARTESIAN_POINT('Ctrl Pts',(0.00904446199994412,12.2,-4.41443067300002));
#327537=CARTESIAN_POINT('Ctrl Pts',(0.00904446199994412,5.2,-4.41443067300002));
#327538=CARTESIAN_POINT('Ctrl Pts',(0.00904446199994412,2.2,-4.41443067300002));
#327539=CARTESIAN_POINT('Ctrl Pts',(0.00993286099994494,12.2,-4.41630437500002));
#327540=CARTESIAN_POINT('Ctrl Pts',(0.00993286099994494,5.2,-4.41630437500002));
#327541=CARTESIAN_POINT('Ctrl Pts',(0.00993286099994494,2.2,-4.41630437500002));
#327542=CARTESIAN_POINT('Ctrl Pts',(0.0108250329999449,12.2,-4.41818069600002));
#327543=CARTESIAN_POINT('Ctrl Pts',(0.0108250329999449,5.2,-4.41818069600002));
#327544=CARTESIAN_POINT('Ctrl Pts',(0.0108250329999449,2.2,-4.41818069600002));
#327545=CARTESIAN_POINT('Ctrl Pts',(0.0117209829999432,12.2,-4.42005962600001));
#327546=CARTESIAN_POINT('Ctrl Pts',(0.0117209829999432,5.2,-4.42005962600001));
#327547=CARTESIAN_POINT('Ctrl Pts',(0.0117209829999432,2.2,-4.42005962600001));
#327548=CARTESIAN_POINT('Ctrl Pts',(0.0126207139999435,12.2,-4.42194115800001));
#327549=CARTESIAN_POINT('Ctrl Pts',(0.0126207139999435,5.2,-4.42194115800001));
#327550=CARTESIAN_POINT('Ctrl Pts',(0.0126207139999435,2.2,-4.42194115800001));
#327551=CARTESIAN_POINT('Ctrl Pts',(0.013524230999945,12.2,-4.42382528100001));
#327552=CARTESIAN_POINT('Ctrl Pts',(0.013524230999945,5.2,-4.42382528100001));
#327553=CARTESIAN_POINT('Ctrl Pts',(0.013524230999945,2.2,-4.42382528100001));
#327554=CARTESIAN_POINT('Ctrl Pts',(0.0144315379999438,12.2,-4.42571198400001));
#327555=CARTESIAN_POINT('Ctrl Pts',(0.0144315379999438,5.2,-4.42571198400001));
#327556=CARTESIAN_POINT('Ctrl Pts',(0.0144315379999438,2.2,-4.42571198400001));
#327557=CARTESIAN_POINT('Ctrl Pts',(0.0153426389999434,12.2,-4.42760125800001));
#327558=CARTESIAN_POINT('Ctrl Pts',(0.0153426389999434,5.2,-4.42760125800001));
#327559=CARTESIAN_POINT('Ctrl Pts',(0.0153426389999434,2.2,-4.42760125800001));
#327560=CARTESIAN_POINT('Ctrl Pts',(0.0162575369999451,12.2,-4.42949309400001));
#327561=CARTESIAN_POINT('Ctrl Pts',(0.0162575369999451,5.2,-4.42949309400001));
#327562=CARTESIAN_POINT('Ctrl Pts',(0.0162575369999451,2.2,-4.42949309400001));
#327563=CARTESIAN_POINT('Ctrl Pts',(0.017176236999944,12.2,-4.43138748200001));
#327564=CARTESIAN_POINT('Ctrl Pts',(0.017176236999944,5.2,-4.43138748200001));
#327565=CARTESIAN_POINT('Ctrl Pts',(0.017176236999944,2.2,-4.43138748200001));
#327566=CARTESIAN_POINT('Ctrl Pts',(0.0180987419999445,12.2,-4.43328441100002));
#327567=CARTESIAN_POINT('Ctrl Pts',(0.0180987419999445,5.2,-4.43328441100002));
#327568=CARTESIAN_POINT('Ctrl Pts',(0.0180987419999445,2.2,-4.43328441100002));
#327569=CARTESIAN_POINT('Ctrl Pts',(0.0190250569999439,12.2,-4.43518387300001));
#327570=CARTESIAN_POINT('Ctrl Pts',(0.0190250569999439,5.2,-4.43518387300001));
#327571=CARTESIAN_POINT('Ctrl Pts',(0.0190250569999439,2.2,-4.43518387300001));
#327572=CARTESIAN_POINT('Ctrl Pts',(0.0199551849999435,12.2,-4.43708585900001));
#327573=CARTESIAN_POINT('Ctrl Pts',(0.0199551849999435,5.2,-4.43708585900001));
#327574=CARTESIAN_POINT('Ctrl Pts',(0.0199551849999435,2.2,-4.43708585900001));
#327575=CARTESIAN_POINT('Ctrl Pts',(0.0208891289999435,12.2,-4.43899035600001));
#327576=CARTESIAN_POINT('Ctrl Pts',(0.0208891289999435,5.2,-4.43899035600001));
#327577=CARTESIAN_POINT('Ctrl Pts',(0.0208891289999435,2.2,-4.43899035600001));
#327578=CARTESIAN_POINT('Ctrl Pts',(0.0218268949999434,12.2,-4.44089735800001));
#327579=CARTESIAN_POINT('Ctrl Pts',(0.0218268949999434,5.2,-4.44089735800001));
#327580=CARTESIAN_POINT('Ctrl Pts',(0.0218268949999434,2.2,-4.44089735800001));
#327581=CARTESIAN_POINT('Ctrl Pts',(0.0227684839999431,12.2,-4.44280685300001));
#327582=CARTESIAN_POINT('Ctrl Pts',(0.0227684839999431,5.2,-4.44280685300001));
#327583=CARTESIAN_POINT('Ctrl Pts',(0.0227684839999431,2.2,-4.44280685300001));
#327584=CARTESIAN_POINT('Ctrl Pts',(0.0237139019999444,12.2,-4.44471883200002));
#327585=CARTESIAN_POINT('Ctrl Pts',(0.0237139019999444,5.2,-4.44471883200002));
#327586=CARTESIAN_POINT('Ctrl Pts',(0.0237139019999444,2.2,-4.44471883200002));
#327587=CARTESIAN_POINT('Ctrl Pts',(0.0246631529999441,12.2,-4.44663328500001));
#327588=CARTESIAN_POINT('Ctrl Pts',(0.0246631529999441,5.2,-4.44663328500001));
#327589=CARTESIAN_POINT('Ctrl Pts',(0.0246631529999441,2.2,-4.44663328500001));
#327590=CARTESIAN_POINT('Ctrl Pts',(0.0256162389999448,12.2,-4.44855020400002));
#327591=CARTESIAN_POINT('Ctrl Pts',(0.0256162389999448,5.2,-4.44855020400002));
#327592=CARTESIAN_POINT('Ctrl Pts',(0.0256162389999448,2.2,-4.44855020400002));
#327593=CARTESIAN_POINT('Ctrl Pts',(0.0265731639999434,12.2,-4.45046957800002));
#327594=CARTESIAN_POINT('Ctrl Pts',(0.0265731639999434,5.2,-4.45046957800002));
#327595=CARTESIAN_POINT('Ctrl Pts',(0.0265731639999434,2.2,-4.45046957800002));
#327596=CARTESIAN_POINT('Ctrl Pts',(0.0275339329999447,12.2,-4.45239139700002));
#327597=CARTESIAN_POINT('Ctrl Pts',(0.0275339329999447,5.2,-4.45239139700002));
#327598=CARTESIAN_POINT('Ctrl Pts',(0.0275339329999447,2.2,-4.45239139700002));
#327599=CARTESIAN_POINT('Ctrl Pts',(0.0284985489999434,12.2,-4.45431565300002));
#327600=CARTESIAN_POINT('Ctrl Pts',(0.0284985489999434,5.2,-4.45431565300002));
#327601=CARTESIAN_POINT('Ctrl Pts',(0.0284985489999434,2.2,-4.45431565300002));
#327602=CARTESIAN_POINT('Ctrl Pts',(0.0294670149999454,12.2,-4.45624233500002));
#327603=CARTESIAN_POINT('Ctrl Pts',(0.0294670149999454,5.2,-4.45624233500002));
#327604=CARTESIAN_POINT('Ctrl Pts',(0.0294670149999454,2.2,-4.45624233500002));
#327605=CARTESIAN_POINT('Ctrl Pts',(0.0304393349999443,12.2,-4.45817143400001));
#327606=CARTESIAN_POINT('Ctrl Pts',(0.0304393349999443,5.2,-4.45817143400001));
#327607=CARTESIAN_POINT('Ctrl Pts',(0.0304393349999443,2.2,-4.45817143400001));
#327608=CARTESIAN_POINT('Ctrl Pts',(0.0314155129999438,12.2,-4.46010294100001));
#327609=CARTESIAN_POINT('Ctrl Pts',(0.0314155129999438,5.2,-4.46010294100001));
#327610=CARTESIAN_POINT('Ctrl Pts',(0.0314155129999438,2.2,-4.46010294100001));
#327611=CARTESIAN_POINT('Ctrl Pts',(0.0323955529999442,12.2,-4.46203684400002));
#327612=CARTESIAN_POINT('Ctrl Pts',(0.0323955529999442,5.2,-4.46203684400002));
#327613=CARTESIAN_POINT('Ctrl Pts',(0.0323955529999442,2.2,-4.46203684400002));
#327614=CARTESIAN_POINT('Ctrl Pts',(0.0333794569999435,12.2,-4.46397313600002));
#327615=CARTESIAN_POINT('Ctrl Pts',(0.0333794569999435,5.2,-4.46397313600002));
#327616=CARTESIAN_POINT('Ctrl Pts',(0.0333794569999435,2.2,-4.46397313600002));
#327617=CARTESIAN_POINT('Ctrl Pts',(0.0343672309999443,12.2,-4.46591180700001));
#327618=CARTESIAN_POINT('Ctrl Pts',(0.0343672309999443,5.2,-4.46591180700001));
#327619=CARTESIAN_POINT('Ctrl Pts',(0.0343672309999443,2.2,-4.46591180700001));
#327620=CARTESIAN_POINT('Ctrl Pts',(0.0353588759999435,12.2,-4.46785284800002));
#327621=CARTESIAN_POINT('Ctrl Pts',(0.0353588759999435,5.2,-4.46785284800002));
#327622=CARTESIAN_POINT('Ctrl Pts',(0.0353588759999435,2.2,-4.46785284800002));
#327623=CARTESIAN_POINT('Ctrl Pts',(0.0363543979999437,12.2,-4.46979624600001));
#327624=CARTESIAN_POINT('Ctrl Pts',(0.0363543979999437,5.2,-4.46979624600001));
#327625=CARTESIAN_POINT('Ctrl Pts',(0.0363543979999437,2.2,-4.46979624600001));
#327626=CARTESIAN_POINT('Ctrl Pts',(0.037353797999945,12.2,-4.47174199600001));
#327627=CARTESIAN_POINT('Ctrl Pts',(0.037353797999945,5.2,-4.47174199600001));
#327628=CARTESIAN_POINT('Ctrl Pts',(0.037353797999945,2.2,-4.47174199600001));
#327629=CARTESIAN_POINT('Ctrl Pts',(0.0383570819999446,12.2,-4.47369008700001));
#327630=CARTESIAN_POINT('Ctrl Pts',(0.0383570819999446,5.2,-4.47369008700001));
#327631=CARTESIAN_POINT('Ctrl Pts',(0.0383570819999446,2.2,-4.47369008700001));
#327632=CARTESIAN_POINT('Ctrl Pts',(0.0393642509999437,12.2,-4.47564050800001));
#327633=CARTESIAN_POINT('Ctrl Pts',(0.0393642509999437,5.2,-4.47564050800001));
#327634=CARTESIAN_POINT('Ctrl Pts',(0.0393642509999437,2.2,-4.47564050800001));
#327635=CARTESIAN_POINT('Ctrl Pts',(0.0403753099999438,12.2,-4.47759325200002));
#327636=CARTESIAN_POINT('Ctrl Pts',(0.0403753099999438,5.2,-4.47759325200002));
#327637=CARTESIAN_POINT('Ctrl Pts',(0.0403753099999438,2.2,-4.47759325200002));
#327638=CARTESIAN_POINT('Ctrl Pts',(0.041390261999944,12.2,-4.47954830700001));
#327639=CARTESIAN_POINT('Ctrl Pts',(0.041390261999944,5.2,-4.47954830700001));
#327640=CARTESIAN_POINT('Ctrl Pts',(0.041390261999944,2.2,-4.47954830700001));
#327641=CARTESIAN_POINT('Ctrl Pts',(0.0424091099999446,12.2,-4.48150566500002));
#327642=CARTESIAN_POINT('Ctrl Pts',(0.0424091099999446,5.2,-4.48150566500002));
#327643=CARTESIAN_POINT('Ctrl Pts',(0.0424091099999446,2.2,-4.48150566500002));
#327644=CARTESIAN_POINT('Ctrl Pts',(0.0434318589999438,12.2,-4.48346531700002));
#327645=CARTESIAN_POINT('Ctrl Pts',(0.0434318589999438,5.2,-4.48346531700002));
#327646=CARTESIAN_POINT('Ctrl Pts',(0.0434318589999438,2.2,-4.48346531700002));
#327647=CARTESIAN_POINT('Ctrl Pts',(0.044458510999944,12.2,-4.48542725200001));
#327648=CARTESIAN_POINT('Ctrl Pts',(0.044458510999944,5.2,-4.48542725200001));
#327649=CARTESIAN_POINT('Ctrl Pts',(0.044458510999944,2.2,-4.48542725200001));
#327650=CARTESIAN_POINT('Ctrl Pts',(0.0454890689999432,12.2,-4.48739146100001));
#327651=CARTESIAN_POINT('Ctrl Pts',(0.0454890689999432,5.2,-4.48739146100001));
#327652=CARTESIAN_POINT('Ctrl Pts',(0.0454890689999432,2.2,-4.48739146100001));
#327653=CARTESIAN_POINT('Ctrl Pts',(0.046523537999944,12.2,-4.48935793600001));
#327654=CARTESIAN_POINT('Ctrl Pts',(0.046523537999944,5.2,-4.48935793600001));
#327655=CARTESIAN_POINT('Ctrl Pts',(0.046523537999944,2.2,-4.48935793600001));
#327656=CARTESIAN_POINT('Ctrl Pts',(0.0475619189999443,12.2,-4.49132666500001));
#327657=CARTESIAN_POINT('Ctrl Pts',(0.0475619189999443,5.2,-4.49132666500001));
#327658=CARTESIAN_POINT('Ctrl Pts',(0.0475619189999443,2.2,-4.49132666500001));
#327659=CARTESIAN_POINT('Ctrl Pts',(0.0486042179999446,12.2,-4.49329764200002));
#327660=CARTESIAN_POINT('Ctrl Pts',(0.0486042179999446,5.2,-4.49329764200002));
#327661=CARTESIAN_POINT('Ctrl Pts',(0.0486042179999446,2.2,-4.49329764200002));
#327662=CARTESIAN_POINT('Ctrl Pts',(0.049650436999944,12.2,-4.49527085400002));
#327663=CARTESIAN_POINT('Ctrl Pts',(0.049650436999944,5.2,-4.49527085400002));
#327664=CARTESIAN_POINT('Ctrl Pts',(0.049650436999944,2.2,-4.49527085400002));
#327665=CARTESIAN_POINT('Ctrl Pts',(0.0507005789999437,12.2,-4.49724629400002));
#327666=CARTESIAN_POINT('Ctrl Pts',(0.0507005789999437,5.2,-4.49724629400002));
#327667=CARTESIAN_POINT('Ctrl Pts',(0.0507005789999437,2.2,-4.49724629400002));
#327668=CARTESIAN_POINT('Ctrl Pts',(0.0517546479999442,12.2,-4.49922395100002));
#327669=CARTESIAN_POINT('Ctrl Pts',(0.0517546479999442,5.2,-4.49922395100002));
#327670=CARTESIAN_POINT('Ctrl Pts',(0.0517546479999442,2.2,-4.49922395100002));
#327671=CARTESIAN_POINT('Ctrl Pts',(0.0528126449999444,12.2,-4.50120381900001));
#327672=CARTESIAN_POINT('Ctrl Pts',(0.0528126449999444,5.2,-4.50120381900001));
#327673=CARTESIAN_POINT('Ctrl Pts',(0.0528126449999444,2.2,-4.50120381900001));
#327674=CARTESIAN_POINT('Ctrl Pts',(0.0538745769999438,12.2,-4.50318588400001));
#327675=CARTESIAN_POINT('Ctrl Pts',(0.0538745769999438,5.2,-4.50318588400001));
#327676=CARTESIAN_POINT('Ctrl Pts',(0.0538745769999438,2.2,-4.50318588400001));
#327677=CARTESIAN_POINT('Ctrl Pts',(0.0549404449999447,12.2,-4.50517014000001));
#327678=CARTESIAN_POINT('Ctrl Pts',(0.0549404449999447,5.2,-4.50517014000001));
#327679=CARTESIAN_POINT('Ctrl Pts',(0.0549404449999447,2.2,-4.50517014000001));
#327680=CARTESIAN_POINT('Ctrl Pts',(0.0560102509999438,12.2,-4.50715657500002));
#327681=CARTESIAN_POINT('Ctrl Pts',(0.0560102509999438,5.2,-4.50715657500002));
#327682=CARTESIAN_POINT('Ctrl Pts',(0.0560102509999438,2.2,-4.50715657500002));
#327683=CARTESIAN_POINT('Ctrl Pts',(0.0570840009999451,12.2,-4.50914518300001));
#327684=CARTESIAN_POINT('Ctrl Pts',(0.0570840009999451,5.2,-4.50914518300001));
#327685=CARTESIAN_POINT('Ctrl Pts',(0.0570840009999451,2.2,-4.50914518300001));
#327686=CARTESIAN_POINT('Ctrl Pts',(0.0581616969999443,12.2,-4.51113595100002));
#327687=CARTESIAN_POINT('Ctrl Pts',(0.0581616969999443,5.2,-4.51113595100002));
#327688=CARTESIAN_POINT('Ctrl Pts',(0.0581616969999443,2.2,-4.51113595100002));
#327689=CARTESIAN_POINT('Ctrl Pts',(0.0592433409999438,12.2,-4.51312887200002));
#327690=CARTESIAN_POINT('Ctrl Pts',(0.0592433409999438,5.2,-4.51312887200002));
#327691=CARTESIAN_POINT('Ctrl Pts',(0.0592433409999438,2.2,-4.51312887200002));
#327692=CARTESIAN_POINT('Ctrl Pts',(0.0603289369999449,12.2,-4.51512393600002));
#327693=CARTESIAN_POINT('Ctrl Pts',(0.0603289369999449,5.2,-4.51512393600002));
#327694=CARTESIAN_POINT('Ctrl Pts',(0.0603289369999449,2.2,-4.51512393600002));
#327695=CARTESIAN_POINT('Ctrl Pts',(0.0614184889999447,12.2,-4.51712113400002));
#327696=CARTESIAN_POINT('Ctrl Pts',(0.0614184889999447,5.2,-4.51712113400002));
#327697=CARTESIAN_POINT('Ctrl Pts',(0.0614184889999447,2.2,-4.51712113400002));
#327698=CARTESIAN_POINT('Ctrl Pts',(0.0625119979999444,12.2,-4.51912045700002));
#327699=CARTESIAN_POINT('Ctrl Pts',(0.0625119979999444,5.2,-4.51912045700002));
#327700=CARTESIAN_POINT('Ctrl Pts',(0.0625119979999444,2.2,-4.51912045700002));
#327701=CARTESIAN_POINT('Ctrl Pts',(0.0636094699999445,12.2,-4.52112189500002));
#327702=CARTESIAN_POINT('Ctrl Pts',(0.0636094699999445,5.2,-4.52112189500002));
#327703=CARTESIAN_POINT('Ctrl Pts',(0.0636094699999445,2.2,-4.52112189500002));
#327704=CARTESIAN_POINT('Ctrl Pts',(0.0647109049999439,12.2,-4.52312544000002));
#327705=CARTESIAN_POINT('Ctrl Pts',(0.0647109049999439,5.2,-4.52312544000002));
#327706=CARTESIAN_POINT('Ctrl Pts',(0.0647109049999439,2.2,-4.52312544000002));
#327707=CARTESIAN_POINT('Ctrl Pts',(0.0658163089999442,12.2,-4.52513108000002));
#327708=CARTESIAN_POINT('Ctrl Pts',(0.0658163089999442,5.2,-4.52513108000002));
#327709=CARTESIAN_POINT('Ctrl Pts',(0.0658163089999442,2.2,-4.52513108000002));
#327710=CARTESIAN_POINT('Ctrl Pts',(0.0669256809999441,12.2,-4.52713880800002));
#327711=CARTESIAN_POINT('Ctrl Pts',(0.0669256809999441,5.2,-4.52713880800002));
#327712=CARTESIAN_POINT('Ctrl Pts',(0.0669256809999441,2.2,-4.52713880800002));
#327713=CARTESIAN_POINT('Ctrl Pts',(0.0680390289999444,12.2,-4.52914861400001));
#327714=CARTESIAN_POINT('Ctrl Pts',(0.0680390289999444,5.2,-4.52914861400001));
#327715=CARTESIAN_POINT('Ctrl Pts',(0.0680390289999444,2.2,-4.52914861400001));
#327716=CARTESIAN_POINT('Ctrl Pts',(0.0691563519999438,12.2,-4.53116048900001));
#327717=CARTESIAN_POINT('Ctrl Pts',(0.0691563519999438,5.2,-4.53116048900001));
#327718=CARTESIAN_POINT('Ctrl Pts',(0.0691563519999438,2.2,-4.53116048900001));
#327719=CARTESIAN_POINT('Ctrl Pts',(0.070277653999945,12.2,-4.53317442400001));
#327720=CARTESIAN_POINT('Ctrl Pts',(0.070277653999945,5.2,-4.53317442400001));
#327721=CARTESIAN_POINT('Ctrl Pts',(0.070277653999945,2.2,-4.53317442400001));
#327722=CARTESIAN_POINT('Ctrl Pts',(0.0714029399999438,12.2,-4.53519041000002));
#327723=CARTESIAN_POINT('Ctrl Pts',(0.0714029399999438,5.2,-4.53519041000002));
#327724=CARTESIAN_POINT('Ctrl Pts',(0.0714029399999438,2.2,-4.53519041000002));
#327725=CARTESIAN_POINT('Ctrl Pts',(0.0725322099999437,12.2,-4.53720843600002));
#327726=CARTESIAN_POINT('Ctrl Pts',(0.0725322099999437,5.2,-4.53720843600002));
#327727=CARTESIAN_POINT('Ctrl Pts',(0.0725322099999437,2.2,-4.53720843600002));
#327728=CARTESIAN_POINT('Ctrl Pts',(0.073665468999945,12.2,-4.53922849500001));
#327729=CARTESIAN_POINT('Ctrl Pts',(0.073665468999945,5.2,-4.53922849500001));
#327730=CARTESIAN_POINT('Ctrl Pts',(0.073665468999945,2.2,-4.53922849500001));
#327731=CARTESIAN_POINT('Ctrl Pts',(0.0748027189999445,12.2,-4.54125057700002));
#327732=CARTESIAN_POINT('Ctrl Pts',(0.0748027189999445,5.2,-4.54125057700002));
#327733=CARTESIAN_POINT('Ctrl Pts',(0.0748027189999445,2.2,-4.54125057700002));
#327734=CARTESIAN_POINT('Ctrl Pts',(0.0759439619999436,12.2,-4.54327467100001));
#327735=CARTESIAN_POINT('Ctrl Pts',(0.0759439619999436,5.2,-4.54327467100001));
#327736=CARTESIAN_POINT('Ctrl Pts',(0.0759439619999436,2.2,-4.54327467100001));
#327737=CARTESIAN_POINT('Ctrl Pts',(0.0770892039999438,12.2,-4.54530077100001));
#327738=CARTESIAN_POINT('Ctrl Pts',(0.0770892039999438,5.2,-4.54530077100001));
#327739=CARTESIAN_POINT('Ctrl Pts',(0.0770892039999438,2.2,-4.54530077100001));
#327740=CARTESIAN_POINT('Ctrl Pts',(0.078238444999944,12.2,-4.54732886600001));
#327741=CARTESIAN_POINT('Ctrl Pts',(0.078238444999944,5.2,-4.54732886600001));
#327742=CARTESIAN_POINT('Ctrl Pts',(0.078238444999944,2.2,-4.54732886600001));
#327743=CARTESIAN_POINT('Ctrl Pts',(0.0793916879999446,12.2,-4.54935894600002));
#327744=CARTESIAN_POINT('Ctrl Pts',(0.0793916879999446,5.2,-4.54935894600002));
#327745=CARTESIAN_POINT('Ctrl Pts',(0.0793916879999446,2.2,-4.54935894600002));
#327746=CARTESIAN_POINT('Ctrl Pts',(0.0805489369999446,12.2,-4.55139100400002));
#327747=CARTESIAN_POINT('Ctrl Pts',(0.0805489369999446,5.2,-4.55139100400002));
#327748=CARTESIAN_POINT('Ctrl Pts',(0.0805489369999446,2.2,-4.55139100400002));
#327749=CARTESIAN_POINT('Ctrl Pts',(0.0817101939999443,12.2,-4.55342503000002));
#327750=CARTESIAN_POINT('Ctrl Pts',(0.0817101939999443,5.2,-4.55342503000002));
#327751=CARTESIAN_POINT('Ctrl Pts',(0.0817101939999443,2.2,-4.55342503000002));
#327752=CARTESIAN_POINT('Ctrl Pts',(0.0828754619999439,12.2,-4.55546101400001));
#327753=CARTESIAN_POINT('Ctrl Pts',(0.0828754619999439,5.2,-4.55546101400001));
#327754=CARTESIAN_POINT('Ctrl Pts',(0.0828754619999439,2.2,-4.55546101400001));
#327755=CARTESIAN_POINT('Ctrl Pts',(0.0840447429999447,12.2,-4.55749894800002));
#327756=CARTESIAN_POINT('Ctrl Pts',(0.0840447429999447,5.2,-4.55749894800002));
#327757=CARTESIAN_POINT('Ctrl Pts',(0.0840447429999447,2.2,-4.55749894800002));
#327758=CARTESIAN_POINT('Ctrl Pts',(0.0852180419999449,12.2,-4.55953882200001));
#327759=CARTESIAN_POINT('Ctrl Pts',(0.0852180419999449,5.2,-4.55953882200001));
#327760=CARTESIAN_POINT('Ctrl Pts',(0.0852180419999449,2.2,-4.55953882200001));
#327761=CARTESIAN_POINT('Ctrl Pts',(0.0863953609999446,12.2,-4.56158062800001));
#327762=CARTESIAN_POINT('Ctrl Pts',(0.0863953609999446,5.2,-4.56158062800001));
#327763=CARTESIAN_POINT('Ctrl Pts',(0.0863953609999446,2.2,-4.56158062800001));
#327764=CARTESIAN_POINT('Ctrl Pts',(0.087576699999945,12.2,-4.56362435600001));
#327765=CARTESIAN_POINT('Ctrl Pts',(0.087576699999945,5.2,-4.56362435600001));
#327766=CARTESIAN_POINT('Ctrl Pts',(0.087576699999945,2.2,-4.56362435600001));
#327767=CARTESIAN_POINT('Ctrl Pts',(0.0887620659999444,12.2,-4.56566999600001));
#327768=CARTESIAN_POINT('Ctrl Pts',(0.0887620659999444,5.2,-4.56566999600001));
#327769=CARTESIAN_POINT('Ctrl Pts',(0.0887620659999444,2.2,-4.56566999600001));
#327770=CARTESIAN_POINT('Ctrl Pts',(0.089951457999945,12.2,-4.56771754100001));
#327771=CARTESIAN_POINT('Ctrl Pts',(0.089951457999945,5.2,-4.56771754100001));
#327772=CARTESIAN_POINT('Ctrl Pts',(0.089951457999945,2.2,-4.56771754100001));
#327773=CARTESIAN_POINT('Ctrl Pts',(0.0911448799999448,12.2,-4.56976698000001));
#327774=CARTESIAN_POINT('Ctrl Pts',(0.0911448799999448,5.2,-4.56976698000001));
#327775=CARTESIAN_POINT('Ctrl Pts',(0.0911448799999448,2.2,-4.56976698000001));
#327776=CARTESIAN_POINT('Ctrl Pts',(0.0923423349999453,12.2,-4.57181830600002));
#327777=CARTESIAN_POINT('Ctrl Pts',(0.0923423349999453,5.2,-4.57181830600002));
#327778=CARTESIAN_POINT('Ctrl Pts',(0.0923423349999453,2.2,-4.57181830600002));
#327779=CARTESIAN_POINT('Ctrl Pts',(0.0935438259999444,12.2,-4.57387150700002));
#327780=CARTESIAN_POINT('Ctrl Pts',(0.0935438259999444,5.2,-4.57387150700002));
#327781=CARTESIAN_POINT('Ctrl Pts',(0.0935438259999444,2.2,-4.57387150700002));
#327782=CARTESIAN_POINT('Ctrl Pts',(0.0947493549999445,12.2,-4.57592657700001));
#327783=CARTESIAN_POINT('Ctrl Pts',(0.0947493549999445,5.2,-4.57592657700001));
#327784=CARTESIAN_POINT('Ctrl Pts',(0.0947493549999445,2.2,-4.57592657700001));
#327785=CARTESIAN_POINT('Ctrl Pts',(0.0959589249999449,12.2,-4.57798350600001));
#327786=CARTESIAN_POINT('Ctrl Pts',(0.0959589249999449,5.2,-4.57798350600001));
#327787=CARTESIAN_POINT('Ctrl Pts',(0.0959589249999449,2.2,-4.57798350600001));
#327788=CARTESIAN_POINT('Ctrl Pts',(0.0971725369999443,12.2,-4.58004228400001));
#327789=CARTESIAN_POINT('Ctrl Pts',(0.0971725369999443,5.2,-4.58004228400001));
#327790=CARTESIAN_POINT('Ctrl Pts',(0.0971725369999443,2.2,-4.58004228400001));
#327791=CARTESIAN_POINT('Ctrl Pts',(0.0983901959999434,12.2,-4.58210290300002));
#327792=CARTESIAN_POINT('Ctrl Pts',(0.0983901959999434,5.2,-4.58210290300002));
#327793=CARTESIAN_POINT('Ctrl Pts',(0.0983901959999434,2.2,-4.58210290300002));
#327794=CARTESIAN_POINT('Ctrl Pts',(0.0996119039999444,12.2,-4.58416535200001));
#327795=CARTESIAN_POINT('Ctrl Pts',(0.0996119039999444,5.2,-4.58416535200001));
#327796=CARTESIAN_POINT('Ctrl Pts',(0.0996119039999444,2.2,-4.58416535200001));
#327797=CARTESIAN_POINT('Ctrl Pts',(0.100837662999943,12.2,-4.58622962500002));
#327798=CARTESIAN_POINT('Ctrl Pts',(0.100837662999943,5.2,-4.58622962500002));
#327799=CARTESIAN_POINT('Ctrl Pts',(0.100837662999943,2.2,-4.58622962500002));
#327800=CARTESIAN_POINT('Ctrl Pts',(0.102067473999944,12.2,-4.58829571100001));
#327801=CARTESIAN_POINT('Ctrl Pts',(0.102067473999944,5.2,-4.58829571100001));
#327802=CARTESIAN_POINT('Ctrl Pts',(0.102067473999944,2.2,-4.58829571100001));
#327803=CARTESIAN_POINT('Ctrl Pts',(0.103301341999943,12.2,-4.59036360200002));
#327804=CARTESIAN_POINT('Ctrl Pts',(0.103301341999943,5.2,-4.59036360200002));
#327805=CARTESIAN_POINT('Ctrl Pts',(0.103301341999943,2.2,-4.59036360200002));
#327806=CARTESIAN_POINT('Ctrl Pts',(0.104539268999944,12.2,-4.59243328800001));
#327807=CARTESIAN_POINT('Ctrl Pts',(0.104539268999944,5.2,-4.59243328800001));
#327808=CARTESIAN_POINT('Ctrl Pts',(0.104539268999944,2.2,-4.59243328800001));
#327809=CARTESIAN_POINT('Ctrl Pts',(0.105781256999944,12.2,-4.59450476100002));
#327810=CARTESIAN_POINT('Ctrl Pts',(0.105781256999944,5.2,-4.59450476100002));
#327811=CARTESIAN_POINT('Ctrl Pts',(0.105781256999944,2.2,-4.59450476100002));
#327812=CARTESIAN_POINT('Ctrl Pts',(0.107027308999944,12.2,-4.59657801100001));
#327813=CARTESIAN_POINT('Ctrl Pts',(0.107027308999944,5.2,-4.59657801100001));
#327814=CARTESIAN_POINT('Ctrl Pts',(0.107027308999944,2.2,-4.59657801100001));
#327815=CARTESIAN_POINT('Ctrl Pts',(0.108277424999944,12.2,-4.59865303000001));
#327816=CARTESIAN_POINT('Ctrl Pts',(0.108277424999944,5.2,-4.59865303000001));
#327817=CARTESIAN_POINT('Ctrl Pts',(0.108277424999944,2.2,-4.59865303000001));
#327818=CARTESIAN_POINT('Ctrl Pts',(0.109531610999944,12.2,-4.60072980900001));
#327819=CARTESIAN_POINT('Ctrl Pts',(0.109531610999944,5.2,-4.60072980900001));
#327820=CARTESIAN_POINT('Ctrl Pts',(0.109531610999944,2.2,-4.60072980900001));
#327821=CARTESIAN_POINT('Ctrl Pts',(0.110789867999944,12.2,-4.60280833800002));
#327822=CARTESIAN_POINT('Ctrl Pts',(0.110789867999944,5.2,-4.60280833800002));
#327823=CARTESIAN_POINT('Ctrl Pts',(0.110789867999944,2.2,-4.60280833800002));
#327824=CARTESIAN_POINT('Ctrl Pts',(0.112052197999944,12.2,-4.60488860800002));
#327825=CARTESIAN_POINT('Ctrl Pts',(0.112052197999944,5.2,-4.60488860800002));
#327826=CARTESIAN_POINT('Ctrl Pts',(0.112052197999944,2.2,-4.60488860800002));
#327827=CARTESIAN_POINT('Ctrl Pts',(0.113318603999945,12.2,-4.60697061200001));
#327828=CARTESIAN_POINT('Ctrl Pts',(0.113318603999945,5.2,-4.60697061200001));
#327829=CARTESIAN_POINT('Ctrl Pts',(0.113318603999945,2.2,-4.60697061200001));
#327830=CARTESIAN_POINT('Ctrl Pts',(0.114589087999944,12.2,-4.60905434000002));
#327831=CARTESIAN_POINT('Ctrl Pts',(0.114589087999944,5.2,-4.60905434000002));
#327832=CARTESIAN_POINT('Ctrl Pts',(0.114589087999944,2.2,-4.60905434000002));
#327833=CARTESIAN_POINT('Ctrl Pts',(0.115863651999945,12.2,-4.61113978200002));
#327834=CARTESIAN_POINT('Ctrl Pts',(0.115863651999945,5.2,-4.61113978200002));
#327835=CARTESIAN_POINT('Ctrl Pts',(0.115863651999945,2.2,-4.61113978200002));
#327836=CARTESIAN_POINT('Ctrl Pts',(0.117142298999945,12.2,-4.61322693100001));
#327837=CARTESIAN_POINT('Ctrl Pts',(0.117142298999945,5.2,-4.61322693100001));
#327838=CARTESIAN_POINT('Ctrl Pts',(0.117142298999945,2.2,-4.61322693100001));
#327839=CARTESIAN_POINT('Ctrl Pts',(0.118425031999945,12.2,-4.61531577700002));
#327840=CARTESIAN_POINT('Ctrl Pts',(0.118425031999945,5.2,-4.61531577700002));
#327841=CARTESIAN_POINT('Ctrl Pts',(0.118425031999945,2.2,-4.61531577700002));
#327842=CARTESIAN_POINT('Ctrl Pts',(0.119711850999943,12.2,-4.61740631000001));
#327843=CARTESIAN_POINT('Ctrl Pts',(0.119711850999943,5.2,-4.61740631000001));
#327844=CARTESIAN_POINT('Ctrl Pts',(0.119711850999943,2.2,-4.61740631000001));
#327845=CARTESIAN_POINT('Ctrl Pts',(0.121002760999945,12.2,-4.61949852400001));
#327846=CARTESIAN_POINT('Ctrl Pts',(0.121002760999945,5.2,-4.61949852400001));
#327847=CARTESIAN_POINT('Ctrl Pts',(0.121002760999945,2.2,-4.61949852400001));
#327848=CARTESIAN_POINT('Ctrl Pts',(0.122297761999944,12.2,-4.62159240800001));
#327849=CARTESIAN_POINT('Ctrl Pts',(0.122297761999944,5.2,-4.62159240800001));
#327850=CARTESIAN_POINT('Ctrl Pts',(0.122297761999944,2.2,-4.62159240800001));
#327851=CARTESIAN_POINT('Ctrl Pts',(0.123596857999945,12.2,-4.62368795400002));
#327852=CARTESIAN_POINT('Ctrl Pts',(0.123596857999945,5.2,-4.62368795400002));
#327853=CARTESIAN_POINT('Ctrl Pts',(0.123596857999945,2.2,-4.62368795400002));
#327854=CARTESIAN_POINT('Ctrl Pts',(0.124900049999944,12.2,-4.62578515200001));
#327855=CARTESIAN_POINT('Ctrl Pts',(0.124900049999944,5.2,-4.62578515200001));
#327856=CARTESIAN_POINT('Ctrl Pts',(0.124900049999944,2.2,-4.62578515200001));
#327857=CARTESIAN_POINT('Ctrl Pts',(0.126207341999944,12.2,-4.62788399400001));
#327858=CARTESIAN_POINT('Ctrl Pts',(0.126207341999944,5.2,-4.62788399400001));
#327859=CARTESIAN_POINT('Ctrl Pts',(0.126207341999944,2.2,-4.62788399400001));
#327860=CARTESIAN_POINT('Ctrl Pts',(0.127518733999944,12.2,-4.62998447200002));
#327861=CARTESIAN_POINT('Ctrl Pts',(0.127518733999944,5.2,-4.62998447200002));
#327862=CARTESIAN_POINT('Ctrl Pts',(0.127518733999944,2.2,-4.62998447200002));
#327863=CARTESIAN_POINT('Ctrl Pts',(0.128834229999945,12.2,-4.63208657500001));
#327864=CARTESIAN_POINT('Ctrl Pts',(0.128834229999945,5.2,-4.63208657500001));
#327865=CARTESIAN_POINT('Ctrl Pts',(0.128834229999945,2.2,-4.63208657500001));
#327866=CARTESIAN_POINT('Ctrl Pts',(0.130153831999945,12.2,-4.63419029600002));
#327867=CARTESIAN_POINT('Ctrl Pts',(0.130153831999945,5.2,-4.63419029600002));
#327868=CARTESIAN_POINT('Ctrl Pts',(0.130153831999945,2.2,-4.63419029600002));
#327869=CARTESIAN_POINT('Ctrl Pts',(0.131477540999944,12.2,-4.63629562500001));
#327870=CARTESIAN_POINT('Ctrl Pts',(0.131477540999944,5.2,-4.63629562500001));
#327871=CARTESIAN_POINT('Ctrl Pts',(0.131477540999944,2.2,-4.63629562500001));
#327872=CARTESIAN_POINT('Ctrl Pts',(0.132805359999945,12.2,-4.63840255500001));
#327873=CARTESIAN_POINT('Ctrl Pts',(0.132805359999945,5.2,-4.63840255500001));
#327874=CARTESIAN_POINT('Ctrl Pts',(0.132805359999945,2.2,-4.63840255500001));
#327875=CARTESIAN_POINT('Ctrl Pts',(0.134137289999944,12.2,-4.64051107500001));
#327876=CARTESIAN_POINT('Ctrl Pts',(0.134137289999944,5.2,-4.64051107500001));
#327877=CARTESIAN_POINT('Ctrl Pts',(0.134137289999944,2.2,-4.64051107500001));
#327878=CARTESIAN_POINT('Ctrl Pts',(0.135473335999944,12.2,-4.64262117800001));
#327879=CARTESIAN_POINT('Ctrl Pts',(0.135473335999944,5.2,-4.64262117800001));
#327880=CARTESIAN_POINT('Ctrl Pts',(0.135473335999944,2.2,-4.64262117800001));
#327881=CARTESIAN_POINT('Ctrl Pts',(0.136813497999944,12.2,-4.64473285400001));
#327882=CARTESIAN_POINT('Ctrl Pts',(0.136813497999944,5.2,-4.64473285400001));
#327883=CARTESIAN_POINT('Ctrl Pts',(0.136813497999944,2.2,-4.64473285400001));
#327884=CARTESIAN_POINT('Ctrl Pts',(0.138157777999943,12.2,-4.64684609400001));
#327885=CARTESIAN_POINT('Ctrl Pts',(0.138157777999943,5.2,-4.64684609400001));
#327886=CARTESIAN_POINT('Ctrl Pts',(0.138157777999943,2.2,-4.64684609400001));
#327887=CARTESIAN_POINT('Ctrl Pts',(0.139506177999945,12.2,-4.64896089100002));
#327888=CARTESIAN_POINT('Ctrl Pts',(0.139506177999945,5.2,-4.64896089100002));
#327889=CARTESIAN_POINT('Ctrl Pts',(0.139506177999945,2.2,-4.64896089100002));
#327890=CARTESIAN_POINT('Ctrl Pts',(0.140858699999944,12.2,-4.65107723400001));
#327891=CARTESIAN_POINT('Ctrl Pts',(0.140858699999944,5.2,-4.65107723400001));
#327892=CARTESIAN_POINT('Ctrl Pts',(0.140858699999944,2.2,-4.65107723400001));
#327893=CARTESIAN_POINT('Ctrl Pts',(0.142215347999944,12.2,-4.65319511600002));
#327894=CARTESIAN_POINT('Ctrl Pts',(0.142215347999944,5.2,-4.65319511600002));
#327895=CARTESIAN_POINT('Ctrl Pts',(0.142215347999944,2.2,-4.65319511600002));
#327896=CARTESIAN_POINT('Ctrl Pts',(0.143576121999944,12.2,-4.65531452700001));
#327897=CARTESIAN_POINT('Ctrl Pts',(0.143576121999944,5.2,-4.65531452700001));
#327898=CARTESIAN_POINT('Ctrl Pts',(0.143576121999944,2.2,-4.65531452700001));
#327899=CARTESIAN_POINT('Ctrl Pts',(0.144941025999945,12.2,-4.65743546000001));
#327900=CARTESIAN_POINT('Ctrl Pts',(0.144941025999945,5.2,-4.65743546000001));
#327901=CARTESIAN_POINT('Ctrl Pts',(0.144941025999945,2.2,-4.65743546000001));
#327902=CARTESIAN_POINT('Ctrl Pts',(0.146310058999944,12.2,-4.65955790400002));
#327903=CARTESIAN_POINT('Ctrl Pts',(0.146310058999944,5.2,-4.65955790400002));
#327904=CARTESIAN_POINT('Ctrl Pts',(0.146310058999944,2.2,-4.65955790400002));
#327905=CARTESIAN_POINT('Ctrl Pts',(0.147683225999945,12.2,-4.66168185200001));
#327906=CARTESIAN_POINT('Ctrl Pts',(0.147683225999945,5.2,-4.66168185200001));
#327907=CARTESIAN_POINT('Ctrl Pts',(0.147683225999945,2.2,-4.66168185200001));
#327908=CARTESIAN_POINT('Ctrl Pts',(0.149060527999945,12.2,-4.66380729400001));
#327909=CARTESIAN_POINT('Ctrl Pts',(0.149060527999945,5.2,-4.66380729400001));
#327910=CARTESIAN_POINT('Ctrl Pts',(0.149060527999945,2.2,-4.66380729400001));
#327911=CARTESIAN_POINT('Ctrl Pts',(0.150441966999945,12.2,-4.66593422200001));
#327912=CARTESIAN_POINT('Ctrl Pts',(0.150441966999945,5.2,-4.66593422200001));
#327913=CARTESIAN_POINT('Ctrl Pts',(0.150441966999945,2.2,-4.66593422200001));
#327914=CARTESIAN_POINT('Ctrl Pts',(0.151827543999945,12.2,-4.66806262700001));
#327915=CARTESIAN_POINT('Ctrl Pts',(0.151827543999945,5.2,-4.66806262700001));
#327916=CARTESIAN_POINT('Ctrl Pts',(0.151827543999945,2.2,-4.66806262700001));
#327917=CARTESIAN_POINT('Ctrl Pts',(0.153217260999944,12.2,-4.67019250200002));
#327918=CARTESIAN_POINT('Ctrl Pts',(0.153217260999944,5.2,-4.67019250200002));
#327919=CARTESIAN_POINT('Ctrl Pts',(0.153217260999944,2.2,-4.67019250200002));
#327920=CARTESIAN_POINT('Ctrl Pts',(0.154611121999944,12.2,-4.67232383600001));
#327921=CARTESIAN_POINT('Ctrl Pts',(0.154611121999944,5.2,-4.67232383600001));
#327922=CARTESIAN_POINT('Ctrl Pts',(0.154611121999944,2.2,-4.67232383600001));
#327923=CARTESIAN_POINT('Ctrl Pts',(0.156009126999944,12.2,-4.67445662200001));
#327924=CARTESIAN_POINT('Ctrl Pts',(0.156009126999944,5.2,-4.67445662200001));
#327925=CARTESIAN_POINT('Ctrl Pts',(0.156009126999944,2.2,-4.67445662200001));
#327926=CARTESIAN_POINT('Ctrl Pts',(0.157411277999945,12.2,-4.67659084900002));
#327927=CARTESIAN_POINT('Ctrl Pts',(0.157411277999945,5.2,-4.67659084900002));
#327928=CARTESIAN_POINT('Ctrl Pts',(0.157411277999945,2.2,-4.67659084900002));
#327929=CARTESIAN_POINT('Ctrl Pts',(0.158817578999945,12.2,-4.67872651000001));
#327930=CARTESIAN_POINT('Ctrl Pts',(0.158817578999945,5.2,-4.67872651000001));
#327931=CARTESIAN_POINT('Ctrl Pts',(0.158817578999945,2.2,-4.67872651000001));
#327932=CARTESIAN_POINT('Ctrl Pts',(0.160228028999944,12.2,-4.68086359800001));
#327933=CARTESIAN_POINT('Ctrl Pts',(0.160228028999944,5.2,-4.68086359800001));
#327934=CARTESIAN_POINT('Ctrl Pts',(0.160228028999944,2.2,-4.68086359800001));
#327935=CARTESIAN_POINT('Ctrl Pts',(0.161642630999944,12.2,-4.68300210100002));
#327936=CARTESIAN_POINT('Ctrl Pts',(0.161642630999944,5.2,-4.68300210100002));
#327937=CARTESIAN_POINT('Ctrl Pts',(0.161642630999944,2.2,-4.68300210100002));
#327938=CARTESIAN_POINT('Ctrl Pts',(0.163061386999944,12.2,-4.68514201200001));
#327939=CARTESIAN_POINT('Ctrl Pts',(0.163061386999944,5.2,-4.68514201200001));
#327940=CARTESIAN_POINT('Ctrl Pts',(0.163061386999944,2.2,-4.68514201200001));
#327941=CARTESIAN_POINT('Ctrl Pts',(0.164484299999945,12.2,-4.68728332300001));
#327942=CARTESIAN_POINT('Ctrl Pts',(0.164484299999945,5.2,-4.68728332300001));
#327943=CARTESIAN_POINT('Ctrl Pts',(0.164484299999945,2.2,-4.68728332300001));
#327944=CARTESIAN_POINT('Ctrl Pts',(0.165911369999945,12.2,-4.68942602400002));
#327945=CARTESIAN_POINT('Ctrl Pts',(0.165911369999945,5.2,-4.68942602400002));
#327946=CARTESIAN_POINT('Ctrl Pts',(0.165911369999945,2.2,-4.68942602400002));
#327947=CARTESIAN_POINT('Ctrl Pts',(0.167342598999944,12.2,-4.69157010700001));
#327948=CARTESIAN_POINT('Ctrl Pts',(0.167342598999944,5.2,-4.69157010700001));
#327949=CARTESIAN_POINT('Ctrl Pts',(0.167342598999944,2.2,-4.69157010700001));
#327950=CARTESIAN_POINT('Ctrl Pts',(0.168777989999944,12.2,-4.69371556500001));
#327951=CARTESIAN_POINT('Ctrl Pts',(0.168777989999944,5.2,-4.69371556500001));
#327952=CARTESIAN_POINT('Ctrl Pts',(0.168777989999944,2.2,-4.69371556500001));
#327953=CARTESIAN_POINT('Ctrl Pts',(0.170217542999945,12.2,-4.69586238700002));
#327954=CARTESIAN_POINT('Ctrl Pts',(0.170217542999945,5.2,-4.69586238700002));
#327955=CARTESIAN_POINT('Ctrl Pts',(0.170217542999945,2.2,-4.69586238700002));
#327956=CARTESIAN_POINT('Ctrl Pts',(0.171661261999944,12.2,-4.69801056600001));
#327957=CARTESIAN_POINT('Ctrl Pts',(0.171661261999944,5.2,-4.69801056600001));
#327958=CARTESIAN_POINT('Ctrl Pts',(0.171661261999944,2.2,-4.69801056600001));
#327959=CARTESIAN_POINT('Ctrl Pts',(0.173109147999944,12.2,-4.70016009300001));
#327960=CARTESIAN_POINT('Ctrl Pts',(0.173109147999944,5.2,-4.70016009300001));
#327961=CARTESIAN_POINT('Ctrl Pts',(0.173109147999944,2.2,-4.70016009300001));
#327962=CARTESIAN_POINT('Ctrl Pts',(0.174561200999944,12.2,-4.70231095900001));
#327963=CARTESIAN_POINT('Ctrl Pts',(0.174561200999944,5.2,-4.70231095900001));
#327964=CARTESIAN_POINT('Ctrl Pts',(0.174561200999944,2.2,-4.70231095900001));
#327965=CARTESIAN_POINT('Ctrl Pts',(0.176017423999945,12.2,-4.70446315400002));
#327966=CARTESIAN_POINT('Ctrl Pts',(0.176017423999945,5.2,-4.70446315400002));
#327967=CARTESIAN_POINT('Ctrl Pts',(0.176017423999945,2.2,-4.70446315400002));
#327968=CARTESIAN_POINT('Ctrl Pts',(0.177477819999944,12.2,-4.70661667200002));
#327969=CARTESIAN_POINT('Ctrl Pts',(0.177477819999944,5.2,-4.70661667200002));
#327970=CARTESIAN_POINT('Ctrl Pts',(0.177477819999944,2.2,-4.70661667200002));
#327971=CARTESIAN_POINT('Ctrl Pts',(0.178942388999944,12.2,-4.70877150100002));
#327972=CARTESIAN_POINT('Ctrl Pts',(0.178942388999944,5.2,-4.70877150100002));
#327973=CARTESIAN_POINT('Ctrl Pts',(0.178942388999944,2.2,-4.70877150100002));
#327974=CARTESIAN_POINT('Ctrl Pts',(0.180411133999945,12.2,-4.71092763500002));
#327975=CARTESIAN_POINT('Ctrl Pts',(0.180411133999945,5.2,-4.71092763500002));
#327976=CARTESIAN_POINT('Ctrl Pts',(0.180411133999945,2.2,-4.71092763500002));
#327977=CARTESIAN_POINT('Ctrl Pts',(0.181884055999945,12.2,-4.71308506500002));
#327978=CARTESIAN_POINT('Ctrl Pts',(0.181884055999945,5.2,-4.71308506500002));
#327979=CARTESIAN_POINT('Ctrl Pts',(0.181884055999945,2.2,-4.71308506500002));
#327980=CARTESIAN_POINT('Ctrl Pts',(0.183361154999944,12.2,-4.71524378400002));
#327981=CARTESIAN_POINT('Ctrl Pts',(0.183361154999944,5.2,-4.71524378400002));
#327982=CARTESIAN_POINT('Ctrl Pts',(0.183361154999944,2.2,-4.71524378400002));
#327983=CARTESIAN_POINT('Ctrl Pts',(0.184842434999943,12.2,-4.71740378300002));
#327984=CARTESIAN_POINT('Ctrl Pts',(0.184842434999943,5.2,-4.71740378300002));
#327985=CARTESIAN_POINT('Ctrl Pts',(0.184842434999943,2.2,-4.71740378300002));
#327986=CARTESIAN_POINT('Ctrl Pts',(0.186327895999945,12.2,-4.71956505600001));
#327987=CARTESIAN_POINT('Ctrl Pts',(0.186327895999945,5.2,-4.71956505600001));
#327988=CARTESIAN_POINT('Ctrl Pts',(0.186327895999945,2.2,-4.71956505600001));
#327989=CARTESIAN_POINT('Ctrl Pts',(0.187817540999945,12.2,-4.72172759400001));
#327990=CARTESIAN_POINT('Ctrl Pts',(0.187817540999945,5.2,-4.72172759400001));
#327991=CARTESIAN_POINT('Ctrl Pts',(0.187817540999945,2.2,-4.72172759400001));
#327992=CARTESIAN_POINT('Ctrl Pts',(0.189311369999944,12.2,-4.72389138700001));
#327993=CARTESIAN_POINT('Ctrl Pts',(0.189311369999944,5.2,-4.72389138700001));
#327994=CARTESIAN_POINT('Ctrl Pts',(0.189311369999944,2.2,-4.72389138700001));
#327995=CARTESIAN_POINT('Ctrl Pts',(0.190809384999945,12.2,-4.72605642400001));
#327996=CARTESIAN_POINT('Ctrl Pts',(0.190809384999945,5.2,-4.72605642400001));
#327997=CARTESIAN_POINT('Ctrl Pts',(0.190809384999945,2.2,-4.72605642400001));
#327998=CARTESIAN_POINT('Ctrl Pts',(0.192311589999944,12.2,-4.72822269600002));
#327999=CARTESIAN_POINT('Ctrl Pts',(0.192311589999944,5.2,-4.72822269600002));
#328000=CARTESIAN_POINT('Ctrl Pts',(0.192311589999944,2.2,-4.72822269600002));
#328001=CARTESIAN_POINT('Ctrl Pts',(0.193817984999944,12.2,-4.73039019200002));
#328002=CARTESIAN_POINT('Ctrl Pts',(0.193817984999944,5.2,-4.73039019200002));
#328003=CARTESIAN_POINT('Ctrl Pts',(0.193817984999944,2.2,-4.73039019200002));
#328004=CARTESIAN_POINT('Ctrl Pts',(0.195328572999944,12.2,-4.73255890000001));
#328005=CARTESIAN_POINT('Ctrl Pts',(0.195328572999944,5.2,-4.73255890000001));
#328006=CARTESIAN_POINT('Ctrl Pts',(0.195328572999944,2.2,-4.73255890000001));
#328007=CARTESIAN_POINT('Ctrl Pts',(0.196843354999944,12.2,-4.73472881600001));
#328008=CARTESIAN_POINT('Ctrl Pts',(0.196843354999944,5.2,-4.73472881600001));
#328009=CARTESIAN_POINT('Ctrl Pts',(0.196843354999944,2.2,-4.73472881600001));
#328010=CARTESIAN_POINT('Ctrl Pts',(0.198362330999944,12.2,-4.73689993200002));
#328011=CARTESIAN_POINT('Ctrl Pts',(0.198362330999944,5.2,-4.73689993200002));
#328012=CARTESIAN_POINT('Ctrl Pts',(0.198362330999944,2.2,-4.73689993200002));
#328013=CARTESIAN_POINT('Ctrl Pts',(0.199885503999945,12.2,-4.73907224400001));
#328014=CARTESIAN_POINT('Ctrl Pts',(0.199885503999945,5.2,-4.73907224400001));
#328015=CARTESIAN_POINT('Ctrl Pts',(0.199885503999945,2.2,-4.73907224400001));
#328016=CARTESIAN_POINT('Ctrl Pts',(0.201412871999944,12.2,-4.74124574900001));
#328017=CARTESIAN_POINT('Ctrl Pts',(0.201412871999944,5.2,-4.74124574900001));
#328018=CARTESIAN_POINT('Ctrl Pts',(0.201412871999944,2.2,-4.74124574900001));
#328019=CARTESIAN_POINT('Ctrl Pts',(0.202638122999945,12.2,-4.74298550700002));
#328020=CARTESIAN_POINT('Ctrl Pts',(0.202638122999945,5.2,-4.74298550700002));
#328021=CARTESIAN_POINT('Ctrl Pts',(0.202638122999945,2.2,-4.74298550700002));
#328022=CARTESIAN_POINT('Ctrl Pts',(0.203558949999945,12.2,-4.74429086200002));
#328023=CARTESIAN_POINT('Ctrl Pts',(0.203558949999945,5.2,-4.74429086200002));
#328024=CARTESIAN_POINT('Ctrl Pts',(0.203558949999945,2.2,-4.74429086200002));
#328025=CARTESIAN_POINT('Ctrl Pts',(0.204173673999944,12.2,-4.74516133800002));
#328026=CARTESIAN_POINT('Ctrl Pts',(0.204173673999944,5.2,-4.74516133800002));
#328027=CARTESIAN_POINT('Ctrl Pts',(0.204173673999944,2.2,-4.74516133800002));
#328028=CARTESIAN_POINT('Ctrl Pts',(0.204481245999943,12.2,-4.74559663400001));
#328029=CARTESIAN_POINT('Ctrl Pts',(0.204481245999943,5.2,-4.74559663400001));
#328030=CARTESIAN_POINT('Ctrl Pts',(0.204481245999943,2.2,-4.74559663400001));
#328031=CARTESIAN_POINT('',(0.204481245999943,2.7,-4.74559663400001));
#328032=CARTESIAN_POINT('',(0.204481245999943,12.2,-4.74559663400001));
#328033=CARTESIAN_POINT('Ctrl Pts',(-0.114861015000055,2.7,-3.99207578600001));
#328034=CARTESIAN_POINT('Ctrl Pts',(-0.114872757025975,2.7,-3.99254553549219));
#328035=CARTESIAN_POINT('Ctrl Pts',(-0.114899241427072,2.70000000000408,
-3.99417468340611));
#328036=CARTESIAN_POINT('Ctrl Pts',(-0.114744299208137,2.70000000000408,
-4.00133406504499));
#328037=CARTESIAN_POINT('Ctrl Pts',(-0.114517346149866,2.70000000000408,
-4.00584622983241));
#328038=CARTESIAN_POINT('Ctrl Pts',(-0.113198568136949,2.70000000000408,
-4.025643335709));
#328039=CARTESIAN_POINT('Ctrl Pts',(-0.111172638029036,2.70000000000408,
-4.04216774748531));
#328040=CARTESIAN_POINT('Ctrl Pts',(-0.101894823642615,2.70000000000408,
-4.10222156454465));
#328041=CARTESIAN_POINT('Ctrl Pts',(-0.0890316803033102,2.7,-4.15849363694796));
#328042=CARTESIAN_POINT('Ctrl Pts',(-0.0185693674509617,2.7,-4.37334076837332));
#328043=CARTESIAN_POINT('Ctrl Pts',(0.0678106861394203,2.7,-4.55217152370141));
#328044=CARTESIAN_POINT('Ctrl Pts',(0.204481245999943,2.7,-4.74559663400001));
#328045=CARTESIAN_POINT('Origin',(-5.66300478732629E-14,15.2,-1.77635683940025E-14));
#328046=CARTESIAN_POINT('',(0.540411127999944,2.7,-4.71915837900002));
#328047=CARTESIAN_POINT('',(0.540411127999944,12.2,-4.71915837900001));
#328048=CARTESIAN_POINT('Origin',(-5.66300478732629E-14,2.7,-1.92943768261394E-14));
#328049=CARTESIAN_POINT('Ctrl Pts',(0.540411127999944,12.2,-4.71915838000001));
#328050=CARTESIAN_POINT('Ctrl Pts',(0.540411127999944,5.2,-4.71915838000001));
#328051=CARTESIAN_POINT('Ctrl Pts',(0.540411127999944,2.2,-4.71915838000001));
#328052=CARTESIAN_POINT('Ctrl Pts',(0.540646816999945,12.2,-4.71868032600002));
#328053=CARTESIAN_POINT('Ctrl Pts',(0.540646816999945,5.2,-4.71868032600002));
#328054=CARTESIAN_POINT('Ctrl Pts',(0.540646816999945,2.2,-4.71868032600002));
#328055=CARTESIAN_POINT('Ctrl Pts',(0.541117799999945,12.2,-4.71772440400001));
#328056=CARTESIAN_POINT('Ctrl Pts',(0.541117799999945,5.2,-4.71772440400001));
#328057=CARTESIAN_POINT('Ctrl Pts',(0.541117799999945,2.2,-4.71772440400001));
#328058=CARTESIAN_POINT('Ctrl Pts',(0.541823087999944,12.2,-4.71629107100001));
#328059=CARTESIAN_POINT('Ctrl Pts',(0.541823087999944,5.2,-4.71629107100001));
#328060=CARTESIAN_POINT('Ctrl Pts',(0.541823087999944,2.2,-4.71629107100001));
#328061=CARTESIAN_POINT('Ctrl Pts',(0.542761095999944,12.2,-4.71438106100001));
#328062=CARTESIAN_POINT('Ctrl Pts',(0.542761095999944,5.2,-4.71438106100001));
#328063=CARTESIAN_POINT('Ctrl Pts',(0.542761095999944,2.2,-4.71438106100001));
#328064=CARTESIAN_POINT('Ctrl Pts',(0.543929649999945,12.2,-4.71199538200001));
#328065=CARTESIAN_POINT('Ctrl Pts',(0.543929649999945,5.2,-4.71199538200001));
#328066=CARTESIAN_POINT('Ctrl Pts',(0.543929649999945,2.2,-4.71199538200001));
#328067=CARTESIAN_POINT('Ctrl Pts',(0.545094244999944,12.2,-4.70961153900001));
#328068=CARTESIAN_POINT('Ctrl Pts',(0.545094244999944,5.2,-4.70961153900001));
#328069=CARTESIAN_POINT('Ctrl Pts',(0.545094244999944,2.2,-4.70961153900001));
#328070=CARTESIAN_POINT('Ctrl Pts',(0.546254882999944,12.2,-4.70722953300001));
#328071=CARTESIAN_POINT('Ctrl Pts',(0.546254882999944,5.2,-4.70722953300001));
#328072=CARTESIAN_POINT('Ctrl Pts',(0.546254882999944,2.2,-4.70722953300001));
#328073=CARTESIAN_POINT('Ctrl Pts',(0.547411564999944,12.2,-4.70484936900001));
#328074=CARTESIAN_POINT('Ctrl Pts',(0.547411564999944,5.2,-4.70484936900001));
#328075=CARTESIAN_POINT('Ctrl Pts',(0.547411564999944,2.2,-4.70484936900001));
#328076=CARTESIAN_POINT('Ctrl Pts',(0.548564294999945,12.2,-4.70247105100002));
#328077=CARTESIAN_POINT('Ctrl Pts',(0.548564294999945,5.2,-4.70247105100002));
#328078=CARTESIAN_POINT('Ctrl Pts',(0.548564294999945,2.2,-4.70247105100002));
#328079=CARTESIAN_POINT('Ctrl Pts',(0.549713072999943,12.2,-4.70009458900002));
#328080=CARTESIAN_POINT('Ctrl Pts',(0.549713072999943,5.2,-4.70009458900002));
#328081=CARTESIAN_POINT('Ctrl Pts',(0.549713072999943,2.2,-4.70009458900002));
#328082=CARTESIAN_POINT('Ctrl Pts',(0.550857902999944,12.2,-4.69771999200002));
#328083=CARTESIAN_POINT('Ctrl Pts',(0.550857902999944,5.2,-4.69771999200002));
#328084=CARTESIAN_POINT('Ctrl Pts',(0.550857902999944,2.2,-4.69771999200002));
#328085=CARTESIAN_POINT('Ctrl Pts',(0.551998788999944,12.2,-4.69534726800001));
#328086=CARTESIAN_POINT('Ctrl Pts',(0.551998788999944,5.2,-4.69534726800001));
#328087=CARTESIAN_POINT('Ctrl Pts',(0.551998788999944,2.2,-4.69534726800001));
#328088=CARTESIAN_POINT('Ctrl Pts',(0.553135733999944,12.2,-4.69297642900001));
#328089=CARTESIAN_POINT('Ctrl Pts',(0.553135733999944,5.2,-4.69297642900001));
#328090=CARTESIAN_POINT('Ctrl Pts',(0.553135733999944,2.2,-4.69297642900001));
#328091=CARTESIAN_POINT('Ctrl Pts',(0.554268742999944,12.2,-4.69060748400001));
#328092=CARTESIAN_POINT('Ctrl Pts',(0.554268742999944,5.2,-4.69060748400001));
#328093=CARTESIAN_POINT('Ctrl Pts',(0.554268742999944,2.2,-4.69060748400001));
#328094=CARTESIAN_POINT('Ctrl Pts',(0.555397818999944,12.2,-4.68824044200002));
#328095=CARTESIAN_POINT('Ctrl Pts',(0.555397818999944,5.2,-4.68824044200002));
#328096=CARTESIAN_POINT('Ctrl Pts',(0.555397818999944,2.2,-4.68824044200002));
#328097=CARTESIAN_POINT('Ctrl Pts',(0.556522961999945,12.2,-4.68587531300001));
#328098=CARTESIAN_POINT('Ctrl Pts',(0.556522961999945,5.2,-4.68587531300001));
#328099=CARTESIAN_POINT('Ctrl Pts',(0.556522961999945,2.2,-4.68587531300001));
#328100=CARTESIAN_POINT('Ctrl Pts',(0.557644178999944,12.2,-4.68351210200002));
#328101=CARTESIAN_POINT('Ctrl Pts',(0.557644178999944,5.2,-4.68351210200002));
#328102=CARTESIAN_POINT('Ctrl Pts',(0.557644178999944,2.2,-4.68351210200002));
#328103=CARTESIAN_POINT('Ctrl Pts',(0.558761469999944,12.2,-4.68115081800001));
#328104=CARTESIAN_POINT('Ctrl Pts',(0.558761469999944,5.2,-4.68115081800001));
#328105=CARTESIAN_POINT('Ctrl Pts',(0.558761469999944,2.2,-4.68115081800001));
#328106=CARTESIAN_POINT('Ctrl Pts',(0.559874837999944,12.2,-4.67879146700001));
#328107=CARTESIAN_POINT('Ctrl Pts',(0.559874837999944,5.2,-4.67879146700001));
#328108=CARTESIAN_POINT('Ctrl Pts',(0.559874837999944,2.2,-4.67879146700001));
#328109=CARTESIAN_POINT('Ctrl Pts',(0.560984286999945,12.2,-4.67643405800001));
#328110=CARTESIAN_POINT('Ctrl Pts',(0.560984286999945,5.2,-4.67643405800001));
#328111=CARTESIAN_POINT('Ctrl Pts',(0.560984286999945,2.2,-4.67643405800001));
#328112=CARTESIAN_POINT('Ctrl Pts',(0.562089818999943,12.2,-4.67407859900002));
#328113=CARTESIAN_POINT('Ctrl Pts',(0.562089818999943,5.2,-4.67407859900002));
#328114=CARTESIAN_POINT('Ctrl Pts',(0.562089818999943,2.2,-4.67407859900002));
#328115=CARTESIAN_POINT('Ctrl Pts',(0.563191435999945,12.2,-4.67172509600001));
#328116=CARTESIAN_POINT('Ctrl Pts',(0.563191435999945,5.2,-4.67172509600001));
#328117=CARTESIAN_POINT('Ctrl Pts',(0.563191435999945,2.2,-4.67172509600001));
#328118=CARTESIAN_POINT('Ctrl Pts',(0.564289141999944,12.2,-4.66937355900002));
#328119=CARTESIAN_POINT('Ctrl Pts',(0.564289141999944,5.2,-4.66937355900002));
#328120=CARTESIAN_POINT('Ctrl Pts',(0.564289141999944,2.2,-4.66937355900002));
#328121=CARTESIAN_POINT('Ctrl Pts',(0.565382941999945,12.2,-4.66702399800001));
#328122=CARTESIAN_POINT('Ctrl Pts',(0.565382941999945,5.2,-4.66702399800001));
#328123=CARTESIAN_POINT('Ctrl Pts',(0.565382941999945,2.2,-4.66702399800001));
#328124=CARTESIAN_POINT('Ctrl Pts',(0.566472835999944,12.2,-4.66467641900001));
#328125=CARTESIAN_POINT('Ctrl Pts',(0.566472835999944,5.2,-4.66467641900001));
#328126=CARTESIAN_POINT('Ctrl Pts',(0.566472835999944,2.2,-4.66467641900001));
#328127=CARTESIAN_POINT('Ctrl Pts',(0.567558829999945,12.2,-4.66233083200001));
#328128=CARTESIAN_POINT('Ctrl Pts',(0.567558829999945,5.2,-4.66233083200001));
#328129=CARTESIAN_POINT('Ctrl Pts',(0.567558829999945,2.2,-4.66233083200001));
#328130=CARTESIAN_POINT('Ctrl Pts',(0.568640924999944,12.2,-4.65998724400002));
#328131=CARTESIAN_POINT('Ctrl Pts',(0.568640924999944,5.2,-4.65998724400002));
#328132=CARTESIAN_POINT('Ctrl Pts',(0.568640924999944,2.2,-4.65998724400002));
#328133=CARTESIAN_POINT('Ctrl Pts',(0.569719124999944,12.2,-4.65764566400001));
#328134=CARTESIAN_POINT('Ctrl Pts',(0.569719124999944,5.2,-4.65764566400001));
#328135=CARTESIAN_POINT('Ctrl Pts',(0.569719124999944,2.2,-4.65764566400001));
#328136=CARTESIAN_POINT('Ctrl Pts',(0.570793433999944,12.2,-4.65530610000001));
#328137=CARTESIAN_POINT('Ctrl Pts',(0.570793433999944,5.2,-4.65530610000001));
#328138=CARTESIAN_POINT('Ctrl Pts',(0.570793433999944,2.2,-4.65530610000001));
#328139=CARTESIAN_POINT('Ctrl Pts',(0.571863851999944,12.2,-4.65296856000001));
#328140=CARTESIAN_POINT('Ctrl Pts',(0.571863851999944,5.2,-4.65296856000001));
#328141=CARTESIAN_POINT('Ctrl Pts',(0.571863851999944,2.2,-4.65296856000001));
#328142=CARTESIAN_POINT('Ctrl Pts',(0.572930385999944,12.2,-4.65063305300002));
#328143=CARTESIAN_POINT('Ctrl Pts',(0.572930385999944,5.2,-4.65063305300002));
#328144=CARTESIAN_POINT('Ctrl Pts',(0.572930385999944,2.2,-4.65063305300002));
#328145=CARTESIAN_POINT('Ctrl Pts',(0.573993035999945,12.2,-4.64829958600002));
#328146=CARTESIAN_POINT('Ctrl Pts',(0.573993035999945,5.2,-4.64829958600002));
#328147=CARTESIAN_POINT('Ctrl Pts',(0.573993035999945,2.2,-4.64829958600002));
#328148=CARTESIAN_POINT('Ctrl Pts',(0.575051807999943,12.2,-4.64596816700002));
#328149=CARTESIAN_POINT('Ctrl Pts',(0.575051807999943,5.2,-4.64596816700002));
#328150=CARTESIAN_POINT('Ctrl Pts',(0.575051807999943,2.2,-4.64596816700002));
#328151=CARTESIAN_POINT('Ctrl Pts',(0.576106702999944,12.2,-4.64363880500001));
#328152=CARTESIAN_POINT('Ctrl Pts',(0.576106702999944,5.2,-4.64363880500001));
#328153=CARTESIAN_POINT('Ctrl Pts',(0.576106702999944,2.2,-4.64363880500001));
#328154=CARTESIAN_POINT('Ctrl Pts',(0.577157724999945,12.2,-4.64131150800001));
#328155=CARTESIAN_POINT('Ctrl Pts',(0.577157724999945,5.2,-4.64131150800001));
#328156=CARTESIAN_POINT('Ctrl Pts',(0.577157724999945,2.2,-4.64131150800001));
#328157=CARTESIAN_POINT('Ctrl Pts',(0.578204876999945,12.2,-4.63898628500001));
#328158=CARTESIAN_POINT('Ctrl Pts',(0.578204876999945,5.2,-4.63898628500001));
#328159=CARTESIAN_POINT('Ctrl Pts',(0.578204876999945,2.2,-4.63898628500001));
#328160=CARTESIAN_POINT('Ctrl Pts',(0.579248161999945,12.2,-4.63666314300001));
#328161=CARTESIAN_POINT('Ctrl Pts',(0.579248161999945,5.2,-4.63666314300001));
#328162=CARTESIAN_POINT('Ctrl Pts',(0.579248161999945,2.2,-4.63666314300001));
#328163=CARTESIAN_POINT('Ctrl Pts',(0.580287583999944,12.2,-4.63434209100001));
#328164=CARTESIAN_POINT('Ctrl Pts',(0.580287583999944,5.2,-4.63434209100001));
#328165=CARTESIAN_POINT('Ctrl Pts',(0.580287583999944,2.2,-4.63434209100001));
#328166=CARTESIAN_POINT('Ctrl Pts',(0.581323146999945,12.2,-4.63202313700001));
#328167=CARTESIAN_POINT('Ctrl Pts',(0.581323146999945,5.2,-4.63202313700001));
#328168=CARTESIAN_POINT('Ctrl Pts',(0.581323146999945,2.2,-4.63202313700001));
#328169=CARTESIAN_POINT('Ctrl Pts',(0.582354852999944,12.2,-4.62970629100001));
#328170=CARTESIAN_POINT('Ctrl Pts',(0.582354852999944,5.2,-4.62970629100001));
#328171=CARTESIAN_POINT('Ctrl Pts',(0.582354852999944,2.2,-4.62970629100001));
#328172=CARTESIAN_POINT('Ctrl Pts',(0.583382704999944,12.2,-4.62739155900001));
#328173=CARTESIAN_POINT('Ctrl Pts',(0.583382704999944,5.2,-4.62739155900001));
#328174=CARTESIAN_POINT('Ctrl Pts',(0.583382704999944,2.2,-4.62739155900001));
#328175=CARTESIAN_POINT('Ctrl Pts',(0.584406706999945,12.2,-4.62507895000002));
#328176=CARTESIAN_POINT('Ctrl Pts',(0.584406706999945,5.2,-4.62507895000002));
#328177=CARTESIAN_POINT('Ctrl Pts',(0.584406706999945,2.2,-4.62507895000002));
#328178=CARTESIAN_POINT('Ctrl Pts',(0.585426862999944,12.2,-4.62276847200001));
#328179=CARTESIAN_POINT('Ctrl Pts',(0.585426862999944,5.2,-4.62276847200001));
#328180=CARTESIAN_POINT('Ctrl Pts',(0.585426862999944,2.2,-4.62276847200001));
#328181=CARTESIAN_POINT('Ctrl Pts',(0.586443174999944,12.2,-4.62046013400002));
#328182=CARTESIAN_POINT('Ctrl Pts',(0.586443174999944,5.2,-4.62046013400002));
#328183=CARTESIAN_POINT('Ctrl Pts',(0.586443174999944,2.2,-4.62046013400002));
#328184=CARTESIAN_POINT('Ctrl Pts',(0.587455645999944,12.2,-4.61815394400002));
#328185=CARTESIAN_POINT('Ctrl Pts',(0.587455645999944,5.2,-4.61815394400002));
#328186=CARTESIAN_POINT('Ctrl Pts',(0.587455645999944,2.2,-4.61815394400002));
#328187=CARTESIAN_POINT('Ctrl Pts',(0.588464282999944,12.2,-4.61584991100001));
#328188=CARTESIAN_POINT('Ctrl Pts',(0.588464282999944,5.2,-4.61584991100001));
#328189=CARTESIAN_POINT('Ctrl Pts',(0.588464282999944,2.2,-4.61584991100001));
#328190=CARTESIAN_POINT('Ctrl Pts',(0.589469083999944,12.2,-4.61354804200001));
#328191=CARTESIAN_POINT('Ctrl Pts',(0.589469083999944,5.2,-4.61354804200001));
#328192=CARTESIAN_POINT('Ctrl Pts',(0.589469083999944,2.2,-4.61354804200001));
#328193=CARTESIAN_POINT('Ctrl Pts',(0.590470056999944,12.2,-4.61124834600001));
#328194=CARTESIAN_POINT('Ctrl Pts',(0.590470056999944,5.2,-4.61124834600001));
#328195=CARTESIAN_POINT('Ctrl Pts',(0.590470056999944,2.2,-4.61124834600001));
#328196=CARTESIAN_POINT('Ctrl Pts',(0.591467202999943,12.2,-4.60895083100001));
#328197=CARTESIAN_POINT('Ctrl Pts',(0.591467202999943,5.2,-4.60895083100001));
#328198=CARTESIAN_POINT('Ctrl Pts',(0.591467202999943,2.2,-4.60895083100001));
#328199=CARTESIAN_POINT('Ctrl Pts',(0.592460524999944,12.2,-4.60665550600002));
#328200=CARTESIAN_POINT('Ctrl Pts',(0.592460524999944,5.2,-4.60665550600002));
#328201=CARTESIAN_POINT('Ctrl Pts',(0.592460524999944,2.2,-4.60665550600002));
#328202=CARTESIAN_POINT('Ctrl Pts',(0.593450028999943,12.2,-4.60436237900002));
#328203=CARTESIAN_POINT('Ctrl Pts',(0.593450028999943,5.2,-4.60436237900002));
#328204=CARTESIAN_POINT('Ctrl Pts',(0.593450028999943,2.2,-4.60436237900002));
#328205=CARTESIAN_POINT('Ctrl Pts',(0.594435716999944,12.2,-4.60207145800001));
#328206=CARTESIAN_POINT('Ctrl Pts',(0.594435716999944,5.2,-4.60207145800001));
#328207=CARTESIAN_POINT('Ctrl Pts',(0.594435716999944,2.2,-4.60207145800001));
#328208=CARTESIAN_POINT('Ctrl Pts',(0.595417591999944,12.2,-4.59978275200001));
#328209=CARTESIAN_POINT('Ctrl Pts',(0.595417591999944,5.2,-4.59978275200001));
#328210=CARTESIAN_POINT('Ctrl Pts',(0.595417591999944,2.2,-4.59978275200001));
#328211=CARTESIAN_POINT('Ctrl Pts',(0.596395656999944,12.2,-4.59749626800001));
#328212=CARTESIAN_POINT('Ctrl Pts',(0.596395656999944,5.2,-4.59749626800001));
#328213=CARTESIAN_POINT('Ctrl Pts',(0.596395656999944,2.2,-4.59749626800001));
#328214=CARTESIAN_POINT('Ctrl Pts',(0.597369917999945,12.2,-4.59521201700001));
#328215=CARTESIAN_POINT('Ctrl Pts',(0.597369917999945,5.2,-4.59521201700001));
#328216=CARTESIAN_POINT('Ctrl Pts',(0.597369917999945,2.2,-4.59521201700001));
#328217=CARTESIAN_POINT('Ctrl Pts',(0.598340375999945,12.2,-4.59293000500002));
#328218=CARTESIAN_POINT('Ctrl Pts',(0.598340375999945,5.2,-4.59293000500002));
#328219=CARTESIAN_POINT('Ctrl Pts',(0.598340375999945,2.2,-4.59293000500002));
#328220=CARTESIAN_POINT('Ctrl Pts',(0.599307035999944,12.2,-4.59065024100001));
#328221=CARTESIAN_POINT('Ctrl Pts',(0.599307035999944,5.2,-4.59065024100001));
#328222=CARTESIAN_POINT('Ctrl Pts',(0.599307035999944,2.2,-4.59065024100001));
#328223=CARTESIAN_POINT('Ctrl Pts',(0.600269900999945,12.2,-4.58837273300002));
#328224=CARTESIAN_POINT('Ctrl Pts',(0.600269900999945,5.2,-4.58837273300002));
#328225=CARTESIAN_POINT('Ctrl Pts',(0.600269900999945,2.2,-4.58837273300002));
#328226=CARTESIAN_POINT('Ctrl Pts',(0.601228974999944,12.2,-4.58609749100002));
#328227=CARTESIAN_POINT('Ctrl Pts',(0.601228974999944,5.2,-4.58609749100002));
#328228=CARTESIAN_POINT('Ctrl Pts',(0.601228974999944,2.2,-4.58609749100002));
#328229=CARTESIAN_POINT('Ctrl Pts',(0.602184260999944,12.2,-4.58382452200001));
#328230=CARTESIAN_POINT('Ctrl Pts',(0.602184260999944,5.2,-4.58382452200001));
#328231=CARTESIAN_POINT('Ctrl Pts',(0.602184260999944,2.2,-4.58382452200001));
#328232=CARTESIAN_POINT('Ctrl Pts',(0.603135763999945,12.2,-4.58155383400001));
#328233=CARTESIAN_POINT('Ctrl Pts',(0.603135763999945,5.2,-4.58155383400001));
#328234=CARTESIAN_POINT('Ctrl Pts',(0.603135763999945,2.2,-4.58155383400001));
#328235=CARTESIAN_POINT('Ctrl Pts',(0.604083485999943,12.2,-4.57928543600001));
#328236=CARTESIAN_POINT('Ctrl Pts',(0.604083485999943,5.2,-4.57928543600001));
#328237=CARTESIAN_POINT('Ctrl Pts',(0.604083485999943,2.2,-4.57928543600001));
#328238=CARTESIAN_POINT('Ctrl Pts',(0.605027431999944,12.2,-4.57701933800001));
#328239=CARTESIAN_POINT('Ctrl Pts',(0.605027431999944,5.2,-4.57701933800001));
#328240=CARTESIAN_POINT('Ctrl Pts',(0.605027431999944,2.2,-4.57701933800001));
#328241=CARTESIAN_POINT('Ctrl Pts',(0.605967602999944,12.2,-4.57475554500002));
#328242=CARTESIAN_POINT('Ctrl Pts',(0.605967602999944,5.2,-4.57475554500002));
#328243=CARTESIAN_POINT('Ctrl Pts',(0.605967602999944,2.2,-4.57475554500002));
#328244=CARTESIAN_POINT('Ctrl Pts',(0.606904005999944,12.2,-4.57249406800001));
#328245=CARTESIAN_POINT('Ctrl Pts',(0.606904005999944,5.2,-4.57249406800001));
#328246=CARTESIAN_POINT('Ctrl Pts',(0.606904005999944,2.2,-4.57249406800001));
#328247=CARTESIAN_POINT('Ctrl Pts',(0.607836643999944,12.2,-4.57023491600001));
#328248=CARTESIAN_POINT('Ctrl Pts',(0.607836643999944,5.2,-4.57023491600001));
#328249=CARTESIAN_POINT('Ctrl Pts',(0.607836643999944,2.2,-4.57023491600001));
#328250=CARTESIAN_POINT('Ctrl Pts',(0.608765518999944,12.2,-4.56797809500001));
#328251=CARTESIAN_POINT('Ctrl Pts',(0.608765518999944,5.2,-4.56797809500001));
#328252=CARTESIAN_POINT('Ctrl Pts',(0.608765518999944,2.2,-4.56797809500001));
#328253=CARTESIAN_POINT('Ctrl Pts',(0.609690635999944,12.2,-4.56572361400001));
#328254=CARTESIAN_POINT('Ctrl Pts',(0.609690635999944,5.2,-4.56572361400001));
#328255=CARTESIAN_POINT('Ctrl Pts',(0.609690635999944,2.2,-4.56572361400001));
#328256=CARTESIAN_POINT('Ctrl Pts',(0.610611998999944,12.2,-4.56347148200001));
#328257=CARTESIAN_POINT('Ctrl Pts',(0.610611998999944,5.2,-4.56347148200001));
#328258=CARTESIAN_POINT('Ctrl Pts',(0.610611998999944,2.2,-4.56347148200001));
#328259=CARTESIAN_POINT('Ctrl Pts',(0.611529610999945,12.2,-4.56122170900001));
#328260=CARTESIAN_POINT('Ctrl Pts',(0.611529610999945,5.2,-4.56122170900001));
#328261=CARTESIAN_POINT('Ctrl Pts',(0.611529610999945,2.2,-4.56122170900001));
#328262=CARTESIAN_POINT('Ctrl Pts',(0.612443475999944,12.2,-4.55897430100002));
#328263=CARTESIAN_POINT('Ctrl Pts',(0.612443475999944,5.2,-4.55897430100002));
#328264=CARTESIAN_POINT('Ctrl Pts',(0.612443475999944,2.2,-4.55897430100002));
#328265=CARTESIAN_POINT('Ctrl Pts',(0.613353596999944,12.2,-4.55672926800001));
#328266=CARTESIAN_POINT('Ctrl Pts',(0.613353596999944,5.2,-4.55672926800001));
#328267=CARTESIAN_POINT('Ctrl Pts',(0.613353596999944,2.2,-4.55672926800001));
#328268=CARTESIAN_POINT('Ctrl Pts',(0.614259979999944,12.2,-4.55448661800002));
#328269=CARTESIAN_POINT('Ctrl Pts',(0.614259979999944,5.2,-4.55448661800002));
#328270=CARTESIAN_POINT('Ctrl Pts',(0.614259979999944,2.2,-4.55448661800002));
#328271=CARTESIAN_POINT('Ctrl Pts',(0.615162626999944,12.2,-4.55224635800001));
#328272=CARTESIAN_POINT('Ctrl Pts',(0.615162626999944,5.2,-4.55224635800001));
#328273=CARTESIAN_POINT('Ctrl Pts',(0.615162626999944,2.2,-4.55224635800001));
#328274=CARTESIAN_POINT('Ctrl Pts',(0.616061541999944,12.2,-4.55000849900001));
#328275=CARTESIAN_POINT('Ctrl Pts',(0.616061541999944,5.2,-4.55000849900001));
#328276=CARTESIAN_POINT('Ctrl Pts',(0.616061541999944,2.2,-4.55000849900001));
#328277=CARTESIAN_POINT('Ctrl Pts',(0.616956729999945,12.2,-4.54777304800002));
#328278=CARTESIAN_POINT('Ctrl Pts',(0.616956729999945,5.2,-4.54777304800002));
#328279=CARTESIAN_POINT('Ctrl Pts',(0.616956729999945,2.2,-4.54777304800002));
#328280=CARTESIAN_POINT('Ctrl Pts',(0.617848193999944,12.2,-4.54554001400002));
#328281=CARTESIAN_POINT('Ctrl Pts',(0.617848193999944,5.2,-4.54554001400002));
#328282=CARTESIAN_POINT('Ctrl Pts',(0.617848193999944,2.2,-4.54554001400002));
#328283=CARTESIAN_POINT('Ctrl Pts',(0.618735937999944,12.2,-4.54330940500002));
#328284=CARTESIAN_POINT('Ctrl Pts',(0.618735937999944,5.2,-4.54330940500002));
#328285=CARTESIAN_POINT('Ctrl Pts',(0.618735937999944,2.2,-4.54330940500002));
#328286=CARTESIAN_POINT('Ctrl Pts',(0.619619964999945,12.2,-4.54108123000001));
#328287=CARTESIAN_POINT('Ctrl Pts',(0.619619964999945,5.2,-4.54108123000001));
#328288=CARTESIAN_POINT('Ctrl Pts',(0.619619964999945,2.2,-4.54108123000001));
#328289=CARTESIAN_POINT('Ctrl Pts',(0.620500280999944,12.2,-4.53885549700002));
#328290=CARTESIAN_POINT('Ctrl Pts',(0.620500280999944,5.2,-4.53885549700002));
#328291=CARTESIAN_POINT('Ctrl Pts',(0.620500280999944,2.2,-4.53885549700002));
#328292=CARTESIAN_POINT('Ctrl Pts',(0.621376888999944,12.2,-4.53663221500001));
#328293=CARTESIAN_POINT('Ctrl Pts',(0.621376888999944,5.2,-4.53663221500001));
#328294=CARTESIAN_POINT('Ctrl Pts',(0.621376888999944,2.2,-4.53663221500001));
#328295=CARTESIAN_POINT('Ctrl Pts',(0.622249792999944,12.2,-4.53441139300002));
#328296=CARTESIAN_POINT('Ctrl Pts',(0.622249792999944,5.2,-4.53441139300002));
#328297=CARTESIAN_POINT('Ctrl Pts',(0.622249792999944,2.2,-4.53441139300002));
#328298=CARTESIAN_POINT('Ctrl Pts',(0.623118994999944,12.2,-4.53219303800001));
#328299=CARTESIAN_POINT('Ctrl Pts',(0.623118994999944,5.2,-4.53219303800001));
#328300=CARTESIAN_POINT('Ctrl Pts',(0.623118994999944,2.2,-4.53219303800001));
#328301=CARTESIAN_POINT('Ctrl Pts',(0.623984501999945,12.2,-4.52997715900001));
#328302=CARTESIAN_POINT('Ctrl Pts',(0.623984501999945,5.2,-4.52997715900001));
#328303=CARTESIAN_POINT('Ctrl Pts',(0.623984501999945,2.2,-4.52997715900001));
#328304=CARTESIAN_POINT('Ctrl Pts',(0.624846316999944,12.2,-4.52776376600001));
#328305=CARTESIAN_POINT('Ctrl Pts',(0.624846316999944,5.2,-4.52776376600001));
#328306=CARTESIAN_POINT('Ctrl Pts',(0.624846316999944,2.2,-4.52776376600001));
#328307=CARTESIAN_POINT('Ctrl Pts',(0.625704442999945,12.2,-4.52555286600001));
#328308=CARTESIAN_POINT('Ctrl Pts',(0.625704442999945,5.2,-4.52555286600001));
#328309=CARTESIAN_POINT('Ctrl Pts',(0.625704442999945,2.2,-4.52555286600001));
#328310=CARTESIAN_POINT('Ctrl Pts',(0.626558884999944,12.2,-4.52334446800001));
#328311=CARTESIAN_POINT('Ctrl Pts',(0.626558884999944,5.2,-4.52334446800001));
#328312=CARTESIAN_POINT('Ctrl Pts',(0.626558884999944,2.2,-4.52334446800001));
#328313=CARTESIAN_POINT('Ctrl Pts',(0.627409647999944,12.2,-4.52113858100001));
#328314=CARTESIAN_POINT('Ctrl Pts',(0.627409647999944,5.2,-4.52113858100001));
#328315=CARTESIAN_POINT('Ctrl Pts',(0.627409647999944,2.2,-4.52113858100001));
#328316=CARTESIAN_POINT('Ctrl Pts',(0.628256733999945,12.2,-4.51893521300001));
#328317=CARTESIAN_POINT('Ctrl Pts',(0.628256733999945,5.2,-4.51893521300001));
#328318=CARTESIAN_POINT('Ctrl Pts',(0.628256733999945,2.2,-4.51893521300001));
#328319=CARTESIAN_POINT('Ctrl Pts',(0.629100147999945,12.2,-4.51673437200002));
#328320=CARTESIAN_POINT('Ctrl Pts',(0.629100147999945,5.2,-4.51673437200002));
#328321=CARTESIAN_POINT('Ctrl Pts',(0.629100147999945,2.2,-4.51673437200002));
#328322=CARTESIAN_POINT('Ctrl Pts',(0.629939894999944,12.2,-4.51453606800001));
#328323=CARTESIAN_POINT('Ctrl Pts',(0.629939894999944,5.2,-4.51453606800001));
#328324=CARTESIAN_POINT('Ctrl Pts',(0.629939894999944,2.2,-4.51453606800001));
#328325=CARTESIAN_POINT('Ctrl Pts',(0.630775978999945,12.2,-4.51234030800002));
#328326=CARTESIAN_POINT('Ctrl Pts',(0.630775978999945,5.2,-4.51234030800002));
#328327=CARTESIAN_POINT('Ctrl Pts',(0.630775978999945,2.2,-4.51234030800002));
#328328=CARTESIAN_POINT('Ctrl Pts',(0.631608402999944,12.2,-4.51014710200001));
#328329=CARTESIAN_POINT('Ctrl Pts',(0.631608402999944,5.2,-4.51014710200001));
#328330=CARTESIAN_POINT('Ctrl Pts',(0.631608402999944,2.2,-4.51014710200001));
#328331=CARTESIAN_POINT('Ctrl Pts',(0.632437170999944,12.2,-4.50795645800001));
#328332=CARTESIAN_POINT('Ctrl Pts',(0.632437170999944,5.2,-4.50795645800001));
#328333=CARTESIAN_POINT('Ctrl Pts',(0.632437170999944,2.2,-4.50795645800001));
#328334=CARTESIAN_POINT('Ctrl Pts',(0.633262287999944,12.2,-4.50576838500002));
#328335=CARTESIAN_POINT('Ctrl Pts',(0.633262287999944,5.2,-4.50576838500002));
#328336=CARTESIAN_POINT('Ctrl Pts',(0.633262287999944,2.2,-4.50576838500002));
#328337=CARTESIAN_POINT('Ctrl Pts',(0.634083757999945,12.2,-4.50358289100001));
#328338=CARTESIAN_POINT('Ctrl Pts',(0.634083757999945,5.2,-4.50358289100001));
#328339=CARTESIAN_POINT('Ctrl Pts',(0.634083757999945,2.2,-4.50358289100001));
#328340=CARTESIAN_POINT('Ctrl Pts',(0.634901585999944,12.2,-4.50139998400001));
#328341=CARTESIAN_POINT('Ctrl Pts',(0.634901585999944,5.2,-4.50139998400001));
#328342=CARTESIAN_POINT('Ctrl Pts',(0.634901585999944,2.2,-4.50139998400001));
#328343=CARTESIAN_POINT('Ctrl Pts',(0.635715774999944,12.2,-4.49921967400002));
#328344=CARTESIAN_POINT('Ctrl Pts',(0.635715774999944,5.2,-4.49921967400002));
#328345=CARTESIAN_POINT('Ctrl Pts',(0.635715774999944,2.2,-4.49921967400002));
#328346=CARTESIAN_POINT('Ctrl Pts',(0.636526330999944,12.2,-4.49704196900001));
#328347=CARTESIAN_POINT('Ctrl Pts',(0.636526330999944,5.2,-4.49704196900001));
#328348=CARTESIAN_POINT('Ctrl Pts',(0.636526330999944,2.2,-4.49704196900001));
#328349=CARTESIAN_POINT('Ctrl Pts',(0.637333255999945,12.2,-4.49486687800002));
#328350=CARTESIAN_POINT('Ctrl Pts',(0.637333255999945,5.2,-4.49486687800002));
#328351=CARTESIAN_POINT('Ctrl Pts',(0.637333255999945,2.2,-4.49486687800002));
#328352=CARTESIAN_POINT('Ctrl Pts',(0.638136555999944,12.2,-4.49269440900002));
#328353=CARTESIAN_POINT('Ctrl Pts',(0.638136555999944,5.2,-4.49269440900002));
#328354=CARTESIAN_POINT('Ctrl Pts',(0.638136555999944,2.2,-4.49269440900002));
#328355=CARTESIAN_POINT('Ctrl Pts',(0.638936233999944,12.2,-4.49052457000001));
#328356=CARTESIAN_POINT('Ctrl Pts',(0.638936233999944,5.2,-4.49052457000001));
#328357=CARTESIAN_POINT('Ctrl Pts',(0.638936233999944,2.2,-4.49052457000001));
#328358=CARTESIAN_POINT('Ctrl Pts',(0.639732295999944,12.2,-4.48835737200001));
#328359=CARTESIAN_POINT('Ctrl Pts',(0.639732295999944,5.2,-4.48835737200001));
#328360=CARTESIAN_POINT('Ctrl Pts',(0.639732295999944,2.2,-4.48835737200001));
#328361=CARTESIAN_POINT('Ctrl Pts',(0.640524743999944,12.2,-4.48619282100001));
#328362=CARTESIAN_POINT('Ctrl Pts',(0.640524743999944,5.2,-4.48619282100001));
#328363=CARTESIAN_POINT('Ctrl Pts',(0.640524743999944,2.2,-4.48619282100001));
#328364=CARTESIAN_POINT('Ctrl Pts',(0.641313584999944,12.2,-4.48403092800001));
#328365=CARTESIAN_POINT('Ctrl Pts',(0.641313584999944,5.2,-4.48403092800001));
#328366=CARTESIAN_POINT('Ctrl Pts',(0.641313584999944,2.2,-4.48403092800001));
#328367=CARTESIAN_POINT('Ctrl Pts',(0.642098820999945,12.2,-4.48187170000002));
#328368=CARTESIAN_POINT('Ctrl Pts',(0.642098820999945,5.2,-4.48187170000002));
#328369=CARTESIAN_POINT('Ctrl Pts',(0.642098820999945,2.2,-4.48187170000002));
#328370=CARTESIAN_POINT('Ctrl Pts',(0.642880458999944,12.2,-4.47971514600002));
#328371=CARTESIAN_POINT('Ctrl Pts',(0.642880458999944,5.2,-4.47971514600002));
#328372=CARTESIAN_POINT('Ctrl Pts',(0.642880458999944,2.2,-4.47971514600002));
#328373=CARTESIAN_POINT('Ctrl Pts',(0.643658500999944,12.2,-4.47756127500002));
#328374=CARTESIAN_POINT('Ctrl Pts',(0.643658500999944,5.2,-4.47756127500002));
#328375=CARTESIAN_POINT('Ctrl Pts',(0.643658500999944,2.2,-4.47756127500002));
#328376=CARTESIAN_POINT('Ctrl Pts',(0.644432952999944,12.2,-4.47541009600001));
#328377=CARTESIAN_POINT('Ctrl Pts',(0.644432952999944,5.2,-4.47541009600001));
#328378=CARTESIAN_POINT('Ctrl Pts',(0.644432952999944,2.2,-4.47541009600001));
#328379=CARTESIAN_POINT('Ctrl Pts',(0.645203818999944,12.2,-4.47326161700001));
#328380=CARTESIAN_POINT('Ctrl Pts',(0.645203818999944,5.2,-4.47326161700001));
#328381=CARTESIAN_POINT('Ctrl Pts',(0.645203818999944,2.2,-4.47326161700001));
#328382=CARTESIAN_POINT('Ctrl Pts',(0.645971102999944,12.2,-4.47111584600002));
#328383=CARTESIAN_POINT('Ctrl Pts',(0.645971102999944,5.2,-4.47111584600002));
#328384=CARTESIAN_POINT('Ctrl Pts',(0.645971102999944,2.2,-4.47111584600002));
#328385=CARTESIAN_POINT('Ctrl Pts',(0.646734808999944,12.2,-4.46897279400002));
#328386=CARTESIAN_POINT('Ctrl Pts',(0.646734808999944,5.2,-4.46897279400002));
#328387=CARTESIAN_POINT('Ctrl Pts',(0.646734808999944,2.2,-4.46897279400002));
#328388=CARTESIAN_POINT('Ctrl Pts',(0.647494942999944,12.2,-4.46683246700001));
#328389=CARTESIAN_POINT('Ctrl Pts',(0.647494942999944,5.2,-4.46683246700001));
#328390=CARTESIAN_POINT('Ctrl Pts',(0.647494942999944,2.2,-4.46683246700001));
#328391=CARTESIAN_POINT('Ctrl Pts',(0.648251508999944,12.2,-4.46469487600002));
#328392=CARTESIAN_POINT('Ctrl Pts',(0.648251508999944,5.2,-4.46469487600002));
#328393=CARTESIAN_POINT('Ctrl Pts',(0.648251508999944,2.2,-4.46469487600002));
#328394=CARTESIAN_POINT('Ctrl Pts',(0.649004510999944,12.2,-4.46256002700002));
#328395=CARTESIAN_POINT('Ctrl Pts',(0.649004510999944,5.2,-4.46256002700002));
#328396=CARTESIAN_POINT('Ctrl Pts',(0.649004510999944,2.2,-4.46256002700002));
#328397=CARTESIAN_POINT('Ctrl Pts',(0.649753954999944,12.2,-4.46042793300002));
#328398=CARTESIAN_POINT('Ctrl Pts',(0.649753954999944,5.2,-4.46042793300002));
#328399=CARTESIAN_POINT('Ctrl Pts',(0.649753954999944,2.2,-4.46042793300002));
#328400=CARTESIAN_POINT('Ctrl Pts',(0.650499842999944,12.2,-4.45829859800002));
#328401=CARTESIAN_POINT('Ctrl Pts',(0.650499842999944,5.2,-4.45829859800002));
#328402=CARTESIAN_POINT('Ctrl Pts',(0.650499842999944,2.2,-4.45829859800002));
#328403=CARTESIAN_POINT('Ctrl Pts',(0.651242182999944,12.2,-4.45617203400001));
#328404=CARTESIAN_POINT('Ctrl Pts',(0.651242182999944,5.2,-4.45617203400001));
#328405=CARTESIAN_POINT('Ctrl Pts',(0.651242182999944,2.2,-4.45617203400001));
#328406=CARTESIAN_POINT('Ctrl Pts',(0.651980975999944,12.2,-4.45404824800002));
#328407=CARTESIAN_POINT('Ctrl Pts',(0.651980975999944,5.2,-4.45404824800002));
#328408=CARTESIAN_POINT('Ctrl Pts',(0.651980975999944,2.2,-4.45404824800002));
#328409=CARTESIAN_POINT('Ctrl Pts',(0.652716228999944,12.2,-4.45192725000001));
#328410=CARTESIAN_POINT('Ctrl Pts',(0.652716228999944,5.2,-4.45192725000001));
#328411=CARTESIAN_POINT('Ctrl Pts',(0.652716228999944,2.2,-4.45192725000001));
#328412=CARTESIAN_POINT('Ctrl Pts',(0.653447946999944,12.2,-4.44980904800001));
#328413=CARTESIAN_POINT('Ctrl Pts',(0.653447946999944,5.2,-4.44980904800001));
#328414=CARTESIAN_POINT('Ctrl Pts',(0.653447946999944,2.2,-4.44980904800001));
#328415=CARTESIAN_POINT('Ctrl Pts',(0.654176132999944,12.2,-4.44769365000001));
#328416=CARTESIAN_POINT('Ctrl Pts',(0.654176132999944,5.2,-4.44769365000001));
#328417=CARTESIAN_POINT('Ctrl Pts',(0.654176132999944,2.2,-4.44769365000001));
#328418=CARTESIAN_POINT('Ctrl Pts',(0.654900792999944,12.2,-4.44558106600002));
#328419=CARTESIAN_POINT('Ctrl Pts',(0.654900792999944,5.2,-4.44558106600002));
#328420=CARTESIAN_POINT('Ctrl Pts',(0.654900792999944,2.2,-4.44558106600002));
#328421=CARTESIAN_POINT('Ctrl Pts',(0.655621929999944,12.2,-4.44347130500002));
#328422=CARTESIAN_POINT('Ctrl Pts',(0.655621929999944,5.2,-4.44347130500002));
#328423=CARTESIAN_POINT('Ctrl Pts',(0.655621929999944,2.2,-4.44347130500002));
#328424=CARTESIAN_POINT('Ctrl Pts',(0.656339550999945,12.2,-4.44136437500001));
#328425=CARTESIAN_POINT('Ctrl Pts',(0.656339550999945,5.2,-4.44136437500001));
#328426=CARTESIAN_POINT('Ctrl Pts',(0.656339550999945,2.2,-4.44136437500001));
#328427=CARTESIAN_POINT('Ctrl Pts',(0.657053658999944,12.2,-4.43926028400002));
#328428=CARTESIAN_POINT('Ctrl Pts',(0.657053658999944,5.2,-4.43926028400002));
#328429=CARTESIAN_POINT('Ctrl Pts',(0.657053658999944,2.2,-4.43926028400002));
#328430=CARTESIAN_POINT('Ctrl Pts',(0.657764258999943,12.2,-4.43715904200001));
#328431=CARTESIAN_POINT('Ctrl Pts',(0.657764258999943,5.2,-4.43715904200001));
#328432=CARTESIAN_POINT('Ctrl Pts',(0.657764258999943,2.2,-4.43715904200001));
#328433=CARTESIAN_POINT('Ctrl Pts',(0.658471356999945,12.2,-4.43506065900001));
#328434=CARTESIAN_POINT('Ctrl Pts',(0.658471356999945,5.2,-4.43506065900001));
#328435=CARTESIAN_POINT('Ctrl Pts',(0.658471356999945,2.2,-4.43506065900001));
#328436=CARTESIAN_POINT('Ctrl Pts',(0.659174956999945,12.2,-4.43296514000002));
#328437=CARTESIAN_POINT('Ctrl Pts',(0.659174956999945,5.2,-4.43296514000002));
#328438=CARTESIAN_POINT('Ctrl Pts',(0.659174956999945,2.2,-4.43296514000002));
#328439=CARTESIAN_POINT('Ctrl Pts',(0.659875062999945,12.2,-4.43087249800001));
#328440=CARTESIAN_POINT('Ctrl Pts',(0.659875062999945,5.2,-4.43087249800001));
#328441=CARTESIAN_POINT('Ctrl Pts',(0.659875062999945,2.2,-4.43087249800001));
#328442=CARTESIAN_POINT('Ctrl Pts',(0.660571681999944,12.2,-4.42878273800002));
#328443=CARTESIAN_POINT('Ctrl Pts',(0.660571681999944,5.2,-4.42878273800002));
#328444=CARTESIAN_POINT('Ctrl Pts',(0.660571681999944,2.2,-4.42878273800002));
#328445=CARTESIAN_POINT('Ctrl Pts',(0.661264816999945,12.2,-4.42669587300001));
#328446=CARTESIAN_POINT('Ctrl Pts',(0.661264816999945,5.2,-4.42669587300001));
#328447=CARTESIAN_POINT('Ctrl Pts',(0.661264816999945,2.2,-4.42669587300001));
#328448=CARTESIAN_POINT('Ctrl Pts',(0.661954472999944,12.2,-4.42461190800001));
#328449=CARTESIAN_POINT('Ctrl Pts',(0.661954472999944,5.2,-4.42461190800001));
#328450=CARTESIAN_POINT('Ctrl Pts',(0.661954472999944,2.2,-4.42461190800001));
#328451=CARTESIAN_POINT('Ctrl Pts',(0.662640655999944,12.2,-4.42253085400001));
#328452=CARTESIAN_POINT('Ctrl Pts',(0.662640655999944,5.2,-4.42253085400001));
#328453=CARTESIAN_POINT('Ctrl Pts',(0.662640655999944,2.2,-4.42253085400001));
#328454=CARTESIAN_POINT('Ctrl Pts',(0.663323368999944,12.2,-4.42045271900001));
#328455=CARTESIAN_POINT('Ctrl Pts',(0.663323368999944,5.2,-4.42045271900001));
#328456=CARTESIAN_POINT('Ctrl Pts',(0.663323368999944,2.2,-4.42045271900001));
#328457=CARTESIAN_POINT('Ctrl Pts',(0.664002618999944,12.2,-4.41837751200001));
#328458=CARTESIAN_POINT('Ctrl Pts',(0.664002618999944,5.2,-4.41837751200001));
#328459=CARTESIAN_POINT('Ctrl Pts',(0.664002618999944,2.2,-4.41837751200001));
#328460=CARTESIAN_POINT('Ctrl Pts',(0.664678409999944,12.2,-4.41630524100002));
#328461=CARTESIAN_POINT('Ctrl Pts',(0.664678409999944,5.2,-4.41630524100002));
#328462=CARTESIAN_POINT('Ctrl Pts',(0.664678409999944,2.2,-4.41630524100002));
#328463=CARTESIAN_POINT('Ctrl Pts',(0.665350747999944,12.2,-4.41423591700001));
#328464=CARTESIAN_POINT('Ctrl Pts',(0.665350747999944,5.2,-4.41423591700001));
#328465=CARTESIAN_POINT('Ctrl Pts',(0.665350747999944,2.2,-4.41423591700001));
#328466=CARTESIAN_POINT('Ctrl Pts',(0.666019636999944,12.2,-4.41216954700002));
#328467=CARTESIAN_POINT('Ctrl Pts',(0.666019636999944,5.2,-4.41216954700002));
#328468=CARTESIAN_POINT('Ctrl Pts',(0.666019636999944,2.2,-4.41216954700002));
#328469=CARTESIAN_POINT('Ctrl Pts',(0.666685079999944,12.2,-4.41010614100001));
#328470=CARTESIAN_POINT('Ctrl Pts',(0.666685079999944,5.2,-4.41010614100001));
#328471=CARTESIAN_POINT('Ctrl Pts',(0.666685079999944,2.2,-4.41010614100001));
#328472=CARTESIAN_POINT('Ctrl Pts',(0.667347085999944,12.2,-4.40804570700001));
#328473=CARTESIAN_POINT('Ctrl Pts',(0.667347085999944,5.2,-4.40804570700001));
#328474=CARTESIAN_POINT('Ctrl Pts',(0.667347085999944,2.2,-4.40804570700001));
#328475=CARTESIAN_POINT('Ctrl Pts',(0.668005658999945,12.2,-4.40598825400001));
#328476=CARTESIAN_POINT('Ctrl Pts',(0.668005658999945,5.2,-4.40598825400001));
#328477=CARTESIAN_POINT('Ctrl Pts',(0.668005658999945,2.2,-4.40598825400001));
#328478=CARTESIAN_POINT('Ctrl Pts',(0.668660801999944,12.2,-4.40393379100001));
#328479=CARTESIAN_POINT('Ctrl Pts',(0.668660801999944,5.2,-4.40393379100001));
#328480=CARTESIAN_POINT('Ctrl Pts',(0.668660801999944,2.2,-4.40393379100001));
#328481=CARTESIAN_POINT('Ctrl Pts',(0.669312520999944,12.2,-4.40188232700002));
#328482=CARTESIAN_POINT('Ctrl Pts',(0.669312520999944,5.2,-4.40188232700002));
#328483=CARTESIAN_POINT('Ctrl Pts',(0.669312520999944,2.2,-4.40188232700002));
#328484=CARTESIAN_POINT('Ctrl Pts',(0.669960822999944,12.2,-4.39983387200002));
#328485=CARTESIAN_POINT('Ctrl Pts',(0.669960822999944,5.2,-4.39983387200002));
#328486=CARTESIAN_POINT('Ctrl Pts',(0.669960822999944,2.2,-4.39983387200002));
#328487=CARTESIAN_POINT('Ctrl Pts',(0.670605710999944,12.2,-4.39778843200001));
#328488=CARTESIAN_POINT('Ctrl Pts',(0.670605710999944,5.2,-4.39778843200001));
#328489=CARTESIAN_POINT('Ctrl Pts',(0.670605710999944,2.2,-4.39778843200001));
#328490=CARTESIAN_POINT('Ctrl Pts',(0.671247190999944,12.2,-4.39574601800001));
#328491=CARTESIAN_POINT('Ctrl Pts',(0.671247190999944,5.2,-4.39574601800001));
#328492=CARTESIAN_POINT('Ctrl Pts',(0.671247190999944,2.2,-4.39574601800001));
#328493=CARTESIAN_POINT('Ctrl Pts',(0.671885266999944,12.2,-4.39370664000001));
#328494=CARTESIAN_POINT('Ctrl Pts',(0.671885266999944,5.2,-4.39370664000001));
#328495=CARTESIAN_POINT('Ctrl Pts',(0.671885266999944,2.2,-4.39370664000001));
#328496=CARTESIAN_POINT('Ctrl Pts',(0.672519945999944,12.2,-4.39167030400001));
#328497=CARTESIAN_POINT('Ctrl Pts',(0.672519945999944,5.2,-4.39167030400001));
#328498=CARTESIAN_POINT('Ctrl Pts',(0.672519945999944,2.2,-4.39167030400001));
#328499=CARTESIAN_POINT('Ctrl Pts',(0.673151232999943,12.2,-4.38963702100001));
#328500=CARTESIAN_POINT('Ctrl Pts',(0.673151232999943,5.2,-4.38963702100001));
#328501=CARTESIAN_POINT('Ctrl Pts',(0.673151232999943,2.2,-4.38963702100001));
#328502=CARTESIAN_POINT('Ctrl Pts',(0.673779131999944,12.2,-4.38760679800001));
#328503=CARTESIAN_POINT('Ctrl Pts',(0.673779131999944,5.2,-4.38760679800001));
#328504=CARTESIAN_POINT('Ctrl Pts',(0.673779131999944,2.2,-4.38760679800001));
#328505=CARTESIAN_POINT('Ctrl Pts',(0.674403648999945,12.2,-4.38557964800002));
#328506=CARTESIAN_POINT('Ctrl Pts',(0.674403648999945,5.2,-4.38557964800002));
#328507=CARTESIAN_POINT('Ctrl Pts',(0.674403648999945,2.2,-4.38557964800002));
#328508=CARTESIAN_POINT('Ctrl Pts',(0.675024788999944,12.2,-4.38355557500001));
#328509=CARTESIAN_POINT('Ctrl Pts',(0.675024788999944,5.2,-4.38355557500001));
#328510=CARTESIAN_POINT('Ctrl Pts',(0.675024788999944,2.2,-4.38355557500001));
#328511=CARTESIAN_POINT('Ctrl Pts',(0.675642557999944,12.2,-4.38153459100001));
#328512=CARTESIAN_POINT('Ctrl Pts',(0.675642557999944,5.2,-4.38153459100001));
#328513=CARTESIAN_POINT('Ctrl Pts',(0.675642557999944,2.2,-4.38153459100001));
#328514=CARTESIAN_POINT('Ctrl Pts',(0.676256959999945,12.2,-4.37951670400002));
#328515=CARTESIAN_POINT('Ctrl Pts',(0.676256959999945,5.2,-4.37951670400002));
#328516=CARTESIAN_POINT('Ctrl Pts',(0.676256959999945,2.2,-4.37951670400002));
#328517=CARTESIAN_POINT('Ctrl Pts',(0.676868000999944,12.2,-4.37750192300001));
#328518=CARTESIAN_POINT('Ctrl Pts',(0.676868000999944,5.2,-4.37750192300001));
#328519=CARTESIAN_POINT('Ctrl Pts',(0.676868000999944,2.2,-4.37750192300001));
#328520=CARTESIAN_POINT('Ctrl Pts',(0.677475687999943,12.2,-4.37549025700001));
#328521=CARTESIAN_POINT('Ctrl Pts',(0.677475687999943,5.2,-4.37549025700001));
#328522=CARTESIAN_POINT('Ctrl Pts',(0.677475687999943,2.2,-4.37549025700001));
#328523=CARTESIAN_POINT('Ctrl Pts',(0.678080023999944,12.2,-4.37348171500001));
#328524=CARTESIAN_POINT('Ctrl Pts',(0.678080023999944,5.2,-4.37348171500001));
#328525=CARTESIAN_POINT('Ctrl Pts',(0.678080023999944,2.2,-4.37348171500001));
#328526=CARTESIAN_POINT('Ctrl Pts',(0.678681014999943,12.2,-4.37147630700002));
#328527=CARTESIAN_POINT('Ctrl Pts',(0.678681014999943,5.2,-4.37147630700002));
#328528=CARTESIAN_POINT('Ctrl Pts',(0.678681014999943,2.2,-4.37147630700002));
#328529=CARTESIAN_POINT('Ctrl Pts',(0.679278665999944,12.2,-4.36947404000001));
#328530=CARTESIAN_POINT('Ctrl Pts',(0.679278665999944,5.2,-4.36947404000001));
#328531=CARTESIAN_POINT('Ctrl Pts',(0.679278665999944,2.2,-4.36947404000001));
#328532=CARTESIAN_POINT('Ctrl Pts',(0.679872984999944,12.2,-4.36747492400002));
#328533=CARTESIAN_POINT('Ctrl Pts',(0.679872984999944,5.2,-4.36747492400002));
#328534=CARTESIAN_POINT('Ctrl Pts',(0.679872984999944,2.2,-4.36747492400002));
#328535=CARTESIAN_POINT('Ctrl Pts',(0.680463973999944,12.2,-4.36547896800001));
#328536=CARTESIAN_POINT('Ctrl Pts',(0.680463973999944,5.2,-4.36547896800001));
#328537=CARTESIAN_POINT('Ctrl Pts',(0.680463973999944,2.2,-4.36547896800001));
#328538=CARTESIAN_POINT('Ctrl Pts',(0.681051641999945,12.2,-4.36348618100002));
#328539=CARTESIAN_POINT('Ctrl Pts',(0.681051641999945,5.2,-4.36348618100002));
#328540=CARTESIAN_POINT('Ctrl Pts',(0.681051641999945,2.2,-4.36348618100002));
#328541=CARTESIAN_POINT('Ctrl Pts',(0.681635990999945,12.2,-4.36149657200001));
#328542=CARTESIAN_POINT('Ctrl Pts',(0.681635990999945,5.2,-4.36149657200001));
#328543=CARTESIAN_POINT('Ctrl Pts',(0.681635990999945,2.2,-4.36149657200001));
#328544=CARTESIAN_POINT('Ctrl Pts',(0.682217027999944,12.2,-4.35951015100001));
#328545=CARTESIAN_POINT('Ctrl Pts',(0.682217027999944,5.2,-4.35951015100001));
#328546=CARTESIAN_POINT('Ctrl Pts',(0.682217027999944,2.2,-4.35951015100001));
#328547=CARTESIAN_POINT('Ctrl Pts',(0.682794759999944,12.2,-4.35752692500001));
#328548=CARTESIAN_POINT('Ctrl Pts',(0.682794759999944,5.2,-4.35752692500001));
#328549=CARTESIAN_POINT('Ctrl Pts',(0.682794759999944,2.2,-4.35752692500001));
#328550=CARTESIAN_POINT('Ctrl Pts',(0.683369188999944,12.2,-4.35554690300001));
#328551=CARTESIAN_POINT('Ctrl Pts',(0.683369188999944,5.2,-4.35554690300001));
#328552=CARTESIAN_POINT('Ctrl Pts',(0.683369188999944,2.2,-4.35554690300001));
#328553=CARTESIAN_POINT('Ctrl Pts',(0.683940323999944,12.2,-4.35357009800001));
#328554=CARTESIAN_POINT('Ctrl Pts',(0.683940323999944,5.2,-4.35357009800001));
#328555=CARTESIAN_POINT('Ctrl Pts',(0.683940323999944,2.2,-4.35357009800001));
#328556=CARTESIAN_POINT('Ctrl Pts',(0.684508169999944,12.2,-4.35159651300001));
#328557=CARTESIAN_POINT('Ctrl Pts',(0.684508169999944,5.2,-4.35159651300001));
#328558=CARTESIAN_POINT('Ctrl Pts',(0.684508169999944,2.2,-4.35159651300001));
#328559=CARTESIAN_POINT('Ctrl Pts',(0.685072730999944,12.2,-4.34962616200002));
#328560=CARTESIAN_POINT('Ctrl Pts',(0.685072730999944,5.2,-4.34962616200002));
#328561=CARTESIAN_POINT('Ctrl Pts',(0.685072730999944,2.2,-4.34962616200002));
#328562=CARTESIAN_POINT('Ctrl Pts',(0.685634014999944,12.2,-4.34765905300001));
#328563=CARTESIAN_POINT('Ctrl Pts',(0.685634014999944,5.2,-4.34765905300001));
#328564=CARTESIAN_POINT('Ctrl Pts',(0.685634014999944,2.2,-4.34765905300001));
#328565=CARTESIAN_POINT('Ctrl Pts',(0.686192024999944,12.2,-4.34569519300001));
#328566=CARTESIAN_POINT('Ctrl Pts',(0.686192024999944,5.2,-4.34569519300001));
#328567=CARTESIAN_POINT('Ctrl Pts',(0.686192024999944,2.2,-4.34569519300001));
#328568=CARTESIAN_POINT('Ctrl Pts',(0.686746768999944,12.2,-4.34373459300001));
#328569=CARTESIAN_POINT('Ctrl Pts',(0.686746768999944,5.2,-4.34373459300001));
#328570=CARTESIAN_POINT('Ctrl Pts',(0.686746768999944,2.2,-4.34373459300001));
#328571=CARTESIAN_POINT('Ctrl Pts',(0.687298250999944,12.2,-4.34177726100001));
#328572=CARTESIAN_POINT('Ctrl Pts',(0.687298250999944,5.2,-4.34177726100001));
#328573=CARTESIAN_POINT('Ctrl Pts',(0.687298250999944,2.2,-4.34177726100001));
#328574=CARTESIAN_POINT('Ctrl Pts',(0.687846477999944,12.2,-4.33982320600002));
#328575=CARTESIAN_POINT('Ctrl Pts',(0.687846477999944,5.2,-4.33982320600002));
#328576=CARTESIAN_POINT('Ctrl Pts',(0.687846477999944,2.2,-4.33982320600002));
#328577=CARTESIAN_POINT('Ctrl Pts',(0.688391454999944,12.2,-4.33787243900001));
#328578=CARTESIAN_POINT('Ctrl Pts',(0.688391454999944,5.2,-4.33787243900001));
#328579=CARTESIAN_POINT('Ctrl Pts',(0.688391454999944,2.2,-4.33787243900001));
#328580=CARTESIAN_POINT('Ctrl Pts',(0.688933188999944,12.2,-4.33592496700001));
#328581=CARTESIAN_POINT('Ctrl Pts',(0.688933188999944,5.2,-4.33592496700001));
#328582=CARTESIAN_POINT('Ctrl Pts',(0.688933188999944,2.2,-4.33592496700001));
#328583=CARTESIAN_POINT('Ctrl Pts',(0.689471683999944,12.2,-4.33398080000002));
#328584=CARTESIAN_POINT('Ctrl Pts',(0.689471683999944,5.2,-4.33398080000002));
#328585=CARTESIAN_POINT('Ctrl Pts',(0.689471683999944,2.2,-4.33398080000002));
#328586=CARTESIAN_POINT('Ctrl Pts',(0.690006945999944,12.2,-4.33203994700001));
#328587=CARTESIAN_POINT('Ctrl Pts',(0.690006945999944,5.2,-4.33203994700001));
#328588=CARTESIAN_POINT('Ctrl Pts',(0.690006945999944,2.2,-4.33203994700001));
#328589=CARTESIAN_POINT('Ctrl Pts',(0.690538980999944,12.2,-4.33010241700002));
#328590=CARTESIAN_POINT('Ctrl Pts',(0.690538980999944,5.2,-4.33010241700002));
#328591=CARTESIAN_POINT('Ctrl Pts',(0.690538980999944,2.2,-4.33010241700002));
#328592=CARTESIAN_POINT('Ctrl Pts',(0.691067796999943,12.2,-4.32816821900001));
#328593=CARTESIAN_POINT('Ctrl Pts',(0.691067796999943,5.2,-4.32816821900001));
#328594=CARTESIAN_POINT('Ctrl Pts',(0.691067796999943,2.2,-4.32816821900001));
#328595=CARTESIAN_POINT('Ctrl Pts',(0.691593397999944,12.2,-4.32623736200001));
#328596=CARTESIAN_POINT('Ctrl Pts',(0.691593397999944,5.2,-4.32623736200001));
#328597=CARTESIAN_POINT('Ctrl Pts',(0.691593397999944,2.2,-4.32623736200001));
#328598=CARTESIAN_POINT('Ctrl Pts',(0.692115789999944,12.2,-4.32430985600002));
#328599=CARTESIAN_POINT('Ctrl Pts',(0.692115789999944,5.2,-4.32430985600002));
#328600=CARTESIAN_POINT('Ctrl Pts',(0.692115789999944,2.2,-4.32430985600002));
#328601=CARTESIAN_POINT('Ctrl Pts',(0.692634977999944,12.2,-4.32238570900001));
#328602=CARTESIAN_POINT('Ctrl Pts',(0.692634977999944,5.2,-4.32238570900001));
#328603=CARTESIAN_POINT('Ctrl Pts',(0.692634977999944,2.2,-4.32238570900001));
#328604=CARTESIAN_POINT('Ctrl Pts',(0.693150969999944,12.2,-4.32046493100001));
#328605=CARTESIAN_POINT('Ctrl Pts',(0.693150969999944,5.2,-4.32046493100001));
#328606=CARTESIAN_POINT('Ctrl Pts',(0.693150969999944,2.2,-4.32046493100001));
#328607=CARTESIAN_POINT('Ctrl Pts',(0.693663770999944,12.2,-4.31854753200001));
#328608=CARTESIAN_POINT('Ctrl Pts',(0.693663770999944,5.2,-4.31854753200001));
#328609=CARTESIAN_POINT('Ctrl Pts',(0.693663770999944,2.2,-4.31854753200001));
#328610=CARTESIAN_POINT('Ctrl Pts',(0.694173386999944,12.2,-4.31663351900001));
#328611=CARTESIAN_POINT('Ctrl Pts',(0.694173386999944,5.2,-4.31663351900001));
#328612=CARTESIAN_POINT('Ctrl Pts',(0.694173386999944,2.2,-4.31663351900001));
#328613=CARTESIAN_POINT('Ctrl Pts',(0.694679823999944,12.2,-4.31472290200002));
#328614=CARTESIAN_POINT('Ctrl Pts',(0.694679823999944,5.2,-4.31472290200002));
#328615=CARTESIAN_POINT('Ctrl Pts',(0.694679823999944,2.2,-4.31472290200002));
#328616=CARTESIAN_POINT('Ctrl Pts',(0.695183087999944,12.2,-4.31281569100001));
#328617=CARTESIAN_POINT('Ctrl Pts',(0.695183087999944,5.2,-4.31281569100001));
#328618=CARTESIAN_POINT('Ctrl Pts',(0.695183087999944,2.2,-4.31281569100001));
#328619=CARTESIAN_POINT('Ctrl Pts',(0.695683184999945,12.2,-4.31091189300002));
#328620=CARTESIAN_POINT('Ctrl Pts',(0.695683184999945,5.2,-4.31091189300002));
#328621=CARTESIAN_POINT('Ctrl Pts',(0.695683184999945,2.2,-4.31091189300002));
#328622=CARTESIAN_POINT('Ctrl Pts',(0.696180120999944,12.2,-4.30901152000001));
#328623=CARTESIAN_POINT('Ctrl Pts',(0.696180120999944,5.2,-4.30901152000001));
#328624=CARTESIAN_POINT('Ctrl Pts',(0.696180120999944,2.2,-4.30901152000001));
#328625=CARTESIAN_POINT('Ctrl Pts',(0.696673901999944,12.2,-4.30711458000001));
#328626=CARTESIAN_POINT('Ctrl Pts',(0.696673901999944,5.2,-4.30711458000001));
#328627=CARTESIAN_POINT('Ctrl Pts',(0.696673901999944,2.2,-4.30711458000001));
#328628=CARTESIAN_POINT('Ctrl Pts',(0.697164535999945,12.2,-4.30522108300002));
#328629=CARTESIAN_POINT('Ctrl Pts',(0.697164535999945,5.2,-4.30522108300002));
#328630=CARTESIAN_POINT('Ctrl Pts',(0.697164535999945,2.2,-4.30522108300002));
#328631=CARTESIAN_POINT('Ctrl Pts',(0.697652025999944,12.2,-4.30333103500002));
#328632=CARTESIAN_POINT('Ctrl Pts',(0.697652025999944,5.2,-4.30333103500002));
#328633=CARTESIAN_POINT('Ctrl Pts',(0.697652025999944,2.2,-4.30333103500002));
#328634=CARTESIAN_POINT('Ctrl Pts',(0.698136379999944,12.2,-4.30144444900002));
#328635=CARTESIAN_POINT('Ctrl Pts',(0.698136379999944,5.2,-4.30144444900002));
#328636=CARTESIAN_POINT('Ctrl Pts',(0.698136379999944,2.2,-4.30144444900002));
#328637=CARTESIAN_POINT('Ctrl Pts',(0.698617604999944,12.2,-4.29956133300001));
#328638=CARTESIAN_POINT('Ctrl Pts',(0.698617604999944,5.2,-4.29956133300001));
#328639=CARTESIAN_POINT('Ctrl Pts',(0.698617604999944,2.2,-4.29956133300001));
#328640=CARTESIAN_POINT('Ctrl Pts',(0.699095704999944,12.2,-4.29768169500001));
#328641=CARTESIAN_POINT('Ctrl Pts',(0.699095704999944,5.2,-4.29768169500001));
#328642=CARTESIAN_POINT('Ctrl Pts',(0.699095704999944,2.2,-4.29768169500001));
#328643=CARTESIAN_POINT('Ctrl Pts',(0.699570687999944,12.2,-4.29580554600001));
#328644=CARTESIAN_POINT('Ctrl Pts',(0.699570687999944,5.2,-4.29580554600001));
#328645=CARTESIAN_POINT('Ctrl Pts',(0.699570687999944,2.2,-4.29580554600001));
#328646=CARTESIAN_POINT('Ctrl Pts',(0.700042559999944,12.2,-4.29393289400001));
#328647=CARTESIAN_POINT('Ctrl Pts',(0.700042559999944,5.2,-4.29393289400001));
#328648=CARTESIAN_POINT('Ctrl Pts',(0.700042559999944,2.2,-4.29393289400001));
#328649=CARTESIAN_POINT('Ctrl Pts',(0.700511326999944,12.2,-4.29206374900001));
#328650=CARTESIAN_POINT('Ctrl Pts',(0.700511326999944,5.2,-4.29206374900001));
#328651=CARTESIAN_POINT('Ctrl Pts',(0.700511326999944,2.2,-4.29206374900001));
#328652=CARTESIAN_POINT('Ctrl Pts',(0.700976993999943,12.2,-4.29019811900002));
#328653=CARTESIAN_POINT('Ctrl Pts',(0.700976993999943,5.2,-4.29019811900002));
#328654=CARTESIAN_POINT('Ctrl Pts',(0.700976993999943,2.2,-4.29019811900002));
#328655=CARTESIAN_POINT('Ctrl Pts',(0.701439569999944,12.2,-4.28833601600001));
#328656=CARTESIAN_POINT('Ctrl Pts',(0.701439569999944,5.2,-4.28833601600001));
#328657=CARTESIAN_POINT('Ctrl Pts',(0.701439569999944,2.2,-4.28833601600001));
#328658=CARTESIAN_POINT('Ctrl Pts',(0.701899058999944,12.2,-4.28647744700001));
#328659=CARTESIAN_POINT('Ctrl Pts',(0.701899058999944,5.2,-4.28647744700001));
#328660=CARTESIAN_POINT('Ctrl Pts',(0.701899058999944,2.2,-4.28647744700001));
#328661=CARTESIAN_POINT('Ctrl Pts',(0.702355468999943,12.2,-4.28462242100002));
#328662=CARTESIAN_POINT('Ctrl Pts',(0.702355468999943,5.2,-4.28462242100002));
#328663=CARTESIAN_POINT('Ctrl Pts',(0.702355468999943,2.2,-4.28462242100002));
#328664=CARTESIAN_POINT('Ctrl Pts',(0.702808804999945,12.2,-4.28277094800002));
#328665=CARTESIAN_POINT('Ctrl Pts',(0.702808804999945,5.2,-4.28277094800002));
#328666=CARTESIAN_POINT('Ctrl Pts',(0.702808804999945,2.2,-4.28277094800002));
#328667=CARTESIAN_POINT('Ctrl Pts',(0.703259075999945,12.2,-4.28092303800002));
#328668=CARTESIAN_POINT('Ctrl Pts',(0.703259075999945,5.2,-4.28092303800002));
#328669=CARTESIAN_POINT('Ctrl Pts',(0.703259075999945,2.2,-4.28092303800002));
#328670=CARTESIAN_POINT('Ctrl Pts',(0.703706284999944,12.2,-4.27907869900002));
#328671=CARTESIAN_POINT('Ctrl Pts',(0.703706284999944,5.2,-4.27907869900002));
#328672=CARTESIAN_POINT('Ctrl Pts',(0.703706284999944,2.2,-4.27907869900002));
#328673=CARTESIAN_POINT('Ctrl Pts',(0.704150439999944,12.2,-4.27723794100002));
#328674=CARTESIAN_POINT('Ctrl Pts',(0.704150439999944,5.2,-4.27723794100002));
#328675=CARTESIAN_POINT('Ctrl Pts',(0.704150439999944,2.2,-4.27723794100002));
#328676=CARTESIAN_POINT('Ctrl Pts',(0.704591548999944,12.2,-4.27540077300002));
#328677=CARTESIAN_POINT('Ctrl Pts',(0.704591548999944,5.2,-4.27540077300002));
#328678=CARTESIAN_POINT('Ctrl Pts',(0.704591548999944,2.2,-4.27540077300002));
#328679=CARTESIAN_POINT('Ctrl Pts',(0.705029615999945,12.2,-4.27356720500002));
#328680=CARTESIAN_POINT('Ctrl Pts',(0.705029615999945,5.2,-4.27356720500002));
#328681=CARTESIAN_POINT('Ctrl Pts',(0.705029615999945,2.2,-4.27356720500002));
#328682=CARTESIAN_POINT('Ctrl Pts',(0.705464648999944,12.2,-4.27173724500001));
#328683=CARTESIAN_POINT('Ctrl Pts',(0.705464648999944,5.2,-4.27173724500001));
#328684=CARTESIAN_POINT('Ctrl Pts',(0.705464648999944,2.2,-4.27173724500001));
#328685=CARTESIAN_POINT('Ctrl Pts',(0.705896653999945,12.2,-4.26991090400001));
#328686=CARTESIAN_POINT('Ctrl Pts',(0.705896653999945,5.2,-4.26991090400001));
#328687=CARTESIAN_POINT('Ctrl Pts',(0.705896653999945,2.2,-4.26991090400001));
#328688=CARTESIAN_POINT('Ctrl Pts',(0.706325638999944,12.2,-4.26808819000001));
#328689=CARTESIAN_POINT('Ctrl Pts',(0.706325638999944,5.2,-4.26808819000001));
#328690=CARTESIAN_POINT('Ctrl Pts',(0.706325638999944,2.2,-4.26808819000001));
#328691=CARTESIAN_POINT('Ctrl Pts',(0.706751607999945,12.2,-4.26626911400001));
#328692=CARTESIAN_POINT('Ctrl Pts',(0.706751607999945,5.2,-4.26626911400001));
#328693=CARTESIAN_POINT('Ctrl Pts',(0.706751607999945,2.2,-4.26626911400001));
#328694=CARTESIAN_POINT('Ctrl Pts',(0.707174569999944,12.2,-4.26445368300001));
#328695=CARTESIAN_POINT('Ctrl Pts',(0.707174569999944,5.2,-4.26445368300001));
#328696=CARTESIAN_POINT('Ctrl Pts',(0.707174569999944,2.2,-4.26445368300001));
#328697=CARTESIAN_POINT('Ctrl Pts',(0.707594530999944,12.2,-4.26264190800001));
#328698=CARTESIAN_POINT('Ctrl Pts',(0.707594530999944,5.2,-4.26264190800001));
#328699=CARTESIAN_POINT('Ctrl Pts',(0.707594530999944,2.2,-4.26264190800001));
#328700=CARTESIAN_POINT('Ctrl Pts',(0.708011496999944,12.2,-4.26083379800001));
#328701=CARTESIAN_POINT('Ctrl Pts',(0.708011496999944,5.2,-4.26083379800001));
#328702=CARTESIAN_POINT('Ctrl Pts',(0.708011496999944,2.2,-4.26083379800001));
#328703=CARTESIAN_POINT('Ctrl Pts',(0.708425474999944,12.2,-4.25902936100002));
#328704=CARTESIAN_POINT('Ctrl Pts',(0.708425474999944,5.2,-4.25902936100002));
#328705=CARTESIAN_POINT('Ctrl Pts',(0.708425474999944,2.2,-4.25902936100002));
#328706=CARTESIAN_POINT('Ctrl Pts',(0.708836471999944,12.2,-4.25722860900001));
#328707=CARTESIAN_POINT('Ctrl Pts',(0.708836471999944,5.2,-4.25722860900001));
#328708=CARTESIAN_POINT('Ctrl Pts',(0.708836471999944,2.2,-4.25722860900001));
#328709=CARTESIAN_POINT('Ctrl Pts',(0.709244494999944,12.2,-4.25543154900001));
#328710=CARTESIAN_POINT('Ctrl Pts',(0.709244494999944,5.2,-4.25543154900001));
#328711=CARTESIAN_POINT('Ctrl Pts',(0.709244494999944,2.2,-4.25543154900001));
#328712=CARTESIAN_POINT('Ctrl Pts',(0.709649549999944,12.2,-4.25363819200001));
#328713=CARTESIAN_POINT('Ctrl Pts',(0.709649549999944,5.2,-4.25363819200001));
#328714=CARTESIAN_POINT('Ctrl Pts',(0.709649549999944,2.2,-4.25363819200001));
#328715=CARTESIAN_POINT('Ctrl Pts',(0.710051644999944,12.2,-4.25184854700001));
#328716=CARTESIAN_POINT('Ctrl Pts',(0.710051644999944,5.2,-4.25184854700001));
#328717=CARTESIAN_POINT('Ctrl Pts',(0.710051644999944,2.2,-4.25184854700001));
#328718=CARTESIAN_POINT('Ctrl Pts',(0.710450784999944,12.2,-4.25006262200001));
#328719=CARTESIAN_POINT('Ctrl Pts',(0.710450784999944,5.2,-4.25006262200001));
#328720=CARTESIAN_POINT('Ctrl Pts',(0.710450784999944,2.2,-4.25006262200001));
#328721=CARTESIAN_POINT('Ctrl Pts',(0.710846977999945,12.2,-4.24828042900002));
#328722=CARTESIAN_POINT('Ctrl Pts',(0.710846977999945,5.2,-4.24828042900002));
#328723=CARTESIAN_POINT('Ctrl Pts',(0.710846977999945,2.2,-4.24828042900002));
#328724=CARTESIAN_POINT('Ctrl Pts',(0.711240232999945,12.2,-4.24650197500001));
#328725=CARTESIAN_POINT('Ctrl Pts',(0.711240232999945,5.2,-4.24650197500001));
#328726=CARTESIAN_POINT('Ctrl Pts',(0.711240232999945,2.2,-4.24650197500001));
#328727=CARTESIAN_POINT('Ctrl Pts',(0.711630551999944,12.2,-4.24472727100001));
#328728=CARTESIAN_POINT('Ctrl Pts',(0.711630551999944,5.2,-4.24472727100001));
#328729=CARTESIAN_POINT('Ctrl Pts',(0.711630551999944,2.2,-4.24472727100001));
#328730=CARTESIAN_POINT('Ctrl Pts',(0.712017946999944,12.2,-4.24295632600002));
#328731=CARTESIAN_POINT('Ctrl Pts',(0.712017946999944,5.2,-4.24295632600002));
#328732=CARTESIAN_POINT('Ctrl Pts',(0.712017946999944,2.2,-4.24295632600002));
#328733=CARTESIAN_POINT('Ctrl Pts',(0.712402421999945,12.2,-4.24118915000002));
#328734=CARTESIAN_POINT('Ctrl Pts',(0.712402421999945,5.2,-4.24118915000002));
#328735=CARTESIAN_POINT('Ctrl Pts',(0.712402421999945,2.2,-4.24118915000002));
#328736=CARTESIAN_POINT('Ctrl Pts',(0.712783982999944,12.2,-4.23942575000002));
#328737=CARTESIAN_POINT('Ctrl Pts',(0.712783982999944,5.2,-4.23942575000002));
#328738=CARTESIAN_POINT('Ctrl Pts',(0.712783982999944,2.2,-4.23942575000002));
#328739=CARTESIAN_POINT('Ctrl Pts',(0.713162640999945,12.2,-4.23766613800002));
#328740=CARTESIAN_POINT('Ctrl Pts',(0.713162640999945,5.2,-4.23766613800002));
#328741=CARTESIAN_POINT('Ctrl Pts',(0.713162640999945,2.2,-4.23766613800002));
#328742=CARTESIAN_POINT('Ctrl Pts',(0.713538398999944,12.2,-4.23591032200001));
#328743=CARTESIAN_POINT('Ctrl Pts',(0.713538398999944,5.2,-4.23591032200001));
#328744=CARTESIAN_POINT('Ctrl Pts',(0.713538398999944,2.2,-4.23591032200001));
#328745=CARTESIAN_POINT('Ctrl Pts',(0.713911265999945,12.2,-4.23415831300002));
#328746=CARTESIAN_POINT('Ctrl Pts',(0.713911265999945,5.2,-4.23415831300002));
#328747=CARTESIAN_POINT('Ctrl Pts',(0.713911265999945,2.2,-4.23415831300002));
#328748=CARTESIAN_POINT('Ctrl Pts',(0.714281250999944,12.2,-4.23241011900001));
#328749=CARTESIAN_POINT('Ctrl Pts',(0.714281250999944,5.2,-4.23241011900001));
#328750=CARTESIAN_POINT('Ctrl Pts',(0.714281250999944,2.2,-4.23241011900001));
#328751=CARTESIAN_POINT('Ctrl Pts',(0.714648356999944,12.2,-4.23066575100002));
#328752=CARTESIAN_POINT('Ctrl Pts',(0.714648356999944,5.2,-4.23066575100002));
#328753=CARTESIAN_POINT('Ctrl Pts',(0.714648356999944,2.2,-4.23066575100002));
#328754=CARTESIAN_POINT('Ctrl Pts',(0.715012592999944,12.2,-4.22892521700001));
#328755=CARTESIAN_POINT('Ctrl Pts',(0.715012592999944,5.2,-4.22892521700001));
#328756=CARTESIAN_POINT('Ctrl Pts',(0.715012592999944,2.2,-4.22892521700001));
#328757=CARTESIAN_POINT('Ctrl Pts',(0.715373966999944,12.2,-4.22718852600001));
#328758=CARTESIAN_POINT('Ctrl Pts',(0.715373966999944,5.2,-4.22718852600001));
#328759=CARTESIAN_POINT('Ctrl Pts',(0.715373966999944,2.2,-4.22718852600001));
#328760=CARTESIAN_POINT('Ctrl Pts',(0.715732484999945,12.2,-4.22545569000001));
#328761=CARTESIAN_POINT('Ctrl Pts',(0.715732484999945,5.2,-4.22545569000001));
#328762=CARTESIAN_POINT('Ctrl Pts',(0.715732484999945,2.2,-4.22545569000001));
#328763=CARTESIAN_POINT('Ctrl Pts',(0.716088154999944,12.2,-4.22372671600002));
#328764=CARTESIAN_POINT('Ctrl Pts',(0.716088154999944,5.2,-4.22372671600002));
#328765=CARTESIAN_POINT('Ctrl Pts',(0.716088154999944,2.2,-4.22372671600002));
#328766=CARTESIAN_POINT('Ctrl Pts',(0.716440982999944,12.2,-4.22200161500002));
#328767=CARTESIAN_POINT('Ctrl Pts',(0.716440982999944,5.2,-4.22200161500002));
#328768=CARTESIAN_POINT('Ctrl Pts',(0.716440982999944,2.2,-4.22200161500002));
#328769=CARTESIAN_POINT('Ctrl Pts',(0.716790976999944,12.2,-4.22028039700002));
#328770=CARTESIAN_POINT('Ctrl Pts',(0.716790976999944,5.2,-4.22028039700002));
#328771=CARTESIAN_POINT('Ctrl Pts',(0.716790976999944,2.2,-4.22028039700002));
#328772=CARTESIAN_POINT('Ctrl Pts',(0.717138145999944,12.2,-4.21856306900001));
#328773=CARTESIAN_POINT('Ctrl Pts',(0.717138145999944,5.2,-4.21856306900001));
#328774=CARTESIAN_POINT('Ctrl Pts',(0.717138145999944,2.2,-4.21856306900001));
#328775=CARTESIAN_POINT('Ctrl Pts',(0.717482494999944,12.2,-4.21684964300002));
#328776=CARTESIAN_POINT('Ctrl Pts',(0.717482494999944,5.2,-4.21684964300002));
#328777=CARTESIAN_POINT('Ctrl Pts',(0.717482494999944,2.2,-4.21684964300002));
#328778=CARTESIAN_POINT('Ctrl Pts',(0.717824032999944,12.2,-4.21514012700001));
#328779=CARTESIAN_POINT('Ctrl Pts',(0.717824032999944,5.2,-4.21514012700001));
#328780=CARTESIAN_POINT('Ctrl Pts',(0.717824032999944,2.2,-4.21514012700001));
#328781=CARTESIAN_POINT('Ctrl Pts',(0.718162764999944,12.2,-4.21343453200001));
#328782=CARTESIAN_POINT('Ctrl Pts',(0.718162764999944,5.2,-4.21343453200001));
#328783=CARTESIAN_POINT('Ctrl Pts',(0.718162764999944,2.2,-4.21343453200001));
#328784=CARTESIAN_POINT('Ctrl Pts',(0.718498699999944,12.2,-4.21173286600002));
#328785=CARTESIAN_POINT('Ctrl Pts',(0.718498699999944,5.2,-4.21173286600002));
#328786=CARTESIAN_POINT('Ctrl Pts',(0.718498699999944,2.2,-4.21173286600002));
#328787=CARTESIAN_POINT('Ctrl Pts',(0.718831845999944,12.2,-4.21003514000001));
#328788=CARTESIAN_POINT('Ctrl Pts',(0.718831845999944,5.2,-4.21003514000001));
#328789=CARTESIAN_POINT('Ctrl Pts',(0.718831845999944,2.2,-4.21003514000001));
#328790=CARTESIAN_POINT('Ctrl Pts',(0.719162208999945,12.2,-4.20834136300002));
#328791=CARTESIAN_POINT('Ctrl Pts',(0.719162208999945,5.2,-4.20834136300002));
#328792=CARTESIAN_POINT('Ctrl Pts',(0.719162208999945,2.2,-4.20834136300002));
#328793=CARTESIAN_POINT('Ctrl Pts',(0.719489797999944,12.2,-4.20665154400002));
#328794=CARTESIAN_POINT('Ctrl Pts',(0.719489797999944,5.2,-4.20665154400002));
#328795=CARTESIAN_POINT('Ctrl Pts',(0.719489797999944,2.2,-4.20665154400002));
#328796=CARTESIAN_POINT('Ctrl Pts',(0.719814618999944,12.2,-4.20496569300001));
#328797=CARTESIAN_POINT('Ctrl Pts',(0.719814618999944,5.2,-4.20496569300001));
#328798=CARTESIAN_POINT('Ctrl Pts',(0.719814618999944,2.2,-4.20496569300001));
#328799=CARTESIAN_POINT('Ctrl Pts',(0.720136680999944,12.2,-4.20328382000001));
#328800=CARTESIAN_POINT('Ctrl Pts',(0.720136680999944,5.2,-4.20328382000001));
#328801=CARTESIAN_POINT('Ctrl Pts',(0.720136680999944,2.2,-4.20328382000001));
#328802=CARTESIAN_POINT('Ctrl Pts',(0.720455989999944,12.2,-4.20160593400002));
#328803=CARTESIAN_POINT('Ctrl Pts',(0.720455989999944,5.2,-4.20160593400002));
#328804=CARTESIAN_POINT('Ctrl Pts',(0.720455989999944,2.2,-4.20160593400002));
#328805=CARTESIAN_POINT('Ctrl Pts',(0.720772555999944,12.2,-4.19993204500001));
#328806=CARTESIAN_POINT('Ctrl Pts',(0.720772555999944,5.2,-4.19993204500001));
#328807=CARTESIAN_POINT('Ctrl Pts',(0.720772555999944,2.2,-4.19993204500001));
#328808=CARTESIAN_POINT('Ctrl Pts',(0.721086382999945,12.2,-4.19826216300001));
#328809=CARTESIAN_POINT('Ctrl Pts',(0.721086382999945,5.2,-4.19826216300001));
#328810=CARTESIAN_POINT('Ctrl Pts',(0.721086382999945,2.2,-4.19826216300001));
#328811=CARTESIAN_POINT('Ctrl Pts',(0.721397480999945,12.2,-4.19659629700002));
#328812=CARTESIAN_POINT('Ctrl Pts',(0.721397480999945,5.2,-4.19659629700002));
#328813=CARTESIAN_POINT('Ctrl Pts',(0.721397480999945,2.2,-4.19659629700002));
#328814=CARTESIAN_POINT('Ctrl Pts',(0.721705857999945,12.2,-4.19493445500001));
#328815=CARTESIAN_POINT('Ctrl Pts',(0.721705857999945,5.2,-4.19493445500001));
#328816=CARTESIAN_POINT('Ctrl Pts',(0.721705857999945,2.2,-4.19493445500001));
#328817=CARTESIAN_POINT('Ctrl Pts',(0.722011521999945,12.2,-4.19327665100001));
#328818=CARTESIAN_POINT('Ctrl Pts',(0.722011521999945,5.2,-4.19327665100001));
#328819=CARTESIAN_POINT('Ctrl Pts',(0.722011521999945,2.2,-4.19327665100001));
#328820=CARTESIAN_POINT('Ctrl Pts',(0.722314477999944,12.2,-4.19162289000001));
#328821=CARTESIAN_POINT('Ctrl Pts',(0.722314477999944,5.2,-4.19162289000001));
#328822=CARTESIAN_POINT('Ctrl Pts',(0.722314477999944,2.2,-4.19162289000001));
#328823=CARTESIAN_POINT('Ctrl Pts',(0.722614734999943,12.2,-4.18997318500002));
#328824=CARTESIAN_POINT('Ctrl Pts',(0.722614734999943,5.2,-4.18997318500002));
#328825=CARTESIAN_POINT('Ctrl Pts',(0.722614734999943,2.2,-4.18997318500002));
#328826=CARTESIAN_POINT('Ctrl Pts',(0.722912302999944,12.2,-4.18832754300002));
#328827=CARTESIAN_POINT('Ctrl Pts',(0.722912302999944,5.2,-4.18832754300002));
#328828=CARTESIAN_POINT('Ctrl Pts',(0.722912302999944,2.2,-4.18832754300002));
#328829=CARTESIAN_POINT('Ctrl Pts',(0.723207185999944,12.2,-4.18668597600002));
#328830=CARTESIAN_POINT('Ctrl Pts',(0.723207185999944,5.2,-4.18668597600002));
#328831=CARTESIAN_POINT('Ctrl Pts',(0.723207185999944,2.2,-4.18668597600002));
#328832=CARTESIAN_POINT('Ctrl Pts',(0.723499394999945,12.2,-4.18504849200001));
#328833=CARTESIAN_POINT('Ctrl Pts',(0.723499394999945,5.2,-4.18504849200001));
#328834=CARTESIAN_POINT('Ctrl Pts',(0.723499394999945,2.2,-4.18504849200001));
#328835=CARTESIAN_POINT('Ctrl Pts',(0.723788936999944,12.2,-4.18341510300001));
#328836=CARTESIAN_POINT('Ctrl Pts',(0.723788936999944,5.2,-4.18341510300001));
#328837=CARTESIAN_POINT('Ctrl Pts',(0.723788936999944,2.2,-4.18341510300001));
#328838=CARTESIAN_POINT('Ctrl Pts',(0.724075819999944,12.2,-4.18178581500001));
#328839=CARTESIAN_POINT('Ctrl Pts',(0.724075819999944,5.2,-4.18178581500001));
#328840=CARTESIAN_POINT('Ctrl Pts',(0.724075819999944,2.2,-4.18178581500001));
#328841=CARTESIAN_POINT('Ctrl Pts',(0.724360049999944,12.2,-4.18016064100001));
#328842=CARTESIAN_POINT('Ctrl Pts',(0.724360049999944,5.2,-4.18016064100001));
#328843=CARTESIAN_POINT('Ctrl Pts',(0.724360049999944,2.2,-4.18016064100001));
#328844=CARTESIAN_POINT('Ctrl Pts',(0.724641636999944,12.2,-4.17853958900002));
#328845=CARTESIAN_POINT('Ctrl Pts',(0.724641636999944,5.2,-4.17853958900002));
#328846=CARTESIAN_POINT('Ctrl Pts',(0.724641636999944,2.2,-4.17853958900002));
#328847=CARTESIAN_POINT('Ctrl Pts',(0.724920587999944,12.2,-4.17692266800001));
#328848=CARTESIAN_POINT('Ctrl Pts',(0.724920587999944,5.2,-4.17692266800001));
#328849=CARTESIAN_POINT('Ctrl Pts',(0.724920587999944,2.2,-4.17692266800001));
#328850=CARTESIAN_POINT('Ctrl Pts',(0.725196911999944,12.2,-4.17530989100001));
#328851=CARTESIAN_POINT('Ctrl Pts',(0.725196911999944,5.2,-4.17530989100001));
#328852=CARTESIAN_POINT('Ctrl Pts',(0.725196911999944,2.2,-4.17530989100001));
#328853=CARTESIAN_POINT('Ctrl Pts',(0.725470616999945,12.2,-4.17370126400002));
#328854=CARTESIAN_POINT('Ctrl Pts',(0.725470616999945,5.2,-4.17370126400002));
#328855=CARTESIAN_POINT('Ctrl Pts',(0.725470616999945,2.2,-4.17370126400002));
#328856=CARTESIAN_POINT('Ctrl Pts',(0.725741709999944,12.2,-4.17209679900001));
#328857=CARTESIAN_POINT('Ctrl Pts',(0.725741709999944,5.2,-4.17209679900001));
#328858=CARTESIAN_POINT('Ctrl Pts',(0.725741709999944,2.2,-4.17209679900001));
#328859=CARTESIAN_POINT('Ctrl Pts',(0.726010198999945,12.2,-4.17049650500001));
#328860=CARTESIAN_POINT('Ctrl Pts',(0.726010198999945,5.2,-4.17049650500001));
#328861=CARTESIAN_POINT('Ctrl Pts',(0.726010198999945,2.2,-4.17049650500001));
#328862=CARTESIAN_POINT('Ctrl Pts',(0.726276091999944,12.2,-4.16890039200001));
#328863=CARTESIAN_POINT('Ctrl Pts',(0.726276091999944,5.2,-4.16890039200001));
#328864=CARTESIAN_POINT('Ctrl Pts',(0.726276091999944,2.2,-4.16890039200001));
#328865=CARTESIAN_POINT('Ctrl Pts',(0.726539398999945,12.2,-4.16730846900002));
#328866=CARTESIAN_POINT('Ctrl Pts',(0.726539398999945,5.2,-4.16730846900002));
#328867=CARTESIAN_POINT('Ctrl Pts',(0.726539398999945,2.2,-4.16730846900002));
#328868=CARTESIAN_POINT('Ctrl Pts',(0.726800126999944,12.2,-4.16572074700001));
#328869=CARTESIAN_POINT('Ctrl Pts',(0.726800126999944,5.2,-4.16572074700001));
#328870=CARTESIAN_POINT('Ctrl Pts',(0.726800126999944,2.2,-4.16572074700001));
#328871=CARTESIAN_POINT('Ctrl Pts',(0.727058282999944,12.2,-4.16413723500002));
#328872=CARTESIAN_POINT('Ctrl Pts',(0.727058282999944,5.2,-4.16413723500002));
#328873=CARTESIAN_POINT('Ctrl Pts',(0.727058282999944,2.2,-4.16413723500002));
#328874=CARTESIAN_POINT('Ctrl Pts',(0.727313877999943,12.2,-4.16255794200001));
#328875=CARTESIAN_POINT('Ctrl Pts',(0.727313877999943,5.2,-4.16255794200001));
#328876=CARTESIAN_POINT('Ctrl Pts',(0.727313877999943,2.2,-4.16255794200001));
#328877=CARTESIAN_POINT('Ctrl Pts',(0.727566916999944,12.2,-4.16098288000001));
#328878=CARTESIAN_POINT('Ctrl Pts',(0.727566916999944,5.2,-4.16098288000001));
#328879=CARTESIAN_POINT('Ctrl Pts',(0.727566916999944,2.2,-4.16098288000001));
#328880=CARTESIAN_POINT('Ctrl Pts',(0.727817410999945,12.2,-4.15941205600001));
#328881=CARTESIAN_POINT('Ctrl Pts',(0.727817410999945,5.2,-4.15941205600001));
#328882=CARTESIAN_POINT('Ctrl Pts',(0.727817410999945,2.2,-4.15941205600001));
#328883=CARTESIAN_POINT('Ctrl Pts',(0.728065366999945,12.2,-4.15784548300001));
#328884=CARTESIAN_POINT('Ctrl Pts',(0.728065366999945,5.2,-4.15784548300001));
#328885=CARTESIAN_POINT('Ctrl Pts',(0.728065366999945,2.2,-4.15784548300001));
#328886=CARTESIAN_POINT('Ctrl Pts',(0.728310792999943,12.2,-4.15628316800001));
#328887=CARTESIAN_POINT('Ctrl Pts',(0.728310792999943,5.2,-4.15628316800001));
#328888=CARTESIAN_POINT('Ctrl Pts',(0.728310792999943,2.2,-4.15628316800001));
#328889=CARTESIAN_POINT('Ctrl Pts',(0.728553698999944,12.2,-4.15472512200001));
#328890=CARTESIAN_POINT('Ctrl Pts',(0.728553698999944,5.2,-4.15472512200001));
#328891=CARTESIAN_POINT('Ctrl Pts',(0.728553698999944,2.2,-4.15472512200001));
#328892=CARTESIAN_POINT('Ctrl Pts',(0.728794090999945,12.2,-4.15317135500001));
#328893=CARTESIAN_POINT('Ctrl Pts',(0.728794090999945,5.2,-4.15317135500001));
#328894=CARTESIAN_POINT('Ctrl Pts',(0.728794090999945,2.2,-4.15317135500001));
#328895=CARTESIAN_POINT('Ctrl Pts',(0.729031978999944,12.2,-4.15162187600002));
#328896=CARTESIAN_POINT('Ctrl Pts',(0.729031978999944,5.2,-4.15162187600002));
#328897=CARTESIAN_POINT('Ctrl Pts',(0.729031978999944,2.2,-4.15162187600002));
#328898=CARTESIAN_POINT('Ctrl Pts',(0.729267370999944,12.2,-4.15007669700001));
#328899=CARTESIAN_POINT('Ctrl Pts',(0.729267370999944,5.2,-4.15007669700001));
#328900=CARTESIAN_POINT('Ctrl Pts',(0.729267370999944,2.2,-4.15007669700001));
#328901=CARTESIAN_POINT('Ctrl Pts',(0.729500276999944,12.2,-4.14853582400001));
#328902=CARTESIAN_POINT('Ctrl Pts',(0.729500276999944,5.2,-4.14853582400001));
#328903=CARTESIAN_POINT('Ctrl Pts',(0.729500276999944,2.2,-4.14853582400001));
#328904=CARTESIAN_POINT('Ctrl Pts',(0.729730702999943,12.2,-4.14699927100001));
#328905=CARTESIAN_POINT('Ctrl Pts',(0.729730702999943,5.2,-4.14699927100001));
#328906=CARTESIAN_POINT('Ctrl Pts',(0.729730702999943,2.2,-4.14699927100001));
#328907=CARTESIAN_POINT('Ctrl Pts',(0.729958658999944,12.2,-4.14546704400002));
#328908=CARTESIAN_POINT('Ctrl Pts',(0.729958658999944,5.2,-4.14546704400002));
#328909=CARTESIAN_POINT('Ctrl Pts',(0.729958658999944,2.2,-4.14546704400002));
#328910=CARTESIAN_POINT('Ctrl Pts',(0.730184153999944,12.2,-4.14393915700002));
#328911=CARTESIAN_POINT('Ctrl Pts',(0.730184153999944,5.2,-4.14393915700002));
#328912=CARTESIAN_POINT('Ctrl Pts',(0.730184153999944,2.2,-4.14393915700002));
#328913=CARTESIAN_POINT('Ctrl Pts',(0.730407194999944,12.2,-4.14241561600001));
#328914=CARTESIAN_POINT('Ctrl Pts',(0.730407194999944,5.2,-4.14241561600001));
#328915=CARTESIAN_POINT('Ctrl Pts',(0.730407194999944,2.2,-4.14241561600001));
#328916=CARTESIAN_POINT('Ctrl Pts',(0.730627791999944,12.2,-4.14089643400001));
#328917=CARTESIAN_POINT('Ctrl Pts',(0.730627791999944,5.2,-4.14089643400001));
#328918=CARTESIAN_POINT('Ctrl Pts',(0.730627791999944,2.2,-4.14089643400001));
#328919=CARTESIAN_POINT('Ctrl Pts',(0.730845953999945,12.2,-4.13938161900001));
#328920=CARTESIAN_POINT('Ctrl Pts',(0.730845953999945,5.2,-4.13938161900001));
#328921=CARTESIAN_POINT('Ctrl Pts',(0.730845953999945,2.2,-4.13938161900001));
#328922=CARTESIAN_POINT('Ctrl Pts',(0.731061687999944,12.2,-4.13787118200001));
#328923=CARTESIAN_POINT('Ctrl Pts',(0.731061687999944,5.2,-4.13787118200001));
#328924=CARTESIAN_POINT('Ctrl Pts',(0.731061687999944,2.2,-4.13787118200001));
#328925=CARTESIAN_POINT('Ctrl Pts',(0.731275002999944,12.2,-4.13636513200001));
#328926=CARTESIAN_POINT('Ctrl Pts',(0.731275002999944,5.2,-4.13636513200001));
#328927=CARTESIAN_POINT('Ctrl Pts',(0.731275002999944,2.2,-4.13636513200001));
#328928=CARTESIAN_POINT('Ctrl Pts',(0.731485909999944,12.2,-4.13486347900001));
#328929=CARTESIAN_POINT('Ctrl Pts',(0.731485909999944,5.2,-4.13486347900001));
#328930=CARTESIAN_POINT('Ctrl Pts',(0.731485909999944,2.2,-4.13486347900001));
#328931=CARTESIAN_POINT('Ctrl Pts',(0.731694414999944,12.2,-4.13336623300002));
#328932=CARTESIAN_POINT('Ctrl Pts',(0.731694414999944,5.2,-4.13336623300002));
#328933=CARTESIAN_POINT('Ctrl Pts',(0.731694414999944,2.2,-4.13336623300002));
#328934=CARTESIAN_POINT('Ctrl Pts',(0.731900528999944,12.2,-4.13187340400002));
#328935=CARTESIAN_POINT('Ctrl Pts',(0.731900528999944,5.2,-4.13187340400002));
#328936=CARTESIAN_POINT('Ctrl Pts',(0.731900528999944,2.2,-4.13187340400002));
#328937=CARTESIAN_POINT('Ctrl Pts',(0.732104258999944,12.2,-4.13038500300001));
#328938=CARTESIAN_POINT('Ctrl Pts',(0.732104258999944,5.2,-4.13038500300001));
#328939=CARTESIAN_POINT('Ctrl Pts',(0.732104258999944,2.2,-4.13038500300001));
#328940=CARTESIAN_POINT('Ctrl Pts',(0.732305614999944,12.2,-4.12890103900001));
#328941=CARTESIAN_POINT('Ctrl Pts',(0.732305614999944,5.2,-4.12890103900001));
#328942=CARTESIAN_POINT('Ctrl Pts',(0.732305614999944,2.2,-4.12890103900001));
#328943=CARTESIAN_POINT('Ctrl Pts',(0.732504605999944,12.2,-4.12742152100002));
#328944=CARTESIAN_POINT('Ctrl Pts',(0.732504605999944,5.2,-4.12742152100002));
#328945=CARTESIAN_POINT('Ctrl Pts',(0.732504605999944,2.2,-4.12742152100002));
#328946=CARTESIAN_POINT('Ctrl Pts',(0.732701239999944,12.2,-4.12594646000001));
#328947=CARTESIAN_POINT('Ctrl Pts',(0.732701239999944,5.2,-4.12594646000001));
#328948=CARTESIAN_POINT('Ctrl Pts',(0.732701239999944,2.2,-4.12594646000001));
#328949=CARTESIAN_POINT('Ctrl Pts',(0.732895527999945,12.2,-4.12447586700001));
#328950=CARTESIAN_POINT('Ctrl Pts',(0.732895527999945,5.2,-4.12447586700001));
#328951=CARTESIAN_POINT('Ctrl Pts',(0.732895527999945,2.2,-4.12447586700001));
#328952=CARTESIAN_POINT('Ctrl Pts',(0.733087475999944,12.2,-4.12300975000001));
#328953=CARTESIAN_POINT('Ctrl Pts',(0.733087475999944,5.2,-4.12300975000001));
#328954=CARTESIAN_POINT('Ctrl Pts',(0.733087475999944,2.2,-4.12300975000001));
#328955=CARTESIAN_POINT('Ctrl Pts',(0.733277095999945,12.2,-4.12154812100002));
#328956=CARTESIAN_POINT('Ctrl Pts',(0.733277095999945,5.2,-4.12154812100002));
#328957=CARTESIAN_POINT('Ctrl Pts',(0.733277095999945,2.2,-4.12154812100002));
#328958=CARTESIAN_POINT('Ctrl Pts',(0.733464394999944,12.2,-4.12009098900001));
#328959=CARTESIAN_POINT('Ctrl Pts',(0.733464394999944,5.2,-4.12009098900001));
#328960=CARTESIAN_POINT('Ctrl Pts',(0.733464394999944,2.2,-4.12009098900001));
#328961=CARTESIAN_POINT('Ctrl Pts',(0.733649382999944,12.2,-4.11863836300002));
#328962=CARTESIAN_POINT('Ctrl Pts',(0.733649382999944,5.2,-4.11863836300002));
#328963=CARTESIAN_POINT('Ctrl Pts',(0.733649382999944,2.2,-4.11863836300002));
#328964=CARTESIAN_POINT('Ctrl Pts',(0.733832068999944,12.2,-4.11719025400001));
#328965=CARTESIAN_POINT('Ctrl Pts',(0.733832068999944,5.2,-4.11719025400001));
#328966=CARTESIAN_POINT('Ctrl Pts',(0.733832068999944,2.2,-4.11719025400001));
#328967=CARTESIAN_POINT('Ctrl Pts',(0.734012461999944,12.2,-4.11574667300002));
#328968=CARTESIAN_POINT('Ctrl Pts',(0.734012461999944,5.2,-4.11574667300002));
#328969=CARTESIAN_POINT('Ctrl Pts',(0.734012461999944,2.2,-4.11574667300002));
#328970=CARTESIAN_POINT('Ctrl Pts',(0.734190571999944,12.2,-4.11430762700002));
#328971=CARTESIAN_POINT('Ctrl Pts',(0.734190571999944,5.2,-4.11430762700002));
#328972=CARTESIAN_POINT('Ctrl Pts',(0.734190571999944,2.2,-4.11430762700002));
#328973=CARTESIAN_POINT('Ctrl Pts',(0.734366405999943,12.2,-4.11287313100001));
#328974=CARTESIAN_POINT('Ctrl Pts',(0.734366405999943,5.2,-4.11287313100001));
#328975=CARTESIAN_POINT('Ctrl Pts',(0.734366405999943,2.2,-4.11287313100001));
#328976=CARTESIAN_POINT('Ctrl Pts',(0.734539975999944,12.2,-4.11144319000002));
#328977=CARTESIAN_POINT('Ctrl Pts',(0.734539975999944,5.2,-4.11144319000002));
#328978=CARTESIAN_POINT('Ctrl Pts',(0.734539975999944,2.2,-4.11144319000002));
#328979=CARTESIAN_POINT('Ctrl Pts',(0.734711289999944,12.2,-4.11001781700001));
#328980=CARTESIAN_POINT('Ctrl Pts',(0.734711289999944,5.2,-4.11001781700001));
#328981=CARTESIAN_POINT('Ctrl Pts',(0.734711289999944,2.2,-4.11001781700001));
#328982=CARTESIAN_POINT('Ctrl Pts',(0.734880356999944,12.2,-4.10859702100002));
#328983=CARTESIAN_POINT('Ctrl Pts',(0.734880356999944,5.2,-4.10859702100002));
#328984=CARTESIAN_POINT('Ctrl Pts',(0.734880356999944,2.2,-4.10859702100002));
#328985=CARTESIAN_POINT('Ctrl Pts',(0.735047187999944,12.2,-4.10718081300002));
#328986=CARTESIAN_POINT('Ctrl Pts',(0.735047187999944,5.2,-4.10718081300002));
#328987=CARTESIAN_POINT('Ctrl Pts',(0.735047187999944,2.2,-4.10718081300002));
#328988=CARTESIAN_POINT('Ctrl Pts',(0.735211790999944,12.2,-4.10576920200001));
#328989=CARTESIAN_POINT('Ctrl Pts',(0.735211790999944,5.2,-4.10576920200001));
#328990=CARTESIAN_POINT('Ctrl Pts',(0.735211790999944,2.2,-4.10576920200001));
#328991=CARTESIAN_POINT('Ctrl Pts',(0.735374174999944,12.2,-4.10436219900001));
#328992=CARTESIAN_POINT('Ctrl Pts',(0.735374174999944,5.2,-4.10436219900001));
#328993=CARTESIAN_POINT('Ctrl Pts',(0.735374174999944,2.2,-4.10436219900001));
#328994=CARTESIAN_POINT('Ctrl Pts',(0.735534349999944,12.2,-4.10295981200001));
#328995=CARTESIAN_POINT('Ctrl Pts',(0.735534349999944,5.2,-4.10295981200001));
#328996=CARTESIAN_POINT('Ctrl Pts',(0.735534349999944,2.2,-4.10295981200001));
#328997=CARTESIAN_POINT('Ctrl Pts',(0.735692325999944,12.2,-4.10156205400002));
#328998=CARTESIAN_POINT('Ctrl Pts',(0.735692325999944,5.2,-4.10156205400002));
#328999=CARTESIAN_POINT('Ctrl Pts',(0.735692325999944,2.2,-4.10156205400002));
#329000=CARTESIAN_POINT('Ctrl Pts',(0.735848111999945,12.2,-4.10016893300002));
#329001=CARTESIAN_POINT('Ctrl Pts',(0.735848111999945,5.2,-4.10016893300002));
#329002=CARTESIAN_POINT('Ctrl Pts',(0.735848111999945,2.2,-4.10016893300002));
#329003=CARTESIAN_POINT('Ctrl Pts',(0.736001718999945,12.2,-4.09878046200001));
#329004=CARTESIAN_POINT('Ctrl Pts',(0.736001718999945,5.2,-4.09878046200001));
#329005=CARTESIAN_POINT('Ctrl Pts',(0.736001718999945,2.2,-4.09878046200001));
#329006=CARTESIAN_POINT('Ctrl Pts',(0.736153152999944,12.2,-4.09739664800002));
#329007=CARTESIAN_POINT('Ctrl Pts',(0.736153152999944,5.2,-4.09739664800002));
#329008=CARTESIAN_POINT('Ctrl Pts',(0.736153152999944,2.2,-4.09739664800002));
#329009=CARTESIAN_POINT('Ctrl Pts',(0.736302427999944,12.2,-4.09601750200002));
#329010=CARTESIAN_POINT('Ctrl Pts',(0.736302427999944,5.2,-4.09601750200002));
#329011=CARTESIAN_POINT('Ctrl Pts',(0.736302427999944,2.2,-4.09601750200002));
#329012=CARTESIAN_POINT('Ctrl Pts',(0.736449549999943,12.2,-4.09464303500001));
#329013=CARTESIAN_POINT('Ctrl Pts',(0.736449549999943,5.2,-4.09464303500001));
#329014=CARTESIAN_POINT('Ctrl Pts',(0.736449549999943,2.2,-4.09464303500001));
#329015=CARTESIAN_POINT('Ctrl Pts',(0.736594531999945,12.2,-4.09327325700001));
#329016=CARTESIAN_POINT('Ctrl Pts',(0.736594531999945,5.2,-4.09327325700001));
#329017=CARTESIAN_POINT('Ctrl Pts',(0.736594531999945,2.2,-4.09327325700001));
#329018=CARTESIAN_POINT('Ctrl Pts',(0.736737380999944,12.2,-4.09190817700001));
#329019=CARTESIAN_POINT('Ctrl Pts',(0.736737380999944,5.2,-4.09190817700001));
#329020=CARTESIAN_POINT('Ctrl Pts',(0.736737380999944,2.2,-4.09190817700001));
#329021=CARTESIAN_POINT('Ctrl Pts',(0.736878106999944,12.2,-4.09054780600002));
#329022=CARTESIAN_POINT('Ctrl Pts',(0.736878106999944,5.2,-4.09054780600002));
#329023=CARTESIAN_POINT('Ctrl Pts',(0.736878106999944,2.2,-4.09054780600002));
#329024=CARTESIAN_POINT('Ctrl Pts',(0.737016721999945,12.2,-4.08919215500001));
#329025=CARTESIAN_POINT('Ctrl Pts',(0.737016721999945,5.2,-4.08919215500001));
#329026=CARTESIAN_POINT('Ctrl Pts',(0.737016721999945,2.2,-4.08919215500001));
#329027=CARTESIAN_POINT('Ctrl Pts',(0.737153233999944,12.2,-4.08784123200002));
#329028=CARTESIAN_POINT('Ctrl Pts',(0.737153233999944,5.2,-4.08784123200002));
#329029=CARTESIAN_POINT('Ctrl Pts',(0.737153233999944,2.2,-4.08784123200002));
#329030=CARTESIAN_POINT('Ctrl Pts',(0.737287653999944,12.2,-4.08649505000001));
#329031=CARTESIAN_POINT('Ctrl Pts',(0.737287653999944,5.2,-4.08649505000001));
#329032=CARTESIAN_POINT('Ctrl Pts',(0.737287653999944,2.2,-4.08649505000001));
#329033=CARTESIAN_POINT('Ctrl Pts',(0.737419989999945,12.2,-4.08515361700001));
#329034=CARTESIAN_POINT('Ctrl Pts',(0.737419989999945,5.2,-4.08515361700001));
#329035=CARTESIAN_POINT('Ctrl Pts',(0.737419989999945,2.2,-4.08515361700001));
#329036=CARTESIAN_POINT('Ctrl Pts',(0.737550252999944,12.2,-4.08381694400001));
#329037=CARTESIAN_POINT('Ctrl Pts',(0.737550252999944,5.2,-4.08381694400001));
#329038=CARTESIAN_POINT('Ctrl Pts',(0.737550252999944,2.2,-4.08381694400001));
#329039=CARTESIAN_POINT('Ctrl Pts',(0.737678454999945,12.2,-4.08248504200001));
#329040=CARTESIAN_POINT('Ctrl Pts',(0.737678454999945,5.2,-4.08248504200001));
#329041=CARTESIAN_POINT('Ctrl Pts',(0.737678454999945,2.2,-4.08248504200001));
#329042=CARTESIAN_POINT('Ctrl Pts',(0.737804602999944,12.2,-4.08115792000002));
#329043=CARTESIAN_POINT('Ctrl Pts',(0.737804602999944,5.2,-4.08115792000002));
#329044=CARTESIAN_POINT('Ctrl Pts',(0.737804602999944,2.2,-4.08115792000002));
#329045=CARTESIAN_POINT('Ctrl Pts',(0.737928706999944,12.2,-4.07983558900002));
#329046=CARTESIAN_POINT('Ctrl Pts',(0.737928706999944,5.2,-4.07983558900002));
#329047=CARTESIAN_POINT('Ctrl Pts',(0.737928706999944,2.2,-4.07983558900002));
#329048=CARTESIAN_POINT('Ctrl Pts',(0.738050778999945,12.2,-4.07851805900001));
#329049=CARTESIAN_POINT('Ctrl Pts',(0.738050778999945,5.2,-4.07851805900001));
#329050=CARTESIAN_POINT('Ctrl Pts',(0.738050778999945,2.2,-4.07851805900001));
#329051=CARTESIAN_POINT('Ctrl Pts',(0.738170829999943,12.2,-4.07720534100001));
#329052=CARTESIAN_POINT('Ctrl Pts',(0.738170829999943,5.2,-4.07720534100001));
#329053=CARTESIAN_POINT('Ctrl Pts',(0.738170829999943,2.2,-4.07720534100001));
#329054=CARTESIAN_POINT('Ctrl Pts',(0.738288867999944,12.2,-4.07589744400001));
#329055=CARTESIAN_POINT('Ctrl Pts',(0.738288867999944,5.2,-4.07589744400001));
#329056=CARTESIAN_POINT('Ctrl Pts',(0.738288867999944,2.2,-4.07589744400001));
#329057=CARTESIAN_POINT('Ctrl Pts',(0.738404901999944,12.2,-4.07459437900001));
#329058=CARTESIAN_POINT('Ctrl Pts',(0.738404901999944,5.2,-4.07459437900001));
#329059=CARTESIAN_POINT('Ctrl Pts',(0.738404901999944,2.2,-4.07459437900001));
#329060=CARTESIAN_POINT('Ctrl Pts',(0.738518944999944,12.2,-4.07329615600001));
#329061=CARTESIAN_POINT('Ctrl Pts',(0.738518944999944,5.2,-4.07329615600001));
#329062=CARTESIAN_POINT('Ctrl Pts',(0.738518944999944,2.2,-4.07329615600001));
#329063=CARTESIAN_POINT('Ctrl Pts',(0.738631005999945,12.2,-4.07200278500001));
#329064=CARTESIAN_POINT('Ctrl Pts',(0.738631005999945,5.2,-4.07200278500001));
#329065=CARTESIAN_POINT('Ctrl Pts',(0.738631005999945,2.2,-4.07200278500001));
#329066=CARTESIAN_POINT('Ctrl Pts',(0.738741095999944,12.2,-4.07071427800001));
#329067=CARTESIAN_POINT('Ctrl Pts',(0.738741095999944,5.2,-4.07071427800001));
#329068=CARTESIAN_POINT('Ctrl Pts',(0.738741095999944,2.2,-4.07071427800001));
#329069=CARTESIAN_POINT('Ctrl Pts',(0.738849224999945,12.2,-4.06943064400001));
#329070=CARTESIAN_POINT('Ctrl Pts',(0.738849224999945,5.2,-4.06943064400001));
#329071=CARTESIAN_POINT('Ctrl Pts',(0.738849224999945,2.2,-4.06943064400001));
#329072=CARTESIAN_POINT('Ctrl Pts',(0.738955402999945,12.2,-4.06815189300001));
#329073=CARTESIAN_POINT('Ctrl Pts',(0.738955402999945,5.2,-4.06815189300001));
#329074=CARTESIAN_POINT('Ctrl Pts',(0.738955402999945,2.2,-4.06815189300001));
#329075=CARTESIAN_POINT('Ctrl Pts',(0.739059639999944,12.2,-4.06687803500001));
#329076=CARTESIAN_POINT('Ctrl Pts',(0.739059639999944,5.2,-4.06687803500001));
#329077=CARTESIAN_POINT('Ctrl Pts',(0.739059639999944,2.2,-4.06687803500001));
#329078=CARTESIAN_POINT('Ctrl Pts',(0.739161947999943,12.2,-4.06560908300001));
#329079=CARTESIAN_POINT('Ctrl Pts',(0.739161947999943,5.2,-4.06560908300001));
#329080=CARTESIAN_POINT('Ctrl Pts',(0.739161947999943,2.2,-4.06560908300001));
#329081=CARTESIAN_POINT('Ctrl Pts',(0.739262335999944,12.2,-4.06434504400002));
#329082=CARTESIAN_POINT('Ctrl Pts',(0.739262335999944,5.2,-4.06434504400002));
#329083=CARTESIAN_POINT('Ctrl Pts',(0.739262335999944,2.2,-4.06434504400002));
#329084=CARTESIAN_POINT('Ctrl Pts',(0.739360815999944,12.2,-4.06308593100002));
#329085=CARTESIAN_POINT('Ctrl Pts',(0.739360815999944,5.2,-4.06308593100002));
#329086=CARTESIAN_POINT('Ctrl Pts',(0.739360815999944,2.2,-4.06308593100002));
#329087=CARTESIAN_POINT('Ctrl Pts',(0.739457395999944,12.2,-4.06183175400002));
#329088=CARTESIAN_POINT('Ctrl Pts',(0.739457395999944,5.2,-4.06183175400002));
#329089=CARTESIAN_POINT('Ctrl Pts',(0.739457395999944,2.2,-4.06183175400002));
#329090=CARTESIAN_POINT('Ctrl Pts',(0.739552088999944,12.2,-4.06058252100001));
#329091=CARTESIAN_POINT('Ctrl Pts',(0.739552088999944,5.2,-4.06058252100001));
#329092=CARTESIAN_POINT('Ctrl Pts',(0.739552088999944,2.2,-4.06058252100001));
#329093=CARTESIAN_POINT('Ctrl Pts',(0.739644903999944,12.2,-4.05933824500002));
#329094=CARTESIAN_POINT('Ctrl Pts',(0.739644903999944,5.2,-4.05933824500002));
#329095=CARTESIAN_POINT('Ctrl Pts',(0.739644903999944,2.2,-4.05933824500002));
#329096=CARTESIAN_POINT('Ctrl Pts',(0.739735853999944,12.2,-4.05809893600001));
#329097=CARTESIAN_POINT('Ctrl Pts',(0.739735853999944,5.2,-4.05809893600001));
#329098=CARTESIAN_POINT('Ctrl Pts',(0.739735853999944,2.2,-4.05809893600001));
#329099=CARTESIAN_POINT('Ctrl Pts',(0.739824947999944,12.2,-4.05686460300001));
#329100=CARTESIAN_POINT('Ctrl Pts',(0.739824947999944,5.2,-4.05686460300001));
#329101=CARTESIAN_POINT('Ctrl Pts',(0.739824947999944,2.2,-4.05686460300001));
#329102=CARTESIAN_POINT('Ctrl Pts',(0.739912195999944,12.2,-4.05563525900002));
#329103=CARTESIAN_POINT('Ctrl Pts',(0.739912195999944,5.2,-4.05563525900002));
#329104=CARTESIAN_POINT('Ctrl Pts',(0.739912195999944,2.2,-4.05563525900002));
#329105=CARTESIAN_POINT('Ctrl Pts',(0.739997609999944,12.2,-4.05441091100001));
#329106=CARTESIAN_POINT('Ctrl Pts',(0.739997609999944,5.2,-4.05441091100001));
#329107=CARTESIAN_POINT('Ctrl Pts',(0.739997609999944,2.2,-4.05441091100001));
#329108=CARTESIAN_POINT('Ctrl Pts',(0.740081200999944,12.2,-4.05319157200001));
#329109=CARTESIAN_POINT('Ctrl Pts',(0.740081200999944,5.2,-4.05319157200001));
#329110=CARTESIAN_POINT('Ctrl Pts',(0.740081200999944,2.2,-4.05319157200001));
#329111=CARTESIAN_POINT('Ctrl Pts',(0.740162978999944,12.2,-4.05197725200001));
#329112=CARTESIAN_POINT('Ctrl Pts',(0.740162978999944,5.2,-4.05197725200001));
#329113=CARTESIAN_POINT('Ctrl Pts',(0.740162978999944,2.2,-4.05197725200001));
#329114=CARTESIAN_POINT('Ctrl Pts',(0.740242954999945,12.2,-4.05076796100001));
#329115=CARTESIAN_POINT('Ctrl Pts',(0.740242954999945,5.2,-4.05076796100001));
#329116=CARTESIAN_POINT('Ctrl Pts',(0.740242954999945,2.2,-4.05076796100001));
#329117=CARTESIAN_POINT('Ctrl Pts',(0.740321139999944,12.2,-4.04956371000001));
#329118=CARTESIAN_POINT('Ctrl Pts',(0.740321139999944,5.2,-4.04956371000001));
#329119=CARTESIAN_POINT('Ctrl Pts',(0.740321139999944,2.2,-4.04956371000001));
#329120=CARTESIAN_POINT('Ctrl Pts',(0.740397545999943,12.2,-4.04836450900001));
#329121=CARTESIAN_POINT('Ctrl Pts',(0.740397545999943,5.2,-4.04836450900001));
#329122=CARTESIAN_POINT('Ctrl Pts',(0.740397545999943,2.2,-4.04836450900001));
#329123=CARTESIAN_POINT('Ctrl Pts',(0.740472182999944,12.2,-4.04717036800001));
#329124=CARTESIAN_POINT('Ctrl Pts',(0.740472182999944,5.2,-4.04717036800001));
#329125=CARTESIAN_POINT('Ctrl Pts',(0.740472182999944,2.2,-4.04717036800001));
#329126=CARTESIAN_POINT('Ctrl Pts',(0.740545062999944,12.2,-4.04598130000001));
#329127=CARTESIAN_POINT('Ctrl Pts',(0.740545062999944,5.2,-4.04598130000001));
#329128=CARTESIAN_POINT('Ctrl Pts',(0.740545062999944,2.2,-4.04598130000001));
#329129=CARTESIAN_POINT('Ctrl Pts',(0.740616194999945,12.2,-4.04479731300002));
#329130=CARTESIAN_POINT('Ctrl Pts',(0.740616194999945,5.2,-4.04479731300002));
#329131=CARTESIAN_POINT('Ctrl Pts',(0.740616194999945,2.2,-4.04479731300002));
#329132=CARTESIAN_POINT('Ctrl Pts',(0.740685591999944,12.2,-4.04361841700001));
#329133=CARTESIAN_POINT('Ctrl Pts',(0.740685591999944,5.2,-4.04361841700001));
#329134=CARTESIAN_POINT('Ctrl Pts',(0.740685591999944,2.2,-4.04361841700001));
#329135=CARTESIAN_POINT('Ctrl Pts',(0.740753264999944,12.2,-4.04244462600001));
#329136=CARTESIAN_POINT('Ctrl Pts',(0.740753264999944,5.2,-4.04244462600001));
#329137=CARTESIAN_POINT('Ctrl Pts',(0.740753264999944,2.2,-4.04244462600001));
#329138=CARTESIAN_POINT('Ctrl Pts',(0.740819223999944,12.2,-4.04127594600002));
#329139=CARTESIAN_POINT('Ctrl Pts',(0.740819223999944,5.2,-4.04127594600002));
#329140=CARTESIAN_POINT('Ctrl Pts',(0.740819223999944,2.2,-4.04127594600002));
#329141=CARTESIAN_POINT('Ctrl Pts',(0.740883481999944,12.2,-4.04011239200001));
#329142=CARTESIAN_POINT('Ctrl Pts',(0.740883481999944,5.2,-4.04011239200001));
#329143=CARTESIAN_POINT('Ctrl Pts',(0.740883481999944,2.2,-4.04011239200001));
#329144=CARTESIAN_POINT('Ctrl Pts',(0.740946048999944,12.2,-4.03895397100001));
#329145=CARTESIAN_POINT('Ctrl Pts',(0.740946048999944,5.2,-4.03895397100001));
#329146=CARTESIAN_POINT('Ctrl Pts',(0.740946048999944,2.2,-4.03895397100001));
#329147=CARTESIAN_POINT('Ctrl Pts',(0.741006936999944,12.2,-4.03780069600002));
#329148=CARTESIAN_POINT('Ctrl Pts',(0.741006936999944,5.2,-4.03780069600002));
#329149=CARTESIAN_POINT('Ctrl Pts',(0.741006936999944,2.2,-4.03780069600002));
#329150=CARTESIAN_POINT('Ctrl Pts',(0.741066156999944,12.2,-4.03665257700002));
#329151=CARTESIAN_POINT('Ctrl Pts',(0.741066156999944,5.2,-4.03665257700002));
#329152=CARTESIAN_POINT('Ctrl Pts',(0.741066156999944,2.2,-4.03665257700002));
#329153=CARTESIAN_POINT('Ctrl Pts',(0.741123719999944,12.2,-4.03550962400002));
#329154=CARTESIAN_POINT('Ctrl Pts',(0.741123719999944,5.2,-4.03550962400002));
#329155=CARTESIAN_POINT('Ctrl Pts',(0.741123719999944,2.2,-4.03550962400002));
#329156=CARTESIAN_POINT('Ctrl Pts',(0.741179638999945,12.2,-4.03437184700001));
#329157=CARTESIAN_POINT('Ctrl Pts',(0.741179638999945,5.2,-4.03437184700001));
#329158=CARTESIAN_POINT('Ctrl Pts',(0.741179638999945,2.2,-4.03437184700001));
#329159=CARTESIAN_POINT('Ctrl Pts',(0.741233922999944,12.2,-4.03323925800001));
#329160=CARTESIAN_POINT('Ctrl Pts',(0.741233922999944,5.2,-4.03323925800001));
#329161=CARTESIAN_POINT('Ctrl Pts',(0.741233922999944,2.2,-4.03323925800001));
#329162=CARTESIAN_POINT('Ctrl Pts',(0.741286585999944,12.2,-4.03211186800001));
#329163=CARTESIAN_POINT('Ctrl Pts',(0.741286585999944,5.2,-4.03211186800001));
#329164=CARTESIAN_POINT('Ctrl Pts',(0.741286585999944,2.2,-4.03211186800001));
#329165=CARTESIAN_POINT('Ctrl Pts',(0.741337637999945,12.2,-4.03098968600001));
#329166=CARTESIAN_POINT('Ctrl Pts',(0.741337637999945,5.2,-4.03098968600001));
#329167=CARTESIAN_POINT('Ctrl Pts',(0.741337637999945,2.2,-4.03098968600001));
#329168=CARTESIAN_POINT('Ctrl Pts',(0.741387091999944,12.2,-4.02987272300001));
#329169=CARTESIAN_POINT('Ctrl Pts',(0.741387091999944,5.2,-4.02987272300001));
#329170=CARTESIAN_POINT('Ctrl Pts',(0.741387091999944,2.2,-4.02987272300001));
#329171=CARTESIAN_POINT('Ctrl Pts',(0.741434957999945,12.2,-4.02876099100002));
#329172=CARTESIAN_POINT('Ctrl Pts',(0.741434957999945,5.2,-4.02876099100002));
#329173=CARTESIAN_POINT('Ctrl Pts',(0.741434957999945,2.2,-4.02876099100002));
#329174=CARTESIAN_POINT('Ctrl Pts',(0.741481247999943,12.2,-4.02765449900001));
#329175=CARTESIAN_POINT('Ctrl Pts',(0.741481247999943,5.2,-4.02765449900001));
#329176=CARTESIAN_POINT('Ctrl Pts',(0.741481247999943,2.2,-4.02765449900001));
#329177=CARTESIAN_POINT('Ctrl Pts',(0.741525974999945,12.2,-4.02655326000001));
#329178=CARTESIAN_POINT('Ctrl Pts',(0.741525974999945,5.2,-4.02655326000001));
#329179=CARTESIAN_POINT('Ctrl Pts',(0.741525974999945,2.2,-4.02655326000001));
#329180=CARTESIAN_POINT('Ctrl Pts',(0.741569149999944,12.2,-4.02545728100002));
#329181=CARTESIAN_POINT('Ctrl Pts',(0.741569149999944,5.2,-4.02545728100002));
#329182=CARTESIAN_POINT('Ctrl Pts',(0.741569149999944,2.2,-4.02545728100002));
#329183=CARTESIAN_POINT('Ctrl Pts',(0.741610784999944,12.2,-4.02436657600001));
#329184=CARTESIAN_POINT('Ctrl Pts',(0.741610784999944,5.2,-4.02436657600001));
#329185=CARTESIAN_POINT('Ctrl Pts',(0.741610784999944,2.2,-4.02436657600001));
#329186=CARTESIAN_POINT('Ctrl Pts',(0.741650891999944,12.2,-4.02328115500001));
#329187=CARTESIAN_POINT('Ctrl Pts',(0.741650891999944,5.2,-4.02328115500001));
#329188=CARTESIAN_POINT('Ctrl Pts',(0.741650891999944,2.2,-4.02328115500001));
#329189=CARTESIAN_POINT('Ctrl Pts',(0.741689481999944,12.2,-4.02220102700001));
#329190=CARTESIAN_POINT('Ctrl Pts',(0.741689481999944,5.2,-4.02220102700001));
#329191=CARTESIAN_POINT('Ctrl Pts',(0.741689481999944,2.2,-4.02220102700001));
#329192=CARTESIAN_POINT('Ctrl Pts',(0.741726566999944,12.2,-4.02112620600001));
#329193=CARTESIAN_POINT('Ctrl Pts',(0.741726566999944,5.2,-4.02112620600001));
#329194=CARTESIAN_POINT('Ctrl Pts',(0.741726566999944,2.2,-4.02112620600001));
#329195=CARTESIAN_POINT('Ctrl Pts',(0.741762160999944,12.2,-4.02005670000001));
#329196=CARTESIAN_POINT('Ctrl Pts',(0.741762160999944,5.2,-4.02005670000001));
#329197=CARTESIAN_POINT('Ctrl Pts',(0.741762160999944,2.2,-4.02005670000001));
#329198=CARTESIAN_POINT('Ctrl Pts',(0.741796273999944,12.2,-4.01899252000002));
#329199=CARTESIAN_POINT('Ctrl Pts',(0.741796273999944,5.2,-4.01899252000002));
#329200=CARTESIAN_POINT('Ctrl Pts',(0.741796273999944,2.2,-4.01899252000002));
#329201=CARTESIAN_POINT('Ctrl Pts',(0.741828917999944,12.2,-4.01793367800002));
#329202=CARTESIAN_POINT('Ctrl Pts',(0.741828917999944,5.2,-4.01793367800002));
#329203=CARTESIAN_POINT('Ctrl Pts',(0.741828917999944,2.2,-4.01793367800002));
#329204=CARTESIAN_POINT('Ctrl Pts',(0.741860106999944,12.2,-4.01688018300002));
#329205=CARTESIAN_POINT('Ctrl Pts',(0.741860106999944,5.2,-4.01688018300002));
#329206=CARTESIAN_POINT('Ctrl Pts',(0.741860106999944,2.2,-4.01688018300002));
#329207=CARTESIAN_POINT('Ctrl Pts',(0.741889850999944,12.2,-4.01583204800001));
#329208=CARTESIAN_POINT('Ctrl Pts',(0.741889850999944,5.2,-4.01583204800001));
#329209=CARTESIAN_POINT('Ctrl Pts',(0.741889850999944,2.2,-4.01583204800001));
#329210=CARTESIAN_POINT('Ctrl Pts',(0.741918163999945,12.2,-4.01478928300001));
#329211=CARTESIAN_POINT('Ctrl Pts',(0.741918163999945,5.2,-4.01478928300001));
#329212=CARTESIAN_POINT('Ctrl Pts',(0.741918163999945,2.2,-4.01478928300001));
#329213=CARTESIAN_POINT('Ctrl Pts',(0.741945055999944,12.2,-4.01375189800001));
#329214=CARTESIAN_POINT('Ctrl Pts',(0.741945055999944,5.2,-4.01375189800001));
#329215=CARTESIAN_POINT('Ctrl Pts',(0.741945055999944,2.2,-4.01375189800001));
#329216=CARTESIAN_POINT('Ctrl Pts',(0.741970542999945,12.2,-4.01271990400001));
#329217=CARTESIAN_POINT('Ctrl Pts',(0.741970542999945,5.2,-4.01271990400001));
#329218=CARTESIAN_POINT('Ctrl Pts',(0.741970542999945,2.2,-4.01271990400001));
#329219=CARTESIAN_POINT('Ctrl Pts',(0.741994632999944,12.2,-4.01169331300002));
#329220=CARTESIAN_POINT('Ctrl Pts',(0.741994632999944,5.2,-4.01169331300002));
#329221=CARTESIAN_POINT('Ctrl Pts',(0.741994632999944,2.2,-4.01169331300002));
#329222=CARTESIAN_POINT('Ctrl Pts',(0.742017340999944,12.2,-4.01067213400002));
#329223=CARTESIAN_POINT('Ctrl Pts',(0.742017340999944,5.2,-4.01067213400002));
#329224=CARTESIAN_POINT('Ctrl Pts',(0.742017340999944,2.2,-4.01067213400002));
#329225=CARTESIAN_POINT('Ctrl Pts',(0.742038679999945,12.2,-4.00965638100002));
#329226=CARTESIAN_POINT('Ctrl Pts',(0.742038679999945,5.2,-4.00965638100002));
#329227=CARTESIAN_POINT('Ctrl Pts',(0.742038679999945,2.2,-4.00965638100002));
#329228=CARTESIAN_POINT('Ctrl Pts',(0.742058659999943,12.2,-4.00864606100001));
#329229=CARTESIAN_POINT('Ctrl Pts',(0.742058659999943,5.2,-4.00864606100001));
#329230=CARTESIAN_POINT('Ctrl Pts',(0.742058659999943,2.2,-4.00864606100001));
#329231=CARTESIAN_POINT('Ctrl Pts',(0.742077295999944,12.2,-4.00764118700002));
#329232=CARTESIAN_POINT('Ctrl Pts',(0.742077295999944,5.2,-4.00764118700002));
#329233=CARTESIAN_POINT('Ctrl Pts',(0.742077295999944,2.2,-4.00764118700002));
#329234=CARTESIAN_POINT('Ctrl Pts',(0.742094599999944,12.2,-4.00664177000001));
#329235=CARTESIAN_POINT('Ctrl Pts',(0.742094599999944,5.2,-4.00664177000001));
#329236=CARTESIAN_POINT('Ctrl Pts',(0.742094599999944,2.2,-4.00664177000001));
#329237=CARTESIAN_POINT('Ctrl Pts',(0.742110582999944,12.2,-4.00564782000002));
#329238=CARTESIAN_POINT('Ctrl Pts',(0.742110582999944,5.2,-4.00564782000002));
#329239=CARTESIAN_POINT('Ctrl Pts',(0.742110582999944,2.2,-4.00564782000002));
#329240=CARTESIAN_POINT('Ctrl Pts',(0.742125258999944,12.2,-4.00465934800001));
#329241=CARTESIAN_POINT('Ctrl Pts',(0.742125258999944,5.2,-4.00465934800001));
#329242=CARTESIAN_POINT('Ctrl Pts',(0.742125258999944,2.2,-4.00465934800001));
#329243=CARTESIAN_POINT('Ctrl Pts',(0.742138639999944,12.2,-4.00367636600001));
#329244=CARTESIAN_POINT('Ctrl Pts',(0.742138639999944,5.2,-4.00367636600001));
#329245=CARTESIAN_POINT('Ctrl Pts',(0.742138639999944,2.2,-4.00367636600001));
#329246=CARTESIAN_POINT('Ctrl Pts',(0.742150738999944,12.2,-4.00269888500001));
#329247=CARTESIAN_POINT('Ctrl Pts',(0.742150738999944,5.2,-4.00269888500001));
#329248=CARTESIAN_POINT('Ctrl Pts',(0.742150738999944,2.2,-4.00269888500001));
#329249=CARTESIAN_POINT('Ctrl Pts',(0.742161569999944,12.2,-4.00172691400002));
#329250=CARTESIAN_POINT('Ctrl Pts',(0.742161569999944,5.2,-4.00172691400002));
#329251=CARTESIAN_POINT('Ctrl Pts',(0.742161569999944,2.2,-4.00172691400002));
#329252=CARTESIAN_POINT('Ctrl Pts',(0.742171144999944,12.2,-4.00076046600002));
#329253=CARTESIAN_POINT('Ctrl Pts',(0.742171144999944,5.2,-4.00076046600002));
#329254=CARTESIAN_POINT('Ctrl Pts',(0.742171144999944,2.2,-4.00076046600002));
#329255=CARTESIAN_POINT('Ctrl Pts',(0.742179474999943,12.2,-3.99979955000001));
#329256=CARTESIAN_POINT('Ctrl Pts',(0.742179474999943,5.2,-3.99979955000001));
#329257=CARTESIAN_POINT('Ctrl Pts',(0.742179474999943,2.2,-3.99979955000001));
#329258=CARTESIAN_POINT('Ctrl Pts',(0.742186576999945,12.2,-3.99884418000001));
#329259=CARTESIAN_POINT('Ctrl Pts',(0.742186576999945,5.2,-3.99884418000001));
#329260=CARTESIAN_POINT('Ctrl Pts',(0.742186576999945,2.2,-3.99884418000001));
#329261=CARTESIAN_POINT('Ctrl Pts',(0.742192459999944,12.2,-3.99789436300001));
#329262=CARTESIAN_POINT('Ctrl Pts',(0.742192459999944,5.2,-3.99789436300001));
#329263=CARTESIAN_POINT('Ctrl Pts',(0.742192459999944,2.2,-3.99789436300001));
#329264=CARTESIAN_POINT('Ctrl Pts',(0.742197139999944,12.2,-3.99695011400001));
#329265=CARTESIAN_POINT('Ctrl Pts',(0.742197139999944,5.2,-3.99695011400001));
#329266=CARTESIAN_POINT('Ctrl Pts',(0.742197139999944,2.2,-3.99695011400001));
#329267=CARTESIAN_POINT('Ctrl Pts',(0.742200627999944,12.2,-3.99601144100002));
#329268=CARTESIAN_POINT('Ctrl Pts',(0.742200627999944,5.2,-3.99601144100002));
#329269=CARTESIAN_POINT('Ctrl Pts',(0.742200627999944,2.2,-3.99601144100002));
#329270=CARTESIAN_POINT('Ctrl Pts',(0.742202937999944,12.2,-3.99507835700001));
#329271=CARTESIAN_POINT('Ctrl Pts',(0.742202937999944,5.2,-3.99507835700001));
#329272=CARTESIAN_POINT('Ctrl Pts',(0.742202937999944,2.2,-3.99507835700001));
#329273=CARTESIAN_POINT('Ctrl Pts',(0.742204082999944,12.2,-3.99415087100001));
#329274=CARTESIAN_POINT('Ctrl Pts',(0.742204082999944,5.2,-3.99415087100001));
#329275=CARTESIAN_POINT('Ctrl Pts',(0.742204082999944,2.2,-3.99415087100001));
#329276=CARTESIAN_POINT('Ctrl Pts',(0.742204076999945,12.2,-3.99322899600001));
#329277=CARTESIAN_POINT('Ctrl Pts',(0.742204076999945,5.2,-3.99322899600001));
#329278=CARTESIAN_POINT('Ctrl Pts',(0.742204076999945,2.2,-3.99322899600001));
#329279=CARTESIAN_POINT('Ctrl Pts',(0.742202931999943,12.2,-3.99231274300002));
#329280=CARTESIAN_POINT('Ctrl Pts',(0.742202931999943,5.2,-3.99231274300002));
#329281=CARTESIAN_POINT('Ctrl Pts',(0.742202931999943,2.2,-3.99231274300002));
#329282=CARTESIAN_POINT('Ctrl Pts',(0.742200661999944,12.2,-3.99140212200002));
#329283=CARTESIAN_POINT('Ctrl Pts',(0.742200661999944,5.2,-3.99140212200002));
#329284=CARTESIAN_POINT('Ctrl Pts',(0.742200661999944,2.2,-3.99140212200002));
#329285=CARTESIAN_POINT('Ctrl Pts',(0.742197279999944,12.2,-3.99049714400002));
#329286=CARTESIAN_POINT('Ctrl Pts',(0.742197279999944,5.2,-3.99049714400002));
#329287=CARTESIAN_POINT('Ctrl Pts',(0.742197279999944,2.2,-3.99049714400002));
#329288=CARTESIAN_POINT('Ctrl Pts',(0.742192799999944,12.2,-3.98959782100002));
#329289=CARTESIAN_POINT('Ctrl Pts',(0.742192799999944,5.2,-3.98959782100002));
#329290=CARTESIAN_POINT('Ctrl Pts',(0.742192799999944,2.2,-3.98959782100002));
#329291=CARTESIAN_POINT('Ctrl Pts',(0.742187234999945,12.2,-3.98870416500001));
#329292=CARTESIAN_POINT('Ctrl Pts',(0.742187234999945,5.2,-3.98870416500001));
#329293=CARTESIAN_POINT('Ctrl Pts',(0.742187234999945,2.2,-3.98870416500001));
#329294=CARTESIAN_POINT('Ctrl Pts',(0.742180598999944,12.2,-3.98781618500001));
#329295=CARTESIAN_POINT('Ctrl Pts',(0.742180598999944,5.2,-3.98781618500001));
#329296=CARTESIAN_POINT('Ctrl Pts',(0.742180598999944,2.2,-3.98781618500001));
#329297=CARTESIAN_POINT('Ctrl Pts',(0.742172904999945,12.2,-3.98693389300002));
#329298=CARTESIAN_POINT('Ctrl Pts',(0.742172904999945,5.2,-3.98693389300002));
#329299=CARTESIAN_POINT('Ctrl Pts',(0.742172904999945,2.2,-3.98693389300002));
#329300=CARTESIAN_POINT('Ctrl Pts',(0.742164167999944,12.2,-3.98605730100002));
#329301=CARTESIAN_POINT('Ctrl Pts',(0.742164167999944,5.2,-3.98605730100002));
#329302=CARTESIAN_POINT('Ctrl Pts',(0.742164167999944,2.2,-3.98605730100002));
#329303=CARTESIAN_POINT('Ctrl Pts',(0.742154399999944,12.2,-3.98518641800001));
#329304=CARTESIAN_POINT('Ctrl Pts',(0.742154399999944,5.2,-3.98518641800001));
#329305=CARTESIAN_POINT('Ctrl Pts',(0.742154399999944,2.2,-3.98518641800001));
#329306=CARTESIAN_POINT('Ctrl Pts',(0.742143613999944,12.2,-3.98432125700001));
#329307=CARTESIAN_POINT('Ctrl Pts',(0.742143613999944,5.2,-3.98432125700001));
#329308=CARTESIAN_POINT('Ctrl Pts',(0.742143613999944,2.2,-3.98432125700001));
#329309=CARTESIAN_POINT('Ctrl Pts',(0.742131825999944,12.2,-3.98346182900001));
#329310=CARTESIAN_POINT('Ctrl Pts',(0.742131825999944,5.2,-3.98346182900001));
#329311=CARTESIAN_POINT('Ctrl Pts',(0.742131825999944,2.2,-3.98346182900001));
#329312=CARTESIAN_POINT('Ctrl Pts',(0.742119048999944,12.2,-3.98260814600001));
#329313=CARTESIAN_POINT('Ctrl Pts',(0.742119048999944,5.2,-3.98260814600001));
#329314=CARTESIAN_POINT('Ctrl Pts',(0.742119048999944,2.2,-3.98260814600001));
#329315=CARTESIAN_POINT('Ctrl Pts',(0.742105296999944,12.2,-3.98176021700001));
#329316=CARTESIAN_POINT('Ctrl Pts',(0.742105296999944,5.2,-3.98176021700001));
#329317=CARTESIAN_POINT('Ctrl Pts',(0.742105296999944,2.2,-3.98176021700001));
#329318=CARTESIAN_POINT('Ctrl Pts',(0.742090582999944,12.2,-3.98091805500002));
#329319=CARTESIAN_POINT('Ctrl Pts',(0.742090582999944,5.2,-3.98091805500002));
#329320=CARTESIAN_POINT('Ctrl Pts',(0.742090582999944,2.2,-3.98091805500002));
#329321=CARTESIAN_POINT('Ctrl Pts',(0.742074920999943,12.2,-3.98008167000001));
#329322=CARTESIAN_POINT('Ctrl Pts',(0.742074920999943,5.2,-3.98008167000001));
#329323=CARTESIAN_POINT('Ctrl Pts',(0.742074920999943,2.2,-3.98008167000001));
#329324=CARTESIAN_POINT('Ctrl Pts',(0.742058326999944,12.2,-3.97925107500001));
#329325=CARTESIAN_POINT('Ctrl Pts',(0.742058326999944,5.2,-3.97925107500001));
#329326=CARTESIAN_POINT('Ctrl Pts',(0.742058326999944,2.2,-3.97925107500001));
#329327=CARTESIAN_POINT('Ctrl Pts',(0.742040812999945,12.2,-3.97842628000001));
#329328=CARTESIAN_POINT('Ctrl Pts',(0.742040812999945,5.2,-3.97842628000001));
#329329=CARTESIAN_POINT('Ctrl Pts',(0.742040812999945,2.2,-3.97842628000001));
#329330=CARTESIAN_POINT('Ctrl Pts',(0.742022392999945,12.2,-3.97760729600002));
#329331=CARTESIAN_POINT('Ctrl Pts',(0.742022392999945,5.2,-3.97760729600002));
#329332=CARTESIAN_POINT('Ctrl Pts',(0.742022392999945,2.2,-3.97760729600002));
#329333=CARTESIAN_POINT('Ctrl Pts',(0.742003082999945,12.2,-3.97679413600001));
#329334=CARTESIAN_POINT('Ctrl Pts',(0.742003082999945,5.2,-3.97679413600001));
#329335=CARTESIAN_POINT('Ctrl Pts',(0.742003082999945,2.2,-3.97679413600001));
#329336=CARTESIAN_POINT('Ctrl Pts',(0.741982896999944,12.2,-3.97598680900002));
#329337=CARTESIAN_POINT('Ctrl Pts',(0.741982896999944,5.2,-3.97598680900002));
#329338=CARTESIAN_POINT('Ctrl Pts',(0.741982896999944,2.2,-3.97598680900002));
#329339=CARTESIAN_POINT('Ctrl Pts',(0.741961847999945,12.2,-3.97518532700001));
#329340=CARTESIAN_POINT('Ctrl Pts',(0.741961847999945,5.2,-3.97518532700001));
#329341=CARTESIAN_POINT('Ctrl Pts',(0.741961847999945,2.2,-3.97518532700001));
#329342=CARTESIAN_POINT('Ctrl Pts',(0.741939950999945,12.2,-3.97438970300001));
#329343=CARTESIAN_POINT('Ctrl Pts',(0.741939950999945,5.2,-3.97438970300001));
#329344=CARTESIAN_POINT('Ctrl Pts',(0.741939950999945,2.2,-3.97438970300001));
#329345=CARTESIAN_POINT('Ctrl Pts',(0.741917219999944,12.2,-3.97359994600002));
#329346=CARTESIAN_POINT('Ctrl Pts',(0.741917219999944,5.2,-3.97359994600002));
#329347=CARTESIAN_POINT('Ctrl Pts',(0.741917219999944,2.2,-3.97359994600002));
#329348=CARTESIAN_POINT('Ctrl Pts',(0.741893669999943,12.2,-3.97281606900002));
#329349=CARTESIAN_POINT('Ctrl Pts',(0.741893669999943,5.2,-3.97281606900002));
#329350=CARTESIAN_POINT('Ctrl Pts',(0.741893669999943,2.2,-3.97281606900002));
#329351=CARTESIAN_POINT('Ctrl Pts',(0.741869314999944,12.2,-3.97203808400001));
#329352=CARTESIAN_POINT('Ctrl Pts',(0.741869314999944,5.2,-3.97203808400001));
#329353=CARTESIAN_POINT('Ctrl Pts',(0.741869314999944,2.2,-3.97203808400001));
#329354=CARTESIAN_POINT('Ctrl Pts',(0.741844169999945,12.2,-3.97126600100002));
#329355=CARTESIAN_POINT('Ctrl Pts',(0.741844169999945,5.2,-3.97126600100002));
#329356=CARTESIAN_POINT('Ctrl Pts',(0.741844169999945,2.2,-3.97126600100002));
#329357=CARTESIAN_POINT('Ctrl Pts',(0.741818249999944,12.2,-3.97049983000001));
#329358=CARTESIAN_POINT('Ctrl Pts',(0.741818249999944,5.2,-3.97049983000001));
#329359=CARTESIAN_POINT('Ctrl Pts',(0.741818249999944,2.2,-3.97049983000001));
#329360=CARTESIAN_POINT('Ctrl Pts',(0.741791566999944,12.2,-3.96973958600002));
#329361=CARTESIAN_POINT('Ctrl Pts',(0.741791566999944,5.2,-3.96973958600002));
#329362=CARTESIAN_POINT('Ctrl Pts',(0.741791566999944,2.2,-3.96973958600002));
#329363=CARTESIAN_POINT('Ctrl Pts',(0.741764139999944,12.2,-3.96898527800001));
#329364=CARTESIAN_POINT('Ctrl Pts',(0.741764139999944,5.2,-3.96898527800001));
#329365=CARTESIAN_POINT('Ctrl Pts',(0.741764139999944,2.2,-3.96898527800001));
#329366=CARTESIAN_POINT('Ctrl Pts',(0.741735980999944,12.2,-3.96823691800002));
#329367=CARTESIAN_POINT('Ctrl Pts',(0.741735980999944,5.2,-3.96823691800002));
#329368=CARTESIAN_POINT('Ctrl Pts',(0.741735980999944,2.2,-3.96823691800002));
#329369=CARTESIAN_POINT('Ctrl Pts',(0.741707104999944,12.2,-3.96749451800002));
#329370=CARTESIAN_POINT('Ctrl Pts',(0.741707104999944,5.2,-3.96749451800002));
#329371=CARTESIAN_POINT('Ctrl Pts',(0.741707104999944,2.2,-3.96749451800002));
#329372=CARTESIAN_POINT('Ctrl Pts',(0.741677527999944,12.2,-3.96675808800001));
#329373=CARTESIAN_POINT('Ctrl Pts',(0.741677527999944,5.2,-3.96675808800001));
#329374=CARTESIAN_POINT('Ctrl Pts',(0.741677527999944,2.2,-3.96675808800001));
#329375=CARTESIAN_POINT('Ctrl Pts',(0.741647263999944,12.2,-3.96602764100002));
#329376=CARTESIAN_POINT('Ctrl Pts',(0.741647263999944,5.2,-3.96602764100002));
#329377=CARTESIAN_POINT('Ctrl Pts',(0.741647263999944,2.2,-3.96602764100002));
#329378=CARTESIAN_POINT('Ctrl Pts',(0.741616327999944,12.2,-3.96530318800002));
#329379=CARTESIAN_POINT('Ctrl Pts',(0.741616327999944,5.2,-3.96530318800002));
#329380=CARTESIAN_POINT('Ctrl Pts',(0.741616327999944,2.2,-3.96530318800002));
#329381=CARTESIAN_POINT('Ctrl Pts',(0.741584735999944,12.2,-3.96458474000001));
#329382=CARTESIAN_POINT('Ctrl Pts',(0.741584735999944,5.2,-3.96458474000001));
#329383=CARTESIAN_POINT('Ctrl Pts',(0.741584735999944,2.2,-3.96458474000001));
#329384=CARTESIAN_POINT('Ctrl Pts',(0.741552500999945,12.2,-3.96387230900002));
#329385=CARTESIAN_POINT('Ctrl Pts',(0.741552500999945,5.2,-3.96387230900002));
#329386=CARTESIAN_POINT('Ctrl Pts',(0.741552500999945,2.2,-3.96387230900002));
#329387=CARTESIAN_POINT('Ctrl Pts',(0.741519640999945,12.2,-3.96316590700001));
#329388=CARTESIAN_POINT('Ctrl Pts',(0.741519640999945,5.2,-3.96316590700001));
#329389=CARTESIAN_POINT('Ctrl Pts',(0.741519640999945,2.2,-3.96316590700001));
#329390=CARTESIAN_POINT('Ctrl Pts',(0.741486168999944,12.2,-3.96246554600001));
#329391=CARTESIAN_POINT('Ctrl Pts',(0.741486168999944,5.2,-3.96246554600001));
#329392=CARTESIAN_POINT('Ctrl Pts',(0.741486168999944,2.2,-3.96246554600001));
#329393=CARTESIAN_POINT('Ctrl Pts',(0.741452101999944,12.2,-3.96177123600001));
#329394=CARTESIAN_POINT('Ctrl Pts',(0.741452101999944,5.2,-3.96177123600001));
#329395=CARTESIAN_POINT('Ctrl Pts',(0.741452101999944,2.2,-3.96177123600001));
#329396=CARTESIAN_POINT('Ctrl Pts',(0.741417452999944,12.2,-3.96108298900002));
#329397=CARTESIAN_POINT('Ctrl Pts',(0.741417452999944,5.2,-3.96108298900002));
#329398=CARTESIAN_POINT('Ctrl Pts',(0.741417452999944,2.2,-3.96108298900002));
#329399=CARTESIAN_POINT('Ctrl Pts',(0.741382239999945,12.2,-3.96040081700002));
#329400=CARTESIAN_POINT('Ctrl Pts',(0.741382239999945,5.2,-3.96040081700002));
#329401=CARTESIAN_POINT('Ctrl Pts',(0.741382239999945,2.2,-3.96040081700002));
#329402=CARTESIAN_POINT('Ctrl Pts',(0.741346476999943,12.2,-3.95972473100001));
#329403=CARTESIAN_POINT('Ctrl Pts',(0.741346476999943,5.2,-3.95972473100001));
#329404=CARTESIAN_POINT('Ctrl Pts',(0.741346476999943,2.2,-3.95972473100001));
#329405=CARTESIAN_POINT('Ctrl Pts',(0.741310179999944,12.2,-3.95905474400001));
#329406=CARTESIAN_POINT('Ctrl Pts',(0.741310179999944,5.2,-3.95905474400001));
#329407=CARTESIAN_POINT('Ctrl Pts',(0.741310179999944,2.2,-3.95905474400001));
#329408=CARTESIAN_POINT('Ctrl Pts',(0.741273364999944,12.2,-3.95839086700001));
#329409=CARTESIAN_POINT('Ctrl Pts',(0.741273364999944,5.2,-3.95839086700001));
#329410=CARTESIAN_POINT('Ctrl Pts',(0.741273364999944,2.2,-3.95839086700001));
#329411=CARTESIAN_POINT('Ctrl Pts',(0.741236044999944,12.2,-3.95773311200001));
#329412=CARTESIAN_POINT('Ctrl Pts',(0.741236044999944,5.2,-3.95773311200001));
#329413=CARTESIAN_POINT('Ctrl Pts',(0.741236044999944,2.2,-3.95773311200001));
#329414=CARTESIAN_POINT('Ctrl Pts',(0.741198239999944,12.2,-3.95708148800002));
#329415=CARTESIAN_POINT('Ctrl Pts',(0.741198239999944,5.2,-3.95708148800002));
#329416=CARTESIAN_POINT('Ctrl Pts',(0.741198239999944,2.2,-3.95708148800002));
#329417=CARTESIAN_POINT('Ctrl Pts',(0.741159961999944,12.2,-3.95643601100002));
#329418=CARTESIAN_POINT('Ctrl Pts',(0.741159961999944,5.2,-3.95643601100002));
#329419=CARTESIAN_POINT('Ctrl Pts',(0.741159961999944,2.2,-3.95643601100002));
#329420=CARTESIAN_POINT('Ctrl Pts',(0.741121229999945,12.2,-3.95579668900002));
#329421=CARTESIAN_POINT('Ctrl Pts',(0.741121229999945,5.2,-3.95579668900002));
#329422=CARTESIAN_POINT('Ctrl Pts',(0.741121229999945,2.2,-3.95579668900002));
#329423=CARTESIAN_POINT('Ctrl Pts',(0.741082055999944,12.2,-3.95516353700001));
#329424=CARTESIAN_POINT('Ctrl Pts',(0.741082055999944,5.2,-3.95516353700001));
#329425=CARTESIAN_POINT('Ctrl Pts',(0.741082055999944,2.2,-3.95516353700001));
#329426=CARTESIAN_POINT('Ctrl Pts',(0.741042459999944,12.2,-3.95453656400001));
#329427=CARTESIAN_POINT('Ctrl Pts',(0.741042459999944,5.2,-3.95453656400001));
#329428=CARTESIAN_POINT('Ctrl Pts',(0.741042459999944,2.2,-3.95453656400001));
#329429=CARTESIAN_POINT('Ctrl Pts',(0.741002455999944,12.2,-3.95391578400002));
#329430=CARTESIAN_POINT('Ctrl Pts',(0.741002455999944,5.2,-3.95391578400002));
#329431=CARTESIAN_POINT('Ctrl Pts',(0.741002455999944,2.2,-3.95391578400002));
#329432=CARTESIAN_POINT('Ctrl Pts',(0.740962058999944,12.2,-3.95330120700002));
#329433=CARTESIAN_POINT('Ctrl Pts',(0.740962058999944,5.2,-3.95330120700002));
#329434=CARTESIAN_POINT('Ctrl Pts',(0.740962058999944,2.2,-3.95330120700002));
#329435=CARTESIAN_POINT('Ctrl Pts',(0.740921286999944,12.2,-3.95269284500001));
#329436=CARTESIAN_POINT('Ctrl Pts',(0.740921286999944,5.2,-3.95269284500001));
#329437=CARTESIAN_POINT('Ctrl Pts',(0.740921286999944,2.2,-3.95269284500001));
#329438=CARTESIAN_POINT('Ctrl Pts',(0.740880156999945,12.2,-3.95209071000002));
#329439=CARTESIAN_POINT('Ctrl Pts',(0.740880156999945,5.2,-3.95209071000002));
#329440=CARTESIAN_POINT('Ctrl Pts',(0.740880156999945,2.2,-3.95209071000002));
#329441=CARTESIAN_POINT('Ctrl Pts',(0.740838681999944,12.2,-3.95149481500002));
#329442=CARTESIAN_POINT('Ctrl Pts',(0.740838681999944,5.2,-3.95149481500002));
#329443=CARTESIAN_POINT('Ctrl Pts',(0.740838681999944,2.2,-3.95149481500002));
#329444=CARTESIAN_POINT('Ctrl Pts',(0.740796879999944,12.2,-3.95090517000002));
#329445=CARTESIAN_POINT('Ctrl Pts',(0.740796879999944,5.2,-3.95090517000002));
#329446=CARTESIAN_POINT('Ctrl Pts',(0.740796879999944,2.2,-3.95090517000002));
#329447=CARTESIAN_POINT('Ctrl Pts',(0.740754768999944,12.2,-3.95032178800002));
#329448=CARTESIAN_POINT('Ctrl Pts',(0.740754768999944,5.2,-3.95032178800002));
#329449=CARTESIAN_POINT('Ctrl Pts',(0.740754768999944,2.2,-3.95032178800002));
#329450=CARTESIAN_POINT('Ctrl Pts',(0.740712361999945,12.2,-3.94974468100001));
#329451=CARTESIAN_POINT('Ctrl Pts',(0.740712361999945,5.2,-3.94974468100001));
#329452=CARTESIAN_POINT('Ctrl Pts',(0.740712361999945,2.2,-3.94974468100001));
#329453=CARTESIAN_POINT('Ctrl Pts',(0.740669678999945,12.2,-3.94917386000001));
#329454=CARTESIAN_POINT('Ctrl Pts',(0.740669678999945,5.2,-3.94917386000001));
#329455=CARTESIAN_POINT('Ctrl Pts',(0.740669678999945,2.2,-3.94917386000001));
#329456=CARTESIAN_POINT('Ctrl Pts',(0.740626733999944,12.2,-3.94860933800001));
#329457=CARTESIAN_POINT('Ctrl Pts',(0.740626733999944,5.2,-3.94860933800001));
#329458=CARTESIAN_POINT('Ctrl Pts',(0.740626733999944,2.2,-3.94860933800001));
#329459=CARTESIAN_POINT('Ctrl Pts',(0.740583544999944,12.2,-3.94805112600002));
#329460=CARTESIAN_POINT('Ctrl Pts',(0.740583544999944,5.2,-3.94805112600002));
#329461=CARTESIAN_POINT('Ctrl Pts',(0.740583544999944,2.2,-3.94805112600002));
#329462=CARTESIAN_POINT('Ctrl Pts',(0.740540128999945,12.2,-3.94749923600001));
#329463=CARTESIAN_POINT('Ctrl Pts',(0.740540128999945,5.2,-3.94749923600001));
#329464=CARTESIAN_POINT('Ctrl Pts',(0.740540128999945,2.2,-3.94749923600001));
#329465=CARTESIAN_POINT('Ctrl Pts',(0.740496500999944,12.2,-3.94695368100002));
#329466=CARTESIAN_POINT('Ctrl Pts',(0.740496500999944,5.2,-3.94695368100002));
#329467=CARTESIAN_POINT('Ctrl Pts',(0.740496500999944,2.2,-3.94695368100002));
#329468=CARTESIAN_POINT('Ctrl Pts',(0.740452678999944,12.2,-3.94641447100001));
#329469=CARTESIAN_POINT('Ctrl Pts',(0.740452678999944,5.2,-3.94641447100001));
#329470=CARTESIAN_POINT('Ctrl Pts',(0.740452678999944,2.2,-3.94641447100001));
#329471=CARTESIAN_POINT('Ctrl Pts',(0.740408679999944,12.2,-3.94588162100002));
#329472=CARTESIAN_POINT('Ctrl Pts',(0.740408679999944,5.2,-3.94588162100002));
#329473=CARTESIAN_POINT('Ctrl Pts',(0.740408679999944,2.2,-3.94588162100002));
#329474=CARTESIAN_POINT('Ctrl Pts',(0.740364520999944,12.2,-3.94535513900002));
#329475=CARTESIAN_POINT('Ctrl Pts',(0.740364520999944,5.2,-3.94535513900002));
#329476=CARTESIAN_POINT('Ctrl Pts',(0.740364520999944,2.2,-3.94535513900002));
#329477=CARTESIAN_POINT('Ctrl Pts',(0.740320218999945,12.2,-3.94483504100001));
#329478=CARTESIAN_POINT('Ctrl Pts',(0.740320218999945,5.2,-3.94483504100001));
#329479=CARTESIAN_POINT('Ctrl Pts',(0.740320218999945,2.2,-3.94483504100001));
#329480=CARTESIAN_POINT('Ctrl Pts',(0.740275790999945,12.2,-3.94432133700001));
#329481=CARTESIAN_POINT('Ctrl Pts',(0.740275790999945,5.2,-3.94432133700001));
#329482=CARTESIAN_POINT('Ctrl Pts',(0.740275790999945,2.2,-3.94432133700001));
#329483=CARTESIAN_POINT('Ctrl Pts',(0.740231253999944,12.2,-3.94381403900002));
#329484=CARTESIAN_POINT('Ctrl Pts',(0.740231253999944,5.2,-3.94381403900002));
#329485=CARTESIAN_POINT('Ctrl Pts',(0.740231253999944,2.2,-3.94381403900002));
#329486=CARTESIAN_POINT('Ctrl Pts',(0.740186624999944,12.2,-3.94331315900001));
#329487=CARTESIAN_POINT('Ctrl Pts',(0.740186624999944,5.2,-3.94331315900001));
#329488=CARTESIAN_POINT('Ctrl Pts',(0.740186624999944,2.2,-3.94331315900001));
#329489=CARTESIAN_POINT('Ctrl Pts',(0.740141921999945,12.2,-3.94281871000001));
#329490=CARTESIAN_POINT('Ctrl Pts',(0.740141921999945,5.2,-3.94281871000001));
#329491=CARTESIAN_POINT('Ctrl Pts',(0.740141921999945,2.2,-3.94281871000001));
#329492=CARTESIAN_POINT('Ctrl Pts',(0.740097160999944,12.2,-3.94233070300002));
#329493=CARTESIAN_POINT('Ctrl Pts',(0.740097160999944,5.2,-3.94233070300002));
#329494=CARTESIAN_POINT('Ctrl Pts',(0.740097160999944,2.2,-3.94233070300002));
#329495=CARTESIAN_POINT('Ctrl Pts',(0.740052360999944,12.2,-3.94184915200002));
#329496=CARTESIAN_POINT('Ctrl Pts',(0.740052360999944,5.2,-3.94184915200002));
#329497=CARTESIAN_POINT('Ctrl Pts',(0.740052360999944,2.2,-3.94184915200002));
#329498=CARTESIAN_POINT('Ctrl Pts',(0.740007537999944,12.2,-3.94137406700001));
#329499=CARTESIAN_POINT('Ctrl Pts',(0.740007537999944,5.2,-3.94137406700001));
#329500=CARTESIAN_POINT('Ctrl Pts',(0.740007537999944,2.2,-3.94137406700001));
#329501=CARTESIAN_POINT('Ctrl Pts',(0.739962711999944,12.2,-3.94090546000001));
#329502=CARTESIAN_POINT('Ctrl Pts',(0.739962711999944,5.2,-3.94090546000001));
#329503=CARTESIAN_POINT('Ctrl Pts',(0.739962711999944,2.2,-3.94090546000001));
#329504=CARTESIAN_POINT('Ctrl Pts',(0.739917897999944,12.2,-3.94044334500002));
#329505=CARTESIAN_POINT('Ctrl Pts',(0.739917897999944,5.2,-3.94044334500002));
#329506=CARTESIAN_POINT('Ctrl Pts',(0.739917897999944,2.2,-3.94044334500002));
#329507=CARTESIAN_POINT('Ctrl Pts',(0.739873114999944,12.2,-3.93998773400002));
#329508=CARTESIAN_POINT('Ctrl Pts',(0.739873114999944,5.2,-3.93998773400002));
#329509=CARTESIAN_POINT('Ctrl Pts',(0.739873114999944,2.2,-3.93998773400002));
#329510=CARTESIAN_POINT('Ctrl Pts',(0.739828380999944,12.2,-3.93953863800002));
#329511=CARTESIAN_POINT('Ctrl Pts',(0.739828380999944,5.2,-3.93953863800002));
#329512=CARTESIAN_POINT('Ctrl Pts',(0.739828380999944,2.2,-3.93953863800002));
#329513=CARTESIAN_POINT('Ctrl Pts',(0.739783712999944,12.2,-3.93909607000001));
#329514=CARTESIAN_POINT('Ctrl Pts',(0.739783712999944,5.2,-3.93909607000001));
#329515=CARTESIAN_POINT('Ctrl Pts',(0.739783712999944,2.2,-3.93909607000001));
#329516=CARTESIAN_POINT('Ctrl Pts',(0.739739128999944,12.2,-3.93866004200001));
#329517=CARTESIAN_POINT('Ctrl Pts',(0.739739128999944,5.2,-3.93866004200001));
#329518=CARTESIAN_POINT('Ctrl Pts',(0.739739128999944,2.2,-3.93866004200001));
#329519=CARTESIAN_POINT('Ctrl Pts',(0.739694648999943,12.2,-3.93823056700001));
#329520=CARTESIAN_POINT('Ctrl Pts',(0.739694648999943,5.2,-3.93823056700001));
#329521=CARTESIAN_POINT('Ctrl Pts',(0.739694648999943,2.2,-3.93823056700001));
#329522=CARTESIAN_POINT('Ctrl Pts',(0.739650287999944,12.2,-3.93780765600001));
#329523=CARTESIAN_POINT('Ctrl Pts',(0.739650287999944,5.2,-3.93780765600001));
#329524=CARTESIAN_POINT('Ctrl Pts',(0.739650287999944,2.2,-3.93780765600001));
#329525=CARTESIAN_POINT('Ctrl Pts',(0.739606065999945,12.2,-3.93739132200002));
#329526=CARTESIAN_POINT('Ctrl Pts',(0.739606065999945,5.2,-3.93739132200002));
#329527=CARTESIAN_POINT('Ctrl Pts',(0.739606065999945,2.2,-3.93739132200002));
#329528=CARTESIAN_POINT('Ctrl Pts',(0.739562000999944,12.2,-3.93698157800001));
#329529=CARTESIAN_POINT('Ctrl Pts',(0.739562000999944,5.2,-3.93698157800001));
#329530=CARTESIAN_POINT('Ctrl Pts',(0.739562000999944,2.2,-3.93698157800001));
#329531=CARTESIAN_POINT('Ctrl Pts',(0.739518110999944,12.2,-3.93657843600002));
#329532=CARTESIAN_POINT('Ctrl Pts',(0.739518110999944,5.2,-3.93657843600002));
#329533=CARTESIAN_POINT('Ctrl Pts',(0.739518110999944,2.2,-3.93657843600002));
#329534=CARTESIAN_POINT('Ctrl Pts',(0.739474413999944,12.2,-3.93618190600002));
#329535=CARTESIAN_POINT('Ctrl Pts',(0.739474413999944,5.2,-3.93618190600002));
#329536=CARTESIAN_POINT('Ctrl Pts',(0.739474413999944,2.2,-3.93618190600002));
#329537=CARTESIAN_POINT('Ctrl Pts',(0.739430928999945,12.2,-3.93579200400001));
#329538=CARTESIAN_POINT('Ctrl Pts',(0.739430928999945,5.2,-3.93579200400001));
#329539=CARTESIAN_POINT('Ctrl Pts',(0.739430928999945,2.2,-3.93579200400001));
#329540=CARTESIAN_POINT('Ctrl Pts',(0.739387674999944,12.2,-3.93540874100001));
#329541=CARTESIAN_POINT('Ctrl Pts',(0.739387674999944,5.2,-3.93540874100001));
#329542=CARTESIAN_POINT('Ctrl Pts',(0.739387674999944,2.2,-3.93540874100001));
#329543=CARTESIAN_POINT('Ctrl Pts',(0.739344668999945,12.2,-3.93503212900002));
#329544=CARTESIAN_POINT('Ctrl Pts',(0.739344668999945,5.2,-3.93503212900002));
#329545=CARTESIAN_POINT('Ctrl Pts',(0.739344668999945,2.2,-3.93503212900002));
#329546=CARTESIAN_POINT('Ctrl Pts',(0.739301930999944,12.2,-3.93466218000002));
#329547=CARTESIAN_POINT('Ctrl Pts',(0.739301930999944,5.2,-3.93466218000002));
#329548=CARTESIAN_POINT('Ctrl Pts',(0.739301930999944,2.2,-3.93466218000002));
#329549=CARTESIAN_POINT('Ctrl Pts',(0.739259478999944,12.2,-3.93429890800002));
#329550=CARTESIAN_POINT('Ctrl Pts',(0.739259478999944,5.2,-3.93429890800002));
#329551=CARTESIAN_POINT('Ctrl Pts',(0.739259478999944,2.2,-3.93429890800002));
#329552=CARTESIAN_POINT('Ctrl Pts',(0.739217332999944,12.2,-3.93394232400002));
#329553=CARTESIAN_POINT('Ctrl Pts',(0.739217332999944,5.2,-3.93394232400002));
#329554=CARTESIAN_POINT('Ctrl Pts',(0.739217332999944,2.2,-3.93394232400002));
#329555=CARTESIAN_POINT('Ctrl Pts',(0.739175509999944,12.2,-3.93359244200001));
#329556=CARTESIAN_POINT('Ctrl Pts',(0.739175509999944,5.2,-3.93359244200001));
#329557=CARTESIAN_POINT('Ctrl Pts',(0.739175509999944,2.2,-3.93359244200001));
#329558=CARTESIAN_POINT('Ctrl Pts',(0.739134030999944,12.2,-3.93324927300001));
#329559=CARTESIAN_POINT('Ctrl Pts',(0.739134030999944,5.2,-3.93324927300001));
#329560=CARTESIAN_POINT('Ctrl Pts',(0.739134030999944,2.2,-3.93324927300001));
#329561=CARTESIAN_POINT('Ctrl Pts',(0.739092914999944,12.2,-3.93291283000002));
#329562=CARTESIAN_POINT('Ctrl Pts',(0.739092914999944,5.2,-3.93291283000002));
#329563=CARTESIAN_POINT('Ctrl Pts',(0.739092914999944,2.2,-3.93291283000002));
#329564=CARTESIAN_POINT('Ctrl Pts',(0.739052177999944,12.2,-3.93258312600001));
#329565=CARTESIAN_POINT('Ctrl Pts',(0.739052177999944,5.2,-3.93258312600001));
#329566=CARTESIAN_POINT('Ctrl Pts',(0.739052177999944,2.2,-3.93258312600001));
#329567=CARTESIAN_POINT('Ctrl Pts',(0.739011842999945,12.2,-3.93226017400002));
#329568=CARTESIAN_POINT('Ctrl Pts',(0.739011842999945,5.2,-3.93226017400002));
#329569=CARTESIAN_POINT('Ctrl Pts',(0.739011842999945,2.2,-3.93226017400002));
#329570=CARTESIAN_POINT('Ctrl Pts',(0.738971926999944,12.2,-3.93194398500002));
#329571=CARTESIAN_POINT('Ctrl Pts',(0.738971926999944,5.2,-3.93194398500002));
#329572=CARTESIAN_POINT('Ctrl Pts',(0.738971926999944,2.2,-3.93194398500002));
#329573=CARTESIAN_POINT('Ctrl Pts',(0.738932449999944,12.2,-3.93163457300002));
#329574=CARTESIAN_POINT('Ctrl Pts',(0.738932449999944,5.2,-3.93163457300002));
#329575=CARTESIAN_POINT('Ctrl Pts',(0.738932449999944,2.2,-3.93163457300002));
#329576=CARTESIAN_POINT('Ctrl Pts',(0.738893430999944,12.2,-3.93133195000001));
#329577=CARTESIAN_POINT('Ctrl Pts',(0.738893430999944,5.2,-3.93133195000001));
#329578=CARTESIAN_POINT('Ctrl Pts',(0.738893430999944,2.2,-3.93133195000001));
#329579=CARTESIAN_POINT('Ctrl Pts',(0.738854890999944,12.2,-3.93103612900001));
#329580=CARTESIAN_POINT('Ctrl Pts',(0.738854890999944,5.2,-3.93103612900001));
#329581=CARTESIAN_POINT('Ctrl Pts',(0.738854890999944,2.2,-3.93103612900001));
#329582=CARTESIAN_POINT('Ctrl Pts',(0.738816847999945,12.2,-3.93074712400002));
#329583=CARTESIAN_POINT('Ctrl Pts',(0.738816847999945,5.2,-3.93074712400002));
#329584=CARTESIAN_POINT('Ctrl Pts',(0.738816847999945,2.2,-3.93074712400002));
#329585=CARTESIAN_POINT('Ctrl Pts',(0.738779321999944,12.2,-3.93046494500001));
#329586=CARTESIAN_POINT('Ctrl Pts',(0.738779321999944,5.2,-3.93046494500001));
#329587=CARTESIAN_POINT('Ctrl Pts',(0.738779321999944,2.2,-3.93046494500001));
#329588=CARTESIAN_POINT('Ctrl Pts',(0.738742333999944,12.2,-3.93018960500001));
#329589=CARTESIAN_POINT('Ctrl Pts',(0.738742333999944,5.2,-3.93018960500001));
#329590=CARTESIAN_POINT('Ctrl Pts',(0.738742333999944,2.2,-3.93018960500001));
#329591=CARTESIAN_POINT('Ctrl Pts',(0.738705901999944,12.2,-3.92992111900002));
#329592=CARTESIAN_POINT('Ctrl Pts',(0.738705901999944,5.2,-3.92992111900002));
#329593=CARTESIAN_POINT('Ctrl Pts',(0.738705901999944,2.2,-3.92992111900002));
#329594=CARTESIAN_POINT('Ctrl Pts',(0.738670047999944,12.2,-3.92965949900002));
#329595=CARTESIAN_POINT('Ctrl Pts',(0.738670047999944,5.2,-3.92965949900002));
#329596=CARTESIAN_POINT('Ctrl Pts',(0.738670047999944,2.2,-3.92965949900002));
#329597=CARTESIAN_POINT('Ctrl Pts',(0.738634788999945,12.2,-3.92940475700001));
#329598=CARTESIAN_POINT('Ctrl Pts',(0.738634788999945,5.2,-3.92940475700001));
#329599=CARTESIAN_POINT('Ctrl Pts',(0.738634788999945,2.2,-3.92940475700001));
#329600=CARTESIAN_POINT('Ctrl Pts',(0.738600147999944,12.2,-3.92915690600002));
#329601=CARTESIAN_POINT('Ctrl Pts',(0.738600147999944,5.2,-3.92915690600002));
#329602=CARTESIAN_POINT('Ctrl Pts',(0.738600147999944,2.2,-3.92915690600002));
#329603=CARTESIAN_POINT('Ctrl Pts',(0.738566144999945,12.2,-3.92891595800001));
#329604=CARTESIAN_POINT('Ctrl Pts',(0.738566144999945,5.2,-3.92891595800001));
#329605=CARTESIAN_POINT('Ctrl Pts',(0.738566144999945,2.2,-3.92891595800001));
#329606=CARTESIAN_POINT('Ctrl Pts',(0.738532797999943,12.2,-3.92868192900002));
#329607=CARTESIAN_POINT('Ctrl Pts',(0.738532797999943,5.2,-3.92868192900002));
#329608=CARTESIAN_POINT('Ctrl Pts',(0.738532797999943,2.2,-3.92868192900002));
#329609=CARTESIAN_POINT('Ctrl Pts',(0.738500128999945,12.2,-3.92845482900002));
#329610=CARTESIAN_POINT('Ctrl Pts',(0.738500128999945,5.2,-3.92845482900002));
#329611=CARTESIAN_POINT('Ctrl Pts',(0.738500128999945,2.2,-3.92845482900002));
#329612=CARTESIAN_POINT('Ctrl Pts',(0.738468156999944,12.2,-3.92823467100001));
#329613=CARTESIAN_POINT('Ctrl Pts',(0.738468156999944,5.2,-3.92823467100001));
#329614=CARTESIAN_POINT('Ctrl Pts',(0.738468156999944,2.2,-3.92823467100001));
#329615=CARTESIAN_POINT('Ctrl Pts',(0.738436904999944,12.2,-3.92802146900001));
#329616=CARTESIAN_POINT('Ctrl Pts',(0.738436904999944,5.2,-3.92802146900001));
#329617=CARTESIAN_POINT('Ctrl Pts',(0.738436904999944,2.2,-3.92802146900001));
#329618=CARTESIAN_POINT('Ctrl Pts',(0.738406391999944,12.2,-3.92781523500001));
#329619=CARTESIAN_POINT('Ctrl Pts',(0.738406391999944,5.2,-3.92781523500001));
#329620=CARTESIAN_POINT('Ctrl Pts',(0.738406391999944,2.2,-3.92781523500001));
#329621=CARTESIAN_POINT('Ctrl Pts',(0.738376637999945,12.2,-3.92761598300002));
#329622=CARTESIAN_POINT('Ctrl Pts',(0.738376637999945,5.2,-3.92761598300002));
#329623=CARTESIAN_POINT('Ctrl Pts',(0.738376637999945,2.2,-3.92761598300002));
#329624=CARTESIAN_POINT('Ctrl Pts',(0.738347665999944,12.2,-3.92742372600001));
#329625=CARTESIAN_POINT('Ctrl Pts',(0.738347665999944,5.2,-3.92742372600001));
#329626=CARTESIAN_POINT('Ctrl Pts',(0.738347665999944,2.2,-3.92742372600001));
#329627=CARTESIAN_POINT('Ctrl Pts',(0.738319495999944,12.2,-3.92723847700001));
#329628=CARTESIAN_POINT('Ctrl Pts',(0.738319495999944,5.2,-3.92723847700001));
#329629=CARTESIAN_POINT('Ctrl Pts',(0.738319495999944,2.2,-3.92723847700001));
#329630=CARTESIAN_POINT('Ctrl Pts',(0.738292148999945,12.2,-3.92706024900002));
#329631=CARTESIAN_POINT('Ctrl Pts',(0.738292148999945,5.2,-3.92706024900002));
#329632=CARTESIAN_POINT('Ctrl Pts',(0.738292148999945,2.2,-3.92706024900002));
#329633=CARTESIAN_POINT('Ctrl Pts',(0.738265644999945,12.2,-3.92688905300002));
#329634=CARTESIAN_POINT('Ctrl Pts',(0.738265644999945,5.2,-3.92688905300002));
#329635=CARTESIAN_POINT('Ctrl Pts',(0.738265644999945,2.2,-3.92688905300002));
#329636=CARTESIAN_POINT('Ctrl Pts',(0.738240003999944,12.2,-3.92672490400002));
#329637=CARTESIAN_POINT('Ctrl Pts',(0.738240003999944,5.2,-3.92672490400002));
#329638=CARTESIAN_POINT('Ctrl Pts',(0.738240003999944,2.2,-3.92672490400002));
#329639=CARTESIAN_POINT('Ctrl Pts',(0.738215248999944,12.2,-3.92656781500001));
#329640=CARTESIAN_POINT('Ctrl Pts',(0.738215248999944,5.2,-3.92656781500001));
#329641=CARTESIAN_POINT('Ctrl Pts',(0.738215248999944,2.2,-3.92656781500001));
#329642=CARTESIAN_POINT('Ctrl Pts',(0.738191399999945,12.2,-3.92641779800002));
#329643=CARTESIAN_POINT('Ctrl Pts',(0.738191399999945,5.2,-3.92641779800002));
#329644=CARTESIAN_POINT('Ctrl Pts',(0.738191399999945,2.2,-3.92641779800002));
#329645=CARTESIAN_POINT('Ctrl Pts',(0.738168480999944,12.2,-3.92627486800002));
#329646=CARTESIAN_POINT('Ctrl Pts',(0.738168480999944,5.2,-3.92627486800002));
#329647=CARTESIAN_POINT('Ctrl Pts',(0.738168480999944,2.2,-3.92627486800002));
#329648=CARTESIAN_POINT('Ctrl Pts',(0.738146512999944,12.2,-3.92613903800001));
#329649=CARTESIAN_POINT('Ctrl Pts',(0.738146512999944,5.2,-3.92613903800001));
#329650=CARTESIAN_POINT('Ctrl Pts',(0.738146512999944,2.2,-3.92613903800001));
#329651=CARTESIAN_POINT('Ctrl Pts',(0.738125519999944,12.2,-3.92601032300002));
#329652=CARTESIAN_POINT('Ctrl Pts',(0.738125519999944,5.2,-3.92601032300002));
#329653=CARTESIAN_POINT('Ctrl Pts',(0.738125519999944,2.2,-3.92601032300002));
#329654=CARTESIAN_POINT('Ctrl Pts',(0.738105520999944,12.2,-3.92588873400001));
#329655=CARTESIAN_POINT('Ctrl Pts',(0.738105520999944,5.2,-3.92588873400001));
#329656=CARTESIAN_POINT('Ctrl Pts',(0.738105520999944,2.2,-3.92588873400001));
#329657=CARTESIAN_POINT('Ctrl Pts',(0.738086536999945,12.2,-3.92577428400001));
#329658=CARTESIAN_POINT('Ctrl Pts',(0.738086536999945,5.2,-3.92577428400001));
#329659=CARTESIAN_POINT('Ctrl Pts',(0.738086536999945,2.2,-3.92577428400001));
#329660=CARTESIAN_POINT('Ctrl Pts',(0.738068587999944,12.2,-3.92566698400001));
#329661=CARTESIAN_POINT('Ctrl Pts',(0.738068587999944,5.2,-3.92566698400001));
#329662=CARTESIAN_POINT('Ctrl Pts',(0.738068587999944,2.2,-3.92566698400001));
#329663=CARTESIAN_POINT('Ctrl Pts',(0.738051691999945,12.2,-3.92556684800001));
#329664=CARTESIAN_POINT('Ctrl Pts',(0.738051691999945,5.2,-3.92556684800001));
#329665=CARTESIAN_POINT('Ctrl Pts',(0.738051691999945,2.2,-3.92556684800001));
#329666=CARTESIAN_POINT('Ctrl Pts',(0.738035872999945,12.2,-3.92547388800002));
#329667=CARTESIAN_POINT('Ctrl Pts',(0.738035872999945,5.2,-3.92547388800002));
#329668=CARTESIAN_POINT('Ctrl Pts',(0.738035872999945,2.2,-3.92547388800002));
#329669=CARTESIAN_POINT('Ctrl Pts',(0.738021155999945,12.2,-3.92538811900002));
#329670=CARTESIAN_POINT('Ctrl Pts',(0.738021155999945,5.2,-3.92538811900002));
#329671=CARTESIAN_POINT('Ctrl Pts',(0.738021155999945,2.2,-3.92538811900002));
#329672=CARTESIAN_POINT('Ctrl Pts',(0.738007569999944,12.2,-3.92530956000002));
#329673=CARTESIAN_POINT('Ctrl Pts',(0.738007569999944,5.2,-3.92530956000002));
#329674=CARTESIAN_POINT('Ctrl Pts',(0.738007569999944,2.2,-3.92530956000002));
#329675=CARTESIAN_POINT('Ctrl Pts',(0.737995141999944,12.2,-3.92523822500001));
#329676=CARTESIAN_POINT('Ctrl Pts',(0.737995141999944,5.2,-3.92523822500001));
#329677=CARTESIAN_POINT('Ctrl Pts',(0.737995141999944,2.2,-3.92523822500001));
#329678=CARTESIAN_POINT('Ctrl Pts',(0.737983896999944,12.2,-3.92517413200002));
#329679=CARTESIAN_POINT('Ctrl Pts',(0.737983896999944,5.2,-3.92517413200002));
#329680=CARTESIAN_POINT('Ctrl Pts',(0.737983896999944,2.2,-3.92517413200002));
#329681=CARTESIAN_POINT('Ctrl Pts',(0.737973852999944,12.2,-3.92511728900002));
#329682=CARTESIAN_POINT('Ctrl Pts',(0.737973852999944,5.2,-3.92511728900002));
#329683=CARTESIAN_POINT('Ctrl Pts',(0.737973852999944,2.2,-3.92511728900002));
#329684=CARTESIAN_POINT('Ctrl Pts',(0.737964075508447,12.2,-3.92506239688743));
#329685=CARTESIAN_POINT('Ctrl Pts',(0.737964075508447,5.2,-3.92506239688743));
#329686=CARTESIAN_POINT('Ctrl Pts',(0.737964075508447,2.2,-3.92506239688743));
#329687=CARTESIAN_POINT('Ctrl Pts',(0.737957318588985,12.2,-3.92502488824354));
#329688=CARTESIAN_POINT('Ctrl Pts',(0.737957318588985,5.2,-3.92502488824354));
#329689=CARTESIAN_POINT('Ctrl Pts',(0.737957318588985,2.2,-3.92502488824354));
#329690=CARTESIAN_POINT('Ctrl Pts',(0.737952809879958,12.2,-3.92500018886681));
#329691=CARTESIAN_POINT('Ctrl Pts',(0.737952809879958,5.2,-3.92500018886681));
#329692=CARTESIAN_POINT('Ctrl Pts',(0.737952809879958,2.2,-3.92500018886681));
#329693=CARTESIAN_POINT('Ctrl Pts',(0.737949974070314,12.2,-3.9249848052472));
#329694=CARTESIAN_POINT('Ctrl Pts',(0.737949974070314,5.2,-3.9249848052472));
#329695=CARTESIAN_POINT('Ctrl Pts',(0.737949974070314,2.2,-3.9249848052472));
#329696=CARTESIAN_POINT('Ctrl Pts',(0.737948220999944,12.2,-3.92497531000001));
#329697=CARTESIAN_POINT('Ctrl Pts',(0.737948220999944,5.2,-3.92497531000001));
#329698=CARTESIAN_POINT('Ctrl Pts',(0.737948220999944,2.2,-3.92497531000001));
#329699=CARTESIAN_POINT('',(0.737948419999944,2.7,-3.92497527300002));
#329700=CARTESIAN_POINT('',(0.737948419999944,12.2,-3.92497527300002));
#329701=CARTESIAN_POINT('Ctrl Pts',(0.540411127999944,2.7,-4.71915838000001));
#329702=CARTESIAN_POINT('Ctrl Pts',(0.665652104973256,2.7,-4.46512891742156));
#329703=CARTESIAN_POINT('Ctrl Pts',(0.707703770492112,2.70000000000005,
-4.27722825213315));
#329704=CARTESIAN_POINT('Ctrl Pts',(0.751313867273993,2.70000000000005,
-4.02314857199238));
#329705=CARTESIAN_POINT('Ctrl Pts',(0.740087973051188,2.70000000000455,
-3.93748559824036));
#329706=CARTESIAN_POINT('Ctrl Pts',(0.738030284168778,2.70000000000455,
-3.92544135994311));
#329707=CARTESIAN_POINT('Ctrl Pts',(0.737990568056458,2.7,-3.92520467658791));
#329708=CARTESIAN_POINT('Ctrl Pts',(0.737948220999944,2.7,-3.92497531000001));
#329709=CARTESIAN_POINT('Origin',(0.737938937999945,15.2,-3.92492484000002));
#329710=CARTESIAN_POINT('',(0.669813182999944,2.7,-3.56257986500002));
#329711=CARTESIAN_POINT('',(0.669813182999944,2.2,-3.56257986500002));
#329712=CARTESIAN_POINT('',(0.368969468486324,2.7,-1.96246242009659));
#329713=CARTESIAN_POINT('Origin',(-5.66300478732629E-14,2.7,-1.7702336056717E-14));
#329714=CARTESIAN_POINT('',(1.21174314999994,2.7,-3.41647530900001));
#329715=CARTESIAN_POINT('Origin',(-5.66300478732629E-14,2.7,-1.92943768261394E-14));
#329716=CARTESIAN_POINT('',(1.33499927399995,2.7,-3.76399243800002));
#329717=CARTESIAN_POINT('',(-5.68808302581349E-14,2.7,-1.85873030340881E-14));
#329718=CARTESIAN_POINT('',(1.90498031899994,2.7,-4.35126992700001));
#329719=CARTESIAN_POINT('Ctrl Pts',(1.33499940099994,2.7,-3.76399239200001));
#329720=CARTESIAN_POINT('Ctrl Pts',(1.33505318590947,2.7,-3.76414216657697));
#329721=CARTESIAN_POINT('Ctrl Pts',(1.33510842838262,2.70000000000379,-3.76429141658972));
#329722=CARTESIAN_POINT('Ctrl Pts',(1.3352798572439,2.70000000000379,-3.76475137816303));
#329723=CARTESIAN_POINT('Ctrl Pts',(1.33540406083887,2.70000000000408,-3.76507710840355));
#329724=CARTESIAN_POINT('Ctrl Pts',(1.33593626418945,2.70000000000408,-3.76645590419181));
#329725=CARTESIAN_POINT('Ctrl Pts',(1.3363951343922,2.70000000000408,-3.76759527567173));
#329726=CARTESIAN_POINT('Ctrl Pts',(1.33845293758698,2.70000000000408,-3.77258387700579));
#329727=CARTESIAN_POINT('Ctrl Pts',(1.34029389818348,2.70000000000408,-3.77670788059791));
#329728=CARTESIAN_POINT('Ctrl Pts',(1.34867811834044,2.70000000000408,-3.79469813505244));
#329729=CARTESIAN_POINT('Ctrl Pts',(1.35653894621658,2.70000000000408,-3.80937791673359));
#329730=CARTESIAN_POINT('Ctrl Pts',(1.38680573533928,2.70000000000408,-3.86188878113129));
#329731=CARTESIAN_POINT('Ctrl Pts',(1.41908990349611,2.7,-3.90970550382703));
#329732=CARTESIAN_POINT('Ctrl Pts',(1.55514657451191,2.7,-4.07573224600064));
#329733=CARTESIAN_POINT('Ctrl Pts',(1.69711667034069,2.7,-4.21327383678026));
#329734=CARTESIAN_POINT('Ctrl Pts',(1.90498031899994,2.7,-4.35126992800001));
#329735=CARTESIAN_POINT('',(2.20867500599994,2.7,-4.20526511800002));
#329736=CARTESIAN_POINT('Origin',(-5.66300478732629E-14,2.7,-1.92943768261394E-14));
#329737=CARTESIAN_POINT('',(2.10598101599994,2.7,-3.39335272700002));
#329738=CARTESIAN_POINT('Ctrl Pts',(2.20867500599994,2.7,-4.20526511900002));
#329739=CARTESIAN_POINT('Ctrl Pts',(2.23054550490679,2.7,-3.95864099641364));
#329740=CARTESIAN_POINT('Ctrl Pts',(2.21200258882908,2.7,-3.76641859286599));
#329741=CARTESIAN_POINT('Ctrl Pts',(2.15359897116276,2.7,-3.47945049981984));
#329742=CARTESIAN_POINT('Ctrl Pts',(2.11239855701061,2.7,-3.40405190689996));
#329743=CARTESIAN_POINT('Ctrl Pts',(2.10612617646059,2.7,-3.39359173223168));
#329744=CARTESIAN_POINT('Ctrl Pts',(2.10605412404705,2.7,-3.39347190592633));
#329745=CARTESIAN_POINT('Ctrl Pts',(2.10598084399995,2.7,-3.39335283300001));
#329746=CARTESIAN_POINT('',(1.91153447899994,2.7,-3.08004235900002));
#329747=CARTESIAN_POINT('',(1.05297697809741,2.7,-1.69665456162922));
#329748=CARTESIAN_POINT('',(2.36409006999994,2.7,-2.74803623300001));
#329749=CARTESIAN_POINT('Origin',(-5.66300478732629E-14,2.7,-1.92943768261394E-14));
#329750=CARTESIAN_POINT('',(2.60456064899994,2.7,-3.02756105800002));
#329751=CARTESIAN_POINT('',(-5.70235930926259E-14,2.7,-1.88369168773884E-14));
#329752=CARTESIAN_POINT('',(3.34820124399994,2.7,-3.36928010500001));
#329753=CARTESIAN_POINT('Ctrl Pts',(2.60456075099994,2.7,-3.02756096900001));
#329754=CARTESIAN_POINT('Ctrl Pts',(2.60466500709798,2.7,-3.02768120188421));
#329755=CARTESIAN_POINT('Ctrl Pts',(2.6047704354198,2.69999999999987,-3.02780041686978));
#329756=CARTESIAN_POINT('Ctrl Pts',(2.60509625096573,2.69999999999987,-3.02816717075809));
#329757=CARTESIAN_POINT('Ctrl Pts',(2.60532946277246,2.7,-3.02842574326169));
#329758=CARTESIAN_POINT('Ctrl Pts',(2.60632500711197,2.7,-3.02952050165491));
#329759=CARTESIAN_POINT('Ctrl Pts',(2.60716450668402,2.7,-3.03041715663214));
#329760=CARTESIAN_POINT('Ctrl Pts',(2.61088625784452,2.7,-3.03432639867292));
#329761=CARTESIAN_POINT('Ctrl Pts',(2.61409560992509,2.7,-3.03750956461736));
#329762=CARTESIAN_POINT('Ctrl Pts',(2.62840201211911,2.7,-3.05124616104321));
#329763=CARTESIAN_POINT('Ctrl Pts',(2.64103233645551,2.7,-3.0620938237245));
#329764=CARTESIAN_POINT('Ctrl Pts',(2.68823087033611,2.7,-3.10013029786383));
#329765=CARTESIAN_POINT('Ctrl Pts',(2.73560912439619,2.7,-3.13305665019956));
#329766=CARTESIAN_POINT('Ctrl Pts',(2.9319957262991,2.7,-3.24411877831512));
#329767=CARTESIAN_POINT('Ctrl Pts',(3.11606392248859,2.7,-3.3182297564467));
#329768=CARTESIAN_POINT('Ctrl Pts',(3.34820124399994,2.7,-3.36928010500001));
#329769=CARTESIAN_POINT('',(3.57864508499994,2.7,-3.12342750100001));
#329770=CARTESIAN_POINT('Origin',(-5.66300478732629E-14,2.7,-1.92943768261394E-14));
#329771=CARTESIAN_POINT('',(3.18958920499994,2.7,-2.40343909200002));
#329772=CARTESIAN_POINT('Ctrl Pts',(3.57864508499994,2.7,-3.12342750100001));
#329773=CARTESIAN_POINT('Ctrl Pts',(3.51005252440388,2.7,-2.88591939399924));
#329774=CARTESIAN_POINT('Ctrl Pts',(3.42511647090323,2.69999999999088,-2.71873794461971));
#329775=CARTESIAN_POINT('Ctrl Pts',(3.27332372189986,2.69999999999088,-2.4763086239477));
#329776=CARTESIAN_POINT('Ctrl Pts',(3.20549137962071,2.69999999999088,-2.41612390951146));
#329777=CARTESIAN_POINT('Ctrl Pts',(3.19023885271594,2.69999999999088,-2.40394068962246));
#329778=CARTESIAN_POINT('Ctrl Pts',(3.18967095409694,2.7,-2.40350137821559));
#329779=CARTESIAN_POINT('Ctrl Pts',(3.18958908308186,2.7,-2.40343925206217));
#329780=CARTESIAN_POINT('',(2.89509244999994,2.7,-2.18152806500001));
#329781=CARTESIAN_POINT('',(1.59477411092506,2.7,-1.20170410393585));
#329782=CARTESIAN_POINT('',(3.19715352599995,2.7,-1.70845963700002));
#329783=CARTESIAN_POINT('Origin',(-5.66300478732629E-14,2.7,-1.92943768261394E-14));
#329784=CARTESIAN_POINT('',(3.52236167599994,2.7,-1.88224078000002));
#329785=CARTESIAN_POINT('',(-5.69609323413902E-14,2.7,-1.91175624338592E-14));
#329786=CARTESIAN_POINT('',(4.33922903699994,2.7,-1.93225033600002));
#329787=CARTESIAN_POINT('Ctrl Pts',(3.52236173899994,2.7,-1.88224066100001));
#329788=CARTESIAN_POINT('Ctrl Pts',(3.52250239789438,2.7,-1.88231509464184));
#329789=CARTESIAN_POINT('Ctrl Pts',(3.52264376260884,2.69999999999987,-1.88238819257901));
#329790=CARTESIAN_POINT('Ctrl Pts',(3.52307936983357,2.69999999999987,-1.88261212568366));
#329791=CARTESIAN_POINT('Ctrl Pts',(3.52338953221521,2.7,-1.88276864836628));
#329792=CARTESIAN_POINT('Ctrl Pts',(3.524715395624,2.7,-1.88343088035005));
#329793=CARTESIAN_POINT('Ctrl Pts',(3.52582171235091,2.7,-1.88396352252172));
#329794=CARTESIAN_POINT('Ctrl Pts',(3.53070391512716,2.7,-1.88626411944967));
#329795=CARTESIAN_POINT('Ctrl Pts',(3.53484594800583,2.7,-1.88807280192899));
#329796=CARTESIAN_POINT('Ctrl Pts',(3.55314920490717,2.7,-1.89571400990757));
#329797=CARTESIAN_POINT('Ctrl Pts',(3.56885036242802,2.7,-1.90126819174153));
#329798=CARTESIAN_POINT('Ctrl Pts',(3.62652324888264,2.7,-1.91966091085629));
#329799=CARTESIAN_POINT('Ctrl Pts',(3.68259524212757,2.7,-1.93326135998433));
#329800=CARTESIAN_POINT('Ctrl Pts',(3.88845402391619,2.7,-1.96334031610243));
#329801=CARTESIAN_POINT('Ctrl Pts',(4.0855706716694,2.7,-1.97139908700959));
#329802=CARTESIAN_POINT('Ctrl Pts',(4.33922903699994,2.7,-1.93225033600001));
#329803=CARTESIAN_POINT('',(4.46529931499995,2.7,-1.61975369200002));
#329804=CARTESIAN_POINT('Origin',(-5.66300478732629E-14,2.7,-1.92943768261394E-14));
#329805=CARTESIAN_POINT('',(3.84242569899994,2.7,-1.08892768900002));
#329806=CARTESIAN_POINT('Ctrl Pts',(4.46529931499995,2.7,-1.61975369200002));
#329807=CARTESIAN_POINT('Ctrl Pts',(4.29358758119907,2.7,-1.39422941109806));
#329808=CARTESIAN_POINT('Ctrl Pts',(4.14405887002337,2.69999999999094,-1.27286083842864));
#329809=CARTESIAN_POINT('Ctrl Pts',(3.93634800541175,2.69999999999094,-1.12078426790825));
#329810=CARTESIAN_POINT('Ctrl Pts',(3.85463885449721,2.69999999999544,-1.09260715575166));
#329811=CARTESIAN_POINT('Ctrl Pts',(3.84274996213715,2.69999999999544,-1.08902313452261));
#329812=CARTESIAN_POINT('Ctrl Pts',(3.84258808458359,2.7,-1.08897453261456));
#329813=CARTESIAN_POINT('Ctrl Pts',(3.84242564299994,2.7,-1.08892788300002));
#329814=CARTESIAN_POINT('',(3.48765214499994,2.7,-0.988386318000014));
#329815=CARTESIAN_POINT('',(1.92118816307637,2.7,-0.544456849994655));
#329816=CARTESIAN_POINT('',(3.59842368199994,2.7,-0.438146099000015));
#329817=CARTESIAN_POINT('Origin',(-5.66300478732629E-14,2.7,-1.92943768261394E-14));
#329818=CARTESIAN_POINT('',(3.96444824099994,2.7,-0.482713455000018));
#329819=CARTESIAN_POINT('',(-5.67255557987442E-14,2.7,-1.92827477272514E-14));
#329820=CARTESIAN_POINT('',(4.74421990499994,2.7,-0.234259451000015));
#329821=CARTESIAN_POINT('Ctrl Pts',(3.96444825599994,2.7,-0.482713322000015));
#329822=CARTESIAN_POINT('Ctrl Pts',(3.96497547528596,2.7,-0.482775452743841));
#329823=CARTESIAN_POINT('Ctrl Pts',(3.96655962681762,2.70000000000098,-0.482946807487822));
#329824=CARTESIAN_POINT('Ctrl Pts',(3.9736780106965,2.70000000000098,-0.483451374626115));
#329825=CARTESIAN_POINT('Ctrl Pts',(3.97819360075364,2.7,-0.483641747904727));
#329826=CARTESIAN_POINT('Ctrl Pts',(3.99802246284191,2.7,-0.484155087954969));
#329827=CARTESIAN_POINT('Ctrl Pts',(4.01466717880949,2.7,-0.483662565437282));
#329828=CARTESIAN_POINT('Ctrl Pts',(4.07519067554633,2.7,-0.479973318483465));
#329829=CARTESIAN_POINT('Ctrl Pts',(4.13240045706223,2.7,-0.472381001980205));
#329830=CARTESIAN_POINT('Ctrl Pts',(4.32840548403216,2.7,-0.427621068241287));
#329831=CARTESIAN_POINT('Ctrl Pts',(4.51557914880521,2.7,-0.365999725911413));
#329832=CARTESIAN_POINT('Ctrl Pts',(4.74421990499994,2.7,-0.234259451000014));
#329833=CARTESIAN_POINT('',(4.74889012999994,2.7,0.102676828999985));
#329834=CARTESIAN_POINT('Origin',(-5.66300478732629E-14,2.7,-1.92943768261394E-14));
#329835=CARTESIAN_POINT('',(3.97632130999995,2.7,0.372649431999984));
#329836=CARTESIAN_POINT('Ctrl Pts',(4.74889012999994,2.7,0.102676827999986));
#329837=CARTESIAN_POINT('Ctrl Pts',(4.53436175012147,2.7,0.234337488975898));
#329838=CARTESIAN_POINT('Ctrl Pts',(4.35470102702024,2.70000000000136,0.301734470466299));
#329839=CARTESIAN_POINT('Ctrl Pts',(4.07614478832924,2.70000000000136,0.376824070144407));
#329840=CARTESIAN_POINT('Ctrl Pts',(3.9893662305862,2.70000000000136,0.373641676368157));
#329841=CARTESIAN_POINT('Ctrl Pts',(3.97670805493192,2.70000000000136,0.372681581585382));
#329842=CARTESIAN_POINT('Ctrl Pts',(3.9765145886927,2.7,0.37266656994227));
#329843=CARTESIAN_POINT('Ctrl Pts',(3.97632132799994,2.7,0.372649231999986));
#329844=CARTESIAN_POINT('',(3.60918509199994,2.7,0.338242477999984));
#329845=CARTESIAN_POINT('',(1.98813510850398,2.7,0.186322321956948));
#329846=CARTESIAN_POINT('',(3.51370677999994,2.7,0.891341496999986));
#329847=CARTESIAN_POINT('Origin',(-5.66300478732629E-14,2.7,-1.92943768261394E-14));
#329848=CARTESIAN_POINT('',(3.87111410199994,2.7,0.982006995999985));
#329849=CARTESIAN_POINT('',(-5.64403258229752E-14,2.7,-1.9246248980943E-14));
#329850=CARTESIAN_POINT('',(4.50847758599994,2.7,1.49536946999998));
#329851=CARTESIAN_POINT('Ctrl Pts',(3.87111406899994,2.7,0.982007125999989));
#329852=CARTESIAN_POINT('Ctrl Pts',(3.87126816493785,2.7,0.982046870939275));
#329853=CARTESIAN_POINT('Ctrl Pts',(3.87142187737795,2.69999999999987,0.982088098741952));
#329854=CARTESIAN_POINT('Ctrl Pts',(3.87189501533044,2.69999999999987,0.982216169587049));
#329855=CARTESIAN_POINT('Ctrl Pts',(3.87223055398195,2.7,0.982309707816934));
#329856=CARTESIAN_POINT('Ctrl Pts',(3.87365399687205,2.7,0.982712826320259));
#329857=CARTESIAN_POINT('Ctrl Pts',(3.87483183053987,2.7,0.983064923222153));
#329858=CARTESIAN_POINT('Ctrl Pts',(3.87998483279679,2.7,0.984652376245422));
#329859=CARTESIAN_POINT('Ctrl Pts',(3.88426244359151,2.69999999986206,0.986105300970037));
#329860=CARTESIAN_POINT('Ctrl Pts',(3.90294453748838,2.69999999986206,0.992792044582336));
#329861=CARTESIAN_POINT('Ctrl Pts',(3.91828518273234,2.69999999986206,0.999263364476566));
#329862=CARTESIAN_POINT('Ctrl Pts',(3.97345252689468,2.69999999986206,1.02459627187225));
#329863=CARTESIAN_POINT('Ctrl Pts',(4.02405430856334,2.69999999986206,1.05235489225042));
#329864=CARTESIAN_POINT('Ctrl Pts',(4.19593946187621,2.69999999986206,1.16846769640984));
#329865=CARTESIAN_POINT('Ctrl Pts',(4.34710585219733,2.7,1.2951894823555));
#329866=CARTESIAN_POINT('Ctrl Pts',(4.50847758551134,2.7,1.49536947039387));
#329867=CARTESIAN_POINT('',(4.39111701799995,2.7,1.81124027399999));
#329868=CARTESIAN_POINT('Origin',(-5.66300478732629E-14,2.7,-1.92943768261394E-14));
#329869=CARTESIAN_POINT('',(3.57319269599994,2.7,1.78389818299998));
#329870=CARTESIAN_POINT('Ctrl Pts',(4.39111701799995,2.7,1.81124027399999));
#329871=CARTESIAN_POINT('Ctrl Pts',(4.16446456139502,2.7,1.85268289602666));
#329872=CARTESIAN_POINT('Ctrl Pts',(3.98092498875472,2.6999999999957,1.85499572109631));
#329873=CARTESIAN_POINT('Ctrl Pts',(3.68606585001811,2.6999999999957,1.82867373173923));
#329874=CARTESIAN_POINT('Ctrl Pts',(3.59791443406951,2.6999999999957,1.79511456173619));
#329875=CARTESIAN_POINT('Ctrl Pts',(3.57422435482557,2.6999999999957,1.78440390906306));
#329876=CARTESIAN_POINT('Ctrl Pts',(3.5733518983807,2.7,1.78397669582644));
#329877=CARTESIAN_POINT('Ctrl Pts',(3.57320811899994,2.7,1.78390558399999));
#329878=CARTESIAN_POINT('',(3.24327759199994,2.7,1.61918975399999));
#329879=CARTESIAN_POINT('',(1.78657339171225,2.7,0.89193763007472));
#329880=CARTESIAN_POINT('',(2.95444430699995,2.7,2.10044848399999));
#329881=CARTESIAN_POINT('Origin',(-5.66300478732629E-14,2.7,-1.92943768261394E-14));
#329882=CARTESIAN_POINT('',(3.25496455399994,2.7,2.31410196199999));
#329883=CARTESIAN_POINT('',(-5.62541273730178E-14,2.7,-1.90271178888999E-14));
#329884=CARTESIAN_POINT('',(3.66384038699994,2.7,3.02304045899999));
#329885=CARTESIAN_POINT('Ctrl Pts',(3.25496447599994,2.7,2.31410207099998));
#329886=CARTESIAN_POINT('Ctrl Pts',(3.25509380911664,2.7,2.31419479733641));
#329887=CARTESIAN_POINT('Ctrl Pts',(3.25522224824814,2.7,2.31428876886345));
#329888=CARTESIAN_POINT('Ctrl Pts',(3.25561768780298,2.7,2.31457948816326));
#329889=CARTESIAN_POINT('Ctrl Pts',(3.25589686040589,2.7,2.31478799213888));
#329890=CARTESIAN_POINT('Ctrl Pts',(3.25707841110901,2.7,2.31567798214903));
#329891=CARTESIAN_POINT('Ctrl Pts',(3.25804922226441,2.7,2.31643157262964));
#329892=CARTESIAN_POINT('Ctrl Pts',(3.26228208001726,2.7,2.31977431503512));
#329893=CARTESIAN_POINT('Ctrl Pts',(3.26574629644654,2.7,2.32267476697699));
#329894=CARTESIAN_POINT('Ctrl Pts',(3.28074968457772,2.7,2.3356573222311));
#329895=CARTESIAN_POINT('Ctrl Pts',(3.29271501724893,2.7,2.34723161070611));
#329896=CARTESIAN_POINT('Ctrl Pts',(3.33492074366084,2.7,2.3906951000267));
#329897=CARTESIAN_POINT('Ctrl Pts',(3.37207270647139,2.7,2.43481567022442));
#329898=CARTESIAN_POINT('Ctrl Pts',(3.50029625949204,2.7,2.61941870425912));
#329899=CARTESIAN_POINT('Ctrl Pts',(3.5912406264507,2.7,2.79551317498595));
#329900=CARTESIAN_POINT('Ctrl Pts',(3.66384038671035,2.7,3.02304045909239));
#329901=CARTESIAN_POINT('',(3.44029922199995,2.7,3.27518568399999));
#329902=CARTESIAN_POINT('Origin',(-5.66300478732629E-14,2.7,-1.92943768261394E-14));
#329903=CARTESIAN_POINT('',(2.68748460699994,2.7,2.95422159799998));
#329904=CARTESIAN_POINT('Ctrl Pts',(3.44029922199995,2.7,3.27518568399999));
#329905=CARTESIAN_POINT('Ctrl Pts',(3.21786882806739,2.7,3.23269647807893));
#329906=CARTESIAN_POINT('Ctrl Pts',(3.03797835476827,2.69999999991388,3.16794335198484));
#329907=CARTESIAN_POINT('Ctrl Pts',(2.76277297310063,2.69999999991388,3.02746870010843));
#329908=CARTESIAN_POINT('Ctrl Pts',(2.6988645801551,2.7,2.96618934843886));
#329909=CARTESIAN_POINT('Ctrl Pts',(2.68791813750504,2.7,2.95468644111427));
#329910=CARTESIAN_POINT('Ctrl Pts',(2.68769951805849,2.7,2.95445572616322));
#329911=CARTESIAN_POINT('Ctrl Pts',(2.68748475499994,2.7,2.95422146199999));
#329912=CARTESIAN_POINT('',(2.43934748299994,2.7,2.68145648099999));
#329913=CARTESIAN_POINT('',(1.34372503703575,2.7,1.47709181992227));
#329914=CARTESIAN_POINT('',(1.99616775999994,2.7,3.02587826499998));
#329915=CARTESIAN_POINT('Origin',(-5.66300478732629E-14,2.7,-1.92943768261394E-14));
#329916=CARTESIAN_POINT('',(2.19921400599994,2.7,3.33366463399998));
#329917=CARTESIAN_POINT('',(-5.62641527204106E-14,2.7,-1.87397369739548E-14));
#329918=CARTESIAN_POINT('',(2.32438124199994,2.7,4.14243308299999));
#329919=CARTESIAN_POINT('Ctrl Pts',(2.19921389299994,2.7,3.33366470799999));
#329920=CARTESIAN_POINT('Ctrl Pts',(2.19931588681345,2.7,3.33382057043879));
#329921=CARTESIAN_POINT('Ctrl Pts',(2.19945522257332,2.7,3.33403928857926));
#329922=CARTESIAN_POINT('Ctrl Pts',(2.19965044880653,2.7,3.33434572647333));
#329923=CARTESIAN_POINT('Ctrl Pts',(2.1998356694566,2.70000000003935,3.33464134712214));
#329924=CARTESIAN_POINT('Ctrl Pts',(2.20061503722166,2.70000000003935,3.33589661910806));
#329925=CARTESIAN_POINT('Ctrl Pts',(2.20124779639401,2.70000000003925,3.33694950778106));
#329926=CARTESIAN_POINT('Ctrl Pts',(2.2039889246851,2.70000000003925,3.34159838370012));
#329927=CARTESIAN_POINT('Ctrl Pts',(2.20617219748561,2.70000000003925,3.34555593602161));
#329928=CARTESIAN_POINT('Ctrl Pts',(2.21546987923668,2.70000000003925,3.36307652428032));
#329929=CARTESIAN_POINT('Ctrl Pts',(2.22244615778148,2.70000000004265,3.37819108197411));
#329930=CARTESIAN_POINT('Ctrl Pts',(2.24613361740207,2.70000000004265,3.43404298918454));
#329931=CARTESIAN_POINT('Ctrl Pts',(2.26483106300591,2.7,3.48862949035665));
#329932=CARTESIAN_POINT('Ctrl Pts',(2.31198289469397,2.7,3.68342718120813));
#329933=CARTESIAN_POINT('Ctrl Pts',(2.34044050484888,2.7,3.87831359748762));
#329934=CARTESIAN_POINT('Ctrl Pts',(2.32438124099994,2.7,4.14243308299999));
#329935=CARTESIAN_POINT('',(2.02484994999994,2.7,4.29679911999998));
#329936=CARTESIAN_POINT('Origin',(-5.66300478732629E-14,2.7,-1.92943768261394E-14));
#329937=CARTESIAN_POINT('',(1.43881682999994,2.7,3.72556101799999));
#329938=CARTESIAN_POINT('Ctrl Pts',(2.02484995099994,2.7,4.29679911999998));
#329939=CARTESIAN_POINT('Ctrl Pts',(1.8076091663063,2.7,4.16109889870302));
#329940=CARTESIAN_POINT('Ctrl Pts',(1.66719638754842,2.69999999999827,4.02884779679555));
#329941=CARTESIAN_POINT('Ctrl Pts',(1.47880267972745,2.69999999999827,3.81539272798213));
#329942=CARTESIAN_POINT('Ctrl Pts',(1.44348902206156,2.69999999999827,3.73713776031853));
#329943=CARTESIAN_POINT('Ctrl Pts',(1.43891818135105,2.69999999999827,3.72581613794803));
#329944=CARTESIAN_POINT('Ctrl Pts',(1.43886694677176,2.7,3.72568879689252));
#329945=CARTESIAN_POINT('Ctrl Pts',(1.43881701799994,2.7,3.72556094399998));
#329946=CARTESIAN_POINT('',(1.30596997799994,2.7,3.38157765299999));
#329947=CARTESIAN_POINT('',(0.719399171412685,2.7,1.86275657353368));
#329948=CARTESIAN_POINT('',(0.768297694999944,2.7,3.54264641999999));
#329949=CARTESIAN_POINT('Origin',(-5.66300478732629E-14,2.7,-1.92943768261394E-14));
#329950=CARTESIAN_POINT('',(0.846447418999944,2.7,3.90299742599998));
#329951=CARTESIAN_POINT('',(-5.6465168812309E-14,2.7,-1.85341139478339E-14));
#329952=CARTESIAN_POINT('',(0.671001528999944,2.7,4.70236716499999));
#329953=CARTESIAN_POINT('Ctrl Pts',(0.846447287999944,2.7,3.90299745399999));
#329954=CARTESIAN_POINT('Ctrl Pts',(0.846467846681651,2.7,3.90309401488272));
#329955=CARTESIAN_POINT('Ctrl Pts',(0.846597772797866,2.70000000003935,
3.90372626137044));
#329956=CARTESIAN_POINT('Ctrl Pts',(0.846948074033169,2.70000000003935,
3.9055875681682));
#329957=CARTESIAN_POINT('Ctrl Pts',(0.847157926835858,2.70000000003925,
3.90679934491583));
#329958=CARTESIAN_POINT('Ctrl Pts',(0.848033633711593,2.70000000003925,
3.91211870052104));
#329959=CARTESIAN_POINT('Ctrl Pts',(0.848639829978756,2.70000000003925,
3.91659698430345));
#329960=CARTESIAN_POINT('Ctrl Pts',(0.850980875269782,2.70000000003925,
3.9362963901345));
#329961=CARTESIAN_POINT('Ctrl Pts',(0.852026119632535,2.70000000004265,
3.95291500911878));
#329962=CARTESIAN_POINT('Ctrl Pts',(0.853935255767777,2.70000000004265,
4.01346555886468));
#329963=CARTESIAN_POINT('Ctrl Pts',(0.851665052634113,2.7,4.07111646661862));
#329964=CARTESIAN_POINT('Ctrl Pts',(0.823079825617721,2.7,4.28622758807126));
#329965=CARTESIAN_POINT('Ctrl Pts',(0.774023401236597,2.7,4.47792766603638));
#329966=CARTESIAN_POINT('Ctrl Pts',(0.671001528999944,2.7,4.70236716399998));
#329967=CARTESIAN_POINT('',(0.335933473999944,2.7,4.73810602499999));
#329968=CARTESIAN_POINT('Origin',(-5.66300478732629E-14,2.7,-1.92943768261394E-14));
#329969=CARTESIAN_POINT('',(-0.00417113200005593,2.7,3.99374277699999));
#329970=CARTESIAN_POINT('Ctrl Pts',(0.335933474999944,2.7,4.73810602399999));
#329971=CARTESIAN_POINT('Ctrl Pts',(0.191001992066463,2.7,4.54460111419137));
#329972=CARTESIAN_POINT('Ctrl Pts',(0.104334236466074,2.69999999999544,
4.37236491648483));
#329973=CARTESIAN_POINT('Ctrl Pts',(0.000727985133453244,2.69999999999544,
4.09269413395091));
#329974=CARTESIAN_POINT('Ctrl Pts',(-0.00397622061450719,2.69999999999544,
4.00638406225539));
#329975=CARTESIAN_POINT('Ctrl Pts',(-0.00416806805312489,2.69999999999544,
3.99408078084134));
#329976=CARTESIAN_POINT('Ctrl Pts',(-0.00417050122958008,2.7,3.9939117830049));
#329977=CARTESIAN_POINT('Ctrl Pts',(-0.00417093000005587,2.7,3.99374277699999));
#329978=CARTESIAN_POINT('',(-0.00378600900005525,2.7,3.62499802299999));
#329979=CARTESIAN_POINT('',(-0.00208553923349334,2.7,1.99684572999974));
#329980=CARTESIAN_POINT('',(-0.563335230000056,2.7,3.58096054499998));
#329981=CARTESIAN_POINT('Origin',(-5.66300478732629E-14,2.7,-1.92943768261394E-14));
#329982=CARTESIAN_POINT('',(-0.620636577000055,2.7,3.94520878799998));
#329983=CARTESIAN_POINT('',(-5.67522488325669E-14,2.7,-1.85175803632247E-14));
#329984=CARTESIAN_POINT('Ctrl Pts',(-0.620636713000057,2.7,3.94520876599999));
#329985=CARTESIAN_POINT('Ctrl Pts',(-0.62073983719734,2.7,3.94584843905133));
#329986=CARTESIAN_POINT('Ctrl Pts',(-0.621830449136101,2.70000000003925,
3.95215994345551));
#329987=CARTESIAN_POINT('Ctrl Pts',(-0.628437841084849,2.70000000003925,
3.97789527472828));
#329988=CARTESIAN_POINT('Ctrl Pts',(-0.633466261820168,2.70000000004265,
3.99376897413103));
#329989=CARTESIAN_POINT('Ctrl Pts',(-0.653589700676736,2.70000000004265,
4.05100641397367));
#329990=CARTESIAN_POINT('Ctrl Pts',(-0.676556548929634,2.7,4.10395776250158));
#329991=CARTESIAN_POINT('Ctrl Pts',(-0.759803833912682,2.7,4.25572319419894));
#329992=CARTESIAN_POINT('Ctrl Pts',(-0.863318865366222,2.7,4.42354419280542));
#329993=CARTESIAN_POINT('Ctrl Pts',(-1.07300065800006,2.7,4.62722050399999));
#329994=CARTESIAN_POINT('Origin',(-5.66300478732629E-14,15.2,-1.77635683940025E-14));
#329995=CARTESIAN_POINT('',(-0.620636577000055,12.2,3.94520878799998));
#329996=CARTESIAN_POINT('',(-0.563335230000056,12.2,3.58096054499998));
#329997=CARTESIAN_POINT('Ctrl Pts',(-0.620636713000057,12.2,3.94520876599999));
#329998=CARTESIAN_POINT('Ctrl Pts',(-0.620636713000057,5.2,3.94520876599999));
#329999=CARTESIAN_POINT('Ctrl Pts',(-0.620636713000057,2.2,3.94520876599999));
#330000=CARTESIAN_POINT('Ctrl Pts',(-0.620637801933522,12.2,3.94521552058728));
#330001=CARTESIAN_POINT('Ctrl Pts',(-0.620637801933522,5.2,3.94521552058728));
#330002=CARTESIAN_POINT('Ctrl Pts',(-0.620637801933522,2.2,3.94521552058728));
#330003=CARTESIAN_POINT('Ctrl Pts',(-0.620639908278723,12.2,3.94522858611743));
#330004=CARTESIAN_POINT('Ctrl Pts',(-0.620639908278723,5.2,3.94522858611743));
#330005=CARTESIAN_POINT('Ctrl Pts',(-0.620639908278723,2.2,3.94522858611743));
#330006=CARTESIAN_POINT('Ctrl Pts',(-0.620643037501306,12.2,3.94524796762661));
#330007=CARTESIAN_POINT('Ctrl Pts',(-0.620643037501306,5.2,3.94524796762661));
#330008=CARTESIAN_POINT('Ctrl Pts',(-0.620643037501306,2.2,3.94524796762661));
#330009=CARTESIAN_POINT('Ctrl Pts',(-0.620647175670436,12.2,3.94527360898568));
#330010=CARTESIAN_POINT('Ctrl Pts',(-0.620647175670436,5.2,3.94527360898568));
#330011=CARTESIAN_POINT('Ctrl Pts',(-0.620647175670436,2.2,3.94527360898568));
#330012=CARTESIAN_POINT('Ctrl Pts',(-0.620654584000055,12.2,3.94531833299999));
#330013=CARTESIAN_POINT('Ctrl Pts',(-0.620654584000055,5.2,3.94531833299999));
#330014=CARTESIAN_POINT('Ctrl Pts',(-0.620654584000055,2.2,3.94531833299999));
#330015=CARTESIAN_POINT('Ctrl Pts',(-0.620662887000056,12.2,3.94536800899999));
#330016=CARTESIAN_POINT('Ctrl Pts',(-0.620662887000056,5.2,3.94536800899999));
#330017=CARTESIAN_POINT('Ctrl Pts',(-0.620662887000056,2.2,3.94536800899999));
#330018=CARTESIAN_POINT('Ctrl Pts',(-0.620672482000056,12.2,3.94542492999998));
#330019=CARTESIAN_POINT('Ctrl Pts',(-0.620672482000056,5.2,3.94542492999998));
#330020=CARTESIAN_POINT('Ctrl Pts',(-0.620672482000056,2.2,3.94542492999998));
#330021=CARTESIAN_POINT('Ctrl Pts',(-0.620683376000055,12.2,3.94548908399998));
#330022=CARTESIAN_POINT('Ctrl Pts',(-0.620683376000055,5.2,3.94548908399998));
#330023=CARTESIAN_POINT('Ctrl Pts',(-0.620683376000055,2.2,3.94548908399998));
#330024=CARTESIAN_POINT('Ctrl Pts',(-0.620695582000056,12.2,3.94556045499999));
#330025=CARTESIAN_POINT('Ctrl Pts',(-0.620695582000056,5.2,3.94556045499999));
#330026=CARTESIAN_POINT('Ctrl Pts',(-0.620695582000056,2.2,3.94556045499999));
#330027=CARTESIAN_POINT('Ctrl Pts',(-0.620709120000056,12.2,3.94563902299998));
#330028=CARTESIAN_POINT('Ctrl Pts',(-0.620709120000056,5.2,3.94563902299998));
#330029=CARTESIAN_POINT('Ctrl Pts',(-0.620709120000056,2.2,3.94563902299998));
#330030=CARTESIAN_POINT('Ctrl Pts',(-0.620724009000057,12.2,3.94572476199999));
#330031=CARTESIAN_POINT('Ctrl Pts',(-0.620724009000057,5.2,3.94572476199999));
#330032=CARTESIAN_POINT('Ctrl Pts',(-0.620724009000057,2.2,3.94572476199999));
#330033=CARTESIAN_POINT('Ctrl Pts',(-0.620740272000055,12.2,3.94581764599998));
#330034=CARTESIAN_POINT('Ctrl Pts',(-0.620740272000055,5.2,3.94581764599998));
#330035=CARTESIAN_POINT('Ctrl Pts',(-0.620740272000055,2.2,3.94581764599998));
#330036=CARTESIAN_POINT('Ctrl Pts',(-0.620757926000056,12.2,3.94591765199999));
#330037=CARTESIAN_POINT('Ctrl Pts',(-0.620757926000056,5.2,3.94591765199999));
#330038=CARTESIAN_POINT('Ctrl Pts',(-0.620757926000056,2.2,3.94591765199999));
#330039=CARTESIAN_POINT('Ctrl Pts',(-0.620776988000056,12.2,3.94602475899998));
#330040=CARTESIAN_POINT('Ctrl Pts',(-0.620776988000056,5.2,3.94602475899998));
#330041=CARTESIAN_POINT('Ctrl Pts',(-0.620776988000056,2.2,3.94602475899998));
#330042=CARTESIAN_POINT('Ctrl Pts',(-0.620797473000056,12.2,3.94613894999999));
#330043=CARTESIAN_POINT('Ctrl Pts',(-0.620797473000056,5.2,3.94613894999999));
#330044=CARTESIAN_POINT('Ctrl Pts',(-0.620797473000056,2.2,3.94613894999999));
#330045=CARTESIAN_POINT('Ctrl Pts',(-0.620819395000056,12.2,3.94626020699998));
#330046=CARTESIAN_POINT('Ctrl Pts',(-0.620819395000056,5.2,3.94626020699998));
#330047=CARTESIAN_POINT('Ctrl Pts',(-0.620819395000056,2.2,3.94626020699998));
#330048=CARTESIAN_POINT('Ctrl Pts',(-0.620842770000056,12.2,3.94638851099998));
#330049=CARTESIAN_POINT('Ctrl Pts',(-0.620842770000056,5.2,3.94638851099998));
#330050=CARTESIAN_POINT('Ctrl Pts',(-0.620842770000056,2.2,3.94638851099998));
#330051=CARTESIAN_POINT('Ctrl Pts',(-0.620867612000057,12.2,3.94652384499998));
#330052=CARTESIAN_POINT('Ctrl Pts',(-0.620867612000057,5.2,3.94652384499998));
#330053=CARTESIAN_POINT('Ctrl Pts',(-0.620867612000057,2.2,3.94652384499998));
#330054=CARTESIAN_POINT('Ctrl Pts',(-0.620893937000057,12.2,3.94666618599998));
#330055=CARTESIAN_POINT('Ctrl Pts',(-0.620893937000057,5.2,3.94666618599998));
#330056=CARTESIAN_POINT('Ctrl Pts',(-0.620893937000057,2.2,3.94666618599998));
#330057=CARTESIAN_POINT('Ctrl Pts',(-0.620921763000055,12.2,3.94681551699998));
#330058=CARTESIAN_POINT('Ctrl Pts',(-0.620921763000055,5.2,3.94681551699998));
#330059=CARTESIAN_POINT('Ctrl Pts',(-0.620921763000055,2.2,3.94681551699998));
#330060=CARTESIAN_POINT('Ctrl Pts',(-0.620951105000056,12.2,3.94697181399999));
#330061=CARTESIAN_POINT('Ctrl Pts',(-0.620951105000056,5.2,3.94697181399999));
#330062=CARTESIAN_POINT('Ctrl Pts',(-0.620951105000056,2.2,3.94697181399999));
#330063=CARTESIAN_POINT('Ctrl Pts',(-0.620981981000056,12.2,3.94713505999999));
#330064=CARTESIAN_POINT('Ctrl Pts',(-0.620981981000056,5.2,3.94713505999999));
#330065=CARTESIAN_POINT('Ctrl Pts',(-0.620981981000056,2.2,3.94713505999999));
#330066=CARTESIAN_POINT('Ctrl Pts',(-0.621014405000055,12.2,3.94730523299998));
#330067=CARTESIAN_POINT('Ctrl Pts',(-0.621014405000055,5.2,3.94730523299998));
#330068=CARTESIAN_POINT('Ctrl Pts',(-0.621014405000055,2.2,3.94730523299998));
#330069=CARTESIAN_POINT('Ctrl Pts',(-0.621048393000055,12.2,3.94748231499998));
#330070=CARTESIAN_POINT('Ctrl Pts',(-0.621048393000055,5.2,3.94748231499998));
#330071=CARTESIAN_POINT('Ctrl Pts',(-0.621048393000055,2.2,3.94748231499998));
#330072=CARTESIAN_POINT('Ctrl Pts',(-0.621083959000056,12.2,3.94766628699998));
#330073=CARTESIAN_POINT('Ctrl Pts',(-0.621083959000056,5.2,3.94766628699998));
#330074=CARTESIAN_POINT('Ctrl Pts',(-0.621083959000056,2.2,3.94766628699998));
#330075=CARTESIAN_POINT('Ctrl Pts',(-0.621121120000057,12.2,3.94785713099999));
#330076=CARTESIAN_POINT('Ctrl Pts',(-0.621121120000057,5.2,3.94785713099999));
#330077=CARTESIAN_POINT('Ctrl Pts',(-0.621121120000057,2.2,3.94785713099999));
#330078=CARTESIAN_POINT('Ctrl Pts',(-0.621159890000056,12.2,3.94805482699999));
#330079=CARTESIAN_POINT('Ctrl Pts',(-0.621159890000056,5.2,3.94805482699999));
#330080=CARTESIAN_POINT('Ctrl Pts',(-0.621159890000056,2.2,3.94805482699999));
#330081=CARTESIAN_POINT('Ctrl Pts',(-0.621200283000055,12.2,3.94825935499998));
#330082=CARTESIAN_POINT('Ctrl Pts',(-0.621200283000055,5.2,3.94825935499998));
#330083=CARTESIAN_POINT('Ctrl Pts',(-0.621200283000055,2.2,3.94825935499998));
#330084=CARTESIAN_POINT('Ctrl Pts',(-0.621242317000057,12.2,3.94847069599999));
#330085=CARTESIAN_POINT('Ctrl Pts',(-0.621242317000057,5.2,3.94847069599999));
#330086=CARTESIAN_POINT('Ctrl Pts',(-0.621242317000057,2.2,3.94847069599999));
#330087=CARTESIAN_POINT('Ctrl Pts',(-0.621286006000057,12.2,3.94868882999998));
#330088=CARTESIAN_POINT('Ctrl Pts',(-0.621286006000057,5.2,3.94868882999998));
#330089=CARTESIAN_POINT('Ctrl Pts',(-0.621286006000057,2.2,3.94868882999998));
#330090=CARTESIAN_POINT('Ctrl Pts',(-0.621331365000056,12.2,3.94891373999998));
#330091=CARTESIAN_POINT('Ctrl Pts',(-0.621331365000056,5.2,3.94891373999998));
#330092=CARTESIAN_POINT('Ctrl Pts',(-0.621331365000056,2.2,3.94891373999998));
#330093=CARTESIAN_POINT('Ctrl Pts',(-0.621378409000056,12.2,3.94914540499999));
#330094=CARTESIAN_POINT('Ctrl Pts',(-0.621378409000056,5.2,3.94914540499999));
#330095=CARTESIAN_POINT('Ctrl Pts',(-0.621378409000056,2.2,3.94914540499999));
#330096=CARTESIAN_POINT('Ctrl Pts',(-0.621427152000056,12.2,3.94938380899998));
#330097=CARTESIAN_POINT('Ctrl Pts',(-0.621427152000056,5.2,3.94938380899998));
#330098=CARTESIAN_POINT('Ctrl Pts',(-0.621427152000056,2.2,3.94938380899998));
#330099=CARTESIAN_POINT('Ctrl Pts',(-0.621477610000056,12.2,3.94962892899999));
#330100=CARTESIAN_POINT('Ctrl Pts',(-0.621477610000056,5.2,3.94962892899999));
#330101=CARTESIAN_POINT('Ctrl Pts',(-0.621477610000056,2.2,3.94962892899999));
#330102=CARTESIAN_POINT('Ctrl Pts',(-0.621529797000056,12.2,3.94988074799999));
#330103=CARTESIAN_POINT('Ctrl Pts',(-0.621529797000056,5.2,3.94988074799999));
#330104=CARTESIAN_POINT('Ctrl Pts',(-0.621529797000056,2.2,3.94988074799999));
#330105=CARTESIAN_POINT('Ctrl Pts',(-0.621583728000056,12.2,3.95013924799999));
#330106=CARTESIAN_POINT('Ctrl Pts',(-0.621583728000056,5.2,3.95013924799999));
#330107=CARTESIAN_POINT('Ctrl Pts',(-0.621583728000056,2.2,3.95013924799999));
#330108=CARTESIAN_POINT('Ctrl Pts',(-0.621639416000056,12.2,3.95040441099999));
#330109=CARTESIAN_POINT('Ctrl Pts',(-0.621639416000056,5.2,3.95040441099999));
#330110=CARTESIAN_POINT('Ctrl Pts',(-0.621639416000056,2.2,3.95040441099999));
#330111=CARTESIAN_POINT('Ctrl Pts',(-0.621696878000056,12.2,3.95067621599999));
#330112=CARTESIAN_POINT('Ctrl Pts',(-0.621696878000056,5.2,3.95067621599999));
#330113=CARTESIAN_POINT('Ctrl Pts',(-0.621696878000056,2.2,3.95067621599999));
#330114=CARTESIAN_POINT('Ctrl Pts',(-0.621756127000056,12.2,3.95095464499998));
#330115=CARTESIAN_POINT('Ctrl Pts',(-0.621756127000056,5.2,3.95095464499998));
#330116=CARTESIAN_POINT('Ctrl Pts',(-0.621756127000056,2.2,3.95095464499998));
#330117=CARTESIAN_POINT('Ctrl Pts',(-0.621817178000056,12.2,3.95123967899998));
#330118=CARTESIAN_POINT('Ctrl Pts',(-0.621817178000056,5.2,3.95123967899998));
#330119=CARTESIAN_POINT('Ctrl Pts',(-0.621817178000056,2.2,3.95123967899998));
#330120=CARTESIAN_POINT('Ctrl Pts',(-0.621880043000056,12.2,3.95153129999999));
#330121=CARTESIAN_POINT('Ctrl Pts',(-0.621880043000056,5.2,3.95153129999999));
#330122=CARTESIAN_POINT('Ctrl Pts',(-0.621880043000056,2.2,3.95153129999999));
#330123=CARTESIAN_POINT('Ctrl Pts',(-0.621944740000057,12.2,3.95182949099999));
#330124=CARTESIAN_POINT('Ctrl Pts',(-0.621944740000057,5.2,3.95182949099999));
#330125=CARTESIAN_POINT('Ctrl Pts',(-0.621944740000057,2.2,3.95182949099999));
#330126=CARTESIAN_POINT('Ctrl Pts',(-0.622011281000056,12.2,3.95213423099998));
#330127=CARTESIAN_POINT('Ctrl Pts',(-0.622011281000056,5.2,3.95213423099998));
#330128=CARTESIAN_POINT('Ctrl Pts',(-0.622011281000056,2.2,3.95213423099998));
#330129=CARTESIAN_POINT('Ctrl Pts',(-0.622079680000055,12.2,3.95244550299999));
#330130=CARTESIAN_POINT('Ctrl Pts',(-0.622079680000055,5.2,3.95244550299999));
#330131=CARTESIAN_POINT('Ctrl Pts',(-0.622079680000055,2.2,3.95244550299999));
#330132=CARTESIAN_POINT('Ctrl Pts',(-0.622149951000056,12.2,3.95276328699998));
#330133=CARTESIAN_POINT('Ctrl Pts',(-0.622149951000056,5.2,3.95276328699998));
#330134=CARTESIAN_POINT('Ctrl Pts',(-0.622149951000056,2.2,3.95276328699998));
#330135=CARTESIAN_POINT('Ctrl Pts',(-0.622222109000056,12.2,3.95308756699999));
#330136=CARTESIAN_POINT('Ctrl Pts',(-0.622222109000056,5.2,3.95308756699999));
#330137=CARTESIAN_POINT('Ctrl Pts',(-0.622222109000056,2.2,3.95308756699999));
#330138=CARTESIAN_POINT('Ctrl Pts',(-0.622296167000057,12.2,3.95341832299999));
#330139=CARTESIAN_POINT('Ctrl Pts',(-0.622296167000057,5.2,3.95341832299999));
#330140=CARTESIAN_POINT('Ctrl Pts',(-0.622296167000057,2.2,3.95341832299999));
#330141=CARTESIAN_POINT('Ctrl Pts',(-0.622372137000056,12.2,3.95375553799998));
#330142=CARTESIAN_POINT('Ctrl Pts',(-0.622372137000056,5.2,3.95375553799998));
#330143=CARTESIAN_POINT('Ctrl Pts',(-0.622372137000056,2.2,3.95375553799998));
#330144=CARTESIAN_POINT('Ctrl Pts',(-0.622450037000055,12.2,3.95409919299999));
#330145=CARTESIAN_POINT('Ctrl Pts',(-0.622450037000055,5.2,3.95409919299999));
#330146=CARTESIAN_POINT('Ctrl Pts',(-0.622450037000055,2.2,3.95409919299999));
#330147=CARTESIAN_POINT('Ctrl Pts',(-0.622529878000057,12.2,3.95444926999998));
#330148=CARTESIAN_POINT('Ctrl Pts',(-0.622529878000057,5.2,3.95444926999998));
#330149=CARTESIAN_POINT('Ctrl Pts',(-0.622529878000057,2.2,3.95444926999998));
#330150=CARTESIAN_POINT('Ctrl Pts',(-0.622611672000056,12.2,3.95480575099998));
#330151=CARTESIAN_POINT('Ctrl Pts',(-0.622611672000056,5.2,3.95480575099998));
#330152=CARTESIAN_POINT('Ctrl Pts',(-0.622611672000056,2.2,3.95480575099998));
#330153=CARTESIAN_POINT('Ctrl Pts',(-0.622695436000056,12.2,3.95516861799998));
#330154=CARTESIAN_POINT('Ctrl Pts',(-0.622695436000056,5.2,3.95516861799998));
#330155=CARTESIAN_POINT('Ctrl Pts',(-0.622695436000056,2.2,3.95516861799998));
#330156=CARTESIAN_POINT('Ctrl Pts',(-0.622781182000055,12.2,3.95553785199999));
#330157=CARTESIAN_POINT('Ctrl Pts',(-0.622781182000055,5.2,3.95553785199999));
#330158=CARTESIAN_POINT('Ctrl Pts',(-0.622781182000055,2.2,3.95553785199999));
#330159=CARTESIAN_POINT('Ctrl Pts',(-0.622868923000055,12.2,3.95591343599998));
#330160=CARTESIAN_POINT('Ctrl Pts',(-0.622868923000055,5.2,3.95591343599998));
#330161=CARTESIAN_POINT('Ctrl Pts',(-0.622868923000055,2.2,3.95591343599998));
#330162=CARTESIAN_POINT('Ctrl Pts',(-0.622958672000056,12.2,3.95629535099999));
#330163=CARTESIAN_POINT('Ctrl Pts',(-0.622958672000056,5.2,3.95629535099999));
#330164=CARTESIAN_POINT('Ctrl Pts',(-0.622958672000056,2.2,3.95629535099999));
#330165=CARTESIAN_POINT('Ctrl Pts',(-0.623050444000055,12.2,3.95668358099999));
#330166=CARTESIAN_POINT('Ctrl Pts',(-0.623050444000055,5.2,3.95668358099999));
#330167=CARTESIAN_POINT('Ctrl Pts',(-0.623050444000055,2.2,3.95668358099999));
#330168=CARTESIAN_POINT('Ctrl Pts',(-0.623144251000056,12.2,3.95707810699999));
#330169=CARTESIAN_POINT('Ctrl Pts',(-0.623144251000056,5.2,3.95707810699999));
#330170=CARTESIAN_POINT('Ctrl Pts',(-0.623144251000056,2.2,3.95707810699999));
#330171=CARTESIAN_POINT('Ctrl Pts',(-0.623240106000056,12.2,3.95747891199999));
#330172=CARTESIAN_POINT('Ctrl Pts',(-0.623240106000056,5.2,3.95747891199999));
#330173=CARTESIAN_POINT('Ctrl Pts',(-0.623240106000056,2.2,3.95747891199999));
#330174=CARTESIAN_POINT('Ctrl Pts',(-0.623338022000055,12.2,3.95788597599999));
#330175=CARTESIAN_POINT('Ctrl Pts',(-0.623338022000055,5.2,3.95788597599999));
#330176=CARTESIAN_POINT('Ctrl Pts',(-0.623338022000055,2.2,3.95788597599999));
#330177=CARTESIAN_POINT('Ctrl Pts',(-0.623438013000056,12.2,3.95829928399999));
#330178=CARTESIAN_POINT('Ctrl Pts',(-0.623438013000056,5.2,3.95829928399999));
#330179=CARTESIAN_POINT('Ctrl Pts',(-0.623438013000056,2.2,3.95829928399999));
#330180=CARTESIAN_POINT('Ctrl Pts',(-0.623540092000056,12.2,3.95871881699998));
#330181=CARTESIAN_POINT('Ctrl Pts',(-0.623540092000056,5.2,3.95871881699998));
#330182=CARTESIAN_POINT('Ctrl Pts',(-0.623540092000056,2.2,3.95871881699998));
#330183=CARTESIAN_POINT('Ctrl Pts',(-0.623644270000057,12.2,3.95914455699998));
#330184=CARTESIAN_POINT('Ctrl Pts',(-0.623644270000057,5.2,3.95914455699998));
#330185=CARTESIAN_POINT('Ctrl Pts',(-0.623644270000057,2.2,3.95914455699998));
#330186=CARTESIAN_POINT('Ctrl Pts',(-0.623750562000056,12.2,3.95957648599998));
#330187=CARTESIAN_POINT('Ctrl Pts',(-0.623750562000056,5.2,3.95957648599998));
#330188=CARTESIAN_POINT('Ctrl Pts',(-0.623750562000056,2.2,3.95957648599998));
#330189=CARTESIAN_POINT('Ctrl Pts',(-0.623858980000056,12.2,3.96001458899998));
#330190=CARTESIAN_POINT('Ctrl Pts',(-0.623858980000056,5.2,3.96001458899998));
#330191=CARTESIAN_POINT('Ctrl Pts',(-0.623858980000056,2.2,3.96001458899998));
#330192=CARTESIAN_POINT('Ctrl Pts',(-0.623969536000055,12.2,3.96045884699999));
#330193=CARTESIAN_POINT('Ctrl Pts',(-0.623969536000055,5.2,3.96045884699999));
#330194=CARTESIAN_POINT('Ctrl Pts',(-0.623969536000055,2.2,3.96045884699999));
#330195=CARTESIAN_POINT('Ctrl Pts',(-0.624082244000055,12.2,3.96090924099998));
#330196=CARTESIAN_POINT('Ctrl Pts',(-0.624082244000055,5.2,3.96090924099998));
#330197=CARTESIAN_POINT('Ctrl Pts',(-0.624082244000055,2.2,3.96090924099998));
#330198=CARTESIAN_POINT('Ctrl Pts',(-0.624197116000056,12.2,3.96136575499998));
#330199=CARTESIAN_POINT('Ctrl Pts',(-0.624197116000056,5.2,3.96136575499998));
#330200=CARTESIAN_POINT('Ctrl Pts',(-0.624197116000056,2.2,3.96136575499998));
#330201=CARTESIAN_POINT('Ctrl Pts',(-0.624314163000056,12.2,3.96182837299998));
#330202=CARTESIAN_POINT('Ctrl Pts',(-0.624314163000056,5.2,3.96182837299998));
#330203=CARTESIAN_POINT('Ctrl Pts',(-0.624314163000056,2.2,3.96182837299998));
#330204=CARTESIAN_POINT('Ctrl Pts',(-0.624433400000056,12.2,3.96229707499998));
#330205=CARTESIAN_POINT('Ctrl Pts',(-0.624433400000056,5.2,3.96229707499998));
#330206=CARTESIAN_POINT('Ctrl Pts',(-0.624433400000056,2.2,3.96229707499998));
#330207=CARTESIAN_POINT('Ctrl Pts',(-0.624554838000057,12.2,3.96277184599998));
#330208=CARTESIAN_POINT('Ctrl Pts',(-0.624554838000057,5.2,3.96277184599998));
#330209=CARTESIAN_POINT('Ctrl Pts',(-0.624554838000057,2.2,3.96277184599998));
#330210=CARTESIAN_POINT('Ctrl Pts',(-0.624678490000056,12.2,3.96325266599998));
#330211=CARTESIAN_POINT('Ctrl Pts',(-0.624678490000056,5.2,3.96325266599998));
#330212=CARTESIAN_POINT('Ctrl Pts',(-0.624678490000056,2.2,3.96325266599998));
#330213=CARTESIAN_POINT('Ctrl Pts',(-0.624804368000056,12.2,3.96373951999998));
#330214=CARTESIAN_POINT('Ctrl Pts',(-0.624804368000056,5.2,3.96373951999998));
#330215=CARTESIAN_POINT('Ctrl Pts',(-0.624804368000056,2.2,3.96373951999998));
#330216=CARTESIAN_POINT('Ctrl Pts',(-0.624932484000055,12.2,3.96423239099998));
#330217=CARTESIAN_POINT('Ctrl Pts',(-0.624932484000055,5.2,3.96423239099998));
#330218=CARTESIAN_POINT('Ctrl Pts',(-0.624932484000055,2.2,3.96423239099998));
#330219=CARTESIAN_POINT('Ctrl Pts',(-0.625062850000055,12.2,3.96473125899998));
#330220=CARTESIAN_POINT('Ctrl Pts',(-0.625062850000055,5.2,3.96473125899998));
#330221=CARTESIAN_POINT('Ctrl Pts',(-0.625062850000055,2.2,3.96473125899998));
#330222=CARTESIAN_POINT('Ctrl Pts',(-0.625195479000055,12.2,3.96523611099998));
#330223=CARTESIAN_POINT('Ctrl Pts',(-0.625195479000055,5.2,3.96523611099998));
#330224=CARTESIAN_POINT('Ctrl Pts',(-0.625195479000055,2.2,3.96523611099998));
#330225=CARTESIAN_POINT('Ctrl Pts',(-0.625330383000057,12.2,3.96574692699998));
#330226=CARTESIAN_POINT('Ctrl Pts',(-0.625330383000057,5.2,3.96574692699998));
#330227=CARTESIAN_POINT('Ctrl Pts',(-0.625330383000057,2.2,3.96574692699998));
#330228=CARTESIAN_POINT('Ctrl Pts',(-0.625467573000057,12.2,3.96626369099998));
#330229=CARTESIAN_POINT('Ctrl Pts',(-0.625467573000057,5.2,3.96626369099998));
#330230=CARTESIAN_POINT('Ctrl Pts',(-0.625467573000057,2.2,3.96626369099998));
#330231=CARTESIAN_POINT('Ctrl Pts',(-0.625607062000055,12.2,3.96678638599998));
#330232=CARTESIAN_POINT('Ctrl Pts',(-0.625607062000055,5.2,3.96678638599998));
#330233=CARTESIAN_POINT('Ctrl Pts',(-0.625607062000055,2.2,3.96678638599998));
#330234=CARTESIAN_POINT('Ctrl Pts',(-0.625748861000056,12.2,3.96731499499998));
#330235=CARTESIAN_POINT('Ctrl Pts',(-0.625748861000056,5.2,3.96731499499998));
#330236=CARTESIAN_POINT('Ctrl Pts',(-0.625748861000056,2.2,3.96731499499998));
#330237=CARTESIAN_POINT('Ctrl Pts',(-0.625892983000057,12.2,3.96784949999999));
#330238=CARTESIAN_POINT('Ctrl Pts',(-0.625892983000057,5.2,3.96784949999999));
#330239=CARTESIAN_POINT('Ctrl Pts',(-0.625892983000057,2.2,3.96784949999999));
#330240=CARTESIAN_POINT('Ctrl Pts',(-0.626039438000056,12.2,3.96838988599999));
#330241=CARTESIAN_POINT('Ctrl Pts',(-0.626039438000056,5.2,3.96838988599999));
#330242=CARTESIAN_POINT('Ctrl Pts',(-0.626039438000056,2.2,3.96838988599999));
#330243=CARTESIAN_POINT('Ctrl Pts',(-0.626188240000056,12.2,3.96893613399998));
#330244=CARTESIAN_POINT('Ctrl Pts',(-0.626188240000056,5.2,3.96893613399998));
#330245=CARTESIAN_POINT('Ctrl Pts',(-0.626188240000056,2.2,3.96893613399998));
#330246=CARTESIAN_POINT('Ctrl Pts',(-0.626339399000055,12.2,3.96948822899999));
#330247=CARTESIAN_POINT('Ctrl Pts',(-0.626339399000055,5.2,3.96948822899999));
#330248=CARTESIAN_POINT('Ctrl Pts',(-0.626339399000055,2.2,3.96948822899999));
#330249=CARTESIAN_POINT('Ctrl Pts',(-0.626492927000056,12.2,3.97004615499998));
#330250=CARTESIAN_POINT('Ctrl Pts',(-0.626492927000056,5.2,3.97004615499998));
#330251=CARTESIAN_POINT('Ctrl Pts',(-0.626492927000056,2.2,3.97004615499998));
#330252=CARTESIAN_POINT('Ctrl Pts',(-0.626648836000055,12.2,3.97060989199999));
#330253=CARTESIAN_POINT('Ctrl Pts',(-0.626648836000055,5.2,3.97060989199999));
#330254=CARTESIAN_POINT('Ctrl Pts',(-0.626648836000055,2.2,3.97060989199999));
#330255=CARTESIAN_POINT('Ctrl Pts',(-0.626807136000057,12.2,3.97117942599999));
#330256=CARTESIAN_POINT('Ctrl Pts',(-0.626807136000057,5.2,3.97117942599999));
#330257=CARTESIAN_POINT('Ctrl Pts',(-0.626807136000057,2.2,3.97117942599999));
#330258=CARTESIAN_POINT('Ctrl Pts',(-0.626967841000056,12.2,3.97175473999998));
#330259=CARTESIAN_POINT('Ctrl Pts',(-0.626967841000056,5.2,3.97175473999998));
#330260=CARTESIAN_POINT('Ctrl Pts',(-0.626967841000056,2.2,3.97175473999998));
#330261=CARTESIAN_POINT('Ctrl Pts',(-0.627130961000055,12.2,3.97233581699999));
#330262=CARTESIAN_POINT('Ctrl Pts',(-0.627130961000055,5.2,3.97233581699999));
#330263=CARTESIAN_POINT('Ctrl Pts',(-0.627130961000055,2.2,3.97233581699999));
#330264=CARTESIAN_POINT('Ctrl Pts',(-0.627296507000056,12.2,3.97292263899998));
#330265=CARTESIAN_POINT('Ctrl Pts',(-0.627296507000056,5.2,3.97292263899998));
#330266=CARTESIAN_POINT('Ctrl Pts',(-0.627296507000056,2.2,3.97292263899998));
#330267=CARTESIAN_POINT('Ctrl Pts',(-0.627464491000056,12.2,3.97351519199999));
#330268=CARTESIAN_POINT('Ctrl Pts',(-0.627464491000056,5.2,3.97351519199999));
#330269=CARTESIAN_POINT('Ctrl Pts',(-0.627464491000056,2.2,3.97351519199999));
#330270=CARTESIAN_POINT('Ctrl Pts',(-0.627634923000056,12.2,3.97411345799998));
#330271=CARTESIAN_POINT('Ctrl Pts',(-0.627634923000056,5.2,3.97411345799998));
#330272=CARTESIAN_POINT('Ctrl Pts',(-0.627634923000056,2.2,3.97411345799998));
#330273=CARTESIAN_POINT('Ctrl Pts',(-0.627807816000056,12.2,3.97471741999999));
#330274=CARTESIAN_POINT('Ctrl Pts',(-0.627807816000056,5.2,3.97471741999999));
#330275=CARTESIAN_POINT('Ctrl Pts',(-0.627807816000056,2.2,3.97471741999999));
#330276=CARTESIAN_POINT('Ctrl Pts',(-0.627983180000056,12.2,3.97532706299998));
#330277=CARTESIAN_POINT('Ctrl Pts',(-0.627983180000056,5.2,3.97532706299998));
#330278=CARTESIAN_POINT('Ctrl Pts',(-0.627983180000056,2.2,3.97532706299998));
#330279=CARTESIAN_POINT('Ctrl Pts',(-0.628161026000056,12.2,3.97594236899998));
#330280=CARTESIAN_POINT('Ctrl Pts',(-0.628161026000056,5.2,3.97594236899998));
#330281=CARTESIAN_POINT('Ctrl Pts',(-0.628161026000056,2.2,3.97594236899998));
#330282=CARTESIAN_POINT('Ctrl Pts',(-0.628341365000056,12.2,3.97656332399999));
#330283=CARTESIAN_POINT('Ctrl Pts',(-0.628341365000056,5.2,3.97656332399999));
#330284=CARTESIAN_POINT('Ctrl Pts',(-0.628341365000056,2.2,3.97656332399999));
#330285=CARTESIAN_POINT('Ctrl Pts',(-0.628524210000055,12.2,3.97718990899998));
#330286=CARTESIAN_POINT('Ctrl Pts',(-0.628524210000055,5.2,3.97718990899998));
#330287=CARTESIAN_POINT('Ctrl Pts',(-0.628524210000055,2.2,3.97718990899998));
#330288=CARTESIAN_POINT('Ctrl Pts',(-0.628709569000057,12.2,3.97782210999999));
#330289=CARTESIAN_POINT('Ctrl Pts',(-0.628709569000057,5.2,3.97782210999999));
#330290=CARTESIAN_POINT('Ctrl Pts',(-0.628709569000057,2.2,3.97782210999999));
#330291=CARTESIAN_POINT('Ctrl Pts',(-0.628897453000056,12.2,3.97845990899999));
#330292=CARTESIAN_POINT('Ctrl Pts',(-0.628897453000056,5.2,3.97845990899999));
#330293=CARTESIAN_POINT('Ctrl Pts',(-0.628897453000056,2.2,3.97845990899999));
#330294=CARTESIAN_POINT('Ctrl Pts',(-0.629087876000056,12.2,3.97910328999998));
#330295=CARTESIAN_POINT('Ctrl Pts',(-0.629087876000056,5.2,3.97910328999998));
#330296=CARTESIAN_POINT('Ctrl Pts',(-0.629087876000056,2.2,3.97910328999998));
#330297=CARTESIAN_POINT('Ctrl Pts',(-0.629280845000055,12.2,3.97975223799998));
#330298=CARTESIAN_POINT('Ctrl Pts',(-0.629280845000055,5.2,3.97975223799998));
#330299=CARTESIAN_POINT('Ctrl Pts',(-0.629280845000055,2.2,3.97975223799998));
#330300=CARTESIAN_POINT('Ctrl Pts',(-0.629476374000056,12.2,3.98040673499998));
#330301=CARTESIAN_POINT('Ctrl Pts',(-0.629476374000056,5.2,3.98040673499998));
#330302=CARTESIAN_POINT('Ctrl Pts',(-0.629476374000056,2.2,3.98040673499998));
#330303=CARTESIAN_POINT('Ctrl Pts',(-0.629674471000056,12.2,3.98106676699998));
#330304=CARTESIAN_POINT('Ctrl Pts',(-0.629674471000056,5.2,3.98106676699998));
#330305=CARTESIAN_POINT('Ctrl Pts',(-0.629674471000056,2.2,3.98106676699998));
#330306=CARTESIAN_POINT('Ctrl Pts',(-0.629875149000056,12.2,3.98173231599999));
#330307=CARTESIAN_POINT('Ctrl Pts',(-0.629875149000056,5.2,3.98173231599999));
#330308=CARTESIAN_POINT('Ctrl Pts',(-0.629875149000056,2.2,3.98173231599999));
#330309=CARTESIAN_POINT('Ctrl Pts',(-0.630078416000056,12.2,3.98240336699998));
#330310=CARTESIAN_POINT('Ctrl Pts',(-0.630078416000056,5.2,3.98240336699998));
#330311=CARTESIAN_POINT('Ctrl Pts',(-0.630078416000056,2.2,3.98240336699998));
#330312=CARTESIAN_POINT('Ctrl Pts',(-0.630284284000057,12.2,3.98307990399999));
#330313=CARTESIAN_POINT('Ctrl Pts',(-0.630284284000057,5.2,3.98307990399999));
#330314=CARTESIAN_POINT('Ctrl Pts',(-0.630284284000057,2.2,3.98307990399999));
#330315=CARTESIAN_POINT('Ctrl Pts',(-0.630492764000056,12.2,3.98376190999999));
#330316=CARTESIAN_POINT('Ctrl Pts',(-0.630492764000056,5.2,3.98376190999999));
#330317=CARTESIAN_POINT('Ctrl Pts',(-0.630492764000056,2.2,3.98376190999999));
#330318=CARTESIAN_POINT('Ctrl Pts',(-0.630703865000056,12.2,3.98444936999999));
#330319=CARTESIAN_POINT('Ctrl Pts',(-0.630703865000056,5.2,3.98444936999999));
#330320=CARTESIAN_POINT('Ctrl Pts',(-0.630703865000056,2.2,3.98444936999999));
#330321=CARTESIAN_POINT('Ctrl Pts',(-0.630917599000057,12.2,3.98514226799998));
#330322=CARTESIAN_POINT('Ctrl Pts',(-0.630917599000057,5.2,3.98514226799998));
#330323=CARTESIAN_POINT('Ctrl Pts',(-0.630917599000057,2.2,3.98514226799998));
#330324=CARTESIAN_POINT('Ctrl Pts',(-0.631133974000055,12.2,3.98584058799998));
#330325=CARTESIAN_POINT('Ctrl Pts',(-0.631133974000055,5.2,3.98584058799998));
#330326=CARTESIAN_POINT('Ctrl Pts',(-0.631133974000055,2.2,3.98584058799998));
#330327=CARTESIAN_POINT('Ctrl Pts',(-0.631353003000056,12.2,3.98654431399999));
#330328=CARTESIAN_POINT('Ctrl Pts',(-0.631353003000056,5.2,3.98654431399999));
#330329=CARTESIAN_POINT('Ctrl Pts',(-0.631353003000056,2.2,3.98654431399999));
#330330=CARTESIAN_POINT('Ctrl Pts',(-0.631574693000055,12.2,3.98725342999998));
#330331=CARTESIAN_POINT('Ctrl Pts',(-0.631574693000055,5.2,3.98725342999998));
#330332=CARTESIAN_POINT('Ctrl Pts',(-0.631574693000055,2.2,3.98725342999998));
#330333=CARTESIAN_POINT('Ctrl Pts',(-0.631799058000055,12.2,3.98796791999998));
#330334=CARTESIAN_POINT('Ctrl Pts',(-0.631799058000055,5.2,3.98796791999998));
#330335=CARTESIAN_POINT('Ctrl Pts',(-0.631799058000055,2.2,3.98796791999998));
#330336=CARTESIAN_POINT('Ctrl Pts',(-0.632026106000056,12.2,3.98868776899998));
#330337=CARTESIAN_POINT('Ctrl Pts',(-0.632026106000056,5.2,3.98868776899998));
#330338=CARTESIAN_POINT('Ctrl Pts',(-0.632026106000056,2.2,3.98868776899998));
#330339=CARTESIAN_POINT('Ctrl Pts',(-0.632255847000056,12.2,3.98941295999999));
#330340=CARTESIAN_POINT('Ctrl Pts',(-0.632255847000056,5.2,3.98941295999999));
#330341=CARTESIAN_POINT('Ctrl Pts',(-0.632255847000056,2.2,3.98941295999999));
#330342=CARTESIAN_POINT('Ctrl Pts',(-0.632488291000056,12.2,3.99014347899998));
#330343=CARTESIAN_POINT('Ctrl Pts',(-0.632488291000056,5.2,3.99014347899998));
#330344=CARTESIAN_POINT('Ctrl Pts',(-0.632488291000056,2.2,3.99014347899998));
#330345=CARTESIAN_POINT('Ctrl Pts',(-0.632723447000056,12.2,3.99087930899999));
#330346=CARTESIAN_POINT('Ctrl Pts',(-0.632723447000056,5.2,3.99087930899999));
#330347=CARTESIAN_POINT('Ctrl Pts',(-0.632723447000056,2.2,3.99087930899999));
#330348=CARTESIAN_POINT('Ctrl Pts',(-0.632961328000056,12.2,3.99162043499998));
#330349=CARTESIAN_POINT('Ctrl Pts',(-0.632961328000056,5.2,3.99162043499998));
#330350=CARTESIAN_POINT('Ctrl Pts',(-0.632961328000056,2.2,3.99162043499998));
#330351=CARTESIAN_POINT('Ctrl Pts',(-0.633201942000056,12.2,3.99236684199998));
#330352=CARTESIAN_POINT('Ctrl Pts',(-0.633201942000056,5.2,3.99236684199998));
#330353=CARTESIAN_POINT('Ctrl Pts',(-0.633201942000056,2.2,3.99236684199998));
#330354=CARTESIAN_POINT('Ctrl Pts',(-0.633445299000056,12.2,3.99311851299998));
#330355=CARTESIAN_POINT('Ctrl Pts',(-0.633445299000056,5.2,3.99311851299998));
#330356=CARTESIAN_POINT('Ctrl Pts',(-0.633445299000056,2.2,3.99311851299998));
#330357=CARTESIAN_POINT('Ctrl Pts',(-0.633691409000056,12.2,3.99387543199998));
#330358=CARTESIAN_POINT('Ctrl Pts',(-0.633691409000056,5.2,3.99387543199998));
#330359=CARTESIAN_POINT('Ctrl Pts',(-0.633691409000056,2.2,3.99387543199998));
#330360=CARTESIAN_POINT('Ctrl Pts',(-0.633940281000056,12.2,3.99463758599998));
#330361=CARTESIAN_POINT('Ctrl Pts',(-0.633940281000056,5.2,3.99463758599998));
#330362=CARTESIAN_POINT('Ctrl Pts',(-0.633940281000056,2.2,3.99463758599998));
#330363=CARTESIAN_POINT('Ctrl Pts',(-0.634191925000056,12.2,3.99540495699998));
#330364=CARTESIAN_POINT('Ctrl Pts',(-0.634191925000056,5.2,3.99540495699998));
#330365=CARTESIAN_POINT('Ctrl Pts',(-0.634191925000056,2.2,3.99540495699998));
#330366=CARTESIAN_POINT('Ctrl Pts',(-0.634446352000057,12.2,3.99617753199998));
#330367=CARTESIAN_POINT('Ctrl Pts',(-0.634446352000057,5.2,3.99617753199998));
#330368=CARTESIAN_POINT('Ctrl Pts',(-0.634446352000057,2.2,3.99617753199998));
#330369=CARTESIAN_POINT('Ctrl Pts',(-0.634703570000056,12.2,3.99695529299999));
#330370=CARTESIAN_POINT('Ctrl Pts',(-0.634703570000056,5.2,3.99695529299999));
#330371=CARTESIAN_POINT('Ctrl Pts',(-0.634703570000056,2.2,3.99695529299999));
#330372=CARTESIAN_POINT('Ctrl Pts',(-0.634963589000056,12.2,3.99773822599998));
#330373=CARTESIAN_POINT('Ctrl Pts',(-0.634963589000056,5.2,3.99773822599998));
#330374=CARTESIAN_POINT('Ctrl Pts',(-0.634963589000056,2.2,3.99773822599998));
#330375=CARTESIAN_POINT('Ctrl Pts',(-0.635226419000056,12.2,3.99852631499999));
#330376=CARTESIAN_POINT('Ctrl Pts',(-0.635226419000056,5.2,3.99852631499999));
#330377=CARTESIAN_POINT('Ctrl Pts',(-0.635226419000056,2.2,3.99852631499999));
#330378=CARTESIAN_POINT('Ctrl Pts',(-0.635492068000056,12.2,3.99931954599998));
#330379=CARTESIAN_POINT('Ctrl Pts',(-0.635492068000056,5.2,3.99931954599998));
#330380=CARTESIAN_POINT('Ctrl Pts',(-0.635492068000056,2.2,3.99931954599998));
#330381=CARTESIAN_POINT('Ctrl Pts',(-0.635760548000055,12.2,4.00011790099998));
#330382=CARTESIAN_POINT('Ctrl Pts',(-0.635760548000055,5.2,4.00011790099998));
#330383=CARTESIAN_POINT('Ctrl Pts',(-0.635760548000055,2.2,4.00011790099998));
#330384=CARTESIAN_POINT('Ctrl Pts',(-0.636031867000056,12.2,4.00092136699998));
#330385=CARTESIAN_POINT('Ctrl Pts',(-0.636031867000056,5.2,4.00092136699998));
#330386=CARTESIAN_POINT('Ctrl Pts',(-0.636031867000056,2.2,4.00092136699998));
#330387=CARTESIAN_POINT('Ctrl Pts',(-0.636306033000055,12.2,4.00172992899999));
#330388=CARTESIAN_POINT('Ctrl Pts',(-0.636306033000055,5.2,4.00172992899999));
#330389=CARTESIAN_POINT('Ctrl Pts',(-0.636306033000055,2.2,4.00172992899999));
#330390=CARTESIAN_POINT('Ctrl Pts',(-0.636583058000056,12.2,4.00254357099998));
#330391=CARTESIAN_POINT('Ctrl Pts',(-0.636583058000056,5.2,4.00254357099998));
#330392=CARTESIAN_POINT('Ctrl Pts',(-0.636583058000056,2.2,4.00254357099998));
#330393=CARTESIAN_POINT('Ctrl Pts',(-0.636862948000055,12.2,4.00336227799999));
#330394=CARTESIAN_POINT('Ctrl Pts',(-0.636862948000055,5.2,4.00336227799999));
#330395=CARTESIAN_POINT('Ctrl Pts',(-0.636862948000055,2.2,4.00336227799999));
#330396=CARTESIAN_POINT('Ctrl Pts',(-0.637145716000056,12.2,4.00418603399999));
#330397=CARTESIAN_POINT('Ctrl Pts',(-0.637145716000056,5.2,4.00418603399999));
#330398=CARTESIAN_POINT('Ctrl Pts',(-0.637145716000056,2.2,4.00418603399999));
#330399=CARTESIAN_POINT('Ctrl Pts',(-0.637431369000057,12.2,4.00501482399999));
#330400=CARTESIAN_POINT('Ctrl Pts',(-0.637431369000057,5.2,4.00501482399999));
#330401=CARTESIAN_POINT('Ctrl Pts',(-0.637431369000057,2.2,4.00501482399999));
#330402=CARTESIAN_POINT('Ctrl Pts',(-0.637719916000057,12.2,4.00584863399998));
#330403=CARTESIAN_POINT('Ctrl Pts',(-0.637719916000057,5.2,4.00584863399998));
#330404=CARTESIAN_POINT('Ctrl Pts',(-0.637719916000057,2.2,4.00584863399998));
#330405=CARTESIAN_POINT('Ctrl Pts',(-0.638011366000055,12.2,4.00668744799999));
#330406=CARTESIAN_POINT('Ctrl Pts',(-0.638011366000055,5.2,4.00668744799999));
#330407=CARTESIAN_POINT('Ctrl Pts',(-0.638011366000055,2.2,4.00668744799999));
#330408=CARTESIAN_POINT('Ctrl Pts',(-0.638305729000056,12.2,4.00753125199999));
#330409=CARTESIAN_POINT('Ctrl Pts',(-0.638305729000056,5.2,4.00753125199999));
#330410=CARTESIAN_POINT('Ctrl Pts',(-0.638305729000056,2.2,4.00753125199999));
#330411=CARTESIAN_POINT('Ctrl Pts',(-0.638603013000055,12.2,4.00838002899999));
#330412=CARTESIAN_POINT('Ctrl Pts',(-0.638603013000055,5.2,4.00838002899999));
#330413=CARTESIAN_POINT('Ctrl Pts',(-0.638603013000055,2.2,4.00838002899999));
#330414=CARTESIAN_POINT('Ctrl Pts',(-0.638903229000055,12.2,4.00923376599999));
#330415=CARTESIAN_POINT('Ctrl Pts',(-0.638903229000055,5.2,4.00923376599999));
#330416=CARTESIAN_POINT('Ctrl Pts',(-0.638903229000055,2.2,4.00923376599999));
#330417=CARTESIAN_POINT('Ctrl Pts',(-0.639206383000056,12.2,4.01009244699999));
#330418=CARTESIAN_POINT('Ctrl Pts',(-0.639206383000056,5.2,4.01009244699999));
#330419=CARTESIAN_POINT('Ctrl Pts',(-0.639206383000056,2.2,4.01009244699999));
#330420=CARTESIAN_POINT('Ctrl Pts',(-0.639512486000056,12.2,4.01095605699999));
#330421=CARTESIAN_POINT('Ctrl Pts',(-0.639512486000056,5.2,4.01095605699999));
#330422=CARTESIAN_POINT('Ctrl Pts',(-0.639512486000056,2.2,4.01095605699999));
#330423=CARTESIAN_POINT('Ctrl Pts',(-0.639821545000056,12.2,4.01182458199998));
#330424=CARTESIAN_POINT('Ctrl Pts',(-0.639821545000056,5.2,4.01182458199998));
#330425=CARTESIAN_POINT('Ctrl Pts',(-0.639821545000056,2.2,4.01182458199998));
#330426=CARTESIAN_POINT('Ctrl Pts',(-0.640133571000057,12.2,4.01269800599999));
#330427=CARTESIAN_POINT('Ctrl Pts',(-0.640133571000057,5.2,4.01269800599999));
#330428=CARTESIAN_POINT('Ctrl Pts',(-0.640133571000057,2.2,4.01269800599999));
#330429=CARTESIAN_POINT('Ctrl Pts',(-0.640448571000055,12.2,4.01357631499998));
#330430=CARTESIAN_POINT('Ctrl Pts',(-0.640448571000055,5.2,4.01357631499998));
#330431=CARTESIAN_POINT('Ctrl Pts',(-0.640448571000055,2.2,4.01357631499998));
#330432=CARTESIAN_POINT('Ctrl Pts',(-0.640766556000055,12.2,4.01445949299998));
#330433=CARTESIAN_POINT('Ctrl Pts',(-0.640766556000055,5.2,4.01445949299998));
#330434=CARTESIAN_POINT('Ctrl Pts',(-0.640766556000055,2.2,4.01445949299998));
#330435=CARTESIAN_POINT('Ctrl Pts',(-0.641087532000055,12.2,4.01534752699998));
#330436=CARTESIAN_POINT('Ctrl Pts',(-0.641087532000055,5.2,4.01534752699998));
#330437=CARTESIAN_POINT('Ctrl Pts',(-0.641087532000055,2.2,4.01534752699998));
#330438=CARTESIAN_POINT('Ctrl Pts',(-0.641411509000056,12.2,4.01624040099998));
#330439=CARTESIAN_POINT('Ctrl Pts',(-0.641411509000056,5.2,4.01624040099998));
#330440=CARTESIAN_POINT('Ctrl Pts',(-0.641411509000056,2.2,4.01624040099998));
#330441=CARTESIAN_POINT('Ctrl Pts',(-0.641738495000055,12.2,4.01713810099999));
#330442=CARTESIAN_POINT('Ctrl Pts',(-0.641738495000055,5.2,4.01713810099999));
#330443=CARTESIAN_POINT('Ctrl Pts',(-0.641738495000055,2.2,4.01713810099999));
#330444=CARTESIAN_POINT('Ctrl Pts',(-0.642068498000056,12.2,4.01804061099998));
#330445=CARTESIAN_POINT('Ctrl Pts',(-0.642068498000056,5.2,4.01804061099998));
#330446=CARTESIAN_POINT('Ctrl Pts',(-0.642068498000056,2.2,4.01804061099998));
#330447=CARTESIAN_POINT('Ctrl Pts',(-0.642401528000055,12.2,4.01894791799998));
#330448=CARTESIAN_POINT('Ctrl Pts',(-0.642401528000055,5.2,4.01894791799998));
#330449=CARTESIAN_POINT('Ctrl Pts',(-0.642401528000055,2.2,4.01894791799998));
#330450=CARTESIAN_POINT('Ctrl Pts',(-0.642737593000057,12.2,4.01986000599998));
#330451=CARTESIAN_POINT('Ctrl Pts',(-0.642737593000057,5.2,4.01986000599998));
#330452=CARTESIAN_POINT('Ctrl Pts',(-0.642737593000057,2.2,4.01986000599998));
#330453=CARTESIAN_POINT('Ctrl Pts',(-0.643076701000057,12.2,4.02077686099998));
#330454=CARTESIAN_POINT('Ctrl Pts',(-0.643076701000057,5.2,4.02077686099998));
#330455=CARTESIAN_POINT('Ctrl Pts',(-0.643076701000057,2.2,4.02077686099998));
#330456=CARTESIAN_POINT('Ctrl Pts',(-0.643418861000056,12.2,4.02169846799998));
#330457=CARTESIAN_POINT('Ctrl Pts',(-0.643418861000056,5.2,4.02169846799998));
#330458=CARTESIAN_POINT('Ctrl Pts',(-0.643418861000056,2.2,4.02169846799998));
#330459=CARTESIAN_POINT('Ctrl Pts',(-0.643764080000055,12.2,4.02262481199998));
#330460=CARTESIAN_POINT('Ctrl Pts',(-0.643764080000055,5.2,4.02262481199998));
#330461=CARTESIAN_POINT('Ctrl Pts',(-0.643764080000055,2.2,4.02262481199998));
#330462=CARTESIAN_POINT('Ctrl Pts',(-0.644112369000055,12.2,4.02355587999998));
#330463=CARTESIAN_POINT('Ctrl Pts',(-0.644112369000055,5.2,4.02355587999998));
#330464=CARTESIAN_POINT('Ctrl Pts',(-0.644112369000055,2.2,4.02355587999998));
#330465=CARTESIAN_POINT('Ctrl Pts',(-0.644463733000055,12.2,4.02449165699998));
#330466=CARTESIAN_POINT('Ctrl Pts',(-0.644463733000055,5.2,4.02449165699998));
#330467=CARTESIAN_POINT('Ctrl Pts',(-0.644463733000055,2.2,4.02449165699998));
#330468=CARTESIAN_POINT('Ctrl Pts',(-0.644818182000056,12.2,4.02543212699998));
#330469=CARTESIAN_POINT('Ctrl Pts',(-0.644818182000056,5.2,4.02543212699998));
#330470=CARTESIAN_POINT('Ctrl Pts',(-0.644818182000056,2.2,4.02543212699998));
#330471=CARTESIAN_POINT('Ctrl Pts',(-0.645175724000057,12.2,4.02637727699998));
#330472=CARTESIAN_POINT('Ctrl Pts',(-0.645175724000057,5.2,4.02637727699998));
#330473=CARTESIAN_POINT('Ctrl Pts',(-0.645175724000057,2.2,4.02637727699998));
#330474=CARTESIAN_POINT('Ctrl Pts',(-0.645536368000055,12.2,4.02732709299999));
#330475=CARTESIAN_POINT('Ctrl Pts',(-0.645536368000055,5.2,4.02732709299999));
#330476=CARTESIAN_POINT('Ctrl Pts',(-0.645536368000055,2.2,4.02732709299999));
#330477=CARTESIAN_POINT('Ctrl Pts',(-0.645900120000055,12.2,4.02828155799998));
#330478=CARTESIAN_POINT('Ctrl Pts',(-0.645900120000055,5.2,4.02828155799998));
#330479=CARTESIAN_POINT('Ctrl Pts',(-0.645900120000055,2.2,4.02828155799998));
#330480=CARTESIAN_POINT('Ctrl Pts',(-0.646266990000056,12.2,4.02924065999999));
#330481=CARTESIAN_POINT('Ctrl Pts',(-0.646266990000056,5.2,4.02924065999999));
#330482=CARTESIAN_POINT('Ctrl Pts',(-0.646266990000056,2.2,4.02924065999999));
#330483=CARTESIAN_POINT('Ctrl Pts',(-0.646636985000055,12.2,4.03020438399999));
#330484=CARTESIAN_POINT('Ctrl Pts',(-0.646636985000055,5.2,4.03020438399999));
#330485=CARTESIAN_POINT('Ctrl Pts',(-0.646636985000055,2.2,4.03020438399999));
#330486=CARTESIAN_POINT('Ctrl Pts',(-0.647010113000055,12.2,4.03117271499998));
#330487=CARTESIAN_POINT('Ctrl Pts',(-0.647010113000055,5.2,4.03117271499998));
#330488=CARTESIAN_POINT('Ctrl Pts',(-0.647010113000055,2.2,4.03117271499998));
#330489=CARTESIAN_POINT('Ctrl Pts',(-0.647386383000056,12.2,4.03214563999998));
#330490=CARTESIAN_POINT('Ctrl Pts',(-0.647386383000056,5.2,4.03214563999998));
#330491=CARTESIAN_POINT('Ctrl Pts',(-0.647386383000056,2.2,4.03214563999998));
#330492=CARTESIAN_POINT('Ctrl Pts',(-0.647765802000055,12.2,4.03312314399999));
#330493=CARTESIAN_POINT('Ctrl Pts',(-0.647765802000055,5.2,4.03312314399999));
#330494=CARTESIAN_POINT('Ctrl Pts',(-0.647765802000055,2.2,4.03312314399999));
#330495=CARTESIAN_POINT('Ctrl Pts',(-0.648148378000055,12.2,4.03410521199999));
#330496=CARTESIAN_POINT('Ctrl Pts',(-0.648148378000055,5.2,4.03410521199999));
#330497=CARTESIAN_POINT('Ctrl Pts',(-0.648148378000055,2.2,4.03410521199999));
#330498=CARTESIAN_POINT('Ctrl Pts',(-0.648534119000056,12.2,4.03509183099998));
#330499=CARTESIAN_POINT('Ctrl Pts',(-0.648534119000056,5.2,4.03509183099998));
#330500=CARTESIAN_POINT('Ctrl Pts',(-0.648534119000056,2.2,4.03509183099998));
#330501=CARTESIAN_POINT('Ctrl Pts',(-0.648923032000056,12.2,4.03608298599998));
#330502=CARTESIAN_POINT('Ctrl Pts',(-0.648923032000056,5.2,4.03608298599998));
#330503=CARTESIAN_POINT('Ctrl Pts',(-0.648923032000056,2.2,4.03608298599998));
#330504=CARTESIAN_POINT('Ctrl Pts',(-0.649315126000056,12.2,4.03707866299998));
#330505=CARTESIAN_POINT('Ctrl Pts',(-0.649315126000056,5.2,4.03707866299998));
#330506=CARTESIAN_POINT('Ctrl Pts',(-0.649315126000056,2.2,4.03707866299998));
#330507=CARTESIAN_POINT('Ctrl Pts',(-0.649710408000056,12.2,4.03807884799999));
#330508=CARTESIAN_POINT('Ctrl Pts',(-0.649710408000056,5.2,4.03807884799999));
#330509=CARTESIAN_POINT('Ctrl Pts',(-0.649710408000056,2.2,4.03807884799999));
#330510=CARTESIAN_POINT('Ctrl Pts',(-0.650108887000057,12.2,4.03908352699998));
#330511=CARTESIAN_POINT('Ctrl Pts',(-0.650108887000057,5.2,4.03908352699998));
#330512=CARTESIAN_POINT('Ctrl Pts',(-0.650108887000057,2.2,4.03908352699998));
#330513=CARTESIAN_POINT('Ctrl Pts',(-0.650510568000057,12.2,4.04009268399999));
#330514=CARTESIAN_POINT('Ctrl Pts',(-0.650510568000057,5.2,4.04009268399999));
#330515=CARTESIAN_POINT('Ctrl Pts',(-0.650510568000057,2.2,4.04009268399999));
#330516=CARTESIAN_POINT('Ctrl Pts',(-0.650915461000056,12.2,4.04110630799998));
#330517=CARTESIAN_POINT('Ctrl Pts',(-0.650915461000056,5.2,4.04110630799998));
#330518=CARTESIAN_POINT('Ctrl Pts',(-0.650915461000056,2.2,4.04110630799998));
#330519=CARTESIAN_POINT('Ctrl Pts',(-0.651323572000055,12.2,4.04212438299999));
#330520=CARTESIAN_POINT('Ctrl Pts',(-0.651323572000055,5.2,4.04212438299999));
#330521=CARTESIAN_POINT('Ctrl Pts',(-0.651323572000055,2.2,4.04212438299999));
#330522=CARTESIAN_POINT('Ctrl Pts',(-0.651734911000055,12.2,4.04314689499999));
#330523=CARTESIAN_POINT('Ctrl Pts',(-0.651734911000055,5.2,4.04314689499999));
#330524=CARTESIAN_POINT('Ctrl Pts',(-0.651734911000055,2.2,4.04314689499999));
#330525=CARTESIAN_POINT('Ctrl Pts',(-0.652149483000055,12.2,4.04417382999998));
#330526=CARTESIAN_POINT('Ctrl Pts',(-0.652149483000055,5.2,4.04417382999998));
#330527=CARTESIAN_POINT('Ctrl Pts',(-0.652149483000055,2.2,4.04417382999998));
#330528=CARTESIAN_POINT('Ctrl Pts',(-0.652567296000056,12.2,4.04520517499999));
#330529=CARTESIAN_POINT('Ctrl Pts',(-0.652567296000056,5.2,4.04520517499999));
#330530=CARTESIAN_POINT('Ctrl Pts',(-0.652567296000056,2.2,4.04520517499999));
#330531=CARTESIAN_POINT('Ctrl Pts',(-0.652988358000056,12.2,4.04624091499999));
#330532=CARTESIAN_POINT('Ctrl Pts',(-0.652988358000056,5.2,4.04624091499999));
#330533=CARTESIAN_POINT('Ctrl Pts',(-0.652988358000056,2.2,4.04624091499999));
#330534=CARTESIAN_POINT('Ctrl Pts',(-0.653412676000055,12.2,4.04728103699998));
#330535=CARTESIAN_POINT('Ctrl Pts',(-0.653412676000055,5.2,4.04728103699998));
#330536=CARTESIAN_POINT('Ctrl Pts',(-0.653412676000055,2.2,4.04728103699998));
#330537=CARTESIAN_POINT('Ctrl Pts',(-0.653840258000056,12.2,4.04832552499998));
#330538=CARTESIAN_POINT('Ctrl Pts',(-0.653840258000056,5.2,4.04832552499998));
#330539=CARTESIAN_POINT('Ctrl Pts',(-0.653840258000056,2.2,4.04832552499998));
#330540=CARTESIAN_POINT('Ctrl Pts',(-0.654271111000057,12.2,4.04937436799998));
#330541=CARTESIAN_POINT('Ctrl Pts',(-0.654271111000057,5.2,4.04937436799998));
#330542=CARTESIAN_POINT('Ctrl Pts',(-0.654271111000057,2.2,4.04937436799998));
#330543=CARTESIAN_POINT('Ctrl Pts',(-0.654705242000055,12.2,4.05042754999998));
#330544=CARTESIAN_POINT('Ctrl Pts',(-0.654705242000055,5.2,4.05042754999998));
#330545=CARTESIAN_POINT('Ctrl Pts',(-0.654705242000055,2.2,4.05042754999998));
#330546=CARTESIAN_POINT('Ctrl Pts',(-0.655142658000055,12.2,4.05148505699999));
#330547=CARTESIAN_POINT('Ctrl Pts',(-0.655142658000055,5.2,4.05148505699999));
#330548=CARTESIAN_POINT('Ctrl Pts',(-0.655142658000055,2.2,4.05148505699999));
#330549=CARTESIAN_POINT('Ctrl Pts',(-0.655583367000055,12.2,4.05254687799999));
#330550=CARTESIAN_POINT('Ctrl Pts',(-0.655583367000055,5.2,4.05254687799999));
#330551=CARTESIAN_POINT('Ctrl Pts',(-0.655583367000055,2.2,4.05254687799999));
#330552=CARTESIAN_POINT('Ctrl Pts',(-0.656027376000056,12.2,4.05361299499998));
#330553=CARTESIAN_POINT('Ctrl Pts',(-0.656027376000056,5.2,4.05361299499998));
#330554=CARTESIAN_POINT('Ctrl Pts',(-0.656027376000056,2.2,4.05361299499998));
#330555=CARTESIAN_POINT('Ctrl Pts',(-0.656474692000056,12.2,4.05468339699999));
#330556=CARTESIAN_POINT('Ctrl Pts',(-0.656474692000056,5.2,4.05468339699999));
#330557=CARTESIAN_POINT('Ctrl Pts',(-0.656474692000056,2.2,4.05468339699999));
#330558=CARTESIAN_POINT('Ctrl Pts',(-0.656925322000056,12.2,4.05575806999998));
#330559=CARTESIAN_POINT('Ctrl Pts',(-0.656925322000056,5.2,4.05575806999998));
#330560=CARTESIAN_POINT('Ctrl Pts',(-0.656925322000056,2.2,4.05575806999998));
#330561=CARTESIAN_POINT('Ctrl Pts',(-0.657379273000057,12.2,4.05683699999998));
#330562=CARTESIAN_POINT('Ctrl Pts',(-0.657379273000057,5.2,4.05683699999998));
#330563=CARTESIAN_POINT('Ctrl Pts',(-0.657379273000057,2.2,4.05683699999998));
#330564=CARTESIAN_POINT('Ctrl Pts',(-0.657836552000056,12.2,4.05792017199998));
#330565=CARTESIAN_POINT('Ctrl Pts',(-0.657836552000056,5.2,4.05792017199998));
#330566=CARTESIAN_POINT('Ctrl Pts',(-0.657836552000056,2.2,4.05792017199998));
#330567=CARTESIAN_POINT('Ctrl Pts',(-0.658297168000056,12.2,4.05900757499998));
#330568=CARTESIAN_POINT('Ctrl Pts',(-0.658297168000056,5.2,4.05900757499998));
#330569=CARTESIAN_POINT('Ctrl Pts',(-0.658297168000056,2.2,4.05900757499998));
#330570=CARTESIAN_POINT('Ctrl Pts',(-0.658761125000057,12.2,4.06009919199998));
#330571=CARTESIAN_POINT('Ctrl Pts',(-0.658761125000057,5.2,4.06009919199998));
#330572=CARTESIAN_POINT('Ctrl Pts',(-0.658761125000057,2.2,4.06009919199998));
#330573=CARTESIAN_POINT('Ctrl Pts',(-0.659228431000055,12.2,4.06119501299998));
#330574=CARTESIAN_POINT('Ctrl Pts',(-0.659228431000055,5.2,4.06119501299998));
#330575=CARTESIAN_POINT('Ctrl Pts',(-0.659228431000055,2.2,4.06119501299998));
#330576=CARTESIAN_POINT('Ctrl Pts',(-0.659699094000056,12.2,4.06229501999999));
#330577=CARTESIAN_POINT('Ctrl Pts',(-0.659699094000056,5.2,4.06229501999999));
#330578=CARTESIAN_POINT('Ctrl Pts',(-0.659699094000056,2.2,4.06229501999999));
#330579=CARTESIAN_POINT('Ctrl Pts',(-0.660173120000056,12.2,4.06339920299998));
#330580=CARTESIAN_POINT('Ctrl Pts',(-0.660173120000056,5.2,4.06339920299998));
#330581=CARTESIAN_POINT('Ctrl Pts',(-0.660173120000056,2.2,4.06339920299998));
#330582=CARTESIAN_POINT('Ctrl Pts',(-0.660650515000055,12.2,4.06450754799998));
#330583=CARTESIAN_POINT('Ctrl Pts',(-0.660650515000055,5.2,4.06450754799998));
#330584=CARTESIAN_POINT('Ctrl Pts',(-0.660650515000055,2.2,4.06450754799998));
#330585=CARTESIAN_POINT('Ctrl Pts',(-0.661131288000056,12.2,4.06562003999999));
#330586=CARTESIAN_POINT('Ctrl Pts',(-0.661131288000056,5.2,4.06562003999999));
#330587=CARTESIAN_POINT('Ctrl Pts',(-0.661131288000056,2.2,4.06562003999999));
#330588=CARTESIAN_POINT('Ctrl Pts',(-0.661615444000055,12.2,4.06673666599998));
#330589=CARTESIAN_POINT('Ctrl Pts',(-0.661615444000055,5.2,4.06673666599998));
#330590=CARTESIAN_POINT('Ctrl Pts',(-0.661615444000055,2.2,4.06673666599998));
#330591=CARTESIAN_POINT('Ctrl Pts',(-0.662102990000056,12.2,4.06785741199998));
#330592=CARTESIAN_POINT('Ctrl Pts',(-0.662102990000056,5.2,4.06785741199998));
#330593=CARTESIAN_POINT('Ctrl Pts',(-0.662102990000056,2.2,4.06785741199998));
#330594=CARTESIAN_POINT('Ctrl Pts',(-0.662593934000055,12.2,4.06898226699998));
#330595=CARTESIAN_POINT('Ctrl Pts',(-0.662593934000055,5.2,4.06898226699998));
#330596=CARTESIAN_POINT('Ctrl Pts',(-0.662593934000055,2.2,4.06898226699998));
#330597=CARTESIAN_POINT('Ctrl Pts',(-0.663088280000055,12.2,4.07011121399999));
#330598=CARTESIAN_POINT('Ctrl Pts',(-0.663088280000055,5.2,4.07011121399999));
#330599=CARTESIAN_POINT('Ctrl Pts',(-0.663088280000055,2.2,4.07011121399999));
#330600=CARTESIAN_POINT('Ctrl Pts',(-0.663586038000057,12.2,4.07124424199999));
#330601=CARTESIAN_POINT('Ctrl Pts',(-0.663586038000057,5.2,4.07124424199999));
#330602=CARTESIAN_POINT('Ctrl Pts',(-0.663586038000057,2.2,4.07124424199999));
#330603=CARTESIAN_POINT('Ctrl Pts',(-0.664087212000056,12.2,4.07238133699998));
#330604=CARTESIAN_POINT('Ctrl Pts',(-0.664087212000056,5.2,4.07238133699998));
#330605=CARTESIAN_POINT('Ctrl Pts',(-0.664087212000056,2.2,4.07238133699998));
#330606=CARTESIAN_POINT('Ctrl Pts',(-0.664591809000056,12.2,4.07352248499999));
#330607=CARTESIAN_POINT('Ctrl Pts',(-0.664591809000056,5.2,4.07352248499999));
#330608=CARTESIAN_POINT('Ctrl Pts',(-0.664591809000056,2.2,4.07352248499999));
#330609=CARTESIAN_POINT('Ctrl Pts',(-0.665099838000056,12.2,4.07466767299999));
#330610=CARTESIAN_POINT('Ctrl Pts',(-0.665099838000056,5.2,4.07466767299999));
#330611=CARTESIAN_POINT('Ctrl Pts',(-0.665099838000056,2.2,4.07466767299999));
#330612=CARTESIAN_POINT('Ctrl Pts',(-0.665611302000055,12.2,4.07581688699998));
#330613=CARTESIAN_POINT('Ctrl Pts',(-0.665611302000055,5.2,4.07581688699998));
#330614=CARTESIAN_POINT('Ctrl Pts',(-0.665611302000055,2.2,4.07581688699998));
#330615=CARTESIAN_POINT('Ctrl Pts',(-0.666126210000056,12.2,4.07697011499998));
#330616=CARTESIAN_POINT('Ctrl Pts',(-0.666126210000056,5.2,4.07697011499998));
#330617=CARTESIAN_POINT('Ctrl Pts',(-0.666126210000056,2.2,4.07697011499998));
#330618=CARTESIAN_POINT('Ctrl Pts',(-0.666644568000055,12.2,4.07812734299998));
#330619=CARTESIAN_POINT('Ctrl Pts',(-0.666644568000055,5.2,4.07812734299998));
#330620=CARTESIAN_POINT('Ctrl Pts',(-0.666644568000055,2.2,4.07812734299998));
#330621=CARTESIAN_POINT('Ctrl Pts',(-0.667166381000056,12.2,4.07928855699998));
#330622=CARTESIAN_POINT('Ctrl Pts',(-0.667166381000056,5.2,4.07928855699998));
#330623=CARTESIAN_POINT('Ctrl Pts',(-0.667166381000056,2.2,4.07928855699998));
#330624=CARTESIAN_POINT('Ctrl Pts',(-0.667691657000056,12.2,4.08045374499999));
#330625=CARTESIAN_POINT('Ctrl Pts',(-0.667691657000056,5.2,4.08045374499999));
#330626=CARTESIAN_POINT('Ctrl Pts',(-0.667691657000056,2.2,4.08045374499999));
#330627=CARTESIAN_POINT('Ctrl Pts',(-0.668220401000056,12.2,4.08162289299998));
#330628=CARTESIAN_POINT('Ctrl Pts',(-0.668220401000056,5.2,4.08162289299998));
#330629=CARTESIAN_POINT('Ctrl Pts',(-0.668220401000056,2.2,4.08162289299998));
#330630=CARTESIAN_POINT('Ctrl Pts',(-0.668752621000056,12.2,4.08279598699998));
#330631=CARTESIAN_POINT('Ctrl Pts',(-0.668752621000056,5.2,4.08279598699998));
#330632=CARTESIAN_POINT('Ctrl Pts',(-0.668752621000056,2.2,4.08279598699998));
#330633=CARTESIAN_POINT('Ctrl Pts',(-0.669288322000057,12.2,4.08397301599998));
#330634=CARTESIAN_POINT('Ctrl Pts',(-0.669288322000057,5.2,4.08397301599998));
#330635=CARTESIAN_POINT('Ctrl Pts',(-0.669288322000057,2.2,4.08397301599998));
#330636=CARTESIAN_POINT('Ctrl Pts',(-0.669827511000056,12.2,4.08515396399999));
#330637=CARTESIAN_POINT('Ctrl Pts',(-0.669827511000056,5.2,4.08515396399999));
#330638=CARTESIAN_POINT('Ctrl Pts',(-0.669827511000056,2.2,4.08515396399999));
#330639=CARTESIAN_POINT('Ctrl Pts',(-0.670370194000055,12.2,4.08633882099998));
#330640=CARTESIAN_POINT('Ctrl Pts',(-0.670370194000055,5.2,4.08633882099998));
#330641=CARTESIAN_POINT('Ctrl Pts',(-0.670370194000055,2.2,4.08633882099998));
#330642=CARTESIAN_POINT('Ctrl Pts',(-0.670916377000056,12.2,4.08752756999998));
#330643=CARTESIAN_POINT('Ctrl Pts',(-0.670916377000056,5.2,4.08752756999998));
#330644=CARTESIAN_POINT('Ctrl Pts',(-0.670916377000056,2.2,4.08752756999998));
#330645=CARTESIAN_POINT('Ctrl Pts',(-0.671466066000056,12.2,4.08872020199999));
#330646=CARTESIAN_POINT('Ctrl Pts',(-0.671466066000056,5.2,4.08872020199999));
#330647=CARTESIAN_POINT('Ctrl Pts',(-0.671466066000056,2.2,4.08872020199999));
#330648=CARTESIAN_POINT('Ctrl Pts',(-0.672019267000056,12.2,4.08991670099999));
#330649=CARTESIAN_POINT('Ctrl Pts',(-0.672019267000056,5.2,4.08991670099999));
#330650=CARTESIAN_POINT('Ctrl Pts',(-0.672019267000056,2.2,4.08991670099999));
#330651=CARTESIAN_POINT('Ctrl Pts',(-0.672575988000055,12.2,4.09111705399998));
#330652=CARTESIAN_POINT('Ctrl Pts',(-0.672575988000055,5.2,4.09111705399998));
#330653=CARTESIAN_POINT('Ctrl Pts',(-0.672575988000055,2.2,4.09111705399998));
#330654=CARTESIAN_POINT('Ctrl Pts',(-0.673136233000056,12.2,4.09232124999999));
#330655=CARTESIAN_POINT('Ctrl Pts',(-0.673136233000056,5.2,4.09232124999999));
#330656=CARTESIAN_POINT('Ctrl Pts',(-0.673136233000056,2.2,4.09232124999999));
#330657=CARTESIAN_POINT('Ctrl Pts',(-0.673700008000055,12.2,4.09352927399999));
#330658=CARTESIAN_POINT('Ctrl Pts',(-0.673700008000055,5.2,4.09352927399999));
#330659=CARTESIAN_POINT('Ctrl Pts',(-0.673700008000055,2.2,4.09352927399999));
#330660=CARTESIAN_POINT('Ctrl Pts',(-0.674267321000055,12.2,4.09474111499998));
#330661=CARTESIAN_POINT('Ctrl Pts',(-0.674267321000055,5.2,4.09474111499998));
#330662=CARTESIAN_POINT('Ctrl Pts',(-0.674267321000055,2.2,4.09474111499998));
#330663=CARTESIAN_POINT('Ctrl Pts',(-0.674838176000057,12.2,4.09595675699999));
#330664=CARTESIAN_POINT('Ctrl Pts',(-0.674838176000057,5.2,4.09595675699999));
#330665=CARTESIAN_POINT('Ctrl Pts',(-0.674838176000057,2.2,4.09595675699999));
#330666=CARTESIAN_POINT('Ctrl Pts',(-0.675412580000057,12.2,4.09717618899998));
#330667=CARTESIAN_POINT('Ctrl Pts',(-0.675412580000057,5.2,4.09717618899998));
#330668=CARTESIAN_POINT('Ctrl Pts',(-0.675412580000057,2.2,4.09717618899998));
#330669=CARTESIAN_POINT('Ctrl Pts',(-0.675990538000055,12.2,4.09839939799999));
#330670=CARTESIAN_POINT('Ctrl Pts',(-0.675990538000055,5.2,4.09839939799999));
#330671=CARTESIAN_POINT('Ctrl Pts',(-0.675990538000055,2.2,4.09839939799999));
#330672=CARTESIAN_POINT('Ctrl Pts',(-0.676572058000057,12.2,4.09962637099999));
#330673=CARTESIAN_POINT('Ctrl Pts',(-0.676572058000057,5.2,4.09962637099999));
#330674=CARTESIAN_POINT('Ctrl Pts',(-0.676572058000057,2.2,4.09962637099999));
#330675=CARTESIAN_POINT('Ctrl Pts',(-0.677157144000056,12.2,4.10085709399999));
#330676=CARTESIAN_POINT('Ctrl Pts',(-0.677157144000056,5.2,4.10085709399999));
#330677=CARTESIAN_POINT('Ctrl Pts',(-0.677157144000056,2.2,4.10085709399999));
#330678=CARTESIAN_POINT('Ctrl Pts',(-0.677745802000055,12.2,4.10209155499999));
#330679=CARTESIAN_POINT('Ctrl Pts',(-0.677745802000055,5.2,4.10209155499999));
#330680=CARTESIAN_POINT('Ctrl Pts',(-0.677745802000055,2.2,4.10209155499999));
#330681=CARTESIAN_POINT('Ctrl Pts',(-0.678338038000056,12.2,4.10332974099998));
#330682=CARTESIAN_POINT('Ctrl Pts',(-0.678338038000056,5.2,4.10332974099998));
#330683=CARTESIAN_POINT('Ctrl Pts',(-0.678338038000056,2.2,4.10332974099998));
#330684=CARTESIAN_POINT('Ctrl Pts',(-0.678933857000056,12.2,4.10457163999999));
#330685=CARTESIAN_POINT('Ctrl Pts',(-0.678933857000056,5.2,4.10457163999999));
#330686=CARTESIAN_POINT('Ctrl Pts',(-0.678933857000056,2.2,4.10457163999999));
#330687=CARTESIAN_POINT('Ctrl Pts',(-0.679533266000056,12.2,4.10581723699998));
#330688=CARTESIAN_POINT('Ctrl Pts',(-0.679533266000056,5.2,4.10581723699998));
#330689=CARTESIAN_POINT('Ctrl Pts',(-0.679533266000056,2.2,4.10581723699998));
#330690=CARTESIAN_POINT('Ctrl Pts',(-0.680136271000055,12.2,4.10706652199998));
#330691=CARTESIAN_POINT('Ctrl Pts',(-0.680136271000055,5.2,4.10706652199998));
#330692=CARTESIAN_POINT('Ctrl Pts',(-0.680136271000055,2.2,4.10706652199998));
#330693=CARTESIAN_POINT('Ctrl Pts',(-0.680742878000055,12.2,4.10831947899998));
#330694=CARTESIAN_POINT('Ctrl Pts',(-0.680742878000055,5.2,4.10831947899998));
#330695=CARTESIAN_POINT('Ctrl Pts',(-0.680742878000055,2.2,4.10831947899998));
#330696=CARTESIAN_POINT('Ctrl Pts',(-0.681353090000056,12.2,4.10957609699998));
#330697=CARTESIAN_POINT('Ctrl Pts',(-0.681353090000056,5.2,4.10957609699998));
#330698=CARTESIAN_POINT('Ctrl Pts',(-0.681353090000056,2.2,4.10957609699998));
#330699=CARTESIAN_POINT('Ctrl Pts',(-0.681966916000055,12.2,4.11083636399999));
#330700=CARTESIAN_POINT('Ctrl Pts',(-0.681966916000055,5.2,4.11083636399999));
#330701=CARTESIAN_POINT('Ctrl Pts',(-0.681966916000055,2.2,4.11083636399999));
#330702=CARTESIAN_POINT('Ctrl Pts',(-0.682584358000057,12.2,4.11210026599999));
#330703=CARTESIAN_POINT('Ctrl Pts',(-0.682584358000057,5.2,4.11210026599999));
#330704=CARTESIAN_POINT('Ctrl Pts',(-0.682584358000057,2.2,4.11210026599999));
#330705=CARTESIAN_POINT('Ctrl Pts',(-0.683205425000055,12.2,4.11336778999999));
#330706=CARTESIAN_POINT('Ctrl Pts',(-0.683205425000055,5.2,4.11336778999999));
#330707=CARTESIAN_POINT('Ctrl Pts',(-0.683205425000055,2.2,4.11336778999999));
#330708=CARTESIAN_POINT('Ctrl Pts',(-0.683830121000056,12.2,4.11463892399999));
#330709=CARTESIAN_POINT('Ctrl Pts',(-0.683830121000056,5.2,4.11463892399999));
#330710=CARTESIAN_POINT('Ctrl Pts',(-0.683830121000056,2.2,4.11463892399999));
#330711=CARTESIAN_POINT('Ctrl Pts',(-0.684458451000056,12.2,4.11591365699999));
#330712=CARTESIAN_POINT('Ctrl Pts',(-0.684458451000056,5.2,4.11591365699999));
#330713=CARTESIAN_POINT('Ctrl Pts',(-0.684458451000056,2.2,4.11591365699999));
#330714=CARTESIAN_POINT('Ctrl Pts',(-0.685090423000055,12.2,4.11719197299998));
#330715=CARTESIAN_POINT('Ctrl Pts',(-0.685090423000055,5.2,4.11719197299998));
#330716=CARTESIAN_POINT('Ctrl Pts',(-0.685090423000055,2.2,4.11719197299998));
#330717=CARTESIAN_POINT('Ctrl Pts',(-0.685726038000055,12.2,4.11847385999998));
#330718=CARTESIAN_POINT('Ctrl Pts',(-0.685726038000055,5.2,4.11847385999998));
#330719=CARTESIAN_POINT('Ctrl Pts',(-0.685726038000055,2.2,4.11847385999998));
#330720=CARTESIAN_POINT('Ctrl Pts',(-0.686365306000055,12.2,4.11975930699998));
#330721=CARTESIAN_POINT('Ctrl Pts',(-0.686365306000055,5.2,4.11975930699998));
#330722=CARTESIAN_POINT('Ctrl Pts',(-0.686365306000055,2.2,4.11975930699998));
#330723=CARTESIAN_POINT('Ctrl Pts',(-0.687008229000057,12.2,4.12104830099998));
#330724=CARTESIAN_POINT('Ctrl Pts',(-0.687008229000057,5.2,4.12104830099998));
#330725=CARTESIAN_POINT('Ctrl Pts',(-0.687008229000057,2.2,4.12104830099998));
#330726=CARTESIAN_POINT('Ctrl Pts',(-0.687654816000055,12.2,4.12234082799999));
#330727=CARTESIAN_POINT('Ctrl Pts',(-0.687654816000055,5.2,4.12234082799999));
#330728=CARTESIAN_POINT('Ctrl Pts',(-0.687654816000055,2.2,4.12234082799999));
#330729=CARTESIAN_POINT('Ctrl Pts',(-0.688305069000055,12.2,4.12363687799999));
#330730=CARTESIAN_POINT('Ctrl Pts',(-0.688305069000055,5.2,4.12363687799999));
#330731=CARTESIAN_POINT('Ctrl Pts',(-0.688305069000055,2.2,4.12363687799999));
#330732=CARTESIAN_POINT('Ctrl Pts',(-0.688958994000056,12.2,4.12493643499998));
#330733=CARTESIAN_POINT('Ctrl Pts',(-0.688958994000056,5.2,4.12493643499998));
#330734=CARTESIAN_POINT('Ctrl Pts',(-0.688958994000056,2.2,4.12493643499998));
#330735=CARTESIAN_POINT('Ctrl Pts',(-0.689616598000056,12.2,4.12623949099999));
#330736=CARTESIAN_POINT('Ctrl Pts',(-0.689616598000056,5.2,4.12623949099999));
#330737=CARTESIAN_POINT('Ctrl Pts',(-0.689616598000056,2.2,4.12623949099999));
#330738=CARTESIAN_POINT('Ctrl Pts',(-0.690277884000056,12.2,4.12754602799998));
#330739=CARTESIAN_POINT('Ctrl Pts',(-0.690277884000056,5.2,4.12754602799998));
#330740=CARTESIAN_POINT('Ctrl Pts',(-0.690277884000056,2.2,4.12754602799998));
#330741=CARTESIAN_POINT('Ctrl Pts',(-0.690942859000057,12.2,4.12885603799998));
#330742=CARTESIAN_POINT('Ctrl Pts',(-0.690942859000057,5.2,4.12885603799998));
#330743=CARTESIAN_POINT('Ctrl Pts',(-0.690942859000057,2.2,4.12885603799998));
#330744=CARTESIAN_POINT('Ctrl Pts',(-0.691611527000056,12.2,4.13016950599999));
#330745=CARTESIAN_POINT('Ctrl Pts',(-0.691611527000056,5.2,4.13016950599999));
#330746=CARTESIAN_POINT('Ctrl Pts',(-0.691611527000056,2.2,4.13016950599999));
#330747=CARTESIAN_POINT('Ctrl Pts',(-0.692283895000055,12.2,4.13148642099999));
#330748=CARTESIAN_POINT('Ctrl Pts',(-0.692283895000055,5.2,4.13148642099999));
#330749=CARTESIAN_POINT('Ctrl Pts',(-0.692283895000055,2.2,4.13148642099999));
#330750=CARTESIAN_POINT('Ctrl Pts',(-0.692959966000056,12.2,4.13280676999998));
#330751=CARTESIAN_POINT('Ctrl Pts',(-0.692959966000056,5.2,4.13280676999998));
#330752=CARTESIAN_POINT('Ctrl Pts',(-0.692959966000056,2.2,4.13280676999998));
#330753=CARTESIAN_POINT('Ctrl Pts',(-0.693639747000055,12.2,4.13413053899998));
#330754=CARTESIAN_POINT('Ctrl Pts',(-0.693639747000055,5.2,4.13413053899998));
#330755=CARTESIAN_POINT('Ctrl Pts',(-0.693639747000055,2.2,4.13413053899998));
#330756=CARTESIAN_POINT('Ctrl Pts',(-0.694323241000055,12.2,4.13545771799999));
#330757=CARTESIAN_POINT('Ctrl Pts',(-0.694323241000055,5.2,4.13545771799999));
#330758=CARTESIAN_POINT('Ctrl Pts',(-0.694323241000055,2.2,4.13545771799999));
#330759=CARTESIAN_POINT('Ctrl Pts',(-0.695010455000055,12.2,4.13678829299998));
#330760=CARTESIAN_POINT('Ctrl Pts',(-0.695010455000055,5.2,4.13678829299998));
#330761=CARTESIAN_POINT('Ctrl Pts',(-0.695010455000055,2.2,4.13678829299998));
#330762=CARTESIAN_POINT('Ctrl Pts',(-0.695701394000056,12.2,4.13812225399998));
#330763=CARTESIAN_POINT('Ctrl Pts',(-0.695701394000056,5.2,4.13812225399998));
#330764=CARTESIAN_POINT('Ctrl Pts',(-0.695701394000056,2.2,4.13812225399998));
#330765=CARTESIAN_POINT('Ctrl Pts',(-0.696396062000056,12.2,4.13945958499998));
#330766=CARTESIAN_POINT('Ctrl Pts',(-0.696396062000056,5.2,4.13945958499998));
#330767=CARTESIAN_POINT('Ctrl Pts',(-0.696396062000056,2.2,4.13945958499998));
#330768=CARTESIAN_POINT('Ctrl Pts',(-0.697094464000055,12.2,4.14080027599999));
#330769=CARTESIAN_POINT('Ctrl Pts',(-0.697094464000055,5.2,4.14080027599999));
#330770=CARTESIAN_POINT('Ctrl Pts',(-0.697094464000055,2.2,4.14080027599999));
#330771=CARTESIAN_POINT('Ctrl Pts',(-0.697796606000055,12.2,4.14214431499998));
#330772=CARTESIAN_POINT('Ctrl Pts',(-0.697796606000055,5.2,4.14214431499998));
#330773=CARTESIAN_POINT('Ctrl Pts',(-0.697796606000055,2.2,4.14214431499998));
#330774=CARTESIAN_POINT('Ctrl Pts',(-0.698502492000056,12.2,4.14349168899999));
#330775=CARTESIAN_POINT('Ctrl Pts',(-0.698502492000056,5.2,4.14349168899999));
#330776=CARTESIAN_POINT('Ctrl Pts',(-0.698502492000056,2.2,4.14349168899999));
#330777=CARTESIAN_POINT('Ctrl Pts',(-0.699212127000056,12.2,4.14484238499998));
#330778=CARTESIAN_POINT('Ctrl Pts',(-0.699212127000056,5.2,4.14484238499998));
#330779=CARTESIAN_POINT('Ctrl Pts',(-0.699212127000056,2.2,4.14484238499998));
#330780=CARTESIAN_POINT('Ctrl Pts',(-0.699925517000055,12.2,4.14619639199999));
#330781=CARTESIAN_POINT('Ctrl Pts',(-0.699925517000055,5.2,4.14619639199999));
#330782=CARTESIAN_POINT('Ctrl Pts',(-0.699925517000055,2.2,4.14619639199999));
#330783=CARTESIAN_POINT('Ctrl Pts',(-0.700642665000055,12.2,4.14755369699999));
#330784=CARTESIAN_POINT('Ctrl Pts',(-0.700642665000055,5.2,4.14755369699999));
#330785=CARTESIAN_POINT('Ctrl Pts',(-0.700642665000055,2.2,4.14755369699999));
#330786=CARTESIAN_POINT('Ctrl Pts',(-0.701363578000055,12.2,4.14891428699999));
#330787=CARTESIAN_POINT('Ctrl Pts',(-0.701363578000055,5.2,4.14891428699999));
#330788=CARTESIAN_POINT('Ctrl Pts',(-0.701363578000055,2.2,4.14891428699999));
#330789=CARTESIAN_POINT('Ctrl Pts',(-0.702088258000056,12.2,4.15027815199998));
#330790=CARTESIAN_POINT('Ctrl Pts',(-0.702088258000056,5.2,4.15027815199998));
#330791=CARTESIAN_POINT('Ctrl Pts',(-0.702088258000056,2.2,4.15027815199998));
#330792=CARTESIAN_POINT('Ctrl Pts',(-0.702816713000055,12.2,4.15164527899999));
#330793=CARTESIAN_POINT('Ctrl Pts',(-0.702816713000055,5.2,4.15164527899999));
#330794=CARTESIAN_POINT('Ctrl Pts',(-0.702816713000055,2.2,4.15164527899999));
#330795=CARTESIAN_POINT('Ctrl Pts',(-0.703548946000057,12.2,4.15301565399999));
#330796=CARTESIAN_POINT('Ctrl Pts',(-0.703548946000057,5.2,4.15301565399999));
#330797=CARTESIAN_POINT('Ctrl Pts',(-0.703548946000057,2.2,4.15301565399999));
#330798=CARTESIAN_POINT('Ctrl Pts',(-0.704284962000056,12.2,4.15438926699998));
#330799=CARTESIAN_POINT('Ctrl Pts',(-0.704284962000056,5.2,4.15438926699998));
#330800=CARTESIAN_POINT('Ctrl Pts',(-0.704284962000056,2.2,4.15438926699998));
#330801=CARTESIAN_POINT('Ctrl Pts',(-0.705024766000056,12.2,4.15576610399999));
#330802=CARTESIAN_POINT('Ctrl Pts',(-0.705024766000056,5.2,4.15576610399999));
#330803=CARTESIAN_POINT('Ctrl Pts',(-0.705024766000056,2.2,4.15576610399999));
#330804=CARTESIAN_POINT('Ctrl Pts',(-0.705768362000055,12.2,4.15714615499999));
#330805=CARTESIAN_POINT('Ctrl Pts',(-0.705768362000055,5.2,4.15714615499999));
#330806=CARTESIAN_POINT('Ctrl Pts',(-0.705768362000055,2.2,4.15714615499999));
#330807=CARTESIAN_POINT('Ctrl Pts',(-0.706515755000057,12.2,4.15852940599999));
#330808=CARTESIAN_POINT('Ctrl Pts',(-0.706515755000057,5.2,4.15852940599999));
#330809=CARTESIAN_POINT('Ctrl Pts',(-0.706515755000057,2.2,4.15852940599999));
#330810=CARTESIAN_POINT('Ctrl Pts',(-0.707266950000056,12.2,4.15991584599999));
#330811=CARTESIAN_POINT('Ctrl Pts',(-0.707266950000056,5.2,4.15991584599999));
#330812=CARTESIAN_POINT('Ctrl Pts',(-0.707266950000056,2.2,4.15991584599999));
#330813=CARTESIAN_POINT('Ctrl Pts',(-0.708021951000056,12.2,4.16130546299998));
#330814=CARTESIAN_POINT('Ctrl Pts',(-0.708021951000056,5.2,4.16130546299998));
#330815=CARTESIAN_POINT('Ctrl Pts',(-0.708021951000056,2.2,4.16130546299998));
#330816=CARTESIAN_POINT('Ctrl Pts',(-0.708780763000056,12.2,4.16269824399999));
#330817=CARTESIAN_POINT('Ctrl Pts',(-0.708780763000056,5.2,4.16269824399999));
#330818=CARTESIAN_POINT('Ctrl Pts',(-0.708780763000056,2.2,4.16269824399999));
#330819=CARTESIAN_POINT('Ctrl Pts',(-0.709543392000055,12.2,4.16409417799999));
#330820=CARTESIAN_POINT('Ctrl Pts',(-0.709543392000055,5.2,4.16409417799999));
#330821=CARTESIAN_POINT('Ctrl Pts',(-0.709543392000055,2.2,4.16409417799999));
#330822=CARTESIAN_POINT('Ctrl Pts',(-0.710309839000055,12.2,4.16549325299999));
#330823=CARTESIAN_POINT('Ctrl Pts',(-0.710309839000055,5.2,4.16549325299999));
#330824=CARTESIAN_POINT('Ctrl Pts',(-0.710309839000055,2.2,4.16549325299999));
#330825=CARTESIAN_POINT('Ctrl Pts',(-0.711080112000056,12.2,4.16689545499998));
#330826=CARTESIAN_POINT('Ctrl Pts',(-0.711080112000056,5.2,4.16689545499998));
#330827=CARTESIAN_POINT('Ctrl Pts',(-0.711080112000056,2.2,4.16689545499998));
#330828=CARTESIAN_POINT('Ctrl Pts',(-0.711854213000055,12.2,4.16830077499998));
#330829=CARTESIAN_POINT('Ctrl Pts',(-0.711854213000055,5.2,4.16830077499998));
#330830=CARTESIAN_POINT('Ctrl Pts',(-0.711854213000055,2.2,4.16830077499998));
#330831=CARTESIAN_POINT('Ctrl Pts',(-0.712632149000055,12.2,4.16970919899998));
#330832=CARTESIAN_POINT('Ctrl Pts',(-0.712632149000055,5.2,4.16970919899998));
#330833=CARTESIAN_POINT('Ctrl Pts',(-0.712632149000055,2.2,4.16970919899998));
#330834=CARTESIAN_POINT('Ctrl Pts',(-0.713413922000056,12.2,4.17112071399998));
#330835=CARTESIAN_POINT('Ctrl Pts',(-0.713413922000056,5.2,4.17112071399998));
#330836=CARTESIAN_POINT('Ctrl Pts',(-0.713413922000056,2.2,4.17112071399998));
#330837=CARTESIAN_POINT('Ctrl Pts',(-0.714199538000055,12.2,4.17253531199999));
#330838=CARTESIAN_POINT('Ctrl Pts',(-0.714199538000055,5.2,4.17253531199999));
#330839=CARTESIAN_POINT('Ctrl Pts',(-0.714199538000055,2.2,4.17253531199999));
#330840=CARTESIAN_POINT('Ctrl Pts',(-0.714988999000056,12.2,4.17395297699999));
#330841=CARTESIAN_POINT('Ctrl Pts',(-0.714988999000056,5.2,4.17395297699999));
#330842=CARTESIAN_POINT('Ctrl Pts',(-0.714988999000056,2.2,4.17395297699999));
#330843=CARTESIAN_POINT('Ctrl Pts',(-0.715782313000056,12.2,4.17537369999998));
#330844=CARTESIAN_POINT('Ctrl Pts',(-0.715782313000056,5.2,4.17537369999998));
#330845=CARTESIAN_POINT('Ctrl Pts',(-0.715782313000056,2.2,4.17537369999998));
#330846=CARTESIAN_POINT('Ctrl Pts',(-0.716579482000055,12.2,4.17679746799998));
#330847=CARTESIAN_POINT('Ctrl Pts',(-0.716579482000055,5.2,4.17679746799998));
#330848=CARTESIAN_POINT('Ctrl Pts',(-0.716579482000055,2.2,4.17679746799998));
#330849=CARTESIAN_POINT('Ctrl Pts',(-0.717380511000056,12.2,4.17822426999999));
#330850=CARTESIAN_POINT('Ctrl Pts',(-0.717380511000056,5.2,4.17822426999999));
#330851=CARTESIAN_POINT('Ctrl Pts',(-0.717380511000056,2.2,4.17822426999999));
#330852=CARTESIAN_POINT('Ctrl Pts',(-0.718185404000057,12.2,4.17965409099998));
#330853=CARTESIAN_POINT('Ctrl Pts',(-0.718185404000057,5.2,4.17965409099998));
#330854=CARTESIAN_POINT('Ctrl Pts',(-0.718185404000057,2.2,4.17965409099998));
#330855=CARTESIAN_POINT('Ctrl Pts',(-0.718994165000056,12.2,4.18108692299998));
#330856=CARTESIAN_POINT('Ctrl Pts',(-0.718994165000056,5.2,4.18108692299998));
#330857=CARTESIAN_POINT('Ctrl Pts',(-0.718994165000056,2.2,4.18108692299998));
#330858=CARTESIAN_POINT('Ctrl Pts',(-0.719806800000056,12.2,4.18252275099999));
#330859=CARTESIAN_POINT('Ctrl Pts',(-0.719806800000056,5.2,4.18252275099999));
#330860=CARTESIAN_POINT('Ctrl Pts',(-0.719806800000056,2.2,4.18252275099999));
#330861=CARTESIAN_POINT('Ctrl Pts',(-0.720623311000056,12.2,4.18396156599999));
#330862=CARTESIAN_POINT('Ctrl Pts',(-0.720623311000056,5.2,4.18396156599999));
#330863=CARTESIAN_POINT('Ctrl Pts',(-0.720623311000056,2.2,4.18396156599999));
#330864=CARTESIAN_POINT('Ctrl Pts',(-0.721443703000055,12.2,4.18540335499999));
#330865=CARTESIAN_POINT('Ctrl Pts',(-0.721443703000055,5.2,4.18540335499999));
#330866=CARTESIAN_POINT('Ctrl Pts',(-0.721443703000055,2.2,4.18540335499999));
#330867=CARTESIAN_POINT('Ctrl Pts',(-0.722267980000056,12.2,4.18684810599999));
#330868=CARTESIAN_POINT('Ctrl Pts',(-0.722267980000056,5.2,4.18684810599999));
#330869=CARTESIAN_POINT('Ctrl Pts',(-0.722267980000056,2.2,4.18684810599999));
#330870=CARTESIAN_POINT('Ctrl Pts',(-0.723096147000056,12.2,4.18829580799999));
#330871=CARTESIAN_POINT('Ctrl Pts',(-0.723096147000056,5.2,4.18829580799999));
#330872=CARTESIAN_POINT('Ctrl Pts',(-0.723096147000056,2.2,4.18829580799999));
#330873=CARTESIAN_POINT('Ctrl Pts',(-0.723928208000055,12.2,4.18974644799999));
#330874=CARTESIAN_POINT('Ctrl Pts',(-0.723928208000055,5.2,4.18974644799999));
#330875=CARTESIAN_POINT('Ctrl Pts',(-0.723928208000055,2.2,4.18974644799999));
#330876=CARTESIAN_POINT('Ctrl Pts',(-0.724764166000057,12.2,4.19120001499999));
#330877=CARTESIAN_POINT('Ctrl Pts',(-0.724764166000057,5.2,4.19120001499999));
#330878=CARTESIAN_POINT('Ctrl Pts',(-0.724764166000057,2.2,4.19120001499999));
#330879=CARTESIAN_POINT('Ctrl Pts',(-0.725604025000056,12.2,4.19265649699998));
#330880=CARTESIAN_POINT('Ctrl Pts',(-0.725604025000056,5.2,4.19265649699998));
#330881=CARTESIAN_POINT('Ctrl Pts',(-0.725604025000056,2.2,4.19265649699998));
#330882=CARTESIAN_POINT('Ctrl Pts',(-0.726447791000057,12.2,4.19411588299998));
#330883=CARTESIAN_POINT('Ctrl Pts',(-0.726447791000057,5.2,4.19411588299998));
#330884=CARTESIAN_POINT('Ctrl Pts',(-0.726447791000057,2.2,4.19411588299998));
#330885=CARTESIAN_POINT('Ctrl Pts',(-0.727295466000056,12.2,4.19557816099999));
#330886=CARTESIAN_POINT('Ctrl Pts',(-0.727295466000056,5.2,4.19557816099999));
#330887=CARTESIAN_POINT('Ctrl Pts',(-0.727295466000056,2.2,4.19557816099999));
#330888=CARTESIAN_POINT('Ctrl Pts',(-0.728147055000056,12.2,4.19704331899998));
#330889=CARTESIAN_POINT('Ctrl Pts',(-0.728147055000056,5.2,4.19704331899998));
#330890=CARTESIAN_POINT('Ctrl Pts',(-0.728147055000056,2.2,4.19704331899998));
#330891=CARTESIAN_POINT('Ctrl Pts',(-0.729002563000056,12.2,4.19851134599998));
#330892=CARTESIAN_POINT('Ctrl Pts',(-0.729002563000056,5.2,4.19851134599998));
#330893=CARTESIAN_POINT('Ctrl Pts',(-0.729002563000056,2.2,4.19851134599998));
#330894=CARTESIAN_POINT('Ctrl Pts',(-0.729861992000057,12.2,4.19998222999999));
#330895=CARTESIAN_POINT('Ctrl Pts',(-0.729861992000057,5.2,4.19998222999999));
#330896=CARTESIAN_POINT('Ctrl Pts',(-0.729861992000057,2.2,4.19998222999999));
#330897=CARTESIAN_POINT('Ctrl Pts',(-0.730725346000056,12.2,4.20145595999998));
#330898=CARTESIAN_POINT('Ctrl Pts',(-0.730725346000056,5.2,4.20145595999998));
#330899=CARTESIAN_POINT('Ctrl Pts',(-0.730725346000056,2.2,4.20145595999998));
#330900=CARTESIAN_POINT('Ctrl Pts',(-0.731592631000056,12.2,4.20293252199999));
#330901=CARTESIAN_POINT('Ctrl Pts',(-0.731592631000056,5.2,4.20293252199999));
#330902=CARTESIAN_POINT('Ctrl Pts',(-0.731592631000056,2.2,4.20293252199999));
#330903=CARTESIAN_POINT('Ctrl Pts',(-0.732463849000055,12.2,4.20441190799998));
#330904=CARTESIAN_POINT('Ctrl Pts',(-0.732463849000055,5.2,4.20441190799998));
#330905=CARTESIAN_POINT('Ctrl Pts',(-0.732463849000055,2.2,4.20441190799998));
#330906=CARTESIAN_POINT('Ctrl Pts',(-0.733339005000057,12.2,4.20589410399998));
#330907=CARTESIAN_POINT('Ctrl Pts',(-0.733339005000057,5.2,4.20589410399998));
#330908=CARTESIAN_POINT('Ctrl Pts',(-0.733339005000057,2.2,4.20589410399998));
#330909=CARTESIAN_POINT('Ctrl Pts',(-0.734218101000056,12.2,4.20737909899999));
#330910=CARTESIAN_POINT('Ctrl Pts',(-0.734218101000056,5.2,4.20737909899999));
#330911=CARTESIAN_POINT('Ctrl Pts',(-0.734218101000056,2.2,4.20737909899999));
#330912=CARTESIAN_POINT('Ctrl Pts',(-0.735101143000056,12.2,4.20886688199998));
#330913=CARTESIAN_POINT('Ctrl Pts',(-0.735101143000056,5.2,4.20886688199998));
#330914=CARTESIAN_POINT('Ctrl Pts',(-0.735101143000056,2.2,4.20886688199998));
#330915=CARTESIAN_POINT('Ctrl Pts',(-0.735988134000056,12.2,4.21035744099999));
#330916=CARTESIAN_POINT('Ctrl Pts',(-0.735988134000056,5.2,4.21035744099999));
#330917=CARTESIAN_POINT('Ctrl Pts',(-0.735988134000056,2.2,4.21035744099999));
#330918=CARTESIAN_POINT('Ctrl Pts',(-0.736879077000056,12.2,4.21185076399999));
#330919=CARTESIAN_POINT('Ctrl Pts',(-0.736879077000056,5.2,4.21185076399999));
#330920=CARTESIAN_POINT('Ctrl Pts',(-0.736879077000056,2.2,4.21185076399999));
#330921=CARTESIAN_POINT('Ctrl Pts',(-0.737773977000057,12.2,4.21334684099998));
#330922=CARTESIAN_POINT('Ctrl Pts',(-0.737773977000057,5.2,4.21334684099998));
#330923=CARTESIAN_POINT('Ctrl Pts',(-0.737773977000057,2.2,4.21334684099998));
#330924=CARTESIAN_POINT('Ctrl Pts',(-0.738672837000056,12.2,4.21484565899998));
#330925=CARTESIAN_POINT('Ctrl Pts',(-0.738672837000056,5.2,4.21484565899998));
#330926=CARTESIAN_POINT('Ctrl Pts',(-0.738672837000056,2.2,4.21484565899998));
#330927=CARTESIAN_POINT('Ctrl Pts',(-0.739575662000057,12.2,4.21634720699998));
#330928=CARTESIAN_POINT('Ctrl Pts',(-0.739575662000057,5.2,4.21634720699998));
#330929=CARTESIAN_POINT('Ctrl Pts',(-0.739575662000057,2.2,4.21634720699998));
#330930=CARTESIAN_POINT('Ctrl Pts',(-0.740482454000055,12.2,4.21785147499998));
#330931=CARTESIAN_POINT('Ctrl Pts',(-0.740482454000055,5.2,4.21785147499998));
#330932=CARTESIAN_POINT('Ctrl Pts',(-0.740482454000055,2.2,4.21785147499998));
#330933=CARTESIAN_POINT('Ctrl Pts',(-0.741393217000056,12.2,4.21935844899998));
#330934=CARTESIAN_POINT('Ctrl Pts',(-0.741393217000056,5.2,4.21935844899998));
#330935=CARTESIAN_POINT('Ctrl Pts',(-0.741393217000056,2.2,4.21935844899998));
#330936=CARTESIAN_POINT('Ctrl Pts',(-0.742307956000056,12.2,4.22086811899998));
#330937=CARTESIAN_POINT('Ctrl Pts',(-0.742307956000056,5.2,4.22086811899998));
#330938=CARTESIAN_POINT('Ctrl Pts',(-0.742307956000056,2.2,4.22086811899998));
#330939=CARTESIAN_POINT('Ctrl Pts',(-0.743226673000056,12.2,4.22238047399999));
#330940=CARTESIAN_POINT('Ctrl Pts',(-0.743226673000056,5.2,4.22238047399999));
#330941=CARTESIAN_POINT('Ctrl Pts',(-0.743226673000056,2.2,4.22238047399999));
#330942=CARTESIAN_POINT('Ctrl Pts',(-0.744149371000056,12.2,4.22389550199998));
#330943=CARTESIAN_POINT('Ctrl Pts',(-0.744149371000056,5.2,4.22389550199998));
#330944=CARTESIAN_POINT('Ctrl Pts',(-0.744149371000056,2.2,4.22389550199998));
#330945=CARTESIAN_POINT('Ctrl Pts',(-0.745076057000055,12.2,4.22541319099999));
#330946=CARTESIAN_POINT('Ctrl Pts',(-0.745076057000055,5.2,4.22541319099999));
#330947=CARTESIAN_POINT('Ctrl Pts',(-0.745076057000055,2.2,4.22541319099999));
#330948=CARTESIAN_POINT('Ctrl Pts',(-0.746006730000056,12.2,4.22693353199998));
#330949=CARTESIAN_POINT('Ctrl Pts',(-0.746006730000056,5.2,4.22693353199998));
#330950=CARTESIAN_POINT('Ctrl Pts',(-0.746006730000056,2.2,4.22693353199998));
#330951=CARTESIAN_POINT('Ctrl Pts',(-0.746941397000055,12.2,4.22845651199999));
#330952=CARTESIAN_POINT('Ctrl Pts',(-0.746941397000055,5.2,4.22845651199999));
#330953=CARTESIAN_POINT('Ctrl Pts',(-0.746941397000055,2.2,4.22845651199999));
#330954=CARTESIAN_POINT('Ctrl Pts',(-0.747880061000057,12.2,4.22998211899999));
#330955=CARTESIAN_POINT('Ctrl Pts',(-0.747880061000057,5.2,4.22998211899999));
#330956=CARTESIAN_POINT('Ctrl Pts',(-0.747880061000057,2.2,4.22998211899999));
#330957=CARTESIAN_POINT('Ctrl Pts',(-0.748822725000055,12.2,4.23151034299998));
#330958=CARTESIAN_POINT('Ctrl Pts',(-0.748822725000055,5.2,4.23151034299998));
#330959=CARTESIAN_POINT('Ctrl Pts',(-0.748822725000055,2.2,4.23151034299998));
#330960=CARTESIAN_POINT('Ctrl Pts',(-0.749769392000056,12.2,4.23304117199999));
#330961=CARTESIAN_POINT('Ctrl Pts',(-0.749769392000056,5.2,4.23304117199999));
#330962=CARTESIAN_POINT('Ctrl Pts',(-0.749769392000056,2.2,4.23304117199999));
#330963=CARTESIAN_POINT('Ctrl Pts',(-0.750720065000056,12.2,4.23457459399999));
#330964=CARTESIAN_POINT('Ctrl Pts',(-0.750720065000056,5.2,4.23457459399999));
#330965=CARTESIAN_POINT('Ctrl Pts',(-0.750720065000056,2.2,4.23457459399999));
#330966=CARTESIAN_POINT('Ctrl Pts',(-0.751674750000056,12.2,4.23611059999998));
#330967=CARTESIAN_POINT('Ctrl Pts',(-0.751674750000056,5.2,4.23611059999998));
#330968=CARTESIAN_POINT('Ctrl Pts',(-0.751674750000056,2.2,4.23611059999998));
#330969=CARTESIAN_POINT('Ctrl Pts',(-0.752633448000056,12.2,4.23764917699998));
#330970=CARTESIAN_POINT('Ctrl Pts',(-0.752633448000056,5.2,4.23764917699998));
#330971=CARTESIAN_POINT('Ctrl Pts',(-0.752633448000056,2.2,4.23764917699998));
#330972=CARTESIAN_POINT('Ctrl Pts',(-0.753596163000055,12.2,4.23919031499998));
#330973=CARTESIAN_POINT('Ctrl Pts',(-0.753596163000055,5.2,4.23919031499998));
#330974=CARTESIAN_POINT('Ctrl Pts',(-0.753596163000055,2.2,4.23919031499998));
#330975=CARTESIAN_POINT('Ctrl Pts',(-0.754562898000056,12.2,4.24073399999998));
#330976=CARTESIAN_POINT('Ctrl Pts',(-0.754562898000056,5.2,4.24073399999998));
#330977=CARTESIAN_POINT('Ctrl Pts',(-0.754562898000056,2.2,4.24073399999998));
#330978=CARTESIAN_POINT('Ctrl Pts',(-0.755533657000056,12.2,4.24228022499998));
#330979=CARTESIAN_POINT('Ctrl Pts',(-0.755533657000056,5.2,4.24228022499998));
#330980=CARTESIAN_POINT('Ctrl Pts',(-0.755533657000056,2.2,4.24228022499998));
#330981=CARTESIAN_POINT('Ctrl Pts',(-0.756508444000056,12.2,4.24382897599998));
#330982=CARTESIAN_POINT('Ctrl Pts',(-0.756508444000056,5.2,4.24382897599998));
#330983=CARTESIAN_POINT('Ctrl Pts',(-0.756508444000056,2.2,4.24382897599998));
#330984=CARTESIAN_POINT('Ctrl Pts',(-0.757487261000056,12.2,4.24538024199999));
#330985=CARTESIAN_POINT('Ctrl Pts',(-0.757487261000056,5.2,4.24538024199999));
#330986=CARTESIAN_POINT('Ctrl Pts',(-0.757487261000056,2.2,4.24538024199999));
#330987=CARTESIAN_POINT('Ctrl Pts',(-0.758470112000056,12.2,4.24693401299999));
#330988=CARTESIAN_POINT('Ctrl Pts',(-0.758470112000056,5.2,4.24693401299999));
#330989=CARTESIAN_POINT('Ctrl Pts',(-0.758470112000056,2.2,4.24693401299999));
#330990=CARTESIAN_POINT('Ctrl Pts',(-0.759457000000056,12.2,4.24849027799999));
#330991=CARTESIAN_POINT('Ctrl Pts',(-0.759457000000056,5.2,4.24849027799999));
#330992=CARTESIAN_POINT('Ctrl Pts',(-0.759457000000056,2.2,4.24849027799999));
#330993=CARTESIAN_POINT('Ctrl Pts',(-0.760447928000056,12.2,4.25004902299998));
#330994=CARTESIAN_POINT('Ctrl Pts',(-0.760447928000056,5.2,4.25004902299998));
#330995=CARTESIAN_POINT('Ctrl Pts',(-0.760447928000056,2.2,4.25004902299998));
#330996=CARTESIAN_POINT('Ctrl Pts',(-0.761442900000056,12.2,4.25161024099998));
#330997=CARTESIAN_POINT('Ctrl Pts',(-0.761442900000056,5.2,4.25161024099998));
#330998=CARTESIAN_POINT('Ctrl Pts',(-0.761442900000056,2.2,4.25161024099998));
#330999=CARTESIAN_POINT('Ctrl Pts',(-0.762441918000055,12.2,4.25317391799998));
#331000=CARTESIAN_POINT('Ctrl Pts',(-0.762441918000055,5.2,4.25317391799998));
#331001=CARTESIAN_POINT('Ctrl Pts',(-0.762441918000055,2.2,4.25317391799998));
#331002=CARTESIAN_POINT('Ctrl Pts',(-0.763444986000056,12.2,4.25474004399998));
#331003=CARTESIAN_POINT('Ctrl Pts',(-0.763444986000056,5.2,4.25474004399998));
#331004=CARTESIAN_POINT('Ctrl Pts',(-0.763444986000056,2.2,4.25474004399998));
#331005=CARTESIAN_POINT('Ctrl Pts',(-0.764452107000055,12.2,4.25630860699999));
#331006=CARTESIAN_POINT('Ctrl Pts',(-0.764452107000055,5.2,4.25630860699999));
#331007=CARTESIAN_POINT('Ctrl Pts',(-0.764452107000055,2.2,4.25630860699999));
#331008=CARTESIAN_POINT('Ctrl Pts',(-0.765463285000055,12.2,4.25787959799998));
#331009=CARTESIAN_POINT('Ctrl Pts',(-0.765463285000055,5.2,4.25787959799998));
#331010=CARTESIAN_POINT('Ctrl Pts',(-0.765463285000055,2.2,4.25787959799998));
#331011=CARTESIAN_POINT('Ctrl Pts',(-0.766478522000057,12.2,4.25945300399999));
#331012=CARTESIAN_POINT('Ctrl Pts',(-0.766478522000057,5.2,4.25945300399999));
#331013=CARTESIAN_POINT('Ctrl Pts',(-0.766478522000057,2.2,4.25945300399999));
#331014=CARTESIAN_POINT('Ctrl Pts',(-0.767497821000056,12.2,4.26102881499999));
#331015=CARTESIAN_POINT('Ctrl Pts',(-0.767497821000056,5.2,4.26102881499999));
#331016=CARTESIAN_POINT('Ctrl Pts',(-0.767497821000056,2.2,4.26102881499999));
#331017=CARTESIAN_POINT('Ctrl Pts',(-0.768521186000056,12.2,4.26260701899999));
#331018=CARTESIAN_POINT('Ctrl Pts',(-0.768521186000056,5.2,4.26260701899999));
#331019=CARTESIAN_POINT('Ctrl Pts',(-0.768521186000056,2.2,4.26260701899999));
#331020=CARTESIAN_POINT('Ctrl Pts',(-0.769548620000055,12.2,4.26418760599999));
#331021=CARTESIAN_POINT('Ctrl Pts',(-0.769548620000055,5.2,4.26418760599999));
#331022=CARTESIAN_POINT('Ctrl Pts',(-0.769548620000055,2.2,4.26418760599999));
#331023=CARTESIAN_POINT('Ctrl Pts',(-0.770580124000055,12.2,4.26577056599999));
#331024=CARTESIAN_POINT('Ctrl Pts',(-0.770580124000055,5.2,4.26577056599999));
#331025=CARTESIAN_POINT('Ctrl Pts',(-0.770580124000055,2.2,4.26577056599999));
#331026=CARTESIAN_POINT('Ctrl Pts',(-0.771615704000055,12.2,4.26735588499999));
#331027=CARTESIAN_POINT('Ctrl Pts',(-0.771615704000055,5.2,4.26735588499999));
#331028=CARTESIAN_POINT('Ctrl Pts',(-0.771615704000055,2.2,4.26735588499999));
#331029=CARTESIAN_POINT('Ctrl Pts',(-0.772655361000056,12.2,4.26894355499999));
#331030=CARTESIAN_POINT('Ctrl Pts',(-0.772655361000056,5.2,4.26894355499999));
#331031=CARTESIAN_POINT('Ctrl Pts',(-0.772655361000056,2.2,4.26894355499999));
#331032=CARTESIAN_POINT('Ctrl Pts',(-0.773699100000057,12.2,4.27053356399998));
#331033=CARTESIAN_POINT('Ctrl Pts',(-0.773699100000057,5.2,4.27053356399998));
#331034=CARTESIAN_POINT('Ctrl Pts',(-0.773699100000057,2.2,4.27053356399998));
#331035=CARTESIAN_POINT('Ctrl Pts',(-0.774746921000055,12.2,4.27212589999999));
#331036=CARTESIAN_POINT('Ctrl Pts',(-0.774746921000055,5.2,4.27212589999999));
#331037=CARTESIAN_POINT('Ctrl Pts',(-0.774746921000055,2.2,4.27212589999999));
#331038=CARTESIAN_POINT('Ctrl Pts',(-0.775798829000056,12.2,4.27372055299998));
#331039=CARTESIAN_POINT('Ctrl Pts',(-0.775798829000056,5.2,4.27372055299998));
#331040=CARTESIAN_POINT('Ctrl Pts',(-0.775798829000056,2.2,4.27372055299998));
#331041=CARTESIAN_POINT('Ctrl Pts',(-0.776854827000056,12.2,4.27531751299998));
#331042=CARTESIAN_POINT('Ctrl Pts',(-0.776854827000056,5.2,4.27531751299998));
#331043=CARTESIAN_POINT('Ctrl Pts',(-0.776854827000056,2.2,4.27531751299998));
#331044=CARTESIAN_POINT('Ctrl Pts',(-0.777914917000055,12.2,4.27691676699999));
#331045=CARTESIAN_POINT('Ctrl Pts',(-0.777914917000055,5.2,4.27691676699999));
#331046=CARTESIAN_POINT('Ctrl Pts',(-0.777914917000055,2.2,4.27691676699999));
#331047=CARTESIAN_POINT('Ctrl Pts',(-0.778979103000056,12.2,4.27851830699999));
#331048=CARTESIAN_POINT('Ctrl Pts',(-0.778979103000056,5.2,4.27851830699999));
#331049=CARTESIAN_POINT('Ctrl Pts',(-0.778979103000056,2.2,4.27851830699999));
#331050=CARTESIAN_POINT('Ctrl Pts',(-0.780047386000057,12.2,4.28012212099999));
#331051=CARTESIAN_POINT('Ctrl Pts',(-0.780047386000057,5.2,4.28012212099999));
#331052=CARTESIAN_POINT('Ctrl Pts',(-0.780047386000057,2.2,4.28012212099999));
#331053=CARTESIAN_POINT('Ctrl Pts',(-0.781119770000055,12.2,4.28172819599999));
#331054=CARTESIAN_POINT('Ctrl Pts',(-0.781119770000055,5.2,4.28172819599999));
#331055=CARTESIAN_POINT('Ctrl Pts',(-0.781119770000055,2.2,4.28172819599999));
#331056=CARTESIAN_POINT('Ctrl Pts',(-0.782196258000055,12.2,4.28333652299998));
#331057=CARTESIAN_POINT('Ctrl Pts',(-0.782196258000055,5.2,4.28333652299998));
#331058=CARTESIAN_POINT('Ctrl Pts',(-0.782196258000055,2.2,4.28333652299998));
#331059=CARTESIAN_POINT('Ctrl Pts',(-0.783276853000056,12.2,4.28494709199998));
#331060=CARTESIAN_POINT('Ctrl Pts',(-0.783276853000056,5.2,4.28494709199998));
#331061=CARTESIAN_POINT('Ctrl Pts',(-0.783276853000056,2.2,4.28494709199998));
#331062=CARTESIAN_POINT('Ctrl Pts',(-0.784361558000055,12.2,4.28655989199999));
#331063=CARTESIAN_POINT('Ctrl Pts',(-0.784361558000055,5.2,4.28655989199999));
#331064=CARTESIAN_POINT('Ctrl Pts',(-0.784361558000055,2.2,4.28655989199999));
#331065=CARTESIAN_POINT('Ctrl Pts',(-0.785450374000056,12.2,4.28817490999998));
#331066=CARTESIAN_POINT('Ctrl Pts',(-0.785450374000056,5.2,4.28817490999998));
#331067=CARTESIAN_POINT('Ctrl Pts',(-0.785450374000056,2.2,4.28817490999998));
#331068=CARTESIAN_POINT('Ctrl Pts',(-0.786543305000055,12.2,4.28979213799998));
#331069=CARTESIAN_POINT('Ctrl Pts',(-0.786543305000055,5.2,4.28979213799998));
#331070=CARTESIAN_POINT('Ctrl Pts',(-0.786543305000055,2.2,4.28979213799998));
#331071=CARTESIAN_POINT('Ctrl Pts',(-0.787640354000055,12.2,4.29141156299998));
#331072=CARTESIAN_POINT('Ctrl Pts',(-0.787640354000055,5.2,4.29141156299998));
#331073=CARTESIAN_POINT('Ctrl Pts',(-0.787640354000055,2.2,4.29141156299998));
#331074=CARTESIAN_POINT('Ctrl Pts',(-0.788741523000055,12.2,4.29303317699999));
#331075=CARTESIAN_POINT('Ctrl Pts',(-0.788741523000055,5.2,4.29303317699999));
#331076=CARTESIAN_POINT('Ctrl Pts',(-0.788741523000055,2.2,4.29303317699999));
#331077=CARTESIAN_POINT('Ctrl Pts',(-0.789846815000056,12.2,4.29465696599999));
#331078=CARTESIAN_POINT('Ctrl Pts',(-0.789846815000056,5.2,4.29465696599999));
#331079=CARTESIAN_POINT('Ctrl Pts',(-0.789846815000056,2.2,4.29465696599999));
#331080=CARTESIAN_POINT('Ctrl Pts',(-0.790956233000056,12.2,4.29628292199999));
#331081=CARTESIAN_POINT('Ctrl Pts',(-0.790956233000056,5.2,4.29628292199999));
#331082=CARTESIAN_POINT('Ctrl Pts',(-0.790956233000056,2.2,4.29628292199999));
#331083=CARTESIAN_POINT('Ctrl Pts',(-0.792069779000055,12.2,4.29791103299999));
#331084=CARTESIAN_POINT('Ctrl Pts',(-0.792069779000055,5.2,4.29791103299999));
#331085=CARTESIAN_POINT('Ctrl Pts',(-0.792069779000055,2.2,4.29791103299999));
#331086=CARTESIAN_POINT('Ctrl Pts',(-0.793187456000056,12.2,4.29954128799999));
#331087=CARTESIAN_POINT('Ctrl Pts',(-0.793187456000056,5.2,4.29954128799999));
#331088=CARTESIAN_POINT('Ctrl Pts',(-0.793187456000056,2.2,4.29954128799999));
#331089=CARTESIAN_POINT('Ctrl Pts',(-0.794309268000056,12.2,4.30117367699999));
#331090=CARTESIAN_POINT('Ctrl Pts',(-0.794309268000056,5.2,4.30117367699999));
#331091=CARTESIAN_POINT('Ctrl Pts',(-0.794309268000056,2.2,4.30117367699999));
#331092=CARTESIAN_POINT('Ctrl Pts',(-0.795435215000057,12.2,4.30280818899998));
#331093=CARTESIAN_POINT('Ctrl Pts',(-0.795435215000057,5.2,4.30280818899998));
#331094=CARTESIAN_POINT('Ctrl Pts',(-0.795435215000057,2.2,4.30280818899998));
#331095=CARTESIAN_POINT('Ctrl Pts',(-0.796565301000056,12.2,4.30444481399999));
#331096=CARTESIAN_POINT('Ctrl Pts',(-0.796565301000056,5.2,4.30444481399999));
#331097=CARTESIAN_POINT('Ctrl Pts',(-0.796565301000056,2.2,4.30444481399999));
#331098=CARTESIAN_POINT('Ctrl Pts',(-0.797699528000055,12.2,4.30608354099999));
#331099=CARTESIAN_POINT('Ctrl Pts',(-0.797699528000055,5.2,4.30608354099999));
#331100=CARTESIAN_POINT('Ctrl Pts',(-0.797699528000055,2.2,4.30608354099999));
#331101=CARTESIAN_POINT('Ctrl Pts',(-0.798837899000056,12.2,4.30772435899998));
#331102=CARTESIAN_POINT('Ctrl Pts',(-0.798837899000056,5.2,4.30772435899998));
#331103=CARTESIAN_POINT('Ctrl Pts',(-0.798837899000056,2.2,4.30772435899998));
#331104=CARTESIAN_POINT('Ctrl Pts',(-0.799980417000056,12.2,4.30936725799998));
#331105=CARTESIAN_POINT('Ctrl Pts',(-0.799980417000056,5.2,4.30936725799998));
#331106=CARTESIAN_POINT('Ctrl Pts',(-0.799980417000056,2.2,4.30936725799998));
#331107=CARTESIAN_POINT('Ctrl Pts',(-0.801127083000056,12.2,4.31101222699999));
#331108=CARTESIAN_POINT('Ctrl Pts',(-0.801127083000056,5.2,4.31101222699999));
#331109=CARTESIAN_POINT('Ctrl Pts',(-0.801127083000056,2.2,4.31101222699999));
#331110=CARTESIAN_POINT('Ctrl Pts',(-0.802277901000057,12.2,4.31265925599998));
#331111=CARTESIAN_POINT('Ctrl Pts',(-0.802277901000057,5.2,4.31265925599998));
#331112=CARTESIAN_POINT('Ctrl Pts',(-0.802277901000057,2.2,4.31265925599998));
#331113=CARTESIAN_POINT('Ctrl Pts',(-0.803432873000055,12.2,4.31430833399999));
#331114=CARTESIAN_POINT('Ctrl Pts',(-0.803432873000055,5.2,4.31430833399999));
#331115=CARTESIAN_POINT('Ctrl Pts',(-0.803432873000055,2.2,4.31430833399999));
#331116=CARTESIAN_POINT('Ctrl Pts',(-0.804592000000056,12.2,4.31595944899998));
#331117=CARTESIAN_POINT('Ctrl Pts',(-0.804592000000056,5.2,4.31595944899998));
#331118=CARTESIAN_POINT('Ctrl Pts',(-0.804592000000056,2.2,4.31595944899998));
#331119=CARTESIAN_POINT('Ctrl Pts',(-0.805755288000055,12.2,4.31761259299999));
#331120=CARTESIAN_POINT('Ctrl Pts',(-0.805755288000055,5.2,4.31761259299999));
#331121=CARTESIAN_POINT('Ctrl Pts',(-0.805755288000055,2.2,4.31761259299999));
#331122=CARTESIAN_POINT('Ctrl Pts',(-0.806922735000055,12.2,4.31926775499999));
#331123=CARTESIAN_POINT('Ctrl Pts',(-0.806922735000055,5.2,4.31926775499999));
#331124=CARTESIAN_POINT('Ctrl Pts',(-0.806922735000055,2.2,4.31926775499999));
#331125=CARTESIAN_POINT('Ctrl Pts',(-0.808094347000056,12.2,4.32092492399998));
#331126=CARTESIAN_POINT('Ctrl Pts',(-0.808094347000056,5.2,4.32092492399998));
#331127=CARTESIAN_POINT('Ctrl Pts',(-0.808094347000056,2.2,4.32092492399998));
#331128=CARTESIAN_POINT('Ctrl Pts',(-0.809270125000056,12.2,4.32258408799999));
#331129=CARTESIAN_POINT('Ctrl Pts',(-0.809270125000056,5.2,4.32258408799999));
#331130=CARTESIAN_POINT('Ctrl Pts',(-0.809270125000056,2.2,4.32258408799999));
#331131=CARTESIAN_POINT('Ctrl Pts',(-0.810450070000056,12.2,4.32424523999998));
#331132=CARTESIAN_POINT('Ctrl Pts',(-0.810450070000056,5.2,4.32424523999998));
#331133=CARTESIAN_POINT('Ctrl Pts',(-0.810450070000056,2.2,4.32424523999998));
#331134=CARTESIAN_POINT('Ctrl Pts',(-0.811634187000055,12.2,4.32590836599999));
#331135=CARTESIAN_POINT('Ctrl Pts',(-0.811634187000055,5.2,4.32590836599999));
#331136=CARTESIAN_POINT('Ctrl Pts',(-0.811634187000055,2.2,4.32590836599999));
#331137=CARTESIAN_POINT('Ctrl Pts',(-0.812822475000056,12.2,4.32757345699999));
#331138=CARTESIAN_POINT('Ctrl Pts',(-0.812822475000056,5.2,4.32757345699999));
#331139=CARTESIAN_POINT('Ctrl Pts',(-0.812822475000056,2.2,4.32757345699999));
#331140=CARTESIAN_POINT('Ctrl Pts',(-0.814014940000056,12.2,4.32924050299999));
#331141=CARTESIAN_POINT('Ctrl Pts',(-0.814014940000056,5.2,4.32924050299999));
#331142=CARTESIAN_POINT('Ctrl Pts',(-0.814014940000056,2.2,4.32924050299999));
#331143=CARTESIAN_POINT('Ctrl Pts',(-0.815211583000056,12.2,4.33090949299999));
#331144=CARTESIAN_POINT('Ctrl Pts',(-0.815211583000056,5.2,4.33090949299999));
#331145=CARTESIAN_POINT('Ctrl Pts',(-0.815211583000056,2.2,4.33090949299999));
#331146=CARTESIAN_POINT('Ctrl Pts',(-0.816412405000057,12.2,4.33258041699998));
#331147=CARTESIAN_POINT('Ctrl Pts',(-0.816412405000057,5.2,4.33258041699998));
#331148=CARTESIAN_POINT('Ctrl Pts',(-0.816412405000057,2.2,4.33258041699998));
#331149=CARTESIAN_POINT('Ctrl Pts',(-0.817617408000055,12.2,4.33425326399998));
#331150=CARTESIAN_POINT('Ctrl Pts',(-0.817617408000055,5.2,4.33425326399998));
#331151=CARTESIAN_POINT('Ctrl Pts',(-0.817617408000055,2.2,4.33425326399998));
#331152=CARTESIAN_POINT('Ctrl Pts',(-0.818826596000056,12.2,4.33592802399998));
#331153=CARTESIAN_POINT('Ctrl Pts',(-0.818826596000056,5.2,4.33592802399998));
#331154=CARTESIAN_POINT('Ctrl Pts',(-0.818826596000056,2.2,4.33592802399998));
#331155=CARTESIAN_POINT('Ctrl Pts',(-0.820039971000056,12.2,4.33760468699998));
#331156=CARTESIAN_POINT('Ctrl Pts',(-0.820039971000056,5.2,4.33760468699998));
#331157=CARTESIAN_POINT('Ctrl Pts',(-0.820039971000056,2.2,4.33760468699998));
#331158=CARTESIAN_POINT('Ctrl Pts',(-0.821257535000056,12.2,4.33928324199999));
#331159=CARTESIAN_POINT('Ctrl Pts',(-0.821257535000056,5.2,4.33928324199999));
#331160=CARTESIAN_POINT('Ctrl Pts',(-0.821257535000056,2.2,4.33928324199999));
#331161=CARTESIAN_POINT('Ctrl Pts',(-0.822479289000055,12.2,4.34096367899999));
#331162=CARTESIAN_POINT('Ctrl Pts',(-0.822479289000055,5.2,4.34096367899999));
#331163=CARTESIAN_POINT('Ctrl Pts',(-0.822479289000055,2.2,4.34096367899999));
#331164=CARTESIAN_POINT('Ctrl Pts',(-0.823705236000055,12.2,4.34264598699999));
#331165=CARTESIAN_POINT('Ctrl Pts',(-0.823705236000055,5.2,4.34264598699999));
#331166=CARTESIAN_POINT('Ctrl Pts',(-0.823705236000055,2.2,4.34264598699999));
#331167=CARTESIAN_POINT('Ctrl Pts',(-0.824935379000056,12.2,4.34433015699998));
#331168=CARTESIAN_POINT('Ctrl Pts',(-0.824935379000056,5.2,4.34433015699998));
#331169=CARTESIAN_POINT('Ctrl Pts',(-0.824935379000056,2.2,4.34433015699998));
#331170=CARTESIAN_POINT('Ctrl Pts',(-0.826169719000056,12.2,4.34601617799999));
#331171=CARTESIAN_POINT('Ctrl Pts',(-0.826169719000056,5.2,4.34601617799999));
#331172=CARTESIAN_POINT('Ctrl Pts',(-0.826169719000056,2.2,4.34601617799999));
#331173=CARTESIAN_POINT('Ctrl Pts',(-0.827408258000055,12.2,4.34770403899999));
#331174=CARTESIAN_POINT('Ctrl Pts',(-0.827408258000055,5.2,4.34770403899999));
#331175=CARTESIAN_POINT('Ctrl Pts',(-0.827408258000055,2.2,4.34770403899999));
#331176=CARTESIAN_POINT('Ctrl Pts',(-0.828650998000056,12.2,4.34939372999998));
#331177=CARTESIAN_POINT('Ctrl Pts',(-0.828650998000056,5.2,4.34939372999998));
#331178=CARTESIAN_POINT('Ctrl Pts',(-0.828650998000056,2.2,4.34939372999998));
#331179=CARTESIAN_POINT('Ctrl Pts',(-0.829897943000055,12.2,4.35108524199999));
#331180=CARTESIAN_POINT('Ctrl Pts',(-0.829897943000055,5.2,4.35108524199999));
#331181=CARTESIAN_POINT('Ctrl Pts',(-0.829897943000055,2.2,4.35108524199999));
#331182=CARTESIAN_POINT('Ctrl Pts',(-0.831149093000055,12.2,4.35277856399999));
#331183=CARTESIAN_POINT('Ctrl Pts',(-0.831149093000055,5.2,4.35277856399999));
#331184=CARTESIAN_POINT('Ctrl Pts',(-0.831149093000055,2.2,4.35277856399999));
#331185=CARTESIAN_POINT('Ctrl Pts',(-0.832404451000055,12.2,4.35447368499998));
#331186=CARTESIAN_POINT('Ctrl Pts',(-0.832404451000055,5.2,4.35447368499998));
#331187=CARTESIAN_POINT('Ctrl Pts',(-0.832404451000055,2.2,4.35447368499998));
#331188=CARTESIAN_POINT('Ctrl Pts',(-0.833664018000055,12.2,4.35617059399998));
#331189=CARTESIAN_POINT('Ctrl Pts',(-0.833664018000055,5.2,4.35617059399998));
#331190=CARTESIAN_POINT('Ctrl Pts',(-0.833664018000055,2.2,4.35617059399998));
#331191=CARTESIAN_POINT('Ctrl Pts',(-0.834927797000056,12.2,4.35786928399998));
#331192=CARTESIAN_POINT('Ctrl Pts',(-0.834927797000056,5.2,4.35786928399998));
#331193=CARTESIAN_POINT('Ctrl Pts',(-0.834927797000056,2.2,4.35786928399998));
#331194=CARTESIAN_POINT('Ctrl Pts',(-0.836195790000056,12.2,4.35956974299998));
#331195=CARTESIAN_POINT('Ctrl Pts',(-0.836195790000056,5.2,4.35956974299998));
#331196=CARTESIAN_POINT('Ctrl Pts',(-0.836195790000056,2.2,4.35956974299998));
#331197=CARTESIAN_POINT('Ctrl Pts',(-0.837467999000056,12.2,4.36127195899999));
#331198=CARTESIAN_POINT('Ctrl Pts',(-0.837467999000056,5.2,4.36127195899999));
#331199=CARTESIAN_POINT('Ctrl Pts',(-0.837467999000056,2.2,4.36127195899999));
#331200=CARTESIAN_POINT('Ctrl Pts',(-0.838744426000056,12.2,4.36297592499999));
#331201=CARTESIAN_POINT('Ctrl Pts',(-0.838744426000056,5.2,4.36297592499999));
#331202=CARTESIAN_POINT('Ctrl Pts',(-0.838744426000056,2.2,4.36297592499999));
#331203=CARTESIAN_POINT('Ctrl Pts',(-0.840025071000056,12.2,4.36468162899998));
#331204=CARTESIAN_POINT('Ctrl Pts',(-0.840025071000056,5.2,4.36468162899998));
#331205=CARTESIAN_POINT('Ctrl Pts',(-0.840025071000056,2.2,4.36468162899998));
#331206=CARTESIAN_POINT('Ctrl Pts',(-0.841309938000055,12.2,4.36638906199998));
#331207=CARTESIAN_POINT('Ctrl Pts',(-0.841309938000055,5.2,4.36638906199998));
#331208=CARTESIAN_POINT('Ctrl Pts',(-0.841309938000055,2.2,4.36638906199998));
#331209=CARTESIAN_POINT('Ctrl Pts',(-0.842599029000055,12.2,4.36809821199999));
#331210=CARTESIAN_POINT('Ctrl Pts',(-0.842599029000055,5.2,4.36809821199999));
#331211=CARTESIAN_POINT('Ctrl Pts',(-0.842599029000055,2.2,4.36809821199999));
#331212=CARTESIAN_POINT('Ctrl Pts',(-0.843892345000056,12.2,4.36980906999998));
#331213=CARTESIAN_POINT('Ctrl Pts',(-0.843892345000056,5.2,4.36980906999998));
#331214=CARTESIAN_POINT('Ctrl Pts',(-0.843892345000056,2.2,4.36980906999998));
#331215=CARTESIAN_POINT('Ctrl Pts',(-0.845189888000055,12.2,4.37152162599999));
#331216=CARTESIAN_POINT('Ctrl Pts',(-0.845189888000055,5.2,4.37152162599999));
#331217=CARTESIAN_POINT('Ctrl Pts',(-0.845189888000055,2.2,4.37152162599999));
#331218=CARTESIAN_POINT('Ctrl Pts',(-0.846491661000056,12.2,4.37323586999998));
#331219=CARTESIAN_POINT('Ctrl Pts',(-0.846491661000056,5.2,4.37323586999998));
#331220=CARTESIAN_POINT('Ctrl Pts',(-0.846491661000056,2.2,4.37323586999998));
#331221=CARTESIAN_POINT('Ctrl Pts',(-0.847797664000056,12.2,4.37495179199999));
#331222=CARTESIAN_POINT('Ctrl Pts',(-0.847797664000056,5.2,4.37495179199999));
#331223=CARTESIAN_POINT('Ctrl Pts',(-0.847797664000056,2.2,4.37495179199999));
#331224=CARTESIAN_POINT('Ctrl Pts',(-0.849107900000057,12.2,4.37666937999998));
#331225=CARTESIAN_POINT('Ctrl Pts',(-0.849107900000057,5.2,4.37666937999998));
#331226=CARTESIAN_POINT('Ctrl Pts',(-0.849107900000057,2.2,4.37666937999998));
#331227=CARTESIAN_POINT('Ctrl Pts',(-0.850422370000056,12.2,4.37838862699999));
#331228=CARTESIAN_POINT('Ctrl Pts',(-0.850422370000056,5.2,4.37838862699999));
#331229=CARTESIAN_POINT('Ctrl Pts',(-0.850422370000056,2.2,4.37838862699999));
#331230=CARTESIAN_POINT('Ctrl Pts',(-0.851741076000057,12.2,4.38010951999999));
#331231=CARTESIAN_POINT('Ctrl Pts',(-0.851741076000057,5.2,4.38010951999999));
#331232=CARTESIAN_POINT('Ctrl Pts',(-0.851741076000057,2.2,4.38010951999999));
#331233=CARTESIAN_POINT('Ctrl Pts',(-0.853064021000056,12.2,4.38183205199999));
#331234=CARTESIAN_POINT('Ctrl Pts',(-0.853064021000056,5.2,4.38183205199999));
#331235=CARTESIAN_POINT('Ctrl Pts',(-0.853064021000056,2.2,4.38183205199999));
#331236=CARTESIAN_POINT('Ctrl Pts',(-0.854391206000056,12.2,4.38355620999998));
#331237=CARTESIAN_POINT('Ctrl Pts',(-0.854391206000056,5.2,4.38355620999998));
#331238=CARTESIAN_POINT('Ctrl Pts',(-0.854391206000056,2.2,4.38355620999998));
#331239=CARTESIAN_POINT('Ctrl Pts',(-0.855722632000055,12.2,4.38528198599998));
#331240=CARTESIAN_POINT('Ctrl Pts',(-0.855722632000055,5.2,4.38528198599998));
#331241=CARTESIAN_POINT('Ctrl Pts',(-0.855722632000055,2.2,4.38528198599998));
#331242=CARTESIAN_POINT('Ctrl Pts',(-0.857058301000055,12.2,4.38700936899998));
#331243=CARTESIAN_POINT('Ctrl Pts',(-0.857058301000055,5.2,4.38700936899998));
#331244=CARTESIAN_POINT('Ctrl Pts',(-0.857058301000055,2.2,4.38700936899998));
#331245=CARTESIAN_POINT('Ctrl Pts',(-0.858398215000056,12.2,4.38873834899999));
#331246=CARTESIAN_POINT('Ctrl Pts',(-0.858398215000056,5.2,4.38873834899999));
#331247=CARTESIAN_POINT('Ctrl Pts',(-0.858398215000056,2.2,4.38873834899999));
#331248=CARTESIAN_POINT('Ctrl Pts',(-0.859742376000057,12.2,4.39046891699999));
#331249=CARTESIAN_POINT('Ctrl Pts',(-0.859742376000057,5.2,4.39046891699999));
#331250=CARTESIAN_POINT('Ctrl Pts',(-0.859742376000057,2.2,4.39046891699999));
#331251=CARTESIAN_POINT('Ctrl Pts',(-0.861090785000057,12.2,4.39220106199999));
#331252=CARTESIAN_POINT('Ctrl Pts',(-0.861090785000057,5.2,4.39220106199999));
#331253=CARTESIAN_POINT('Ctrl Pts',(-0.861090785000057,2.2,4.39220106199999));
#331254=CARTESIAN_POINT('Ctrl Pts',(-0.862443445000055,12.2,4.39393477399998));
#331255=CARTESIAN_POINT('Ctrl Pts',(-0.862443445000055,5.2,4.39393477399998));
#331256=CARTESIAN_POINT('Ctrl Pts',(-0.862443445000055,2.2,4.39393477399998));
#331257=CARTESIAN_POINT('Ctrl Pts',(-0.863800356000055,12.2,4.39567004399999));
#331258=CARTESIAN_POINT('Ctrl Pts',(-0.863800356000055,5.2,4.39567004399999));
#331259=CARTESIAN_POINT('Ctrl Pts',(-0.863800356000055,2.2,4.39567004399999));
#331260=CARTESIAN_POINT('Ctrl Pts',(-0.865161520000056,12.2,4.39740686199999));
#331261=CARTESIAN_POINT('Ctrl Pts',(-0.865161520000056,5.2,4.39740686199999));
#331262=CARTESIAN_POINT('Ctrl Pts',(-0.865161520000056,2.2,4.39740686199999));
#331263=CARTESIAN_POINT('Ctrl Pts',(-0.866526939000056,12.2,4.39914521599999));
#331264=CARTESIAN_POINT('Ctrl Pts',(-0.866526939000056,5.2,4.39914521599999));
#331265=CARTESIAN_POINT('Ctrl Pts',(-0.866526939000056,2.2,4.39914521599999));
#331266=CARTESIAN_POINT('Ctrl Pts',(-0.867896616000056,12.2,4.40088509899999));
#331267=CARTESIAN_POINT('Ctrl Pts',(-0.867896616000056,5.2,4.40088509899999));
#331268=CARTESIAN_POINT('Ctrl Pts',(-0.867896616000056,2.2,4.40088509899999));
#331269=CARTESIAN_POINT('Ctrl Pts',(-0.869270549000056,12.2,4.40262649999998));
#331270=CARTESIAN_POINT('Ctrl Pts',(-0.869270549000056,5.2,4.40262649999998));
#331271=CARTESIAN_POINT('Ctrl Pts',(-0.869270549000056,2.2,4.40262649999998));
#331272=CARTESIAN_POINT('Ctrl Pts',(-0.870648743000055,12.2,4.40436940799999));
#331273=CARTESIAN_POINT('Ctrl Pts',(-0.870648743000055,5.2,4.40436940799999));
#331274=CARTESIAN_POINT('Ctrl Pts',(-0.870648743000055,2.2,4.40436940799999));
#331275=CARTESIAN_POINT('Ctrl Pts',(-0.872031197000057,12.2,4.40611381399999));
#331276=CARTESIAN_POINT('Ctrl Pts',(-0.872031197000057,5.2,4.40611381399999));
#331277=CARTESIAN_POINT('Ctrl Pts',(-0.872031197000057,2.2,4.40611381399999));
#331278=CARTESIAN_POINT('Ctrl Pts',(-0.873417915000055,12.2,4.40785970899999));
#331279=CARTESIAN_POINT('Ctrl Pts',(-0.873417915000055,5.2,4.40785970899999));
#331280=CARTESIAN_POINT('Ctrl Pts',(-0.873417915000055,2.2,4.40785970899999));
#331281=CARTESIAN_POINT('Ctrl Pts',(-0.874808897000056,12.2,4.40960708199999));
#331282=CARTESIAN_POINT('Ctrl Pts',(-0.874808897000056,5.2,4.40960708199999));
#331283=CARTESIAN_POINT('Ctrl Pts',(-0.874808897000056,2.2,4.40960708199999));
#331284=CARTESIAN_POINT('Ctrl Pts',(-0.876204144000056,12.2,4.41135592299998));
#331285=CARTESIAN_POINT('Ctrl Pts',(-0.876204144000056,5.2,4.41135592299998));
#331286=CARTESIAN_POINT('Ctrl Pts',(-0.876204144000056,2.2,4.41135592299998));
#331287=CARTESIAN_POINT('Ctrl Pts',(-0.877603659000057,12.2,4.41310622299999));
#331288=CARTESIAN_POINT('Ctrl Pts',(-0.877603659000057,5.2,4.41310622299999));
#331289=CARTESIAN_POINT('Ctrl Pts',(-0.877603659000057,2.2,4.41310622299999));
#331290=CARTESIAN_POINT('Ctrl Pts',(-0.879007443000056,12.2,4.41485797199999));
#331291=CARTESIAN_POINT('Ctrl Pts',(-0.879007443000056,5.2,4.41485797199999));
#331292=CARTESIAN_POINT('Ctrl Pts',(-0.879007443000056,2.2,4.41485797199999));
#331293=CARTESIAN_POINT('Ctrl Pts',(-0.880415495000056,12.2,4.41661115999998));
#331294=CARTESIAN_POINT('Ctrl Pts',(-0.880415495000056,5.2,4.41661115999998));
#331295=CARTESIAN_POINT('Ctrl Pts',(-0.880415495000056,2.2,4.41661115999998));
#331296=CARTESIAN_POINT('Ctrl Pts',(-0.881827821000056,12.2,4.41836577599998));
#331297=CARTESIAN_POINT('Ctrl Pts',(-0.881827821000056,5.2,4.41836577599998));
#331298=CARTESIAN_POINT('Ctrl Pts',(-0.881827821000056,2.2,4.41836577599998));
#331299=CARTESIAN_POINT('Ctrl Pts',(-0.883244419000055,12.2,4.42012181299998));
#331300=CARTESIAN_POINT('Ctrl Pts',(-0.883244419000055,5.2,4.42012181299998));
#331301=CARTESIAN_POINT('Ctrl Pts',(-0.883244419000055,2.2,4.42012181299998));
#331302=CARTESIAN_POINT('Ctrl Pts',(-0.884665291000056,12.2,4.42187925899999));
#331303=CARTESIAN_POINT('Ctrl Pts',(-0.884665291000056,5.2,4.42187925899999));
#331304=CARTESIAN_POINT('Ctrl Pts',(-0.884665291000056,2.2,4.42187925899999));
#331305=CARTESIAN_POINT('Ctrl Pts',(-0.886090440000055,12.2,4.42363810499998));
#331306=CARTESIAN_POINT('Ctrl Pts',(-0.886090440000055,5.2,4.42363810499998));
#331307=CARTESIAN_POINT('Ctrl Pts',(-0.886090440000055,2.2,4.42363810499998));
#331308=CARTESIAN_POINT('Ctrl Pts',(-0.887519865000056,12.2,4.42539834199999));
#331309=CARTESIAN_POINT('Ctrl Pts',(-0.887519865000056,5.2,4.42539834199999));
#331310=CARTESIAN_POINT('Ctrl Pts',(-0.887519865000056,2.2,4.42539834199999));
#331311=CARTESIAN_POINT('Ctrl Pts',(-0.888953570000056,12.2,4.42715995899999));
#331312=CARTESIAN_POINT('Ctrl Pts',(-0.888953570000056,5.2,4.42715995899999));
#331313=CARTESIAN_POINT('Ctrl Pts',(-0.888953570000056,2.2,4.42715995899999));
#331314=CARTESIAN_POINT('Ctrl Pts',(-0.890391553000055,12.2,4.42892294599999));
#331315=CARTESIAN_POINT('Ctrl Pts',(-0.890391553000055,5.2,4.42892294599999));
#331316=CARTESIAN_POINT('Ctrl Pts',(-0.890391553000055,2.2,4.42892294599999));
#331317=CARTESIAN_POINT('Ctrl Pts',(-0.891833819000055,12.2,4.43068729499998));
#331318=CARTESIAN_POINT('Ctrl Pts',(-0.891833819000055,5.2,4.43068729499998));
#331319=CARTESIAN_POINT('Ctrl Pts',(-0.891833819000055,2.2,4.43068729499998));
#331320=CARTESIAN_POINT('Ctrl Pts',(-0.893280366000055,12.2,4.43245299399998));
#331321=CARTESIAN_POINT('Ctrl Pts',(-0.893280366000055,5.2,4.43245299399998));
#331322=CARTESIAN_POINT('Ctrl Pts',(-0.893280366000055,2.2,4.43245299399998));
#331323=CARTESIAN_POINT('Ctrl Pts',(-0.894731198000055,12.2,4.43422003599999));
#331324=CARTESIAN_POINT('Ctrl Pts',(-0.894731198000055,5.2,4.43422003599999));
#331325=CARTESIAN_POINT('Ctrl Pts',(-0.894731198000055,2.2,4.43422003599999));
#331326=CARTESIAN_POINT('Ctrl Pts',(-0.896186315000056,12.2,4.43598840999999));
#331327=CARTESIAN_POINT('Ctrl Pts',(-0.896186315000056,5.2,4.43598840999999));
#331328=CARTESIAN_POINT('Ctrl Pts',(-0.896186315000056,2.2,4.43598840999999));
#331329=CARTESIAN_POINT('Ctrl Pts',(-0.897645718000056,12.2,4.43775810499999));
#331330=CARTESIAN_POINT('Ctrl Pts',(-0.897645718000056,5.2,4.43775810499999));
#331331=CARTESIAN_POINT('Ctrl Pts',(-0.897645718000056,2.2,4.43775810499999));
#331332=CARTESIAN_POINT('Ctrl Pts',(-0.899109409000056,12.2,4.43952911299998));
#331333=CARTESIAN_POINT('Ctrl Pts',(-0.899109409000056,5.2,4.43952911299998));
#331334=CARTESIAN_POINT('Ctrl Pts',(-0.899109409000056,2.2,4.43952911299998));
#331335=CARTESIAN_POINT('Ctrl Pts',(-0.900577389000056,12.2,4.44130142499999));
#331336=CARTESIAN_POINT('Ctrl Pts',(-0.900577389000056,5.2,4.44130142499999));
#331337=CARTESIAN_POINT('Ctrl Pts',(-0.900577389000056,2.2,4.44130142499999));
#331338=CARTESIAN_POINT('Ctrl Pts',(-0.902049660000056,12.2,4.44307502999998));
#331339=CARTESIAN_POINT('Ctrl Pts',(-0.902049660000056,5.2,4.44307502999998));
#331340=CARTESIAN_POINT('Ctrl Pts',(-0.902049660000056,2.2,4.44307502999998));
#331341=CARTESIAN_POINT('Ctrl Pts',(-0.903526221000056,12.2,4.44484991899999));
#331342=CARTESIAN_POINT('Ctrl Pts',(-0.903526221000056,5.2,4.44484991899999));
#331343=CARTESIAN_POINT('Ctrl Pts',(-0.903526221000056,2.2,4.44484991899999));
#331344=CARTESIAN_POINT('Ctrl Pts',(-0.905007075000055,12.2,4.44662608099998));
#331345=CARTESIAN_POINT('Ctrl Pts',(-0.905007075000055,5.2,4.44662608099998));
#331346=CARTESIAN_POINT('Ctrl Pts',(-0.905007075000055,2.2,4.44662608099998));
#331347=CARTESIAN_POINT('Ctrl Pts',(-0.906492222000056,12.2,4.44840350899998));
#331348=CARTESIAN_POINT('Ctrl Pts',(-0.906492222000056,5.2,4.44840350899998));
#331349=CARTESIAN_POINT('Ctrl Pts',(-0.906492222000056,2.2,4.44840350899998));
#331350=CARTESIAN_POINT('Ctrl Pts',(-0.907981665000056,12.2,4.45018219199999));
#331351=CARTESIAN_POINT('Ctrl Pts',(-0.907981665000056,5.2,4.45018219199999));
#331352=CARTESIAN_POINT('Ctrl Pts',(-0.907981665000056,2.2,4.45018219199999));
#331353=CARTESIAN_POINT('Ctrl Pts',(-0.909475403000056,12.2,4.45196211899999));
#331354=CARTESIAN_POINT('Ctrl Pts',(-0.909475403000056,5.2,4.45196211899999));
#331355=CARTESIAN_POINT('Ctrl Pts',(-0.909475403000056,2.2,4.45196211899999));
#331356=CARTESIAN_POINT('Ctrl Pts',(-0.910973439000056,12.2,4.45374328299999));
#331357=CARTESIAN_POINT('Ctrl Pts',(-0.910973439000056,5.2,4.45374328299999));
#331358=CARTESIAN_POINT('Ctrl Pts',(-0.910973439000056,2.2,4.45374328299999));
#331359=CARTESIAN_POINT('Ctrl Pts',(-0.912475773000055,12.2,4.45552567399999));
#331360=CARTESIAN_POINT('Ctrl Pts',(-0.912475773000055,5.2,4.45552567399999));
#331361=CARTESIAN_POINT('Ctrl Pts',(-0.912475773000055,2.2,4.45552567399999));
#331362=CARTESIAN_POINT('Ctrl Pts',(-0.913982407000056,12.2,4.45730928099999));
#331363=CARTESIAN_POINT('Ctrl Pts',(-0.913982407000056,5.2,4.45730928099999));
#331364=CARTESIAN_POINT('Ctrl Pts',(-0.913982407000056,2.2,4.45730928099999));
#331365=CARTESIAN_POINT('Ctrl Pts',(-0.915493341000057,12.2,4.45909409499999));
#331366=CARTESIAN_POINT('Ctrl Pts',(-0.915493341000057,5.2,4.45909409499999));
#331367=CARTESIAN_POINT('Ctrl Pts',(-0.915493341000057,2.2,4.45909409499999));
#331368=CARTESIAN_POINT('Ctrl Pts',(-0.917008577000056,12.2,4.46088010699999));
#331369=CARTESIAN_POINT('Ctrl Pts',(-0.917008577000056,5.2,4.46088010699999));
#331370=CARTESIAN_POINT('Ctrl Pts',(-0.917008577000056,2.2,4.46088010699999));
#331371=CARTESIAN_POINT('Ctrl Pts',(-0.918528116000056,12.2,4.46266730699998));
#331372=CARTESIAN_POINT('Ctrl Pts',(-0.918528116000056,5.2,4.46266730699998));
#331373=CARTESIAN_POINT('Ctrl Pts',(-0.918528116000056,2.2,4.46266730699998));
#331374=CARTESIAN_POINT('Ctrl Pts',(-0.920051957000056,12.2,4.46445568599999));
#331375=CARTESIAN_POINT('Ctrl Pts',(-0.920051957000056,5.2,4.46445568599999));
#331376=CARTESIAN_POINT('Ctrl Pts',(-0.920051957000056,2.2,4.46445568599999));
#331377=CARTESIAN_POINT('Ctrl Pts',(-0.921580104000055,12.2,4.46624523499998));
#331378=CARTESIAN_POINT('Ctrl Pts',(-0.921580104000055,5.2,4.46624523499998));
#331379=CARTESIAN_POINT('Ctrl Pts',(-0.921580104000055,2.2,4.46624523499998));
#331380=CARTESIAN_POINT('Ctrl Pts',(-0.923112557000056,12.2,4.46803594299999));
#331381=CARTESIAN_POINT('Ctrl Pts',(-0.923112557000056,5.2,4.46803594299999));
#331382=CARTESIAN_POINT('Ctrl Pts',(-0.923112557000056,2.2,4.46803594299999));
#331383=CARTESIAN_POINT('Ctrl Pts',(-0.924649317000057,12.2,4.46982780199999));
#331384=CARTESIAN_POINT('Ctrl Pts',(-0.924649317000057,5.2,4.46982780199999));
#331385=CARTESIAN_POINT('Ctrl Pts',(-0.924649317000057,2.2,4.46982780199999));
#331386=CARTESIAN_POINT('Ctrl Pts',(-0.926190383000056,12.2,4.47162080099999));
#331387=CARTESIAN_POINT('Ctrl Pts',(-0.926190383000056,5.2,4.47162080099999));
#331388=CARTESIAN_POINT('Ctrl Pts',(-0.926190383000056,2.2,4.47162080099999));
#331389=CARTESIAN_POINT('Ctrl Pts',(-0.927735760000056,12.2,4.47341493299999));
#331390=CARTESIAN_POINT('Ctrl Pts',(-0.927735760000056,5.2,4.47341493299999));
#331391=CARTESIAN_POINT('Ctrl Pts',(-0.927735760000056,2.2,4.47341493299999));
#331392=CARTESIAN_POINT('Ctrl Pts',(-0.929285445000056,12.2,4.47521018599998));
#331393=CARTESIAN_POINT('Ctrl Pts',(-0.929285445000056,5.2,4.47521018599998));
#331394=CARTESIAN_POINT('Ctrl Pts',(-0.929285445000056,2.2,4.47521018599998));
#331395=CARTESIAN_POINT('Ctrl Pts',(-0.930839442000057,12.2,4.47700655099998));
#331396=CARTESIAN_POINT('Ctrl Pts',(-0.930839442000057,5.2,4.47700655099998));
#331397=CARTESIAN_POINT('Ctrl Pts',(-0.930839442000057,2.2,4.47700655099998));
#331398=CARTESIAN_POINT('Ctrl Pts',(-0.932397750000057,12.2,4.47880401999999));
#331399=CARTESIAN_POINT('Ctrl Pts',(-0.932397750000057,5.2,4.47880401999999));
#331400=CARTESIAN_POINT('Ctrl Pts',(-0.932397750000057,2.2,4.47880401999999));
#331401=CARTESIAN_POINT('Ctrl Pts',(-0.933960370000056,12.2,4.48060258399998));
#331402=CARTESIAN_POINT('Ctrl Pts',(-0.933960370000056,5.2,4.48060258399998));
#331403=CARTESIAN_POINT('Ctrl Pts',(-0.933960370000056,2.2,4.48060258399998));
#331404=CARTESIAN_POINT('Ctrl Pts',(-0.935527304000056,12.2,4.48240223099998));
#331405=CARTESIAN_POINT('Ctrl Pts',(-0.935527304000056,5.2,4.48240223099998));
#331406=CARTESIAN_POINT('Ctrl Pts',(-0.935527304000056,2.2,4.48240223099998));
#331407=CARTESIAN_POINT('Ctrl Pts',(-0.937098553000055,12.2,4.48420295299999));
#331408=CARTESIAN_POINT('Ctrl Pts',(-0.937098553000055,5.2,4.48420295299999));
#331409=CARTESIAN_POINT('Ctrl Pts',(-0.937098553000055,2.2,4.48420295299999));
#331410=CARTESIAN_POINT('Ctrl Pts',(-0.938674116000057,12.2,4.48600474199999));
#331411=CARTESIAN_POINT('Ctrl Pts',(-0.938674116000057,5.2,4.48600474199999));
#331412=CARTESIAN_POINT('Ctrl Pts',(-0.938674116000057,2.2,4.48600474199999));
#331413=CARTESIAN_POINT('Ctrl Pts',(-0.940253996000056,12.2,4.48780758699999));
#331414=CARTESIAN_POINT('Ctrl Pts',(-0.940253996000056,5.2,4.48780758699999));
#331415=CARTESIAN_POINT('Ctrl Pts',(-0.940253996000056,2.2,4.48780758699999));
#331416=CARTESIAN_POINT('Ctrl Pts',(-0.941838193000055,12.2,4.48961147899999));
#331417=CARTESIAN_POINT('Ctrl Pts',(-0.941838193000055,5.2,4.48961147899999));
#331418=CARTESIAN_POINT('Ctrl Pts',(-0.941838193000055,2.2,4.48961147899999));
#331419=CARTESIAN_POINT('Ctrl Pts',(-0.943426707000056,12.2,4.49141640799999));
#331420=CARTESIAN_POINT('Ctrl Pts',(-0.943426707000056,5.2,4.49141640799999));
#331421=CARTESIAN_POINT('Ctrl Pts',(-0.943426707000056,2.2,4.49141640799999));
#331422=CARTESIAN_POINT('Ctrl Pts',(-0.945019539000055,12.2,4.49322236599999));
#331423=CARTESIAN_POINT('Ctrl Pts',(-0.945019539000055,5.2,4.49322236599999));
#331424=CARTESIAN_POINT('Ctrl Pts',(-0.945019539000055,2.2,4.49322236599999));
#331425=CARTESIAN_POINT('Ctrl Pts',(-0.946616692000056,12.2,4.49502934399998));
#331426=CARTESIAN_POINT('Ctrl Pts',(-0.946616692000056,5.2,4.49502934399998));
#331427=CARTESIAN_POINT('Ctrl Pts',(-0.946616692000056,2.2,4.49502934399998));
#331428=CARTESIAN_POINT('Ctrl Pts',(-0.948218165000055,12.2,4.49683733099998));
#331429=CARTESIAN_POINT('Ctrl Pts',(-0.948218165000055,5.2,4.49683733099998));
#331430=CARTESIAN_POINT('Ctrl Pts',(-0.948218165000055,2.2,4.49683733099998));
#331431=CARTESIAN_POINT('Ctrl Pts',(-0.949823959000057,12.2,4.49864631999999));
#331432=CARTESIAN_POINT('Ctrl Pts',(-0.949823959000057,5.2,4.49864631999999));
#331433=CARTESIAN_POINT('Ctrl Pts',(-0.949823959000057,2.2,4.49864631999999));
#331434=CARTESIAN_POINT('Ctrl Pts',(-0.951434074000056,12.2,4.50045629899999));
#331435=CARTESIAN_POINT('Ctrl Pts',(-0.951434074000056,5.2,4.50045629899999));
#331436=CARTESIAN_POINT('Ctrl Pts',(-0.951434074000056,2.2,4.50045629899999));
#331437=CARTESIAN_POINT('Ctrl Pts',(-0.953048512000055,12.2,4.50226725999999));
#331438=CARTESIAN_POINT('Ctrl Pts',(-0.953048512000055,5.2,4.50226725999999));
#331439=CARTESIAN_POINT('Ctrl Pts',(-0.953048512000055,2.2,4.50226725999999));
#331440=CARTESIAN_POINT('Ctrl Pts',(-0.954667273000057,12.2,4.50407919399999));
#331441=CARTESIAN_POINT('Ctrl Pts',(-0.954667273000057,5.2,4.50407919399999));
#331442=CARTESIAN_POINT('Ctrl Pts',(-0.954667273000057,2.2,4.50407919399999));
#331443=CARTESIAN_POINT('Ctrl Pts',(-0.956290358000055,12.2,4.50589209199999));
#331444=CARTESIAN_POINT('Ctrl Pts',(-0.956290358000055,5.2,4.50589209199999));
#331445=CARTESIAN_POINT('Ctrl Pts',(-0.956290358000055,2.2,4.50589209199999));
#331446=CARTESIAN_POINT('Ctrl Pts',(-0.957917768000056,12.2,4.50770594399999));
#331447=CARTESIAN_POINT('Ctrl Pts',(-0.957917768000056,5.2,4.50770594399999));
#331448=CARTESIAN_POINT('Ctrl Pts',(-0.957917768000056,2.2,4.50770594399999));
#331449=CARTESIAN_POINT('Ctrl Pts',(-0.959549503000057,12.2,4.50952074099998));
#331450=CARTESIAN_POINT('Ctrl Pts',(-0.959549503000057,5.2,4.50952074099998));
#331451=CARTESIAN_POINT('Ctrl Pts',(-0.959549503000057,2.2,4.50952074099998));
#331452=CARTESIAN_POINT('Ctrl Pts',(-0.961185565000056,12.2,4.51133647499999));
#331453=CARTESIAN_POINT('Ctrl Pts',(-0.961185565000056,5.2,4.51133647499999));
#331454=CARTESIAN_POINT('Ctrl Pts',(-0.961185565000056,2.2,4.51133647499999));
#331455=CARTESIAN_POINT('Ctrl Pts',(-0.962825953000056,12.2,4.51315313599999));
#331456=CARTESIAN_POINT('Ctrl Pts',(-0.962825953000056,5.2,4.51315313599999));
#331457=CARTESIAN_POINT('Ctrl Pts',(-0.962825953000056,2.2,4.51315313599999));
#331458=CARTESIAN_POINT('Ctrl Pts',(-0.964470669000056,12.2,4.51497071299999));
#331459=CARTESIAN_POINT('Ctrl Pts',(-0.964470669000056,5.2,4.51497071299999));
#331460=CARTESIAN_POINT('Ctrl Pts',(-0.964470669000056,2.2,4.51497071299999));
#331461=CARTESIAN_POINT('Ctrl Pts',(-0.966119713000057,12.2,4.51678919899998));
#331462=CARTESIAN_POINT('Ctrl Pts',(-0.966119713000057,5.2,4.51678919899998));
#331463=CARTESIAN_POINT('Ctrl Pts',(-0.966119713000057,2.2,4.51678919899998));
#331464=CARTESIAN_POINT('Ctrl Pts',(-0.967773085000055,12.2,4.51860858499998));
#331465=CARTESIAN_POINT('Ctrl Pts',(-0.967773085000055,5.2,4.51860858499998));
#331466=CARTESIAN_POINT('Ctrl Pts',(-0.967773085000055,2.2,4.51860858499998));
#331467=CARTESIAN_POINT('Ctrl Pts',(-0.969430788000055,12.2,4.52042885999998));
#331468=CARTESIAN_POINT('Ctrl Pts',(-0.969430788000055,5.2,4.52042885999998));
#331469=CARTESIAN_POINT('Ctrl Pts',(-0.969430788000055,2.2,4.52042885999998));
#331470=CARTESIAN_POINT('Ctrl Pts',(-0.971092819000056,12.2,4.52225001699999));
#331471=CARTESIAN_POINT('Ctrl Pts',(-0.971092819000056,5.2,4.52225001699999));
#331472=CARTESIAN_POINT('Ctrl Pts',(-0.971092819000056,2.2,4.52225001699999));
#331473=CARTESIAN_POINT('Ctrl Pts',(-0.972759181000056,12.2,4.52407204499998));
#331474=CARTESIAN_POINT('Ctrl Pts',(-0.972759181000056,5.2,4.52407204499998));
#331475=CARTESIAN_POINT('Ctrl Pts',(-0.972759181000056,2.2,4.52407204499998));
#331476=CARTESIAN_POINT('Ctrl Pts',(-0.974429875000055,12.2,4.52589493699998));
#331477=CARTESIAN_POINT('Ctrl Pts',(-0.974429875000055,5.2,4.52589493699998));
#331478=CARTESIAN_POINT('Ctrl Pts',(-0.974429875000055,2.2,4.52589493699998));
#331479=CARTESIAN_POINT('Ctrl Pts',(-0.976104901000056,12.2,4.52771868199999));
#331480=CARTESIAN_POINT('Ctrl Pts',(-0.976104901000056,5.2,4.52771868199999));
#331481=CARTESIAN_POINT('Ctrl Pts',(-0.976104901000056,2.2,4.52771868199999));
#331482=CARTESIAN_POINT('Ctrl Pts',(-0.977784258000056,12.2,4.52954327099999));
#331483=CARTESIAN_POINT('Ctrl Pts',(-0.977784258000056,5.2,4.52954327099999));
#331484=CARTESIAN_POINT('Ctrl Pts',(-0.977784258000056,2.2,4.52954327099999));
#331485=CARTESIAN_POINT('Ctrl Pts',(-0.979467948000057,12.2,4.53136869699998));
#331486=CARTESIAN_POINT('Ctrl Pts',(-0.979467948000057,5.2,4.53136869699998));
#331487=CARTESIAN_POINT('Ctrl Pts',(-0.979467948000057,2.2,4.53136869699998));
#331488=CARTESIAN_POINT('Ctrl Pts',(-0.981155972000056,12.2,4.53319494799998));
#331489=CARTESIAN_POINT('Ctrl Pts',(-0.981155972000056,5.2,4.53319494799998));
#331490=CARTESIAN_POINT('Ctrl Pts',(-0.981155972000056,2.2,4.53319494799998));
#331491=CARTESIAN_POINT('Ctrl Pts',(-0.982848330000056,12.2,4.53502201599999));
#331492=CARTESIAN_POINT('Ctrl Pts',(-0.982848330000056,5.2,4.53502201599999));
#331493=CARTESIAN_POINT('Ctrl Pts',(-0.982848330000056,2.2,4.53502201599999));
#331494=CARTESIAN_POINT('Ctrl Pts',(-0.984545022000055,12.2,4.53684989399999));
#331495=CARTESIAN_POINT('Ctrl Pts',(-0.984545022000055,5.2,4.53684989399999));
#331496=CARTESIAN_POINT('Ctrl Pts',(-0.984545022000055,2.2,4.53684989399999));
#331497=CARTESIAN_POINT('Ctrl Pts',(-0.986246049000057,12.2,4.53867856999998));
#331498=CARTESIAN_POINT('Ctrl Pts',(-0.986246049000057,5.2,4.53867856999998));
#331499=CARTESIAN_POINT('Ctrl Pts',(-0.986246049000057,2.2,4.53867856999998));
#331500=CARTESIAN_POINT('Ctrl Pts',(-0.987951411000055,12.2,4.54050803599999));
#331501=CARTESIAN_POINT('Ctrl Pts',(-0.987951411000055,5.2,4.54050803599999));
#331502=CARTESIAN_POINT('Ctrl Pts',(-0.987951411000055,2.2,4.54050803599999));
#331503=CARTESIAN_POINT('Ctrl Pts',(-0.989661108000056,12.2,4.54233828499999));
#331504=CARTESIAN_POINT('Ctrl Pts',(-0.989661108000056,5.2,4.54233828499999));
#331505=CARTESIAN_POINT('Ctrl Pts',(-0.989661108000056,2.2,4.54233828499999));
#331506=CARTESIAN_POINT('Ctrl Pts',(-0.991375143000056,12.2,4.54416930499999));
#331507=CARTESIAN_POINT('Ctrl Pts',(-0.991375143000056,5.2,4.54416930499999));
#331508=CARTESIAN_POINT('Ctrl Pts',(-0.991375143000056,2.2,4.54416930499999));
#331509=CARTESIAN_POINT('Ctrl Pts',(-0.993093514000056,12.2,4.54600108699999));
#331510=CARTESIAN_POINT('Ctrl Pts',(-0.993093514000056,5.2,4.54600108699999));
#331511=CARTESIAN_POINT('Ctrl Pts',(-0.993093514000056,2.2,4.54600108699999));
#331512=CARTESIAN_POINT('Ctrl Pts',(-0.994816221000056,12.2,4.54783362499998));
#331513=CARTESIAN_POINT('Ctrl Pts',(-0.994816221000056,5.2,4.54783362499998));
#331514=CARTESIAN_POINT('Ctrl Pts',(-0.994816221000056,2.2,4.54783362499998));
#331515=CARTESIAN_POINT('Ctrl Pts',(-0.996543267000056,12.2,4.54966690799999));
#331516=CARTESIAN_POINT('Ctrl Pts',(-0.996543267000056,5.2,4.54966690799999));
#331517=CARTESIAN_POINT('Ctrl Pts',(-0.996543267000056,2.2,4.54966690799999));
#331518=CARTESIAN_POINT('Ctrl Pts',(-0.998274650000056,12.2,4.55150092699999));
#331519=CARTESIAN_POINT('Ctrl Pts',(-0.998274650000056,5.2,4.55150092699999));
#331520=CARTESIAN_POINT('Ctrl Pts',(-0.998274650000056,2.2,4.55150092699999));
#331521=CARTESIAN_POINT('Ctrl Pts',(-1.00001037100006,12.2,4.55333567299999));
#331522=CARTESIAN_POINT('Ctrl Pts',(-1.00001037100006,5.2,4.55333567299999));
#331523=CARTESIAN_POINT('Ctrl Pts',(-1.00001037100006,2.2,4.55333567299999));
#331524=CARTESIAN_POINT('Ctrl Pts',(-1.00175043200006,12.2,4.55517113699998));
#331525=CARTESIAN_POINT('Ctrl Pts',(-1.00175043200006,5.2,4.55517113699998));
#331526=CARTESIAN_POINT('Ctrl Pts',(-1.00175043200006,2.2,4.55517113699998));
#331527=CARTESIAN_POINT('Ctrl Pts',(-1.00349483100006,12.2,4.55700731099999));
#331528=CARTESIAN_POINT('Ctrl Pts',(-1.00349483100006,5.2,4.55700731099999));
#331529=CARTESIAN_POINT('Ctrl Pts',(-1.00349483100006,2.2,4.55700731099999));
#331530=CARTESIAN_POINT('Ctrl Pts',(-1.00524357000006,12.2,4.55884418699998));
#331531=CARTESIAN_POINT('Ctrl Pts',(-1.00524357000006,5.2,4.55884418699998));
#331532=CARTESIAN_POINT('Ctrl Pts',(-1.00524357000006,2.2,4.55884418699998));
#331533=CARTESIAN_POINT('Ctrl Pts',(-1.00699664800006,12.2,4.56068175199999));
#331534=CARTESIAN_POINT('Ctrl Pts',(-1.00699664800006,5.2,4.56068175199999));
#331535=CARTESIAN_POINT('Ctrl Pts',(-1.00699664800006,2.2,4.56068175199999));
#331536=CARTESIAN_POINT('Ctrl Pts',(-1.00875406700006,12.2,4.56252000199999));
#331537=CARTESIAN_POINT('Ctrl Pts',(-1.00875406700006,5.2,4.56252000199999));
#331538=CARTESIAN_POINT('Ctrl Pts',(-1.00875406700006,2.2,4.56252000199999));
#331539=CARTESIAN_POINT('Ctrl Pts',(-1.01051582600006,12.2,4.56435892399998));
#331540=CARTESIAN_POINT('Ctrl Pts',(-1.01051582600006,5.2,4.56435892399998));
#331541=CARTESIAN_POINT('Ctrl Pts',(-1.01051582600006,2.2,4.56435892399998));
#331542=CARTESIAN_POINT('Ctrl Pts',(-1.01228192600006,12.2,4.56619851199999));
#331543=CARTESIAN_POINT('Ctrl Pts',(-1.01228192600006,5.2,4.56619851199999));
#331544=CARTESIAN_POINT('Ctrl Pts',(-1.01228192600006,2.2,4.56619851199999));
#331545=CARTESIAN_POINT('Ctrl Pts',(-1.01405236700006,12.2,4.56803875599999));
#331546=CARTESIAN_POINT('Ctrl Pts',(-1.01405236700006,5.2,4.56803875599999));
#331547=CARTESIAN_POINT('Ctrl Pts',(-1.01405236700006,2.2,4.56803875599999));
#331548=CARTESIAN_POINT('Ctrl Pts',(-1.01582714800006,12.2,4.56987964799998));
#331549=CARTESIAN_POINT('Ctrl Pts',(-1.01582714800006,5.2,4.56987964799998));
#331550=CARTESIAN_POINT('Ctrl Pts',(-1.01582714800006,2.2,4.56987964799998));
#331551=CARTESIAN_POINT('Ctrl Pts',(-1.01760627200006,12.2,4.57172117699999));
#331552=CARTESIAN_POINT('Ctrl Pts',(-1.01760627200006,5.2,4.57172117699999));
#331553=CARTESIAN_POINT('Ctrl Pts',(-1.01760627200006,2.2,4.57172117699999));
#331554=CARTESIAN_POINT('Ctrl Pts',(-1.01938973700006,12.2,4.57356333599999));
#331555=CARTESIAN_POINT('Ctrl Pts',(-1.01938973700006,5.2,4.57356333599999));
#331556=CARTESIAN_POINT('Ctrl Pts',(-1.01938973700006,2.2,4.57356333599999));
#331557=CARTESIAN_POINT('Ctrl Pts',(-1.02117754400005,12.2,4.57540611499999));
#331558=CARTESIAN_POINT('Ctrl Pts',(-1.02117754400005,5.2,4.57540611499999));
#331559=CARTESIAN_POINT('Ctrl Pts',(-1.02117754400005,2.2,4.57540611499999));
#331560=CARTESIAN_POINT('Ctrl Pts',(-1.02296969300006,12.2,4.57724950599999));
#331561=CARTESIAN_POINT('Ctrl Pts',(-1.02296969300006,5.2,4.57724950599999));
#331562=CARTESIAN_POINT('Ctrl Pts',(-1.02296969300006,2.2,4.57724950599999));
#331563=CARTESIAN_POINT('Ctrl Pts',(-1.02476618500006,12.2,4.57909349999999));
#331564=CARTESIAN_POINT('Ctrl Pts',(-1.02476618500006,5.2,4.57909349999999));
#331565=CARTESIAN_POINT('Ctrl Pts',(-1.02476618500006,2.2,4.57909349999999));
#331566=CARTESIAN_POINT('Ctrl Pts',(-1.02656701900006,12.2,4.58093808899999));
#331567=CARTESIAN_POINT('Ctrl Pts',(-1.02656701900006,5.2,4.58093808899999));
#331568=CARTESIAN_POINT('Ctrl Pts',(-1.02656701900006,2.2,4.58093808899999));
#331569=CARTESIAN_POINT('Ctrl Pts',(-1.02837219600006,12.2,4.58278326299999));
#331570=CARTESIAN_POINT('Ctrl Pts',(-1.02837219600006,5.2,4.58278326299999));
#331571=CARTESIAN_POINT('Ctrl Pts',(-1.02837219600006,2.2,4.58278326299999));
#331572=CARTESIAN_POINT('Ctrl Pts',(-1.03018171600006,12.2,4.58462901499999));
#331573=CARTESIAN_POINT('Ctrl Pts',(-1.03018171600006,5.2,4.58462901499999));
#331574=CARTESIAN_POINT('Ctrl Pts',(-1.03018171600006,2.2,4.58462901499999));
#331575=CARTESIAN_POINT('Ctrl Pts',(-1.03199558000005,12.2,4.58647533399999));
#331576=CARTESIAN_POINT('Ctrl Pts',(-1.03199558000005,5.2,4.58647533399999));
#331577=CARTESIAN_POINT('Ctrl Pts',(-1.03199558000005,2.2,4.58647533399999));
#331578=CARTESIAN_POINT('Ctrl Pts',(-1.03381378600006,12.2,4.58832221299998));
#331579=CARTESIAN_POINT('Ctrl Pts',(-1.03381378600006,5.2,4.58832221299998));
#331580=CARTESIAN_POINT('Ctrl Pts',(-1.03381378600006,2.2,4.58832221299998));
#331581=CARTESIAN_POINT('Ctrl Pts',(-1.03563633600006,12.2,4.59016964299998));
#331582=CARTESIAN_POINT('Ctrl Pts',(-1.03563633600006,5.2,4.59016964299998));
#331583=CARTESIAN_POINT('Ctrl Pts',(-1.03563633600006,2.2,4.59016964299998));
#331584=CARTESIAN_POINT('Ctrl Pts',(-1.03746322900006,12.2,4.59201761299998));
#331585=CARTESIAN_POINT('Ctrl Pts',(-1.03746322900006,5.2,4.59201761299998));
#331586=CARTESIAN_POINT('Ctrl Pts',(-1.03746322900006,2.2,4.59201761299998));
#331587=CARTESIAN_POINT('Ctrl Pts',(-1.03929446800006,12.2,4.59386611499998));
#331588=CARTESIAN_POINT('Ctrl Pts',(-1.03929446800006,5.2,4.59386611499998));
#331589=CARTESIAN_POINT('Ctrl Pts',(-1.03929446800006,2.2,4.59386611499998));
#331590=CARTESIAN_POINT('Ctrl Pts',(-1.04113004900006,12.2,4.59571514099999));
#331591=CARTESIAN_POINT('Ctrl Pts',(-1.04113004900006,5.2,4.59571514099999));
#331592=CARTESIAN_POINT('Ctrl Pts',(-1.04113004900006,2.2,4.59571514099999));
#331593=CARTESIAN_POINT('Ctrl Pts',(-1.04296997400006,12.2,4.59756468099998));
#331594=CARTESIAN_POINT('Ctrl Pts',(-1.04296997400006,5.2,4.59756468099998));
#331595=CARTESIAN_POINT('Ctrl Pts',(-1.04296997400006,2.2,4.59756468099998));
#331596=CARTESIAN_POINT('Ctrl Pts',(-1.04481424200006,12.2,4.59941472799999));
#331597=CARTESIAN_POINT('Ctrl Pts',(-1.04481424200006,5.2,4.59941472799999));
#331598=CARTESIAN_POINT('Ctrl Pts',(-1.04481424200006,2.2,4.59941472799999));
#331599=CARTESIAN_POINT('Ctrl Pts',(-1.04666285500006,12.2,4.60126527399999));
#331600=CARTESIAN_POINT('Ctrl Pts',(-1.04666285500006,5.2,4.60126527399999));
#331601=CARTESIAN_POINT('Ctrl Pts',(-1.04666285500006,2.2,4.60126527399999));
#331602=CARTESIAN_POINT('Ctrl Pts',(-1.04851581200006,12.2,4.60311631099999));
#331603=CARTESIAN_POINT('Ctrl Pts',(-1.04851581200006,5.2,4.60311631099999));
#331604=CARTESIAN_POINT('Ctrl Pts',(-1.04851581200006,2.2,4.60311631099999));
#331605=CARTESIAN_POINT('Ctrl Pts',(-1.05037311400006,12.2,4.60496783199999));
#331606=CARTESIAN_POINT('Ctrl Pts',(-1.05037311400006,5.2,4.60496783199999));
#331607=CARTESIAN_POINT('Ctrl Pts',(-1.05037311400006,2.2,4.60496783199999));
#331608=CARTESIAN_POINT('Ctrl Pts',(-1.05223475900006,12.2,4.60681982699998));
#331609=CARTESIAN_POINT('Ctrl Pts',(-1.05223475900006,5.2,4.60681982699998));
#331610=CARTESIAN_POINT('Ctrl Pts',(-1.05223475900006,2.2,4.60681982699998));
#331611=CARTESIAN_POINT('Ctrl Pts',(-1.05410074900006,12.2,4.60867228699998));
#331612=CARTESIAN_POINT('Ctrl Pts',(-1.05410074900006,5.2,4.60867228699998));
#331613=CARTESIAN_POINT('Ctrl Pts',(-1.05410074900006,2.2,4.60867228699998));
#331614=CARTESIAN_POINT('Ctrl Pts',(-1.05597108200006,12.2,4.61052519999999));
#331615=CARTESIAN_POINT('Ctrl Pts',(-1.05597108200006,5.2,4.61052519999999));
#331616=CARTESIAN_POINT('Ctrl Pts',(-1.05597108200006,2.2,4.61052519999999));
#331617=CARTESIAN_POINT('Ctrl Pts',(-1.05784576100006,12.2,4.61237855699999));
#331618=CARTESIAN_POINT('Ctrl Pts',(-1.05784576100006,5.2,4.61237855699999));
#331619=CARTESIAN_POINT('Ctrl Pts',(-1.05784576100006,2.2,4.61237855699999));
#331620=CARTESIAN_POINT('Ctrl Pts',(-1.05972478300006,12.2,4.61423234699998));
#331621=CARTESIAN_POINT('Ctrl Pts',(-1.05972478300006,5.2,4.61423234699998));
#331622=CARTESIAN_POINT('Ctrl Pts',(-1.05972478300006,2.2,4.61423234699998));
#331623=CARTESIAN_POINT('Ctrl Pts',(-1.06160814900006,12.2,4.61608656099998));
#331624=CARTESIAN_POINT('Ctrl Pts',(-1.06160814900006,5.2,4.61608656099998));
#331625=CARTESIAN_POINT('Ctrl Pts',(-1.06160814900006,2.2,4.61608656099998));
#331626=CARTESIAN_POINT('Ctrl Pts',(-1.06349586000006,12.2,4.61794118999999));
#331627=CARTESIAN_POINT('Ctrl Pts',(-1.06349586000006,5.2,4.61794118999999));
#331628=CARTESIAN_POINT('Ctrl Pts',(-1.06349586000006,2.2,4.61794118999999));
#331629=CARTESIAN_POINT('Ctrl Pts',(-1.06538791400006,12.2,4.61979622599999));
#331630=CARTESIAN_POINT('Ctrl Pts',(-1.06538791400006,5.2,4.61979622599999));
#331631=CARTESIAN_POINT('Ctrl Pts',(-1.06538791400006,2.2,4.61979622599999));
#331632=CARTESIAN_POINT('Ctrl Pts',(-1.06728431400006,12.2,4.62165166799998));
#331633=CARTESIAN_POINT('Ctrl Pts',(-1.06728431400006,5.2,4.62165166799998));
#331634=CARTESIAN_POINT('Ctrl Pts',(-1.06728431400006,2.2,4.62165166799998));
#331635=CARTESIAN_POINT('Ctrl Pts',(-1.06918505607982,12.2,4.62350751207786));
#331636=CARTESIAN_POINT('Ctrl Pts',(-1.06918505607982,5.2,4.62350751207786));
#331637=CARTESIAN_POINT('Ctrl Pts',(-1.06918505607982,2.2,4.62350751207786));
#331638=CARTESIAN_POINT('Ctrl Pts',(-1.07070912515995,12.2,4.62499250815578));
#331639=CARTESIAN_POINT('Ctrl Pts',(-1.07070912515995,5.2,4.62499250815578));
#331640=CARTESIAN_POINT('Ctrl Pts',(-1.07070912515995,2.2,4.62499250815578));
#331641=CARTESIAN_POINT('Ctrl Pts',(-1.07185413124031,12.2,4.62610643623372));
#331642=CARTESIAN_POINT('Ctrl Pts',(-1.07185413124031,5.2,4.62610643623372));
#331643=CARTESIAN_POINT('Ctrl Pts',(-1.07185413124031,2.2,4.62610643623372));
#331644=CARTESIAN_POINT('Ctrl Pts',(-1.07261833832076,12.2,4.62684913431167));
#331645=CARTESIAN_POINT('Ctrl Pts',(-1.07261833832076,5.2,4.62684913431167));
#331646=CARTESIAN_POINT('Ctrl Pts',(-1.07261833832076,2.2,4.62684913431167));
#331647=CARTESIAN_POINT('Ctrl Pts',(-1.07300065800006,12.2,4.62722050399999));
#331648=CARTESIAN_POINT('Ctrl Pts',(-1.07300065800006,5.2,4.62722050399999));
#331649=CARTESIAN_POINT('Ctrl Pts',(-1.07300065800006,2.2,4.62722050399999));
#331650=CARTESIAN_POINT('Origin',(-5.66300478732629E-14,15.2,-1.77635683940025E-14));
#331651=CARTESIAN_POINT('',(-0.00378600900005522,2.2,3.62499802299999));
#331652=CARTESIAN_POINT('Origin',(-0.0041710780000559,15.2,3.99369145999999));
#331653=CARTESIAN_POINT('',(-0.00417113200005593,12.2,3.99374277699999));
#331654=CARTESIAN_POINT('Ctrl Pts',(0.335933474999944,12.2,4.73810602399999));
#331655=CARTESIAN_POINT('Ctrl Pts',(0.335933474999944,5.2,4.73810602399999));
#331656=CARTESIAN_POINT('Ctrl Pts',(0.335933474999944,2.2,4.73810602399999));
#331657=CARTESIAN_POINT('Ctrl Pts',(0.335613955999945,12.2,4.73767941899998));
#331658=CARTESIAN_POINT('Ctrl Pts',(0.335613955999945,5.2,4.73767941899998));
#331659=CARTESIAN_POINT('Ctrl Pts',(0.335613955999945,2.2,4.73767941899998));
#331660=CARTESIAN_POINT('Ctrl Pts',(0.334975341999945,12.2,4.73682631699998));
#331661=CARTESIAN_POINT('Ctrl Pts',(0.334975341999945,5.2,4.73682631699998));
#331662=CARTESIAN_POINT('Ctrl Pts',(0.334975341999945,2.2,4.73682631699998));
#331663=CARTESIAN_POINT('Ctrl Pts',(0.334018688999944,12.2,4.73554698499999));
#331664=CARTESIAN_POINT('Ctrl Pts',(0.334018688999944,5.2,4.73554698499999));
#331665=CARTESIAN_POINT('Ctrl Pts',(0.334018688999944,2.2,4.73554698499999));
#331666=CARTESIAN_POINT('Ctrl Pts',(0.332745688999945,12.2,4.73384185399999));
#331667=CARTESIAN_POINT('Ctrl Pts',(0.332745688999945,5.2,4.73384185399999));
#331668=CARTESIAN_POINT('Ctrl Pts',(0.332745688999945,2.2,4.73384185399999));
#331669=CARTESIAN_POINT('Ctrl Pts',(0.331158665999943,12.2,4.73171151799999));
#331670=CARTESIAN_POINT('Ctrl Pts',(0.331158665999943,5.2,4.73171151799999));
#331671=CARTESIAN_POINT('Ctrl Pts',(0.331158665999943,2.2,4.73171151799999));
#331672=CARTESIAN_POINT('Ctrl Pts',(0.329575868999944,12.2,4.72958225699998));
#331673=CARTESIAN_POINT('Ctrl Pts',(0.329575868999944,5.2,4.72958225699998));
#331674=CARTESIAN_POINT('Ctrl Pts',(0.329575868999944,2.2,4.72958225699998));
#331675=CARTESIAN_POINT('Ctrl Pts',(0.327997300999944,12.2,4.72745407599999));
#331676=CARTESIAN_POINT('Ctrl Pts',(0.327997300999944,5.2,4.72745407599999));
#331677=CARTESIAN_POINT('Ctrl Pts',(0.327997300999944,2.2,4.72745407599999));
#331678=CARTESIAN_POINT('Ctrl Pts',(0.326422958999943,12.2,4.72532697899998));
#331679=CARTESIAN_POINT('Ctrl Pts',(0.326422958999943,5.2,4.72532697899998));
#331680=CARTESIAN_POINT('Ctrl Pts',(0.326422958999943,2.2,4.72532697899998));
#331681=CARTESIAN_POINT('Ctrl Pts',(0.324852842999944,12.2,4.72320096999999));
#331682=CARTESIAN_POINT('Ctrl Pts',(0.324852842999944,5.2,4.72320096999999));
#331683=CARTESIAN_POINT('Ctrl Pts',(0.324852842999944,2.2,4.72320096999999));
#331684=CARTESIAN_POINT('Ctrl Pts',(0.323286950999944,12.2,4.72107605899998));
#331685=CARTESIAN_POINT('Ctrl Pts',(0.323286950999944,5.2,4.72107605899998));
#331686=CARTESIAN_POINT('Ctrl Pts',(0.323286950999944,2.2,4.72107605899998));
#331687=CARTESIAN_POINT('Ctrl Pts',(0.321725282999944,12.2,4.71895225599999));
#331688=CARTESIAN_POINT('Ctrl Pts',(0.321725282999944,5.2,4.71895225599999));
#331689=CARTESIAN_POINT('Ctrl Pts',(0.321725282999944,2.2,4.71895225599999));
#331690=CARTESIAN_POINT('Ctrl Pts',(0.320167835999945,12.2,4.71682956899999));
#331691=CARTESIAN_POINT('Ctrl Pts',(0.320167835999945,5.2,4.71682956899999));
#331692=CARTESIAN_POINT('Ctrl Pts',(0.320167835999945,2.2,4.71682956899999));
#331693=CARTESIAN_POINT('Ctrl Pts',(0.318614607999944,12.2,4.71470801099999));
#331694=CARTESIAN_POINT('Ctrl Pts',(0.318614607999944,5.2,4.71470801099999));
#331695=CARTESIAN_POINT('Ctrl Pts',(0.318614607999944,2.2,4.71470801099999));
#331696=CARTESIAN_POINT('Ctrl Pts',(0.317065597999945,12.2,4.71258759299998));
#331697=CARTESIAN_POINT('Ctrl Pts',(0.317065597999945,5.2,4.71258759299998));
#331698=CARTESIAN_POINT('Ctrl Pts',(0.317065597999945,2.2,4.71258759299998));
#331699=CARTESIAN_POINT('Ctrl Pts',(0.315520804999944,12.2,4.71046832199999));
#331700=CARTESIAN_POINT('Ctrl Pts',(0.315520804999944,5.2,4.71046832199999));
#331701=CARTESIAN_POINT('Ctrl Pts',(0.315520804999944,2.2,4.71046832199999));
#331702=CARTESIAN_POINT('Ctrl Pts',(0.313980226999944,12.2,4.70835020699998));
#331703=CARTESIAN_POINT('Ctrl Pts',(0.313980226999944,5.2,4.70835020699998));
#331704=CARTESIAN_POINT('Ctrl Pts',(0.313980226999944,2.2,4.70835020699998));
#331705=CARTESIAN_POINT('Ctrl Pts',(0.312443861999944,12.2,4.70623325799998));
#331706=CARTESIAN_POINT('Ctrl Pts',(0.312443861999944,5.2,4.70623325799998));
#331707=CARTESIAN_POINT('Ctrl Pts',(0.312443861999944,2.2,4.70623325799998));
#331708=CARTESIAN_POINT('Ctrl Pts',(0.310911710999945,12.2,4.70411747999999));
#331709=CARTESIAN_POINT('Ctrl Pts',(0.310911710999945,5.2,4.70411747999999));
#331710=CARTESIAN_POINT('Ctrl Pts',(0.310911710999945,2.2,4.70411747999999));
#331711=CARTESIAN_POINT('Ctrl Pts',(0.309383769999944,12.2,4.70200288399998));
#331712=CARTESIAN_POINT('Ctrl Pts',(0.309383769999944,5.2,4.70200288399998));
#331713=CARTESIAN_POINT('Ctrl Pts',(0.309383769999944,2.2,4.70200288399998));
#331714=CARTESIAN_POINT('Ctrl Pts',(0.307860039999944,12.2,4.69988947399998));
#331715=CARTESIAN_POINT('Ctrl Pts',(0.307860039999944,5.2,4.69988947399998));
#331716=CARTESIAN_POINT('Ctrl Pts',(0.307860039999944,2.2,4.69988947399998));
#331717=CARTESIAN_POINT('Ctrl Pts',(0.306340516999944,12.2,4.69777726199998));
#331718=CARTESIAN_POINT('Ctrl Pts',(0.306340516999944,5.2,4.69777726199998));
#331719=CARTESIAN_POINT('Ctrl Pts',(0.306340516999944,2.2,4.69777726199998));
#331720=CARTESIAN_POINT('Ctrl Pts',(0.304825201999943,12.2,4.69566625299999));
#331721=CARTESIAN_POINT('Ctrl Pts',(0.304825201999943,5.2,4.69566625299999));
#331722=CARTESIAN_POINT('Ctrl Pts',(0.304825201999943,2.2,4.69566625299999));
#331723=CARTESIAN_POINT('Ctrl Pts',(0.303314091999944,12.2,4.69355645999999));
#331724=CARTESIAN_POINT('Ctrl Pts',(0.303314091999944,5.2,4.69355645999999));
#331725=CARTESIAN_POINT('Ctrl Pts',(0.303314091999944,2.2,4.69355645999999));
#331726=CARTESIAN_POINT('Ctrl Pts',(0.301807185999945,12.2,4.69144788799999));
#331727=CARTESIAN_POINT('Ctrl Pts',(0.301807185999945,5.2,4.69144788799999));
#331728=CARTESIAN_POINT('Ctrl Pts',(0.301807185999945,2.2,4.69144788799999));
#331729=CARTESIAN_POINT('Ctrl Pts',(0.300304481999945,12.2,4.68934054899999));
#331730=CARTESIAN_POINT('Ctrl Pts',(0.300304481999945,5.2,4.68934054899999));
#331731=CARTESIAN_POINT('Ctrl Pts',(0.300304481999945,2.2,4.68934054899999));
#331732=CARTESIAN_POINT('Ctrl Pts',(0.298805979999944,12.2,4.68723445099998));
#331733=CARTESIAN_POINT('Ctrl Pts',(0.298805979999944,5.2,4.68723445099998));
#331734=CARTESIAN_POINT('Ctrl Pts',(0.298805979999944,2.2,4.68723445099998));
#331735=CARTESIAN_POINT('Ctrl Pts',(0.297311675999945,12.2,4.68512960199998));
#331736=CARTESIAN_POINT('Ctrl Pts',(0.297311675999945,5.2,4.68512960199998));
#331737=CARTESIAN_POINT('Ctrl Pts',(0.297311675999945,2.2,4.68512960199998));
#331738=CARTESIAN_POINT('Ctrl Pts',(0.295821569999944,12.2,4.68302601099998));
#331739=CARTESIAN_POINT('Ctrl Pts',(0.295821569999944,5.2,4.68302601099998));
#331740=CARTESIAN_POINT('Ctrl Pts',(0.295821569999944,2.2,4.68302601099998));
#331741=CARTESIAN_POINT('Ctrl Pts',(0.294335659999945,12.2,4.68092368599999));
#331742=CARTESIAN_POINT('Ctrl Pts',(0.294335659999945,5.2,4.68092368599999));
#331743=CARTESIAN_POINT('Ctrl Pts',(0.294335659999945,2.2,4.68092368599999));
#331744=CARTESIAN_POINT('Ctrl Pts',(0.292853944999945,12.2,4.67882263599999));
#331745=CARTESIAN_POINT('Ctrl Pts',(0.292853944999945,5.2,4.67882263599999));
#331746=CARTESIAN_POINT('Ctrl Pts',(0.292853944999945,2.2,4.67882263599999));
#331747=CARTESIAN_POINT('Ctrl Pts',(0.291376422999944,12.2,4.67672286999999));
#331748=CARTESIAN_POINT('Ctrl Pts',(0.291376422999944,5.2,4.67672286999999));
#331749=CARTESIAN_POINT('Ctrl Pts',(0.291376422999944,2.2,4.67672286999999));
#331750=CARTESIAN_POINT('Ctrl Pts',(0.289903092999945,12.2,4.67462439599998));
#331751=CARTESIAN_POINT('Ctrl Pts',(0.289903092999945,5.2,4.67462439599998));
#331752=CARTESIAN_POINT('Ctrl Pts',(0.289903092999945,2.2,4.67462439599998));
#331753=CARTESIAN_POINT('Ctrl Pts',(0.288433951999943,12.2,4.67252722199999));
#331754=CARTESIAN_POINT('Ctrl Pts',(0.288433951999943,5.2,4.67252722199999));
#331755=CARTESIAN_POINT('Ctrl Pts',(0.288433951999943,2.2,4.67252722199999));
#331756=CARTESIAN_POINT('Ctrl Pts',(0.286968998999945,12.2,4.67043135899999));
#331757=CARTESIAN_POINT('Ctrl Pts',(0.286968998999945,5.2,4.67043135899999));
#331758=CARTESIAN_POINT('Ctrl Pts',(0.286968998999945,2.2,4.67043135899999));
#331759=CARTESIAN_POINT('Ctrl Pts',(0.285508232999945,12.2,4.66833681299998));
#331760=CARTESIAN_POINT('Ctrl Pts',(0.285508232999945,5.2,4.66833681299998));
#331761=CARTESIAN_POINT('Ctrl Pts',(0.285508232999945,2.2,4.66833681299998));
#331762=CARTESIAN_POINT('Ctrl Pts',(0.284051652999944,12.2,4.66624359399999));
#331763=CARTESIAN_POINT('Ctrl Pts',(0.284051652999944,5.2,4.66624359399999));
#331764=CARTESIAN_POINT('Ctrl Pts',(0.284051652999944,2.2,4.66624359399999));
#331765=CARTESIAN_POINT('Ctrl Pts',(0.282599253999944,12.2,4.66415171199999));
#331766=CARTESIAN_POINT('Ctrl Pts',(0.282599253999944,5.2,4.66415171199999));
#331767=CARTESIAN_POINT('Ctrl Pts',(0.282599253999944,2.2,4.66415171199999));
#331768=CARTESIAN_POINT('Ctrl Pts',(0.281151037999944,12.2,4.66206117399998));
#331769=CARTESIAN_POINT('Ctrl Pts',(0.281151037999944,5.2,4.66206117399998));
#331770=CARTESIAN_POINT('Ctrl Pts',(0.281151037999944,2.2,4.66206117399998));
#331771=CARTESIAN_POINT('Ctrl Pts',(0.279707001999944,12.2,4.65997198899998));
#331772=CARTESIAN_POINT('Ctrl Pts',(0.279707001999944,5.2,4.65997198899998));
#331773=CARTESIAN_POINT('Ctrl Pts',(0.279707001999944,2.2,4.65997198899998));
#331774=CARTESIAN_POINT('Ctrl Pts',(0.278267143999944,12.2,4.65788416699999));
#331775=CARTESIAN_POINT('Ctrl Pts',(0.278267143999944,5.2,4.65788416699999));
#331776=CARTESIAN_POINT('Ctrl Pts',(0.278267143999944,2.2,4.65788416699999));
#331777=CARTESIAN_POINT('Ctrl Pts',(0.276831460999943,12.2,4.65579771499999));
#331778=CARTESIAN_POINT('Ctrl Pts',(0.276831460999943,5.2,4.65579771499999));
#331779=CARTESIAN_POINT('Ctrl Pts',(0.276831460999943,2.2,4.65579771499999));
#331780=CARTESIAN_POINT('Ctrl Pts',(0.275399953999944,12.2,4.65371264199998));
#331781=CARTESIAN_POINT('Ctrl Pts',(0.275399953999944,5.2,4.65371264199998));
#331782=CARTESIAN_POINT('Ctrl Pts',(0.275399953999944,2.2,4.65371264199998));
#331783=CARTESIAN_POINT('Ctrl Pts',(0.273972618999944,12.2,4.65162895899999));
#331784=CARTESIAN_POINT('Ctrl Pts',(0.273972618999944,5.2,4.65162895899999));
#331785=CARTESIAN_POINT('Ctrl Pts',(0.273972618999944,2.2,4.65162895899999));
#331786=CARTESIAN_POINT('Ctrl Pts',(0.272549455999943,12.2,4.64954667099998));
#331787=CARTESIAN_POINT('Ctrl Pts',(0.272549455999943,5.2,4.64954667099998));
#331788=CARTESIAN_POINT('Ctrl Pts',(0.272549455999943,2.2,4.64954667099998));
#331789=CARTESIAN_POINT('Ctrl Pts',(0.271130461999943,12.2,4.64746578999998));
#331790=CARTESIAN_POINT('Ctrl Pts',(0.271130461999943,5.2,4.64746578999998));
#331791=CARTESIAN_POINT('Ctrl Pts',(0.271130461999943,2.2,4.64746578999998));
#331792=CARTESIAN_POINT('Ctrl Pts',(0.269715634999944,12.2,4.64538632299998));
#331793=CARTESIAN_POINT('Ctrl Pts',(0.269715634999944,5.2,4.64538632299998));
#331794=CARTESIAN_POINT('Ctrl Pts',(0.269715634999944,2.2,4.64538632299998));
#331795=CARTESIAN_POINT('Ctrl Pts',(0.268304974999944,12.2,4.64330827999999));
#331796=CARTESIAN_POINT('Ctrl Pts',(0.268304974999944,5.2,4.64330827999999));
#331797=CARTESIAN_POINT('Ctrl Pts',(0.268304974999944,2.2,4.64330827999999));
#331798=CARTESIAN_POINT('Ctrl Pts',(0.266898477999945,12.2,4.64123166799999));
#331799=CARTESIAN_POINT('Ctrl Pts',(0.266898477999945,5.2,4.64123166799999));
#331800=CARTESIAN_POINT('Ctrl Pts',(0.266898477999945,2.2,4.64123166799999));
#331801=CARTESIAN_POINT('Ctrl Pts',(0.265496142999944,12.2,4.63915649899998));
#331802=CARTESIAN_POINT('Ctrl Pts',(0.265496142999944,5.2,4.63915649899998));
#331803=CARTESIAN_POINT('Ctrl Pts',(0.265496142999944,2.2,4.63915649899998));
#331804=CARTESIAN_POINT('Ctrl Pts',(0.264097967999944,12.2,4.63708277799999));
#331805=CARTESIAN_POINT('Ctrl Pts',(0.264097967999944,5.2,4.63708277799999));
#331806=CARTESIAN_POINT('Ctrl Pts',(0.264097967999944,2.2,4.63708277799999));
#331807=CARTESIAN_POINT('Ctrl Pts',(0.262703951999944,12.2,4.63501051699998));
#331808=CARTESIAN_POINT('Ctrl Pts',(0.262703951999944,5.2,4.63501051699998));
#331809=CARTESIAN_POINT('Ctrl Pts',(0.262703951999944,2.2,4.63501051699998));
#331810=CARTESIAN_POINT('Ctrl Pts',(0.261314091999945,12.2,4.63293972199998));
#331811=CARTESIAN_POINT('Ctrl Pts',(0.261314091999945,5.2,4.63293972199998));
#331812=CARTESIAN_POINT('Ctrl Pts',(0.261314091999945,2.2,4.63293972199998));
#331813=CARTESIAN_POINT('Ctrl Pts',(0.259928386999944,12.2,4.63087040499998));
#331814=CARTESIAN_POINT('Ctrl Pts',(0.259928386999944,5.2,4.63087040499998));
#331815=CARTESIAN_POINT('Ctrl Pts',(0.259928386999944,2.2,4.63087040499998));
#331816=CARTESIAN_POINT('Ctrl Pts',(0.258546834999944,12.2,4.62880257299998));
#331817=CARTESIAN_POINT('Ctrl Pts',(0.258546834999944,5.2,4.62880257299998));
#331818=CARTESIAN_POINT('Ctrl Pts',(0.258546834999944,2.2,4.62880257299998));
#331819=CARTESIAN_POINT('Ctrl Pts',(0.257169431999945,12.2,4.62673623399999));
#331820=CARTESIAN_POINT('Ctrl Pts',(0.257169431999945,5.2,4.62673623399999));
#331821=CARTESIAN_POINT('Ctrl Pts',(0.257169431999945,2.2,4.62673623399999));
#331822=CARTESIAN_POINT('Ctrl Pts',(0.255796178999944,12.2,4.62467139899999));
#331823=CARTESIAN_POINT('Ctrl Pts',(0.255796178999944,5.2,4.62467139899999));
#331824=CARTESIAN_POINT('Ctrl Pts',(0.255796178999944,2.2,4.62467139899999));
#331825=CARTESIAN_POINT('Ctrl Pts',(0.254427072999944,12.2,4.62260807599999));
#331826=CARTESIAN_POINT('Ctrl Pts',(0.254427072999944,5.2,4.62260807599999));
#331827=CARTESIAN_POINT('Ctrl Pts',(0.254427072999944,2.2,4.62260807599999));
#331828=CARTESIAN_POINT('Ctrl Pts',(0.253062110999943,12.2,4.62054627299998));
#331829=CARTESIAN_POINT('Ctrl Pts',(0.253062110999943,5.2,4.62054627299998));
#331830=CARTESIAN_POINT('Ctrl Pts',(0.253062110999943,2.2,4.62054627299998));
#331831=CARTESIAN_POINT('Ctrl Pts',(0.251701291999943,12.2,4.61848599999998));
#331832=CARTESIAN_POINT('Ctrl Pts',(0.251701291999943,5.2,4.61848599999998));
#331833=CARTESIAN_POINT('Ctrl Pts',(0.251701291999943,2.2,4.61848599999998));
#331834=CARTESIAN_POINT('Ctrl Pts',(0.250344613999944,12.2,4.61642726599998));
#331835=CARTESIAN_POINT('Ctrl Pts',(0.250344613999944,5.2,4.61642726599998));
#331836=CARTESIAN_POINT('Ctrl Pts',(0.250344613999944,2.2,4.61642726599998));
#331837=CARTESIAN_POINT('Ctrl Pts',(0.248992075999944,12.2,4.61437007899999));
#331838=CARTESIAN_POINT('Ctrl Pts',(0.248992075999944,5.2,4.61437007899999));
#331839=CARTESIAN_POINT('Ctrl Pts',(0.248992075999944,2.2,4.61437007899999));
#331840=CARTESIAN_POINT('Ctrl Pts',(0.247643673999944,12.2,4.61231444999999));
#331841=CARTESIAN_POINT('Ctrl Pts',(0.247643673999944,5.2,4.61231444999999));
#331842=CARTESIAN_POINT('Ctrl Pts',(0.247643673999944,2.2,4.61231444999999));
#331843=CARTESIAN_POINT('Ctrl Pts',(0.246299405999943,12.2,4.61026038399999));
#331844=CARTESIAN_POINT('Ctrl Pts',(0.246299405999943,5.2,4.61026038399999));
#331845=CARTESIAN_POINT('Ctrl Pts',(0.246299405999943,2.2,4.61026038399999));
#331846=CARTESIAN_POINT('Ctrl Pts',(0.244959270999944,12.2,4.60820789399998));
#331847=CARTESIAN_POINT('Ctrl Pts',(0.244959270999944,5.2,4.60820789399998));
#331848=CARTESIAN_POINT('Ctrl Pts',(0.244959270999944,2.2,4.60820789399998));
#331849=CARTESIAN_POINT('Ctrl Pts',(0.243623266999944,12.2,4.60615698599998));
#331850=CARTESIAN_POINT('Ctrl Pts',(0.243623266999944,5.2,4.60615698599998));
#331851=CARTESIAN_POINT('Ctrl Pts',(0.243623266999944,2.2,4.60615698599998));
#331852=CARTESIAN_POINT('Ctrl Pts',(0.242291391999944,12.2,4.60410767099999));
#331853=CARTESIAN_POINT('Ctrl Pts',(0.242291391999944,5.2,4.60410767099999));
#331854=CARTESIAN_POINT('Ctrl Pts',(0.242291391999944,2.2,4.60410767099999));
#331855=CARTESIAN_POINT('Ctrl Pts',(0.240963642999944,12.2,4.60205995699998));
#331856=CARTESIAN_POINT('Ctrl Pts',(0.240963642999944,5.2,4.60205995699998));
#331857=CARTESIAN_POINT('Ctrl Pts',(0.240963642999944,2.2,4.60205995699998));
#331858=CARTESIAN_POINT('Ctrl Pts',(0.239640017999945,12.2,4.60001385399998));
#331859=CARTESIAN_POINT('Ctrl Pts',(0.239640017999945,5.2,4.60001385399998));
#331860=CARTESIAN_POINT('Ctrl Pts',(0.239640017999945,2.2,4.60001385399998));
#331861=CARTESIAN_POINT('Ctrl Pts',(0.238320514999945,12.2,4.59796936899998));
#331862=CARTESIAN_POINT('Ctrl Pts',(0.238320514999945,5.2,4.59796936899998));
#331863=CARTESIAN_POINT('Ctrl Pts',(0.238320514999945,2.2,4.59796936899998));
#331864=CARTESIAN_POINT('Ctrl Pts',(0.237005132999943,12.2,4.59592651299998));
#331865=CARTESIAN_POINT('Ctrl Pts',(0.237005132999943,5.2,4.59592651299998));
#331866=CARTESIAN_POINT('Ctrl Pts',(0.237005132999943,2.2,4.59592651299998));
#331867=CARTESIAN_POINT('Ctrl Pts',(0.235693867999943,12.2,4.59388529299999));
#331868=CARTESIAN_POINT('Ctrl Pts',(0.235693867999943,5.2,4.59388529299999));
#331869=CARTESIAN_POINT('Ctrl Pts',(0.235693867999943,2.2,4.59388529299999));
#331870=CARTESIAN_POINT('Ctrl Pts',(0.234386717999945,12.2,4.59184572099999));
#331871=CARTESIAN_POINT('Ctrl Pts',(0.234386717999945,5.2,4.59184572099999));
#331872=CARTESIAN_POINT('Ctrl Pts',(0.234386717999945,2.2,4.59184572099999));
#331873=CARTESIAN_POINT('Ctrl Pts',(0.233083682999944,12.2,4.58980780299999));
#331874=CARTESIAN_POINT('Ctrl Pts',(0.233083682999944,5.2,4.58980780299999));
#331875=CARTESIAN_POINT('Ctrl Pts',(0.233083682999944,2.2,4.58980780299999));
#331876=CARTESIAN_POINT('Ctrl Pts',(0.231784757999945,12.2,4.58777154899998));
#331877=CARTESIAN_POINT('Ctrl Pts',(0.231784757999945,5.2,4.58777154899998));
#331878=CARTESIAN_POINT('Ctrl Pts',(0.231784757999945,2.2,4.58777154899998));
#331879=CARTESIAN_POINT('Ctrl Pts',(0.230489942999944,12.2,4.58573696899998));
#331880=CARTESIAN_POINT('Ctrl Pts',(0.230489942999944,5.2,4.58573696899998));
#331881=CARTESIAN_POINT('Ctrl Pts',(0.230489942999944,2.2,4.58573696899998));
#331882=CARTESIAN_POINT('Ctrl Pts',(0.229199234999945,12.2,4.58370407099999));
#331883=CARTESIAN_POINT('Ctrl Pts',(0.229199234999945,5.2,4.58370407099999));
#331884=CARTESIAN_POINT('Ctrl Pts',(0.229199234999945,2.2,4.58370407099999));
#331885=CARTESIAN_POINT('Ctrl Pts',(0.227912629999943,12.2,4.58167286499998));
#331886=CARTESIAN_POINT('Ctrl Pts',(0.227912629999943,5.2,4.58167286499998));
#331887=CARTESIAN_POINT('Ctrl Pts',(0.227912629999943,2.2,4.58167286499998));
#331888=CARTESIAN_POINT('Ctrl Pts',(0.226630128999944,12.2,4.57964335899998));
#331889=CARTESIAN_POINT('Ctrl Pts',(0.226630128999944,5.2,4.57964335899998));
#331890=CARTESIAN_POINT('Ctrl Pts',(0.226630128999944,2.2,4.57964335899998));
#331891=CARTESIAN_POINT('Ctrl Pts',(0.225351726999945,12.2,4.57761556199999));
#331892=CARTESIAN_POINT('Ctrl Pts',(0.225351726999945,5.2,4.57761556199999));
#331893=CARTESIAN_POINT('Ctrl Pts',(0.225351726999945,2.2,4.57761556199999));
#331894=CARTESIAN_POINT('Ctrl Pts',(0.224077423999944,12.2,4.57558948499998));
#331895=CARTESIAN_POINT('Ctrl Pts',(0.224077423999944,5.2,4.57558948499998));
#331896=CARTESIAN_POINT('Ctrl Pts',(0.224077423999944,2.2,4.57558948499998));
#331897=CARTESIAN_POINT('Ctrl Pts',(0.222807214999945,12.2,4.57356513499998));
#331898=CARTESIAN_POINT('Ctrl Pts',(0.222807214999945,5.2,4.57356513499998));
#331899=CARTESIAN_POINT('Ctrl Pts',(0.222807214999945,2.2,4.57356513499998));
#331900=CARTESIAN_POINT('Ctrl Pts',(0.221541099999945,12.2,4.57154252199999));
#331901=CARTESIAN_POINT('Ctrl Pts',(0.221541099999945,5.2,4.57154252199999));
#331902=CARTESIAN_POINT('Ctrl Pts',(0.221541099999945,2.2,4.57154252199999));
#331903=CARTESIAN_POINT('Ctrl Pts',(0.220279073999944,12.2,4.56952165399999));
#331904=CARTESIAN_POINT('Ctrl Pts',(0.220279073999944,5.2,4.56952165399999));
#331905=CARTESIAN_POINT('Ctrl Pts',(0.220279073999944,2.2,4.56952165399999));
#331906=CARTESIAN_POINT('Ctrl Pts',(0.219021137999944,12.2,4.56750254099998));
#331907=CARTESIAN_POINT('Ctrl Pts',(0.219021137999944,5.2,4.56750254099998));
#331908=CARTESIAN_POINT('Ctrl Pts',(0.219021137999944,2.2,4.56750254099998));
#331909=CARTESIAN_POINT('Ctrl Pts',(0.217767286999945,12.2,4.56548519299999));
#331910=CARTESIAN_POINT('Ctrl Pts',(0.217767286999945,5.2,4.56548519299999));
#331911=CARTESIAN_POINT('Ctrl Pts',(0.217767286999945,2.2,4.56548519299999));
#331912=CARTESIAN_POINT('Ctrl Pts',(0.216517519999944,12.2,4.56346961899998));
#331913=CARTESIAN_POINT('Ctrl Pts',(0.216517519999944,5.2,4.56346961899998));
#331914=CARTESIAN_POINT('Ctrl Pts',(0.216517519999944,2.2,4.56346961899998));
#331915=CARTESIAN_POINT('Ctrl Pts',(0.215271834999945,12.2,4.56145582599999));
#331916=CARTESIAN_POINT('Ctrl Pts',(0.215271834999945,5.2,4.56145582599999));
#331917=CARTESIAN_POINT('Ctrl Pts',(0.215271834999945,2.2,4.56145582599999));
#331918=CARTESIAN_POINT('Ctrl Pts',(0.214030226999944,12.2,4.55944382499998));
#331919=CARTESIAN_POINT('Ctrl Pts',(0.214030226999944,5.2,4.55944382499998));
#331920=CARTESIAN_POINT('Ctrl Pts',(0.214030226999944,2.2,4.55944382499998));
#331921=CARTESIAN_POINT('Ctrl Pts',(0.212792695999945,12.2,4.55743362599998));
#331922=CARTESIAN_POINT('Ctrl Pts',(0.212792695999945,5.2,4.55743362599998));
#331923=CARTESIAN_POINT('Ctrl Pts',(0.212792695999945,2.2,4.55743362599998));
#331924=CARTESIAN_POINT('Ctrl Pts',(0.211559238999944,12.2,4.55542523499999));
#331925=CARTESIAN_POINT('Ctrl Pts',(0.211559238999944,5.2,4.55542523499999));
#331926=CARTESIAN_POINT('Ctrl Pts',(0.211559238999944,2.2,4.55542523499999));
#331927=CARTESIAN_POINT('Ctrl Pts',(0.210329852999944,12.2,4.55341866399999));
#331928=CARTESIAN_POINT('Ctrl Pts',(0.210329852999944,5.2,4.55341866399999));
#331929=CARTESIAN_POINT('Ctrl Pts',(0.210329852999944,2.2,4.55341866399999));
#331930=CARTESIAN_POINT('Ctrl Pts',(0.209104535999945,12.2,4.55141392199998));
#331931=CARTESIAN_POINT('Ctrl Pts',(0.209104535999945,5.2,4.55141392199998));
#331932=CARTESIAN_POINT('Ctrl Pts',(0.209104535999945,2.2,4.55141392199998));
#331933=CARTESIAN_POINT('Ctrl Pts',(0.207883285999945,12.2,4.54941101699998));
#331934=CARTESIAN_POINT('Ctrl Pts',(0.207883285999945,5.2,4.54941101699998));
#331935=CARTESIAN_POINT('Ctrl Pts',(0.207883285999945,2.2,4.54941101699998));
#331936=CARTESIAN_POINT('Ctrl Pts',(0.206666098999945,12.2,4.54740995799998));
#331937=CARTESIAN_POINT('Ctrl Pts',(0.206666098999945,5.2,4.54740995799998));
#331938=CARTESIAN_POINT('Ctrl Pts',(0.206666098999945,2.2,4.54740995799998));
#331939=CARTESIAN_POINT('Ctrl Pts',(0.205452972999945,12.2,4.54541075599998));
#331940=CARTESIAN_POINT('Ctrl Pts',(0.205452972999945,5.2,4.54541075599998));
#331941=CARTESIAN_POINT('Ctrl Pts',(0.205452972999945,2.2,4.54541075599998));
#331942=CARTESIAN_POINT('Ctrl Pts',(0.204243906999944,12.2,4.54341341899998));
#331943=CARTESIAN_POINT('Ctrl Pts',(0.204243906999944,5.2,4.54341341899998));
#331944=CARTESIAN_POINT('Ctrl Pts',(0.204243906999944,2.2,4.54341341899998));
#331945=CARTESIAN_POINT('Ctrl Pts',(0.203038895999944,12.2,4.54141795499999));
#331946=CARTESIAN_POINT('Ctrl Pts',(0.203038895999944,5.2,4.54141795499999));
#331947=CARTESIAN_POINT('Ctrl Pts',(0.203038895999944,2.2,4.54141795499999));
#331948=CARTESIAN_POINT('Ctrl Pts',(0.201837938999944,12.2,4.53942437699999));
#331949=CARTESIAN_POINT('Ctrl Pts',(0.201837938999944,5.2,4.53942437699999));
#331950=CARTESIAN_POINT('Ctrl Pts',(0.201837938999944,2.2,4.53942437699999));
#331951=CARTESIAN_POINT('Ctrl Pts',(0.200641032999943,12.2,4.53743268999999));
#331952=CARTESIAN_POINT('Ctrl Pts',(0.200641032999943,5.2,4.53743268999999));
#331953=CARTESIAN_POINT('Ctrl Pts',(0.200641032999943,2.2,4.53743268999999));
#331954=CARTESIAN_POINT('Ctrl Pts',(0.199448174999944,12.2,4.53544290599999));
#331955=CARTESIAN_POINT('Ctrl Pts',(0.199448174999944,5.2,4.53544290599999));
#331956=CARTESIAN_POINT('Ctrl Pts',(0.199448174999944,2.2,4.53544290599999));
#331957=CARTESIAN_POINT('Ctrl Pts',(0.198259362999943,12.2,4.53345503399999));
#331958=CARTESIAN_POINT('Ctrl Pts',(0.198259362999943,5.2,4.53345503399999));
#331959=CARTESIAN_POINT('Ctrl Pts',(0.198259362999943,2.2,4.53345503399999));
#331960=CARTESIAN_POINT('Ctrl Pts',(0.197074592999943,12.2,4.53146908099999));
#331961=CARTESIAN_POINT('Ctrl Pts',(0.197074592999943,5.2,4.53146908099999));
#331962=CARTESIAN_POINT('Ctrl Pts',(0.197074592999943,2.2,4.53146908099999));
#331963=CARTESIAN_POINT('Ctrl Pts',(0.195893864999944,12.2,4.52948505899998));
#331964=CARTESIAN_POINT('Ctrl Pts',(0.195893864999944,5.2,4.52948505899998));
#331965=CARTESIAN_POINT('Ctrl Pts',(0.195893864999944,2.2,4.52948505899998));
#331966=CARTESIAN_POINT('Ctrl Pts',(0.194717173999944,12.2,4.52750297699998));
#331967=CARTESIAN_POINT('Ctrl Pts',(0.194717173999944,5.2,4.52750297699998));
#331968=CARTESIAN_POINT('Ctrl Pts',(0.194717173999944,2.2,4.52750297699998));
#331969=CARTESIAN_POINT('Ctrl Pts',(0.193544517999945,12.2,4.52552284299998));
#331970=CARTESIAN_POINT('Ctrl Pts',(0.193544517999945,5.2,4.52552284299998));
#331971=CARTESIAN_POINT('Ctrl Pts',(0.193544517999945,2.2,4.52552284299998));
#331972=CARTESIAN_POINT('Ctrl Pts',(0.192375894999944,12.2,4.52354466699998));
#331973=CARTESIAN_POINT('Ctrl Pts',(0.192375894999944,5.2,4.52354466699998));
#331974=CARTESIAN_POINT('Ctrl Pts',(0.192375894999944,2.2,4.52354466699998));
#331975=CARTESIAN_POINT('Ctrl Pts',(0.191211299999944,12.2,4.52156845699999));
#331976=CARTESIAN_POINT('Ctrl Pts',(0.191211299999944,5.2,4.52156845699999));
#331977=CARTESIAN_POINT('Ctrl Pts',(0.191211299999944,2.2,4.52156845699999));
#331978=CARTESIAN_POINT('Ctrl Pts',(0.190050732999945,12.2,4.51959422499999));
#331979=CARTESIAN_POINT('Ctrl Pts',(0.190050732999945,5.2,4.51959422499999));
#331980=CARTESIAN_POINT('Ctrl Pts',(0.190050732999945,2.2,4.51959422499999));
#331981=CARTESIAN_POINT('Ctrl Pts',(0.188894189999944,12.2,4.51762197899999));
#331982=CARTESIAN_POINT('Ctrl Pts',(0.188894189999944,5.2,4.51762197899999));
#331983=CARTESIAN_POINT('Ctrl Pts',(0.188894189999944,2.2,4.51762197899999));
#331984=CARTESIAN_POINT('Ctrl Pts',(0.187741667999944,12.2,4.51565172799998));
#331985=CARTESIAN_POINT('Ctrl Pts',(0.187741667999944,5.2,4.51565172799998));
#331986=CARTESIAN_POINT('Ctrl Pts',(0.187741667999944,2.2,4.51565172799998));
#331987=CARTESIAN_POINT('Ctrl Pts',(0.186593162999945,12.2,4.51368348099999));
#331988=CARTESIAN_POINT('Ctrl Pts',(0.186593162999945,5.2,4.51368348099999));
#331989=CARTESIAN_POINT('Ctrl Pts',(0.186593162999945,2.2,4.51368348099999));
#331990=CARTESIAN_POINT('Ctrl Pts',(0.185448674999943,12.2,4.51171724899999));
#331991=CARTESIAN_POINT('Ctrl Pts',(0.185448674999943,5.2,4.51171724899999));
#331992=CARTESIAN_POINT('Ctrl Pts',(0.185448674999943,2.2,4.51171724899999));
#331993=CARTESIAN_POINT('Ctrl Pts',(0.184308199999944,12.2,4.50975303999999));
#331994=CARTESIAN_POINT('Ctrl Pts',(0.184308199999944,5.2,4.50975303999999));
#331995=CARTESIAN_POINT('Ctrl Pts',(0.184308199999944,2.2,4.50975303999999));
#331996=CARTESIAN_POINT('Ctrl Pts',(0.183171734999944,12.2,4.50779086399999));
#331997=CARTESIAN_POINT('Ctrl Pts',(0.183171734999944,5.2,4.50779086399999));
#331998=CARTESIAN_POINT('Ctrl Pts',(0.183171734999944,2.2,4.50779086399999));
#331999=CARTESIAN_POINT('Ctrl Pts',(0.182039276999945,12.2,4.50583072899998));
#332000=CARTESIAN_POINT('Ctrl Pts',(0.182039276999945,5.2,4.50583072899998));
#332001=CARTESIAN_POINT('Ctrl Pts',(0.182039276999945,2.2,4.50583072899998));
#332002=CARTESIAN_POINT('Ctrl Pts',(0.180910821999944,12.2,4.50387264599998));
#332003=CARTESIAN_POINT('Ctrl Pts',(0.180910821999944,5.2,4.50387264599998));
#332004=CARTESIAN_POINT('Ctrl Pts',(0.180910821999944,2.2,4.50387264599998));
#332005=CARTESIAN_POINT('Ctrl Pts',(0.179786368999943,12.2,4.50191662499999));
#332006=CARTESIAN_POINT('Ctrl Pts',(0.179786368999943,5.2,4.50191662499999));
#332007=CARTESIAN_POINT('Ctrl Pts',(0.179786368999943,2.2,4.50191662499999));
#332008=CARTESIAN_POINT('Ctrl Pts',(0.178665914999945,12.2,4.49996267399998));
#332009=CARTESIAN_POINT('Ctrl Pts',(0.178665914999945,5.2,4.49996267399998));
#332010=CARTESIAN_POINT('Ctrl Pts',(0.178665914999945,2.2,4.49996267399998));
#332011=CARTESIAN_POINT('Ctrl Pts',(0.177549455999945,12.2,4.49801080299999));
#332012=CARTESIAN_POINT('Ctrl Pts',(0.177549455999945,5.2,4.49801080299999));
#332013=CARTESIAN_POINT('Ctrl Pts',(0.177549455999945,2.2,4.49801080299999));
#332014=CARTESIAN_POINT('Ctrl Pts',(0.176436989999944,12.2,4.49606102099998));
#332015=CARTESIAN_POINT('Ctrl Pts',(0.176436989999944,5.2,4.49606102099998));
#332016=CARTESIAN_POINT('Ctrl Pts',(0.176436989999944,2.2,4.49606102099998));
#332017=CARTESIAN_POINT('Ctrl Pts',(0.175328511999944,12.2,4.49411333799999));
#332018=CARTESIAN_POINT('Ctrl Pts',(0.175328511999944,5.2,4.49411333799999));
#332019=CARTESIAN_POINT('Ctrl Pts',(0.175328511999944,2.2,4.49411333799999));
#332020=CARTESIAN_POINT('Ctrl Pts',(0.174224021999944,12.2,4.49216776299998));
#332021=CARTESIAN_POINT('Ctrl Pts',(0.174224021999944,5.2,4.49216776299998));
#332022=CARTESIAN_POINT('Ctrl Pts',(0.174224021999944,2.2,4.49216776299998));
#332023=CARTESIAN_POINT('Ctrl Pts',(0.173123514999943,12.2,4.49022430599998));
#332024=CARTESIAN_POINT('Ctrl Pts',(0.173123514999943,5.2,4.49022430599998));
#332025=CARTESIAN_POINT('Ctrl Pts',(0.173123514999943,2.2,4.49022430599998));
#332026=CARTESIAN_POINT('Ctrl Pts',(0.172026987999944,12.2,4.48828297499999));
#332027=CARTESIAN_POINT('Ctrl Pts',(0.172026987999944,5.2,4.48828297499999));
#332028=CARTESIAN_POINT('Ctrl Pts',(0.172026987999944,2.2,4.48828297499999));
#332029=CARTESIAN_POINT('Ctrl Pts',(0.170934438999945,12.2,4.48634378299998));
#332030=CARTESIAN_POINT('Ctrl Pts',(0.170934438999945,5.2,4.48634378299998));
#332031=CARTESIAN_POINT('Ctrl Pts',(0.170934438999945,2.2,4.48634378299998));
#332032=CARTESIAN_POINT('Ctrl Pts',(0.169845864999945,12.2,4.48440673499999));
#332033=CARTESIAN_POINT('Ctrl Pts',(0.169845864999945,5.2,4.48440673499999));
#332034=CARTESIAN_POINT('Ctrl Pts',(0.169845864999945,2.2,4.48440673499999));
#332035=CARTESIAN_POINT('Ctrl Pts',(0.168761260999943,12.2,4.48247184299999));
#332036=CARTESIAN_POINT('Ctrl Pts',(0.168761260999943,5.2,4.48247184299999));
#332037=CARTESIAN_POINT('Ctrl Pts',(0.168761260999943,2.2,4.48247184299999));
#332038=CARTESIAN_POINT('Ctrl Pts',(0.167680625999944,12.2,4.48053911699999));
#332039=CARTESIAN_POINT('Ctrl Pts',(0.167680625999944,5.2,4.48053911699999));
#332040=CARTESIAN_POINT('Ctrl Pts',(0.167680625999944,2.2,4.48053911699999));
#332041=CARTESIAN_POINT('Ctrl Pts',(0.166603955999944,12.2,4.47860856599998));
#332042=CARTESIAN_POINT('Ctrl Pts',(0.166603955999944,5.2,4.47860856599998));
#332043=CARTESIAN_POINT('Ctrl Pts',(0.166603955999944,2.2,4.47860856599998));
#332044=CARTESIAN_POINT('Ctrl Pts',(0.165531247999944,12.2,4.47668019799998));
#332045=CARTESIAN_POINT('Ctrl Pts',(0.165531247999944,5.2,4.47668019799998));
#332046=CARTESIAN_POINT('Ctrl Pts',(0.165531247999944,2.2,4.47668019799998));
#332047=CARTESIAN_POINT('Ctrl Pts',(0.164462497999944,12.2,4.47475402499999));
#332048=CARTESIAN_POINT('Ctrl Pts',(0.164462497999944,5.2,4.47475402499999));
#332049=CARTESIAN_POINT('Ctrl Pts',(0.164462497999944,2.2,4.47475402499999));
#332050=CARTESIAN_POINT('Ctrl Pts',(0.163397704999945,12.2,4.47283005399999));
#332051=CARTESIAN_POINT('Ctrl Pts',(0.163397704999945,5.2,4.47283005399999));
#332052=CARTESIAN_POINT('Ctrl Pts',(0.163397704999945,2.2,4.47283005399999));
#332053=CARTESIAN_POINT('Ctrl Pts',(0.162336863999943,12.2,4.47090829699999));
#332054=CARTESIAN_POINT('Ctrl Pts',(0.162336863999943,5.2,4.47090829699999));
#332055=CARTESIAN_POINT('Ctrl Pts',(0.162336863999943,2.2,4.47090829699999));
#332056=CARTESIAN_POINT('Ctrl Pts',(0.161279971999945,12.2,4.46898876299999));
#332057=CARTESIAN_POINT('Ctrl Pts',(0.161279971999945,5.2,4.46898876299999));
#332058=CARTESIAN_POINT('Ctrl Pts',(0.161279971999945,2.2,4.46898876299999));
#332059=CARTESIAN_POINT('Ctrl Pts',(0.160227026999945,12.2,4.46707146099998));
#332060=CARTESIAN_POINT('Ctrl Pts',(0.160227026999945,5.2,4.46707146099998));
#332061=CARTESIAN_POINT('Ctrl Pts',(0.160227026999945,2.2,4.46707146099998));
#332062=CARTESIAN_POINT('Ctrl Pts',(0.159178023999944,12.2,4.46515639899999));
#332063=CARTESIAN_POINT('Ctrl Pts',(0.159178023999944,5.2,4.46515639899999));
#332064=CARTESIAN_POINT('Ctrl Pts',(0.159178023999944,2.2,4.46515639899999));
#332065=CARTESIAN_POINT('Ctrl Pts',(0.158132960999945,12.2,4.46324358999998));
#332066=CARTESIAN_POINT('Ctrl Pts',(0.158132960999945,5.2,4.46324358999998));
#332067=CARTESIAN_POINT('Ctrl Pts',(0.158132960999945,2.2,4.46324358999998));
#332068=CARTESIAN_POINT('Ctrl Pts',(0.157091832999944,12.2,4.46133304099998));
#332069=CARTESIAN_POINT('Ctrl Pts',(0.157091832999944,5.2,4.46133304099998));
#332070=CARTESIAN_POINT('Ctrl Pts',(0.157091832999944,2.2,4.46133304099998));
#332071=CARTESIAN_POINT('Ctrl Pts',(0.156054640999944,12.2,4.45942476299999));
#332072=CARTESIAN_POINT('Ctrl Pts',(0.156054640999944,5.2,4.45942476299999));
#332073=CARTESIAN_POINT('Ctrl Pts',(0.156054640999944,2.2,4.45942476299999));
#332074=CARTESIAN_POINT('Ctrl Pts',(0.155021375999944,12.2,4.45751876499998));
#332075=CARTESIAN_POINT('Ctrl Pts',(0.155021375999944,5.2,4.45751876499998));
#332076=CARTESIAN_POINT('Ctrl Pts',(0.155021375999944,2.2,4.45751876499998));
#332077=CARTESIAN_POINT('Ctrl Pts',(0.153992038999944,12.2,4.45561505699998));
#332078=CARTESIAN_POINT('Ctrl Pts',(0.153992038999944,5.2,4.45561505699998));
#332079=CARTESIAN_POINT('Ctrl Pts',(0.153992038999944,2.2,4.45561505699998));
#332080=CARTESIAN_POINT('Ctrl Pts',(0.152966623999945,12.2,4.45371364899999));
#332081=CARTESIAN_POINT('Ctrl Pts',(0.152966623999945,5.2,4.45371364899999));
#332082=CARTESIAN_POINT('Ctrl Pts',(0.152966623999945,2.2,4.45371364899999));
#332083=CARTESIAN_POINT('Ctrl Pts',(0.151945128999945,12.2,4.45181454999998));
#332084=CARTESIAN_POINT('Ctrl Pts',(0.151945128999945,5.2,4.45181454999998));
#332085=CARTESIAN_POINT('Ctrl Pts',(0.151945128999945,2.2,4.45181454999998));
#332086=CARTESIAN_POINT('Ctrl Pts',(0.150927550999944,12.2,4.44991776899998));
#332087=CARTESIAN_POINT('Ctrl Pts',(0.150927550999944,5.2,4.44991776899998));
#332088=CARTESIAN_POINT('Ctrl Pts',(0.150927550999944,2.2,4.44991776899998));
#332089=CARTESIAN_POINT('Ctrl Pts',(0.149913884999944,12.2,4.44802331699999));
#332090=CARTESIAN_POINT('Ctrl Pts',(0.149913884999944,5.2,4.44802331699999));
#332091=CARTESIAN_POINT('Ctrl Pts',(0.149913884999944,2.2,4.44802331699999));
#332092=CARTESIAN_POINT('Ctrl Pts',(0.148904129999944,12.2,4.44613120299999));
#332093=CARTESIAN_POINT('Ctrl Pts',(0.148904129999944,5.2,4.44613120299999));
#332094=CARTESIAN_POINT('Ctrl Pts',(0.148904129999944,2.2,4.44613120299999));
#332095=CARTESIAN_POINT('Ctrl Pts',(0.147898278999945,12.2,4.44424143699998));
#332096=CARTESIAN_POINT('Ctrl Pts',(0.147898278999945,5.2,4.44424143699998));
#332097=CARTESIAN_POINT('Ctrl Pts',(0.147898278999945,2.2,4.44424143699998));
#332098=CARTESIAN_POINT('Ctrl Pts',(0.146896331999944,12.2,4.44235402799999));
#332099=CARTESIAN_POINT('Ctrl Pts',(0.146896331999944,5.2,4.44235402799999));
#332100=CARTESIAN_POINT('Ctrl Pts',(0.146896331999944,2.2,4.44235402799999));
#332101=CARTESIAN_POINT('Ctrl Pts',(0.145898283999945,12.2,4.44046898699998));
#332102=CARTESIAN_POINT('Ctrl Pts',(0.145898283999945,5.2,4.44046898699998));
#332103=CARTESIAN_POINT('Ctrl Pts',(0.145898283999945,2.2,4.44046898699998));
#332104=CARTESIAN_POINT('Ctrl Pts',(0.144904131999944,12.2,4.43858632299998));
#332105=CARTESIAN_POINT('Ctrl Pts',(0.144904131999944,5.2,4.43858632299998));
#332106=CARTESIAN_POINT('Ctrl Pts',(0.144904131999944,2.2,4.43858632299998));
#332107=CARTESIAN_POINT('Ctrl Pts',(0.143913870999944,12.2,4.43670604599999));
#332108=CARTESIAN_POINT('Ctrl Pts',(0.143913870999944,5.2,4.43670604599999));
#332109=CARTESIAN_POINT('Ctrl Pts',(0.143913870999944,2.2,4.43670604599999));
#332110=CARTESIAN_POINT('Ctrl Pts',(0.142927499999944,12.2,4.43482816499999));
#332111=CARTESIAN_POINT('Ctrl Pts',(0.142927499999944,5.2,4.43482816499999));
#332112=CARTESIAN_POINT('Ctrl Pts',(0.142927499999944,2.2,4.43482816499999));
#332113=CARTESIAN_POINT('Ctrl Pts',(0.141945013999945,12.2,4.43295269099998));
#332114=CARTESIAN_POINT('Ctrl Pts',(0.141945013999945,5.2,4.43295269099998));
#332115=CARTESIAN_POINT('Ctrl Pts',(0.141945013999945,2.2,4.43295269099998));
#332116=CARTESIAN_POINT('Ctrl Pts',(0.140966408999944,12.2,4.43107963199999));
#332117=CARTESIAN_POINT('Ctrl Pts',(0.140966408999944,5.2,4.43107963199999));
#332118=CARTESIAN_POINT('Ctrl Pts',(0.140966408999944,2.2,4.43107963199999));
#332119=CARTESIAN_POINT('Ctrl Pts',(0.139991681999945,12.2,4.42920899999999));
#332120=CARTESIAN_POINT('Ctrl Pts',(0.139991681999945,5.2,4.42920899999999));
#332121=CARTESIAN_POINT('Ctrl Pts',(0.139991681999945,2.2,4.42920899999999));
#332122=CARTESIAN_POINT('Ctrl Pts',(0.139020829999945,12.2,4.42734080299999));
#332123=CARTESIAN_POINT('Ctrl Pts',(0.139020829999945,5.2,4.42734080299999));
#332124=CARTESIAN_POINT('Ctrl Pts',(0.139020829999945,2.2,4.42734080299999));
#332125=CARTESIAN_POINT('Ctrl Pts',(0.138053847999944,12.2,4.42547505199999));
#332126=CARTESIAN_POINT('Ctrl Pts',(0.138053847999944,5.2,4.42547505199999));
#332127=CARTESIAN_POINT('Ctrl Pts',(0.138053847999944,2.2,4.42547505199999));
#332128=CARTESIAN_POINT('Ctrl Pts',(0.137090732999944,12.2,4.42361175499999));
#332129=CARTESIAN_POINT('Ctrl Pts',(0.137090732999944,5.2,4.42361175499999));
#332130=CARTESIAN_POINT('Ctrl Pts',(0.137090732999944,2.2,4.42361175499999));
#332131=CARTESIAN_POINT('Ctrl Pts',(0.136131481999945,12.2,4.42175092399999));
#332132=CARTESIAN_POINT('Ctrl Pts',(0.136131481999945,5.2,4.42175092399999));
#332133=CARTESIAN_POINT('Ctrl Pts',(0.136131481999945,2.2,4.42175092399999));
#332134=CARTESIAN_POINT('Ctrl Pts',(0.135176090999943,12.2,4.41989256899999));
#332135=CARTESIAN_POINT('Ctrl Pts',(0.135176090999943,5.2,4.41989256899999));
#332136=CARTESIAN_POINT('Ctrl Pts',(0.135176090999943,2.2,4.41989256899999));
#332137=CARTESIAN_POINT('Ctrl Pts',(0.134224555999944,12.2,4.41803669699999));
#332138=CARTESIAN_POINT('Ctrl Pts',(0.134224555999944,5.2,4.41803669699999));
#332139=CARTESIAN_POINT('Ctrl Pts',(0.134224555999944,2.2,4.41803669699999));
#332140=CARTESIAN_POINT('Ctrl Pts',(0.133276872999945,12.2,4.41618331999998));
#332141=CARTESIAN_POINT('Ctrl Pts',(0.133276872999945,5.2,4.41618331999998));
#332142=CARTESIAN_POINT('Ctrl Pts',(0.133276872999945,2.2,4.41618331999998));
#332143=CARTESIAN_POINT('Ctrl Pts',(0.132333037999944,12.2,4.41433244799998));
#332144=CARTESIAN_POINT('Ctrl Pts',(0.132333037999944,5.2,4.41433244799998));
#332145=CARTESIAN_POINT('Ctrl Pts',(0.132333037999944,2.2,4.41433244799998));
#332146=CARTESIAN_POINT('Ctrl Pts',(0.131393048999945,12.2,4.41248408899998));
#332147=CARTESIAN_POINT('Ctrl Pts',(0.131393048999945,5.2,4.41248408899998));
#332148=CARTESIAN_POINT('Ctrl Pts',(0.131393048999945,2.2,4.41248408899998));
#332149=CARTESIAN_POINT('Ctrl Pts',(0.130456900999943,12.2,4.41063825499998));
#332150=CARTESIAN_POINT('Ctrl Pts',(0.130456900999943,5.2,4.41063825499998));
#332151=CARTESIAN_POINT('Ctrl Pts',(0.130456900999943,2.2,4.41063825499998));
#332152=CARTESIAN_POINT('Ctrl Pts',(0.129524589999944,12.2,4.40879495599999));
#332153=CARTESIAN_POINT('Ctrl Pts',(0.129524589999944,5.2,4.40879495599999));
#332154=CARTESIAN_POINT('Ctrl Pts',(0.129524589999944,2.2,4.40879495599999));
#332155=CARTESIAN_POINT('Ctrl Pts',(0.128596111999943,12.2,4.40695419999999));
#332156=CARTESIAN_POINT('Ctrl Pts',(0.128596111999943,5.2,4.40695419999999));
#332157=CARTESIAN_POINT('Ctrl Pts',(0.128596111999943,2.2,4.40695419999999));
#332158=CARTESIAN_POINT('Ctrl Pts',(0.127671463999944,12.2,4.40511599799999));
#332159=CARTESIAN_POINT('Ctrl Pts',(0.127671463999944,5.2,4.40511599799999));
#332160=CARTESIAN_POINT('Ctrl Pts',(0.127671463999944,2.2,4.40511599799999));
#332161=CARTESIAN_POINT('Ctrl Pts',(0.126750642999944,12.2,4.40328035999999));
#332162=CARTESIAN_POINT('Ctrl Pts',(0.126750642999944,5.2,4.40328035999999));
#332163=CARTESIAN_POINT('Ctrl Pts',(0.126750642999944,2.2,4.40328035999999));
#332164=CARTESIAN_POINT('Ctrl Pts',(0.125833642999943,12.2,4.40144729499998));
#332165=CARTESIAN_POINT('Ctrl Pts',(0.125833642999943,5.2,4.40144729499998));
#332166=CARTESIAN_POINT('Ctrl Pts',(0.125833642999943,2.2,4.40144729499998));
#332167=CARTESIAN_POINT('Ctrl Pts',(0.124920460999943,12.2,4.39961681499998));
#332168=CARTESIAN_POINT('Ctrl Pts',(0.124920460999943,5.2,4.39961681499998));
#332169=CARTESIAN_POINT('Ctrl Pts',(0.124920460999943,2.2,4.39961681499998));
#332170=CARTESIAN_POINT('Ctrl Pts',(0.124011093999944,12.2,4.39778892799998));
#332171=CARTESIAN_POINT('Ctrl Pts',(0.124011093999944,5.2,4.39778892799998));
#332172=CARTESIAN_POINT('Ctrl Pts',(0.124011093999944,2.2,4.39778892799998));
#332173=CARTESIAN_POINT('Ctrl Pts',(0.123105536999945,12.2,4.39596364399998));
#332174=CARTESIAN_POINT('Ctrl Pts',(0.123105536999945,5.2,4.39596364399998));
#332175=CARTESIAN_POINT('Ctrl Pts',(0.123105536999945,2.2,4.39596364399998));
#332176=CARTESIAN_POINT('Ctrl Pts',(0.122203784999944,12.2,4.39414097499998));
#332177=CARTESIAN_POINT('Ctrl Pts',(0.122203784999944,5.2,4.39414097499998));
#332178=CARTESIAN_POINT('Ctrl Pts',(0.122203784999944,2.2,4.39414097499998));
#332179=CARTESIAN_POINT('Ctrl Pts',(0.121305836999944,12.2,4.39232092799998));
#332180=CARTESIAN_POINT('Ctrl Pts',(0.121305836999944,5.2,4.39232092799998));
#332181=CARTESIAN_POINT('Ctrl Pts',(0.121305836999944,2.2,4.39232092799998));
#332182=CARTESIAN_POINT('Ctrl Pts',(0.120411685999944,12.2,4.39050351499999));
#332183=CARTESIAN_POINT('Ctrl Pts',(0.120411685999944,5.2,4.39050351499999));
#332184=CARTESIAN_POINT('Ctrl Pts',(0.120411685999944,2.2,4.39050351499999));
#332185=CARTESIAN_POINT('Ctrl Pts',(0.119521329999944,12.2,4.38868874599999));
#332186=CARTESIAN_POINT('Ctrl Pts',(0.119521329999944,5.2,4.38868874599999));
#332187=CARTESIAN_POINT('Ctrl Pts',(0.119521329999944,2.2,4.38868874599999));
#332188=CARTESIAN_POINT('Ctrl Pts',(0.118634763999944,12.2,4.38687662999998));
#332189=CARTESIAN_POINT('Ctrl Pts',(0.118634763999944,5.2,4.38687662999998));
#332190=CARTESIAN_POINT('Ctrl Pts',(0.118634763999944,2.2,4.38687662999998));
#332191=CARTESIAN_POINT('Ctrl Pts',(0.117751984999943,12.2,4.38506717799999));
#332192=CARTESIAN_POINT('Ctrl Pts',(0.117751984999943,5.2,4.38506717799999));
#332193=CARTESIAN_POINT('Ctrl Pts',(0.117751984999943,2.2,4.38506717799999));
#332194=CARTESIAN_POINT('Ctrl Pts',(0.116872986999944,12.2,4.38326039899999));
#332195=CARTESIAN_POINT('Ctrl Pts',(0.116872986999944,5.2,4.38326039899999));
#332196=CARTESIAN_POINT('Ctrl Pts',(0.116872986999944,2.2,4.38326039899999));
#332197=CARTESIAN_POINT('Ctrl Pts',(0.115997767999945,12.2,4.38145630499999));
#332198=CARTESIAN_POINT('Ctrl Pts',(0.115997767999945,5.2,4.38145630499999));
#332199=CARTESIAN_POINT('Ctrl Pts',(0.115997767999945,2.2,4.38145630499999));
#332200=CARTESIAN_POINT('Ctrl Pts',(0.115126322999943,12.2,4.37965490299998));
#332201=CARTESIAN_POINT('Ctrl Pts',(0.115126322999943,5.2,4.37965490299998));
#332202=CARTESIAN_POINT('Ctrl Pts',(0.115126322999943,2.2,4.37965490299998));
#332203=CARTESIAN_POINT('Ctrl Pts',(0.114258647999945,12.2,4.37785620599998));
#332204=CARTESIAN_POINT('Ctrl Pts',(0.114258647999945,5.2,4.37785620599998));
#332205=CARTESIAN_POINT('Ctrl Pts',(0.114258647999945,2.2,4.37785620599998));
#332206=CARTESIAN_POINT('Ctrl Pts',(0.113394737999943,12.2,4.37606022199999));
#332207=CARTESIAN_POINT('Ctrl Pts',(0.113394737999943,5.2,4.37606022199999));
#332208=CARTESIAN_POINT('Ctrl Pts',(0.113394737999943,2.2,4.37606022199999));
#332209=CARTESIAN_POINT('Ctrl Pts',(0.112534589999944,12.2,4.37426696199999));
#332210=CARTESIAN_POINT('Ctrl Pts',(0.112534589999944,5.2,4.37426696199999));
#332211=CARTESIAN_POINT('Ctrl Pts',(0.112534589999944,2.2,4.37426696199999));
#332212=CARTESIAN_POINT('Ctrl Pts',(0.111678198999944,12.2,4.37247643699998));
#332213=CARTESIAN_POINT('Ctrl Pts',(0.111678198999944,5.2,4.37247643699998));
#332214=CARTESIAN_POINT('Ctrl Pts',(0.111678198999944,2.2,4.37247643699998));
#332215=CARTESIAN_POINT('Ctrl Pts',(0.110825560999944,12.2,4.37068865499998));
#332216=CARTESIAN_POINT('Ctrl Pts',(0.110825560999944,5.2,4.37068865499998));
#332217=CARTESIAN_POINT('Ctrl Pts',(0.110825560999944,2.2,4.37068865499998));
#332218=CARTESIAN_POINT('Ctrl Pts',(0.109976672999944,12.2,4.36890362799998));
#332219=CARTESIAN_POINT('Ctrl Pts',(0.109976672999944,5.2,4.36890362799998));
#332220=CARTESIAN_POINT('Ctrl Pts',(0.109976672999944,2.2,4.36890362799998));
#332221=CARTESIAN_POINT('Ctrl Pts',(0.109131527999944,12.2,4.36712136499998));
#332222=CARTESIAN_POINT('Ctrl Pts',(0.109131527999944,5.2,4.36712136499998));
#332223=CARTESIAN_POINT('Ctrl Pts',(0.109131527999944,2.2,4.36712136499998));
#332224=CARTESIAN_POINT('Ctrl Pts',(0.108290123999945,12.2,4.36534187599998));
#332225=CARTESIAN_POINT('Ctrl Pts',(0.108290123999945,5.2,4.36534187599998));
#332226=CARTESIAN_POINT('Ctrl Pts',(0.108290123999945,2.2,4.36534187599998));
#332227=CARTESIAN_POINT('Ctrl Pts',(0.107452456999945,12.2,4.36356517299998));
#332228=CARTESIAN_POINT('Ctrl Pts',(0.107452456999945,5.2,4.36356517299998));
#332229=CARTESIAN_POINT('Ctrl Pts',(0.107452456999945,2.2,4.36356517299998));
#332230=CARTESIAN_POINT('Ctrl Pts',(0.106618521999945,12.2,4.36179126299999));
#332231=CARTESIAN_POINT('Ctrl Pts',(0.106618521999945,5.2,4.36179126299999));
#332232=CARTESIAN_POINT('Ctrl Pts',(0.106618521999945,2.2,4.36179126299999));
#332233=CARTESIAN_POINT('Ctrl Pts',(0.105788312999945,12.2,4.36002015999998));
#332234=CARTESIAN_POINT('Ctrl Pts',(0.105788312999945,5.2,4.36002015999998));
#332235=CARTESIAN_POINT('Ctrl Pts',(0.105788312999945,2.2,4.36002015999998));
#332236=CARTESIAN_POINT('Ctrl Pts',(0.104961826999944,12.2,4.35825186999999));
#332237=CARTESIAN_POINT('Ctrl Pts',(0.104961826999944,5.2,4.35825186999999));
#332238=CARTESIAN_POINT('Ctrl Pts',(0.104961826999944,2.2,4.35825186999999));
#332239=CARTESIAN_POINT('Ctrl Pts',(0.104139060999945,12.2,4.35648640699998));
#332240=CARTESIAN_POINT('Ctrl Pts',(0.104139060999945,5.2,4.35648640699998));
#332241=CARTESIAN_POINT('Ctrl Pts',(0.104139060999945,2.2,4.35648640699998));
#332242=CARTESIAN_POINT('Ctrl Pts',(0.103320008999944,12.2,4.35472377899998));
#332243=CARTESIAN_POINT('Ctrl Pts',(0.103320008999944,5.2,4.35472377899998));
#332244=CARTESIAN_POINT('Ctrl Pts',(0.103320008999944,2.2,4.35472377899998));
#332245=CARTESIAN_POINT('Ctrl Pts',(0.102504665999945,12.2,4.35296399599999));
#332246=CARTESIAN_POINT('Ctrl Pts',(0.102504665999945,5.2,4.35296399599999));
#332247=CARTESIAN_POINT('Ctrl Pts',(0.102504665999945,2.2,4.35296399599999));
#332248=CARTESIAN_POINT('Ctrl Pts',(0.101693028999945,12.2,4.35120706999999));
#332249=CARTESIAN_POINT('Ctrl Pts',(0.101693028999945,5.2,4.35120706999999));
#332250=CARTESIAN_POINT('Ctrl Pts',(0.101693028999945,2.2,4.35120706999999));
#332251=CARTESIAN_POINT('Ctrl Pts',(0.100885093999944,12.2,4.34945300999999));
#332252=CARTESIAN_POINT('Ctrl Pts',(0.100885093999944,5.2,4.34945300999999));
#332253=CARTESIAN_POINT('Ctrl Pts',(0.100885093999944,2.2,4.34945300999999));
#332254=CARTESIAN_POINT('Ctrl Pts',(0.100080853999945,12.2,4.34770182599999));
#332255=CARTESIAN_POINT('Ctrl Pts',(0.100080853999945,5.2,4.34770182599999));
#332256=CARTESIAN_POINT('Ctrl Pts',(0.100080853999945,2.2,4.34770182599999));
#332257=CARTESIAN_POINT('Ctrl Pts',(0.0992803059999436,12.2,4.34595352899999));
#332258=CARTESIAN_POINT('Ctrl Pts',(0.0992803059999436,5.2,4.34595352899999));
#332259=CARTESIAN_POINT('Ctrl Pts',(0.0992803059999436,2.2,4.34595352899999));
#332260=CARTESIAN_POINT('Ctrl Pts',(0.0984834469999452,12.2,4.34420812899998));
#332261=CARTESIAN_POINT('Ctrl Pts',(0.0984834469999452,5.2,4.34420812899998));
#332262=CARTESIAN_POINT('Ctrl Pts',(0.0984834469999452,2.2,4.34420812899998));
#332263=CARTESIAN_POINT('Ctrl Pts',(0.0976902699999449,12.2,4.34246563599999));
#332264=CARTESIAN_POINT('Ctrl Pts',(0.0976902699999449,5.2,4.34246563599999));
#332265=CARTESIAN_POINT('Ctrl Pts',(0.0976902699999449,2.2,4.34246563599999));
#332266=CARTESIAN_POINT('Ctrl Pts',(0.0969007709999448,12.2,4.34072606099999));
#332267=CARTESIAN_POINT('Ctrl Pts',(0.0969007709999448,5.2,4.34072606099999));
#332268=CARTESIAN_POINT('Ctrl Pts',(0.0969007709999448,2.2,4.34072606099999));
#332269=CARTESIAN_POINT('Ctrl Pts',(0.0961149459999433,12.2,4.33898941299999));
#332270=CARTESIAN_POINT('Ctrl Pts',(0.0961149459999433,5.2,4.33898941299999));
#332271=CARTESIAN_POINT('Ctrl Pts',(0.0961149459999433,2.2,4.33898941299999));
#332272=CARTESIAN_POINT('Ctrl Pts',(0.0953327899999434,12.2,4.33725570399999));
#332273=CARTESIAN_POINT('Ctrl Pts',(0.0953327899999434,5.2,4.33725570399999));
#332274=CARTESIAN_POINT('Ctrl Pts',(0.0953327899999434,2.2,4.33725570399999));
#332275=CARTESIAN_POINT('Ctrl Pts',(0.0945542979999436,12.2,4.33552494299998));
#332276=CARTESIAN_POINT('Ctrl Pts',(0.0945542979999436,5.2,4.33552494299998));
#332277=CARTESIAN_POINT('Ctrl Pts',(0.0945542979999436,2.2,4.33552494299998));
#332278=CARTESIAN_POINT('Ctrl Pts',(0.0937794679999449,12.2,4.33379714099999));
#332279=CARTESIAN_POINT('Ctrl Pts',(0.0937794679999449,5.2,4.33379714099999));
#332280=CARTESIAN_POINT('Ctrl Pts',(0.0937794679999449,2.2,4.33379714099999));
#332281=CARTESIAN_POINT('Ctrl Pts',(0.0930082919999442,12.2,4.33207230799999));
#332282=CARTESIAN_POINT('Ctrl Pts',(0.0930082919999442,5.2,4.33207230799999));
#332283=CARTESIAN_POINT('Ctrl Pts',(0.0930082919999442,2.2,4.33207230799999));
#332284=CARTESIAN_POINT('Ctrl Pts',(0.0922407659999447,12.2,4.33035045399999));
#332285=CARTESIAN_POINT('Ctrl Pts',(0.0922407659999447,5.2,4.33035045399999));
#332286=CARTESIAN_POINT('Ctrl Pts',(0.0922407659999447,2.2,4.33035045399999));
#332287=CARTESIAN_POINT('Ctrl Pts',(0.0914768859999437,12.2,4.32863159099998));
#332288=CARTESIAN_POINT('Ctrl Pts',(0.0914768859999437,5.2,4.32863159099998));
#332289=CARTESIAN_POINT('Ctrl Pts',(0.0914768859999437,2.2,4.32863159099998));
#332290=CARTESIAN_POINT('Ctrl Pts',(0.0907166469999443,12.2,4.32691572699999));
#332291=CARTESIAN_POINT('Ctrl Pts',(0.0907166469999443,5.2,4.32691572699999));
#332292=CARTESIAN_POINT('Ctrl Pts',(0.0907166469999443,2.2,4.32691572699999));
#332293=CARTESIAN_POINT('Ctrl Pts',(0.0899600449999449,12.2,4.32520287399999));
#332294=CARTESIAN_POINT('Ctrl Pts',(0.0899600449999449,5.2,4.32520287399999));
#332295=CARTESIAN_POINT('Ctrl Pts',(0.0899600449999449,2.2,4.32520287399999));
#332296=CARTESIAN_POINT('Ctrl Pts',(0.0892070729999439,12.2,4.32349304199998));
#332297=CARTESIAN_POINT('Ctrl Pts',(0.0892070729999439,5.2,4.32349304199998));
#332298=CARTESIAN_POINT('Ctrl Pts',(0.0892070729999439,2.2,4.32349304199998));
#332299=CARTESIAN_POINT('Ctrl Pts',(0.0884577279999454,12.2,4.32178624099999));
#332300=CARTESIAN_POINT('Ctrl Pts',(0.0884577279999454,5.2,4.32178624099999));
#332301=CARTESIAN_POINT('Ctrl Pts',(0.0884577279999454,2.2,4.32178624099999));
#332302=CARTESIAN_POINT('Ctrl Pts',(0.0877120049999436,12.2,4.32008248299999));
#332303=CARTESIAN_POINT('Ctrl Pts',(0.0877120049999436,5.2,4.32008248299999));
#332304=CARTESIAN_POINT('Ctrl Pts',(0.0877120049999436,2.2,4.32008248299999));
#332305=CARTESIAN_POINT('Ctrl Pts',(0.0869698999999446,12.2,4.31838177599998));
#332306=CARTESIAN_POINT('Ctrl Pts',(0.0869698999999446,5.2,4.31838177599998));
#332307=CARTESIAN_POINT('Ctrl Pts',(0.0869698999999446,2.2,4.31838177599998));
#332308=CARTESIAN_POINT('Ctrl Pts',(0.0862314059999447,12.2,4.31668413199999));
#332309=CARTESIAN_POINT('Ctrl Pts',(0.0862314059999447,5.2,4.31668413199999));
#332310=CARTESIAN_POINT('Ctrl Pts',(0.0862314059999447,2.2,4.31668413199999));
#332311=CARTESIAN_POINT('Ctrl Pts',(0.0854965199999447,12.2,4.31498956099999));
#332312=CARTESIAN_POINT('Ctrl Pts',(0.0854965199999447,5.2,4.31498956099999));
#332313=CARTESIAN_POINT('Ctrl Pts',(0.0854965199999447,2.2,4.31498956099999));
#332314=CARTESIAN_POINT('Ctrl Pts',(0.084765235999944,12.2,4.31329807399998));
#332315=CARTESIAN_POINT('Ctrl Pts',(0.084765235999944,5.2,4.31329807399998));
#332316=CARTESIAN_POINT('Ctrl Pts',(0.084765235999944,2.2,4.31329807399998));
#332317=CARTESIAN_POINT('Ctrl Pts',(0.0840375479999445,12.2,4.31160968099999));
#332318=CARTESIAN_POINT('Ctrl Pts',(0.0840375479999445,5.2,4.31160968099999));
#332319=CARTESIAN_POINT('Ctrl Pts',(0.0840375479999445,2.2,4.31160968099999));
#332320=CARTESIAN_POINT('Ctrl Pts',(0.0833134539999436,12.2,4.30992439199999));
#332321=CARTESIAN_POINT('Ctrl Pts',(0.0833134539999436,5.2,4.30992439199999));
#332322=CARTESIAN_POINT('Ctrl Pts',(0.0833134539999436,2.2,4.30992439199999));
#332323=CARTESIAN_POINT('Ctrl Pts',(0.0825929469999431,12.2,4.30824221899999));
#332324=CARTESIAN_POINT('Ctrl Pts',(0.0825929469999431,5.2,4.30824221899999));
#332325=CARTESIAN_POINT('Ctrl Pts',(0.0825929469999431,2.2,4.30824221899999));
#332326=CARTESIAN_POINT('Ctrl Pts',(0.0818760219999448,12.2,4.30656317199999));
#332327=CARTESIAN_POINT('Ctrl Pts',(0.0818760219999448,5.2,4.30656317199999));
#332328=CARTESIAN_POINT('Ctrl Pts',(0.0818760219999448,2.2,4.30656317199999));
#332329=CARTESIAN_POINT('Ctrl Pts',(0.0811626739999449,12.2,4.30488725899998));
#332330=CARTESIAN_POINT('Ctrl Pts',(0.0811626739999449,5.2,4.30488725899998));
#332331=CARTESIAN_POINT('Ctrl Pts',(0.0811626739999449,2.2,4.30488725899998));
#332332=CARTESIAN_POINT('Ctrl Pts',(0.0804528979999442,12.2,4.30321449499999));
#332333=CARTESIAN_POINT('Ctrl Pts',(0.0804528979999442,5.2,4.30321449499999));
#332334=CARTESIAN_POINT('Ctrl Pts',(0.0804528979999442,2.2,4.30321449499999));
#332335=CARTESIAN_POINT('Ctrl Pts',(0.0797466899999433,12.2,4.30154488699999));
#332336=CARTESIAN_POINT('Ctrl Pts',(0.0797466899999433,5.2,4.30154488699999));
#332337=CARTESIAN_POINT('Ctrl Pts',(0.0797466899999433,2.2,4.30154488699999));
#332338=CARTESIAN_POINT('Ctrl Pts',(0.0790440439999451,12.2,4.29987844599999));
#332339=CARTESIAN_POINT('Ctrl Pts',(0.0790440439999451,5.2,4.29987844599999));
#332340=CARTESIAN_POINT('Ctrl Pts',(0.0790440439999451,2.2,4.29987844599999));
#332341=CARTESIAN_POINT('Ctrl Pts',(0.0783449549999438,12.2,4.29821518399999));
#332342=CARTESIAN_POINT('Ctrl Pts',(0.0783449549999438,5.2,4.29821518399999));
#332343=CARTESIAN_POINT('Ctrl Pts',(0.0783449549999438,2.2,4.29821518399999));
#332344=CARTESIAN_POINT('Ctrl Pts',(0.0776494169999431,12.2,4.29655511099998));
#332345=CARTESIAN_POINT('Ctrl Pts',(0.0776494169999431,5.2,4.29655511099998));
#332346=CARTESIAN_POINT('Ctrl Pts',(0.0776494169999431,2.2,4.29655511099998));
#332347=CARTESIAN_POINT('Ctrl Pts',(0.076957425999945,12.2,4.29489823699999));
#332348=CARTESIAN_POINT('Ctrl Pts',(0.076957425999945,5.2,4.29489823699999));
#332349=CARTESIAN_POINT('Ctrl Pts',(0.076957425999945,2.2,4.29489823699999));
#332350=CARTESIAN_POINT('Ctrl Pts',(0.0762689769999447,12.2,4.29324457299998));
#332351=CARTESIAN_POINT('Ctrl Pts',(0.0762689769999447,5.2,4.29324457299998));
#332352=CARTESIAN_POINT('Ctrl Pts',(0.0762689769999447,2.2,4.29324457299998));
#332353=CARTESIAN_POINT('Ctrl Pts',(0.0755840629999438,12.2,4.29159412999999));
#332354=CARTESIAN_POINT('Ctrl Pts',(0.0755840629999438,5.2,4.29159412999999));
#332355=CARTESIAN_POINT('Ctrl Pts',(0.0755840629999438,2.2,4.29159412999999));
#332356=CARTESIAN_POINT('Ctrl Pts',(0.0749026809999442,12.2,4.28994691799998));
#332357=CARTESIAN_POINT('Ctrl Pts',(0.0749026809999442,5.2,4.28994691799998));
#332358=CARTESIAN_POINT('Ctrl Pts',(0.0749026809999442,2.2,4.28994691799998));
#332359=CARTESIAN_POINT('Ctrl Pts',(0.0742248239999454,12.2,4.28830294699999));
#332360=CARTESIAN_POINT('Ctrl Pts',(0.0742248239999454,5.2,4.28830294699999));
#332361=CARTESIAN_POINT('Ctrl Pts',(0.0742248239999454,2.2,4.28830294699999));
#332362=CARTESIAN_POINT('Ctrl Pts',(0.0735504879999438,12.2,4.28666222999999));
#332363=CARTESIAN_POINT('Ctrl Pts',(0.0735504879999438,5.2,4.28666222999999));
#332364=CARTESIAN_POINT('Ctrl Pts',(0.0735504879999438,2.2,4.28666222999999));
#332365=CARTESIAN_POINT('Ctrl Pts',(0.0728796659999442,12.2,4.28502477699999));
#332366=CARTESIAN_POINT('Ctrl Pts',(0.0728796659999442,5.2,4.28502477699999));
#332367=CARTESIAN_POINT('Ctrl Pts',(0.0728796659999442,2.2,4.28502477699999));
#332368=CARTESIAN_POINT('Ctrl Pts',(0.0722123539999442,12.2,4.28339059599999));
#332369=CARTESIAN_POINT('Ctrl Pts',(0.0722123539999442,5.2,4.28339059599999));
#332370=CARTESIAN_POINT('Ctrl Pts',(0.0722123539999442,2.2,4.28339059599999));
#332371=CARTESIAN_POINT('Ctrl Pts',(0.0715485469999444,12.2,4.28175969999998));
#332372=CARTESIAN_POINT('Ctrl Pts',(0.0715485469999444,5.2,4.28175969999998));
#332373=CARTESIAN_POINT('Ctrl Pts',(0.0715485469999444,2.2,4.28175969999998));
#332374=CARTESIAN_POINT('Ctrl Pts',(0.0708882379999431,12.2,4.28013209899999));
#332375=CARTESIAN_POINT('Ctrl Pts',(0.0708882379999431,5.2,4.28013209899999));
#332376=CARTESIAN_POINT('Ctrl Pts',(0.0708882379999431,2.2,4.28013209899999));
#332377=CARTESIAN_POINT('Ctrl Pts',(0.0702314229999445,12.2,4.27850780499998));
#332378=CARTESIAN_POINT('Ctrl Pts',(0.0702314229999445,5.2,4.27850780499998));
#332379=CARTESIAN_POINT('Ctrl Pts',(0.0702314229999445,2.2,4.27850780499998));
#332380=CARTESIAN_POINT('Ctrl Pts',(0.0695780959999437,12.2,4.27688682699999));
#332381=CARTESIAN_POINT('Ctrl Pts',(0.0695780959999437,5.2,4.27688682699999));
#332382=CARTESIAN_POINT('Ctrl Pts',(0.0695780959999437,2.2,4.27688682699999));
#332383=CARTESIAN_POINT('Ctrl Pts',(0.0689282519999446,12.2,4.27526917599998));
#332384=CARTESIAN_POINT('Ctrl Pts',(0.0689282519999446,5.2,4.27526917599998));
#332385=CARTESIAN_POINT('Ctrl Pts',(0.0689282519999446,2.2,4.27526917599998));
#332386=CARTESIAN_POINT('Ctrl Pts',(0.0682818839999444,12.2,4.27365486399999));
#332387=CARTESIAN_POINT('Ctrl Pts',(0.0682818839999444,5.2,4.27365486399999));
#332388=CARTESIAN_POINT('Ctrl Pts',(0.0682818839999444,2.2,4.27365486399999));
#332389=CARTESIAN_POINT('Ctrl Pts',(0.067638988999944,12.2,4.27204390099998));
#332390=CARTESIAN_POINT('Ctrl Pts',(0.067638988999944,5.2,4.27204390099998));
#332391=CARTESIAN_POINT('Ctrl Pts',(0.067638988999944,2.2,4.27204390099998));
#332392=CARTESIAN_POINT('Ctrl Pts',(0.0669995589999439,12.2,4.27043629599999));
#332393=CARTESIAN_POINT('Ctrl Pts',(0.0669995589999439,5.2,4.27043629599999));
#332394=CARTESIAN_POINT('Ctrl Pts',(0.0669995589999439,2.2,4.27043629599999));
#332395=CARTESIAN_POINT('Ctrl Pts',(0.0663635899999437,12.2,4.26883206299999));
#332396=CARTESIAN_POINT('Ctrl Pts',(0.0663635899999437,5.2,4.26883206299999));
#332397=CARTESIAN_POINT('Ctrl Pts',(0.0663635899999437,2.2,4.26883206299999));
#332398=CARTESIAN_POINT('Ctrl Pts',(0.065731074999944,12.2,4.26723121099998));
#332399=CARTESIAN_POINT('Ctrl Pts',(0.065731074999944,5.2,4.26723121099998));
#332400=CARTESIAN_POINT('Ctrl Pts',(0.065731074999944,2.2,4.26723121099998));
#332401=CARTESIAN_POINT('Ctrl Pts',(0.0651020109999434,12.2,4.26563375099998));
#332402=CARTESIAN_POINT('Ctrl Pts',(0.0651020109999434,5.2,4.26563375099998));
#332403=CARTESIAN_POINT('Ctrl Pts',(0.0651020109999434,2.2,4.26563375099998));
#332404=CARTESIAN_POINT('Ctrl Pts',(0.0644763889999444,12.2,4.26403969299999));
#332405=CARTESIAN_POINT('Ctrl Pts',(0.0644763889999444,5.2,4.26403969299999));
#332406=CARTESIAN_POINT('Ctrl Pts',(0.0644763889999444,2.2,4.26403969299999));
#332407=CARTESIAN_POINT('Ctrl Pts',(0.0638542059999436,12.2,4.26244904999999));
#332408=CARTESIAN_POINT('Ctrl Pts',(0.0638542059999436,5.2,4.26244904999999));
#332409=CARTESIAN_POINT('Ctrl Pts',(0.0638542059999436,2.2,4.26244904999999));
#332410=CARTESIAN_POINT('Ctrl Pts',(0.0632354539999447,12.2,4.26086183099999));
#332411=CARTESIAN_POINT('Ctrl Pts',(0.0632354539999447,5.2,4.26086183099999));
#332412=CARTESIAN_POINT('Ctrl Pts',(0.0632354539999447,2.2,4.26086183099999));
#332413=CARTESIAN_POINT('Ctrl Pts',(0.062620129999944,12.2,4.25927804699998));
#332414=CARTESIAN_POINT('Ctrl Pts',(0.062620129999944,5.2,4.25927804699998));
#332415=CARTESIAN_POINT('Ctrl Pts',(0.062620129999944,2.2,4.25927804699998));
#332416=CARTESIAN_POINT('Ctrl Pts',(0.0620082269999445,12.2,4.25769770899999));
#332417=CARTESIAN_POINT('Ctrl Pts',(0.0620082269999445,5.2,4.25769770899999));
#332418=CARTESIAN_POINT('Ctrl Pts',(0.0620082269999445,2.2,4.25769770899999));
#332419=CARTESIAN_POINT('Ctrl Pts',(0.0613997379999442,12.2,4.25612082899999));
#332420=CARTESIAN_POINT('Ctrl Pts',(0.0613997379999442,5.2,4.25612082899999));
#332421=CARTESIAN_POINT('Ctrl Pts',(0.0613997379999442,2.2,4.25612082899999));
#332422=CARTESIAN_POINT('Ctrl Pts',(0.0607946599999443,12.2,4.25454741599999));
#332423=CARTESIAN_POINT('Ctrl Pts',(0.0607946599999443,5.2,4.25454741599999));
#332424=CARTESIAN_POINT('Ctrl Pts',(0.0607946599999443,2.2,4.25454741599999));
#332425=CARTESIAN_POINT('Ctrl Pts',(0.0601929839999438,12.2,4.25297748199998));
#332426=CARTESIAN_POINT('Ctrl Pts',(0.0601929839999438,5.2,4.25297748199998));
#332427=CARTESIAN_POINT('Ctrl Pts',(0.0601929839999438,2.2,4.25297748199998));
#332428=CARTESIAN_POINT('Ctrl Pts',(0.0595947059999435,12.2,4.25141103799999));
#332429=CARTESIAN_POINT('Ctrl Pts',(0.0595947059999435,5.2,4.25141103799999));
#332430=CARTESIAN_POINT('Ctrl Pts',(0.0595947059999435,2.2,4.25141103799999));
#332431=CARTESIAN_POINT('Ctrl Pts',(0.0589998189999441,12.2,4.24984809499998));
#332432=CARTESIAN_POINT('Ctrl Pts',(0.0589998189999441,5.2,4.24984809499998));
#332433=CARTESIAN_POINT('Ctrl Pts',(0.0589998189999441,2.2,4.24984809499998));
#332434=CARTESIAN_POINT('Ctrl Pts',(0.0584083189999451,12.2,4.24828866399999));
#332435=CARTESIAN_POINT('Ctrl Pts',(0.0584083189999451,5.2,4.24828866399999));
#332436=CARTESIAN_POINT('Ctrl Pts',(0.0584083189999451,2.2,4.24828866399999));
#332437=CARTESIAN_POINT('Ctrl Pts',(0.0578201979999437,12.2,4.24673275499998));
#332438=CARTESIAN_POINT('Ctrl Pts',(0.0578201979999437,5.2,4.24673275499998));
#332439=CARTESIAN_POINT('Ctrl Pts',(0.0578201979999437,2.2,4.24673275499998));
#332440=CARTESIAN_POINT('Ctrl Pts',(0.0572354519999441,12.2,4.24518037899999));
#332441=CARTESIAN_POINT('Ctrl Pts',(0.0572354519999441,5.2,4.24518037899999));
#332442=CARTESIAN_POINT('Ctrl Pts',(0.0572354519999441,2.2,4.24518037899999));
#332443=CARTESIAN_POINT('Ctrl Pts',(0.0566540739999444,12.2,4.24363154799998));
#332444=CARTESIAN_POINT('Ctrl Pts',(0.0566540739999444,5.2,4.24363154799998));
#332445=CARTESIAN_POINT('Ctrl Pts',(0.0566540739999444,2.2,4.24363154799998));
#332446=CARTESIAN_POINT('Ctrl Pts',(0.0560760579999442,12.2,4.24208627199998));
#332447=CARTESIAN_POINT('Ctrl Pts',(0.0560760579999442,5.2,4.24208627199998));
#332448=CARTESIAN_POINT('Ctrl Pts',(0.0560760579999442,2.2,4.24208627199998));
#332449=CARTESIAN_POINT('Ctrl Pts',(0.0555013979999441,12.2,4.24054456199999));
#332450=CARTESIAN_POINT('Ctrl Pts',(0.0555013979999441,5.2,4.24054456199999));
#332451=CARTESIAN_POINT('Ctrl Pts',(0.0555013979999441,2.2,4.24054456199999));
#332452=CARTESIAN_POINT('Ctrl Pts',(0.0549300879999437,12.2,4.23900643199998));
#332453=CARTESIAN_POINT('Ctrl Pts',(0.0549300879999437,5.2,4.23900643199998));
#332454=CARTESIAN_POINT('Ctrl Pts',(0.0549300879999437,2.2,4.23900643199998));
#332455=CARTESIAN_POINT('Ctrl Pts',(0.0543621219999435,12.2,4.23747188799998));
#332456=CARTESIAN_POINT('Ctrl Pts',(0.0543621219999435,5.2,4.23747188799998));
#332457=CARTESIAN_POINT('Ctrl Pts',(0.0543621219999435,2.2,4.23747188799998));
#332458=CARTESIAN_POINT('Ctrl Pts',(0.0537974939999442,12.2,4.23594094499999));
#332459=CARTESIAN_POINT('Ctrl Pts',(0.0537974939999442,5.2,4.23594094499999));
#332460=CARTESIAN_POINT('Ctrl Pts',(0.0537974939999442,2.2,4.23594094499999));
#332461=CARTESIAN_POINT('Ctrl Pts',(0.053236196999944,12.2,4.23441361199998));
#332462=CARTESIAN_POINT('Ctrl Pts',(0.053236196999944,5.2,4.23441361199998));
#332463=CARTESIAN_POINT('Ctrl Pts',(0.053236196999944,2.2,4.23441361199998));
#332464=CARTESIAN_POINT('Ctrl Pts',(0.0526782259999448,12.2,4.23288990099999));
#332465=CARTESIAN_POINT('Ctrl Pts',(0.0526782259999448,5.2,4.23288990099999));
#332466=CARTESIAN_POINT('Ctrl Pts',(0.0526782259999448,2.2,4.23288990099999));
#332467=CARTESIAN_POINT('Ctrl Pts',(0.0521235739999448,12.2,4.23136982199999));
#332468=CARTESIAN_POINT('Ctrl Pts',(0.0521235739999448,5.2,4.23136982199999));
#332469=CARTESIAN_POINT('Ctrl Pts',(0.0521235739999448,2.2,4.23136982199999));
#332470=CARTESIAN_POINT('Ctrl Pts',(0.0515722369999438,12.2,4.22985338699998));
#332471=CARTESIAN_POINT('Ctrl Pts',(0.0515722369999438,5.2,4.22985338699998));
#332472=CARTESIAN_POINT('Ctrl Pts',(0.0515722369999438,2.2,4.22985338699998));
#332473=CARTESIAN_POINT('Ctrl Pts',(0.0510242039999442,12.2,4.22834060799998));
#332474=CARTESIAN_POINT('Ctrl Pts',(0.0510242039999442,5.2,4.22834060799998));
#332475=CARTESIAN_POINT('Ctrl Pts',(0.0510242039999442,2.2,4.22834060799998));
#332476=CARTESIAN_POINT('Ctrl Pts',(0.0504794739999448,12.2,4.22683149399998));
#332477=CARTESIAN_POINT('Ctrl Pts',(0.0504794739999448,5.2,4.22683149399998));
#332478=CARTESIAN_POINT('Ctrl Pts',(0.0504794739999448,2.2,4.22683149399998));
#332479=CARTESIAN_POINT('Ctrl Pts',(0.0499380369999436,12.2,4.22532605799999));
#332480=CARTESIAN_POINT('Ctrl Pts',(0.0499380369999436,5.2,4.22532605799999));
#332481=CARTESIAN_POINT('Ctrl Pts',(0.0499380369999436,2.2,4.22532605799999));
#332482=CARTESIAN_POINT('Ctrl Pts',(0.0493998889999436,12.2,4.22382430899999));
#332483=CARTESIAN_POINT('Ctrl Pts',(0.0493998889999436,5.2,4.22382430899999));
#332484=CARTESIAN_POINT('Ctrl Pts',(0.0493998889999436,2.2,4.22382430899999));
#332485=CARTESIAN_POINT('Ctrl Pts',(0.0488650229999443,12.2,4.22232625999998));
#332486=CARTESIAN_POINT('Ctrl Pts',(0.0488650229999443,5.2,4.22232625999998));
#332487=CARTESIAN_POINT('Ctrl Pts',(0.0488650229999443,2.2,4.22232625999998));
#332488=CARTESIAN_POINT('Ctrl Pts',(0.0483334319999451,12.2,4.22083192199998));
#332489=CARTESIAN_POINT('Ctrl Pts',(0.0483334319999451,5.2,4.22083192199998));
#332490=CARTESIAN_POINT('Ctrl Pts',(0.0483334319999451,2.2,4.22083192199998));
#332491=CARTESIAN_POINT('Ctrl Pts',(0.0478051099999444,12.2,4.21934130599999));
#332492=CARTESIAN_POINT('Ctrl Pts',(0.0478051099999444,5.2,4.21934130599999));
#332493=CARTESIAN_POINT('Ctrl Pts',(0.0478051099999444,2.2,4.21934130599999));
#332494=CARTESIAN_POINT('Ctrl Pts',(0.0472800499999448,12.2,4.21785442199998));
#332495=CARTESIAN_POINT('Ctrl Pts',(0.0472800499999448,5.2,4.21785442199998));
#332496=CARTESIAN_POINT('Ctrl Pts',(0.0472800499999448,2.2,4.21785442199998));
#332497=CARTESIAN_POINT('Ctrl Pts',(0.046758246999945,12.2,4.21637128399999));
#332498=CARTESIAN_POINT('Ctrl Pts',(0.046758246999945,5.2,4.21637128399999));
#332499=CARTESIAN_POINT('Ctrl Pts',(0.046758246999945,2.2,4.21637128399999));
#332500=CARTESIAN_POINT('Ctrl Pts',(0.0462396929999442,12.2,4.21489189899999));
#332501=CARTESIAN_POINT('Ctrl Pts',(0.0462396929999442,5.2,4.21489189899999));
#332502=CARTESIAN_POINT('Ctrl Pts',(0.0462396929999442,2.2,4.21489189899999));
#332503=CARTESIAN_POINT('Ctrl Pts',(0.0457243829999443,12.2,4.21341628199999));
#332504=CARTESIAN_POINT('Ctrl Pts',(0.0457243829999443,5.2,4.21341628199999));
#332505=CARTESIAN_POINT('Ctrl Pts',(0.0457243829999443,2.2,4.21341628199999));
#332506=CARTESIAN_POINT('Ctrl Pts',(0.0452123089999434,12.2,4.21194444299999));
#332507=CARTESIAN_POINT('Ctrl Pts',(0.0452123089999434,5.2,4.21194444299999));
#332508=CARTESIAN_POINT('Ctrl Pts',(0.0452123089999434,2.2,4.21194444299999));
#332509=CARTESIAN_POINT('Ctrl Pts',(0.0447034649999445,12.2,4.21047639199998));
#332510=CARTESIAN_POINT('Ctrl Pts',(0.0447034649999445,5.2,4.21047639199998));
#332511=CARTESIAN_POINT('Ctrl Pts',(0.0447034649999445,2.2,4.21047639199998));
#332512=CARTESIAN_POINT('Ctrl Pts',(0.0441978439999446,12.2,4.20901214299998));
#332513=CARTESIAN_POINT('Ctrl Pts',(0.0441978439999446,5.2,4.20901214299998));
#332514=CARTESIAN_POINT('Ctrl Pts',(0.0441978439999446,2.2,4.20901214299998));
#332515=CARTESIAN_POINT('Ctrl Pts',(0.0436954399999434,12.2,4.20755170399998));
#332516=CARTESIAN_POINT('Ctrl Pts',(0.0436954399999434,5.2,4.20755170399998));
#332517=CARTESIAN_POINT('Ctrl Pts',(0.0436954399999434,2.2,4.20755170399998));
#332518=CARTESIAN_POINT('Ctrl Pts',(0.0431962469999447,12.2,4.20609508999998));
#332519=CARTESIAN_POINT('Ctrl Pts',(0.0431962469999447,5.2,4.20609508999998));
#332520=CARTESIAN_POINT('Ctrl Pts',(0.0431962469999447,2.2,4.20609508999998));
#332521=CARTESIAN_POINT('Ctrl Pts',(0.0427002569999435,12.2,4.20464230799999));
#332522=CARTESIAN_POINT('Ctrl Pts',(0.0427002569999435,5.2,4.20464230799999));
#332523=CARTESIAN_POINT('Ctrl Pts',(0.0427002569999435,2.2,4.20464230799999));
#332524=CARTESIAN_POINT('Ctrl Pts',(0.0422074639999437,12.2,4.20319337299999));
#332525=CARTESIAN_POINT('Ctrl Pts',(0.0422074639999437,5.2,4.20319337299999));
#332526=CARTESIAN_POINT('Ctrl Pts',(0.0422074639999437,2.2,4.20319337299999));
#332527=CARTESIAN_POINT('Ctrl Pts',(0.0417178609999436,12.2,4.20174829399999));
#332528=CARTESIAN_POINT('Ctrl Pts',(0.0417178609999436,5.2,4.20174829399999));
#332529=CARTESIAN_POINT('Ctrl Pts',(0.0417178609999436,2.2,4.20174829399999));
#332530=CARTESIAN_POINT('Ctrl Pts',(0.0412314409999437,12.2,4.20030708399998));
#332531=CARTESIAN_POINT('Ctrl Pts',(0.0412314409999437,5.2,4.20030708399998));
#332532=CARTESIAN_POINT('Ctrl Pts',(0.0412314409999437,2.2,4.20030708399998));
#332533=CARTESIAN_POINT('Ctrl Pts',(0.0407481979999447,12.2,4.19886975299999));
#332534=CARTESIAN_POINT('Ctrl Pts',(0.0407481979999447,5.2,4.19886975299999));
#332535=CARTESIAN_POINT('Ctrl Pts',(0.0407481979999447,2.2,4.19886975299999));
#332536=CARTESIAN_POINT('Ctrl Pts',(0.0402681239999436,12.2,4.19743631399999));
#332537=CARTESIAN_POINT('Ctrl Pts',(0.0402681239999436,5.2,4.19743631399999));
#332538=CARTESIAN_POINT('Ctrl Pts',(0.0402681239999436,2.2,4.19743631399999));
#332539=CARTESIAN_POINT('Ctrl Pts',(0.0397912139999446,12.2,4.19600677699999));
#332540=CARTESIAN_POINT('Ctrl Pts',(0.0397912139999446,5.2,4.19600677699999));
#332541=CARTESIAN_POINT('Ctrl Pts',(0.0397912139999446,2.2,4.19600677699999));
#332542=CARTESIAN_POINT('Ctrl Pts',(0.0393174589999445,12.2,4.19458115399999));
#332543=CARTESIAN_POINT('Ctrl Pts',(0.0393174589999445,5.2,4.19458115399999));
#332544=CARTESIAN_POINT('Ctrl Pts',(0.0393174589999445,2.2,4.19458115399999));
#332545=CARTESIAN_POINT('Ctrl Pts',(0.0388468539999442,12.2,4.19315945499999));
#332546=CARTESIAN_POINT('Ctrl Pts',(0.0388468539999442,5.2,4.19315945499999));
#332547=CARTESIAN_POINT('Ctrl Pts',(0.0388468539999442,2.2,4.19315945499999));
#332548=CARTESIAN_POINT('Ctrl Pts',(0.0383793899999441,12.2,4.19174169399999));
#332549=CARTESIAN_POINT('Ctrl Pts',(0.0383793899999441,5.2,4.19174169399999));
#332550=CARTESIAN_POINT('Ctrl Pts',(0.0383793899999441,2.2,4.19174169399999));
#332551=CARTESIAN_POINT('Ctrl Pts',(0.0379150629999447,12.2,4.19032788099998));
#332552=CARTESIAN_POINT('Ctrl Pts',(0.0379150629999447,5.2,4.19032788099998));
#332553=CARTESIAN_POINT('Ctrl Pts',(0.0379150629999447,2.2,4.19032788099998));
#332554=CARTESIAN_POINT('Ctrl Pts',(0.0374538629999443,12.2,4.18891802799998));
#332555=CARTESIAN_POINT('Ctrl Pts',(0.0374538629999443,5.2,4.18891802799998));
#332556=CARTESIAN_POINT('Ctrl Pts',(0.0374538629999443,2.2,4.18891802799998));
#332557=CARTESIAN_POINT('Ctrl Pts',(0.0369957849999436,12.2,4.18751214499999));
#332558=CARTESIAN_POINT('Ctrl Pts',(0.0369957849999436,5.2,4.18751214499999));
#332559=CARTESIAN_POINT('Ctrl Pts',(0.0369957849999436,2.2,4.18751214499999));
#332560=CARTESIAN_POINT('Ctrl Pts',(0.036540819999944,12.2,4.18611024499998));
#332561=CARTESIAN_POINT('Ctrl Pts',(0.036540819999944,5.2,4.18611024499998));
#332562=CARTESIAN_POINT('Ctrl Pts',(0.036540819999944,2.2,4.18611024499998));
#332563=CARTESIAN_POINT('Ctrl Pts',(0.0360889629999439,12.2,4.18471233899999));
#332564=CARTESIAN_POINT('Ctrl Pts',(0.0360889629999439,5.2,4.18471233899999));
#332565=CARTESIAN_POINT('Ctrl Pts',(0.0360889629999439,2.2,4.18471233899999));
#332566=CARTESIAN_POINT('Ctrl Pts',(0.0356402039999448,12.2,4.18331843899999));
#332567=CARTESIAN_POINT('Ctrl Pts',(0.0356402039999448,5.2,4.18331843899999));
#332568=CARTESIAN_POINT('Ctrl Pts',(0.0356402039999448,2.2,4.18331843899999));
#332569=CARTESIAN_POINT('Ctrl Pts',(0.0351945409999443,12.2,4.18192855499999));
#332570=CARTESIAN_POINT('Ctrl Pts',(0.0351945409999443,5.2,4.18192855499999));
#332571=CARTESIAN_POINT('Ctrl Pts',(0.0351945409999443,2.2,4.18192855499999));
#332572=CARTESIAN_POINT('Ctrl Pts',(0.0347519609999447,12.2,4.18054269999999));
#332573=CARTESIAN_POINT('Ctrl Pts',(0.0347519609999447,5.2,4.18054269999999));
#332574=CARTESIAN_POINT('Ctrl Pts',(0.0347519609999447,2.2,4.18054269999999));
#332575=CARTESIAN_POINT('Ctrl Pts',(0.0343124599999445,12.2,4.17916088499998));
#332576=CARTESIAN_POINT('Ctrl Pts',(0.0343124599999445,5.2,4.17916088499998));
#332577=CARTESIAN_POINT('Ctrl Pts',(0.0343124599999445,2.2,4.17916088499998));
#332578=CARTESIAN_POINT('Ctrl Pts',(0.0338760309999431,12.2,4.17778312299999));
#332579=CARTESIAN_POINT('Ctrl Pts',(0.0338760309999431,5.2,4.17778312299999));
#332580=CARTESIAN_POINT('Ctrl Pts',(0.0338760309999431,2.2,4.17778312299999));
#332581=CARTESIAN_POINT('Ctrl Pts',(0.0334426659999443,12.2,4.17640942299998));
#332582=CARTESIAN_POINT('Ctrl Pts',(0.0334426659999443,5.2,4.17640942299998));
#332583=CARTESIAN_POINT('Ctrl Pts',(0.0334426659999443,2.2,4.17640942299998));
#332584=CARTESIAN_POINT('Ctrl Pts',(0.0330123569999441,12.2,4.17503979899998));
#332585=CARTESIAN_POINT('Ctrl Pts',(0.0330123569999441,5.2,4.17503979899998));
#332586=CARTESIAN_POINT('Ctrl Pts',(0.0330123569999441,2.2,4.17503979899998));
#332587=CARTESIAN_POINT('Ctrl Pts',(0.0325850979999431,12.2,4.17367426099998));
#332588=CARTESIAN_POINT('Ctrl Pts',(0.0325850979999431,5.2,4.17367426099998));
#332589=CARTESIAN_POINT('Ctrl Pts',(0.0325850979999431,2.2,4.17367426099998));
#332590=CARTESIAN_POINT('Ctrl Pts',(0.032160879999944,12.2,4.17231282099999));
#332591=CARTESIAN_POINT('Ctrl Pts',(0.032160879999944,5.2,4.17231282099999));
#332592=CARTESIAN_POINT('Ctrl Pts',(0.032160879999944,2.2,4.17231282099999));
#332593=CARTESIAN_POINT('Ctrl Pts',(0.031739697999944,12.2,4.17095549099999));
#332594=CARTESIAN_POINT('Ctrl Pts',(0.031739697999944,5.2,4.17095549099999));
#332595=CARTESIAN_POINT('Ctrl Pts',(0.031739697999944,2.2,4.17095549099999));
#332596=CARTESIAN_POINT('Ctrl Pts',(0.0313215419999435,12.2,4.16960228199999));
#332597=CARTESIAN_POINT('Ctrl Pts',(0.0313215419999435,5.2,4.16960228199999));
#332598=CARTESIAN_POINT('Ctrl Pts',(0.0313215419999435,2.2,4.16960228199999));
#332599=CARTESIAN_POINT('Ctrl Pts',(0.0309064059999453,12.2,4.16825320699999));
#332600=CARTESIAN_POINT('Ctrl Pts',(0.0309064059999453,5.2,4.16825320699999));
#332601=CARTESIAN_POINT('Ctrl Pts',(0.0309064059999453,2.2,4.16825320699999));
#332602=CARTESIAN_POINT('Ctrl Pts',(0.0304942829999444,12.2,4.16690827599999));
#332603=CARTESIAN_POINT('Ctrl Pts',(0.0304942829999444,5.2,4.16690827599999));
#332604=CARTESIAN_POINT('Ctrl Pts',(0.0304942829999444,2.2,4.16690827599999));
#332605=CARTESIAN_POINT('Ctrl Pts',(0.0300851639999444,12.2,4.16556750299999));
#332606=CARTESIAN_POINT('Ctrl Pts',(0.0300851639999444,5.2,4.16556750299999));
#332607=CARTESIAN_POINT('Ctrl Pts',(0.0300851639999444,2.2,4.16556750299999));
#332608=CARTESIAN_POINT('Ctrl Pts',(0.0296790429999449,12.2,4.16423089699999));
#332609=CARTESIAN_POINT('Ctrl Pts',(0.0296790429999449,5.2,4.16423089699999));
#332610=CARTESIAN_POINT('Ctrl Pts',(0.0296790429999449,2.2,4.16423089699999));
#332611=CARTESIAN_POINT('Ctrl Pts',(0.0292759109999441,12.2,4.16289846999998));
#332612=CARTESIAN_POINT('Ctrl Pts',(0.0292759109999441,5.2,4.16289846999998));
#332613=CARTESIAN_POINT('Ctrl Pts',(0.0292759109999441,2.2,4.16289846999998));
#332614=CARTESIAN_POINT('Ctrl Pts',(0.0288757609999435,12.2,4.16157023699999));
#332615=CARTESIAN_POINT('Ctrl Pts',(0.0288757609999435,5.2,4.16157023699999));
#332616=CARTESIAN_POINT('Ctrl Pts',(0.0288757609999435,2.2,4.16157023699999));
#332617=CARTESIAN_POINT('Ctrl Pts',(0.0284785859999437,12.2,4.16024620599998));
#332618=CARTESIAN_POINT('Ctrl Pts',(0.0284785859999437,5.2,4.16024620599998));
#332619=CARTESIAN_POINT('Ctrl Pts',(0.0284785859999437,2.2,4.16024620599998));
#332620=CARTESIAN_POINT('Ctrl Pts',(0.0280843769999439,12.2,4.15892639099999));
#332621=CARTESIAN_POINT('Ctrl Pts',(0.0280843769999439,5.2,4.15892639099999));
#332622=CARTESIAN_POINT('Ctrl Pts',(0.0280843769999439,2.2,4.15892639099999));
#332623=CARTESIAN_POINT('Ctrl Pts',(0.0276931269999447,12.2,4.15761080299998));
#332624=CARTESIAN_POINT('Ctrl Pts',(0.0276931269999447,5.2,4.15761080299998));
#332625=CARTESIAN_POINT('Ctrl Pts',(0.0276931269999447,2.2,4.15761080299998));
#332626=CARTESIAN_POINT('Ctrl Pts',(0.0273048289999433,12.2,4.15629945299998));
#332627=CARTESIAN_POINT('Ctrl Pts',(0.0273048289999433,5.2,4.15629945299998));
#332628=CARTESIAN_POINT('Ctrl Pts',(0.0273048289999433,2.2,4.15629945299998));
#332629=CARTESIAN_POINT('Ctrl Pts',(0.0269194739999445,12.2,4.15499235399999));
#332630=CARTESIAN_POINT('Ctrl Pts',(0.0269194739999445,5.2,4.15499235399999));
#332631=CARTESIAN_POINT('Ctrl Pts',(0.0269194739999445,2.2,4.15499235399999));
#332632=CARTESIAN_POINT('Ctrl Pts',(0.0265370559999434,12.2,4.15368951899998));
#332633=CARTESIAN_POINT('Ctrl Pts',(0.0265370559999434,5.2,4.15368951899998));
#332634=CARTESIAN_POINT('Ctrl Pts',(0.0265370559999434,2.2,4.15368951899998));
#332635=CARTESIAN_POINT('Ctrl Pts',(0.0261575649999435,12.2,4.15239095699998));
#332636=CARTESIAN_POINT('Ctrl Pts',(0.0261575649999435,5.2,4.15239095699998));
#332637=CARTESIAN_POINT('Ctrl Pts',(0.0261575649999435,2.2,4.15239095699998));
#332638=CARTESIAN_POINT('Ctrl Pts',(0.0257809939999454,12.2,4.15109668199998));
#332639=CARTESIAN_POINT('Ctrl Pts',(0.0257809939999454,5.2,4.15109668199998));
#332640=CARTESIAN_POINT('Ctrl Pts',(0.0257809939999454,2.2,4.15109668199998));
#332641=CARTESIAN_POINT('Ctrl Pts',(0.025407334999944,12.2,4.14980670399999));
#332642=CARTESIAN_POINT('Ctrl Pts',(0.025407334999944,5.2,4.14980670399999));
#332643=CARTESIAN_POINT('Ctrl Pts',(0.025407334999944,2.2,4.14980670399999));
#332644=CARTESIAN_POINT('Ctrl Pts',(0.0250365809999431,12.2,4.14852103699998));
#332645=CARTESIAN_POINT('Ctrl Pts',(0.0250365809999431,5.2,4.14852103699998));
#332646=CARTESIAN_POINT('Ctrl Pts',(0.0250365809999431,2.2,4.14852103699998));
#332647=CARTESIAN_POINT('Ctrl Pts',(0.0246687219999442,12.2,4.14723969099998));
#332648=CARTESIAN_POINT('Ctrl Pts',(0.0246687219999442,5.2,4.14723969099998));
#332649=CARTESIAN_POINT('Ctrl Pts',(0.0246687219999442,2.2,4.14723969099998));
#332650=CARTESIAN_POINT('Ctrl Pts',(0.0243037529999446,12.2,4.14596267999999));
#332651=CARTESIAN_POINT('Ctrl Pts',(0.0243037529999446,5.2,4.14596267999999));
#332652=CARTESIAN_POINT('Ctrl Pts',(0.0243037529999446,2.2,4.14596267999999));
#332653=CARTESIAN_POINT('Ctrl Pts',(0.0239416629999434,12.2,4.14469001399999));
#332654=CARTESIAN_POINT('Ctrl Pts',(0.0239416629999434,5.2,4.14469001399999));
#332655=CARTESIAN_POINT('Ctrl Pts',(0.0239416629999434,2.2,4.14469001399999));
#332656=CARTESIAN_POINT('Ctrl Pts',(0.0235824469999446,12.2,4.14342170599999));
#332657=CARTESIAN_POINT('Ctrl Pts',(0.0235824469999446,5.2,4.14342170599999));
#332658=CARTESIAN_POINT('Ctrl Pts',(0.0235824469999446,2.2,4.14342170599999));
#332659=CARTESIAN_POINT('Ctrl Pts',(0.023226092999945,12.2,4.14215776799999));
#332660=CARTESIAN_POINT('Ctrl Pts',(0.023226092999945,5.2,4.14215776799999));
#332661=CARTESIAN_POINT('Ctrl Pts',(0.023226092999945,2.2,4.14215776799999));
#332662=CARTESIAN_POINT('Ctrl Pts',(0.0228725969999444,12.2,4.14089821099999));
#332663=CARTESIAN_POINT('Ctrl Pts',(0.0228725969999444,5.2,4.14089821099999));
#332664=CARTESIAN_POINT('Ctrl Pts',(0.0228725969999444,2.2,4.14089821099999));
#332665=CARTESIAN_POINT('Ctrl Pts',(0.0225219469999449,12.2,4.13964304799999));
#332666=CARTESIAN_POINT('Ctrl Pts',(0.0225219469999449,5.2,4.13964304799999));
#332667=CARTESIAN_POINT('Ctrl Pts',(0.0225219469999449,2.2,4.13964304799999));
#332668=CARTESIAN_POINT('Ctrl Pts',(0.022174136999944,12.2,4.13839229099998));
#332669=CARTESIAN_POINT('Ctrl Pts',(0.022174136999944,5.2,4.13839229099998));
#332670=CARTESIAN_POINT('Ctrl Pts',(0.022174136999944,2.2,4.13839229099998));
#332671=CARTESIAN_POINT('Ctrl Pts',(0.0218291599999443,12.2,4.13714595299999));
#332672=CARTESIAN_POINT('Ctrl Pts',(0.0218291599999443,5.2,4.13714595299999));
#332673=CARTESIAN_POINT('Ctrl Pts',(0.0218291599999443,2.2,4.13714595299999));
#332674=CARTESIAN_POINT('Ctrl Pts',(0.0214870049999438,12.2,4.13590404299998));
#332675=CARTESIAN_POINT('Ctrl Pts',(0.0214870049999438,5.2,4.13590404299998));
#332676=CARTESIAN_POINT('Ctrl Pts',(0.0214870049999438,2.2,4.13590404299998));
#332677=CARTESIAN_POINT('Ctrl Pts',(0.0211476659999443,12.2,4.13466657499999));
#332678=CARTESIAN_POINT('Ctrl Pts',(0.0211476659999443,5.2,4.13466657499999));
#332679=CARTESIAN_POINT('Ctrl Pts',(0.0211476659999443,2.2,4.13466657499999));
#332680=CARTESIAN_POINT('Ctrl Pts',(0.0208111309999437,12.2,4.13343356199999));
#332681=CARTESIAN_POINT('Ctrl Pts',(0.0208111309999437,5.2,4.13343356199999));
#332682=CARTESIAN_POINT('Ctrl Pts',(0.0208111309999437,2.2,4.13343356199999));
#332683=CARTESIAN_POINT('Ctrl Pts',(0.0204773969999439,12.2,4.13220501399999));
#332684=CARTESIAN_POINT('Ctrl Pts',(0.0204773969999439,5.2,4.13220501399999));
#332685=CARTESIAN_POINT('Ctrl Pts',(0.0204773969999439,2.2,4.13220501399999));
#332686=CARTESIAN_POINT('Ctrl Pts',(0.0201464519999439,12.2,4.13098094499999));
#332687=CARTESIAN_POINT('Ctrl Pts',(0.0201464519999439,5.2,4.13098094499999));
#332688=CARTESIAN_POINT('Ctrl Pts',(0.0201464519999439,2.2,4.13098094499999));
#332689=CARTESIAN_POINT('Ctrl Pts',(0.0198182879999453,12.2,4.12976136599998));
#332690=CARTESIAN_POINT('Ctrl Pts',(0.0198182879999453,5.2,4.12976136599998));
#332691=CARTESIAN_POINT('Ctrl Pts',(0.0198182879999453,2.2,4.12976136599998));
#332692=CARTESIAN_POINT('Ctrl Pts',(0.0194928969999442,12.2,4.12854628899999));
#332693=CARTESIAN_POINT('Ctrl Pts',(0.0194928969999442,5.2,4.12854628899999));
#332694=CARTESIAN_POINT('Ctrl Pts',(0.0194928969999442,2.2,4.12854628899999));
#332695=CARTESIAN_POINT('Ctrl Pts',(0.019170269999943,12.2,4.12733572799999));
#332696=CARTESIAN_POINT('Ctrl Pts',(0.019170269999943,5.2,4.12733572799999));
#332697=CARTESIAN_POINT('Ctrl Pts',(0.019170269999943,2.2,4.12733572799999));
#332698=CARTESIAN_POINT('Ctrl Pts',(0.0188503999999445,12.2,4.12612969199999));
#332699=CARTESIAN_POINT('Ctrl Pts',(0.0188503999999445,5.2,4.12612969199999));
#332700=CARTESIAN_POINT('Ctrl Pts',(0.0188503999999445,2.2,4.12612969199999));
#332701=CARTESIAN_POINT('Ctrl Pts',(0.0185332769999447,12.2,4.12492819699998));
#332702=CARTESIAN_POINT('Ctrl Pts',(0.0185332769999447,5.2,4.12492819699998));
#332703=CARTESIAN_POINT('Ctrl Pts',(0.0185332769999447,2.2,4.12492819699998));
#332704=CARTESIAN_POINT('Ctrl Pts',(0.0182188929999438,12.2,4.12373125199998));
#332705=CARTESIAN_POINT('Ctrl Pts',(0.0182188929999438,5.2,4.12373125199998));
#332706=CARTESIAN_POINT('Ctrl Pts',(0.0182188929999438,2.2,4.12373125199998));
#332707=CARTESIAN_POINT('Ctrl Pts',(0.0179072379999445,12.2,4.12253887099999));
#332708=CARTESIAN_POINT('Ctrl Pts',(0.0179072379999445,5.2,4.12253887099999));
#332709=CARTESIAN_POINT('Ctrl Pts',(0.0179072379999445,2.2,4.12253887099999));
#332710=CARTESIAN_POINT('Ctrl Pts',(0.0175983049999429,12.2,4.12135106499999));
#332711=CARTESIAN_POINT('Ctrl Pts',(0.0175983049999429,5.2,4.12135106499999));
#332712=CARTESIAN_POINT('Ctrl Pts',(0.0175983049999429,2.2,4.12135106499999));
#332713=CARTESIAN_POINT('Ctrl Pts',(0.0172920849999447,12.2,4.12016784699999));
#332714=CARTESIAN_POINT('Ctrl Pts',(0.0172920849999447,5.2,4.12016784699999));
#332715=CARTESIAN_POINT('Ctrl Pts',(0.0172920849999447,2.2,4.12016784699999));
#332716=CARTESIAN_POINT('Ctrl Pts',(0.0169885679999437,12.2,4.11898922899999));
#332717=CARTESIAN_POINT('Ctrl Pts',(0.0169885679999437,5.2,4.11898922899999));
#332718=CARTESIAN_POINT('Ctrl Pts',(0.0169885679999437,2.2,4.11898922899999));
#332719=CARTESIAN_POINT('Ctrl Pts',(0.0166877469999438,12.2,4.11781522499999));
#332720=CARTESIAN_POINT('Ctrl Pts',(0.0166877469999438,5.2,4.11781522499999));
#332721=CARTESIAN_POINT('Ctrl Pts',(0.0166877469999438,2.2,4.11781522499999));
#332722=CARTESIAN_POINT('Ctrl Pts',(0.0163896129999441,12.2,4.11664584499999));
#332723=CARTESIAN_POINT('Ctrl Pts',(0.0163896129999441,5.2,4.11664584499999));
#332724=CARTESIAN_POINT('Ctrl Pts',(0.0163896129999441,2.2,4.11664584499999));
#332725=CARTESIAN_POINT('Ctrl Pts',(0.0160941549999449,12.2,4.11548110199998));
#332726=CARTESIAN_POINT('Ctrl Pts',(0.0160941549999449,5.2,4.11548110199998));
#332727=CARTESIAN_POINT('Ctrl Pts',(0.0160941549999449,2.2,4.11548110199998));
#332728=CARTESIAN_POINT('Ctrl Pts',(0.0158013659999445,12.2,4.11432100899999));
#332729=CARTESIAN_POINT('Ctrl Pts',(0.0158013659999445,5.2,4.11432100899999));
#332730=CARTESIAN_POINT('Ctrl Pts',(0.0158013659999445,2.2,4.11432100899999));
#332731=CARTESIAN_POINT('Ctrl Pts',(0.0155112359999432,12.2,4.11316557799999));
#332732=CARTESIAN_POINT('Ctrl Pts',(0.0155112359999432,5.2,4.11316557799999));
#332733=CARTESIAN_POINT('Ctrl Pts',(0.0155112359999432,2.2,4.11316557799999));
#332734=CARTESIAN_POINT('Ctrl Pts',(0.0152237589999449,12.2,4.11201482099998));
#332735=CARTESIAN_POINT('Ctrl Pts',(0.0152237589999449,5.2,4.11201482099998));
#332736=CARTESIAN_POINT('Ctrl Pts',(0.0152237589999449,2.2,4.11201482099998));
#332737=CARTESIAN_POINT('Ctrl Pts',(0.014938920999944,12.2,4.11086874999998));
#332738=CARTESIAN_POINT('Ctrl Pts',(0.014938920999944,5.2,4.11086874999998));
#332739=CARTESIAN_POINT('Ctrl Pts',(0.014938920999944,2.2,4.11086874999998));
#332740=CARTESIAN_POINT('Ctrl Pts',(0.0146567169999445,12.2,4.10972737899999));
#332741=CARTESIAN_POINT('Ctrl Pts',(0.0146567169999445,5.2,4.10972737899999));
#332742=CARTESIAN_POINT('Ctrl Pts',(0.0146567169999445,2.2,4.10972737899999));
#332743=CARTESIAN_POINT('Ctrl Pts',(0.0143771369999435,12.2,4.10859071899999));
#332744=CARTESIAN_POINT('Ctrl Pts',(0.0143771369999435,5.2,4.10859071899999));
#332745=CARTESIAN_POINT('Ctrl Pts',(0.0143771369999435,2.2,4.10859071899999));
#332746=CARTESIAN_POINT('Ctrl Pts',(0.0141001709999444,12.2,4.10745878299998));
#332747=CARTESIAN_POINT('Ctrl Pts',(0.0141001709999444,5.2,4.10745878299998));
#332748=CARTESIAN_POINT('Ctrl Pts',(0.0141001709999444,2.2,4.10745878299998));
#332749=CARTESIAN_POINT('Ctrl Pts',(0.0138258089999432,12.2,4.10633158399998));
#332750=CARTESIAN_POINT('Ctrl Pts',(0.0138258089999432,5.2,4.10633158399998));
#332751=CARTESIAN_POINT('Ctrl Pts',(0.0138258089999432,2.2,4.10633158399998));
#332752=CARTESIAN_POINT('Ctrl Pts',(0.0135540449999449,12.2,4.10520913399999));
#332753=CARTESIAN_POINT('Ctrl Pts',(0.0135540449999449,5.2,4.10520913399999));
#332754=CARTESIAN_POINT('Ctrl Pts',(0.0135540449999449,2.2,4.10520913399999));
#332755=CARTESIAN_POINT('Ctrl Pts',(0.013284865999944,12.2,4.10409144399999));
#332756=CARTESIAN_POINT('Ctrl Pts',(0.013284865999944,5.2,4.10409144399999));
#332757=CARTESIAN_POINT('Ctrl Pts',(0.013284865999944,2.2,4.10409144399999));
#332758=CARTESIAN_POINT('Ctrl Pts',(0.0130182669999446,12.2,4.10297852999999));
#332759=CARTESIAN_POINT('Ctrl Pts',(0.0130182669999446,5.2,4.10297852999999));
#332760=CARTESIAN_POINT('Ctrl Pts',(0.0130182669999446,2.2,4.10297852999999));
#332761=CARTESIAN_POINT('Ctrl Pts',(0.0127542339999442,12.2,4.10187040099999));
#332762=CARTESIAN_POINT('Ctrl Pts',(0.0127542339999442,5.2,4.10187040099999));
#332763=CARTESIAN_POINT('Ctrl Pts',(0.0127542339999442,2.2,4.10187040099999));
#332764=CARTESIAN_POINT('Ctrl Pts',(0.0124927609999437,12.2,4.10076707099999));
#332765=CARTESIAN_POINT('Ctrl Pts',(0.0124927609999437,5.2,4.10076707099999));
#332766=CARTESIAN_POINT('Ctrl Pts',(0.0124927609999437,2.2,4.10076707099999));
#332767=CARTESIAN_POINT('Ctrl Pts',(0.0122338369999431,12.2,4.09966855299999));
#332768=CARTESIAN_POINT('Ctrl Pts',(0.0122338369999431,5.2,4.09966855299999));
#332769=CARTESIAN_POINT('Ctrl Pts',(0.0122338369999431,2.2,4.09966855299999));
#332770=CARTESIAN_POINT('Ctrl Pts',(0.0119774549999441,12.2,4.09857485999999));
#332771=CARTESIAN_POINT('Ctrl Pts',(0.0119774549999441,5.2,4.09857485999999));
#332772=CARTESIAN_POINT('Ctrl Pts',(0.0119774549999441,2.2,4.09857485999999));
#332773=CARTESIAN_POINT('Ctrl Pts',(0.0117236019999434,12.2,4.09748600299999));
#332774=CARTESIAN_POINT('Ctrl Pts',(0.0117236019999434,5.2,4.09748600299999));
#332775=CARTESIAN_POINT('Ctrl Pts',(0.0117236019999434,2.2,4.09748600299999));
#332776=CARTESIAN_POINT('Ctrl Pts',(0.0114722699999437,12.2,4.09640199399998));
#332777=CARTESIAN_POINT('Ctrl Pts',(0.0114722699999437,5.2,4.09640199399998));
#332778=CARTESIAN_POINT('Ctrl Pts',(0.0114722699999437,2.2,4.09640199399998));
#332779=CARTESIAN_POINT('Ctrl Pts',(0.0112234509999443,12.2,4.09532284999998));
#332780=CARTESIAN_POINT('Ctrl Pts',(0.0112234509999443,5.2,4.09532284999998));
#332781=CARTESIAN_POINT('Ctrl Pts',(0.0112234509999443,2.2,4.09532284999998));
#332782=CARTESIAN_POINT('Ctrl Pts',(0.0109771329999442,12.2,4.09424857899998));
#332783=CARTESIAN_POINT('Ctrl Pts',(0.0109771329999442,5.2,4.09424857899998));
#332784=CARTESIAN_POINT('Ctrl Pts',(0.0109771329999442,2.2,4.09424857899998));
#332785=CARTESIAN_POINT('Ctrl Pts',(0.0107333079999439,12.2,4.09317919499999));
#332786=CARTESIAN_POINT('Ctrl Pts',(0.0107333079999439,5.2,4.09317919499999));
#332787=CARTESIAN_POINT('Ctrl Pts',(0.0107333079999439,2.2,4.09317919499999));
#332788=CARTESIAN_POINT('Ctrl Pts',(0.0104919659999436,12.2,4.09211471199999));
#332789=CARTESIAN_POINT('Ctrl Pts',(0.0104919659999436,5.2,4.09211471199999));
#332790=CARTESIAN_POINT('Ctrl Pts',(0.0104919659999436,2.2,4.09211471199999));
#332791=CARTESIAN_POINT('Ctrl Pts',(0.0102530959999447,12.2,4.09105514199998));
#332792=CARTESIAN_POINT('Ctrl Pts',(0.0102530959999447,5.2,4.09105514199998));
#332793=CARTESIAN_POINT('Ctrl Pts',(0.0102530959999447,2.2,4.09105514199998));
#332794=CARTESIAN_POINT('Ctrl Pts',(0.0100166899999443,12.2,4.09000049599998));
#332795=CARTESIAN_POINT('Ctrl Pts',(0.0100166899999443,5.2,4.09000049599998));
#332796=CARTESIAN_POINT('Ctrl Pts',(0.0100166899999443,2.2,4.09000049599998));
#332797=CARTESIAN_POINT('Ctrl Pts',(0.00978273799994377,12.2,4.08895078999999));
#332798=CARTESIAN_POINT('Ctrl Pts',(0.00978273799994377,5.2,4.08895078999999));
#332799=CARTESIAN_POINT('Ctrl Pts',(0.00978273799994377,2.2,4.08895078999999));
#332800=CARTESIAN_POINT('Ctrl Pts',(0.0095512299999445,12.2,4.08790603499998));
#332801=CARTESIAN_POINT('Ctrl Pts',(0.0095512299999445,5.2,4.08790603499998));
#332802=CARTESIAN_POINT('Ctrl Pts',(0.0095512299999445,2.2,4.08790603499998));
#332803=CARTESIAN_POINT('Ctrl Pts',(0.00932215499994448,12.2,4.08686624199999));
#332804=CARTESIAN_POINT('Ctrl Pts',(0.00932215499994448,5.2,4.08686624199999));
#332805=CARTESIAN_POINT('Ctrl Pts',(0.00932215499994448,2.2,4.08686624199999));
#332806=CARTESIAN_POINT('Ctrl Pts',(0.00909550499994415,12.2,4.08583142799999));
#332807=CARTESIAN_POINT('Ctrl Pts',(0.00909550499994415,5.2,4.08583142799999));
#332808=CARTESIAN_POINT('Ctrl Pts',(0.00909550499994415,2.2,4.08583142799999));
#332809=CARTESIAN_POINT('Ctrl Pts',(0.00887126799994364,12.2,4.08480160199999));
#332810=CARTESIAN_POINT('Ctrl Pts',(0.00887126799994364,5.2,4.08480160199999));
#332811=CARTESIAN_POINT('Ctrl Pts',(0.00887126799994364,2.2,4.08480160199999));
#332812=CARTESIAN_POINT('Ctrl Pts',(0.00864943599994449,12.2,4.08377677799999));
#332813=CARTESIAN_POINT('Ctrl Pts',(0.00864943599994449,5.2,4.08377677799999));
#332814=CARTESIAN_POINT('Ctrl Pts',(0.00864943599994449,2.2,4.08377677799999));
#332815=CARTESIAN_POINT('Ctrl Pts',(0.00842999799994359,12.2,4.08275697099998));
#332816=CARTESIAN_POINT('Ctrl Pts',(0.00842999799994359,5.2,4.08275697099998));
#332817=CARTESIAN_POINT('Ctrl Pts',(0.00842999799994359,2.2,4.08275697099998));
#332818=CARTESIAN_POINT('Ctrl Pts',(0.00821294299994334,12.2,4.08174219099998));
#332819=CARTESIAN_POINT('Ctrl Pts',(0.00821294299994334,5.2,4.08174219099998));
#332820=CARTESIAN_POINT('Ctrl Pts',(0.00821294299994334,2.2,4.08174219099998));
#332821=CARTESIAN_POINT('Ctrl Pts',(0.00799826299994421,12.2,4.08073245199999));
#332822=CARTESIAN_POINT('Ctrl Pts',(0.00799826299994421,5.2,4.08073245199999));
#332823=CARTESIAN_POINT('Ctrl Pts',(0.00799826299994421,2.2,4.08073245199999));
#332824=CARTESIAN_POINT('Ctrl Pts',(0.00778594599994408,12.2,4.07972776699999));
#332825=CARTESIAN_POINT('Ctrl Pts',(0.00778594599994408,5.2,4.07972776699999));
#332826=CARTESIAN_POINT('Ctrl Pts',(0.00778594599994408,2.2,4.07972776699999));
#332827=CARTESIAN_POINT('Ctrl Pts',(0.0075759849999446,12.2,4.07872814899999));
#332828=CARTESIAN_POINT('Ctrl Pts',(0.0075759849999446,5.2,4.07872814899999));
#332829=CARTESIAN_POINT('Ctrl Pts',(0.0075759849999446,2.2,4.07872814899999));
#332830=CARTESIAN_POINT('Ctrl Pts',(0.00736836499994452,12.2,4.07773361099999));
#332831=CARTESIAN_POINT('Ctrl Pts',(0.00736836499994452,5.2,4.07773361099999));
#332832=CARTESIAN_POINT('Ctrl Pts',(0.00736836499994452,2.2,4.07773361099999));
#332833=CARTESIAN_POINT('Ctrl Pts',(0.00716307899994439,12.2,4.07674416499999));
#332834=CARTESIAN_POINT('Ctrl Pts',(0.00716307899994439,5.2,4.07674416499999));
#332835=CARTESIAN_POINT('Ctrl Pts',(0.00716307899994439,2.2,4.07674416499999));
#332836=CARTESIAN_POINT('Ctrl Pts',(0.00696011599994328,12.2,4.07575982599998));
#332837=CARTESIAN_POINT('Ctrl Pts',(0.00696011599994328,5.2,4.07575982599998));
#332838=CARTESIAN_POINT('Ctrl Pts',(0.00696011599994328,2.2,4.07575982599998));
#332839=CARTESIAN_POINT('Ctrl Pts',(0.00675946399994353,12.2,4.07478060399999));
#332840=CARTESIAN_POINT('Ctrl Pts',(0.00675946399994353,5.2,4.07478060399999));
#332841=CARTESIAN_POINT('Ctrl Pts',(0.00675946399994353,2.2,4.07478060399999));
#332842=CARTESIAN_POINT('Ctrl Pts',(0.00656111499994338,12.2,4.07380651499999));
#332843=CARTESIAN_POINT('Ctrl Pts',(0.00656111499994338,5.2,4.07380651499999));
#332844=CARTESIAN_POINT('Ctrl Pts',(0.00656111499994338,2.2,4.07380651499999));
#332845=CARTESIAN_POINT('Ctrl Pts',(0.00636505799994302,12.2,4.07283757099999));
#332846=CARTESIAN_POINT('Ctrl Pts',(0.00636505799994302,5.2,4.07283757099999));
#332847=CARTESIAN_POINT('Ctrl Pts',(0.00636505799994302,2.2,4.07283757099999));
#332848=CARTESIAN_POINT('Ctrl Pts',(0.00617128199994376,12.2,4.07187378599998));
#332849=CARTESIAN_POINT('Ctrl Pts',(0.00617128199994376,5.2,4.07187378599998));
#332850=CARTESIAN_POINT('Ctrl Pts',(0.00617128199994376,2.2,4.07187378599998));
#332851=CARTESIAN_POINT('Ctrl Pts',(0.00597977699994367,12.2,4.07091516999999));
#332852=CARTESIAN_POINT('Ctrl Pts',(0.00597977699994367,5.2,4.07091516999999));
#332853=CARTESIAN_POINT('Ctrl Pts',(0.00597977699994367,2.2,4.07091516999999));
#332854=CARTESIAN_POINT('Ctrl Pts',(0.00579053099994397,12.2,4.06996173999998));
#332855=CARTESIAN_POINT('Ctrl Pts',(0.00579053099994397,5.2,4.06996173999998));
#332856=CARTESIAN_POINT('Ctrl Pts',(0.00579053099994397,2.2,4.06996173999998));
#332857=CARTESIAN_POINT('Ctrl Pts',(0.00560353499994392,12.2,4.06901350599998));
#332858=CARTESIAN_POINT('Ctrl Pts',(0.00560353499994392,5.2,4.06901350599998));
#332859=CARTESIAN_POINT('Ctrl Pts',(0.00560353499994392,2.2,4.06901350599998));
#332860=CARTESIAN_POINT('Ctrl Pts',(0.00541877899994491,12.2,4.06807048299999));
#332861=CARTESIAN_POINT('Ctrl Pts',(0.00541877899994491,5.2,4.06807048299999));
#332862=CARTESIAN_POINT('Ctrl Pts',(0.00541877899994491,2.2,4.06807048299999));
#332863=CARTESIAN_POINT('Ctrl Pts',(0.00523624899994467,12.2,4.06713268299999));
#332864=CARTESIAN_POINT('Ctrl Pts',(0.00523624899994467,5.2,4.06713268299999));
#332865=CARTESIAN_POINT('Ctrl Pts',(0.00523624899994467,2.2,4.06713268299999));
#332866=CARTESIAN_POINT('Ctrl Pts',(0.00505593799994374,12.2,4.06620012199999));
#332867=CARTESIAN_POINT('Ctrl Pts',(0.00505593799994374,5.2,4.06620012199999));
#332868=CARTESIAN_POINT('Ctrl Pts',(0.00505593799994374,2.2,4.06620012199999));
#332869=CARTESIAN_POINT('Ctrl Pts',(0.00487783199994317,12.2,4.06527280899999));
#332870=CARTESIAN_POINT('Ctrl Pts',(0.00487783199994317,5.2,4.06527280899999));
#332871=CARTESIAN_POINT('Ctrl Pts',(0.00487783199994317,2.2,4.06527280899999));
#332872=CARTESIAN_POINT('Ctrl Pts',(0.00470192299994453,12.2,4.06435075999998));
#332873=CARTESIAN_POINT('Ctrl Pts',(0.00470192299994453,5.2,4.06435075999998));
#332874=CARTESIAN_POINT('Ctrl Pts',(0.00470192299994453,2.2,4.06435075999998));
#332875=CARTESIAN_POINT('Ctrl Pts',(0.0045281989999446,12.2,4.06343398799999));
#332876=CARTESIAN_POINT('Ctrl Pts',(0.0045281989999446,5.2,4.06343398799999));
#332877=CARTESIAN_POINT('Ctrl Pts',(0.0045281989999446,2.2,4.06343398799999));
#332878=CARTESIAN_POINT('Ctrl Pts',(0.0043566479999435,12.2,4.06252250499998));
#332879=CARTESIAN_POINT('Ctrl Pts',(0.0043566479999435,5.2,4.06252250499998));
#332880=CARTESIAN_POINT('Ctrl Pts',(0.0043566479999435,2.2,4.06252250499998));
#332881=CARTESIAN_POINT('Ctrl Pts',(0.00418725999994373,12.2,4.06161632599999));
#332882=CARTESIAN_POINT('Ctrl Pts',(0.00418725999994373,5.2,4.06161632599999));
#332883=CARTESIAN_POINT('Ctrl Pts',(0.00418725999994373,2.2,4.06161632599999));
#332884=CARTESIAN_POINT('Ctrl Pts',(0.00402002399994438,12.2,4.06071546299999));
#332885=CARTESIAN_POINT('Ctrl Pts',(0.00402002399994438,5.2,4.06071546299999));
#332886=CARTESIAN_POINT('Ctrl Pts',(0.00402002399994438,2.2,4.06071546299999));
#332887=CARTESIAN_POINT('Ctrl Pts',(0.00385492899994454,12.2,4.05981992999998));
#332888=CARTESIAN_POINT('Ctrl Pts',(0.00385492899994454,5.2,4.05981992999998));
#332889=CARTESIAN_POINT('Ctrl Pts',(0.00385492899994454,2.2,4.05981992999998));
#332890=CARTESIAN_POINT('Ctrl Pts',(0.00369196399994442,12.2,4.05892973999999));
#332891=CARTESIAN_POINT('Ctrl Pts',(0.00369196399994442,5.2,4.05892973999999));
#332892=CARTESIAN_POINT('Ctrl Pts',(0.00369196399994442,2.2,4.05892973999999));
#332893=CARTESIAN_POINT('Ctrl Pts',(0.00353111799994531,12.2,4.05804490699998));
#332894=CARTESIAN_POINT('Ctrl Pts',(0.00353111799994531,5.2,4.05804490699998));
#332895=CARTESIAN_POINT('Ctrl Pts',(0.00353111799994531,2.2,4.05804490699998));
#332896=CARTESIAN_POINT('Ctrl Pts',(0.00337237899994291,12.2,4.05716544299998));
#332897=CARTESIAN_POINT('Ctrl Pts',(0.00337237899994291,5.2,4.05716544299998));
#332898=CARTESIAN_POINT('Ctrl Pts',(0.00337237899994291,2.2,4.05716544299998));
#332899=CARTESIAN_POINT('Ctrl Pts',(0.00321573599994517,12.2,4.05629136299999));
#332900=CARTESIAN_POINT('Ctrl Pts',(0.00321573599994517,5.2,4.05629136299999));
#332901=CARTESIAN_POINT('Ctrl Pts',(0.00321573599994517,2.2,4.05629136299999));
#332902=CARTESIAN_POINT('Ctrl Pts',(0.00306117799994453,12.2,4.05542268099998));
#332903=CARTESIAN_POINT('Ctrl Pts',(0.00306117799994453,5.2,4.05542268099998));
#332904=CARTESIAN_POINT('Ctrl Pts',(0.00306117799994453,2.2,4.05542268099998));
#332905=CARTESIAN_POINT('Ctrl Pts',(0.00290869399994341,12.2,4.05455940799998));
#332906=CARTESIAN_POINT('Ctrl Pts',(0.00290869399994341,5.2,4.05455940799998));
#332907=CARTESIAN_POINT('Ctrl Pts',(0.00290869399994341,2.2,4.05455940799998));
#332908=CARTESIAN_POINT('Ctrl Pts',(0.00275827199994415,12.2,4.05370155899998));
#332909=CARTESIAN_POINT('Ctrl Pts',(0.00275827199994415,5.2,4.05370155899998));
#332910=CARTESIAN_POINT('Ctrl Pts',(0.00275827199994415,2.2,4.05370155899998));
#332911=CARTESIAN_POINT('Ctrl Pts',(0.00260990099994473,12.2,4.05284914799999));
#332912=CARTESIAN_POINT('Ctrl Pts',(0.00260990099994473,5.2,4.05284914799999));
#332913=CARTESIAN_POINT('Ctrl Pts',(0.00260990099994473,2.2,4.05284914799999));
#332914=CARTESIAN_POINT('Ctrl Pts',(0.00246356899994526,12.2,4.05200218699999));
#332915=CARTESIAN_POINT('Ctrl Pts',(0.00246356899994526,5.2,4.05200218699999));
#332916=CARTESIAN_POINT('Ctrl Pts',(0.00246356899994526,2.2,4.05200218699999));
#332917=CARTESIAN_POINT('Ctrl Pts',(0.00231926399994364,12.2,4.05116069199998));
#332918=CARTESIAN_POINT('Ctrl Pts',(0.00231926399994364,5.2,4.05116069199998));
#332919=CARTESIAN_POINT('Ctrl Pts',(0.00231926399994364,2.2,4.05116069199998));
#332920=CARTESIAN_POINT('Ctrl Pts',(0.00217697599994459,12.2,4.05032467299999));
#332921=CARTESIAN_POINT('Ctrl Pts',(0.00217697599994459,5.2,4.05032467299999));
#332922=CARTESIAN_POINT('Ctrl Pts',(0.00217697599994459,2.2,4.05032467299999));
#332923=CARTESIAN_POINT('Ctrl Pts',(0.00203669299994379,12.2,4.04949414699999));
#332924=CARTESIAN_POINT('Ctrl Pts',(0.00203669299994379,5.2,4.04949414699999));
#332925=CARTESIAN_POINT('Ctrl Pts',(0.00203669299994379,2.2,4.04949414699999));
#332926=CARTESIAN_POINT('Ctrl Pts',(0.0018984019999435,12.2,4.04866912499998));
#332927=CARTESIAN_POINT('Ctrl Pts',(0.0018984019999435,5.2,4.04866912499998));
#332928=CARTESIAN_POINT('Ctrl Pts',(0.0018984019999435,2.2,4.04866912499998));
#332929=CARTESIAN_POINT('Ctrl Pts',(0.00176209299994289,12.2,4.04784962399999));
#332930=CARTESIAN_POINT('Ctrl Pts',(0.00176209299994289,5.2,4.04784962399999));
#332931=CARTESIAN_POINT('Ctrl Pts',(0.00176209299994289,2.2,4.04784962399999));
#332932=CARTESIAN_POINT('Ctrl Pts',(0.00162775199994413,12.2,4.04703565399998));
#332933=CARTESIAN_POINT('Ctrl Pts',(0.00162775199994413,5.2,4.04703565399998));
#332934=CARTESIAN_POINT('Ctrl Pts',(0.00162775199994413,2.2,4.04703565399998));
#332935=CARTESIAN_POINT('Ctrl Pts',(0.00149536999994425,12.2,4.04622722999999));
#332936=CARTESIAN_POINT('Ctrl Pts',(0.00149536999994425,5.2,4.04622722999999));
#332937=CARTESIAN_POINT('Ctrl Pts',(0.00149536999994425,2.2,4.04622722999999));
#332938=CARTESIAN_POINT('Ctrl Pts',(0.00136493299994433,12.2,4.04542436699998));
#332939=CARTESIAN_POINT('Ctrl Pts',(0.00136493299994433,5.2,4.04542436699998));
#332940=CARTESIAN_POINT('Ctrl Pts',(0.00136493299994433,2.2,4.04542436699998));
#332941=CARTESIAN_POINT('Ctrl Pts',(0.00123642999994344,12.2,4.04462707699999));
#332942=CARTESIAN_POINT('Ctrl Pts',(0.00123642999994344,5.2,4.04462707699999));
#332943=CARTESIAN_POINT('Ctrl Pts',(0.00123642999994344,2.2,4.04462707699999));
#332944=CARTESIAN_POINT('Ctrl Pts',(0.00110984899994392,12.2,4.04383537399998));
#332945=CARTESIAN_POINT('Ctrl Pts',(0.00110984899994392,5.2,4.04383537399998));
#332946=CARTESIAN_POINT('Ctrl Pts',(0.00110984899994392,2.2,4.04383537399998));
#332947=CARTESIAN_POINT('Ctrl Pts',(0.000985176999943596,12.2,4.04304927399998));
#332948=CARTESIAN_POINT('Ctrl Pts',(0.000985176999943596,5.2,4.04304927399998));
#332949=CARTESIAN_POINT('Ctrl Pts',(0.000985176999943596,2.2,4.04304927399998));
#332950=CARTESIAN_POINT('Ctrl Pts',(0.000862403999944963,12.2,4.04226878799999));
#332951=CARTESIAN_POINT('Ctrl Pts',(0.000862403999944963,5.2,4.04226878799999));
#332952=CARTESIAN_POINT('Ctrl Pts',(0.000862403999944963,2.2,4.04226878799999));
#332953=CARTESIAN_POINT('Ctrl Pts',(0.000741515999944644,12.2,4.04149393099999));
#332954=CARTESIAN_POINT('Ctrl Pts',(0.000741515999944644,5.2,4.04149393099999));
#332955=CARTESIAN_POINT('Ctrl Pts',(0.000741515999944644,2.2,4.04149393099999));
#332956=CARTESIAN_POINT('Ctrl Pts',(0.00062250199994395,12.2,4.04072471599999));
#332957=CARTESIAN_POINT('Ctrl Pts',(0.00062250199994395,5.2,4.04072471599999));
#332958=CARTESIAN_POINT('Ctrl Pts',(0.00062250199994395,2.2,4.04072471599999));
#332959=CARTESIAN_POINT('Ctrl Pts',(0.000505348999944024,12.2,4.03996115799998));
#332960=CARTESIAN_POINT('Ctrl Pts',(0.000505348999944024,5.2,4.03996115799998));
#332961=CARTESIAN_POINT('Ctrl Pts',(0.000505348999944024,2.2,4.03996115799998));
#332962=CARTESIAN_POINT('Ctrl Pts',(0.000390043999944903,12.2,4.03920327199998));
#332963=CARTESIAN_POINT('Ctrl Pts',(0.000390043999944903,5.2,4.03920327199998));
#332964=CARTESIAN_POINT('Ctrl Pts',(0.000390043999944903,2.2,4.03920327199998));
#332965=CARTESIAN_POINT('Ctrl Pts',(0.000276576999944647,12.2,4.03845106799999));
#332966=CARTESIAN_POINT('Ctrl Pts',(0.000276576999944647,5.2,4.03845106799999));
#332967=CARTESIAN_POINT('Ctrl Pts',(0.000276576999944647,2.2,4.03845106799999));
#332968=CARTESIAN_POINT('Ctrl Pts',(0.000164934999944402,12.2,4.03770456499998));
#332969=CARTESIAN_POINT('Ctrl Pts',(0.000164934999944402,5.2,4.03770456499998));
#332970=CARTESIAN_POINT('Ctrl Pts',(0.000164934999944402,2.2,4.03770456499998));
#332971=CARTESIAN_POINT('Ctrl Pts',(5.51029999440369E-5,12.2,4.03696377299998));
#332972=CARTESIAN_POINT('Ctrl Pts',(5.51029999440369E-5,5.2,4.03696377299998));
#332973=CARTESIAN_POINT('Ctrl Pts',(5.51029999440369E-5,2.2,4.03696377299998));
#332974=CARTESIAN_POINT('Ctrl Pts',(-5.29290000550551E-5,12.2,4.03622870699999));
#332975=CARTESIAN_POINT('Ctrl Pts',(-5.29290000550551E-5,5.2,4.03622870699999));
#332976=CARTESIAN_POINT('Ctrl Pts',(-5.29290000550551E-5,2.2,4.03622870699999));
#332977=CARTESIAN_POINT('Ctrl Pts',(-0.000159173000054977,12.2,4.03549938199999));
#332978=CARTESIAN_POINT('Ctrl Pts',(-0.000159173000054977,5.2,4.03549938199999));
#332979=CARTESIAN_POINT('Ctrl Pts',(-0.000159173000054977,2.2,4.03549938199999));
#332980=CARTESIAN_POINT('Ctrl Pts',(-0.00026364400005475,12.2,4.03477581099998));
#332981=CARTESIAN_POINT('Ctrl Pts',(-0.00026364400005475,5.2,4.03477581099998));
#332982=CARTESIAN_POINT('Ctrl Pts',(-0.00026364400005475,2.2,4.03477581099998));
#332983=CARTESIAN_POINT('Ctrl Pts',(-0.000366352000055201,12.2,4.03405800899999));
#332984=CARTESIAN_POINT('Ctrl Pts',(-0.000366352000055201,5.2,4.03405800899999));
#332985=CARTESIAN_POINT('Ctrl Pts',(-0.000366352000055201,2.2,4.03405800899999));
#332986=CARTESIAN_POINT('Ctrl Pts',(-0.000467312000056461,12.2,4.03334598799999));
#332987=CARTESIAN_POINT('Ctrl Pts',(-0.000467312000056461,5.2,4.03334598799999));
#332988=CARTESIAN_POINT('Ctrl Pts',(-0.000467312000056461,2.2,4.03334598799999));
#332989=CARTESIAN_POINT('Ctrl Pts',(-0.000566536000056192,12.2,4.03263976499999));
#332990=CARTESIAN_POINT('Ctrl Pts',(-0.000566536000056192,5.2,4.03263976499999));
#332991=CARTESIAN_POINT('Ctrl Pts',(-0.000566536000056192,2.2,4.03263976499999));
#332992=CARTESIAN_POINT('Ctrl Pts',(-0.000664036000056498,12.2,4.03193935299999));
#332993=CARTESIAN_POINT('Ctrl Pts',(-0.000664036000056498,5.2,4.03193935299999));
#332994=CARTESIAN_POINT('Ctrl Pts',(-0.000664036000056498,2.2,4.03193935299999));
#332995=CARTESIAN_POINT('Ctrl Pts',(-0.000759825000056233,12.2,4.03124476599999));
#332996=CARTESIAN_POINT('Ctrl Pts',(-0.000759825000056233,5.2,4.03124476599999));
#332997=CARTESIAN_POINT('Ctrl Pts',(-0.000759825000056233,2.2,4.03124476599999));
#332998=CARTESIAN_POINT('Ctrl Pts',(-0.000853916000055363,12.2,4.03055601799998));
#332999=CARTESIAN_POINT('Ctrl Pts',(-0.000853916000055363,5.2,4.03055601799998));
#333000=CARTESIAN_POINT('Ctrl Pts',(-0.000853916000055363,2.2,4.03055601799998));
#333001=CARTESIAN_POINT('Ctrl Pts',(-0.00094632400005624,12.2,4.02987312299998));
#333002=CARTESIAN_POINT('Ctrl Pts',(-0.00094632400005624,5.2,4.02987312299998));
#333003=CARTESIAN_POINT('Ctrl Pts',(-0.00094632400005624,2.2,4.02987312299998));
#333004=CARTESIAN_POINT('Ctrl Pts',(-0.00103705900005636,12.2,4.02919609599999));
#333005=CARTESIAN_POINT('Ctrl Pts',(-0.00103705900005636,5.2,4.02919609599999));
#333006=CARTESIAN_POINT('Ctrl Pts',(-0.00103705900005636,2.2,4.02919609599999));
#333007=CARTESIAN_POINT('Ctrl Pts',(-0.0011261340000568,12.2,4.02852495099999));
#333008=CARTESIAN_POINT('Ctrl Pts',(-0.0011261340000568,5.2,4.02852495099999));
#333009=CARTESIAN_POINT('Ctrl Pts',(-0.0011261340000568,2.2,4.02852495099999));
#333010=CARTESIAN_POINT('Ctrl Pts',(-0.00121356600005563,12.2,4.02785970199999));
#333011=CARTESIAN_POINT('Ctrl Pts',(-0.00121356600005563,5.2,4.02785970199999));
#333012=CARTESIAN_POINT('Ctrl Pts',(-0.00121356600005563,2.2,4.02785970199999));
#333013=CARTESIAN_POINT('Ctrl Pts',(-0.00129936400005582,12.2,4.02720036299999));
#333014=CARTESIAN_POINT('Ctrl Pts',(-0.00129936400005582,5.2,4.02720036299999));
#333015=CARTESIAN_POINT('Ctrl Pts',(-0.00129936400005582,2.2,4.02720036299999));
#333016=CARTESIAN_POINT('Ctrl Pts',(-0.0013835430000564,12.2,4.02654694999999));
#333017=CARTESIAN_POINT('Ctrl Pts',(-0.0013835430000564,5.2,4.02654694999999));
#333018=CARTESIAN_POINT('Ctrl Pts',(-0.0013835430000564,2.2,4.02654694999999));
#333019=CARTESIAN_POINT('Ctrl Pts',(-0.0014661160000562,12.2,4.02589947499998));
#333020=CARTESIAN_POINT('Ctrl Pts',(-0.0014661160000562,5.2,4.02589947499998));
#333021=CARTESIAN_POINT('Ctrl Pts',(-0.0014661160000562,2.2,4.02589947499998));
#333022=CARTESIAN_POINT('Ctrl Pts',(-0.00154709700005641,12.2,4.02525795499999));
#333023=CARTESIAN_POINT('Ctrl Pts',(-0.00154709700005641,5.2,4.02525795499999));
#333024=CARTESIAN_POINT('Ctrl Pts',(-0.00154709700005641,2.2,4.02525795499999));
#333025=CARTESIAN_POINT('Ctrl Pts',(-0.00162649800005466,12.2,4.02462240299998));
#333026=CARTESIAN_POINT('Ctrl Pts',(-0.00162649800005466,5.2,4.02462240299998));
#333027=CARTESIAN_POINT('Ctrl Pts',(-0.00162649800005466,2.2,4.02462240299998));
#333028=CARTESIAN_POINT('Ctrl Pts',(-0.00170433400005555,12.2,4.02399283199999));
#333029=CARTESIAN_POINT('Ctrl Pts',(-0.00170433400005555,5.2,4.02399283199999));
#333030=CARTESIAN_POINT('Ctrl Pts',(-0.00170433400005555,2.2,4.02399283199999));
#333031=CARTESIAN_POINT('Ctrl Pts',(-0.00178061700005673,12.2,4.02336925899998));
#333032=CARTESIAN_POINT('Ctrl Pts',(-0.00178061700005673,5.2,4.02336925899998));
#333033=CARTESIAN_POINT('Ctrl Pts',(-0.00178061700005673,2.2,4.02336925899998));
#333034=CARTESIAN_POINT('Ctrl Pts',(-0.00185536300005507,12.2,4.02275169799999));
#333035=CARTESIAN_POINT('Ctrl Pts',(-0.00185536300005507,5.2,4.02275169799999));
#333036=CARTESIAN_POINT('Ctrl Pts',(-0.00185536300005507,2.2,4.02275169799999));
#333037=CARTESIAN_POINT('Ctrl Pts',(-0.00192858300005595,12.2,4.02214016199999));
#333038=CARTESIAN_POINT('Ctrl Pts',(-0.00192858300005595,5.2,4.02214016199999));
#333039=CARTESIAN_POINT('Ctrl Pts',(-0.00192858300005595,2.2,4.02214016199999));
#333040=CARTESIAN_POINT('Ctrl Pts',(-0.00200029100005606,12.2,4.02153466699998));
#333041=CARTESIAN_POINT('Ctrl Pts',(-0.00200029100005606,5.2,4.02153466699998));
#333042=CARTESIAN_POINT('Ctrl Pts',(-0.00200029100005606,2.2,4.02153466699998));
#333043=CARTESIAN_POINT('Ctrl Pts',(-0.00207050200005555,12.2,4.02093522699998));
#333044=CARTESIAN_POINT('Ctrl Pts',(-0.00207050200005555,5.2,4.02093522699998));
#333045=CARTESIAN_POINT('Ctrl Pts',(-0.00207050200005555,2.2,4.02093522699998));
#333046=CARTESIAN_POINT('Ctrl Pts',(-0.00213922900005548,12.2,4.02034185699998));
#333047=CARTESIAN_POINT('Ctrl Pts',(-0.00213922900005548,5.2,4.02034185699998));
#333048=CARTESIAN_POINT('Ctrl Pts',(-0.00213922900005548,2.2,4.02034185699998));
#333049=CARTESIAN_POINT('Ctrl Pts',(-0.00220648600005481,12.2,4.01975457099999));
#333050=CARTESIAN_POINT('Ctrl Pts',(-0.00220648600005481,5.2,4.01975457099999));
#333051=CARTESIAN_POINT('Ctrl Pts',(-0.00220648600005481,2.2,4.01975457099999));
#333052=CARTESIAN_POINT('Ctrl Pts',(-0.00227228800005475,12.2,4.01917338499998));
#333053=CARTESIAN_POINT('Ctrl Pts',(-0.00227228800005475,5.2,4.01917338499998));
#333054=CARTESIAN_POINT('Ctrl Pts',(-0.00227228800005475,2.2,4.01917338499998));
#333055=CARTESIAN_POINT('Ctrl Pts',(-0.00233664700005632,12.2,4.01859831199998));
#333056=CARTESIAN_POINT('Ctrl Pts',(-0.00233664700005632,5.2,4.01859831199998));
#333057=CARTESIAN_POINT('Ctrl Pts',(-0.00233664700005632,2.2,4.01859831199998));
#333058=CARTESIAN_POINT('Ctrl Pts',(-0.0023995780000552,12.2,4.01802936699998));
#333059=CARTESIAN_POINT('Ctrl Pts',(-0.0023995780000552,5.2,4.01802936699998));
#333060=CARTESIAN_POINT('Ctrl Pts',(-0.0023995780000552,2.2,4.01802936699998));
#333061=CARTESIAN_POINT('Ctrl Pts',(-0.00246109500005588,12.2,4.01746656599999));
#333062=CARTESIAN_POINT('Ctrl Pts',(-0.00246109500005588,5.2,4.01746656599999));
#333063=CARTESIAN_POINT('Ctrl Pts',(-0.00246109500005588,2.2,4.01746656599999));
#333064=CARTESIAN_POINT('Ctrl Pts',(-0.00252121300005626,12.2,4.01690992299999));
#333065=CARTESIAN_POINT('Ctrl Pts',(-0.00252121300005626,5.2,4.01690992299999));
#333066=CARTESIAN_POINT('Ctrl Pts',(-0.00252121300005626,2.2,4.01690992299999));
#333067=CARTESIAN_POINT('Ctrl Pts',(-0.00257994500005521,12.2,4.01635945199998));
#333068=CARTESIAN_POINT('Ctrl Pts',(-0.00257994500005521,5.2,4.01635945199998));
#333069=CARTESIAN_POINT('Ctrl Pts',(-0.00257994500005521,2.2,4.01635945199998));
#333070=CARTESIAN_POINT('Ctrl Pts',(-0.00263730600005508,12.2,4.01581516899999));
#333071=CARTESIAN_POINT('Ctrl Pts',(-0.00263730600005508,5.2,4.01581516899999));
#333072=CARTESIAN_POINT('Ctrl Pts',(-0.00263730600005508,2.2,4.01581516899999));
#333073=CARTESIAN_POINT('Ctrl Pts',(-0.00269331000005591,12.2,4.01527708799998));
#333074=CARTESIAN_POINT('Ctrl Pts',(-0.00269331000005591,5.2,4.01527708799998));
#333075=CARTESIAN_POINT('Ctrl Pts',(-0.00269331000005591,2.2,4.01527708799998));
#333076=CARTESIAN_POINT('Ctrl Pts',(-0.00274797200005673,12.2,4.01474522599998));
#333077=CARTESIAN_POINT('Ctrl Pts',(-0.00274797200005673,5.2,4.01474522599998));
#333078=CARTESIAN_POINT('Ctrl Pts',(-0.00274797200005673,2.2,4.01474522599998));
#333079=CARTESIAN_POINT('Ctrl Pts',(-0.00280130500005527,12.2,4.01421959499999));
#333080=CARTESIAN_POINT('Ctrl Pts',(-0.00280130500005527,5.2,4.01421959499999));
#333081=CARTESIAN_POINT('Ctrl Pts',(-0.00280130500005527,2.2,4.01421959499999));
#333082=CARTESIAN_POINT('Ctrl Pts',(-0.00285332500005509,12.2,4.01370021099999));
#333083=CARTESIAN_POINT('Ctrl Pts',(-0.00285332500005509,5.2,4.01370021099999));
#333084=CARTESIAN_POINT('Ctrl Pts',(-0.00285332500005509,2.2,4.01370021099999));
#333085=CARTESIAN_POINT('Ctrl Pts',(-0.00290404600005623,12.2,4.01318708999998));
#333086=CARTESIAN_POINT('Ctrl Pts',(-0.00290404600005623,5.2,4.01318708999998));
#333087=CARTESIAN_POINT('Ctrl Pts',(-0.00290404600005623,2.2,4.01318708999998));
#333088=CARTESIAN_POINT('Ctrl Pts',(-0.0029534830000555,12.2,4.01268024599998));
#333089=CARTESIAN_POINT('Ctrl Pts',(-0.0029534830000555,5.2,4.01268024599998));
#333090=CARTESIAN_POINT('Ctrl Pts',(-0.0029534830000555,2.2,4.01268024599998));
#333091=CARTESIAN_POINT('Ctrl Pts',(-0.00300165000005626,12.2,4.01217969399998));
#333092=CARTESIAN_POINT('Ctrl Pts',(-0.00300165000005626,5.2,4.01217969399998));
#333093=CARTESIAN_POINT('Ctrl Pts',(-0.00300165000005626,2.2,4.01217969399998));
#333094=CARTESIAN_POINT('Ctrl Pts',(-0.00304856200005644,12.2,4.01168544899999));
#333095=CARTESIAN_POINT('Ctrl Pts',(-0.00304856200005644,5.2,4.01168544899999));
#333096=CARTESIAN_POINT('Ctrl Pts',(-0.00304856200005644,2.2,4.01168544899999));
#333097=CARTESIAN_POINT('Ctrl Pts',(-0.00309423600005521,12.2,4.01119752799998));
#333098=CARTESIAN_POINT('Ctrl Pts',(-0.00309423600005521,5.2,4.01119752799998));
#333099=CARTESIAN_POINT('Ctrl Pts',(-0.00309423600005521,2.2,4.01119752799998));
#333100=CARTESIAN_POINT('Ctrl Pts',(-0.00313868200005563,12.2,4.01071594299999));
#333101=CARTESIAN_POINT('Ctrl Pts',(-0.00313868200005563,5.2,4.01071594299999));
#333102=CARTESIAN_POINT('Ctrl Pts',(-0.00313868200005563,2.2,4.01071594299999));
#333103=CARTESIAN_POINT('Ctrl Pts',(-0.00318192000005602,12.2,4.01024071099998));
#333104=CARTESIAN_POINT('Ctrl Pts',(-0.00318192000005602,5.2,4.01024071099998));
#333105=CARTESIAN_POINT('Ctrl Pts',(-0.00318192000005602,2.2,4.01024071099998));
#333106=CARTESIAN_POINT('Ctrl Pts',(-0.00322396300005635,12.2,4.00977184799999));
#333107=CARTESIAN_POINT('Ctrl Pts',(-0.00322396300005635,5.2,4.00977184799999));
#333108=CARTESIAN_POINT('Ctrl Pts',(-0.00322396300005635,2.2,4.00977184799999));
#333109=CARTESIAN_POINT('Ctrl Pts',(-0.00326482500005555,12.2,4.00930936699999));
#333110=CARTESIAN_POINT('Ctrl Pts',(-0.00326482500005555,5.2,4.00930936699999));
#333111=CARTESIAN_POINT('Ctrl Pts',(-0.00326482500005555,2.2,4.00930936699999));
#333112=CARTESIAN_POINT('Ctrl Pts',(-0.00330452400005511,12.2,4.00885328399998));
#333113=CARTESIAN_POINT('Ctrl Pts',(-0.00330452400005511,5.2,4.00885328399998));
#333114=CARTESIAN_POINT('Ctrl Pts',(-0.00330452400005511,2.2,4.00885328399998));
#333115=CARTESIAN_POINT('Ctrl Pts',(-0.00334307200005602,12.2,4.00840361499998));
#333116=CARTESIAN_POINT('Ctrl Pts',(-0.00334307200005602,5.2,4.00840361499998));
#333117=CARTESIAN_POINT('Ctrl Pts',(-0.00334307200005602,2.2,4.00840361499998));
#333118=CARTESIAN_POINT('Ctrl Pts',(-0.00338048600005637,12.2,4.00796037499998));
#333119=CARTESIAN_POINT('Ctrl Pts',(-0.00338048600005637,5.2,4.00796037499998));
#333120=CARTESIAN_POINT('Ctrl Pts',(-0.00338048600005637,2.2,4.00796037499998));
#333121=CARTESIAN_POINT('Ctrl Pts',(-0.00341678200005525,12.2,4.00752357899999));
#333122=CARTESIAN_POINT('Ctrl Pts',(-0.00341678200005525,5.2,4.00752357899999));
#333123=CARTESIAN_POINT('Ctrl Pts',(-0.00341678200005525,2.2,4.00752357899999));
#333124=CARTESIAN_POINT('Ctrl Pts',(-0.00345197500005613,12.2,4.00709324299999));
#333125=CARTESIAN_POINT('Ctrl Pts',(-0.00345197500005613,5.2,4.00709324299999));
#333126=CARTESIAN_POINT('Ctrl Pts',(-0.00345197500005613,2.2,4.00709324299999));
#333127=CARTESIAN_POINT('Ctrl Pts',(-0.00348607900005683,12.2,4.00666938199999));
#333128=CARTESIAN_POINT('Ctrl Pts',(-0.00348607900005683,5.2,4.00666938199999));
#333129=CARTESIAN_POINT('Ctrl Pts',(-0.00348607900005683,2.2,4.00666938199999));
#333130=CARTESIAN_POINT('Ctrl Pts',(-0.00351911100005543,12.2,4.00625201199999));
#333131=CARTESIAN_POINT('Ctrl Pts',(-0.00351911100005543,5.2,4.00625201199999));
#333132=CARTESIAN_POINT('Ctrl Pts',(-0.00351911100005543,2.2,4.00625201199999));
#333133=CARTESIAN_POINT('Ctrl Pts',(-0.0035510860000565,12.2,4.00584114699999));
#333134=CARTESIAN_POINT('Ctrl Pts',(-0.0035510860000565,5.2,4.00584114699999));
#333135=CARTESIAN_POINT('Ctrl Pts',(-0.0035510860000565,2.2,4.00584114699999));
#333136=CARTESIAN_POINT('Ctrl Pts',(-0.0035820210000559,12.2,4.00543680299998));
#333137=CARTESIAN_POINT('Ctrl Pts',(-0.0035820210000559,5.2,4.00543680299998));
#333138=CARTESIAN_POINT('Ctrl Pts',(-0.0035820210000559,2.2,4.00543680299998));
#333139=CARTESIAN_POINT('Ctrl Pts',(-0.003611930000057,12.2,4.00503899699999));
#333140=CARTESIAN_POINT('Ctrl Pts',(-0.003611930000057,5.2,4.00503899699999));
#333141=CARTESIAN_POINT('Ctrl Pts',(-0.003611930000057,2.2,4.00503899699999));
#333142=CARTESIAN_POINT('Ctrl Pts',(-0.00364083000005456,12.2,4.00464774299999));
#333143=CARTESIAN_POINT('Ctrl Pts',(-0.00364083000005456,5.2,4.00464774299999));
#333144=CARTESIAN_POINT('Ctrl Pts',(-0.00364083000005456,2.2,4.00464774299999));
#333145=CARTESIAN_POINT('Ctrl Pts',(-0.00366873600005647,12.2,4.00426305799999));
#333146=CARTESIAN_POINT('Ctrl Pts',(-0.00366873600005647,5.2,4.00426305799999));
#333147=CARTESIAN_POINT('Ctrl Pts',(-0.00366873600005647,2.2,4.00426305799999));
#333148=CARTESIAN_POINT('Ctrl Pts',(-0.00369566500005526,12.2,4.00388495599999));
#333149=CARTESIAN_POINT('Ctrl Pts',(-0.00369566500005526,5.2,4.00388495599999));
#333150=CARTESIAN_POINT('Ctrl Pts',(-0.00369566500005526,2.2,4.00388495599999));
#333151=CARTESIAN_POINT('Ctrl Pts',(-0.00372163300005669,12.2,4.00351345299998));
#333152=CARTESIAN_POINT('Ctrl Pts',(-0.00372163300005669,5.2,4.00351345299998));
#333153=CARTESIAN_POINT('Ctrl Pts',(-0.00372163300005669,2.2,4.00351345299998));
#333154=CARTESIAN_POINT('Ctrl Pts',(-0.00374665500005534,12.2,4.00314856599999));
#333155=CARTESIAN_POINT('Ctrl Pts',(-0.00374665500005534,5.2,4.00314856599999));
#333156=CARTESIAN_POINT('Ctrl Pts',(-0.00374665500005534,2.2,4.00314856599999));
#333157=CARTESIAN_POINT('Ctrl Pts',(-0.00377074800005595,12.2,4.00279030999998));
#333158=CARTESIAN_POINT('Ctrl Pts',(-0.00377074800005595,5.2,4.00279030999998));
#333159=CARTESIAN_POINT('Ctrl Pts',(-0.00377074800005595,2.2,4.00279030999998));
#333160=CARTESIAN_POINT('Ctrl Pts',(-0.00379393000005558,12.2,4.00243869999999));
#333161=CARTESIAN_POINT('Ctrl Pts',(-0.00379393000005558,5.2,4.00243869999999));
#333162=CARTESIAN_POINT('Ctrl Pts',(-0.00379393000005558,2.2,4.00243869999999));
#333163=CARTESIAN_POINT('Ctrl Pts',(-0.00381621400005528,12.2,4.00209375199999));
#333164=CARTESIAN_POINT('Ctrl Pts',(-0.00381621400005528,5.2,4.00209375199999));
#333165=CARTESIAN_POINT('Ctrl Pts',(-0.00381621400005528,2.2,4.00209375199999));
#333166=CARTESIAN_POINT('Ctrl Pts',(-0.00383761700005537,12.2,4.00175548199999));
#333167=CARTESIAN_POINT('Ctrl Pts',(-0.00383761700005537,5.2,4.00175548199999));
#333168=CARTESIAN_POINT('Ctrl Pts',(-0.00383761700005537,2.2,4.00175548199999));
#333169=CARTESIAN_POINT('Ctrl Pts',(-0.0038581580000563,12.2,4.00142390699998));
#333170=CARTESIAN_POINT('Ctrl Pts',(-0.0038581580000563,5.2,4.00142390699998));
#333171=CARTESIAN_POINT('Ctrl Pts',(-0.0038581580000563,2.2,4.00142390699998));
#333172=CARTESIAN_POINT('Ctrl Pts',(-0.00387785200005487,12.2,4.00109904099998));
#333173=CARTESIAN_POINT('Ctrl Pts',(-0.00387785200005487,5.2,4.00109904099998));
#333174=CARTESIAN_POINT('Ctrl Pts',(-0.00387785200005487,2.2,4.00109904099998));
#333175=CARTESIAN_POINT('Ctrl Pts',(-0.00389671400005676,12.2,4.00078090299999));
#333176=CARTESIAN_POINT('Ctrl Pts',(-0.00389671400005676,5.2,4.00078090299999));
#333177=CARTESIAN_POINT('Ctrl Pts',(-0.00389671400005676,2.2,4.00078090299999));
#333178=CARTESIAN_POINT('Ctrl Pts',(-0.00391476500005595,12.2,4.00046950499998));
#333179=CARTESIAN_POINT('Ctrl Pts',(-0.00391476500005595,5.2,4.00046950499998));
#333180=CARTESIAN_POINT('Ctrl Pts',(-0.00391476500005595,2.2,4.00046950499998));
#333181=CARTESIAN_POINT('Ctrl Pts',(-0.00393201700005564,12.2,4.00016486499998));
#333182=CARTESIAN_POINT('Ctrl Pts',(-0.00393201700005564,5.2,4.00016486499998));
#333183=CARTESIAN_POINT('Ctrl Pts',(-0.00393201700005564,2.2,4.00016486499998));
#333184=CARTESIAN_POINT('Ctrl Pts',(-0.00394849000005527,12.2,3.99986699899999));
#333185=CARTESIAN_POINT('Ctrl Pts',(-0.00394849000005527,5.2,3.99986699899999));
#333186=CARTESIAN_POINT('Ctrl Pts',(-0.00394849000005527,2.2,3.99986699899999));
#333187=CARTESIAN_POINT('Ctrl Pts',(-0.00396419900005497,12.2,3.99957592299998));
#333188=CARTESIAN_POINT('Ctrl Pts',(-0.00396419900005497,5.2,3.99957592299998));
#333189=CARTESIAN_POINT('Ctrl Pts',(-0.00396419900005497,2.2,3.99957592299998));
#333190=CARTESIAN_POINT('Ctrl Pts',(-0.00397916300005519,12.2,3.99929165399998));
#333191=CARTESIAN_POINT('Ctrl Pts',(-0.00397916300005519,5.2,3.99929165399998));
#333192=CARTESIAN_POINT('Ctrl Pts',(-0.00397916300005519,2.2,3.99929165399998));
#333193=CARTESIAN_POINT('Ctrl Pts',(-0.00399339700005497,12.2,3.99901420599999));
#333194=CARTESIAN_POINT('Ctrl Pts',(-0.00399339700005497,5.2,3.99901420599999));
#333195=CARTESIAN_POINT('Ctrl Pts',(-0.00399339700005497,2.2,3.99901420599999));
#333196=CARTESIAN_POINT('Ctrl Pts',(-0.00400692000005477,12.2,3.99874359799998));
#333197=CARTESIAN_POINT('Ctrl Pts',(-0.00400692000005477,5.2,3.99874359799998));
#333198=CARTESIAN_POINT('Ctrl Pts',(-0.00400692000005477,2.2,3.99874359799998));
#333199=CARTESIAN_POINT('Ctrl Pts',(-0.00401974900005598,12.2,3.99847984399998));
#333200=CARTESIAN_POINT('Ctrl Pts',(-0.00401974900005598,5.2,3.99847984399998));
#333201=CARTESIAN_POINT('Ctrl Pts',(-0.00401974900005598,2.2,3.99847984399998));
#333202=CARTESIAN_POINT('Ctrl Pts',(-0.0040319000000555,12.2,3.99822295999999));
#333203=CARTESIAN_POINT('Ctrl Pts',(-0.0040319000000555,5.2,3.99822295999999));
#333204=CARTESIAN_POINT('Ctrl Pts',(-0.0040319000000555,2.2,3.99822295999999));
#333205=CARTESIAN_POINT('Ctrl Pts',(-0.00404339100005592,12.2,3.99797296399999));
#333206=CARTESIAN_POINT('Ctrl Pts',(-0.00404339100005592,5.2,3.99797296399999));
#333207=CARTESIAN_POINT('Ctrl Pts',(-0.00404339100005592,2.2,3.99797296399999));
#333208=CARTESIAN_POINT('Ctrl Pts',(-0.0040542400000554,12.2,3.99772987199999));
#333209=CARTESIAN_POINT('Ctrl Pts',(-0.0040542400000554,5.2,3.99772987199999));
#333210=CARTESIAN_POINT('Ctrl Pts',(-0.0040542400000554,2.2,3.99772987199999));
#333211=CARTESIAN_POINT('Ctrl Pts',(-0.00406446400005534,12.2,3.99749369899999));
#333212=CARTESIAN_POINT('Ctrl Pts',(-0.00406446400005534,5.2,3.99749369899999));
#333213=CARTESIAN_POINT('Ctrl Pts',(-0.00406446400005534,2.2,3.99749369899999));
#333214=CARTESIAN_POINT('Ctrl Pts',(-0.00407408100005503,12.2,3.99726446299999));
#333215=CARTESIAN_POINT('Ctrl Pts',(-0.00407408100005503,5.2,3.99726446299999));
#333216=CARTESIAN_POINT('Ctrl Pts',(-0.00407408100005503,2.2,3.99726446299999));
#333217=CARTESIAN_POINT('Ctrl Pts',(-0.00408310700005577,12.2,3.99704217899998));
#333218=CARTESIAN_POINT('Ctrl Pts',(-0.00408310700005577,5.2,3.99704217899998));
#333219=CARTESIAN_POINT('Ctrl Pts',(-0.00408310700005577,2.2,3.99704217899998));
#333220=CARTESIAN_POINT('Ctrl Pts',(-0.00409156300005598,12.2,3.99682686399998));
#333221=CARTESIAN_POINT('Ctrl Pts',(-0.00409156300005598,5.2,3.99682686399998));
#333222=CARTESIAN_POINT('Ctrl Pts',(-0.00409156300005598,2.2,3.99682686399998));
#333223=CARTESIAN_POINT('Ctrl Pts',(-0.00409946400005579,12.2,3.99661853599999));
#333224=CARTESIAN_POINT('Ctrl Pts',(-0.00409946400005579,5.2,3.99661853599999));
#333225=CARTESIAN_POINT('Ctrl Pts',(-0.00409946400005579,2.2,3.99661853599999));
#333226=CARTESIAN_POINT('Ctrl Pts',(-0.00410683100005583,12.2,3.99641720899999));
#333227=CARTESIAN_POINT('Ctrl Pts',(-0.00410683100005583,5.2,3.99641720899999));
#333228=CARTESIAN_POINT('Ctrl Pts',(-0.00410683100005583,2.2,3.99641720899999));
#333229=CARTESIAN_POINT('Ctrl Pts',(-0.00411367900005622,12.2,3.99622290199999));
#333230=CARTESIAN_POINT('Ctrl Pts',(-0.00411367900005622,5.2,3.99622290199999));
#333231=CARTESIAN_POINT('Ctrl Pts',(-0.00411367900005622,2.2,3.99622290199999));
#333232=CARTESIAN_POINT('Ctrl Pts',(-0.0041200280000553,12.2,3.99603563099999));
#333233=CARTESIAN_POINT('Ctrl Pts',(-0.0041200280000553,5.2,3.99603563099999));
#333234=CARTESIAN_POINT('Ctrl Pts',(-0.0041200280000553,2.2,3.99603563099999));
#333235=CARTESIAN_POINT('Ctrl Pts',(-0.00412589600005676,12.2,3.99585541199999));
#333236=CARTESIAN_POINT('Ctrl Pts',(-0.00412589600005676,5.2,3.99585541199999));
#333237=CARTESIAN_POINT('Ctrl Pts',(-0.00412589600005676,2.2,3.99585541199999));
#333238=CARTESIAN_POINT('Ctrl Pts',(-0.00413130000005536,12.2,3.99568226099999));
#333239=CARTESIAN_POINT('Ctrl Pts',(-0.00413130000005536,5.2,3.99568226099999));
#333240=CARTESIAN_POINT('Ctrl Pts',(-0.00413130000005536,2.2,3.99568226099999));
#333241=CARTESIAN_POINT('Ctrl Pts',(-0.00413625800005591,12.2,3.99551619599999));
#333242=CARTESIAN_POINT('Ctrl Pts',(-0.00413625800005591,5.2,3.99551619599999));
#333243=CARTESIAN_POINT('Ctrl Pts',(-0.00413625800005591,2.2,3.99551619599999));
#333244=CARTESIAN_POINT('Ctrl Pts',(-0.00414079000005564,12.2,3.99535723299999));
#333245=CARTESIAN_POINT('Ctrl Pts',(-0.00414079000005564,5.2,3.99535723299999));
#333246=CARTESIAN_POINT('Ctrl Pts',(-0.00414079000005564,2.2,3.99535723299999));
#333247=CARTESIAN_POINT('Ctrl Pts',(-0.00414491200005585,12.2,3.99520538699999));
#333248=CARTESIAN_POINT('Ctrl Pts',(-0.00414491200005585,5.2,3.99520538699999));
#333249=CARTESIAN_POINT('Ctrl Pts',(-0.00414491200005585,2.2,3.99520538699999));
#333250=CARTESIAN_POINT('Ctrl Pts',(-0.00414864600005616,12.2,3.99506067999998));
#333251=CARTESIAN_POINT('Ctrl Pts',(-0.00414864600005616,5.2,3.99506067999998));
#333252=CARTESIAN_POINT('Ctrl Pts',(-0.00414864600005616,2.2,3.99506067999998));
#333253=CARTESIAN_POINT('Ctrl Pts',(-0.00415201100005481,12.2,3.99492312699999));
#333254=CARTESIAN_POINT('Ctrl Pts',(-0.00415201100005481,5.2,3.99492312699999));
#333255=CARTESIAN_POINT('Ctrl Pts',(-0.00415201100005481,2.2,3.99492312699999));
#333256=CARTESIAN_POINT('Ctrl Pts',(-0.00415502700005566,12.2,3.99479274399998));
#333257=CARTESIAN_POINT('Ctrl Pts',(-0.00415502700005566,5.2,3.99479274399998));
#333258=CARTESIAN_POINT('Ctrl Pts',(-0.00415502700005566,2.2,3.99479274399998));
#333259=CARTESIAN_POINT('Ctrl Pts',(-0.00415771000005561,12.2,3.99466955099999));
#333260=CARTESIAN_POINT('Ctrl Pts',(-0.00415771000005561,5.2,3.99466955099999));
#333261=CARTESIAN_POINT('Ctrl Pts',(-0.00415771000005561,2.2,3.99466955099999));
#333262=CARTESIAN_POINT('Ctrl Pts',(-0.0041600800000552,12.2,3.99455356199999));
#333263=CARTESIAN_POINT('Ctrl Pts',(-0.0041600800000552,5.2,3.99455356199999));
#333264=CARTESIAN_POINT('Ctrl Pts',(-0.0041600800000552,2.2,3.99455356199999));
#333265=CARTESIAN_POINT('Ctrl Pts',(-0.00416215300005574,12.2,3.99444479099999));
#333266=CARTESIAN_POINT('Ctrl Pts',(-0.00416215300005574,5.2,3.99444479099999));
#333267=CARTESIAN_POINT('Ctrl Pts',(-0.00416215300005574,2.2,3.99444479099999));
#333268=CARTESIAN_POINT('Ctrl Pts',(-0.00416394400005627,12.2,3.99434325499998));
#333269=CARTESIAN_POINT('Ctrl Pts',(-0.00416394400005627,5.2,3.99434325499998));
#333270=CARTESIAN_POINT('Ctrl Pts',(-0.00416394400005627,2.2,3.99434325499998));
#333271=CARTESIAN_POINT('Ctrl Pts',(-0.00416547700005544,12.2,3.99424897099999));
#333272=CARTESIAN_POINT('Ctrl Pts',(-0.00416547700005544,5.2,3.99424897099999));
#333273=CARTESIAN_POINT('Ctrl Pts',(-0.00416547700005544,2.2,3.99424897099999));
#333274=CARTESIAN_POINT('Ctrl Pts',(-0.00416677000005584,12.2,3.99416195899998));
#333275=CARTESIAN_POINT('Ctrl Pts',(-0.00416677000005584,5.2,3.99416195899998));
#333276=CARTESIAN_POINT('Ctrl Pts',(-0.00416677000005584,2.2,3.99416195899998));
#333277=CARTESIAN_POINT('Ctrl Pts',(-0.00416785000005638,12.2,3.99408223999998));
#333278=CARTESIAN_POINT('Ctrl Pts',(-0.00416785000005638,5.2,3.99408223999998));
#333279=CARTESIAN_POINT('Ctrl Pts',(-0.00416785000005638,2.2,3.99408223999998));
#333280=CARTESIAN_POINT('Ctrl Pts',(-0.0041687420000558,12.2,3.99400983799998));
#333281=CARTESIAN_POINT('Ctrl Pts',(-0.0041687420000558,5.2,3.99400983799998));
#333282=CARTESIAN_POINT('Ctrl Pts',(-0.0041687420000558,2.2,3.99400983799998));
#333283=CARTESIAN_POINT('Ctrl Pts',(-0.00416946500005567,12.2,3.99394476899998));
#333284=CARTESIAN_POINT('Ctrl Pts',(-0.00416946500005567,5.2,3.99394476899998));
#333285=CARTESIAN_POINT('Ctrl Pts',(-0.00416946500005567,2.2,3.99394476899998));
#333286=CARTESIAN_POINT('Ctrl Pts',(-0.00417003700005637,12.2,3.99388704899999));
#333287=CARTESIAN_POINT('Ctrl Pts',(-0.00417003700005637,5.2,3.99388704899999));
#333288=CARTESIAN_POINT('Ctrl Pts',(-0.00417003700005637,2.2,3.99388704899999));
#333289=CARTESIAN_POINT('Ctrl Pts',(-0.00417051303328587,12.2,3.99383129333122));
#333290=CARTESIAN_POINT('Ctrl Pts',(-0.00417051303328587,5.2,3.99383129333122));
#333291=CARTESIAN_POINT('Ctrl Pts',(-0.00417051303328587,2.2,3.99383129333122));
#333292=CARTESIAN_POINT('Ctrl Pts',(-0.00417076165687092,12.2,3.99379318127802));
#333293=CARTESIAN_POINT('Ctrl Pts',(-0.00417076165687092,5.2,3.99379318127802));
#333294=CARTESIAN_POINT('Ctrl Pts',(-0.00417076165687092,2.2,3.99379318127802));
#333295=CARTESIAN_POINT('Ctrl Pts',(-0.00417087178589682,12.2,3.99376807430458));
#333296=CARTESIAN_POINT('Ctrl Pts',(-0.00417087178589682,5.2,3.99376807430458));
#333297=CARTESIAN_POINT('Ctrl Pts',(-0.00417087178589682,2.2,3.99376807430458));
#333298=CARTESIAN_POINT('Ctrl Pts',(-0.00417090550046129,12.2,3.99375243386499));
#333299=CARTESIAN_POINT('Ctrl Pts',(-0.00417090550046129,5.2,3.99375243386499));
#333300=CARTESIAN_POINT('Ctrl Pts',(-0.00417090550046129,2.2,3.99375243386499));
#333301=CARTESIAN_POINT('Ctrl Pts',(-0.00417093000005587,12.2,3.99374277699999));
#333302=CARTESIAN_POINT('Ctrl Pts',(-0.00417093000005587,5.2,3.99374277699999));
#333303=CARTESIAN_POINT('Ctrl Pts',(-0.00417093000005587,2.2,3.99374277699999));
#333304=CARTESIAN_POINT('',(0.335933473999944,12.2,4.73810602499999));
#333305=CARTESIAN_POINT('Origin',(-5.66300478732629E-14,15.2,-1.77635683940025E-14));
#333306=CARTESIAN_POINT('',(0.671001528999944,12.2,4.70236716499999));
#333307=CARTESIAN_POINT('Ctrl Pts',(0.846447287999944,12.2,3.90299745399999));
#333308=CARTESIAN_POINT('Ctrl Pts',(0.846447287999944,5.2,3.90299745399999));
#333309=CARTESIAN_POINT('Ctrl Pts',(0.846447287999944,2.2,3.90299745399999));
#333310=CARTESIAN_POINT('Ctrl Pts',(0.846448712915784,12.2,3.90300414660476));
#333311=CARTESIAN_POINT('Ctrl Pts',(0.846448712915784,5.2,3.90300414660476));
#333312=CARTESIAN_POINT('Ctrl Pts',(0.846448712915784,2.2,3.90300414660476));
#333313=CARTESIAN_POINT('Ctrl Pts',(0.846451469166328,12.2,3.90301709034366));
#333314=CARTESIAN_POINT('Ctrl Pts',(0.846451469166328,5.2,3.90301709034366));
#333315=CARTESIAN_POINT('Ctrl Pts',(0.846451469166328,2.2,3.90301709034366));
#333316=CARTESIAN_POINT('Ctrl Pts',(0.846455551098625,12.2,3.90303629127475));
#333317=CARTESIAN_POINT('Ctrl Pts',(0.846455551098625,5.19999999999999,
3.90303629127475));
#333318=CARTESIAN_POINT('Ctrl Pts',(0.846455551098625,2.2,3.90303629127475));
#333319=CARTESIAN_POINT('Ctrl Pts',(0.846460993740913,12.2,3.90306169326758));
#333320=CARTESIAN_POINT('Ctrl Pts',(0.846460993740913,5.2,3.90306169326758));
#333321=CARTESIAN_POINT('Ctrl Pts',(0.846460993740913,2.2,3.90306169326758));
#333322=CARTESIAN_POINT('Ctrl Pts',(0.846470204999944,12.2,3.90310607699998));
#333323=CARTESIAN_POINT('Ctrl Pts',(0.846470204999944,5.2,3.90310607699998));
#333324=CARTESIAN_POINT('Ctrl Pts',(0.846470204999944,2.2,3.90310607699998));
#333325=CARTESIAN_POINT('Ctrl Pts',(0.846480406999944,12.2,3.90315539799998));
#333326=CARTESIAN_POINT('Ctrl Pts',(0.846480406999944,5.2,3.90315539799998));
#333327=CARTESIAN_POINT('Ctrl Pts',(0.846480406999944,2.2,3.90315539799998));
#333328=CARTESIAN_POINT('Ctrl Pts',(0.846492022999944,12.2,3.90321194099998));
#333329=CARTESIAN_POINT('Ctrl Pts',(0.846492022999944,5.2,3.90321194099998));
#333330=CARTESIAN_POINT('Ctrl Pts',(0.846492022999944,2.2,3.90321194099998));
#333331=CARTESIAN_POINT('Ctrl Pts',(0.846505039999944,12.2,3.90327569799998));
#333332=CARTESIAN_POINT('Ctrl Pts',(0.846505039999944,5.2,3.90327569799998));
#333333=CARTESIAN_POINT('Ctrl Pts',(0.846505039999944,2.2,3.90327569799998));
#333334=CARTESIAN_POINT('Ctrl Pts',(0.846519438999944,12.2,3.90334666099999));
#333335=CARTESIAN_POINT('Ctrl Pts',(0.846519438999944,5.2,3.90334666099999));
#333336=CARTESIAN_POINT('Ctrl Pts',(0.846519438999944,2.2,3.90334666099999));
#333337=CARTESIAN_POINT('Ctrl Pts',(0.846535197999944,12.2,3.90342481399998));
#333338=CARTESIAN_POINT('Ctrl Pts',(0.846535197999944,5.2,3.90342481399998));
#333339=CARTESIAN_POINT('Ctrl Pts',(0.846535197999944,2.2,3.90342481399998));
#333340=CARTESIAN_POINT('Ctrl Pts',(0.846552286999944,12.2,3.90351014099998));
#333341=CARTESIAN_POINT('Ctrl Pts',(0.846552286999944,5.2,3.90351014099998));
#333342=CARTESIAN_POINT('Ctrl Pts',(0.846552286999944,2.2,3.90351014099998));
#333343=CARTESIAN_POINT('Ctrl Pts',(0.846570675999944,12.2,3.90360262699998));
#333344=CARTESIAN_POINT('Ctrl Pts',(0.846570675999944,5.2,3.90360262699998));
#333345=CARTESIAN_POINT('Ctrl Pts',(0.846570675999944,2.2,3.90360262699998));
#333346=CARTESIAN_POINT('Ctrl Pts',(0.846590339999944,12.2,3.90370225599998));
#333347=CARTESIAN_POINT('Ctrl Pts',(0.846590339999944,5.2,3.90370225599998));
#333348=CARTESIAN_POINT('Ctrl Pts',(0.846590339999944,2.2,3.90370225599998));
#333349=CARTESIAN_POINT('Ctrl Pts',(0.846611256999944,12.2,3.90380901799999));
#333350=CARTESIAN_POINT('Ctrl Pts',(0.846611256999944,5.2,3.90380901799999));
#333351=CARTESIAN_POINT('Ctrl Pts',(0.846611256999944,2.2,3.90380901799999));
#333352=CARTESIAN_POINT('Ctrl Pts',(0.846633405999944,12.2,3.90392289699999));
#333353=CARTESIAN_POINT('Ctrl Pts',(0.846633405999944,5.2,3.90392289699999));
#333354=CARTESIAN_POINT('Ctrl Pts',(0.846633405999944,2.2,3.90392289699999));
#333355=CARTESIAN_POINT('Ctrl Pts',(0.846656765999944,12.2,3.90404388499999));
#333356=CARTESIAN_POINT('Ctrl Pts',(0.846656765999944,5.2,3.90404388499999));
#333357=CARTESIAN_POINT('Ctrl Pts',(0.846656765999944,2.2,3.90404388499999));
#333358=CARTESIAN_POINT('Ctrl Pts',(0.846681319999945,12.2,3.90417196899998));
#333359=CARTESIAN_POINT('Ctrl Pts',(0.846681319999945,5.2,3.90417196899998));
#333360=CARTESIAN_POINT('Ctrl Pts',(0.846681319999945,2.2,3.90417196899998));
#333361=CARTESIAN_POINT('Ctrl Pts',(0.846707043999944,12.2,3.90430713799999));
#333362=CARTESIAN_POINT('Ctrl Pts',(0.846707043999944,5.2,3.90430713799999));
#333363=CARTESIAN_POINT('Ctrl Pts',(0.846707043999944,2.2,3.90430713799999));
#333364=CARTESIAN_POINT('Ctrl Pts',(0.846733914999944,12.2,3.90444937799998));
#333365=CARTESIAN_POINT('Ctrl Pts',(0.846733914999944,5.2,3.90444937799998));
#333366=CARTESIAN_POINT('Ctrl Pts',(0.846733914999944,2.2,3.90444937799998));
#333367=CARTESIAN_POINT('Ctrl Pts',(0.846761912999944,12.2,3.90459867599999));
#333368=CARTESIAN_POINT('Ctrl Pts',(0.846761912999944,5.2,3.90459867599999));
#333369=CARTESIAN_POINT('Ctrl Pts',(0.846761912999944,2.2,3.90459867599999));
#333370=CARTESIAN_POINT('Ctrl Pts',(0.846791012999945,12.2,3.90475501999998));
#333371=CARTESIAN_POINT('Ctrl Pts',(0.846791012999945,5.2,3.90475501999998));
#333372=CARTESIAN_POINT('Ctrl Pts',(0.846791012999945,2.2,3.90475501999998));
#333373=CARTESIAN_POINT('Ctrl Pts',(0.846821192999945,12.2,3.90491839499998));
#333374=CARTESIAN_POINT('Ctrl Pts',(0.846821192999945,5.2,3.90491839499998));
#333375=CARTESIAN_POINT('Ctrl Pts',(0.846821192999945,2.2,3.90491839499998));
#333376=CARTESIAN_POINT('Ctrl Pts',(0.846852431999944,12.2,3.90508878899999));
#333377=CARTESIAN_POINT('Ctrl Pts',(0.846852431999944,5.2,3.90508878899999));
#333378=CARTESIAN_POINT('Ctrl Pts',(0.846852431999944,2.2,3.90508878899999));
#333379=CARTESIAN_POINT('Ctrl Pts',(0.846884708999944,12.2,3.90526619099998));
#333380=CARTESIAN_POINT('Ctrl Pts',(0.846884708999944,5.2,3.90526619099998));
#333381=CARTESIAN_POINT('Ctrl Pts',(0.846884708999944,2.2,3.90526619099998));
#333382=CARTESIAN_POINT('Ctrl Pts',(0.846918002999945,12.2,3.90545058899999));
#333383=CARTESIAN_POINT('Ctrl Pts',(0.846918002999945,5.2,3.90545058899999));
#333384=CARTESIAN_POINT('Ctrl Pts',(0.846918002999945,2.2,3.90545058899999));
#333385=CARTESIAN_POINT('Ctrl Pts',(0.846952291999944,12.2,3.90564196899999));
#333386=CARTESIAN_POINT('Ctrl Pts',(0.846952291999944,5.2,3.90564196899999));
#333387=CARTESIAN_POINT('Ctrl Pts',(0.846952291999944,2.2,3.90564196899999));
#333388=CARTESIAN_POINT('Ctrl Pts',(0.846987556999944,12.2,3.90584031899999));
#333389=CARTESIAN_POINT('Ctrl Pts',(0.846987556999944,5.2,3.90584031899999));
#333390=CARTESIAN_POINT('Ctrl Pts',(0.846987556999944,2.2,3.90584031899999));
#333391=CARTESIAN_POINT('Ctrl Pts',(0.847023773999944,12.2,3.90604562799999));
#333392=CARTESIAN_POINT('Ctrl Pts',(0.847023773999944,5.2,3.90604562799999));
#333393=CARTESIAN_POINT('Ctrl Pts',(0.847023773999944,2.2,3.90604562799999));
#333394=CARTESIAN_POINT('Ctrl Pts',(0.847060923999944,12.2,3.90625788299998));
#333395=CARTESIAN_POINT('Ctrl Pts',(0.847060923999944,5.2,3.90625788299998));
#333396=CARTESIAN_POINT('Ctrl Pts',(0.847060923999944,2.2,3.90625788299998));
#333397=CARTESIAN_POINT('Ctrl Pts',(0.847098984999944,12.2,3.90647706899999));
#333398=CARTESIAN_POINT('Ctrl Pts',(0.847098984999944,5.2,3.90647706899999));
#333399=CARTESIAN_POINT('Ctrl Pts',(0.847098984999944,2.2,3.90647706899999));
#333400=CARTESIAN_POINT('Ctrl Pts',(0.847137935999944,12.2,3.90670317699998));
#333401=CARTESIAN_POINT('Ctrl Pts',(0.847137935999944,5.2,3.90670317699998));
#333402=CARTESIAN_POINT('Ctrl Pts',(0.847137935999944,2.2,3.90670317699998));
#333403=CARTESIAN_POINT('Ctrl Pts',(0.847177756999944,12.2,3.90693619299999));
#333404=CARTESIAN_POINT('Ctrl Pts',(0.847177756999944,5.2,3.90693619299999));
#333405=CARTESIAN_POINT('Ctrl Pts',(0.847177756999944,2.2,3.90693619299999));
#333406=CARTESIAN_POINT('Ctrl Pts',(0.847218424999945,12.2,3.90717610499999));
#333407=CARTESIAN_POINT('Ctrl Pts',(0.847218424999945,5.2,3.90717610499999));
#333408=CARTESIAN_POINT('Ctrl Pts',(0.847218424999945,2.2,3.90717610499999));
#333409=CARTESIAN_POINT('Ctrl Pts',(0.847259921999944,12.2,3.90742289999999));
#333410=CARTESIAN_POINT('Ctrl Pts',(0.847259921999944,5.2,3.90742289999999));
#333411=CARTESIAN_POINT('Ctrl Pts',(0.847259921999944,2.2,3.90742289999999));
#333412=CARTESIAN_POINT('Ctrl Pts',(0.847302226999944,12.2,3.90767656699998));
#333413=CARTESIAN_POINT('Ctrl Pts',(0.847302226999944,5.2,3.90767656699998));
#333414=CARTESIAN_POINT('Ctrl Pts',(0.847302226999944,2.2,3.90767656699998));
#333415=CARTESIAN_POINT('Ctrl Pts',(0.847345319999944,12.2,3.90793709299999));
#333416=CARTESIAN_POINT('Ctrl Pts',(0.847345319999944,5.2,3.90793709299999));
#333417=CARTESIAN_POINT('Ctrl Pts',(0.847345319999944,2.2,3.90793709299999));
#333418=CARTESIAN_POINT('Ctrl Pts',(0.847389178999944,12.2,3.90820446699998));
#333419=CARTESIAN_POINT('Ctrl Pts',(0.847389178999944,5.2,3.90820446699998));
#333420=CARTESIAN_POINT('Ctrl Pts',(0.847389178999944,2.2,3.90820446699998));
#333421=CARTESIAN_POINT('Ctrl Pts',(0.847433784999944,12.2,3.90847867499998));
#333422=CARTESIAN_POINT('Ctrl Pts',(0.847433784999944,5.2,3.90847867499998));
#333423=CARTESIAN_POINT('Ctrl Pts',(0.847433784999944,2.2,3.90847867499998));
#333424=CARTESIAN_POINT('Ctrl Pts',(0.847479116999944,12.2,3.90875970499999));
#333425=CARTESIAN_POINT('Ctrl Pts',(0.847479116999944,5.2,3.90875970499999));
#333426=CARTESIAN_POINT('Ctrl Pts',(0.847479116999944,2.2,3.90875970499999));
#333427=CARTESIAN_POINT('Ctrl Pts',(0.847525154999944,12.2,3.90904754499999));
#333428=CARTESIAN_POINT('Ctrl Pts',(0.847525154999944,5.2,3.90904754499999));
#333429=CARTESIAN_POINT('Ctrl Pts',(0.847525154999944,2.2,3.90904754499999));
#333430=CARTESIAN_POINT('Ctrl Pts',(0.847571879999944,12.2,3.90934218499999));
#333431=CARTESIAN_POINT('Ctrl Pts',(0.847571879999944,5.2,3.90934218499999));
#333432=CARTESIAN_POINT('Ctrl Pts',(0.847571879999944,2.2,3.90934218499999));
#333433=CARTESIAN_POINT('Ctrl Pts',(0.847619270999944,12.2,3.90964360999998));
#333434=CARTESIAN_POINT('Ctrl Pts',(0.847619270999944,5.2,3.90964360999998));
#333435=CARTESIAN_POINT('Ctrl Pts',(0.847619270999944,2.2,3.90964360999998));
#333436=CARTESIAN_POINT('Ctrl Pts',(0.847667308999944,12.2,3.90995180799998));
#333437=CARTESIAN_POINT('Ctrl Pts',(0.847667308999944,5.2,3.90995180799998));
#333438=CARTESIAN_POINT('Ctrl Pts',(0.847667308999944,2.2,3.90995180799998));
#333439=CARTESIAN_POINT('Ctrl Pts',(0.847715972999944,12.2,3.91026676999999));
#333440=CARTESIAN_POINT('Ctrl Pts',(0.847715972999944,5.2,3.91026676999999));
#333441=CARTESIAN_POINT('Ctrl Pts',(0.847715972999944,2.2,3.91026676999999));
#333442=CARTESIAN_POINT('Ctrl Pts',(0.847765243999944,12.2,3.91058847999999));
#333443=CARTESIAN_POINT('Ctrl Pts',(0.847765243999944,5.2,3.91058847999999));
#333444=CARTESIAN_POINT('Ctrl Pts',(0.847765243999944,2.2,3.91058847999999));
#333445=CARTESIAN_POINT('Ctrl Pts',(0.847815101999945,12.2,3.91091692899998));
#333446=CARTESIAN_POINT('Ctrl Pts',(0.847815101999945,5.2,3.91091692899998));
#333447=CARTESIAN_POINT('Ctrl Pts',(0.847815101999945,2.2,3.91091692899998));
#333448=CARTESIAN_POINT('Ctrl Pts',(0.847865527999944,12.2,3.91125210199998));
#333449=CARTESIAN_POINT('Ctrl Pts',(0.847865527999944,5.2,3.91125210199998));
#333450=CARTESIAN_POINT('Ctrl Pts',(0.847865527999944,2.2,3.91125210199998));
#333451=CARTESIAN_POINT('Ctrl Pts',(0.847916502999944,12.2,3.91159398899998));
#333452=CARTESIAN_POINT('Ctrl Pts',(0.847916502999944,5.2,3.91159398899998));
#333453=CARTESIAN_POINT('Ctrl Pts',(0.847916502999944,2.2,3.91159398899998));
#333454=CARTESIAN_POINT('Ctrl Pts',(0.847968007999944,12.2,3.91194257899999));
#333455=CARTESIAN_POINT('Ctrl Pts',(0.847968007999944,5.2,3.91194257899999));
#333456=CARTESIAN_POINT('Ctrl Pts',(0.847968007999944,2.2,3.91194257899999));
#333457=CARTESIAN_POINT('Ctrl Pts',(0.848020020999944,12.2,3.91229785699998));
#333458=CARTESIAN_POINT('Ctrl Pts',(0.848020020999944,5.2,3.91229785699998));
#333459=CARTESIAN_POINT('Ctrl Pts',(0.848020020999944,2.2,3.91229785699998));
#333460=CARTESIAN_POINT('Ctrl Pts',(0.848072523999944,12.2,3.91265981299998));
#333461=CARTESIAN_POINT('Ctrl Pts',(0.848072523999944,5.2,3.91265981299998));
#333462=CARTESIAN_POINT('Ctrl Pts',(0.848072523999944,2.2,3.91265981299998));
#333463=CARTESIAN_POINT('Ctrl Pts',(0.848125499999944,12.2,3.91302843499999));
#333464=CARTESIAN_POINT('Ctrl Pts',(0.848125499999944,5.2,3.91302843499999));
#333465=CARTESIAN_POINT('Ctrl Pts',(0.848125499999944,2.2,3.91302843499999));
#333466=CARTESIAN_POINT('Ctrl Pts',(0.848178926999944,12.2,3.91340370999998));
#333467=CARTESIAN_POINT('Ctrl Pts',(0.848178926999944,5.2,3.91340370999998));
#333468=CARTESIAN_POINT('Ctrl Pts',(0.848178926999944,2.2,3.91340370999998));
#333469=CARTESIAN_POINT('Ctrl Pts',(0.848232787999944,12.2,3.91378562799999));
#333470=CARTESIAN_POINT('Ctrl Pts',(0.848232787999944,5.2,3.91378562799999));
#333471=CARTESIAN_POINT('Ctrl Pts',(0.848232787999944,2.2,3.91378562799999));
#333472=CARTESIAN_POINT('Ctrl Pts',(0.848287061999944,12.2,3.91417417499999));
#333473=CARTESIAN_POINT('Ctrl Pts',(0.848287061999944,5.2,3.91417417499999));
#333474=CARTESIAN_POINT('Ctrl Pts',(0.848287061999944,2.2,3.91417417499999));
#333475=CARTESIAN_POINT('Ctrl Pts',(0.848341732999944,12.2,3.91456933999999));
#333476=CARTESIAN_POINT('Ctrl Pts',(0.848341732999944,5.2,3.91456933999999));
#333477=CARTESIAN_POINT('Ctrl Pts',(0.848341732999944,2.2,3.91456933999999));
#333478=CARTESIAN_POINT('Ctrl Pts',(0.848396778999944,12.2,3.91497111199998));
#333479=CARTESIAN_POINT('Ctrl Pts',(0.848396778999944,5.2,3.91497111199998));
#333480=CARTESIAN_POINT('Ctrl Pts',(0.848396778999944,2.2,3.91497111199998));
#333481=CARTESIAN_POINT('Ctrl Pts',(0.848452184999945,12.2,3.91537947699998));
#333482=CARTESIAN_POINT('Ctrl Pts',(0.848452184999945,5.2,3.91537947699998));
#333483=CARTESIAN_POINT('Ctrl Pts',(0.848452184999945,2.2,3.91537947699998));
#333484=CARTESIAN_POINT('Ctrl Pts',(0.848507928999944,12.2,3.91579442499999));
#333485=CARTESIAN_POINT('Ctrl Pts',(0.848507928999944,5.2,3.91579442499999));
#333486=CARTESIAN_POINT('Ctrl Pts',(0.848507928999944,2.2,3.91579442499999));
#333487=CARTESIAN_POINT('Ctrl Pts',(0.848563993999945,12.2,3.91621594399999));
#333488=CARTESIAN_POINT('Ctrl Pts',(0.848563993999945,5.2,3.91621594399999));
#333489=CARTESIAN_POINT('Ctrl Pts',(0.848563993999945,2.2,3.91621594399999));
#333490=CARTESIAN_POINT('Ctrl Pts',(0.848620361999944,12.2,3.91664402199999));
#333491=CARTESIAN_POINT('Ctrl Pts',(0.848620361999944,5.2,3.91664402199999));
#333492=CARTESIAN_POINT('Ctrl Pts',(0.848620361999944,2.2,3.91664402199999));
#333493=CARTESIAN_POINT('Ctrl Pts',(0.848677012999944,12.2,3.91707864699999));
#333494=CARTESIAN_POINT('Ctrl Pts',(0.848677012999944,5.2,3.91707864699999));
#333495=CARTESIAN_POINT('Ctrl Pts',(0.848677012999944,2.2,3.91707864699999));
#333496=CARTESIAN_POINT('Ctrl Pts',(0.848733929999944,12.2,3.91751980599999));
#333497=CARTESIAN_POINT('Ctrl Pts',(0.848733929999944,5.2,3.91751980599999));
#333498=CARTESIAN_POINT('Ctrl Pts',(0.848733929999944,2.2,3.91751980599999));
#333499=CARTESIAN_POINT('Ctrl Pts',(0.848791094999944,12.2,3.91796748999998));
#333500=CARTESIAN_POINT('Ctrl Pts',(0.848791094999944,5.2,3.91796748999998));
#333501=CARTESIAN_POINT('Ctrl Pts',(0.848791094999944,2.2,3.91796748999998));
#333502=CARTESIAN_POINT('Ctrl Pts',(0.848848487999944,12.2,3.91842168499998));
#333503=CARTESIAN_POINT('Ctrl Pts',(0.848848487999944,5.2,3.91842168499998));
#333504=CARTESIAN_POINT('Ctrl Pts',(0.848848487999944,2.2,3.91842168499998));
#333505=CARTESIAN_POINT('Ctrl Pts',(0.848906091999945,12.2,3.91888237999999));
#333506=CARTESIAN_POINT('Ctrl Pts',(0.848906091999945,5.2,3.91888237999999));
#333507=CARTESIAN_POINT('Ctrl Pts',(0.848906091999945,2.2,3.91888237999999));
#333508=CARTESIAN_POINT('Ctrl Pts',(0.848963890999944,12.2,3.91934956299998));
#333509=CARTESIAN_POINT('Ctrl Pts',(0.848963890999944,5.2,3.91934956299998));
#333510=CARTESIAN_POINT('Ctrl Pts',(0.848963890999944,2.2,3.91934956299998));
#333511=CARTESIAN_POINT('Ctrl Pts',(0.849021862999945,12.2,3.91982322299998));
#333512=CARTESIAN_POINT('Ctrl Pts',(0.849021862999945,5.2,3.91982322299998));
#333513=CARTESIAN_POINT('Ctrl Pts',(0.849021862999945,2.2,3.91982322299998));
#333514=CARTESIAN_POINT('Ctrl Pts',(0.849079992999945,12.2,3.92030334899999));
#333515=CARTESIAN_POINT('Ctrl Pts',(0.849079992999945,5.2,3.92030334899999));
#333516=CARTESIAN_POINT('Ctrl Pts',(0.849079992999945,2.2,3.92030334899999));
#333517=CARTESIAN_POINT('Ctrl Pts',(0.849138261999944,12.2,3.92078992799998));
#333518=CARTESIAN_POINT('Ctrl Pts',(0.849138261999944,5.2,3.92078992799998));
#333519=CARTESIAN_POINT('Ctrl Pts',(0.849138261999944,2.2,3.92078992799998));
#333520=CARTESIAN_POINT('Ctrl Pts',(0.849196652999944,12.2,3.92128294799999));
#333521=CARTESIAN_POINT('Ctrl Pts',(0.849196652999944,5.2,3.92128294799999));
#333522=CARTESIAN_POINT('Ctrl Pts',(0.849196652999944,2.2,3.92128294799999));
#333523=CARTESIAN_POINT('Ctrl Pts',(0.849255145999944,12.2,3.92178239799998));
#333524=CARTESIAN_POINT('Ctrl Pts',(0.849255145999944,5.2,3.92178239799998));
#333525=CARTESIAN_POINT('Ctrl Pts',(0.849255145999944,2.2,3.92178239799998));
#333526=CARTESIAN_POINT('Ctrl Pts',(0.849313727999944,12.2,3.92228826699998));
#333527=CARTESIAN_POINT('Ctrl Pts',(0.849313727999944,5.2,3.92228826699998));
#333528=CARTESIAN_POINT('Ctrl Pts',(0.849313727999944,2.2,3.92228826699998));
#333529=CARTESIAN_POINT('Ctrl Pts',(0.849372375999944,12.2,3.92280054199999));
#333530=CARTESIAN_POINT('Ctrl Pts',(0.849372375999944,5.2,3.92280054199999));
#333531=CARTESIAN_POINT('Ctrl Pts',(0.849372375999944,2.2,3.92280054199999));
#333532=CARTESIAN_POINT('Ctrl Pts',(0.849431077999945,12.2,3.92331921299998));
#333533=CARTESIAN_POINT('Ctrl Pts',(0.849431077999945,5.2,3.92331921299998));
#333534=CARTESIAN_POINT('Ctrl Pts',(0.849431077999945,2.2,3.92331921299998));
#333535=CARTESIAN_POINT('Ctrl Pts',(0.849489810999944,12.2,3.92384426799998));
#333536=CARTESIAN_POINT('Ctrl Pts',(0.849489810999944,5.2,3.92384426799998));
#333537=CARTESIAN_POINT('Ctrl Pts',(0.849489810999944,2.2,3.92384426799998));
#333538=CARTESIAN_POINT('Ctrl Pts',(0.849548561999944,12.2,3.92437569399998));
#333539=CARTESIAN_POINT('Ctrl Pts',(0.849548561999944,5.2,3.92437569399998));
#333540=CARTESIAN_POINT('Ctrl Pts',(0.849548561999944,2.2,3.92437569399998));
#333541=CARTESIAN_POINT('Ctrl Pts',(0.849607310999944,12.2,3.92491348299998));
#333542=CARTESIAN_POINT('Ctrl Pts',(0.849607310999944,5.2,3.92491348299998));
#333543=CARTESIAN_POINT('Ctrl Pts',(0.849607310999944,2.2,3.92491348299998));
#333544=CARTESIAN_POINT('Ctrl Pts',(0.849666042999945,12.2,3.92545761799998));
#333545=CARTESIAN_POINT('Ctrl Pts',(0.849666042999945,5.2,3.92545761799998));
#333546=CARTESIAN_POINT('Ctrl Pts',(0.849666042999945,2.2,3.92545761799998));
#333547=CARTESIAN_POINT('Ctrl Pts',(0.849724738999944,12.2,3.92600809299999));
#333548=CARTESIAN_POINT('Ctrl Pts',(0.849724738999944,5.2,3.92600809299999));
#333549=CARTESIAN_POINT('Ctrl Pts',(0.849724738999944,2.2,3.92600809299999));
#333550=CARTESIAN_POINT('Ctrl Pts',(0.849783383999945,12.2,3.92656489399998));
#333551=CARTESIAN_POINT('Ctrl Pts',(0.849783383999945,5.2,3.92656489399998));
#333552=CARTESIAN_POINT('Ctrl Pts',(0.849783383999945,2.2,3.92656489399998));
#333553=CARTESIAN_POINT('Ctrl Pts',(0.849841957999944,12.2,3.92712800899999));
#333554=CARTESIAN_POINT('Ctrl Pts',(0.849841957999944,5.2,3.92712800899999));
#333555=CARTESIAN_POINT('Ctrl Pts',(0.849841957999944,2.2,3.92712800899999));
#333556=CARTESIAN_POINT('Ctrl Pts',(0.849900445999944,12.2,3.92769742699999));
#333557=CARTESIAN_POINT('Ctrl Pts',(0.849900445999944,5.2,3.92769742699999));
#333558=CARTESIAN_POINT('Ctrl Pts',(0.849900445999944,2.2,3.92769742699999));
#333559=CARTESIAN_POINT('Ctrl Pts',(0.849958830999944,12.2,3.92827313699998));
#333560=CARTESIAN_POINT('Ctrl Pts',(0.849958830999944,5.2,3.92827313699998));
#333561=CARTESIAN_POINT('Ctrl Pts',(0.849958830999944,2.2,3.92827313699998));
#333562=CARTESIAN_POINT('Ctrl Pts',(0.850017095999944,12.2,3.92885512799998));
#333563=CARTESIAN_POINT('Ctrl Pts',(0.850017095999944,5.2,3.92885512799998));
#333564=CARTESIAN_POINT('Ctrl Pts',(0.850017095999944,2.2,3.92885512799998));
#333565=CARTESIAN_POINT('Ctrl Pts',(0.850075223999944,12.2,3.92944338699999));
#333566=CARTESIAN_POINT('Ctrl Pts',(0.850075223999944,5.2,3.92944338699999));
#333567=CARTESIAN_POINT('Ctrl Pts',(0.850075223999944,2.2,3.92944338699999));
#333568=CARTESIAN_POINT('Ctrl Pts',(0.850133198999944,12.2,3.93003790399998));
#333569=CARTESIAN_POINT('Ctrl Pts',(0.850133198999944,5.2,3.93003790399998));
#333570=CARTESIAN_POINT('Ctrl Pts',(0.850133198999944,2.2,3.93003790399998));
#333571=CARTESIAN_POINT('Ctrl Pts',(0.850191003999944,12.2,3.93063866799999));
#333572=CARTESIAN_POINT('Ctrl Pts',(0.850191003999944,5.2,3.93063866799999));
#333573=CARTESIAN_POINT('Ctrl Pts',(0.850191003999944,2.2,3.93063866799999));
#333574=CARTESIAN_POINT('Ctrl Pts',(0.850248621999944,12.2,3.93124566599998));
#333575=CARTESIAN_POINT('Ctrl Pts',(0.850248621999944,5.2,3.93124566599998));
#333576=CARTESIAN_POINT('Ctrl Pts',(0.850248621999944,2.2,3.93124566599998));
#333577=CARTESIAN_POINT('Ctrl Pts',(0.850306036999945,12.2,3.93185888699998));
#333578=CARTESIAN_POINT('Ctrl Pts',(0.850306036999945,5.2,3.93185888699998));
#333579=CARTESIAN_POINT('Ctrl Pts',(0.850306036999945,2.2,3.93185888699998));
#333580=CARTESIAN_POINT('Ctrl Pts',(0.850363230999944,12.2,3.93247832099998));
#333581=CARTESIAN_POINT('Ctrl Pts',(0.850363230999944,5.2,3.93247832099998));
#333582=CARTESIAN_POINT('Ctrl Pts',(0.850363230999944,2.2,3.93247832099998));
#333583=CARTESIAN_POINT('Ctrl Pts',(0.850420188999944,12.2,3.93310395499999));
#333584=CARTESIAN_POINT('Ctrl Pts',(0.850420188999944,5.2,3.93310395499999));
#333585=CARTESIAN_POINT('Ctrl Pts',(0.850420188999944,2.2,3.93310395499999));
#333586=CARTESIAN_POINT('Ctrl Pts',(0.850476895999944,12.2,3.93373577899998));
#333587=CARTESIAN_POINT('Ctrl Pts',(0.850476895999944,5.2,3.93373577899998));
#333588=CARTESIAN_POINT('Ctrl Pts',(0.850476895999944,2.2,3.93373577899998));
#333589=CARTESIAN_POINT('Ctrl Pts',(0.850533333999944,12.2,3.93437378099998));
#333590=CARTESIAN_POINT('Ctrl Pts',(0.850533333999944,5.2,3.93437378099998));
#333591=CARTESIAN_POINT('Ctrl Pts',(0.850533333999944,2.2,3.93437378099998));
#333592=CARTESIAN_POINT('Ctrl Pts',(0.850589486999944,12.2,3.93501794899999));
#333593=CARTESIAN_POINT('Ctrl Pts',(0.850589486999944,5.2,3.93501794899999));
#333594=CARTESIAN_POINT('Ctrl Pts',(0.850589486999944,2.2,3.93501794899999));
#333595=CARTESIAN_POINT('Ctrl Pts',(0.850645338999944,12.2,3.93566827399999));
#333596=CARTESIAN_POINT('Ctrl Pts',(0.850645338999944,5.2,3.93566827399999));
#333597=CARTESIAN_POINT('Ctrl Pts',(0.850645338999944,2.2,3.93566827399999));
#333598=CARTESIAN_POINT('Ctrl Pts',(0.850700872999944,12.2,3.93632474299999));
#333599=CARTESIAN_POINT('Ctrl Pts',(0.850700872999944,5.2,3.93632474299999));
#333600=CARTESIAN_POINT('Ctrl Pts',(0.850700872999944,2.2,3.93632474299999));
#333601=CARTESIAN_POINT('Ctrl Pts',(0.850756075999944,12.2,3.93698734399998));
#333602=CARTESIAN_POINT('Ctrl Pts',(0.850756075999944,5.2,3.93698734399998));
#333603=CARTESIAN_POINT('Ctrl Pts',(0.850756075999944,2.2,3.93698734399998));
#333604=CARTESIAN_POINT('Ctrl Pts',(0.850810928999944,12.2,3.93765606799998));
#333605=CARTESIAN_POINT('Ctrl Pts',(0.850810928999944,5.2,3.93765606799998));
#333606=CARTESIAN_POINT('Ctrl Pts',(0.850810928999944,2.2,3.93765606799998));
#333607=CARTESIAN_POINT('Ctrl Pts',(0.850865416999944,12.2,3.93833090199998));
#333608=CARTESIAN_POINT('Ctrl Pts',(0.850865416999944,5.2,3.93833090199998));
#333609=CARTESIAN_POINT('Ctrl Pts',(0.850865416999944,2.2,3.93833090199998));
#333610=CARTESIAN_POINT('Ctrl Pts',(0.850919522999944,12.2,3.93901183599999));
#333611=CARTESIAN_POINT('Ctrl Pts',(0.850919522999944,5.2,3.93901183599999));
#333612=CARTESIAN_POINT('Ctrl Pts',(0.850919522999944,2.2,3.93901183599999));
#333613=CARTESIAN_POINT('Ctrl Pts',(0.850973233999944,12.2,3.93969885899998));
#333614=CARTESIAN_POINT('Ctrl Pts',(0.850973233999944,5.2,3.93969885899998));
#333615=CARTESIAN_POINT('Ctrl Pts',(0.850973233999944,2.2,3.93969885899998));
#333616=CARTESIAN_POINT('Ctrl Pts',(0.851026531999944,12.2,3.94039195799999));
#333617=CARTESIAN_POINT('Ctrl Pts',(0.851026531999944,5.2,3.94039195799999));
#333618=CARTESIAN_POINT('Ctrl Pts',(0.851026531999944,2.2,3.94039195799999));
#333619=CARTESIAN_POINT('Ctrl Pts',(0.851079402999945,12.2,3.94109112299999));
#333620=CARTESIAN_POINT('Ctrl Pts',(0.851079402999945,5.2,3.94109112299999));
#333621=CARTESIAN_POINT('Ctrl Pts',(0.851079402999945,2.2,3.94109112299999));
#333622=CARTESIAN_POINT('Ctrl Pts',(0.851131829999944,12.2,3.94179634299999));
#333623=CARTESIAN_POINT('Ctrl Pts',(0.851131829999944,5.2,3.94179634299999));
#333624=CARTESIAN_POINT('Ctrl Pts',(0.851131829999944,2.2,3.94179634299999));
#333625=CARTESIAN_POINT('Ctrl Pts',(0.851183796999945,12.2,3.94250760599999));
#333626=CARTESIAN_POINT('Ctrl Pts',(0.851183796999945,5.2,3.94250760599999));
#333627=CARTESIAN_POINT('Ctrl Pts',(0.851183796999945,2.2,3.94250760599999));
#333628=CARTESIAN_POINT('Ctrl Pts',(0.851235289999944,12.2,3.94322490199999));
#333629=CARTESIAN_POINT('Ctrl Pts',(0.851235289999944,5.2,3.94322490199999));
#333630=CARTESIAN_POINT('Ctrl Pts',(0.851235289999944,2.2,3.94322490199999));
#333631=CARTESIAN_POINT('Ctrl Pts',(0.851286293999944,12.2,3.94394821999998));
#333632=CARTESIAN_POINT('Ctrl Pts',(0.851286293999944,5.2,3.94394821999998));
#333633=CARTESIAN_POINT('Ctrl Pts',(0.851286293999944,2.2,3.94394821999998));
#333634=CARTESIAN_POINT('Ctrl Pts',(0.851336790999944,12.2,3.94467754799999));
#333635=CARTESIAN_POINT('Ctrl Pts',(0.851336790999944,5.2,3.94467754799999));
#333636=CARTESIAN_POINT('Ctrl Pts',(0.851336790999944,2.2,3.94467754799999));
#333637=CARTESIAN_POINT('Ctrl Pts',(0.851386768999944,12.2,3.94541287499998));
#333638=CARTESIAN_POINT('Ctrl Pts',(0.851386768999944,5.2,3.94541287499998));
#333639=CARTESIAN_POINT('Ctrl Pts',(0.851386768999944,2.2,3.94541287499998));
#333640=CARTESIAN_POINT('Ctrl Pts',(0.851436209999944,12.2,3.94615418899999));
#333641=CARTESIAN_POINT('Ctrl Pts',(0.851436209999944,5.2,3.94615418899999));
#333642=CARTESIAN_POINT('Ctrl Pts',(0.851436209999944,2.2,3.94615418899999));
#333643=CARTESIAN_POINT('Ctrl Pts',(0.851485099999943,12.2,3.94690148199999));
#333644=CARTESIAN_POINT('Ctrl Pts',(0.851485099999943,5.2,3.94690148199999));
#333645=CARTESIAN_POINT('Ctrl Pts',(0.851485099999943,2.2,3.94690148199999));
#333646=CARTESIAN_POINT('Ctrl Pts',(0.851533423999945,12.2,3.94765473999998));
#333647=CARTESIAN_POINT('Ctrl Pts',(0.851533423999945,5.2,3.94765473999998));
#333648=CARTESIAN_POINT('Ctrl Pts',(0.851533423999945,2.2,3.94765473999998));
#333649=CARTESIAN_POINT('Ctrl Pts',(0.851581165999944,12.2,3.94841395299999));
#333650=CARTESIAN_POINT('Ctrl Pts',(0.851581165999944,5.2,3.94841395299999));
#333651=CARTESIAN_POINT('Ctrl Pts',(0.851581165999944,2.2,3.94841395299999));
#333652=CARTESIAN_POINT('Ctrl Pts',(0.851628312999945,12.2,3.94917910899999));
#333653=CARTESIAN_POINT('Ctrl Pts',(0.851628312999945,5.2,3.94917910899999));
#333654=CARTESIAN_POINT('Ctrl Pts',(0.851628312999945,2.2,3.94917910899999));
#333655=CARTESIAN_POINT('Ctrl Pts',(0.851674847999945,12.2,3.94995019899999));
#333656=CARTESIAN_POINT('Ctrl Pts',(0.851674847999945,5.2,3.94995019899999));
#333657=CARTESIAN_POINT('Ctrl Pts',(0.851674847999945,2.2,3.94995019899999));
#333658=CARTESIAN_POINT('Ctrl Pts',(0.851720754999944,12.2,3.95072721099999));
#333659=CARTESIAN_POINT('Ctrl Pts',(0.851720754999944,5.2,3.95072721099999));
#333660=CARTESIAN_POINT('Ctrl Pts',(0.851720754999944,2.2,3.95072721099999));
#333661=CARTESIAN_POINT('Ctrl Pts',(0.851766022999944,12.2,3.95151013399998));
#333662=CARTESIAN_POINT('Ctrl Pts',(0.851766022999944,5.2,3.95151013399998));
#333663=CARTESIAN_POINT('Ctrl Pts',(0.851766022999944,2.2,3.95151013399998));
#333664=CARTESIAN_POINT('Ctrl Pts',(0.851810633999944,12.2,3.95229895699998));
#333665=CARTESIAN_POINT('Ctrl Pts',(0.851810633999944,5.2,3.95229895699998));
#333666=CARTESIAN_POINT('Ctrl Pts',(0.851810633999944,2.2,3.95229895699998));
#333667=CARTESIAN_POINT('Ctrl Pts',(0.851854574999944,12.2,3.95309366899999));
#333668=CARTESIAN_POINT('Ctrl Pts',(0.851854574999944,5.2,3.95309366899999));
#333669=CARTESIAN_POINT('Ctrl Pts',(0.851854574999944,2.2,3.95309366899999));
#333670=CARTESIAN_POINT('Ctrl Pts',(0.851897829999944,12.2,3.95389425899998));
#333671=CARTESIAN_POINT('Ctrl Pts',(0.851897829999944,5.2,3.95389425899998));
#333672=CARTESIAN_POINT('Ctrl Pts',(0.851897829999944,2.2,3.95389425899998));
#333673=CARTESIAN_POINT('Ctrl Pts',(0.851940384999944,12.2,3.95470071599998));
#333674=CARTESIAN_POINT('Ctrl Pts',(0.851940384999944,5.2,3.95470071599998));
#333675=CARTESIAN_POINT('Ctrl Pts',(0.851940384999944,2.2,3.95470071599998));
#333676=CARTESIAN_POINT('Ctrl Pts',(0.851982225999944,12.2,3.95551302999999));
#333677=CARTESIAN_POINT('Ctrl Pts',(0.851982225999944,5.2,3.95551302999999));
#333678=CARTESIAN_POINT('Ctrl Pts',(0.851982225999944,2.2,3.95551302999999));
#333679=CARTESIAN_POINT('Ctrl Pts',(0.852023336999944,12.2,3.95633118699998));
#333680=CARTESIAN_POINT('Ctrl Pts',(0.852023336999944,5.2,3.95633118699998));
#333681=CARTESIAN_POINT('Ctrl Pts',(0.852023336999944,2.2,3.95633118699998));
#333682=CARTESIAN_POINT('Ctrl Pts',(0.852063703999945,12.2,3.95715518099998));
#333683=CARTESIAN_POINT('Ctrl Pts',(0.852063703999945,5.2,3.95715518099998));
#333684=CARTESIAN_POINT('Ctrl Pts',(0.852063703999945,2.2,3.95715518099998));
#333685=CARTESIAN_POINT('Ctrl Pts',(0.852103313999945,12.2,3.95798499699998));
#333686=CARTESIAN_POINT('Ctrl Pts',(0.852103313999945,5.2,3.95798499699998));
#333687=CARTESIAN_POINT('Ctrl Pts',(0.852103313999945,2.2,3.95798499699998));
#333688=CARTESIAN_POINT('Ctrl Pts',(0.852142149999944,12.2,3.95882062599998));
#333689=CARTESIAN_POINT('Ctrl Pts',(0.852142149999944,5.2,3.95882062599998));
#333690=CARTESIAN_POINT('Ctrl Pts',(0.852142149999944,2.2,3.95882062599998));
#333691=CARTESIAN_POINT('Ctrl Pts',(0.852180199999945,12.2,3.95966205699998));
#333692=CARTESIAN_POINT('Ctrl Pts',(0.852180199999945,5.2,3.95966205699998));
#333693=CARTESIAN_POINT('Ctrl Pts',(0.852180199999945,2.2,3.95966205699998));
#333694=CARTESIAN_POINT('Ctrl Pts',(0.852217448999945,12.2,3.96050927799998));
#333695=CARTESIAN_POINT('Ctrl Pts',(0.852217448999945,5.2,3.96050927799998));
#333696=CARTESIAN_POINT('Ctrl Pts',(0.852217448999945,2.2,3.96050927799998));
#333697=CARTESIAN_POINT('Ctrl Pts',(0.852253881999945,12.2,3.96136228099999));
#333698=CARTESIAN_POINT('Ctrl Pts',(0.852253881999945,5.2,3.96136228099999));
#333699=CARTESIAN_POINT('Ctrl Pts',(0.852253881999945,2.2,3.96136228099999));
#333700=CARTESIAN_POINT('Ctrl Pts',(0.852289485999944,12.2,3.96222105099999));
#333701=CARTESIAN_POINT('Ctrl Pts',(0.852289485999944,5.2,3.96222105099999));
#333702=CARTESIAN_POINT('Ctrl Pts',(0.852289485999944,2.2,3.96222105099999));
#333703=CARTESIAN_POINT('Ctrl Pts',(0.852324245999945,12.2,3.96308557999999));
#333704=CARTESIAN_POINT('Ctrl Pts',(0.852324245999945,5.2,3.96308557999999));
#333705=CARTESIAN_POINT('Ctrl Pts',(0.852324245999945,2.2,3.96308557999999));
#333706=CARTESIAN_POINT('Ctrl Pts',(0.852358147999944,12.2,3.96395585799999));
#333707=CARTESIAN_POINT('Ctrl Pts',(0.852358147999944,5.2,3.96395585799999));
#333708=CARTESIAN_POINT('Ctrl Pts',(0.852358147999944,2.2,3.96395585799999));
#333709=CARTESIAN_POINT('Ctrl Pts',(0.852391178999944,12.2,3.96483187099999));
#333710=CARTESIAN_POINT('Ctrl Pts',(0.852391178999944,5.2,3.96483187099999));
#333711=CARTESIAN_POINT('Ctrl Pts',(0.852391178999944,2.2,3.96483187099999));
#333712=CARTESIAN_POINT('Ctrl Pts',(0.852423323999945,12.2,3.96571361099999));
#333713=CARTESIAN_POINT('Ctrl Pts',(0.852423323999945,5.2,3.96571361099999));
#333714=CARTESIAN_POINT('Ctrl Pts',(0.852423323999945,2.2,3.96571361099999));
#333715=CARTESIAN_POINT('Ctrl Pts',(0.852454568999944,12.2,3.96660106599998));
#333716=CARTESIAN_POINT('Ctrl Pts',(0.852454568999944,5.2,3.96660106599998));
#333717=CARTESIAN_POINT('Ctrl Pts',(0.852454568999944,2.2,3.96660106599998));
#333718=CARTESIAN_POINT('Ctrl Pts',(0.852484900999944,12.2,3.96749422499998));
#333719=CARTESIAN_POINT('Ctrl Pts',(0.852484900999944,5.2,3.96749422499998));
#333720=CARTESIAN_POINT('Ctrl Pts',(0.852484900999944,2.2,3.96749422499998));
#333721=CARTESIAN_POINT('Ctrl Pts',(0.852514304999944,12.2,3.96839307799999));
#333722=CARTESIAN_POINT('Ctrl Pts',(0.852514304999944,5.2,3.96839307799999));
#333723=CARTESIAN_POINT('Ctrl Pts',(0.852514304999944,2.2,3.96839307799999));
#333724=CARTESIAN_POINT('Ctrl Pts',(0.852542767999944,12.2,3.96929761499998));
#333725=CARTESIAN_POINT('Ctrl Pts',(0.852542767999944,5.2,3.96929761499998));
#333726=CARTESIAN_POINT('Ctrl Pts',(0.852542767999944,2.2,3.96929761499998));
#333727=CARTESIAN_POINT('Ctrl Pts',(0.852570275999944,12.2,3.97020782199998));
#333728=CARTESIAN_POINT('Ctrl Pts',(0.852570275999944,5.2,3.97020782199998));
#333729=CARTESIAN_POINT('Ctrl Pts',(0.852570275999944,2.2,3.97020782199998));
#333730=CARTESIAN_POINT('Ctrl Pts',(0.852596815999944,12.2,3.97112369199998));
#333731=CARTESIAN_POINT('Ctrl Pts',(0.852596815999944,5.2,3.97112369199998));
#333732=CARTESIAN_POINT('Ctrl Pts',(0.852596815999944,2.2,3.97112369199998));
#333733=CARTESIAN_POINT('Ctrl Pts',(0.852622373999944,12.2,3.97204521299999));
#333734=CARTESIAN_POINT('Ctrl Pts',(0.852622373999944,5.2,3.97204521299999));
#333735=CARTESIAN_POINT('Ctrl Pts',(0.852622373999944,2.2,3.97204521299999));
#333736=CARTESIAN_POINT('Ctrl Pts',(0.852646935999944,12.2,3.97297237299998));
#333737=CARTESIAN_POINT('Ctrl Pts',(0.852646935999944,5.2,3.97297237299998));
#333738=CARTESIAN_POINT('Ctrl Pts',(0.852646935999944,2.2,3.97297237299998));
#333739=CARTESIAN_POINT('Ctrl Pts',(0.852670487999945,12.2,3.97390516399999));
#333740=CARTESIAN_POINT('Ctrl Pts',(0.852670487999945,5.2,3.97390516399999));
#333741=CARTESIAN_POINT('Ctrl Pts',(0.852670487999945,2.2,3.97390516399999));
#333742=CARTESIAN_POINT('Ctrl Pts',(0.852693017999945,12.2,3.97484357199998));
#333743=CARTESIAN_POINT('Ctrl Pts',(0.852693017999945,5.2,3.97484357199998));
#333744=CARTESIAN_POINT('Ctrl Pts',(0.852693017999945,2.2,3.97484357199998));
#333745=CARTESIAN_POINT('Ctrl Pts',(0.852714510999945,12.2,3.97578758899999));
#333746=CARTESIAN_POINT('Ctrl Pts',(0.852714510999945,5.2,3.97578758899999));
#333747=CARTESIAN_POINT('Ctrl Pts',(0.852714510999945,2.2,3.97578758899999));
#333748=CARTESIAN_POINT('Ctrl Pts',(0.852734954999944,12.2,3.97673720299998));
#333749=CARTESIAN_POINT('Ctrl Pts',(0.852734954999944,5.2,3.97673720299998));
#333750=CARTESIAN_POINT('Ctrl Pts',(0.852734954999944,2.2,3.97673720299998));
#333751=CARTESIAN_POINT('Ctrl Pts',(0.852754335999945,12.2,3.97769240399998));
#333752=CARTESIAN_POINT('Ctrl Pts',(0.852754335999945,5.2,3.97769240399998));
#333753=CARTESIAN_POINT('Ctrl Pts',(0.852754335999945,2.2,3.97769240399998));
#333754=CARTESIAN_POINT('Ctrl Pts',(0.852772641999944,12.2,3.97865318099999));
#333755=CARTESIAN_POINT('Ctrl Pts',(0.852772641999944,5.2,3.97865318099999));
#333756=CARTESIAN_POINT('Ctrl Pts',(0.852772641999944,2.2,3.97865318099999));
#333757=CARTESIAN_POINT('Ctrl Pts',(0.852789856999945,12.2,3.97961952299998));
#333758=CARTESIAN_POINT('Ctrl Pts',(0.852789856999945,5.2,3.97961952299998));
#333759=CARTESIAN_POINT('Ctrl Pts',(0.852789856999945,2.2,3.97961952299998));
#333760=CARTESIAN_POINT('Ctrl Pts',(0.852805969999944,12.2,3.98059142099999));
#333761=CARTESIAN_POINT('Ctrl Pts',(0.852805969999944,5.2,3.98059142099999));
#333762=CARTESIAN_POINT('Ctrl Pts',(0.852805969999944,2.2,3.98059142099999));
#333763=CARTESIAN_POINT('Ctrl Pts',(0.852820967999944,12.2,3.98156886199998));
#333764=CARTESIAN_POINT('Ctrl Pts',(0.852820967999944,5.2,3.98156886199998));
#333765=CARTESIAN_POINT('Ctrl Pts',(0.852820967999944,2.2,3.98156886199998));
#333766=CARTESIAN_POINT('Ctrl Pts',(0.852834834999944,12.2,3.98255183799999));
#333767=CARTESIAN_POINT('Ctrl Pts',(0.852834834999944,5.2,3.98255183799999));
#333768=CARTESIAN_POINT('Ctrl Pts',(0.852834834999944,2.2,3.98255183799999));
#333769=CARTESIAN_POINT('Ctrl Pts',(0.852847561999944,12.2,3.98354033699999));
#333770=CARTESIAN_POINT('Ctrl Pts',(0.852847561999944,5.2,3.98354033699999));
#333771=CARTESIAN_POINT('Ctrl Pts',(0.852847561999944,2.2,3.98354033699999));
#333772=CARTESIAN_POINT('Ctrl Pts',(0.852859133999945,12.2,3.98453434699999));
#333773=CARTESIAN_POINT('Ctrl Pts',(0.852859133999945,5.2,3.98453434699999));
#333774=CARTESIAN_POINT('Ctrl Pts',(0.852859133999945,2.2,3.98453434699999));
#333775=CARTESIAN_POINT('Ctrl Pts',(0.852869537999944,12.2,3.98553385999998));
#333776=CARTESIAN_POINT('Ctrl Pts',(0.852869537999944,5.2,3.98553385999998));
#333777=CARTESIAN_POINT('Ctrl Pts',(0.852869537999944,2.2,3.98553385999998));
#333778=CARTESIAN_POINT('Ctrl Pts',(0.852878760999943,12.2,3.98653886499999));
#333779=CARTESIAN_POINT('Ctrl Pts',(0.852878760999943,5.2,3.98653886499999));
#333780=CARTESIAN_POINT('Ctrl Pts',(0.852878760999943,2.2,3.98653886499999));
#333781=CARTESIAN_POINT('Ctrl Pts',(0.852886789999945,12.2,3.98754934899999));
#333782=CARTESIAN_POINT('Ctrl Pts',(0.852886789999945,5.2,3.98754934899999));
#333783=CARTESIAN_POINT('Ctrl Pts',(0.852886789999945,2.2,3.98754934899999));
#333784=CARTESIAN_POINT('Ctrl Pts',(0.852893612999944,12.2,3.98856530599998));
#333785=CARTESIAN_POINT('Ctrl Pts',(0.852893612999944,5.2,3.98856530599998));
#333786=CARTESIAN_POINT('Ctrl Pts',(0.852893612999944,2.2,3.98856530599998));
#333787=CARTESIAN_POINT('Ctrl Pts',(0.852899216999944,12.2,3.98958671999999));
#333788=CARTESIAN_POINT('Ctrl Pts',(0.852899216999944,5.2,3.98958671999999));
#333789=CARTESIAN_POINT('Ctrl Pts',(0.852899216999944,2.2,3.98958671999999));
#333790=CARTESIAN_POINT('Ctrl Pts',(0.852903588999945,12.2,3.99061358499999));
#333791=CARTESIAN_POINT('Ctrl Pts',(0.852903588999945,5.2,3.99061358499999));
#333792=CARTESIAN_POINT('Ctrl Pts',(0.852903588999945,2.2,3.99061358499999));
#333793=CARTESIAN_POINT('Ctrl Pts',(0.852906715999944,12.2,3.99164588899998));
#333794=CARTESIAN_POINT('Ctrl Pts',(0.852906715999944,5.2,3.99164588899998));
#333795=CARTESIAN_POINT('Ctrl Pts',(0.852906715999944,2.2,3.99164588899998));
#333796=CARTESIAN_POINT('Ctrl Pts',(0.852908584999944,12.2,3.99268361999999));
#333797=CARTESIAN_POINT('Ctrl Pts',(0.852908584999944,5.2,3.99268361999999));
#333798=CARTESIAN_POINT('Ctrl Pts',(0.852908584999944,2.2,3.99268361999999));
#333799=CARTESIAN_POINT('Ctrl Pts',(0.852909184999944,12.2,3.99372676999998));
#333800=CARTESIAN_POINT('Ctrl Pts',(0.852909184999944,5.2,3.99372676999998));
#333801=CARTESIAN_POINT('Ctrl Pts',(0.852909184999944,2.2,3.99372676999998));
#333802=CARTESIAN_POINT('Ctrl Pts',(0.852908502999944,12.2,3.99477532799998));
#333803=CARTESIAN_POINT('Ctrl Pts',(0.852908502999944,5.2,3.99477532799998));
#333804=CARTESIAN_POINT('Ctrl Pts',(0.852908502999944,2.2,3.99477532799998));
#333805=CARTESIAN_POINT('Ctrl Pts',(0.852906525999945,12.2,3.99582927999998));
#333806=CARTESIAN_POINT('Ctrl Pts',(0.852906525999945,5.2,3.99582927999998));
#333807=CARTESIAN_POINT('Ctrl Pts',(0.852906525999945,2.2,3.99582927999998));
#333808=CARTESIAN_POINT('Ctrl Pts',(0.852903240999944,12.2,3.99688862099998));
#333809=CARTESIAN_POINT('Ctrl Pts',(0.852903240999944,5.2,3.99688862099998));
#333810=CARTESIAN_POINT('Ctrl Pts',(0.852903240999944,2.2,3.99688862099998));
#333811=CARTESIAN_POINT('Ctrl Pts',(0.852898635999945,12.2,3.99795333699998));
#333812=CARTESIAN_POINT('Ctrl Pts',(0.852898635999945,5.2,3.99795333699998));
#333813=CARTESIAN_POINT('Ctrl Pts',(0.852898635999945,2.2,3.99795333699998));
#333814=CARTESIAN_POINT('Ctrl Pts',(0.852892698999944,12.2,3.99902341999999));
#333815=CARTESIAN_POINT('Ctrl Pts',(0.852892698999944,5.2,3.99902341999999));
#333816=CARTESIAN_POINT('Ctrl Pts',(0.852892698999944,2.2,3.99902341999999));
#333817=CARTESIAN_POINT('Ctrl Pts',(0.852885417999943,12.2,4.00009885599999));
#333818=CARTESIAN_POINT('Ctrl Pts',(0.852885417999943,5.2,4.00009885599999));
#333819=CARTESIAN_POINT('Ctrl Pts',(0.852885417999943,2.2,4.00009885599999));
#333820=CARTESIAN_POINT('Ctrl Pts',(0.852876779999944,12.2,4.00117963799998));
#333821=CARTESIAN_POINT('Ctrl Pts',(0.852876779999944,5.2,4.00117963799998));
#333822=CARTESIAN_POINT('Ctrl Pts',(0.852876779999944,2.2,4.00117963799998));
#333823=CARTESIAN_POINT('Ctrl Pts',(0.852866772999944,12.2,4.00226575399999));
#333824=CARTESIAN_POINT('Ctrl Pts',(0.852866772999944,5.2,4.00226575399999));
#333825=CARTESIAN_POINT('Ctrl Pts',(0.852866772999944,2.2,4.00226575399999));
#333826=CARTESIAN_POINT('Ctrl Pts',(0.852855384999944,12.2,4.00335719399998));
#333827=CARTESIAN_POINT('Ctrl Pts',(0.852855384999944,5.2,4.00335719399998));
#333828=CARTESIAN_POINT('Ctrl Pts',(0.852855384999944,2.2,4.00335719399998));
#333829=CARTESIAN_POINT('Ctrl Pts',(0.852842602999945,12.2,4.00445394799998));
#333830=CARTESIAN_POINT('Ctrl Pts',(0.852842602999945,5.2,4.00445394799998));
#333831=CARTESIAN_POINT('Ctrl Pts',(0.852842602999945,2.2,4.00445394799998));
#333832=CARTESIAN_POINT('Ctrl Pts',(0.852828414999944,12.2,4.00555600399999));
#333833=CARTESIAN_POINT('Ctrl Pts',(0.852828414999944,5.2,4.00555600399999));
#333834=CARTESIAN_POINT('Ctrl Pts',(0.852828414999944,2.2,4.00555600399999));
#333835=CARTESIAN_POINT('Ctrl Pts',(0.852812809999944,12.2,4.00666335299999));
#333836=CARTESIAN_POINT('Ctrl Pts',(0.852812809999944,5.2,4.00666335299999));
#333837=CARTESIAN_POINT('Ctrl Pts',(0.852812809999944,2.2,4.00666335299999));
#333838=CARTESIAN_POINT('Ctrl Pts',(0.852795775999944,12.2,4.00777598499998));
#333839=CARTESIAN_POINT('Ctrl Pts',(0.852795775999944,5.2,4.00777598499998));
#333840=CARTESIAN_POINT('Ctrl Pts',(0.852795775999944,2.2,4.00777598499998));
#333841=CARTESIAN_POINT('Ctrl Pts',(0.852777298999944,12.2,4.00889388999998));
#333842=CARTESIAN_POINT('Ctrl Pts',(0.852777298999944,5.2,4.00889388999998));
#333843=CARTESIAN_POINT('Ctrl Pts',(0.852777298999944,2.2,4.00889388999998));
#333844=CARTESIAN_POINT('Ctrl Pts',(0.852757369999945,12.2,4.01001705599998));
#333845=CARTESIAN_POINT('Ctrl Pts',(0.852757369999945,5.2,4.01001705599998));
#333846=CARTESIAN_POINT('Ctrl Pts',(0.852757369999945,2.2,4.01001705599998));
#333847=CARTESIAN_POINT('Ctrl Pts',(0.852735973999944,12.2,4.01114547299999));
#333848=CARTESIAN_POINT('Ctrl Pts',(0.852735973999944,5.2,4.01114547299999));
#333849=CARTESIAN_POINT('Ctrl Pts',(0.852735973999944,2.2,4.01114547299999));
#333850=CARTESIAN_POINT('Ctrl Pts',(0.852713101999945,12.2,4.01227913099999));
#333851=CARTESIAN_POINT('Ctrl Pts',(0.852713101999945,5.2,4.01227913099999));
#333852=CARTESIAN_POINT('Ctrl Pts',(0.852713101999945,2.2,4.01227913099999));
#333853=CARTESIAN_POINT('Ctrl Pts',(0.852688740999944,12.2,4.01341801999998));
#333854=CARTESIAN_POINT('Ctrl Pts',(0.852688740999944,5.2,4.01341801999998));
#333855=CARTESIAN_POINT('Ctrl Pts',(0.852688740999944,2.2,4.01341801999998));
#333856=CARTESIAN_POINT('Ctrl Pts',(0.852662876999944,12.2,4.01456212999998));
#333857=CARTESIAN_POINT('Ctrl Pts',(0.852662876999944,5.2,4.01456212999998));
#333858=CARTESIAN_POINT('Ctrl Pts',(0.852662876999944,2.2,4.01456212999998));
#333859=CARTESIAN_POINT('Ctrl Pts',(0.852635501999944,12.2,4.01571144899999));
#333860=CARTESIAN_POINT('Ctrl Pts',(0.852635501999944,5.2,4.01571144899999));
#333861=CARTESIAN_POINT('Ctrl Pts',(0.852635501999944,2.2,4.01571144899999));
#333862=CARTESIAN_POINT('Ctrl Pts',(0.852606601999945,12.2,4.01686596899999));
#333863=CARTESIAN_POINT('Ctrl Pts',(0.852606601999945,5.2,4.01686596899999));
#333864=CARTESIAN_POINT('Ctrl Pts',(0.852606601999945,2.2,4.01686596899999));
#333865=CARTESIAN_POINT('Ctrl Pts',(0.852576166999944,12.2,4.01802567799999));
#333866=CARTESIAN_POINT('Ctrl Pts',(0.852576166999944,5.2,4.01802567799999));
#333867=CARTESIAN_POINT('Ctrl Pts',(0.852576166999944,2.2,4.01802567799999));
#333868=CARTESIAN_POINT('Ctrl Pts',(0.852544183999945,12.2,4.01919056699998));
#333869=CARTESIAN_POINT('Ctrl Pts',(0.852544183999945,5.2,4.01919056699998));
#333870=CARTESIAN_POINT('Ctrl Pts',(0.852544183999945,2.2,4.01919056699998));
#333871=CARTESIAN_POINT('Ctrl Pts',(0.852510640999945,12.2,4.02036062599999));
#333872=CARTESIAN_POINT('Ctrl Pts',(0.852510640999945,5.2,4.02036062599999));
#333873=CARTESIAN_POINT('Ctrl Pts',(0.852510640999945,2.2,4.02036062599999));
#333874=CARTESIAN_POINT('Ctrl Pts',(0.852475527999944,12.2,4.02153584299998));
#333875=CARTESIAN_POINT('Ctrl Pts',(0.852475527999944,5.2,4.02153584299998));
#333876=CARTESIAN_POINT('Ctrl Pts',(0.852475527999944,2.2,4.02153584299998));
#333877=CARTESIAN_POINT('Ctrl Pts',(0.852438831999944,12.2,4.02271620799999));
#333878=CARTESIAN_POINT('Ctrl Pts',(0.852438831999944,5.2,4.02271620799999));
#333879=CARTESIAN_POINT('Ctrl Pts',(0.852438831999944,2.2,4.02271620799999));
#333880=CARTESIAN_POINT('Ctrl Pts',(0.852400542999944,12.2,4.02390171199999));
#333881=CARTESIAN_POINT('Ctrl Pts',(0.852400542999944,5.2,4.02390171199999));
#333882=CARTESIAN_POINT('Ctrl Pts',(0.852400542999944,2.2,4.02390171199999));
#333883=CARTESIAN_POINT('Ctrl Pts',(0.852360646999945,12.2,4.02509234399999));
#333884=CARTESIAN_POINT('Ctrl Pts',(0.852360646999945,5.2,4.02509234399999));
#333885=CARTESIAN_POINT('Ctrl Pts',(0.852360646999945,2.2,4.02509234399999));
#333886=CARTESIAN_POINT('Ctrl Pts',(0.852319135999945,12.2,4.02628809399998));
#333887=CARTESIAN_POINT('Ctrl Pts',(0.852319135999945,5.2,4.02628809399998));
#333888=CARTESIAN_POINT('Ctrl Pts',(0.852319135999945,2.2,4.02628809399998));
#333889=CARTESIAN_POINT('Ctrl Pts',(0.852275997999944,12.2,4.02748895199998));
#333890=CARTESIAN_POINT('Ctrl Pts',(0.852275997999944,5.2,4.02748895199998));
#333891=CARTESIAN_POINT('Ctrl Pts',(0.852275997999944,2.2,4.02748895199998));
#333892=CARTESIAN_POINT('Ctrl Pts',(0.852231218999945,12.2,4.02869490799999));
#333893=CARTESIAN_POINT('Ctrl Pts',(0.852231218999945,5.2,4.02869490799999));
#333894=CARTESIAN_POINT('Ctrl Pts',(0.852231218999945,2.2,4.02869490799999));
#333895=CARTESIAN_POINT('Ctrl Pts',(0.852184791999945,12.2,4.02990594999999));
#333896=CARTESIAN_POINT('Ctrl Pts',(0.852184791999945,5.2,4.02990594999999));
#333897=CARTESIAN_POINT('Ctrl Pts',(0.852184791999945,2.2,4.02990594999999));
#333898=CARTESIAN_POINT('Ctrl Pts',(0.852136700999945,12.2,4.03112206999998));
#333899=CARTESIAN_POINT('Ctrl Pts',(0.852136700999945,5.2,4.03112206999998));
#333900=CARTESIAN_POINT('Ctrl Pts',(0.852136700999945,2.2,4.03112206999998));
#333901=CARTESIAN_POINT('Ctrl Pts',(0.852086937999944,12.2,4.03234325799998));
#333902=CARTESIAN_POINT('Ctrl Pts',(0.852086937999944,5.2,4.03234325799998));
#333903=CARTESIAN_POINT('Ctrl Pts',(0.852086937999944,2.2,4.03234325799998));
#333904=CARTESIAN_POINT('Ctrl Pts',(0.852035490999944,12.2,4.03356950199999));
#333905=CARTESIAN_POINT('Ctrl Pts',(0.852035490999944,5.2,4.03356950199999));
#333906=CARTESIAN_POINT('Ctrl Pts',(0.852035490999944,2.2,4.03356950199999));
#333907=CARTESIAN_POINT('Ctrl Pts',(0.851982348999945,12.2,4.03480079299998));
#333908=CARTESIAN_POINT('Ctrl Pts',(0.851982348999945,5.2,4.03480079299998));
#333909=CARTESIAN_POINT('Ctrl Pts',(0.851982348999945,2.2,4.03480079299998));
#333910=CARTESIAN_POINT('Ctrl Pts',(0.851927500999944,12.2,4.03603712099999));
#333911=CARTESIAN_POINT('Ctrl Pts',(0.851927500999944,5.2,4.03603712099999));
#333912=CARTESIAN_POINT('Ctrl Pts',(0.851927500999944,2.2,4.03603712099999));
#333913=CARTESIAN_POINT('Ctrl Pts',(0.851870935999944,12.2,4.03727847499999));
#333914=CARTESIAN_POINT('Ctrl Pts',(0.851870935999944,5.2,4.03727847499999));
#333915=CARTESIAN_POINT('Ctrl Pts',(0.851870935999944,2.2,4.03727847499999));
#333916=CARTESIAN_POINT('Ctrl Pts',(0.851812641999944,12.2,4.03852484599999));
#333917=CARTESIAN_POINT('Ctrl Pts',(0.851812641999944,5.2,4.03852484599999));
#333918=CARTESIAN_POINT('Ctrl Pts',(0.851812641999944,2.2,4.03852484599999));
#333919=CARTESIAN_POINT('Ctrl Pts',(0.851752610999944,12.2,4.03977622199999));
#333920=CARTESIAN_POINT('Ctrl Pts',(0.851752610999944,5.2,4.03977622199999));
#333921=CARTESIAN_POINT('Ctrl Pts',(0.851752610999944,2.2,4.03977622199999));
#333922=CARTESIAN_POINT('Ctrl Pts',(0.851690827999944,12.2,4.04103259599999));
#333923=CARTESIAN_POINT('Ctrl Pts',(0.851690827999944,5.2,4.04103259599999));
#333924=CARTESIAN_POINT('Ctrl Pts',(0.851690827999944,2.2,4.04103259599999));
#333925=CARTESIAN_POINT('Ctrl Pts',(0.851627284999944,12.2,4.04229395399998));
#333926=CARTESIAN_POINT('Ctrl Pts',(0.851627284999944,5.2,4.04229395399998));
#333927=CARTESIAN_POINT('Ctrl Pts',(0.851627284999944,2.2,4.04229395399998));
#333928=CARTESIAN_POINT('Ctrl Pts',(0.851561969999944,12.2,4.04356028899999));
#333929=CARTESIAN_POINT('Ctrl Pts',(0.851561969999944,5.2,4.04356028899999));
#333930=CARTESIAN_POINT('Ctrl Pts',(0.851561969999944,2.2,4.04356028899999));
#333931=CARTESIAN_POINT('Ctrl Pts',(0.851494872999944,12.2,4.04483158999999));
#333932=CARTESIAN_POINT('Ctrl Pts',(0.851494872999944,5.2,4.04483158999999));
#333933=CARTESIAN_POINT('Ctrl Pts',(0.851494872999944,2.2,4.04483158999999));
#333934=CARTESIAN_POINT('Ctrl Pts',(0.851425981999945,12.2,4.04610784699998));
#333935=CARTESIAN_POINT('Ctrl Pts',(0.851425981999945,5.2,4.04610784699998));
#333936=CARTESIAN_POINT('Ctrl Pts',(0.851425981999945,2.2,4.04610784699998));
#333937=CARTESIAN_POINT('Ctrl Pts',(0.851355286999944,12.2,4.04738904899999));
#333938=CARTESIAN_POINT('Ctrl Pts',(0.851355286999944,5.2,4.04738904899999));
#333939=CARTESIAN_POINT('Ctrl Pts',(0.851355286999944,2.2,4.04738904899999));
#333940=CARTESIAN_POINT('Ctrl Pts',(0.851282776999944,12.2,4.04867518799998));
#333941=CARTESIAN_POINT('Ctrl Pts',(0.851282776999944,5.2,4.04867518799998));
#333942=CARTESIAN_POINT('Ctrl Pts',(0.851282776999944,2.2,4.04867518799998));
#333943=CARTESIAN_POINT('Ctrl Pts',(0.851208441999944,12.2,4.04996625099999));
#333944=CARTESIAN_POINT('Ctrl Pts',(0.851208441999944,5.2,4.04996625099999));
#333945=CARTESIAN_POINT('Ctrl Pts',(0.851208441999944,2.2,4.04996625099999));
#333946=CARTESIAN_POINT('Ctrl Pts',(0.851132271999945,12.2,4.05126223099998));
#333947=CARTESIAN_POINT('Ctrl Pts',(0.851132271999945,5.2,4.05126223099998));
#333948=CARTESIAN_POINT('Ctrl Pts',(0.851132271999945,2.2,4.05126223099998));
#333949=CARTESIAN_POINT('Ctrl Pts',(0.851054254999944,12.2,4.05256311499999));
#333950=CARTESIAN_POINT('Ctrl Pts',(0.851054254999944,5.2,4.05256311499999));
#333951=CARTESIAN_POINT('Ctrl Pts',(0.851054254999944,2.2,4.05256311499999));
#333952=CARTESIAN_POINT('Ctrl Pts',(0.850974380999945,12.2,4.05386889599999));
#333953=CARTESIAN_POINT('Ctrl Pts',(0.850974380999945,5.2,4.05386889599999));
#333954=CARTESIAN_POINT('Ctrl Pts',(0.850974380999945,2.2,4.05386889599999));
#333955=CARTESIAN_POINT('Ctrl Pts',(0.850892638999944,12.2,4.05517956199999));
#333956=CARTESIAN_POINT('Ctrl Pts',(0.850892638999944,5.2,4.05517956199999));
#333957=CARTESIAN_POINT('Ctrl Pts',(0.850892638999944,2.2,4.05517956199999));
#333958=CARTESIAN_POINT('Ctrl Pts',(0.850809018999944,12.2,4.05649510399999));
#333959=CARTESIAN_POINT('Ctrl Pts',(0.850809018999944,5.2,4.05649510399999));
#333960=CARTESIAN_POINT('Ctrl Pts',(0.850809018999944,2.2,4.05649510399999));
#333961=CARTESIAN_POINT('Ctrl Pts',(0.850723510999944,12.2,4.05781551099999));
#333962=CARTESIAN_POINT('Ctrl Pts',(0.850723510999944,5.2,4.05781551099999));
#333963=CARTESIAN_POINT('Ctrl Pts',(0.850723510999944,2.2,4.05781551099999));
#333964=CARTESIAN_POINT('Ctrl Pts',(0.850636103999944,12.2,4.05914077399999));
#333965=CARTESIAN_POINT('Ctrl Pts',(0.850636103999944,5.2,4.05914077399999));
#333966=CARTESIAN_POINT('Ctrl Pts',(0.850636103999944,2.2,4.05914077399999));
#333967=CARTESIAN_POINT('Ctrl Pts',(0.850546785999944,12.2,4.06047088299999));
#333968=CARTESIAN_POINT('Ctrl Pts',(0.850546785999944,5.2,4.06047088299999));
#333969=CARTESIAN_POINT('Ctrl Pts',(0.850546785999944,2.2,4.06047088299999));
#333970=CARTESIAN_POINT('Ctrl Pts',(0.850455550999943,12.2,4.06180582599998));
#333971=CARTESIAN_POINT('Ctrl Pts',(0.850455550999943,5.2,4.06180582599998));
#333972=CARTESIAN_POINT('Ctrl Pts',(0.850455550999943,2.2,4.06180582599998));
#333973=CARTESIAN_POINT('Ctrl Pts',(0.850362384999944,12.2,4.06314559499998));
#333974=CARTESIAN_POINT('Ctrl Pts',(0.850362384999944,5.2,4.06314559499998));
#333975=CARTESIAN_POINT('Ctrl Pts',(0.850362384999944,2.2,4.06314559499998));
#333976=CARTESIAN_POINT('Ctrl Pts',(0.850267278999944,12.2,4.06449018099998));
#333977=CARTESIAN_POINT('Ctrl Pts',(0.850267278999944,5.2,4.06449018099998));
#333978=CARTESIAN_POINT('Ctrl Pts',(0.850267278999944,2.2,4.06449018099998));
#333979=CARTESIAN_POINT('Ctrl Pts',(0.850170222999944,12.2,4.06583957199998));
#333980=CARTESIAN_POINT('Ctrl Pts',(0.850170222999944,5.2,4.06583957199998));
#333981=CARTESIAN_POINT('Ctrl Pts',(0.850170222999944,2.2,4.06583957199998));
#333982=CARTESIAN_POINT('Ctrl Pts',(0.850071204999944,12.2,4.06719375799998));
#333983=CARTESIAN_POINT('Ctrl Pts',(0.850071204999944,5.2,4.06719375799998));
#333984=CARTESIAN_POINT('Ctrl Pts',(0.850071204999944,2.2,4.06719375799998));
#333985=CARTESIAN_POINT('Ctrl Pts',(0.849970217999945,12.2,4.06855273199999));
#333986=CARTESIAN_POINT('Ctrl Pts',(0.849970217999945,5.2,4.06855273199999));
#333987=CARTESIAN_POINT('Ctrl Pts',(0.849970217999945,2.2,4.06855273199999));
#333988=CARTESIAN_POINT('Ctrl Pts',(0.849867249999944,12.2,4.06991647999998));
#333989=CARTESIAN_POINT('Ctrl Pts',(0.849867249999944,5.2,4.06991647999998));
#333990=CARTESIAN_POINT('Ctrl Pts',(0.849867249999944,2.2,4.06991647999998));
#333991=CARTESIAN_POINT('Ctrl Pts',(0.849762289999945,12.2,4.07128499499999));
#333992=CARTESIAN_POINT('Ctrl Pts',(0.849762289999945,5.2,4.07128499499999));
#333993=CARTESIAN_POINT('Ctrl Pts',(0.849762289999945,2.2,4.07128499499999));
#333994=CARTESIAN_POINT('Ctrl Pts',(0.849655330999944,12.2,4.07265826499999));
#333995=CARTESIAN_POINT('Ctrl Pts',(0.849655330999944,5.2,4.07265826499999));
#333996=CARTESIAN_POINT('Ctrl Pts',(0.849655330999944,2.2,4.07265826499999));
#333997=CARTESIAN_POINT('Ctrl Pts',(0.849546358999944,12.2,4.07403628199998));
#333998=CARTESIAN_POINT('Ctrl Pts',(0.849546358999944,5.2,4.07403628199998));
#333999=CARTESIAN_POINT('Ctrl Pts',(0.849546358999944,2.2,4.07403628199998));
#334000=CARTESIAN_POINT('Ctrl Pts',(0.849435366999944,12.2,4.07541903499999));
#334001=CARTESIAN_POINT('Ctrl Pts',(0.849435366999944,5.2,4.07541903499999));
#334002=CARTESIAN_POINT('Ctrl Pts',(0.849435366999944,2.2,4.07541903499999));
#334003=CARTESIAN_POINT('Ctrl Pts',(0.849322344999944,12.2,4.07680651499999));
#334004=CARTESIAN_POINT('Ctrl Pts',(0.849322344999944,5.2,4.07680651499999));
#334005=CARTESIAN_POINT('Ctrl Pts',(0.849322344999944,2.2,4.07680651499999));
#334006=CARTESIAN_POINT('Ctrl Pts',(0.849207281999944,12.2,4.07819871099999));
#334007=CARTESIAN_POINT('Ctrl Pts',(0.849207281999944,5.2,4.07819871099999));
#334008=CARTESIAN_POINT('Ctrl Pts',(0.849207281999944,2.2,4.07819871099999));
#334009=CARTESIAN_POINT('Ctrl Pts',(0.849090166999944,12.2,4.07959561399998));
#334010=CARTESIAN_POINT('Ctrl Pts',(0.849090166999944,5.2,4.07959561399998));
#334011=CARTESIAN_POINT('Ctrl Pts',(0.849090166999944,2.2,4.07959561399998));
#334012=CARTESIAN_POINT('Ctrl Pts',(0.848970992999944,12.2,4.08099721399999));
#334013=CARTESIAN_POINT('Ctrl Pts',(0.848970992999944,5.2,4.08099721399999));
#334014=CARTESIAN_POINT('Ctrl Pts',(0.848970992999944,2.2,4.08099721399999));
#334015=CARTESIAN_POINT('Ctrl Pts',(0.848849747999945,12.2,4.08240349999998));
#334016=CARTESIAN_POINT('Ctrl Pts',(0.848849747999945,5.2,4.08240349999998));
#334017=CARTESIAN_POINT('Ctrl Pts',(0.848849747999945,2.2,4.08240349999998));
#334018=CARTESIAN_POINT('Ctrl Pts',(0.848726422999944,12.2,4.08381446399999));
#334019=CARTESIAN_POINT('Ctrl Pts',(0.848726422999944,5.2,4.08381446399999));
#334020=CARTESIAN_POINT('Ctrl Pts',(0.848726422999944,2.2,4.08381446399999));
#334021=CARTESIAN_POINT('Ctrl Pts',(0.848601007999944,12.2,4.08523009399998));
#334022=CARTESIAN_POINT('Ctrl Pts',(0.848601007999944,5.2,4.08523009399998));
#334023=CARTESIAN_POINT('Ctrl Pts',(0.848601007999944,2.2,4.08523009399998));
#334024=CARTESIAN_POINT('Ctrl Pts',(0.848473494999944,12.2,4.08665038299999));
#334025=CARTESIAN_POINT('Ctrl Pts',(0.848473494999944,5.2,4.08665038299999));
#334026=CARTESIAN_POINT('Ctrl Pts',(0.848473494999944,2.2,4.08665038299999));
#334027=CARTESIAN_POINT('Ctrl Pts',(0.848343870999945,12.2,4.08807531799999));
#334028=CARTESIAN_POINT('Ctrl Pts',(0.848343870999945,5.2,4.08807531799999));
#334029=CARTESIAN_POINT('Ctrl Pts',(0.848343870999945,2.2,4.08807531799999));
#334030=CARTESIAN_POINT('Ctrl Pts',(0.848212129999945,12.2,4.08950489299999));
#334031=CARTESIAN_POINT('Ctrl Pts',(0.848212129999945,5.2,4.08950489299999));
#334032=CARTESIAN_POINT('Ctrl Pts',(0.848212129999945,2.2,4.08950489299999));
#334033=CARTESIAN_POINT('Ctrl Pts',(0.848078258999945,12.2,4.09093909399999));
#334034=CARTESIAN_POINT('Ctrl Pts',(0.848078258999945,5.2,4.09093909399999));
#334035=CARTESIAN_POINT('Ctrl Pts',(0.848078258999945,2.2,4.09093909399999));
#334036=CARTESIAN_POINT('Ctrl Pts',(0.847942250999945,12.2,4.09237791399998));
#334037=CARTESIAN_POINT('Ctrl Pts',(0.847942250999945,5.2,4.09237791399998));
#334038=CARTESIAN_POINT('Ctrl Pts',(0.847942250999945,2.2,4.09237791399998));
#334039=CARTESIAN_POINT('Ctrl Pts',(0.847804094999944,12.2,4.09382134299998));
#334040=CARTESIAN_POINT('Ctrl Pts',(0.847804094999944,5.2,4.09382134299998));
#334041=CARTESIAN_POINT('Ctrl Pts',(0.847804094999944,2.2,4.09382134299998));
#334042=CARTESIAN_POINT('Ctrl Pts',(0.847663781999944,12.2,4.09526936999999));
#334043=CARTESIAN_POINT('Ctrl Pts',(0.847663781999944,5.2,4.09526936999999));
#334044=CARTESIAN_POINT('Ctrl Pts',(0.847663781999944,2.2,4.09526936999999));
#334045=CARTESIAN_POINT('Ctrl Pts',(0.847521301999944,12.2,4.09672198499998));
#334046=CARTESIAN_POINT('Ctrl Pts',(0.847521301999944,5.2,4.09672198499998));
#334047=CARTESIAN_POINT('Ctrl Pts',(0.847521301999944,2.2,4.09672198499998));
#334048=CARTESIAN_POINT('Ctrl Pts',(0.847376646999944,12.2,4.09817917999998));
#334049=CARTESIAN_POINT('Ctrl Pts',(0.847376646999944,5.2,4.09817917999998));
#334050=CARTESIAN_POINT('Ctrl Pts',(0.847376646999944,2.2,4.09817917999998));
#334051=CARTESIAN_POINT('Ctrl Pts',(0.847229806999944,12.2,4.09964094399999));
#334052=CARTESIAN_POINT('Ctrl Pts',(0.847229806999944,5.2,4.09964094399999));
#334053=CARTESIAN_POINT('Ctrl Pts',(0.847229806999944,2.2,4.09964094399999));
#334054=CARTESIAN_POINT('Ctrl Pts',(0.847080770999944,12.2,4.10110726699998));
#334055=CARTESIAN_POINT('Ctrl Pts',(0.847080770999944,5.2,4.10110726699998));
#334056=CARTESIAN_POINT('Ctrl Pts',(0.847080770999944,2.2,4.10110726699998));
#334057=CARTESIAN_POINT('Ctrl Pts',(0.846929531999944,12.2,4.10257814099998));
#334058=CARTESIAN_POINT('Ctrl Pts',(0.846929531999944,5.2,4.10257814099998));
#334059=CARTESIAN_POINT('Ctrl Pts',(0.846929531999944,2.2,4.10257814099998));
#334060=CARTESIAN_POINT('Ctrl Pts',(0.846776077999943,12.2,4.10405355399998));
#334061=CARTESIAN_POINT('Ctrl Pts',(0.846776077999943,5.2,4.10405355399998));
#334062=CARTESIAN_POINT('Ctrl Pts',(0.846776077999943,2.2,4.10405355399998));
#334063=CARTESIAN_POINT('Ctrl Pts',(0.846620402999945,12.2,4.10553349899998));
#334064=CARTESIAN_POINT('Ctrl Pts',(0.846620402999945,5.2,4.10553349899998));
#334065=CARTESIAN_POINT('Ctrl Pts',(0.846620402999945,2.2,4.10553349899998));
#334066=CARTESIAN_POINT('Ctrl Pts',(0.846462495999944,12.2,4.10701796199999));
#334067=CARTESIAN_POINT('Ctrl Pts',(0.846462495999944,5.2,4.10701796199999));
#334068=CARTESIAN_POINT('Ctrl Pts',(0.846462495999944,2.2,4.10701796199999));
#334069=CARTESIAN_POINT('Ctrl Pts',(0.846302346999944,12.2,4.10850693699999));
#334070=CARTESIAN_POINT('Ctrl Pts',(0.846302346999944,5.2,4.10850693699999));
#334071=CARTESIAN_POINT('Ctrl Pts',(0.846302346999944,2.2,4.10850693699999));
#334072=CARTESIAN_POINT('Ctrl Pts',(0.846139947999944,12.2,4.11000041399999));
#334073=CARTESIAN_POINT('Ctrl Pts',(0.846139947999944,5.2,4.11000041399999));
#334074=CARTESIAN_POINT('Ctrl Pts',(0.846139947999944,2.2,4.11000041399999));
#334075=CARTESIAN_POINT('Ctrl Pts',(0.845975289999944,12.2,4.11149838199999));
#334076=CARTESIAN_POINT('Ctrl Pts',(0.845975289999944,5.2,4.11149838199999));
#334077=CARTESIAN_POINT('Ctrl Pts',(0.845975289999944,2.2,4.11149838199999));
#334078=CARTESIAN_POINT('Ctrl Pts',(0.845808361999943,12.2,4.11300083099999));
#334079=CARTESIAN_POINT('Ctrl Pts',(0.845808361999943,5.2,4.11300083099999));
#334080=CARTESIAN_POINT('Ctrl Pts',(0.845808361999943,2.2,4.11300083099999));
#334081=CARTESIAN_POINT('Ctrl Pts',(0.845639156999944,12.2,4.11450775199998));
#334082=CARTESIAN_POINT('Ctrl Pts',(0.845639156999944,5.2,4.11450775199998));
#334083=CARTESIAN_POINT('Ctrl Pts',(0.845639156999944,2.2,4.11450775199998));
#334084=CARTESIAN_POINT('Ctrl Pts',(0.845467665999945,12.2,4.11601913699998));
#334085=CARTESIAN_POINT('Ctrl Pts',(0.845467665999945,5.2,4.11601913699998));
#334086=CARTESIAN_POINT('Ctrl Pts',(0.845467665999945,2.2,4.11601913699998));
#334087=CARTESIAN_POINT('Ctrl Pts',(0.845293878999944,12.2,4.11753497299999));
#334088=CARTESIAN_POINT('Ctrl Pts',(0.845293878999944,5.2,4.11753497299999));
#334089=CARTESIAN_POINT('Ctrl Pts',(0.845293878999944,2.2,4.11753497299999));
#334090=CARTESIAN_POINT('Ctrl Pts',(0.845117785999945,12.2,4.11905525299999));
#334091=CARTESIAN_POINT('Ctrl Pts',(0.845117785999945,5.2,4.11905525299999));
#334092=CARTESIAN_POINT('Ctrl Pts',(0.845117785999945,2.2,4.11905525299999));
#334093=CARTESIAN_POINT('Ctrl Pts',(0.844939379999944,12.2,4.12057996599999));
#334094=CARTESIAN_POINT('Ctrl Pts',(0.844939379999944,5.2,4.12057996599999));
#334095=CARTESIAN_POINT('Ctrl Pts',(0.844939379999944,2.2,4.12057996599999));
#334096=CARTESIAN_POINT('Ctrl Pts',(0.844758650999945,12.2,4.12210910299999));
#334097=CARTESIAN_POINT('Ctrl Pts',(0.844758650999945,5.2,4.12210910299999));
#334098=CARTESIAN_POINT('Ctrl Pts',(0.844758650999945,2.2,4.12210910299999));
#334099=CARTESIAN_POINT('Ctrl Pts',(0.844575590999944,12.2,4.12364265299999));
#334100=CARTESIAN_POINT('Ctrl Pts',(0.844575590999944,5.2,4.12364265299999));
#334101=CARTESIAN_POINT('Ctrl Pts',(0.844575590999944,2.2,4.12364265299999));
#334102=CARTESIAN_POINT('Ctrl Pts',(0.844390189999944,12.2,4.12518060899998));
#334103=CARTESIAN_POINT('Ctrl Pts',(0.844390189999944,5.2,4.12518060899998));
#334104=CARTESIAN_POINT('Ctrl Pts',(0.844390189999944,2.2,4.12518060899998));
#334105=CARTESIAN_POINT('Ctrl Pts',(0.844202440999945,12.2,4.12672295999998));
#334106=CARTESIAN_POINT('Ctrl Pts',(0.844202440999945,5.2,4.12672295999998));
#334107=CARTESIAN_POINT('Ctrl Pts',(0.844202440999945,2.2,4.12672295999998));
#334108=CARTESIAN_POINT('Ctrl Pts',(0.844012331999945,12.2,4.12826969399998));
#334109=CARTESIAN_POINT('Ctrl Pts',(0.844012331999945,5.2,4.12826969399998));
#334110=CARTESIAN_POINT('Ctrl Pts',(0.844012331999945,2.2,4.12826969399998));
#334111=CARTESIAN_POINT('Ctrl Pts',(0.843819855999944,12.2,4.12982080499999));
#334112=CARTESIAN_POINT('Ctrl Pts',(0.843819855999944,5.2,4.12982080499999));
#334113=CARTESIAN_POINT('Ctrl Pts',(0.843819855999944,2.2,4.12982080499999));
#334114=CARTESIAN_POINT('Ctrl Pts',(0.843625005999944,12.2,4.13137628199999));
#334115=CARTESIAN_POINT('Ctrl Pts',(0.843625005999944,5.2,4.13137628199999));
#334116=CARTESIAN_POINT('Ctrl Pts',(0.843625005999944,2.2,4.13137628199999));
#334117=CARTESIAN_POINT('Ctrl Pts',(0.843427769999944,12.2,4.13293611499999));
#334118=CARTESIAN_POINT('Ctrl Pts',(0.843427769999944,5.2,4.13293611499999));
#334119=CARTESIAN_POINT('Ctrl Pts',(0.843427769999944,2.2,4.13293611499999));
#334120=CARTESIAN_POINT('Ctrl Pts',(0.843228141999944,12.2,4.13450029499998));
#334121=CARTESIAN_POINT('Ctrl Pts',(0.843228141999944,5.2,4.13450029499998));
#334122=CARTESIAN_POINT('Ctrl Pts',(0.843228141999944,2.2,4.13450029499998));
#334123=CARTESIAN_POINT('Ctrl Pts',(0.843026111999944,12.2,4.13606881099999));
#334124=CARTESIAN_POINT('Ctrl Pts',(0.843026111999944,5.2,4.13606881099999));
#334125=CARTESIAN_POINT('Ctrl Pts',(0.843026111999944,2.2,4.13606881099999));
#334126=CARTESIAN_POINT('Ctrl Pts',(0.842821670999945,12.2,4.13764165599999));
#334127=CARTESIAN_POINT('Ctrl Pts',(0.842821670999945,5.2,4.13764165599999));
#334128=CARTESIAN_POINT('Ctrl Pts',(0.842821670999945,2.2,4.13764165599999));
#334129=CARTESIAN_POINT('Ctrl Pts',(0.842614809999944,12.2,4.13921881899999));
#334130=CARTESIAN_POINT('Ctrl Pts',(0.842614809999944,5.2,4.13921881899999));
#334131=CARTESIAN_POINT('Ctrl Pts',(0.842614809999944,2.2,4.13921881899999));
#334132=CARTESIAN_POINT('Ctrl Pts',(0.842405522999944,12.2,4.14080028899999));
#334133=CARTESIAN_POINT('Ctrl Pts',(0.842405522999944,5.2,4.14080028899999));
#334134=CARTESIAN_POINT('Ctrl Pts',(0.842405522999944,2.2,4.14080028899999));
#334135=CARTESIAN_POINT('Ctrl Pts',(0.842193798999944,12.2,4.14238605799999));
#334136=CARTESIAN_POINT('Ctrl Pts',(0.842193798999944,5.2,4.14238605799999));
#334137=CARTESIAN_POINT('Ctrl Pts',(0.842193798999944,2.2,4.14238605799999));
#334138=CARTESIAN_POINT('Ctrl Pts',(0.841979630999944,12.2,4.14397611799998));
#334139=CARTESIAN_POINT('Ctrl Pts',(0.841979630999944,5.2,4.14397611799998));
#334140=CARTESIAN_POINT('Ctrl Pts',(0.841979630999944,2.2,4.14397611799998));
#334141=CARTESIAN_POINT('Ctrl Pts',(0.841763009999944,12.2,4.14557045599998));
#334142=CARTESIAN_POINT('Ctrl Pts',(0.841763009999944,5.2,4.14557045599998));
#334143=CARTESIAN_POINT('Ctrl Pts',(0.841763009999944,2.2,4.14557045599998));
#334144=CARTESIAN_POINT('Ctrl Pts',(0.841543926999945,12.2,4.14716906499999));
#334145=CARTESIAN_POINT('Ctrl Pts',(0.841543926999945,5.2,4.14716906499999));
#334146=CARTESIAN_POINT('Ctrl Pts',(0.841543926999945,2.2,4.14716906499999));
#334147=CARTESIAN_POINT('Ctrl Pts',(0.841322372999944,12.2,4.14877193599998));
#334148=CARTESIAN_POINT('Ctrl Pts',(0.841322372999944,5.2,4.14877193599998));
#334149=CARTESIAN_POINT('Ctrl Pts',(0.841322372999944,2.2,4.14877193599998));
#334150=CARTESIAN_POINT('Ctrl Pts',(0.841098341999944,12.2,4.15037905699998));
#334151=CARTESIAN_POINT('Ctrl Pts',(0.841098341999944,5.2,4.15037905699998));
#334152=CARTESIAN_POINT('Ctrl Pts',(0.841098341999944,2.2,4.15037905699998));
#334153=CARTESIAN_POINT('Ctrl Pts',(0.840871822999943,12.2,4.15199041799998));
#334154=CARTESIAN_POINT('Ctrl Pts',(0.840871822999943,5.2,4.15199041799998));
#334155=CARTESIAN_POINT('Ctrl Pts',(0.840871822999943,2.2,4.15199041799998));
#334156=CARTESIAN_POINT('Ctrl Pts',(0.840642809999944,12.2,4.15360601399998));
#334157=CARTESIAN_POINT('Ctrl Pts',(0.840642809999944,5.2,4.15360601399998));
#334158=CARTESIAN_POINT('Ctrl Pts',(0.840642809999944,2.2,4.15360601399998));
#334159=CARTESIAN_POINT('Ctrl Pts',(0.840411292999944,12.2,4.15522582999999));
#334160=CARTESIAN_POINT('Ctrl Pts',(0.840411292999944,5.2,4.15522582999999));
#334161=CARTESIAN_POINT('Ctrl Pts',(0.840411292999944,2.2,4.15522582999999));
#334162=CARTESIAN_POINT('Ctrl Pts',(0.840177262999945,12.2,4.15684985999999));
#334163=CARTESIAN_POINT('Ctrl Pts',(0.840177262999945,5.2,4.15684985999999));
#334164=CARTESIAN_POINT('Ctrl Pts',(0.840177262999945,2.2,4.15684985999999));
#334165=CARTESIAN_POINT('Ctrl Pts',(0.839940712999944,12.2,4.15847809399998));
#334166=CARTESIAN_POINT('Ctrl Pts',(0.839940712999944,5.2,4.15847809399998));
#334167=CARTESIAN_POINT('Ctrl Pts',(0.839940712999944,2.2,4.15847809399998));
#334168=CARTESIAN_POINT('Ctrl Pts',(0.839701635999944,12.2,4.16011052199998));
#334169=CARTESIAN_POINT('Ctrl Pts',(0.839701635999944,5.2,4.16011052199998));
#334170=CARTESIAN_POINT('Ctrl Pts',(0.839701635999944,2.2,4.16011052199998));
#334171=CARTESIAN_POINT('Ctrl Pts',(0.839460021999944,12.2,4.16174713499998));
#334172=CARTESIAN_POINT('Ctrl Pts',(0.839460021999944,5.2,4.16174713499998));
#334173=CARTESIAN_POINT('Ctrl Pts',(0.839460021999944,2.2,4.16174713499998));
#334174=CARTESIAN_POINT('Ctrl Pts',(0.839215862999944,12.2,4.16338792299998));
#334175=CARTESIAN_POINT('Ctrl Pts',(0.839215862999944,5.2,4.16338792299998));
#334176=CARTESIAN_POINT('Ctrl Pts',(0.839215862999944,2.2,4.16338792299998));
#334177=CARTESIAN_POINT('Ctrl Pts',(0.838969151999944,12.2,4.16503287599999));
#334178=CARTESIAN_POINT('Ctrl Pts',(0.838969151999944,5.2,4.16503287599999));
#334179=CARTESIAN_POINT('Ctrl Pts',(0.838969151999944,2.2,4.16503287599999));
#334180=CARTESIAN_POINT('Ctrl Pts',(0.838719879999944,12.2,4.16668198599999));
#334181=CARTESIAN_POINT('Ctrl Pts',(0.838719879999944,5.2,4.16668198599999));
#334182=CARTESIAN_POINT('Ctrl Pts',(0.838719879999944,2.2,4.16668198599999));
#334183=CARTESIAN_POINT('Ctrl Pts',(0.838468037999944,12.2,4.16833524199999));
#334184=CARTESIAN_POINT('Ctrl Pts',(0.838468037999944,5.2,4.16833524199999));
#334185=CARTESIAN_POINT('Ctrl Pts',(0.838468037999944,2.2,4.16833524199999));
#334186=CARTESIAN_POINT('Ctrl Pts',(0.838213618999945,12.2,4.16999263699999));
#334187=CARTESIAN_POINT('Ctrl Pts',(0.838213618999945,5.2,4.16999263699999));
#334188=CARTESIAN_POINT('Ctrl Pts',(0.838213618999945,2.2,4.16999263699999));
#334189=CARTESIAN_POINT('Ctrl Pts',(0.837956614999944,12.2,4.17165415799998));
#334190=CARTESIAN_POINT('Ctrl Pts',(0.837956614999944,5.2,4.17165415799998));
#334191=CARTESIAN_POINT('Ctrl Pts',(0.837956614999944,2.2,4.17165415799998));
#334192=CARTESIAN_POINT('Ctrl Pts',(0.837697017999944,12.2,4.17331979799999));
#334193=CARTESIAN_POINT('Ctrl Pts',(0.837697017999944,5.2,4.17331979799999));
#334194=CARTESIAN_POINT('Ctrl Pts',(0.837697017999944,2.2,4.17331979799999));
#334195=CARTESIAN_POINT('Ctrl Pts',(0.837434820999944,12.2,4.17498954799999));
#334196=CARTESIAN_POINT('Ctrl Pts',(0.837434820999944,5.2,4.17498954799999));
#334197=CARTESIAN_POINT('Ctrl Pts',(0.837434820999944,2.2,4.17498954799999));
#334198=CARTESIAN_POINT('Ctrl Pts',(0.837170012999944,12.2,4.17666339699998));
#334199=CARTESIAN_POINT('Ctrl Pts',(0.837170012999944,5.2,4.17666339699998));
#334200=CARTESIAN_POINT('Ctrl Pts',(0.837170012999944,2.2,4.17666339699998));
#334201=CARTESIAN_POINT('Ctrl Pts',(0.836902588999945,12.2,4.17834133499999));
#334202=CARTESIAN_POINT('Ctrl Pts',(0.836902588999945,5.2,4.17834133499999));
#334203=CARTESIAN_POINT('Ctrl Pts',(0.836902588999945,2.2,4.17834133499999));
#334204=CARTESIAN_POINT('Ctrl Pts',(0.836632540999944,12.2,4.18002335599999));
#334205=CARTESIAN_POINT('Ctrl Pts',(0.836632540999944,5.2,4.18002335599999));
#334206=CARTESIAN_POINT('Ctrl Pts',(0.836632540999944,2.2,4.18002335599999));
#334207=CARTESIAN_POINT('Ctrl Pts',(0.836359857999944,12.2,4.18170944799999));
#334208=CARTESIAN_POINT('Ctrl Pts',(0.836359857999944,5.2,4.18170944799999));
#334209=CARTESIAN_POINT('Ctrl Pts',(0.836359857999944,2.2,4.18170944799999));
#334210=CARTESIAN_POINT('Ctrl Pts',(0.836084535999944,12.2,4.18339959999999));
#334211=CARTESIAN_POINT('Ctrl Pts',(0.836084535999944,5.2,4.18339959999999));
#334212=CARTESIAN_POINT('Ctrl Pts',(0.836084535999944,2.2,4.18339959999999));
#334213=CARTESIAN_POINT('Ctrl Pts',(0.835806564999944,12.2,4.18509380699999));
#334214=CARTESIAN_POINT('Ctrl Pts',(0.835806564999944,5.2,4.18509380699999));
#334215=CARTESIAN_POINT('Ctrl Pts',(0.835806564999944,2.2,4.18509380699999));
#334216=CARTESIAN_POINT('Ctrl Pts',(0.835525937999945,12.2,4.18679205599998));
#334217=CARTESIAN_POINT('Ctrl Pts',(0.835525937999945,5.2,4.18679205599998));
#334218=CARTESIAN_POINT('Ctrl Pts',(0.835525937999945,2.2,4.18679205599998));
#334219=CARTESIAN_POINT('Ctrl Pts',(0.835242646999944,12.2,4.18849433899998));
#334220=CARTESIAN_POINT('Ctrl Pts',(0.835242646999944,5.2,4.18849433899998));
#334221=CARTESIAN_POINT('Ctrl Pts',(0.835242646999944,2.2,4.18849433899998));
#334222=CARTESIAN_POINT('Ctrl Pts',(0.834956683999944,12.2,4.19020064599999));
#334223=CARTESIAN_POINT('Ctrl Pts',(0.834956683999944,5.2,4.19020064599999));
#334224=CARTESIAN_POINT('Ctrl Pts',(0.834956683999944,2.2,4.19020064599999));
#334225=CARTESIAN_POINT('Ctrl Pts',(0.834668041999944,12.2,4.19191096899999));
#334226=CARTESIAN_POINT('Ctrl Pts',(0.834668041999944,5.2,4.19191096899999));
#334227=CARTESIAN_POINT('Ctrl Pts',(0.834668041999944,2.2,4.19191096899999));
#334228=CARTESIAN_POINT('Ctrl Pts',(0.834376710999944,12.2,4.19362529799999));
#334229=CARTESIAN_POINT('Ctrl Pts',(0.834376710999944,5.2,4.19362529799999));
#334230=CARTESIAN_POINT('Ctrl Pts',(0.834376710999944,2.2,4.19362529799999));
#334231=CARTESIAN_POINT('Ctrl Pts',(0.834082687999944,12.2,4.19534362299999));
#334232=CARTESIAN_POINT('Ctrl Pts',(0.834082687999944,5.2,4.19534362299999));
#334233=CARTESIAN_POINT('Ctrl Pts',(0.834082687999944,2.2,4.19534362299999));
#334234=CARTESIAN_POINT('Ctrl Pts',(0.833785959999944,12.2,4.19706593499999));
#334235=CARTESIAN_POINT('Ctrl Pts',(0.833785959999944,5.2,4.19706593499999));
#334236=CARTESIAN_POINT('Ctrl Pts',(0.833785959999944,2.2,4.19706593499999));
#334237=CARTESIAN_POINT('Ctrl Pts',(0.833486523999943,12.2,4.19879222499999));
#334238=CARTESIAN_POINT('Ctrl Pts',(0.833486523999943,5.2,4.19879222499999));
#334239=CARTESIAN_POINT('Ctrl Pts',(0.833486523999943,2.2,4.19879222499999));
#334240=CARTESIAN_POINT('Ctrl Pts',(0.833184369999944,12.2,4.20052248299999));
#334241=CARTESIAN_POINT('Ctrl Pts',(0.833184369999944,5.2,4.20052248299999));
#334242=CARTESIAN_POINT('Ctrl Pts',(0.833184369999944,2.2,4.20052248299999));
#334243=CARTESIAN_POINT('Ctrl Pts',(0.832879489999944,12.2,4.20225669999999));
#334244=CARTESIAN_POINT('Ctrl Pts',(0.832879489999944,5.2,4.20225669999999));
#334245=CARTESIAN_POINT('Ctrl Pts',(0.832879489999944,2.2,4.20225669999999));
#334246=CARTESIAN_POINT('Ctrl Pts',(0.832571877999944,12.2,4.20399486699999));
#334247=CARTESIAN_POINT('Ctrl Pts',(0.832571877999944,5.2,4.20399486699999));
#334248=CARTESIAN_POINT('Ctrl Pts',(0.832571877999944,2.2,4.20399486699999));
#334249=CARTESIAN_POINT('Ctrl Pts',(0.832261524999944,12.2,4.20573697499999));
#334250=CARTESIAN_POINT('Ctrl Pts',(0.832261524999944,5.2,4.20573697499999));
#334251=CARTESIAN_POINT('Ctrl Pts',(0.832261524999944,2.2,4.20573697499999));
#334252=CARTESIAN_POINT('Ctrl Pts',(0.831948425999944,12.2,4.20748301399998));
#334253=CARTESIAN_POINT('Ctrl Pts',(0.831948425999944,5.2,4.20748301399998));
#334254=CARTESIAN_POINT('Ctrl Pts',(0.831948425999944,2.2,4.20748301399998));
#334255=CARTESIAN_POINT('Ctrl Pts',(0.831632569999944,12.2,4.20923297499999));
#334256=CARTESIAN_POINT('Ctrl Pts',(0.831632569999944,5.2,4.20923297499999));
#334257=CARTESIAN_POINT('Ctrl Pts',(0.831632569999944,2.2,4.20923297499999));
#334258=CARTESIAN_POINT('Ctrl Pts',(0.831313951999944,12.2,4.21098684799999));
#334259=CARTESIAN_POINT('Ctrl Pts',(0.831313951999944,5.2,4.21098684799999));
#334260=CARTESIAN_POINT('Ctrl Pts',(0.831313951999944,2.2,4.21098684799999));
#334261=CARTESIAN_POINT('Ctrl Pts',(0.830992564999944,12.2,4.21274462499999));
#334262=CARTESIAN_POINT('Ctrl Pts',(0.830992564999944,5.2,4.21274462499999));
#334263=CARTESIAN_POINT('Ctrl Pts',(0.830992564999944,2.2,4.21274462499999));
#334264=CARTESIAN_POINT('Ctrl Pts',(0.830668399999944,12.2,4.21450629599998));
#334265=CARTESIAN_POINT('Ctrl Pts',(0.830668399999944,5.2,4.21450629599998));
#334266=CARTESIAN_POINT('Ctrl Pts',(0.830668399999944,2.2,4.21450629599998));
#334267=CARTESIAN_POINT('Ctrl Pts',(0.830341450999944,12.2,4.21627185199998));
#334268=CARTESIAN_POINT('Ctrl Pts',(0.830341450999944,5.2,4.21627185199998));
#334269=CARTESIAN_POINT('Ctrl Pts',(0.830341450999944,2.2,4.21627185199998));
#334270=CARTESIAN_POINT('Ctrl Pts',(0.830011708999944,12.2,4.21804128199998));
#334271=CARTESIAN_POINT('Ctrl Pts',(0.830011708999944,5.2,4.21804128199998));
#334272=CARTESIAN_POINT('Ctrl Pts',(0.830011708999944,2.2,4.21804128199998));
#334273=CARTESIAN_POINT('Ctrl Pts',(0.829679168999945,12.2,4.21981457999999));
#334274=CARTESIAN_POINT('Ctrl Pts',(0.829679168999945,5.2,4.21981457999999));
#334275=CARTESIAN_POINT('Ctrl Pts',(0.829679168999945,2.2,4.21981457999999));
#334276=CARTESIAN_POINT('Ctrl Pts',(0.829343820999945,12.2,4.22159173399999));
#334277=CARTESIAN_POINT('Ctrl Pts',(0.829343820999945,5.2,4.22159173399999));
#334278=CARTESIAN_POINT('Ctrl Pts',(0.829343820999945,2.2,4.22159173399999));
#334279=CARTESIAN_POINT('Ctrl Pts',(0.829005659999944,12.2,4.22337273599998));
#334280=CARTESIAN_POINT('Ctrl Pts',(0.829005659999944,5.2,4.22337273599998));
#334281=CARTESIAN_POINT('Ctrl Pts',(0.829005659999944,2.2,4.22337273599998));
#334282=CARTESIAN_POINT('Ctrl Pts',(0.828664677999944,12.2,4.22515757699998));
#334283=CARTESIAN_POINT('Ctrl Pts',(0.828664677999944,5.2,4.22515757699998));
#334284=CARTESIAN_POINT('Ctrl Pts',(0.828664677999944,2.2,4.22515757699998));
#334285=CARTESIAN_POINT('Ctrl Pts',(0.828320867999944,12.2,4.22694624699999));
#334286=CARTESIAN_POINT('Ctrl Pts',(0.828320867999944,5.2,4.22694624699999));
#334287=CARTESIAN_POINT('Ctrl Pts',(0.828320867999944,2.2,4.22694624699999));
#334288=CARTESIAN_POINT('Ctrl Pts',(0.827974222999944,12.2,4.22873873599999));
#334289=CARTESIAN_POINT('Ctrl Pts',(0.827974222999944,5.2,4.22873873599999));
#334290=CARTESIAN_POINT('Ctrl Pts',(0.827974222999944,2.2,4.22873873599999));
#334291=CARTESIAN_POINT('Ctrl Pts',(0.827624734999944,12.2,4.23053503799999));
#334292=CARTESIAN_POINT('Ctrl Pts',(0.827624734999944,5.2,4.23053503799999));
#334293=CARTESIAN_POINT('Ctrl Pts',(0.827624734999944,2.2,4.23053503799999));
#334294=CARTESIAN_POINT('Ctrl Pts',(0.827272396999944,12.2,4.23233513899999));
#334295=CARTESIAN_POINT('Ctrl Pts',(0.827272396999944,5.2,4.23233513899999));
#334296=CARTESIAN_POINT('Ctrl Pts',(0.827272396999944,2.2,4.23233513899999));
#334297=CARTESIAN_POINT('Ctrl Pts',(0.826917202999944,12.2,4.23413903399998));
#334298=CARTESIAN_POINT('Ctrl Pts',(0.826917202999944,5.2,4.23413903399998));
#334299=CARTESIAN_POINT('Ctrl Pts',(0.826917202999944,2.2,4.23413903399998));
#334300=CARTESIAN_POINT('Ctrl Pts',(0.826559144999944,12.2,4.23594671199999));
#334301=CARTESIAN_POINT('Ctrl Pts',(0.826559144999944,5.2,4.23594671199999));
#334302=CARTESIAN_POINT('Ctrl Pts',(0.826559144999944,2.2,4.23594671199999));
#334303=CARTESIAN_POINT('Ctrl Pts',(0.826198215999944,12.2,4.23775816399999));
#334304=CARTESIAN_POINT('Ctrl Pts',(0.826198215999944,5.2,4.23775816399999));
#334305=CARTESIAN_POINT('Ctrl Pts',(0.826198215999944,2.2,4.23775816399999));
#334306=CARTESIAN_POINT('Ctrl Pts',(0.825834408999944,12.2,4.23957338099999));
#334307=CARTESIAN_POINT('Ctrl Pts',(0.825834408999944,5.2,4.23957338099999));
#334308=CARTESIAN_POINT('Ctrl Pts',(0.825834408999944,2.2,4.23957338099999));
#334309=CARTESIAN_POINT('Ctrl Pts',(0.825467717999944,12.2,4.24139235399998));
#334310=CARTESIAN_POINT('Ctrl Pts',(0.825467717999944,5.2,4.24139235399998));
#334311=CARTESIAN_POINT('Ctrl Pts',(0.825467717999944,2.2,4.24139235399998));
#334312=CARTESIAN_POINT('Ctrl Pts',(0.825098134999944,12.2,4.24321507299998));
#334313=CARTESIAN_POINT('Ctrl Pts',(0.825098134999944,5.2,4.24321507299998));
#334314=CARTESIAN_POINT('Ctrl Pts',(0.825098134999944,2.2,4.24321507299998));
#334315=CARTESIAN_POINT('Ctrl Pts',(0.824725651999944,12.2,4.24504152999998));
#334316=CARTESIAN_POINT('Ctrl Pts',(0.824725651999944,5.2,4.24504152999998));
#334317=CARTESIAN_POINT('Ctrl Pts',(0.824725651999944,2.2,4.24504152999998));
#334318=CARTESIAN_POINT('Ctrl Pts',(0.824350264999943,12.2,4.24687171399999));
#334319=CARTESIAN_POINT('Ctrl Pts',(0.824350264999943,5.2,4.24687171399999));
#334320=CARTESIAN_POINT('Ctrl Pts',(0.824350264999943,2.2,4.24687171399999));
#334321=CARTESIAN_POINT('Ctrl Pts',(0.823971964999944,12.2,4.24870561699999));
#334322=CARTESIAN_POINT('Ctrl Pts',(0.823971964999944,5.2,4.24870561699999));
#334323=CARTESIAN_POINT('Ctrl Pts',(0.823971964999944,2.2,4.24870561699999));
#334324=CARTESIAN_POINT('Ctrl Pts',(0.823590743999943,12.2,4.25054322999999));
#334325=CARTESIAN_POINT('Ctrl Pts',(0.823590743999943,5.2,4.25054322999999));
#334326=CARTESIAN_POINT('Ctrl Pts',(0.823590743999943,2.2,4.25054322999999));
#334327=CARTESIAN_POINT('Ctrl Pts',(0.823206597999944,12.2,4.25238454399998));
#334328=CARTESIAN_POINT('Ctrl Pts',(0.823206597999944,5.2,4.25238454399998));
#334329=CARTESIAN_POINT('Ctrl Pts',(0.823206597999944,2.2,4.25238454399998));
#334330=CARTESIAN_POINT('Ctrl Pts',(0.822819518999944,12.2,4.25422954999998));
#334331=CARTESIAN_POINT('Ctrl Pts',(0.822819518999944,5.2,4.25422954999998));
#334332=CARTESIAN_POINT('Ctrl Pts',(0.822819518999944,2.2,4.25422954999998));
#334333=CARTESIAN_POINT('Ctrl Pts',(0.822429499999945,12.2,4.25607823699998));
#334334=CARTESIAN_POINT('Ctrl Pts',(0.822429499999945,5.2,4.25607823699998));
#334335=CARTESIAN_POINT('Ctrl Pts',(0.822429499999945,2.2,4.25607823699998));
#334336=CARTESIAN_POINT('Ctrl Pts',(0.822036533999944,12.2,4.25793059899998));
#334337=CARTESIAN_POINT('Ctrl Pts',(0.822036533999944,5.2,4.25793059899998));
#334338=CARTESIAN_POINT('Ctrl Pts',(0.822036533999944,2.2,4.25793059899998));
#334339=CARTESIAN_POINT('Ctrl Pts',(0.821640614999944,12.2,4.25978662399999));
#334340=CARTESIAN_POINT('Ctrl Pts',(0.821640614999944,5.2,4.25978662399999));
#334341=CARTESIAN_POINT('Ctrl Pts',(0.821640614999944,2.2,4.25978662399999));
#334342=CARTESIAN_POINT('Ctrl Pts',(0.821241735999945,12.2,4.26164630399998));
#334343=CARTESIAN_POINT('Ctrl Pts',(0.821241735999945,5.2,4.26164630399998));
#334344=CARTESIAN_POINT('Ctrl Pts',(0.821241735999945,2.2,4.26164630399998));
#334345=CARTESIAN_POINT('Ctrl Pts',(0.820839888999945,12.2,4.26350963099999));
#334346=CARTESIAN_POINT('Ctrl Pts',(0.820839888999945,5.2,4.26350963099999));
#334347=CARTESIAN_POINT('Ctrl Pts',(0.820839888999945,2.2,4.26350963099999));
#334348=CARTESIAN_POINT('Ctrl Pts',(0.820435068999944,12.2,4.26537659399998));
#334349=CARTESIAN_POINT('Ctrl Pts',(0.820435068999944,5.2,4.26537659399998));
#334350=CARTESIAN_POINT('Ctrl Pts',(0.820435068999944,2.2,4.26537659399998));
#334351=CARTESIAN_POINT('Ctrl Pts',(0.820027268999944,12.2,4.26724718499998));
#334352=CARTESIAN_POINT('Ctrl Pts',(0.820027268999944,5.2,4.26724718499998));
#334353=CARTESIAN_POINT('Ctrl Pts',(0.820027268999944,2.2,4.26724718499998));
#334354=CARTESIAN_POINT('Ctrl Pts',(0.819616481999944,12.2,4.26912139399998));
#334355=CARTESIAN_POINT('Ctrl Pts',(0.819616481999944,5.2,4.26912139399998));
#334356=CARTESIAN_POINT('Ctrl Pts',(0.819616481999944,2.2,4.26912139399998));
#334357=CARTESIAN_POINT('Ctrl Pts',(0.819202701999945,12.2,4.27099921299998));
#334358=CARTESIAN_POINT('Ctrl Pts',(0.819202701999945,5.2,4.27099921299998));
#334359=CARTESIAN_POINT('Ctrl Pts',(0.819202701999945,2.2,4.27099921299998));
#334360=CARTESIAN_POINT('Ctrl Pts',(0.818785921999944,12.2,4.27288063199998));
#334361=CARTESIAN_POINT('Ctrl Pts',(0.818785921999944,5.2,4.27288063199998));
#334362=CARTESIAN_POINT('Ctrl Pts',(0.818785921999944,2.2,4.27288063199998));
#334363=CARTESIAN_POINT('Ctrl Pts',(0.818366133999944,12.2,4.27476564299998));
#334364=CARTESIAN_POINT('Ctrl Pts',(0.818366133999944,5.2,4.27476564299998));
#334365=CARTESIAN_POINT('Ctrl Pts',(0.818366133999944,2.2,4.27476564299998));
#334366=CARTESIAN_POINT('Ctrl Pts',(0.817943333999944,12.2,4.27665423699998));
#334367=CARTESIAN_POINT('Ctrl Pts',(0.817943333999944,5.2,4.27665423699998));
#334368=CARTESIAN_POINT('Ctrl Pts',(0.817943333999944,2.2,4.27665423699998));
#334369=CARTESIAN_POINT('Ctrl Pts',(0.817517513999944,12.2,4.27854640299999));
#334370=CARTESIAN_POINT('Ctrl Pts',(0.817517513999944,5.2,4.27854640299999));
#334371=CARTESIAN_POINT('Ctrl Pts',(0.817517513999944,2.2,4.27854640299999));
#334372=CARTESIAN_POINT('Ctrl Pts',(0.817088667999945,12.2,4.28044213499999));
#334373=CARTESIAN_POINT('Ctrl Pts',(0.817088667999945,5.2,4.28044213499999));
#334374=CARTESIAN_POINT('Ctrl Pts',(0.817088667999945,2.2,4.28044213499999));
#334375=CARTESIAN_POINT('Ctrl Pts',(0.816656787999944,12.2,4.28234141999998));
#334376=CARTESIAN_POINT('Ctrl Pts',(0.816656787999944,5.2,4.28234141999998));
#334377=CARTESIAN_POINT('Ctrl Pts',(0.816656787999944,2.2,4.28234141999998));
#334378=CARTESIAN_POINT('Ctrl Pts',(0.816221870999944,12.2,4.28424425199999));
#334379=CARTESIAN_POINT('Ctrl Pts',(0.816221870999944,5.2,4.28424425199999));
#334380=CARTESIAN_POINT('Ctrl Pts',(0.816221870999944,2.2,4.28424425199999));
#334381=CARTESIAN_POINT('Ctrl Pts',(0.815783906999944,12.2,4.28615062199999));
#334382=CARTESIAN_POINT('Ctrl Pts',(0.815783906999944,5.2,4.28615062199999));
#334383=CARTESIAN_POINT('Ctrl Pts',(0.815783906999944,2.2,4.28615062199999));
#334384=CARTESIAN_POINT('Ctrl Pts',(0.815342891999945,12.2,4.28806051899999));
#334385=CARTESIAN_POINT('Ctrl Pts',(0.815342891999945,5.2,4.28806051899999));
#334386=CARTESIAN_POINT('Ctrl Pts',(0.815342891999945,2.2,4.28806051899999));
#334387=CARTESIAN_POINT('Ctrl Pts',(0.814898817999944,12.2,4.28997393599998));
#334388=CARTESIAN_POINT('Ctrl Pts',(0.814898817999944,5.2,4.28997393599998));
#334389=CARTESIAN_POINT('Ctrl Pts',(0.814898817999944,2.2,4.28997393599998));
#334390=CARTESIAN_POINT('Ctrl Pts',(0.814451678999945,12.2,4.29189086099999));
#334391=CARTESIAN_POINT('Ctrl Pts',(0.814451678999945,5.2,4.29189086099999));
#334392=CARTESIAN_POINT('Ctrl Pts',(0.814451678999945,2.2,4.29189086099999));
#334393=CARTESIAN_POINT('Ctrl Pts',(0.814001469999944,12.2,4.29381128899998));
#334394=CARTESIAN_POINT('Ctrl Pts',(0.814001469999944,5.2,4.29381128899998));
#334395=CARTESIAN_POINT('Ctrl Pts',(0.814001469999944,2.2,4.29381128899998));
#334396=CARTESIAN_POINT('Ctrl Pts',(0.813548181999945,12.2,4.29573520799998));
#334397=CARTESIAN_POINT('Ctrl Pts',(0.813548181999945,5.2,4.29573520799998));
#334398=CARTESIAN_POINT('Ctrl Pts',(0.813548181999945,2.2,4.29573520799998));
#334399=CARTESIAN_POINT('Ctrl Pts',(0.813091811999944,12.2,4.29766260999998));
#334400=CARTESIAN_POINT('Ctrl Pts',(0.813091811999944,5.2,4.29766260999998));
#334401=CARTESIAN_POINT('Ctrl Pts',(0.813091811999944,2.2,4.29766260999998));
#334402=CARTESIAN_POINT('Ctrl Pts',(0.812632351999943,12.2,4.29959348699998));
#334403=CARTESIAN_POINT('Ctrl Pts',(0.812632351999943,5.2,4.29959348699998));
#334404=CARTESIAN_POINT('Ctrl Pts',(0.812632351999943,2.2,4.29959348699998));
#334405=CARTESIAN_POINT('Ctrl Pts',(0.812169794999944,12.2,4.30152782799999));
#334406=CARTESIAN_POINT('Ctrl Pts',(0.812169794999944,5.2,4.30152782799999));
#334407=CARTESIAN_POINT('Ctrl Pts',(0.812169794999944,2.2,4.30152782799999));
#334408=CARTESIAN_POINT('Ctrl Pts',(0.811704135999943,12.2,4.30346562599999));
#334409=CARTESIAN_POINT('Ctrl Pts',(0.811704135999943,5.2,4.30346562599999));
#334410=CARTESIAN_POINT('Ctrl Pts',(0.811704135999943,2.2,4.30346562599999));
#334411=CARTESIAN_POINT('Ctrl Pts',(0.811235367999944,12.2,4.30540686999999));
#334412=CARTESIAN_POINT('Ctrl Pts',(0.811235367999944,5.2,4.30540686999999));
#334413=CARTESIAN_POINT('Ctrl Pts',(0.811235367999944,2.2,4.30540686999999));
#334414=CARTESIAN_POINT('Ctrl Pts',(0.810763485999945,12.2,4.30735155199999));
#334415=CARTESIAN_POINT('Ctrl Pts',(0.810763485999945,5.2,4.30735155199999));
#334416=CARTESIAN_POINT('Ctrl Pts',(0.810763485999945,2.2,4.30735155199999));
#334417=CARTESIAN_POINT('Ctrl Pts',(0.810288482999945,12.2,4.30929966499999));
#334418=CARTESIAN_POINT('Ctrl Pts',(0.810288482999945,5.2,4.30929966499999));
#334419=CARTESIAN_POINT('Ctrl Pts',(0.810288482999945,2.2,4.30929966499999));
#334420=CARTESIAN_POINT('Ctrl Pts',(0.809810351999943,12.2,4.31125119599999));
#334421=CARTESIAN_POINT('Ctrl Pts',(0.809810351999943,5.2,4.31125119599999));
#334422=CARTESIAN_POINT('Ctrl Pts',(0.809810351999943,2.2,4.31125119599999));
#334423=CARTESIAN_POINT('Ctrl Pts',(0.809329088999945,12.2,4.31320613999999));
#334424=CARTESIAN_POINT('Ctrl Pts',(0.809329088999945,5.2,4.31320613999999));
#334425=CARTESIAN_POINT('Ctrl Pts',(0.809329088999945,2.2,4.31320613999999));
#334426=CARTESIAN_POINT('Ctrl Pts',(0.808844685999944,12.2,4.31516448499998));
#334427=CARTESIAN_POINT('Ctrl Pts',(0.808844685999944,5.2,4.31516448499998));
#334428=CARTESIAN_POINT('Ctrl Pts',(0.808844685999944,2.2,4.31516448499998));
#334429=CARTESIAN_POINT('Ctrl Pts',(0.808357137999944,12.2,4.31712622399999));
#334430=CARTESIAN_POINT('Ctrl Pts',(0.808357137999944,5.2,4.31712622399999));
#334431=CARTESIAN_POINT('Ctrl Pts',(0.808357137999944,2.2,4.31712622399999));
#334432=CARTESIAN_POINT('Ctrl Pts',(0.807866437999943,12.2,4.31909134599999));
#334433=CARTESIAN_POINT('Ctrl Pts',(0.807866437999943,5.2,4.31909134599999));
#334434=CARTESIAN_POINT('Ctrl Pts',(0.807866437999943,2.2,4.31909134599999));
#334435=CARTESIAN_POINT('Ctrl Pts',(0.807372581999944,12.2,4.32105984499999));
#334436=CARTESIAN_POINT('Ctrl Pts',(0.807372581999944,5.2,4.32105984499999));
#334437=CARTESIAN_POINT('Ctrl Pts',(0.807372581999944,2.2,4.32105984499999));
#334438=CARTESIAN_POINT('Ctrl Pts',(0.806875560999945,12.2,4.32303170999998));
#334439=CARTESIAN_POINT('Ctrl Pts',(0.806875560999945,5.2,4.32303170999998));
#334440=CARTESIAN_POINT('Ctrl Pts',(0.806875560999945,2.2,4.32303170999998));
#334441=CARTESIAN_POINT('Ctrl Pts',(0.806375370999944,12.2,4.32500693299998));
#334442=CARTESIAN_POINT('Ctrl Pts',(0.806375370999944,5.2,4.32500693299998));
#334443=CARTESIAN_POINT('Ctrl Pts',(0.806375370999944,2.2,4.32500693299998));
#334444=CARTESIAN_POINT('Ctrl Pts',(0.805872006999944,12.2,4.32698550299998));
#334445=CARTESIAN_POINT('Ctrl Pts',(0.805872006999944,5.2,4.32698550299998));
#334446=CARTESIAN_POINT('Ctrl Pts',(0.805872006999944,2.2,4.32698550299998));
#334447=CARTESIAN_POINT('Ctrl Pts',(0.805365458999944,12.2,4.32896741499999));
#334448=CARTESIAN_POINT('Ctrl Pts',(0.805365458999944,5.2,4.32896741499999));
#334449=CARTESIAN_POINT('Ctrl Pts',(0.805365458999944,2.2,4.32896741499999));
#334450=CARTESIAN_POINT('Ctrl Pts',(0.804855725999943,12.2,4.33095265599999));
#334451=CARTESIAN_POINT('Ctrl Pts',(0.804855725999943,5.2,4.33095265599999));
#334452=CARTESIAN_POINT('Ctrl Pts',(0.804855725999943,2.2,4.33095265599999));
#334453=CARTESIAN_POINT('Ctrl Pts',(0.804342799999944,12.2,4.33294121999998));
#334454=CARTESIAN_POINT('Ctrl Pts',(0.804342799999944,5.2,4.33294121999998));
#334455=CARTESIAN_POINT('Ctrl Pts',(0.804342799999944,2.2,4.33294121999998));
#334456=CARTESIAN_POINT('Ctrl Pts',(0.803826673999944,12.2,4.33493309799999));
#334457=CARTESIAN_POINT('Ctrl Pts',(0.803826673999944,5.2,4.33493309799999));
#334458=CARTESIAN_POINT('Ctrl Pts',(0.803826673999944,2.2,4.33493309799999));
#334459=CARTESIAN_POINT('Ctrl Pts',(0.803307342999945,12.2,4.33692827799998));
#334460=CARTESIAN_POINT('Ctrl Pts',(0.803307342999945,5.2,4.33692827799998));
#334461=CARTESIAN_POINT('Ctrl Pts',(0.803307342999945,2.2,4.33692827799998));
#334462=CARTESIAN_POINT('Ctrl Pts',(0.802784801999944,12.2,4.33892675499998));
#334463=CARTESIAN_POINT('Ctrl Pts',(0.802784801999944,5.2,4.33892675499998));
#334464=CARTESIAN_POINT('Ctrl Pts',(0.802784801999944,2.2,4.33892675499998));
#334465=CARTESIAN_POINT('Ctrl Pts',(0.802259043999943,12.2,4.34092851799999));
#334466=CARTESIAN_POINT('Ctrl Pts',(0.802259043999943,5.2,4.34092851799999));
#334467=CARTESIAN_POINT('Ctrl Pts',(0.802259043999943,2.2,4.34092851799999));
#334468=CARTESIAN_POINT('Ctrl Pts',(0.801730063999945,12.2,4.34293355899998));
#334469=CARTESIAN_POINT('Ctrl Pts',(0.801730063999945,5.2,4.34293355899998));
#334470=CARTESIAN_POINT('Ctrl Pts',(0.801730063999945,2.2,4.34293355899998));
#334471=CARTESIAN_POINT('Ctrl Pts',(0.801197855999944,12.2,4.34494186799999));
#334472=CARTESIAN_POINT('Ctrl Pts',(0.801197855999944,5.2,4.34494186799999));
#334473=CARTESIAN_POINT('Ctrl Pts',(0.801197855999944,2.2,4.34494186799999));
#334474=CARTESIAN_POINT('Ctrl Pts',(0.800662413999944,12.2,4.34695343699998));
#334475=CARTESIAN_POINT('Ctrl Pts',(0.800662413999944,5.2,4.34695343699998));
#334476=CARTESIAN_POINT('Ctrl Pts',(0.800662413999944,2.2,4.34695343699998));
#334477=CARTESIAN_POINT('Ctrl Pts',(0.800123732999943,12.2,4.34896825699998));
#334478=CARTESIAN_POINT('Ctrl Pts',(0.800123732999943,5.2,4.34896825699998));
#334479=CARTESIAN_POINT('Ctrl Pts',(0.800123732999943,2.2,4.34896825699998));
#334480=CARTESIAN_POINT('Ctrl Pts',(0.799581806999944,12.2,4.35098631899999));
#334481=CARTESIAN_POINT('Ctrl Pts',(0.799581806999944,5.2,4.35098631899999));
#334482=CARTESIAN_POINT('Ctrl Pts',(0.799581806999944,2.2,4.35098631899999));
#334483=CARTESIAN_POINT('Ctrl Pts',(0.799036627999944,12.2,4.35300761599999));
#334484=CARTESIAN_POINT('Ctrl Pts',(0.799036627999944,5.2,4.35300761599999));
#334485=CARTESIAN_POINT('Ctrl Pts',(0.799036627999944,2.2,4.35300761599999));
#334486=CARTESIAN_POINT('Ctrl Pts',(0.798488193999944,12.2,4.35503213599999));
#334487=CARTESIAN_POINT('Ctrl Pts',(0.798488193999944,5.2,4.35503213599999));
#334488=CARTESIAN_POINT('Ctrl Pts',(0.798488193999944,2.2,4.35503213599999));
#334489=CARTESIAN_POINT('Ctrl Pts',(0.797936496999945,12.2,4.35705987099999));
#334490=CARTESIAN_POINT('Ctrl Pts',(0.797936496999945,5.2,4.35705987099999));
#334491=CARTESIAN_POINT('Ctrl Pts',(0.797936496999945,2.2,4.35705987099999));
#334492=CARTESIAN_POINT('Ctrl Pts',(0.797381532999945,12.2,4.35909081499998));
#334493=CARTESIAN_POINT('Ctrl Pts',(0.797381532999945,5.2,4.35909081499998));
#334494=CARTESIAN_POINT('Ctrl Pts',(0.797381532999945,2.2,4.35909081499998));
#334495=CARTESIAN_POINT('Ctrl Pts',(0.796823294999944,12.2,4.36112495599998));
#334496=CARTESIAN_POINT('Ctrl Pts',(0.796823294999944,5.2,4.36112495599998));
#334497=CARTESIAN_POINT('Ctrl Pts',(0.796823294999944,2.2,4.36112495599998));
#334498=CARTESIAN_POINT('Ctrl Pts',(0.796261777999944,12.2,4.36316228499999));
#334499=CARTESIAN_POINT('Ctrl Pts',(0.796261777999944,5.2,4.36316228499999));
#334500=CARTESIAN_POINT('Ctrl Pts',(0.796261777999944,2.2,4.36316228499999));
#334501=CARTESIAN_POINT('Ctrl Pts',(0.795696975999944,12.2,4.36520279599999));
#334502=CARTESIAN_POINT('Ctrl Pts',(0.795696975999944,5.2,4.36520279599999));
#334503=CARTESIAN_POINT('Ctrl Pts',(0.795696975999944,2.2,4.36520279599999));
#334504=CARTESIAN_POINT('Ctrl Pts',(0.795128884999944,12.2,4.36724647799998));
#334505=CARTESIAN_POINT('Ctrl Pts',(0.795128884999944,5.2,4.36724647799998));
#334506=CARTESIAN_POINT('Ctrl Pts',(0.795128884999944,2.2,4.36724647799998));
#334507=CARTESIAN_POINT('Ctrl Pts',(0.794557497999944,12.2,4.36929332299999));
#334508=CARTESIAN_POINT('Ctrl Pts',(0.794557497999944,5.2,4.36929332299999));
#334509=CARTESIAN_POINT('Ctrl Pts',(0.794557497999944,2.2,4.36929332299999));
#334510=CARTESIAN_POINT('Ctrl Pts',(0.793982808999945,12.2,4.37134332199999));
#334511=CARTESIAN_POINT('Ctrl Pts',(0.793982808999945,5.2,4.37134332199999));
#334512=CARTESIAN_POINT('Ctrl Pts',(0.793982808999945,2.2,4.37134332199999));
#334513=CARTESIAN_POINT('Ctrl Pts',(0.793404813999944,12.2,4.37339646599998));
#334514=CARTESIAN_POINT('Ctrl Pts',(0.793404813999944,5.2,4.37339646599998));
#334515=CARTESIAN_POINT('Ctrl Pts',(0.793404813999944,2.2,4.37339646599998));
#334516=CARTESIAN_POINT('Ctrl Pts',(0.792823505999943,12.2,4.37545274699998));
#334517=CARTESIAN_POINT('Ctrl Pts',(0.792823505999943,5.2,4.37545274699998));
#334518=CARTESIAN_POINT('Ctrl Pts',(0.792823505999943,2.2,4.37545274699998));
#334519=CARTESIAN_POINT('Ctrl Pts',(0.792238880999945,12.2,4.37751215499999));
#334520=CARTESIAN_POINT('Ctrl Pts',(0.792238880999945,5.2,4.37751215499999));
#334521=CARTESIAN_POINT('Ctrl Pts',(0.792238880999945,2.2,4.37751215499999));
#334522=CARTESIAN_POINT('Ctrl Pts',(0.791650932999944,12.2,4.37957468199999));
#334523=CARTESIAN_POINT('Ctrl Pts',(0.791650932999944,5.2,4.37957468199999));
#334524=CARTESIAN_POINT('Ctrl Pts',(0.791650932999944,2.2,4.37957468199999));
#334525=CARTESIAN_POINT('Ctrl Pts',(0.791059655999944,12.2,4.38164031999998));
#334526=CARTESIAN_POINT('Ctrl Pts',(0.791059655999944,5.2,4.38164031999998));
#334527=CARTESIAN_POINT('Ctrl Pts',(0.791059655999944,2.2,4.38164031999998));
#334528=CARTESIAN_POINT('Ctrl Pts',(0.790465045999944,12.2,4.38370905999999));
#334529=CARTESIAN_POINT('Ctrl Pts',(0.790465045999944,5.2,4.38370905999999));
#334530=CARTESIAN_POINT('Ctrl Pts',(0.790465045999944,2.2,4.38370905999999));
#334531=CARTESIAN_POINT('Ctrl Pts',(0.789867097999944,12.2,4.38578089099998));
#334532=CARTESIAN_POINT('Ctrl Pts',(0.789867097999944,5.2,4.38578089099998));
#334533=CARTESIAN_POINT('Ctrl Pts',(0.789867097999944,2.2,4.38578089099998));
#334534=CARTESIAN_POINT('Ctrl Pts',(0.789265802999944,12.2,4.38785580699999));
#334535=CARTESIAN_POINT('Ctrl Pts',(0.789265802999944,5.2,4.38785580699999));
#334536=CARTESIAN_POINT('Ctrl Pts',(0.789265802999944,2.2,4.38785580699999));
#334537=CARTESIAN_POINT('Ctrl Pts',(0.788661159999945,12.2,4.38993379799999));
#334538=CARTESIAN_POINT('Ctrl Pts',(0.788661159999945,5.2,4.38993379799999));
#334539=CARTESIAN_POINT('Ctrl Pts',(0.788661159999945,2.2,4.38993379799999));
#334540=CARTESIAN_POINT('Ctrl Pts',(0.788053160999944,12.2,4.39201485499999));
#334541=CARTESIAN_POINT('Ctrl Pts',(0.788053160999944,5.2,4.39201485499999));
#334542=CARTESIAN_POINT('Ctrl Pts',(0.788053160999944,2.2,4.39201485499999));
#334543=CARTESIAN_POINT('Ctrl Pts',(0.787441801999944,12.2,4.39409896999998));
#334544=CARTESIAN_POINT('Ctrl Pts',(0.787441801999944,5.2,4.39409896999998));
#334545=CARTESIAN_POINT('Ctrl Pts',(0.787441801999944,2.2,4.39409896999998));
#334546=CARTESIAN_POINT('Ctrl Pts',(0.786827076999944,12.2,4.39618613399999));
#334547=CARTESIAN_POINT('Ctrl Pts',(0.786827076999944,5.2,4.39618613399999));
#334548=CARTESIAN_POINT('Ctrl Pts',(0.786827076999944,2.2,4.39618613399999));
#334549=CARTESIAN_POINT('Ctrl Pts',(0.786208980999944,12.2,4.39827633899998));
#334550=CARTESIAN_POINT('Ctrl Pts',(0.786208980999944,5.2,4.39827633899998));
#334551=CARTESIAN_POINT('Ctrl Pts',(0.786208980999944,2.2,4.39827633899998));
#334552=CARTESIAN_POINT('Ctrl Pts',(0.785587508999944,12.2,4.40036957499998));
#334553=CARTESIAN_POINT('Ctrl Pts',(0.785587508999944,5.2,4.40036957499998));
#334554=CARTESIAN_POINT('Ctrl Pts',(0.785587508999944,2.2,4.40036957499998));
#334555=CARTESIAN_POINT('Ctrl Pts',(0.784962655999945,12.2,4.40246583399999));
#334556=CARTESIAN_POINT('Ctrl Pts',(0.784962655999945,5.2,4.40246583399999));
#334557=CARTESIAN_POINT('Ctrl Pts',(0.784962655999945,2.2,4.40246583399999));
#334558=CARTESIAN_POINT('Ctrl Pts',(0.784334416999944,12.2,4.40456510699998));
#334559=CARTESIAN_POINT('Ctrl Pts',(0.784334416999944,5.2,4.40456510699998));
#334560=CARTESIAN_POINT('Ctrl Pts',(0.784334416999944,2.2,4.40456510699998));
#334561=CARTESIAN_POINT('Ctrl Pts',(0.783702784999945,12.2,4.40666738599998));
#334562=CARTESIAN_POINT('Ctrl Pts',(0.783702784999945,5.2,4.40666738599998));
#334563=CARTESIAN_POINT('Ctrl Pts',(0.783702784999945,2.2,4.40666738599998));
#334564=CARTESIAN_POINT('Ctrl Pts',(0.783067756999943,12.2,4.40877266199998));
#334565=CARTESIAN_POINT('Ctrl Pts',(0.783067756999943,5.2,4.40877266199998));
#334566=CARTESIAN_POINT('Ctrl Pts',(0.783067756999943,2.2,4.40877266199998));
#334567=CARTESIAN_POINT('Ctrl Pts',(0.782429326999944,12.2,4.41088092599998));
#334568=CARTESIAN_POINT('Ctrl Pts',(0.782429326999944,5.2,4.41088092599998));
#334569=CARTESIAN_POINT('Ctrl Pts',(0.782429326999944,2.2,4.41088092599998));
#334570=CARTESIAN_POINT('Ctrl Pts',(0.781787488999944,12.2,4.41299216899999));
#334571=CARTESIAN_POINT('Ctrl Pts',(0.781787488999944,5.2,4.41299216899999));
#334572=CARTESIAN_POINT('Ctrl Pts',(0.781787488999944,2.2,4.41299216899999));
#334573=CARTESIAN_POINT('Ctrl Pts',(0.781142240999944,12.2,4.41510638199999));
#334574=CARTESIAN_POINT('Ctrl Pts',(0.781142240999944,5.2,4.41510638199999));
#334575=CARTESIAN_POINT('Ctrl Pts',(0.781142240999944,2.2,4.41510638199999));
#334576=CARTESIAN_POINT('Ctrl Pts',(0.780493573999944,12.2,4.41722355899999));
#334577=CARTESIAN_POINT('Ctrl Pts',(0.780493573999944,5.2,4.41722355899999));
#334578=CARTESIAN_POINT('Ctrl Pts',(0.780493573999944,2.2,4.41722355899999));
#334579=CARTESIAN_POINT('Ctrl Pts',(0.779841484999944,12.2,4.41934368899998));
#334580=CARTESIAN_POINT('Ctrl Pts',(0.779841484999944,5.2,4.41934368899998));
#334581=CARTESIAN_POINT('Ctrl Pts',(0.779841484999944,2.2,4.41934368899998));
#334582=CARTESIAN_POINT('Ctrl Pts',(0.779185969999945,12.2,4.42146676299998));
#334583=CARTESIAN_POINT('Ctrl Pts',(0.779185969999945,5.2,4.42146676299998));
#334584=CARTESIAN_POINT('Ctrl Pts',(0.779185969999945,2.2,4.42146676299998));
#334585=CARTESIAN_POINT('Ctrl Pts',(0.778527020999944,12.2,4.42359277399999));
#334586=CARTESIAN_POINT('Ctrl Pts',(0.778527020999944,5.2,4.42359277399999));
#334587=CARTESIAN_POINT('Ctrl Pts',(0.778527020999944,2.2,4.42359277399999));
#334588=CARTESIAN_POINT('Ctrl Pts',(0.777864634999944,12.2,4.42572171199998));
#334589=CARTESIAN_POINT('Ctrl Pts',(0.777864634999944,5.2,4.42572171199998));
#334590=CARTESIAN_POINT('Ctrl Pts',(0.777864634999944,2.2,4.42572171199998));
#334591=CARTESIAN_POINT('Ctrl Pts',(0.777198807999944,12.2,4.42785356899999));
#334592=CARTESIAN_POINT('Ctrl Pts',(0.777198807999944,5.2,4.42785356899999));
#334593=CARTESIAN_POINT('Ctrl Pts',(0.777198807999944,2.2,4.42785356899999));
#334594=CARTESIAN_POINT('Ctrl Pts',(0.776529531999944,12.2,4.42998833699999));
#334595=CARTESIAN_POINT('Ctrl Pts',(0.776529531999944,5.2,4.42998833699999));
#334596=CARTESIAN_POINT('Ctrl Pts',(0.776529531999944,2.2,4.42998833699999));
#334597=CARTESIAN_POINT('Ctrl Pts',(0.775856804999945,12.2,4.43212600599999));
#334598=CARTESIAN_POINT('Ctrl Pts',(0.775856804999945,5.2,4.43212600599999));
#334599=CARTESIAN_POINT('Ctrl Pts',(0.775856804999945,2.2,4.43212600599999));
#334600=CARTESIAN_POINT('Ctrl Pts',(0.775180620999943,12.2,4.43426656799998));
#334601=CARTESIAN_POINT('Ctrl Pts',(0.775180620999943,5.2,4.43426656799998));
#334602=CARTESIAN_POINT('Ctrl Pts',(0.775180620999943,2.2,4.43426656799998));
#334603=CARTESIAN_POINT('Ctrl Pts',(0.774500973999944,12.2,4.43641001499999));
#334604=CARTESIAN_POINT('Ctrl Pts',(0.774500973999944,5.2,4.43641001499999));
#334605=CARTESIAN_POINT('Ctrl Pts',(0.774500973999944,2.2,4.43641001499999));
#334606=CARTESIAN_POINT('Ctrl Pts',(0.773817860999944,12.2,4.43855633799998));
#334607=CARTESIAN_POINT('Ctrl Pts',(0.773817860999944,5.2,4.43855633799998));
#334608=CARTESIAN_POINT('Ctrl Pts',(0.773817860999944,2.2,4.43855633799998));
#334609=CARTESIAN_POINT('Ctrl Pts',(0.773131275999944,12.2,4.44070552699999));
#334610=CARTESIAN_POINT('Ctrl Pts',(0.773131275999944,5.2,4.44070552699999));
#334611=CARTESIAN_POINT('Ctrl Pts',(0.773131275999944,2.2,4.44070552699999));
#334612=CARTESIAN_POINT('Ctrl Pts',(0.772441214999944,12.2,4.44285757499999));
#334613=CARTESIAN_POINT('Ctrl Pts',(0.772441214999944,5.2,4.44285757499999));
#334614=CARTESIAN_POINT('Ctrl Pts',(0.772441214999944,2.2,4.44285757499999));
#334615=CARTESIAN_POINT('Ctrl Pts',(0.771747671999944,12.2,4.44501247299999));
#334616=CARTESIAN_POINT('Ctrl Pts',(0.771747671999944,5.2,4.44501247299999));
#334617=CARTESIAN_POINT('Ctrl Pts',(0.771747671999944,2.2,4.44501247299999));
#334618=CARTESIAN_POINT('Ctrl Pts',(0.771050642999944,12.2,4.44717021199998));
#334619=CARTESIAN_POINT('Ctrl Pts',(0.771050642999944,5.2,4.44717021199998));
#334620=CARTESIAN_POINT('Ctrl Pts',(0.771050642999944,2.2,4.44717021199998));
#334621=CARTESIAN_POINT('Ctrl Pts',(0.770350122999944,12.2,4.44933078499999));
#334622=CARTESIAN_POINT('Ctrl Pts',(0.770350122999944,5.2,4.44933078499999));
#334623=CARTESIAN_POINT('Ctrl Pts',(0.770350122999944,2.2,4.44933078499999));
#334624=CARTESIAN_POINT('Ctrl Pts',(0.769646107999944,12.2,4.45149418099999));
#334625=CARTESIAN_POINT('Ctrl Pts',(0.769646107999944,5.2,4.45149418099999));
#334626=CARTESIAN_POINT('Ctrl Pts',(0.769646107999944,2.2,4.45149418099999));
#334627=CARTESIAN_POINT('Ctrl Pts',(0.768938590999944,12.2,4.45366039399998));
#334628=CARTESIAN_POINT('Ctrl Pts',(0.768938590999944,5.2,4.45366039399998));
#334629=CARTESIAN_POINT('Ctrl Pts',(0.768938590999944,2.2,4.45366039399998));
#334630=CARTESIAN_POINT('Ctrl Pts',(0.768227569999944,12.2,4.45582941299998));
#334631=CARTESIAN_POINT('Ctrl Pts',(0.768227569999944,5.2,4.45582941299998));
#334632=CARTESIAN_POINT('Ctrl Pts',(0.768227569999944,2.2,4.45582941299998));
#334633=CARTESIAN_POINT('Ctrl Pts',(0.767513038999944,12.2,4.45800123099998));
#334634=CARTESIAN_POINT('Ctrl Pts',(0.767513038999944,5.2,4.45800123099998));
#334635=CARTESIAN_POINT('Ctrl Pts',(0.767513038999944,2.2,4.45800123099998));
#334636=CARTESIAN_POINT('Ctrl Pts',(0.766794991999945,12.2,4.46017583899998));
#334637=CARTESIAN_POINT('Ctrl Pts',(0.766794991999945,5.2,4.46017583899998));
#334638=CARTESIAN_POINT('Ctrl Pts',(0.766794991999945,2.2,4.46017583899998));
#334639=CARTESIAN_POINT('Ctrl Pts',(0.766073427999945,12.2,4.46235322799998));
#334640=CARTESIAN_POINT('Ctrl Pts',(0.766073427999945,5.2,4.46235322799998));
#334641=CARTESIAN_POINT('Ctrl Pts',(0.766073427999945,2.2,4.46235322799998));
#334642=CARTESIAN_POINT('Ctrl Pts',(0.765348338999944,12.2,4.46453339099998));
#334643=CARTESIAN_POINT('Ctrl Pts',(0.765348338999944,5.2,4.46453339099998));
#334644=CARTESIAN_POINT('Ctrl Pts',(0.765348338999944,2.2,4.46453339099998));
#334645=CARTESIAN_POINT('Ctrl Pts',(0.764619720999944,12.2,4.46671631799998));
#334646=CARTESIAN_POINT('Ctrl Pts',(0.764619720999944,5.2,4.46671631799998));
#334647=CARTESIAN_POINT('Ctrl Pts',(0.764619720999944,2.2,4.46671631799998));
#334648=CARTESIAN_POINT('Ctrl Pts',(0.763887570999944,12.2,4.46890199999999));
#334649=CARTESIAN_POINT('Ctrl Pts',(0.763887570999944,5.2,4.46890199999999));
#334650=CARTESIAN_POINT('Ctrl Pts',(0.763887570999944,2.2,4.46890199999999));
#334651=CARTESIAN_POINT('Ctrl Pts',(0.763151880999944,12.2,4.47109042999998));
#334652=CARTESIAN_POINT('Ctrl Pts',(0.763151880999944,5.2,4.47109042999998));
#334653=CARTESIAN_POINT('Ctrl Pts',(0.763151880999944,2.2,4.47109042999998));
#334654=CARTESIAN_POINT('Ctrl Pts',(0.762412649999944,12.2,4.47328159899998));
#334655=CARTESIAN_POINT('Ctrl Pts',(0.762412649999944,5.2,4.47328159899998));
#334656=CARTESIAN_POINT('Ctrl Pts',(0.762412649999944,2.2,4.47328159899998));
#334657=CARTESIAN_POINT('Ctrl Pts',(0.761669871999944,12.2,4.47547549799998));
#334658=CARTESIAN_POINT('Ctrl Pts',(0.761669871999944,5.2,4.47547549799998));
#334659=CARTESIAN_POINT('Ctrl Pts',(0.761669871999944,2.2,4.47547549799998));
#334660=CARTESIAN_POINT('Ctrl Pts',(0.760923542999944,12.2,4.47767211899999));
#334661=CARTESIAN_POINT('Ctrl Pts',(0.760923542999944,5.2,4.47767211899999));
#334662=CARTESIAN_POINT('Ctrl Pts',(0.760923542999944,2.2,4.47767211899999));
#334663=CARTESIAN_POINT('Ctrl Pts',(0.760173656999944,12.2,4.47987145299999));
#334664=CARTESIAN_POINT('Ctrl Pts',(0.760173656999944,5.2,4.47987145299999));
#334665=CARTESIAN_POINT('Ctrl Pts',(0.760173656999944,2.2,4.47987145299999));
#334666=CARTESIAN_POINT('Ctrl Pts',(0.759420210999945,12.2,4.48207349099999));
#334667=CARTESIAN_POINT('Ctrl Pts',(0.759420210999945,5.2,4.48207349099999));
#334668=CARTESIAN_POINT('Ctrl Pts',(0.759420210999945,2.2,4.48207349099999));
#334669=CARTESIAN_POINT('Ctrl Pts',(0.758663198999944,12.2,4.48427822699998));
#334670=CARTESIAN_POINT('Ctrl Pts',(0.758663198999944,5.2,4.48427822699998));
#334671=CARTESIAN_POINT('Ctrl Pts',(0.758663198999944,2.2,4.48427822699998));
#334672=CARTESIAN_POINT('Ctrl Pts',(0.757902617999945,12.2,4.48648564999999));
#334673=CARTESIAN_POINT('Ctrl Pts',(0.757902617999945,5.2,4.48648564999999));
#334674=CARTESIAN_POINT('Ctrl Pts',(0.757902617999945,2.2,4.48648564999999));
#334675=CARTESIAN_POINT('Ctrl Pts',(0.757138463999943,12.2,4.48869575199998));
#334676=CARTESIAN_POINT('Ctrl Pts',(0.757138463999943,5.2,4.48869575199998));
#334677=CARTESIAN_POINT('Ctrl Pts',(0.757138463999943,2.2,4.48869575199998));
#334678=CARTESIAN_POINT('Ctrl Pts',(0.756370729999943,12.2,4.49090852399999));
#334679=CARTESIAN_POINT('Ctrl Pts',(0.756370729999943,5.2,4.49090852399999));
#334680=CARTESIAN_POINT('Ctrl Pts',(0.756370729999943,2.2,4.49090852399999));
#334681=CARTESIAN_POINT('Ctrl Pts',(0.755599414999945,12.2,4.49312395999999));
#334682=CARTESIAN_POINT('Ctrl Pts',(0.755599414999945,5.2,4.49312395999999));
#334683=CARTESIAN_POINT('Ctrl Pts',(0.755599414999945,2.2,4.49312395999999));
#334684=CARTESIAN_POINT('Ctrl Pts',(0.754824510999944,12.2,4.49534204999999));
#334685=CARTESIAN_POINT('Ctrl Pts',(0.754824510999944,5.2,4.49534204999999));
#334686=CARTESIAN_POINT('Ctrl Pts',(0.754824510999944,2.2,4.49534204999999));
#334687=CARTESIAN_POINT('Ctrl Pts',(0.754046015999944,12.2,4.49756278299999));
#334688=CARTESIAN_POINT('Ctrl Pts',(0.754046015999944,5.2,4.49756278299999));
#334689=CARTESIAN_POINT('Ctrl Pts',(0.754046015999944,2.2,4.49756278299999));
#334690=CARTESIAN_POINT('Ctrl Pts',(0.753263923999944,12.2,4.49978615499998));
#334691=CARTESIAN_POINT('Ctrl Pts',(0.753263923999944,5.2,4.49978615499998));
#334692=CARTESIAN_POINT('Ctrl Pts',(0.753263923999944,2.2,4.49978615499998));
#334693=CARTESIAN_POINT('Ctrl Pts',(0.752478233999944,12.2,4.50201215499998));
#334694=CARTESIAN_POINT('Ctrl Pts',(0.752478233999944,5.2,4.50201215499998));
#334695=CARTESIAN_POINT('Ctrl Pts',(0.752478233999944,2.2,4.50201215499998));
#334696=CARTESIAN_POINT('Ctrl Pts',(0.751688936999945,12.2,4.50424077499999));
#334697=CARTESIAN_POINT('Ctrl Pts',(0.751688936999945,5.2,4.50424077499999));
#334698=CARTESIAN_POINT('Ctrl Pts',(0.751688936999945,2.2,4.50424077499999));
#334699=CARTESIAN_POINT('Ctrl Pts',(0.750896031999945,12.2,4.50647200599998));
#334700=CARTESIAN_POINT('Ctrl Pts',(0.750896031999945,5.2,4.50647200599998));
#334701=CARTESIAN_POINT('Ctrl Pts',(0.750896031999945,2.2,4.50647200599998));
#334702=CARTESIAN_POINT('Ctrl Pts',(0.750099512999944,12.2,4.50870584099999));
#334703=CARTESIAN_POINT('Ctrl Pts',(0.750099512999944,5.2,4.50870584099999));
#334704=CARTESIAN_POINT('Ctrl Pts',(0.750099512999944,2.2,4.50870584099999));
#334705=CARTESIAN_POINT('Ctrl Pts',(0.749299376999945,12.2,4.51094227099999));
#334706=CARTESIAN_POINT('Ctrl Pts',(0.749299376999945,5.2,4.51094227099999));
#334707=CARTESIAN_POINT('Ctrl Pts',(0.749299376999945,2.2,4.51094227099999));
#334708=CARTESIAN_POINT('Ctrl Pts',(0.748495618999944,12.2,4.51318128699998));
#334709=CARTESIAN_POINT('Ctrl Pts',(0.748495618999944,5.2,4.51318128699998));
#334710=CARTESIAN_POINT('Ctrl Pts',(0.748495618999944,2.2,4.51318128699998));
#334711=CARTESIAN_POINT('Ctrl Pts',(0.747688233999945,12.2,4.51542287999998));
#334712=CARTESIAN_POINT('Ctrl Pts',(0.747688233999945,5.2,4.51542287999998));
#334713=CARTESIAN_POINT('Ctrl Pts',(0.747688233999945,2.2,4.51542287999998));
#334714=CARTESIAN_POINT('Ctrl Pts',(0.746877218999944,12.2,4.51766704299998));
#334715=CARTESIAN_POINT('Ctrl Pts',(0.746877218999944,5.2,4.51766704299998));
#334716=CARTESIAN_POINT('Ctrl Pts',(0.746877218999944,2.2,4.51766704299998));
#334717=CARTESIAN_POINT('Ctrl Pts',(0.746062569999945,12.2,4.51991376699999));
#334718=CARTESIAN_POINT('Ctrl Pts',(0.746062569999945,5.2,4.51991376699999));
#334719=CARTESIAN_POINT('Ctrl Pts',(0.746062569999945,2.2,4.51991376699999));
#334720=CARTESIAN_POINT('Ctrl Pts',(0.745244281999944,12.2,4.52216304399998));
#334721=CARTESIAN_POINT('Ctrl Pts',(0.745244281999944,5.2,4.52216304399998));
#334722=CARTESIAN_POINT('Ctrl Pts',(0.745244281999944,2.2,4.52216304399998));
#334723=CARTESIAN_POINT('Ctrl Pts',(0.744422349999944,12.2,4.52441486499998));
#334724=CARTESIAN_POINT('Ctrl Pts',(0.744422349999944,5.2,4.52441486499998));
#334725=CARTESIAN_POINT('Ctrl Pts',(0.744422349999944,2.2,4.52441486499998));
#334726=CARTESIAN_POINT('Ctrl Pts',(0.743596771999945,12.2,4.52666922199998));
#334727=CARTESIAN_POINT('Ctrl Pts',(0.743596771999945,5.2,4.52666922199998));
#334728=CARTESIAN_POINT('Ctrl Pts',(0.743596771999945,2.2,4.52666922199998));
#334729=CARTESIAN_POINT('Ctrl Pts',(0.742767542999945,12.2,4.52892610699998));
#334730=CARTESIAN_POINT('Ctrl Pts',(0.742767542999945,5.2,4.52892610699998));
#334731=CARTESIAN_POINT('Ctrl Pts',(0.742767542999945,2.2,4.52892610699998));
#334732=CARTESIAN_POINT('Ctrl Pts',(0.741934656999944,12.2,4.53118550999999));
#334733=CARTESIAN_POINT('Ctrl Pts',(0.741934656999944,5.2,4.53118550999999));
#334734=CARTESIAN_POINT('Ctrl Pts',(0.741934656999944,2.2,4.53118550999999));
#334735=CARTESIAN_POINT('Ctrl Pts',(0.741098112999944,12.2,4.53344742499999));
#334736=CARTESIAN_POINT('Ctrl Pts',(0.741098112999944,5.2,4.53344742499999));
#334737=CARTESIAN_POINT('Ctrl Pts',(0.741098112999944,2.2,4.53344742499999));
#334738=CARTESIAN_POINT('Ctrl Pts',(0.740257903999945,12.2,4.53571184099999));
#334739=CARTESIAN_POINT('Ctrl Pts',(0.740257903999945,5.2,4.53571184099999));
#334740=CARTESIAN_POINT('Ctrl Pts',(0.740257903999945,2.2,4.53571184099999));
#334741=CARTESIAN_POINT('Ctrl Pts',(0.739414027999944,12.2,4.53797875199999));
#334742=CARTESIAN_POINT('Ctrl Pts',(0.739414027999944,5.2,4.53797875199999));
#334743=CARTESIAN_POINT('Ctrl Pts',(0.739414027999944,2.2,4.53797875199999));
#334744=CARTESIAN_POINT('Ctrl Pts',(0.738566478999945,12.2,4.54024814799999));
#334745=CARTESIAN_POINT('Ctrl Pts',(0.738566478999945,5.2,4.54024814799999));
#334746=CARTESIAN_POINT('Ctrl Pts',(0.738566478999945,2.2,4.54024814799999));
#334747=CARTESIAN_POINT('Ctrl Pts',(0.737715255999943,12.2,4.54252002199999));
#334748=CARTESIAN_POINT('Ctrl Pts',(0.737715255999943,5.2,4.54252002199999));
#334749=CARTESIAN_POINT('Ctrl Pts',(0.737715255999943,2.2,4.54252002199999));
#334750=CARTESIAN_POINT('Ctrl Pts',(0.736860351999944,12.2,4.54479436399998));
#334751=CARTESIAN_POINT('Ctrl Pts',(0.736860351999944,5.2,4.54479436399998));
#334752=CARTESIAN_POINT('Ctrl Pts',(0.736860351999944,2.2,4.54479436399998));
#334753=CARTESIAN_POINT('Ctrl Pts',(0.736001763999944,12.2,4.54707116699999));
#334754=CARTESIAN_POINT('Ctrl Pts',(0.736001763999944,5.2,4.54707116699999));
#334755=CARTESIAN_POINT('Ctrl Pts',(0.736001763999944,2.2,4.54707116699999));
#334756=CARTESIAN_POINT('Ctrl Pts',(0.735139488999944,12.2,4.54935042199998));
#334757=CARTESIAN_POINT('Ctrl Pts',(0.735139488999944,5.2,4.54935042199998));
#334758=CARTESIAN_POINT('Ctrl Pts',(0.735139488999944,2.2,4.54935042199998));
#334759=CARTESIAN_POINT('Ctrl Pts',(0.734273520999944,12.2,4.55163212099999));
#334760=CARTESIAN_POINT('Ctrl Pts',(0.734273520999944,5.2,4.55163212099999));
#334761=CARTESIAN_POINT('Ctrl Pts',(0.734273520999944,2.2,4.55163212099999));
#334762=CARTESIAN_POINT('Ctrl Pts',(0.733403857999945,12.2,4.55391625599999));
#334763=CARTESIAN_POINT('Ctrl Pts',(0.733403857999945,5.2,4.55391625599999));
#334764=CARTESIAN_POINT('Ctrl Pts',(0.733403857999945,2.2,4.55391625599999));
#334765=CARTESIAN_POINT('Ctrl Pts',(0.732530494999944,12.2,4.55620281699999));
#334766=CARTESIAN_POINT('Ctrl Pts',(0.732530494999944,5.2,4.55620281699999));
#334767=CARTESIAN_POINT('Ctrl Pts',(0.732530494999944,2.2,4.55620281699999));
#334768=CARTESIAN_POINT('Ctrl Pts',(0.731653427999944,12.2,4.55849179699998));
#334769=CARTESIAN_POINT('Ctrl Pts',(0.731653427999944,5.2,4.55849179699998));
#334770=CARTESIAN_POINT('Ctrl Pts',(0.731653427999944,2.2,4.55849179699998));
#334771=CARTESIAN_POINT('Ctrl Pts',(0.730772652999944,12.2,4.56078318899999));
#334772=CARTESIAN_POINT('Ctrl Pts',(0.730772652999944,5.2,4.56078318899999));
#334773=CARTESIAN_POINT('Ctrl Pts',(0.730772652999944,2.2,4.56078318899999));
#334774=CARTESIAN_POINT('Ctrl Pts',(0.729888166999944,12.2,4.56307698199999));
#334775=CARTESIAN_POINT('Ctrl Pts',(0.729888166999944,5.2,4.56307698199999));
#334776=CARTESIAN_POINT('Ctrl Pts',(0.729888166999944,2.2,4.56307698199999));
#334777=CARTESIAN_POINT('Ctrl Pts',(0.728999964999945,12.2,4.56537316999999));
#334778=CARTESIAN_POINT('Ctrl Pts',(0.728999964999945,5.2,4.56537316999999));
#334779=CARTESIAN_POINT('Ctrl Pts',(0.728999964999945,2.2,4.56537316999999));
#334780=CARTESIAN_POINT('Ctrl Pts',(0.728108044999944,12.2,4.56767174299999));
#334781=CARTESIAN_POINT('Ctrl Pts',(0.728108044999944,5.2,4.56767174299999));
#334782=CARTESIAN_POINT('Ctrl Pts',(0.728108044999944,2.2,4.56767174299999));
#334783=CARTESIAN_POINT('Ctrl Pts',(0.727212399999945,12.2,4.56997269299999));
#334784=CARTESIAN_POINT('Ctrl Pts',(0.727212399999945,5.2,4.56997269299999));
#334785=CARTESIAN_POINT('Ctrl Pts',(0.727212399999945,2.2,4.56997269299999));
#334786=CARTESIAN_POINT('Ctrl Pts',(0.726313029999944,12.2,4.57227601299999));
#334787=CARTESIAN_POINT('Ctrl Pts',(0.726313029999944,5.2,4.57227601299999));
#334788=CARTESIAN_POINT('Ctrl Pts',(0.726313029999944,2.2,4.57227601299999));
#334789=CARTESIAN_POINT('Ctrl Pts',(0.725409927999944,12.2,4.57458169399998));
#334790=CARTESIAN_POINT('Ctrl Pts',(0.725409927999944,5.2,4.57458169399998));
#334791=CARTESIAN_POINT('Ctrl Pts',(0.725409927999944,2.2,4.57458169399998));
#334792=CARTESIAN_POINT('Ctrl Pts',(0.724503090999944,12.2,4.57688972699999));
#334793=CARTESIAN_POINT('Ctrl Pts',(0.724503090999944,5.2,4.57688972699999));
#334794=CARTESIAN_POINT('Ctrl Pts',(0.724503090999944,2.2,4.57688972699999));
#334795=CARTESIAN_POINT('Ctrl Pts',(0.723592515999945,12.2,4.57920010399998));
#334796=CARTESIAN_POINT('Ctrl Pts',(0.723592515999945,5.2,4.57920010399998));
#334797=CARTESIAN_POINT('Ctrl Pts',(0.723592515999945,2.2,4.57920010399998));
#334798=CARTESIAN_POINT('Ctrl Pts',(0.722678199999944,12.2,4.58151281799999));
#334799=CARTESIAN_POINT('Ctrl Pts',(0.722678199999944,5.2,4.58151281799999));
#334800=CARTESIAN_POINT('Ctrl Pts',(0.722678199999944,2.2,4.58151281799999));
#334801=CARTESIAN_POINT('Ctrl Pts',(0.721760135999945,12.2,4.58382785899998));
#334802=CARTESIAN_POINT('Ctrl Pts',(0.721760135999945,5.2,4.58382785899998));
#334803=CARTESIAN_POINT('Ctrl Pts',(0.721760135999945,2.2,4.58382785899998));
#334804=CARTESIAN_POINT('Ctrl Pts',(0.720838322999944,12.2,4.58614521899998));
#334805=CARTESIAN_POINT('Ctrl Pts',(0.720838322999944,5.2,4.58614521899998));
#334806=CARTESIAN_POINT('Ctrl Pts',(0.720838322999944,2.2,4.58614521899998));
#334807=CARTESIAN_POINT('Ctrl Pts',(0.719912756999944,12.2,4.58846488999999));
#334808=CARTESIAN_POINT('Ctrl Pts',(0.719912756999944,5.2,4.58846488999999));
#334809=CARTESIAN_POINT('Ctrl Pts',(0.719912756999944,2.2,4.58846488999999));
#334810=CARTESIAN_POINT('Ctrl Pts',(0.718983433999945,12.2,4.59078686499999));
#334811=CARTESIAN_POINT('Ctrl Pts',(0.718983433999945,5.2,4.59078686499999));
#334812=CARTESIAN_POINT('Ctrl Pts',(0.718983433999945,2.2,4.59078686499999));
#334813=CARTESIAN_POINT('Ctrl Pts',(0.718050349999944,12.2,4.59311113399998));
#334814=CARTESIAN_POINT('Ctrl Pts',(0.718050349999944,5.2,4.59311113399998));
#334815=CARTESIAN_POINT('Ctrl Pts',(0.718050349999944,2.2,4.59311113399998));
#334816=CARTESIAN_POINT('Ctrl Pts',(0.717113500999944,12.2,4.59543768999998));
#334817=CARTESIAN_POINT('Ctrl Pts',(0.717113500999944,5.2,4.59543768999998));
#334818=CARTESIAN_POINT('Ctrl Pts',(0.717113500999944,2.2,4.59543768999998));
#334819=CARTESIAN_POINT('Ctrl Pts',(0.716172884999944,12.2,4.59776652499999));
#334820=CARTESIAN_POINT('Ctrl Pts',(0.716172884999944,5.2,4.59776652499999));
#334821=CARTESIAN_POINT('Ctrl Pts',(0.716172884999944,2.2,4.59776652499999));
#334822=CARTESIAN_POINT('Ctrl Pts',(0.715228496999945,12.2,4.60009762899999));
#334823=CARTESIAN_POINT('Ctrl Pts',(0.715228496999945,5.2,4.60009762899999));
#334824=CARTESIAN_POINT('Ctrl Pts',(0.715228496999945,2.2,4.60009762899999));
#334825=CARTESIAN_POINT('Ctrl Pts',(0.714280331999944,12.2,4.60243099399998));
#334826=CARTESIAN_POINT('Ctrl Pts',(0.714280331999944,5.2,4.60243099399998));
#334827=CARTESIAN_POINT('Ctrl Pts',(0.714280331999944,2.2,4.60243099399998));
#334828=CARTESIAN_POINT('Ctrl Pts',(0.713328389999944,12.2,4.60476661399999));
#334829=CARTESIAN_POINT('Ctrl Pts',(0.713328389999944,5.2,4.60476661399999));
#334830=CARTESIAN_POINT('Ctrl Pts',(0.713328389999944,2.2,4.60476661399999));
#334831=CARTESIAN_POINT('Ctrl Pts',(0.712372663999944,12.2,4.60710447899999));
#334832=CARTESIAN_POINT('Ctrl Pts',(0.712372663999944,5.2,4.60710447899999));
#334833=CARTESIAN_POINT('Ctrl Pts',(0.712372663999944,2.2,4.60710447899999));
#334834=CARTESIAN_POINT('Ctrl Pts',(0.711413152999943,12.2,4.60944458099998));
#334835=CARTESIAN_POINT('Ctrl Pts',(0.711413152999943,5.2,4.60944458099998));
#334836=CARTESIAN_POINT('Ctrl Pts',(0.711413152999943,2.2,4.60944458099998));
#334837=CARTESIAN_POINT('Ctrl Pts',(0.710449851999945,12.2,4.61178691299998));
#334838=CARTESIAN_POINT('Ctrl Pts',(0.710449851999945,5.2,4.61178691299998));
#334839=CARTESIAN_POINT('Ctrl Pts',(0.710449851999945,2.2,4.61178691299998));
#334840=CARTESIAN_POINT('Ctrl Pts',(0.709482756999944,12.2,4.61413146499999));
#334841=CARTESIAN_POINT('Ctrl Pts',(0.709482756999944,5.2,4.61413146499999));
#334842=CARTESIAN_POINT('Ctrl Pts',(0.709482756999944,2.2,4.61413146499999));
#334843=CARTESIAN_POINT('Ctrl Pts',(0.708511864999944,12.2,4.61647822799998));
#334844=CARTESIAN_POINT('Ctrl Pts',(0.708511864999944,5.2,4.61647822799998));
#334845=CARTESIAN_POINT('Ctrl Pts',(0.708511864999944,2.2,4.61647822799998));
#334846=CARTESIAN_POINT('Ctrl Pts',(0.707537173999944,12.2,4.61882719699998));
#334847=CARTESIAN_POINT('Ctrl Pts',(0.707537173999944,5.2,4.61882719699998));
#334848=CARTESIAN_POINT('Ctrl Pts',(0.707537173999944,2.2,4.61882719699998));
#334849=CARTESIAN_POINT('Ctrl Pts',(0.706558677999943,12.2,4.62117836299999));
#334850=CARTESIAN_POINT('Ctrl Pts',(0.706558677999943,5.2,4.62117836299999));
#334851=CARTESIAN_POINT('Ctrl Pts',(0.706558677999943,2.2,4.62117836299999));
#334852=CARTESIAN_POINT('Ctrl Pts',(0.705576373999944,12.2,4.62353171699998));
#334853=CARTESIAN_POINT('Ctrl Pts',(0.705576373999944,5.2,4.62353171699998));
#334854=CARTESIAN_POINT('Ctrl Pts',(0.705576373999944,2.2,4.62353171699998));
#334855=CARTESIAN_POINT('Ctrl Pts',(0.704590260999944,12.2,4.62588724999998));
#334856=CARTESIAN_POINT('Ctrl Pts',(0.704590260999944,5.2,4.62588724999998));
#334857=CARTESIAN_POINT('Ctrl Pts',(0.704590260999944,2.2,4.62588724999998));
#334858=CARTESIAN_POINT('Ctrl Pts',(0.703600331999944,12.2,4.62824495499999));
#334859=CARTESIAN_POINT('Ctrl Pts',(0.703600331999944,5.2,4.62824495499999));
#334860=CARTESIAN_POINT('Ctrl Pts',(0.703600331999944,2.2,4.62824495499999));
#334861=CARTESIAN_POINT('Ctrl Pts',(0.702606586999944,12.2,4.63060482299999));
#334862=CARTESIAN_POINT('Ctrl Pts',(0.702606586999944,5.2,4.63060482299999));
#334863=CARTESIAN_POINT('Ctrl Pts',(0.702606586999944,2.2,4.63060482299999));
#334864=CARTESIAN_POINT('Ctrl Pts',(0.701609018999945,12.2,4.63296684699999));
#334865=CARTESIAN_POINT('Ctrl Pts',(0.701609018999945,5.2,4.63296684699999));
#334866=CARTESIAN_POINT('Ctrl Pts',(0.701609018999945,2.2,4.63296684699999));
#334867=CARTESIAN_POINT('Ctrl Pts',(0.700607627999944,12.2,4.63533101799998));
#334868=CARTESIAN_POINT('Ctrl Pts',(0.700607627999944,5.2,4.63533101799998));
#334869=CARTESIAN_POINT('Ctrl Pts',(0.700607627999944,2.2,4.63533101799998));
#334870=CARTESIAN_POINT('Ctrl Pts',(0.699602407999944,12.2,4.63769732799998));
#334871=CARTESIAN_POINT('Ctrl Pts',(0.699602407999944,5.2,4.63769732799998));
#334872=CARTESIAN_POINT('Ctrl Pts',(0.699602407999944,2.2,4.63769732799998));
#334873=CARTESIAN_POINT('Ctrl Pts',(0.698593355999945,12.2,4.64006576799999));
#334874=CARTESIAN_POINT('Ctrl Pts',(0.698593355999945,5.2,4.64006576799999));
#334875=CARTESIAN_POINT('Ctrl Pts',(0.698593355999945,2.2,4.64006576799999));
#334876=CARTESIAN_POINT('Ctrl Pts',(0.697580470999944,12.2,4.64243633299999));
#334877=CARTESIAN_POINT('Ctrl Pts',(0.697580470999944,5.2,4.64243633299999));
#334878=CARTESIAN_POINT('Ctrl Pts',(0.697580470999944,2.2,4.64243633299999));
#334879=CARTESIAN_POINT('Ctrl Pts',(0.696563746999944,12.2,4.64480901199998));
#334880=CARTESIAN_POINT('Ctrl Pts',(0.696563746999944,5.2,4.64480901199998));
#334881=CARTESIAN_POINT('Ctrl Pts',(0.696563746999944,2.2,4.64480901199998));
#334882=CARTESIAN_POINT('Ctrl Pts',(0.695543181999944,12.2,4.64718379799999));
#334883=CARTESIAN_POINT('Ctrl Pts',(0.695543181999944,5.2,4.64718379799999));
#334884=CARTESIAN_POINT('Ctrl Pts',(0.695543181999944,2.2,4.64718379799999));
#334885=CARTESIAN_POINT('Ctrl Pts',(0.694518772999944,12.2,4.64956068299998));
#334886=CARTESIAN_POINT('Ctrl Pts',(0.694518772999944,5.2,4.64956068299998));
#334887=CARTESIAN_POINT('Ctrl Pts',(0.694518772999944,2.2,4.64956068299998));
#334888=CARTESIAN_POINT('Ctrl Pts',(0.693490514999944,12.2,4.65193965799998));
#334889=CARTESIAN_POINT('Ctrl Pts',(0.693490514999944,5.2,4.65193965799998));
#334890=CARTESIAN_POINT('Ctrl Pts',(0.693490514999944,2.2,4.65193965799998));
#334891=CARTESIAN_POINT('Ctrl Pts',(0.692458406999944,12.2,4.65432071499999));
#334892=CARTESIAN_POINT('Ctrl Pts',(0.692458406999944,5.2,4.65432071499999));
#334893=CARTESIAN_POINT('Ctrl Pts',(0.692458406999944,2.2,4.65432071499999));
#334894=CARTESIAN_POINT('Ctrl Pts',(0.691422441999944,12.2,4.65670384699998));
#334895=CARTESIAN_POINT('Ctrl Pts',(0.691422441999944,5.2,4.65670384699998));
#334896=CARTESIAN_POINT('Ctrl Pts',(0.691422441999944,2.2,4.65670384699998));
#334897=CARTESIAN_POINT('Ctrl Pts',(0.690382619999944,12.2,4.65908904299998));
#334898=CARTESIAN_POINT('Ctrl Pts',(0.690382619999944,5.2,4.65908904299998));
#334899=CARTESIAN_POINT('Ctrl Pts',(0.690382619999944,2.2,4.65908904299998));
#334900=CARTESIAN_POINT('Ctrl Pts',(0.689338937999944,12.2,4.66147629599998));
#334901=CARTESIAN_POINT('Ctrl Pts',(0.689338937999944,5.2,4.66147629599998));
#334902=CARTESIAN_POINT('Ctrl Pts',(0.689338937999944,2.2,4.66147629599998));
#334903=CARTESIAN_POINT('Ctrl Pts',(0.688291388999944,12.2,4.66386559899998));
#334904=CARTESIAN_POINT('Ctrl Pts',(0.688291388999944,5.2,4.66386559899998));
#334905=CARTESIAN_POINT('Ctrl Pts',(0.688291388999944,2.2,4.66386559899998));
#334906=CARTESIAN_POINT('Ctrl Pts',(0.687239972999943,12.2,4.66625694299999));
#334907=CARTESIAN_POINT('Ctrl Pts',(0.687239972999943,5.2,4.66625694299999));
#334908=CARTESIAN_POINT('Ctrl Pts',(0.687239972999943,2.2,4.66625694299999));
#334909=CARTESIAN_POINT('Ctrl Pts',(0.686184687999944,12.2,4.66865032199999));
#334910=CARTESIAN_POINT('Ctrl Pts',(0.686184687999944,5.2,4.66865032199999));
#334911=CARTESIAN_POINT('Ctrl Pts',(0.686184687999944,2.2,4.66865032199999));
#334912=CARTESIAN_POINT('Ctrl Pts',(0.685125528999944,12.2,4.67104572799999));
#334913=CARTESIAN_POINT('Ctrl Pts',(0.685125528999944,5.2,4.67104572799999));
#334914=CARTESIAN_POINT('Ctrl Pts',(0.685125528999944,2.2,4.67104572799999));
#334915=CARTESIAN_POINT('Ctrl Pts',(0.684062492999944,12.2,4.67344315399998));
#334916=CARTESIAN_POINT('Ctrl Pts',(0.684062492999944,5.2,4.67344315399998));
#334917=CARTESIAN_POINT('Ctrl Pts',(0.684062492999944,2.2,4.67344315399998));
#334918=CARTESIAN_POINT('Ctrl Pts',(0.682995577999944,12.2,4.67584259099999));
#334919=CARTESIAN_POINT('Ctrl Pts',(0.682995577999944,5.2,4.67584259099999));
#334920=CARTESIAN_POINT('Ctrl Pts',(0.682995577999944,2.2,4.67584259099999));
#334921=CARTESIAN_POINT('Ctrl Pts',(0.681924779999944,12.2,4.67824403199998));
#334922=CARTESIAN_POINT('Ctrl Pts',(0.681924779999944,5.2,4.67824403199998));
#334923=CARTESIAN_POINT('Ctrl Pts',(0.681924779999944,2.2,4.67824403199998));
#334924=CARTESIAN_POINT('Ctrl Pts',(0.680850095999944,12.2,4.68064746499999));
#334925=CARTESIAN_POINT('Ctrl Pts',(0.680850095999944,5.2,4.68064746499999));
#334926=CARTESIAN_POINT('Ctrl Pts',(0.680850095999944,2.2,4.68064746499999));
#334927=CARTESIAN_POINT('Ctrl Pts',(0.679771519999944,12.2,4.68305288099998));
#334928=CARTESIAN_POINT('Ctrl Pts',(0.679771519999944,5.2,4.68305288099998));
#334929=CARTESIAN_POINT('Ctrl Pts',(0.679771519999944,2.2,4.68305288099998));
#334930=CARTESIAN_POINT('Ctrl Pts',(0.678689050999944,12.2,4.68546026999999));
#334931=CARTESIAN_POINT('Ctrl Pts',(0.678689050999944,5.2,4.68546026999999));
#334932=CARTESIAN_POINT('Ctrl Pts',(0.678689050999944,2.2,4.68546026999999));
#334933=CARTESIAN_POINT('Ctrl Pts',(0.677602681999944,12.2,4.68786962299998));
#334934=CARTESIAN_POINT('Ctrl Pts',(0.677602681999944,5.2,4.68786962299998));
#334935=CARTESIAN_POINT('Ctrl Pts',(0.677602681999944,2.2,4.68786962299998));
#334936=CARTESIAN_POINT('Ctrl Pts',(0.676512413999945,12.2,4.69028093199999));
#334937=CARTESIAN_POINT('Ctrl Pts',(0.676512413999945,5.2,4.69028093199999));
#334938=CARTESIAN_POINT('Ctrl Pts',(0.676512413999945,2.2,4.69028093199999));
#334939=CARTESIAN_POINT('Ctrl Pts',(0.675418241999944,12.2,4.69269419199998));
#334940=CARTESIAN_POINT('Ctrl Pts',(0.675418241999944,5.2,4.69269419199998));
#334941=CARTESIAN_POINT('Ctrl Pts',(0.675418241999944,2.2,4.69269419199998));
#334942=CARTESIAN_POINT('Ctrl Pts',(0.674320165999944,12.2,4.69510939799999));
#334943=CARTESIAN_POINT('Ctrl Pts',(0.674320165999944,5.2,4.69510939799999));
#334944=CARTESIAN_POINT('Ctrl Pts',(0.674320165999944,2.2,4.69510939799999));
#334945=CARTESIAN_POINT('Ctrl Pts',(0.673218184999944,12.2,4.69752654799999));
#334946=CARTESIAN_POINT('Ctrl Pts',(0.673218184999944,5.2,4.69752654799999));
#334947=CARTESIAN_POINT('Ctrl Pts',(0.673218184999944,2.2,4.69752654799999));
#334948=CARTESIAN_POINT('Ctrl Pts',(0.672333474999944,12.2,4.69946182299999));
#334949=CARTESIAN_POINT('Ctrl Pts',(0.672333474999944,5.2,4.69946182299999));
#334950=CARTESIAN_POINT('Ctrl Pts',(0.672333474999944,2.2,4.69946182299999));
#334951=CARTESIAN_POINT('Ctrl Pts',(0.671668184999944,12.2,4.70091415399998));
#334952=CARTESIAN_POINT('Ctrl Pts',(0.671668184999944,5.2,4.70091415399998));
#334953=CARTESIAN_POINT('Ctrl Pts',(0.671668184999944,2.2,4.70091415399998));
#334954=CARTESIAN_POINT('Ctrl Pts',(0.671223877999945,12.2,4.70188276299999));
#334955=CARTESIAN_POINT('Ctrl Pts',(0.671223877999945,5.2,4.70188276299999));
#334956=CARTESIAN_POINT('Ctrl Pts',(0.671223877999945,2.2,4.70188276299999));
#334957=CARTESIAN_POINT('Ctrl Pts',(0.671001528999944,12.2,4.70236716399998));
#334958=CARTESIAN_POINT('Ctrl Pts',(0.671001528999944,5.2,4.70236716399998));
#334959=CARTESIAN_POINT('Ctrl Pts',(0.671001528999944,2.2,4.70236716399998));
#334960=CARTESIAN_POINT('',(0.846447418999944,12.2,3.90299742599999));
#334961=CARTESIAN_POINT('Origin',(-5.66300478732629E-14,15.2,-1.77635683940025E-14));
#334962=CARTESIAN_POINT('',(0.768297694999944,12.2,3.54264641999999));
#334963=CARTESIAN_POINT('Origin',(-5.66300478732629E-14,15.2,-1.77635683940025E-14));
#334964=CARTESIAN_POINT('',(1.30596997799994,2.2,3.38157765299999));
#334965=CARTESIAN_POINT('Origin',(-5.66300478732629E-14,15.2,-1.77635683940025E-14));
#334966=CARTESIAN_POINT('',(2.19921400599994,12.2,3.33366463399998));
#334967=CARTESIAN_POINT('',(1.99616775999994,12.2,3.02587826499998));
#334968=CARTESIAN_POINT('Origin',(1.43879834299994,15.2,3.72551314699999));
#334969=CARTESIAN_POINT('',(1.43881682999994,12.2,3.72556101799999));
#334970=CARTESIAN_POINT('Ctrl Pts',(2.02484995099994,12.2,4.29679911999998));
#334971=CARTESIAN_POINT('Ctrl Pts',(2.02484995099994,5.2,4.29679911999998));
#334972=CARTESIAN_POINT('Ctrl Pts',(2.02484995099994,2.2,4.29679911999998));
#334973=CARTESIAN_POINT('Ctrl Pts',(2.02439790199994,12.2,4.29651674599998));
#334974=CARTESIAN_POINT('Ctrl Pts',(2.02439790199994,5.2,4.29651674599998));
#334975=CARTESIAN_POINT('Ctrl Pts',(2.02439790199994,2.2,4.29651674599998));
#334976=CARTESIAN_POINT('Ctrl Pts',(2.02349423499994,12.2,4.29595194499999));
#334977=CARTESIAN_POINT('Ctrl Pts',(2.02349423499994,5.2,4.29595194499999));
#334978=CARTESIAN_POINT('Ctrl Pts',(2.02349423499994,2.2,4.29595194499999));
#334979=CARTESIAN_POINT('Ctrl Pts',(2.02214003499994,12.2,4.29510458699998));
#334980=CARTESIAN_POINT('Ctrl Pts',(2.02214003499994,5.2,4.29510458699998));
#334981=CARTESIAN_POINT('Ctrl Pts',(2.02214003499994,2.2,4.29510458699998));
#334982=CARTESIAN_POINT('Ctrl Pts',(2.02033703299994,12.2,4.29397446099999));
#334983=CARTESIAN_POINT('Ctrl Pts',(2.02033703299994,5.2,4.29397446099999));
#334984=CARTESIAN_POINT('Ctrl Pts',(2.02033703299994,2.2,4.29397446099999));
#334985=CARTESIAN_POINT('Ctrl Pts',(2.01808761199994,12.2,4.29256127999999));
#334986=CARTESIAN_POINT('Ctrl Pts',(2.01808761199994,5.2,4.29256127999999));
#334987=CARTESIAN_POINT('Ctrl Pts',(2.01808761199994,2.2,4.29256127999999));
#334988=CARTESIAN_POINT('Ctrl Pts',(2.01584252099994,12.2,4.29114757499999));
#334989=CARTESIAN_POINT('Ctrl Pts',(2.01584252099994,5.2,4.29114757499999));
#334990=CARTESIAN_POINT('Ctrl Pts',(2.01584252099994,2.2,4.29114757499999));
#334991=CARTESIAN_POINT('Ctrl Pts',(2.01360176199994,12.2,4.28973334999998));
#334992=CARTESIAN_POINT('Ctrl Pts',(2.01360176199994,5.2,4.28973334999998));
#334993=CARTESIAN_POINT('Ctrl Pts',(2.01360176199994,2.2,4.28973334999998));
#334994=CARTESIAN_POINT('Ctrl Pts',(2.01136533499994,12.2,4.28831860799999));
#334995=CARTESIAN_POINT('Ctrl Pts',(2.01136533499994,5.2,4.28831860799999));
#334996=CARTESIAN_POINT('Ctrl Pts',(2.01136533499994,2.2,4.28831860799999));
#334997=CARTESIAN_POINT('Ctrl Pts',(2.00913324299994,12.2,4.28690335699999));
#334998=CARTESIAN_POINT('Ctrl Pts',(2.00913324299994,5.2,4.28690335699999));
#334999=CARTESIAN_POINT('Ctrl Pts',(2.00913324299994,2.2,4.28690335699999));
#335000=CARTESIAN_POINT('Ctrl Pts',(2.00690548599994,12.2,4.28548760099999));
#335001=CARTESIAN_POINT('Ctrl Pts',(2.00690548599994,5.2,4.28548760099999));
#335002=CARTESIAN_POINT('Ctrl Pts',(2.00690548599994,2.2,4.28548760099999));
#335003=CARTESIAN_POINT('Ctrl Pts',(2.00468206699994,12.2,4.28407135299998));
#335004=CARTESIAN_POINT('Ctrl Pts',(2.00468206699994,5.2,4.28407135299998));
#335005=CARTESIAN_POINT('Ctrl Pts',(2.00468206699994,2.2,4.28407135299998));
#335006=CARTESIAN_POINT('Ctrl Pts',(2.00246298799994,12.2,4.28265462199998));
#335007=CARTESIAN_POINT('Ctrl Pts',(2.00246298799994,5.2,4.28265462199998));
#335008=CARTESIAN_POINT('Ctrl Pts',(2.00246298799994,2.2,4.28265462199998));
#335009=CARTESIAN_POINT('Ctrl Pts',(2.00024825099994,12.2,4.28123741899999));
#335010=CARTESIAN_POINT('Ctrl Pts',(2.00024825099994,5.2,4.28123741899999));
#335011=CARTESIAN_POINT('Ctrl Pts',(2.00024825099994,2.2,4.28123741899999));
#335012=CARTESIAN_POINT('Ctrl Pts',(1.99803785899994,12.2,4.27981975299998));
#335013=CARTESIAN_POINT('Ctrl Pts',(1.99803785899994,5.2,4.27981975299998));
#335014=CARTESIAN_POINT('Ctrl Pts',(1.99803785899994,2.2,4.27981975299998));
#335015=CARTESIAN_POINT('Ctrl Pts',(1.99583181299994,12.2,4.27840163599999));
#335016=CARTESIAN_POINT('Ctrl Pts',(1.99583181299994,5.2,4.27840163599999));
#335017=CARTESIAN_POINT('Ctrl Pts',(1.99583181299994,2.2,4.27840163599999));
#335018=CARTESIAN_POINT('Ctrl Pts',(1.99363011599994,12.2,4.27698307399999));
#335019=CARTESIAN_POINT('Ctrl Pts',(1.99363011599994,5.2,4.27698307399999));
#335020=CARTESIAN_POINT('Ctrl Pts',(1.99363011599994,2.2,4.27698307399999));
#335021=CARTESIAN_POINT('Ctrl Pts',(1.99143276799994,12.2,4.27556407599998));
#335022=CARTESIAN_POINT('Ctrl Pts',(1.99143276799994,5.2,4.27556407599998));
#335023=CARTESIAN_POINT('Ctrl Pts',(1.99143276799994,2.2,4.27556407599998));
#335024=CARTESIAN_POINT('Ctrl Pts',(1.98923977299994,12.2,4.27414464999998));
#335025=CARTESIAN_POINT('Ctrl Pts',(1.98923977299994,5.2,4.27414464999998));
#335026=CARTESIAN_POINT('Ctrl Pts',(1.98923977299994,2.2,4.27414464999998));
#335027=CARTESIAN_POINT('Ctrl Pts',(1.98705112999994,12.2,4.27272480299998));
#335028=CARTESIAN_POINT('Ctrl Pts',(1.98705112999994,5.2,4.27272480299998));
#335029=CARTESIAN_POINT('Ctrl Pts',(1.98705112999994,2.2,4.27272480299998));
#335030=CARTESIAN_POINT('Ctrl Pts',(1.98486684199994,12.2,4.27130454199999));
#335031=CARTESIAN_POINT('Ctrl Pts',(1.98486684199994,5.2,4.27130454199999));
#335032=CARTESIAN_POINT('Ctrl Pts',(1.98486684199994,2.2,4.27130454199999));
#335033=CARTESIAN_POINT('Ctrl Pts',(1.98268690899994,12.2,4.26988387799998));
#335034=CARTESIAN_POINT('Ctrl Pts',(1.98268690899994,5.2,4.26988387799998));
#335035=CARTESIAN_POINT('Ctrl Pts',(1.98268690899994,2.2,4.26988387799998));
#335036=CARTESIAN_POINT('Ctrl Pts',(1.98051133699994,12.2,4.26846281599998));
#335037=CARTESIAN_POINT('Ctrl Pts',(1.98051133699994,5.2,4.26846281599998));
#335038=CARTESIAN_POINT('Ctrl Pts',(1.98051133699994,2.2,4.26846281599998));
#335039=CARTESIAN_POINT('Ctrl Pts',(1.97834012299994,12.2,4.26704136799999));
#335040=CARTESIAN_POINT('Ctrl Pts',(1.97834012299994,5.2,4.26704136799999));
#335041=CARTESIAN_POINT('Ctrl Pts',(1.97834012299994,2.2,4.26704136799999));
#335042=CARTESIAN_POINT('Ctrl Pts',(1.97617327099994,12.2,4.26561954099999));
#335043=CARTESIAN_POINT('Ctrl Pts',(1.97617327099994,5.2,4.26561954099999));
#335044=CARTESIAN_POINT('Ctrl Pts',(1.97617327099994,2.2,4.26561954099999));
#335045=CARTESIAN_POINT('Ctrl Pts',(1.97401078399994,12.2,4.26419734499999));
#335046=CARTESIAN_POINT('Ctrl Pts',(1.97401078399994,5.2,4.26419734499999));
#335047=CARTESIAN_POINT('Ctrl Pts',(1.97401078399994,2.2,4.26419734499999));
#335048=CARTESIAN_POINT('Ctrl Pts',(1.97185265999994,12.2,4.26277478799998));
#335049=CARTESIAN_POINT('Ctrl Pts',(1.97185265999994,5.2,4.26277478799998));
#335050=CARTESIAN_POINT('Ctrl Pts',(1.97185265999994,2.2,4.26277478799998));
#335051=CARTESIAN_POINT('Ctrl Pts',(1.96969890499994,12.2,4.26135187899998));
#335052=CARTESIAN_POINT('Ctrl Pts',(1.96969890499994,5.2,4.26135187899998));
#335053=CARTESIAN_POINT('Ctrl Pts',(1.96969890499994,2.2,4.26135187899998));
#335054=CARTESIAN_POINT('Ctrl Pts',(1.96754951799994,12.2,4.25992862799998));
#335055=CARTESIAN_POINT('Ctrl Pts',(1.96754951799994,5.2,4.25992862799998));
#335056=CARTESIAN_POINT('Ctrl Pts',(1.96754951799994,2.2,4.25992862799998));
#335057=CARTESIAN_POINT('Ctrl Pts',(1.96540450099994,12.2,4.25850504099999));
#335058=CARTESIAN_POINT('Ctrl Pts',(1.96540450099994,5.2,4.25850504099999));
#335059=CARTESIAN_POINT('Ctrl Pts',(1.96540450099994,2.2,4.25850504099999));
#335060=CARTESIAN_POINT('Ctrl Pts',(1.96326385599994,12.2,4.25708112799998));
#335061=CARTESIAN_POINT('Ctrl Pts',(1.96326385599994,5.2,4.25708112799998));
#335062=CARTESIAN_POINT('Ctrl Pts',(1.96326385599994,2.2,4.25708112799998));
#335063=CARTESIAN_POINT('Ctrl Pts',(1.96112758399994,12.2,4.25565689599999));
#335064=CARTESIAN_POINT('Ctrl Pts',(1.96112758399994,5.2,4.25565689599999));
#335065=CARTESIAN_POINT('Ctrl Pts',(1.96112758399994,2.2,4.25565689599999));
#335066=CARTESIAN_POINT('Ctrl Pts',(1.95899568899994,12.2,4.25423235599999));
#335067=CARTESIAN_POINT('Ctrl Pts',(1.95899568899994,5.2,4.25423235599999));
#335068=CARTESIAN_POINT('Ctrl Pts',(1.95899568899994,2.2,4.25423235599999));
#335069=CARTESIAN_POINT('Ctrl Pts',(1.95686816899994,12.2,4.25280751499999));
#335070=CARTESIAN_POINT('Ctrl Pts',(1.95686816899994,5.2,4.25280751499999));
#335071=CARTESIAN_POINT('Ctrl Pts',(1.95686816899994,2.2,4.25280751499999));
#335072=CARTESIAN_POINT('Ctrl Pts',(1.95474502799994,12.2,4.25138238199998));
#335073=CARTESIAN_POINT('Ctrl Pts',(1.95474502799994,5.2,4.25138238199998));
#335074=CARTESIAN_POINT('Ctrl Pts',(1.95474502799994,2.2,4.25138238199998));
#335075=CARTESIAN_POINT('Ctrl Pts',(1.95262626799994,12.2,4.24995696599999));
#335076=CARTESIAN_POINT('Ctrl Pts',(1.95262626799994,5.2,4.24995696599999));
#335077=CARTESIAN_POINT('Ctrl Pts',(1.95262626799994,2.2,4.24995696599999));
#335078=CARTESIAN_POINT('Ctrl Pts',(1.95051188799995,12.2,4.24853127599999));
#335079=CARTESIAN_POINT('Ctrl Pts',(1.95051188799995,5.2,4.24853127599999));
#335080=CARTESIAN_POINT('Ctrl Pts',(1.95051188799995,2.2,4.24853127599999));
#335081=CARTESIAN_POINT('Ctrl Pts',(1.94840189199994,12.2,4.24710531999998));
#335082=CARTESIAN_POINT('Ctrl Pts',(1.94840189199994,5.2,4.24710531999998));
#335083=CARTESIAN_POINT('Ctrl Pts',(1.94840189199994,2.2,4.24710531999998));
#335084=CARTESIAN_POINT('Ctrl Pts',(1.94629628199994,12.2,4.24567910799999));
#335085=CARTESIAN_POINT('Ctrl Pts',(1.94629628199994,5.2,4.24567910799999));
#335086=CARTESIAN_POINT('Ctrl Pts',(1.94629628199994,2.2,4.24567910799999));
#335087=CARTESIAN_POINT('Ctrl Pts',(1.94419505699994,12.2,4.24425264599999));
#335088=CARTESIAN_POINT('Ctrl Pts',(1.94419505699994,5.2,4.24425264599999));
#335089=CARTESIAN_POINT('Ctrl Pts',(1.94419505699994,2.2,4.24425264599999));
#335090=CARTESIAN_POINT('Ctrl Pts',(1.94209821999994,12.2,4.24282594599998));
#335091=CARTESIAN_POINT('Ctrl Pts',(1.94209821999994,5.2,4.24282594599998));
#335092=CARTESIAN_POINT('Ctrl Pts',(1.94209821999994,2.2,4.24282594599998));
#335093=CARTESIAN_POINT('Ctrl Pts',(1.94000577299994,12.2,4.24139901599998));
#335094=CARTESIAN_POINT('Ctrl Pts',(1.94000577299994,5.2,4.24139901599998));
#335095=CARTESIAN_POINT('Ctrl Pts',(1.94000577299994,2.2,4.24139901599998));
#335096=CARTESIAN_POINT('Ctrl Pts',(1.93791771799994,12.2,4.23997186399999));
#335097=CARTESIAN_POINT('Ctrl Pts',(1.93791771799994,5.2,4.23997186399999));
#335098=CARTESIAN_POINT('Ctrl Pts',(1.93791771799994,2.2,4.23997186399999));
#335099=CARTESIAN_POINT('Ctrl Pts',(1.93583405399994,12.2,4.23854449999999));
#335100=CARTESIAN_POINT('Ctrl Pts',(1.93583405399994,5.2,4.23854449999999));
#335101=CARTESIAN_POINT('Ctrl Pts',(1.93583405399994,2.2,4.23854449999999));
#335102=CARTESIAN_POINT('Ctrl Pts',(1.93375478499994,12.2,4.23711693099998));
#335103=CARTESIAN_POINT('Ctrl Pts',(1.93375478499994,5.2,4.23711693099998));
#335104=CARTESIAN_POINT('Ctrl Pts',(1.93375478499994,2.2,4.23711693099998));
#335105=CARTESIAN_POINT('Ctrl Pts',(1.93167991099994,12.2,4.23568916599999));
#335106=CARTESIAN_POINT('Ctrl Pts',(1.93167991099994,5.2,4.23568916599999));
#335107=CARTESIAN_POINT('Ctrl Pts',(1.93167991099994,2.2,4.23568916599999));
#335108=CARTESIAN_POINT('Ctrl Pts',(1.92960943499994,12.2,4.23426121599999));
#335109=CARTESIAN_POINT('Ctrl Pts',(1.92960943499994,5.2,4.23426121599999));
#335110=CARTESIAN_POINT('Ctrl Pts',(1.92960943499994,2.2,4.23426121599999));
#335111=CARTESIAN_POINT('Ctrl Pts',(1.92754335699994,12.2,4.23283308699999));
#335112=CARTESIAN_POINT('Ctrl Pts',(1.92754335699994,5.2,4.23283308699999));
#335113=CARTESIAN_POINT('Ctrl Pts',(1.92754335699994,2.2,4.23283308699999));
#335114=CARTESIAN_POINT('Ctrl Pts',(1.92548167999994,12.2,4.23140478999999));
#335115=CARTESIAN_POINT('Ctrl Pts',(1.92548167999994,5.2,4.23140478999999));
#335116=CARTESIAN_POINT('Ctrl Pts',(1.92548167999994,2.2,4.23140478999999));
#335117=CARTESIAN_POINT('Ctrl Pts',(1.92342440299994,12.2,4.22997633299998));
#335118=CARTESIAN_POINT('Ctrl Pts',(1.92342440299994,5.2,4.22997633299998));
#335119=CARTESIAN_POINT('Ctrl Pts',(1.92342440299994,2.2,4.22997633299998));
#335120=CARTESIAN_POINT('Ctrl Pts',(1.92137152999994,12.2,4.22854772599998));
#335121=CARTESIAN_POINT('Ctrl Pts',(1.92137152999994,5.2,4.22854772599998));
#335122=CARTESIAN_POINT('Ctrl Pts',(1.92137152999994,2.2,4.22854772599998));
#335123=CARTESIAN_POINT('Ctrl Pts',(1.91932306199994,12.2,4.22711897599999));
#335124=CARTESIAN_POINT('Ctrl Pts',(1.91932306199994,5.2,4.22711897599999));
#335125=CARTESIAN_POINT('Ctrl Pts',(1.91932306199994,2.2,4.22711897599999));
#335126=CARTESIAN_POINT('Ctrl Pts',(1.91727899899994,12.2,4.22569009299998));
#335127=CARTESIAN_POINT('Ctrl Pts',(1.91727899899994,5.2,4.22569009299998));
#335128=CARTESIAN_POINT('Ctrl Pts',(1.91727899899994,2.2,4.22569009299998));
#335129=CARTESIAN_POINT('Ctrl Pts',(1.91523934399994,12.2,4.22426108799999));
#335130=CARTESIAN_POINT('Ctrl Pts',(1.91523934399994,5.2,4.22426108799999));
#335131=CARTESIAN_POINT('Ctrl Pts',(1.91523934399994,2.2,4.22426108799999));
#335132=CARTESIAN_POINT('Ctrl Pts',(1.91320409699994,12.2,4.22283196599999));
#335133=CARTESIAN_POINT('Ctrl Pts',(1.91320409699994,5.2,4.22283196599999));
#335134=CARTESIAN_POINT('Ctrl Pts',(1.91320409699994,2.2,4.22283196599999));
#335135=CARTESIAN_POINT('Ctrl Pts',(1.91117325999994,12.2,4.22140273799998));
#335136=CARTESIAN_POINT('Ctrl Pts',(1.91117325999994,5.2,4.22140273799998));
#335137=CARTESIAN_POINT('Ctrl Pts',(1.91117325999994,2.2,4.22140273799998));
#335138=CARTESIAN_POINT('Ctrl Pts',(1.90914683499994,12.2,4.21997341099999));
#335139=CARTESIAN_POINT('Ctrl Pts',(1.90914683499994,5.2,4.21997341099999));
#335140=CARTESIAN_POINT('Ctrl Pts',(1.90914683499994,2.2,4.21997341099999));
#335141=CARTESIAN_POINT('Ctrl Pts',(1.90712482299994,12.2,4.21854399799999));
#335142=CARTESIAN_POINT('Ctrl Pts',(1.90712482299994,5.2,4.21854399799999));
#335143=CARTESIAN_POINT('Ctrl Pts',(1.90712482299994,2.2,4.21854399799999));
#335144=CARTESIAN_POINT('Ctrl Pts',(1.90510722499994,12.2,4.21711450499998));
#335145=CARTESIAN_POINT('Ctrl Pts',(1.90510722499994,5.2,4.21711450499998));
#335146=CARTESIAN_POINT('Ctrl Pts',(1.90510722499994,2.2,4.21711450499998));
#335147=CARTESIAN_POINT('Ctrl Pts',(1.90309404399994,12.2,4.21568494399998));
#335148=CARTESIAN_POINT('Ctrl Pts',(1.90309404399994,5.2,4.21568494399998));
#335149=CARTESIAN_POINT('Ctrl Pts',(1.90309404399994,2.2,4.21568494399998));
#335150=CARTESIAN_POINT('Ctrl Pts',(1.90108527799994,12.2,4.21425531899998));
#335151=CARTESIAN_POINT('Ctrl Pts',(1.90108527799994,5.2,4.21425531899998));
#335152=CARTESIAN_POINT('Ctrl Pts',(1.90108527799994,2.2,4.21425531899998));
#335153=CARTESIAN_POINT('Ctrl Pts',(1.89908093199994,12.2,4.21282564299998));
#335154=CARTESIAN_POINT('Ctrl Pts',(1.89908093199994,5.2,4.21282564299998));
#335155=CARTESIAN_POINT('Ctrl Pts',(1.89908093199994,2.2,4.21282564299998));
#335156=CARTESIAN_POINT('Ctrl Pts',(1.89708100499994,12.2,4.21139592399999));
#335157=CARTESIAN_POINT('Ctrl Pts',(1.89708100499994,5.2,4.21139592399999));
#335158=CARTESIAN_POINT('Ctrl Pts',(1.89708100499994,2.2,4.21139592399999));
#335159=CARTESIAN_POINT('Ctrl Pts',(1.89508549899994,12.2,4.20996617099998));
#335160=CARTESIAN_POINT('Ctrl Pts',(1.89508549899994,5.2,4.20996617099998));
#335161=CARTESIAN_POINT('Ctrl Pts',(1.89508549899994,2.2,4.20996617099998));
#335162=CARTESIAN_POINT('Ctrl Pts',(1.89309441499994,12.2,4.20853639299998));
#335163=CARTESIAN_POINT('Ctrl Pts',(1.89309441499994,5.2,4.20853639299998));
#335164=CARTESIAN_POINT('Ctrl Pts',(1.89309441499994,2.2,4.20853639299998));
#335165=CARTESIAN_POINT('Ctrl Pts',(1.89110775499994,12.2,4.20710659899999));
#335166=CARTESIAN_POINT('Ctrl Pts',(1.89110775499994,5.2,4.20710659899999));
#335167=CARTESIAN_POINT('Ctrl Pts',(1.89110775499994,2.2,4.20710659899999));
#335168=CARTESIAN_POINT('Ctrl Pts',(1.88912552099994,12.2,4.20567679799999));
#335169=CARTESIAN_POINT('Ctrl Pts',(1.88912552099994,5.2,4.20567679799999));
#335170=CARTESIAN_POINT('Ctrl Pts',(1.88912552099994,2.2,4.20567679799999));
#335171=CARTESIAN_POINT('Ctrl Pts',(1.88714771199994,12.2,4.20424700099999));
#335172=CARTESIAN_POINT('Ctrl Pts',(1.88714771199994,5.2,4.20424700099999));
#335173=CARTESIAN_POINT('Ctrl Pts',(1.88714771199994,2.2,4.20424700099999));
#335174=CARTESIAN_POINT('Ctrl Pts',(1.88517432999994,12.2,4.20281721399999));
#335175=CARTESIAN_POINT('Ctrl Pts',(1.88517432999994,5.2,4.20281721399999));
#335176=CARTESIAN_POINT('Ctrl Pts',(1.88517432999994,2.2,4.20281721399999));
#335177=CARTESIAN_POINT('Ctrl Pts',(1.88320537699994,12.2,4.20138744899998));
#335178=CARTESIAN_POINT('Ctrl Pts',(1.88320537699994,5.2,4.20138744899998));
#335179=CARTESIAN_POINT('Ctrl Pts',(1.88320537699994,2.2,4.20138744899998));
#335180=CARTESIAN_POINT('Ctrl Pts',(1.88124085599994,12.2,4.19995771299998));
#335181=CARTESIAN_POINT('Ctrl Pts',(1.88124085599994,5.2,4.19995771299998));
#335182=CARTESIAN_POINT('Ctrl Pts',(1.88124085599994,2.2,4.19995771299998));
#335183=CARTESIAN_POINT('Ctrl Pts',(1.87928076399994,12.2,4.19852801599998));
#335184=CARTESIAN_POINT('Ctrl Pts',(1.87928076399994,5.2,4.19852801599998));
#335185=CARTESIAN_POINT('Ctrl Pts',(1.87928076399994,2.2,4.19852801599998));
#335186=CARTESIAN_POINT('Ctrl Pts',(1.87732510499994,12.2,4.19709836799999));
#335187=CARTESIAN_POINT('Ctrl Pts',(1.87732510499994,5.2,4.19709836799999));
#335188=CARTESIAN_POINT('Ctrl Pts',(1.87732510499994,2.2,4.19709836799999));
#335189=CARTESIAN_POINT('Ctrl Pts',(1.87537387899994,12.2,4.19566877599999));
#335190=CARTESIAN_POINT('Ctrl Pts',(1.87537387899994,5.2,4.19566877599999));
#335191=CARTESIAN_POINT('Ctrl Pts',(1.87537387899994,2.2,4.19566877599999));
#335192=CARTESIAN_POINT('Ctrl Pts',(1.87342708999994,12.2,4.19423925199998));
#335193=CARTESIAN_POINT('Ctrl Pts',(1.87342708999994,5.2,4.19423925199998));
#335194=CARTESIAN_POINT('Ctrl Pts',(1.87342708999994,2.2,4.19423925199998));
#335195=CARTESIAN_POINT('Ctrl Pts',(1.87148473399994,12.2,4.19280980399999));
#335196=CARTESIAN_POINT('Ctrl Pts',(1.87148473399994,5.2,4.19280980399999));
#335197=CARTESIAN_POINT('Ctrl Pts',(1.87148473399994,2.2,4.19280980399999));
#335198=CARTESIAN_POINT('Ctrl Pts',(1.86954681799994,12.2,4.19138044099999));
#335199=CARTESIAN_POINT('Ctrl Pts',(1.86954681799994,5.2,4.19138044099999));
#335200=CARTESIAN_POINT('Ctrl Pts',(1.86954681799994,2.2,4.19138044099999));
#335201=CARTESIAN_POINT('Ctrl Pts',(1.86761333799994,12.2,4.18995117199999));
#335202=CARTESIAN_POINT('Ctrl Pts',(1.86761333799994,5.2,4.18995117199999));
#335203=CARTESIAN_POINT('Ctrl Pts',(1.86761333799994,2.2,4.18995117199999));
#335204=CARTESIAN_POINT('Ctrl Pts',(1.86568429899994,12.2,4.18852200699998));
#335205=CARTESIAN_POINT('Ctrl Pts',(1.86568429899994,5.2,4.18852200699998));
#335206=CARTESIAN_POINT('Ctrl Pts',(1.86568429899994,2.2,4.18852200699998));
#335207=CARTESIAN_POINT('Ctrl Pts',(1.86375969999994,12.2,4.18709295499998));
#335208=CARTESIAN_POINT('Ctrl Pts',(1.86375969999994,5.2,4.18709295499998));
#335209=CARTESIAN_POINT('Ctrl Pts',(1.86375969999994,2.2,4.18709295499998));
#335210=CARTESIAN_POINT('Ctrl Pts',(1.86183954399994,12.2,4.18566402599998));
#335211=CARTESIAN_POINT('Ctrl Pts',(1.86183954399994,5.2,4.18566402599998));
#335212=CARTESIAN_POINT('Ctrl Pts',(1.86183954399994,2.2,4.18566402599998));
#335213=CARTESIAN_POINT('Ctrl Pts',(1.85992382999994,12.2,4.18423522799999));
#335214=CARTESIAN_POINT('Ctrl Pts',(1.85992382999994,5.2,4.18423522799999));
#335215=CARTESIAN_POINT('Ctrl Pts',(1.85992382999994,2.2,4.18423522799999));
#335216=CARTESIAN_POINT('Ctrl Pts',(1.85801255999994,12.2,4.18280657099999));
#335217=CARTESIAN_POINT('Ctrl Pts',(1.85801255999994,5.2,4.18280657099999));
#335218=CARTESIAN_POINT('Ctrl Pts',(1.85801255999994,2.2,4.18280657099999));
#335219=CARTESIAN_POINT('Ctrl Pts',(1.85610573599994,12.2,4.18137806399999));
#335220=CARTESIAN_POINT('Ctrl Pts',(1.85610573599994,5.2,4.18137806399999));
#335221=CARTESIAN_POINT('Ctrl Pts',(1.85610573599994,2.2,4.18137806399999));
#335222=CARTESIAN_POINT('Ctrl Pts',(1.85420335799994,12.2,4.17994971699999));
#335223=CARTESIAN_POINT('Ctrl Pts',(1.85420335799994,5.2,4.17994971699999));
#335224=CARTESIAN_POINT('Ctrl Pts',(1.85420335799994,2.2,4.17994971699999));
#335225=CARTESIAN_POINT('Ctrl Pts',(1.85230542599994,12.2,4.17852153899998));
#335226=CARTESIAN_POINT('Ctrl Pts',(1.85230542599994,5.2,4.17852153899998));
#335227=CARTESIAN_POINT('Ctrl Pts',(1.85230542599994,2.2,4.17852153899998));
#335228=CARTESIAN_POINT('Ctrl Pts',(1.85041194399994,12.2,4.17709353899999));
#335229=CARTESIAN_POINT('Ctrl Pts',(1.85041194399994,5.2,4.17709353899999));
#335230=CARTESIAN_POINT('Ctrl Pts',(1.85041194399994,2.2,4.17709353899999));
#335231=CARTESIAN_POINT('Ctrl Pts',(1.84852290999994,12.2,4.17566572799998));
#335232=CARTESIAN_POINT('Ctrl Pts',(1.84852290999994,5.2,4.17566572799998));
#335233=CARTESIAN_POINT('Ctrl Pts',(1.84852290999994,2.2,4.17566572799998));
#335234=CARTESIAN_POINT('Ctrl Pts',(1.84663832699994,12.2,4.17423811299999));
#335235=CARTESIAN_POINT('Ctrl Pts',(1.84663832699994,5.2,4.17423811299999));
#335236=CARTESIAN_POINT('Ctrl Pts',(1.84663832699994,2.2,4.17423811299999));
#335237=CARTESIAN_POINT('Ctrl Pts',(1.84475819699994,12.2,4.17281070499998));
#335238=CARTESIAN_POINT('Ctrl Pts',(1.84475819699994,5.2,4.17281070499998));
#335239=CARTESIAN_POINT('Ctrl Pts',(1.84475819699994,2.2,4.17281070499998));
#335240=CARTESIAN_POINT('Ctrl Pts',(1.84288251799994,12.2,4.17138351299998));
#335241=CARTESIAN_POINT('Ctrl Pts',(1.84288251799994,5.2,4.17138351299998));
#335242=CARTESIAN_POINT('Ctrl Pts',(1.84288251799994,2.2,4.17138351299998));
#335243=CARTESIAN_POINT('Ctrl Pts',(1.84101129199994,12.2,4.16995654599998));
#335244=CARTESIAN_POINT('Ctrl Pts',(1.84101129199994,5.2,4.16995654599998));
#335245=CARTESIAN_POINT('Ctrl Pts',(1.84101129199994,2.2,4.16995654599998));
#335246=CARTESIAN_POINT('Ctrl Pts',(1.83914452199994,12.2,4.16852981599998));
#335247=CARTESIAN_POINT('Ctrl Pts',(1.83914452199994,5.2,4.16852981599998));
#335248=CARTESIAN_POINT('Ctrl Pts',(1.83914452199994,2.2,4.16852981599998));
#335249=CARTESIAN_POINT('Ctrl Pts',(1.83728220699995,12.2,4.16710332899999));
#335250=CARTESIAN_POINT('Ctrl Pts',(1.83728220699995,5.2,4.16710332899999));
#335251=CARTESIAN_POINT('Ctrl Pts',(1.83728220699995,2.2,4.16710332899999));
#335252=CARTESIAN_POINT('Ctrl Pts',(1.83542434799994,12.2,4.16567709499999));
#335253=CARTESIAN_POINT('Ctrl Pts',(1.83542434799994,5.2,4.16567709499999));
#335254=CARTESIAN_POINT('Ctrl Pts',(1.83542434799994,2.2,4.16567709499999));
#335255=CARTESIAN_POINT('Ctrl Pts',(1.83357094699994,12.2,4.16425112599998));
#335256=CARTESIAN_POINT('Ctrl Pts',(1.83357094699994,5.2,4.16425112599998));
#335257=CARTESIAN_POINT('Ctrl Pts',(1.83357094699994,2.2,4.16425112599998));
#335258=CARTESIAN_POINT('Ctrl Pts',(1.83172200399994,12.2,4.16282543099998));
#335259=CARTESIAN_POINT('Ctrl Pts',(1.83172200399994,5.2,4.16282543099998));
#335260=CARTESIAN_POINT('Ctrl Pts',(1.83172200399994,2.2,4.16282543099998));
#335261=CARTESIAN_POINT('Ctrl Pts',(1.82987752099994,12.2,4.16140001599998));
#335262=CARTESIAN_POINT('Ctrl Pts',(1.82987752099994,5.2,4.16140001599998));
#335263=CARTESIAN_POINT('Ctrl Pts',(1.82987752099994,2.2,4.16140001599998));
#335264=CARTESIAN_POINT('Ctrl Pts',(1.82803749799994,12.2,4.15997489499999));
#335265=CARTESIAN_POINT('Ctrl Pts',(1.82803749799994,5.2,4.15997489499999));
#335266=CARTESIAN_POINT('Ctrl Pts',(1.82803749799994,2.2,4.15997489499999));
#335267=CARTESIAN_POINT('Ctrl Pts',(1.82620193699994,12.2,4.15855007599998));
#335268=CARTESIAN_POINT('Ctrl Pts',(1.82620193699994,5.2,4.15855007599998));
#335269=CARTESIAN_POINT('Ctrl Pts',(1.82620193699994,2.2,4.15855007599998));
#335270=CARTESIAN_POINT('Ctrl Pts',(1.82437083599994,12.2,4.15712556699999));
#335271=CARTESIAN_POINT('Ctrl Pts',(1.82437083599994,5.2,4.15712556699999));
#335272=CARTESIAN_POINT('Ctrl Pts',(1.82437083599994,2.2,4.15712556699999));
#335273=CARTESIAN_POINT('Ctrl Pts',(1.82254419999994,12.2,4.15570137999998));
#335274=CARTESIAN_POINT('Ctrl Pts',(1.82254419999994,5.2,4.15570137999998));
#335275=CARTESIAN_POINT('Ctrl Pts',(1.82254419999994,2.2,4.15570137999998));
#335276=CARTESIAN_POINT('Ctrl Pts',(1.82072202699994,12.2,4.15427752199999));
#335277=CARTESIAN_POINT('Ctrl Pts',(1.82072202699994,5.2,4.15427752199999));
#335278=CARTESIAN_POINT('Ctrl Pts',(1.82072202699994,2.2,4.15427752199999));
#335279=CARTESIAN_POINT('Ctrl Pts',(1.81890431799994,12.2,4.15285400499998));
#335280=CARTESIAN_POINT('Ctrl Pts',(1.81890431799994,5.2,4.15285400499998));
#335281=CARTESIAN_POINT('Ctrl Pts',(1.81890431799994,2.2,4.15285400499998));
#335282=CARTESIAN_POINT('Ctrl Pts',(1.81709107599994,12.2,4.15143083799999));
#335283=CARTESIAN_POINT('Ctrl Pts',(1.81709107599994,5.2,4.15143083799999));
#335284=CARTESIAN_POINT('Ctrl Pts',(1.81709107599994,2.2,4.15143083799999));
#335285=CARTESIAN_POINT('Ctrl Pts',(1.81528230099994,12.2,4.15000802999998));
#335286=CARTESIAN_POINT('Ctrl Pts',(1.81528230099994,5.2,4.15000802999998));
#335287=CARTESIAN_POINT('Ctrl Pts',(1.81528230099994,2.2,4.15000802999998));
#335288=CARTESIAN_POINT('Ctrl Pts',(1.81347799099994,12.2,4.14858559099999));
#335289=CARTESIAN_POINT('Ctrl Pts',(1.81347799099994,5.2,4.14858559099999));
#335290=CARTESIAN_POINT('Ctrl Pts',(1.81347799099994,2.2,4.14858559099999));
#335291=CARTESIAN_POINT('Ctrl Pts',(1.81167815099994,12.2,4.14716353099998));
#335292=CARTESIAN_POINT('Ctrl Pts',(1.81167815099994,5.2,4.14716353099998));
#335293=CARTESIAN_POINT('Ctrl Pts',(1.81167815099994,2.2,4.14716353099998));
#335294=CARTESIAN_POINT('Ctrl Pts',(1.80988277899994,12.2,4.14574185999999));
#335295=CARTESIAN_POINT('Ctrl Pts',(1.80988277899994,5.2,4.14574185999999));
#335296=CARTESIAN_POINT('Ctrl Pts',(1.80988277899994,2.2,4.14574185999999));
#335297=CARTESIAN_POINT('Ctrl Pts',(1.80809187599994,12.2,4.14432058599999));
#335298=CARTESIAN_POINT('Ctrl Pts',(1.80809187599994,5.2,4.14432058599999));
#335299=CARTESIAN_POINT('Ctrl Pts',(1.80809187599994,2.2,4.14432058599999));
#335300=CARTESIAN_POINT('Ctrl Pts',(1.80630544499994,12.2,4.14289972099999));
#335301=CARTESIAN_POINT('Ctrl Pts',(1.80630544499994,5.2,4.14289972099999));
#335302=CARTESIAN_POINT('Ctrl Pts',(1.80630544499994,2.2,4.14289972099999));
#335303=CARTESIAN_POINT('Ctrl Pts',(1.80452348399994,12.2,4.14147927299998));
#335304=CARTESIAN_POINT('Ctrl Pts',(1.80452348399994,5.2,4.14147927299998));
#335305=CARTESIAN_POINT('Ctrl Pts',(1.80452348399994,2.2,4.14147927299998));
#335306=CARTESIAN_POINT('Ctrl Pts',(1.80274599599994,12.2,4.14005925299998));
#335307=CARTESIAN_POINT('Ctrl Pts',(1.80274599599994,5.2,4.14005925299998));
#335308=CARTESIAN_POINT('Ctrl Pts',(1.80274599599994,2.2,4.14005925299998));
#335309=CARTESIAN_POINT('Ctrl Pts',(1.80097298099994,12.2,4.13863966899999));
#335310=CARTESIAN_POINT('Ctrl Pts',(1.80097298099994,5.2,4.13863966899999));
#335311=CARTESIAN_POINT('Ctrl Pts',(1.80097298099994,2.2,4.13863966899999));
#335312=CARTESIAN_POINT('Ctrl Pts',(1.79920443899994,12.2,4.13722053299999));
#335313=CARTESIAN_POINT('Ctrl Pts',(1.79920443899994,5.2,4.13722053299999));
#335314=CARTESIAN_POINT('Ctrl Pts',(1.79920443899994,2.2,4.13722053299999));
#335315=CARTESIAN_POINT('Ctrl Pts',(1.79744036999994,12.2,4.13580185399999));
#335316=CARTESIAN_POINT('Ctrl Pts',(1.79744036999994,5.2,4.13580185399999));
#335317=CARTESIAN_POINT('Ctrl Pts',(1.79744036999994,2.2,4.13580185399999));
#335318=CARTESIAN_POINT('Ctrl Pts',(1.79568077699994,12.2,4.13438364099999));
#335319=CARTESIAN_POINT('Ctrl Pts',(1.79568077699994,5.2,4.13438364099999));
#335320=CARTESIAN_POINT('Ctrl Pts',(1.79568077699994,2.2,4.13438364099999));
#335321=CARTESIAN_POINT('Ctrl Pts',(1.79392565999994,12.2,4.13296590499999));
#335322=CARTESIAN_POINT('Ctrl Pts',(1.79392565999994,5.2,4.13296590499999));
#335323=CARTESIAN_POINT('Ctrl Pts',(1.79392565999994,2.2,4.13296590499999));
#335324=CARTESIAN_POINT('Ctrl Pts',(1.79217501899994,12.2,4.13154865399999));
#335325=CARTESIAN_POINT('Ctrl Pts',(1.79217501899994,5.2,4.13154865399999));
#335326=CARTESIAN_POINT('Ctrl Pts',(1.79217501899994,2.2,4.13154865399999));
#335327=CARTESIAN_POINT('Ctrl Pts',(1.79042885499994,12.2,4.13013189999998));
#335328=CARTESIAN_POINT('Ctrl Pts',(1.79042885499994,5.2,4.13013189999998));
#335329=CARTESIAN_POINT('Ctrl Pts',(1.79042885499994,2.2,4.13013189999998));
#335330=CARTESIAN_POINT('Ctrl Pts',(1.78868716699994,12.2,4.12871565099999));
#335331=CARTESIAN_POINT('Ctrl Pts',(1.78868716699994,5.2,4.12871565099999));
#335332=CARTESIAN_POINT('Ctrl Pts',(1.78868716699994,2.2,4.12871565099999));
#335333=CARTESIAN_POINT('Ctrl Pts',(1.78694995899994,12.2,4.12729991899998));
#335334=CARTESIAN_POINT('Ctrl Pts',(1.78694995899994,5.2,4.12729991899998));
#335335=CARTESIAN_POINT('Ctrl Pts',(1.78694995899994,2.2,4.12729991899998));
#335336=CARTESIAN_POINT('Ctrl Pts',(1.78521722999994,12.2,4.12588471199999));
#335337=CARTESIAN_POINT('Ctrl Pts',(1.78521722999994,5.2,4.12588471199999));
#335338=CARTESIAN_POINT('Ctrl Pts',(1.78521722999994,2.2,4.12588471199999));
#335339=CARTESIAN_POINT('Ctrl Pts',(1.78348897899994,12.2,4.12447004199999));
#335340=CARTESIAN_POINT('Ctrl Pts',(1.78348897899994,5.2,4.12447004199999));
#335341=CARTESIAN_POINT('Ctrl Pts',(1.78348897899994,2.2,4.12447004199999));
#335342=CARTESIAN_POINT('Ctrl Pts',(1.78176520999994,12.2,4.12305591599999));
#335343=CARTESIAN_POINT('Ctrl Pts',(1.78176520999994,5.2,4.12305591599999));
#335344=CARTESIAN_POINT('Ctrl Pts',(1.78176520999994,2.2,4.12305591599999));
#335345=CARTESIAN_POINT('Ctrl Pts',(1.78004591999994,12.2,4.12164234599998));
#335346=CARTESIAN_POINT('Ctrl Pts',(1.78004591999994,5.2,4.12164234599998));
#335347=CARTESIAN_POINT('Ctrl Pts',(1.78004591999994,2.2,4.12164234599998));
#335348=CARTESIAN_POINT('Ctrl Pts',(1.77833111199994,12.2,4.12022934299999));
#335349=CARTESIAN_POINT('Ctrl Pts',(1.77833111199994,5.2,4.12022934299999));
#335350=CARTESIAN_POINT('Ctrl Pts',(1.77833111199994,2.2,4.12022934299999));
#335351=CARTESIAN_POINT('Ctrl Pts',(1.77662078699994,12.2,4.11881691399999));
#335352=CARTESIAN_POINT('Ctrl Pts',(1.77662078699994,5.2,4.11881691399999));
#335353=CARTESIAN_POINT('Ctrl Pts',(1.77662078699994,2.2,4.11881691399999));
#335354=CARTESIAN_POINT('Ctrl Pts',(1.77491494299994,12.2,4.11740507099999));
#335355=CARTESIAN_POINT('Ctrl Pts',(1.77491494299994,5.2,4.11740507099999));
#335356=CARTESIAN_POINT('Ctrl Pts',(1.77491494299994,2.2,4.11740507099999));
#335357=CARTESIAN_POINT('Ctrl Pts',(1.77321358199995,12.2,4.11599382299999));
#335358=CARTESIAN_POINT('Ctrl Pts',(1.77321358199995,5.2,4.11599382299999));
#335359=CARTESIAN_POINT('Ctrl Pts',(1.77321358199995,2.2,4.11599382299999));
#335360=CARTESIAN_POINT('Ctrl Pts',(1.77151670499994,12.2,4.11458318099999));
#335361=CARTESIAN_POINT('Ctrl Pts',(1.77151670499994,5.2,4.11458318099999));
#335362=CARTESIAN_POINT('Ctrl Pts',(1.77151670499994,2.2,4.11458318099999));
#335363=CARTESIAN_POINT('Ctrl Pts',(1.76982431199994,12.2,4.11317315499999));
#335364=CARTESIAN_POINT('Ctrl Pts',(1.76982431199994,5.2,4.11317315499999));
#335365=CARTESIAN_POINT('Ctrl Pts',(1.76982431199994,2.2,4.11317315499999));
#335366=CARTESIAN_POINT('Ctrl Pts',(1.76813640399994,12.2,4.11176375399998));
#335367=CARTESIAN_POINT('Ctrl Pts',(1.76813640399994,5.2,4.11176375399998));
#335368=CARTESIAN_POINT('Ctrl Pts',(1.76813640399994,2.2,4.11176375399998));
#335369=CARTESIAN_POINT('Ctrl Pts',(1.76645298099994,12.2,4.11035498799999));
#335370=CARTESIAN_POINT('Ctrl Pts',(1.76645298099994,5.2,4.11035498799999));
#335371=CARTESIAN_POINT('Ctrl Pts',(1.76645298099994,2.2,4.11035498799999));
#335372=CARTESIAN_POINT('Ctrl Pts',(1.76477404199994,12.2,4.10894686899999));
#335373=CARTESIAN_POINT('Ctrl Pts',(1.76477404199994,5.2,4.10894686899999));
#335374=CARTESIAN_POINT('Ctrl Pts',(1.76477404199994,2.2,4.10894686899999));
#335375=CARTESIAN_POINT('Ctrl Pts',(1.76309958999994,12.2,4.10753940599999));
#335376=CARTESIAN_POINT('Ctrl Pts',(1.76309958999994,5.2,4.10753940599999));
#335377=CARTESIAN_POINT('Ctrl Pts',(1.76309958999994,2.2,4.10753940599999));
#335378=CARTESIAN_POINT('Ctrl Pts',(1.76142962399994,12.2,4.10613260699999));
#335379=CARTESIAN_POINT('Ctrl Pts',(1.76142962399994,5.2,4.10613260699999));
#335380=CARTESIAN_POINT('Ctrl Pts',(1.76142962399994,2.2,4.10613260699999));
#335381=CARTESIAN_POINT('Ctrl Pts',(1.75976414499994,12.2,4.10472648599999));
#335382=CARTESIAN_POINT('Ctrl Pts',(1.75976414499994,5.2,4.10472648599999));
#335383=CARTESIAN_POINT('Ctrl Pts',(1.75976414499994,2.2,4.10472648599999));
#335384=CARTESIAN_POINT('Ctrl Pts',(1.75810315299994,12.2,4.10332105199998));
#335385=CARTESIAN_POINT('Ctrl Pts',(1.75810315299994,5.2,4.10332105199998));
#335386=CARTESIAN_POINT('Ctrl Pts',(1.75810315299994,2.2,4.10332105199998));
#335387=CARTESIAN_POINT('Ctrl Pts',(1.75644664999994,12.2,4.10191631299998));
#335388=CARTESIAN_POINT('Ctrl Pts',(1.75644664999994,5.2,4.10191631299998));
#335389=CARTESIAN_POINT('Ctrl Pts',(1.75644664999994,2.2,4.10191631299998));
#335390=CARTESIAN_POINT('Ctrl Pts',(1.75479463399994,12.2,4.10051228099999));
#335391=CARTESIAN_POINT('Ctrl Pts',(1.75479463399994,5.2,4.10051228099999));
#335392=CARTESIAN_POINT('Ctrl Pts',(1.75479463399994,2.2,4.10051228099999));
#335393=CARTESIAN_POINT('Ctrl Pts',(1.75314710699994,12.2,4.09910896499999));
#335394=CARTESIAN_POINT('Ctrl Pts',(1.75314710699994,5.2,4.09910896499999));
#335395=CARTESIAN_POINT('Ctrl Pts',(1.75314710699994,2.2,4.09910896499999));
#335396=CARTESIAN_POINT('Ctrl Pts',(1.75150406799994,12.2,4.09770637699998));
#335397=CARTESIAN_POINT('Ctrl Pts',(1.75150406799994,5.2,4.09770637699998));
#335398=CARTESIAN_POINT('Ctrl Pts',(1.75150406799994,2.2,4.09770637699998));
#335399=CARTESIAN_POINT('Ctrl Pts',(1.74986551799994,12.2,4.09630452599998));
#335400=CARTESIAN_POINT('Ctrl Pts',(1.74986551799994,5.2,4.09630452599998));
#335401=CARTESIAN_POINT('Ctrl Pts',(1.74986551799994,2.2,4.09630452599998));
#335402=CARTESIAN_POINT('Ctrl Pts',(1.74823145899994,12.2,4.09490342299998));
#335403=CARTESIAN_POINT('Ctrl Pts',(1.74823145899994,5.2,4.09490342299998));
#335404=CARTESIAN_POINT('Ctrl Pts',(1.74823145899994,2.2,4.09490342299998));
#335405=CARTESIAN_POINT('Ctrl Pts',(1.74660188899994,12.2,4.09350307699999));
#335406=CARTESIAN_POINT('Ctrl Pts',(1.74660188899994,5.2,4.09350307699999));
#335407=CARTESIAN_POINT('Ctrl Pts',(1.74660188899994,2.2,4.09350307699999));
#335408=CARTESIAN_POINT('Ctrl Pts',(1.74497680899994,12.2,4.09210349899999));
#335409=CARTESIAN_POINT('Ctrl Pts',(1.74497680899994,5.2,4.09210349899999));
#335410=CARTESIAN_POINT('Ctrl Pts',(1.74497680899994,2.2,4.09210349899999));
#335411=CARTESIAN_POINT('Ctrl Pts',(1.74335621999994,12.2,4.09070469999998));
#335412=CARTESIAN_POINT('Ctrl Pts',(1.74335621999994,5.2,4.09070469999998));
#335413=CARTESIAN_POINT('Ctrl Pts',(1.74335621999994,2.2,4.09070469999998));
#335414=CARTESIAN_POINT('Ctrl Pts',(1.74174012099995,12.2,4.08930668899998));
#335415=CARTESIAN_POINT('Ctrl Pts',(1.74174012099995,5.2,4.08930668899998));
#335416=CARTESIAN_POINT('Ctrl Pts',(1.74174012099995,2.2,4.08930668899998));
#335417=CARTESIAN_POINT('Ctrl Pts',(1.74012851399994,12.2,4.08790947699998));
#335418=CARTESIAN_POINT('Ctrl Pts',(1.74012851399994,5.2,4.08790947699998));
#335419=CARTESIAN_POINT('Ctrl Pts',(1.74012851399994,2.2,4.08790947699998));
#335420=CARTESIAN_POINT('Ctrl Pts',(1.73852139799994,12.2,4.08651307499999));
#335421=CARTESIAN_POINT('Ctrl Pts',(1.73852139799994,5.2,4.08651307499999));
#335422=CARTESIAN_POINT('Ctrl Pts',(1.73852139799994,2.2,4.08651307499999));
#335423=CARTESIAN_POINT('Ctrl Pts',(1.73691877299994,12.2,4.08511749099999));
#335424=CARTESIAN_POINT('Ctrl Pts',(1.73691877299994,5.2,4.08511749099999));
#335425=CARTESIAN_POINT('Ctrl Pts',(1.73691877299994,2.2,4.08511749099999));
#335426=CARTESIAN_POINT('Ctrl Pts',(1.73532063999994,12.2,4.08372273799999));
#335427=CARTESIAN_POINT('Ctrl Pts',(1.73532063999994,5.2,4.08372273799999));
#335428=CARTESIAN_POINT('Ctrl Pts',(1.73532063999994,2.2,4.08372273799999));
#335429=CARTESIAN_POINT('Ctrl Pts',(1.73372699999994,12.2,4.08232882499998));
#335430=CARTESIAN_POINT('Ctrl Pts',(1.73372699999994,5.2,4.08232882499998));
#335431=CARTESIAN_POINT('Ctrl Pts',(1.73372699999994,2.2,4.08232882499998));
#335432=CARTESIAN_POINT('Ctrl Pts',(1.73213785099994,12.2,4.08093576299999));
#335433=CARTESIAN_POINT('Ctrl Pts',(1.73213785099994,5.2,4.08093576299999));
#335434=CARTESIAN_POINT('Ctrl Pts',(1.73213785099994,2.2,4.08093576299999));
#335435=CARTESIAN_POINT('Ctrl Pts',(1.73055319499994,12.2,4.07954356199999));
#335436=CARTESIAN_POINT('Ctrl Pts',(1.73055319499994,5.2,4.07954356199999));
#335437=CARTESIAN_POINT('Ctrl Pts',(1.73055319499994,2.2,4.07954356199999));
#335438=CARTESIAN_POINT('Ctrl Pts',(1.72897303099994,12.2,4.07815223299998));
#335439=CARTESIAN_POINT('Ctrl Pts',(1.72897303099994,5.2,4.07815223299998));
#335440=CARTESIAN_POINT('Ctrl Pts',(1.72897303099994,2.2,4.07815223299998));
#335441=CARTESIAN_POINT('Ctrl Pts',(1.72739736099994,12.2,4.07676178499998));
#335442=CARTESIAN_POINT('Ctrl Pts',(1.72739736099994,5.2,4.07676178499998));
#335443=CARTESIAN_POINT('Ctrl Pts',(1.72739736099994,2.2,4.07676178499998));
#335444=CARTESIAN_POINT('Ctrl Pts',(1.72582618299994,12.2,4.07537222999999));
#335445=CARTESIAN_POINT('Ctrl Pts',(1.72582618299994,5.2,4.07537222999999));
#335446=CARTESIAN_POINT('Ctrl Pts',(1.72582618299994,2.2,4.07537222999999));
#335447=CARTESIAN_POINT('Ctrl Pts',(1.72425949799994,12.2,4.07398357899999));
#335448=CARTESIAN_POINT('Ctrl Pts',(1.72425949799994,5.2,4.07398357899999));
#335449=CARTESIAN_POINT('Ctrl Pts',(1.72425949799994,2.2,4.07398357899999));
#335450=CARTESIAN_POINT('Ctrl Pts',(1.72269730599994,12.2,4.07259584099998));
#335451=CARTESIAN_POINT('Ctrl Pts',(1.72269730599994,5.2,4.07259584099998));
#335452=CARTESIAN_POINT('Ctrl Pts',(1.72269730599994,2.2,4.07259584099998));
#335453=CARTESIAN_POINT('Ctrl Pts',(1.72113960799994,12.2,4.07120902699998));
#335454=CARTESIAN_POINT('Ctrl Pts',(1.72113960799994,5.2,4.07120902699998));
#335455=CARTESIAN_POINT('Ctrl Pts',(1.72113960799994,2.2,4.07120902699998));
#335456=CARTESIAN_POINT('Ctrl Pts',(1.71958640299994,12.2,4.06982314599999));
#335457=CARTESIAN_POINT('Ctrl Pts',(1.71958640299994,5.2,4.06982314599999));
#335458=CARTESIAN_POINT('Ctrl Pts',(1.71958640299994,2.2,4.06982314599999));
#335459=CARTESIAN_POINT('Ctrl Pts',(1.71803769099994,12.2,4.06843821099999));
#335460=CARTESIAN_POINT('Ctrl Pts',(1.71803769099994,5.2,4.06843821099999));
#335461=CARTESIAN_POINT('Ctrl Pts',(1.71803769099994,2.2,4.06843821099999));
#335462=CARTESIAN_POINT('Ctrl Pts',(1.71649347299994,12.2,4.06705423199998));
#335463=CARTESIAN_POINT('Ctrl Pts',(1.71649347299994,5.2,4.06705423199998));
#335464=CARTESIAN_POINT('Ctrl Pts',(1.71649347299994,2.2,4.06705423199998));
#335465=CARTESIAN_POINT('Ctrl Pts',(1.71495374999994,12.2,4.06567121899998));
#335466=CARTESIAN_POINT('Ctrl Pts',(1.71495374999994,5.2,4.06567121899998));
#335467=CARTESIAN_POINT('Ctrl Pts',(1.71495374999994,2.2,4.06567121899998));
#335468=CARTESIAN_POINT('Ctrl Pts',(1.71341851899994,12.2,4.06428918299999));
#335469=CARTESIAN_POINT('Ctrl Pts',(1.71341851899994,5.2,4.06428918299999));
#335470=CARTESIAN_POINT('Ctrl Pts',(1.71341851899994,2.2,4.06428918299999));
#335471=CARTESIAN_POINT('Ctrl Pts',(1.71188778099994,12.2,4.06290813299999));
#335472=CARTESIAN_POINT('Ctrl Pts',(1.71188778099994,5.2,4.06290813299999));
#335473=CARTESIAN_POINT('Ctrl Pts',(1.71188778099994,2.2,4.06290813299999));
#335474=CARTESIAN_POINT('Ctrl Pts',(1.71036153799994,12.2,4.06152808299999));
#335475=CARTESIAN_POINT('Ctrl Pts',(1.71036153799994,5.2,4.06152808299999));
#335476=CARTESIAN_POINT('Ctrl Pts',(1.71036153799994,2.2,4.06152808299999));
#335477=CARTESIAN_POINT('Ctrl Pts',(1.70883978799994,12.2,4.06014904099998));
#335478=CARTESIAN_POINT('Ctrl Pts',(1.70883978799994,5.2,4.06014904099998));
#335479=CARTESIAN_POINT('Ctrl Pts',(1.70883978799994,2.2,4.06014904099998));
#335480=CARTESIAN_POINT('Ctrl Pts',(1.70732253199994,12.2,4.05877101799998));
#335481=CARTESIAN_POINT('Ctrl Pts',(1.70732253199994,5.2,4.05877101799998));
#335482=CARTESIAN_POINT('Ctrl Pts',(1.70732253199994,2.2,4.05877101799998));
#335483=CARTESIAN_POINT('Ctrl Pts',(1.70580976999994,12.2,4.05739402399998));
#335484=CARTESIAN_POINT('Ctrl Pts',(1.70580976999994,5.2,4.05739402399998));
#335485=CARTESIAN_POINT('Ctrl Pts',(1.70580976999994,2.2,4.05739402399998));
#335486=CARTESIAN_POINT('Ctrl Pts',(1.70430150099994,12.2,4.05601807199999));
#335487=CARTESIAN_POINT('Ctrl Pts',(1.70430150099994,5.2,4.05601807199999));
#335488=CARTESIAN_POINT('Ctrl Pts',(1.70430150099994,2.2,4.05601807199999));
#335489=CARTESIAN_POINT('Ctrl Pts',(1.70279772599994,12.2,4.05464317099998));
#335490=CARTESIAN_POINT('Ctrl Pts',(1.70279772599994,5.2,4.05464317099998));
#335491=CARTESIAN_POINT('Ctrl Pts',(1.70279772599994,2.2,4.05464317099998));
#335492=CARTESIAN_POINT('Ctrl Pts',(1.70129844399994,12.2,4.05326933199999));
#335493=CARTESIAN_POINT('Ctrl Pts',(1.70129844399994,5.2,4.05326933199999));
#335494=CARTESIAN_POINT('Ctrl Pts',(1.70129844399994,2.2,4.05326933199999));
#335495=CARTESIAN_POINT('Ctrl Pts',(1.69980365399994,12.2,4.05189656599998));
#335496=CARTESIAN_POINT('Ctrl Pts',(1.69980365399994,5.2,4.05189656599998));
#335497=CARTESIAN_POINT('Ctrl Pts',(1.69980365399994,2.2,4.05189656599998));
#335498=CARTESIAN_POINT('Ctrl Pts',(1.69831335899994,12.2,4.05052488299999));
#335499=CARTESIAN_POINT('Ctrl Pts',(1.69831335899994,5.2,4.05052488299999));
#335500=CARTESIAN_POINT('Ctrl Pts',(1.69831335899994,2.2,4.05052488299999));
#335501=CARTESIAN_POINT('Ctrl Pts',(1.69682755599994,12.2,4.04915429499999));
#335502=CARTESIAN_POINT('Ctrl Pts',(1.69682755599994,5.2,4.04915429499999));
#335503=CARTESIAN_POINT('Ctrl Pts',(1.69682755599994,2.2,4.04915429499999));
#335504=CARTESIAN_POINT('Ctrl Pts',(1.69534624699994,12.2,4.04778481099999));
#335505=CARTESIAN_POINT('Ctrl Pts',(1.69534624699994,5.2,4.04778481099999));
#335506=CARTESIAN_POINT('Ctrl Pts',(1.69534624699994,2.2,4.04778481099999));
#335507=CARTESIAN_POINT('Ctrl Pts',(1.69386942999994,12.2,4.04641644499999));
#335508=CARTESIAN_POINT('Ctrl Pts',(1.69386942999994,5.2,4.04641644499999));
#335509=CARTESIAN_POINT('Ctrl Pts',(1.69386942999994,2.2,4.04641644499999));
#335510=CARTESIAN_POINT('Ctrl Pts',(1.69239710499994,12.2,4.04504920399999));
#335511=CARTESIAN_POINT('Ctrl Pts',(1.69239710499994,5.2,4.04504920399999));
#335512=CARTESIAN_POINT('Ctrl Pts',(1.69239710499994,2.2,4.04504920399999));
#335513=CARTESIAN_POINT('Ctrl Pts',(1.69092927299994,12.2,4.04368310099999));
#335514=CARTESIAN_POINT('Ctrl Pts',(1.69092927299994,5.2,4.04368310099999));
#335515=CARTESIAN_POINT('Ctrl Pts',(1.69092927299994,2.2,4.04368310099999));
#335516=CARTESIAN_POINT('Ctrl Pts',(1.68946593399994,12.2,4.04231814699998));
#335517=CARTESIAN_POINT('Ctrl Pts',(1.68946593399994,5.2,4.04231814699998));
#335518=CARTESIAN_POINT('Ctrl Pts',(1.68946593399994,2.2,4.04231814699998));
#335519=CARTESIAN_POINT('Ctrl Pts',(1.68800708599994,12.2,4.04095435199999));
#335520=CARTESIAN_POINT('Ctrl Pts',(1.68800708599994,5.2,4.04095435199999));
#335521=CARTESIAN_POINT('Ctrl Pts',(1.68800708599994,2.2,4.04095435199999));
#335522=CARTESIAN_POINT('Ctrl Pts',(1.68655272999994,12.2,4.03959172699999));
#335523=CARTESIAN_POINT('Ctrl Pts',(1.68655272999994,5.2,4.03959172699999));
#335524=CARTESIAN_POINT('Ctrl Pts',(1.68655272999994,2.2,4.03959172699999));
#335525=CARTESIAN_POINT('Ctrl Pts',(1.68510286499994,12.2,4.03823028399999));
#335526=CARTESIAN_POINT('Ctrl Pts',(1.68510286499994,5.2,4.03823028399999));
#335527=CARTESIAN_POINT('Ctrl Pts',(1.68510286499994,2.2,4.03823028399999));
#335528=CARTESIAN_POINT('Ctrl Pts',(1.68365749299994,12.2,4.03687003199998));
#335529=CARTESIAN_POINT('Ctrl Pts',(1.68365749299994,5.2,4.03687003199998));
#335530=CARTESIAN_POINT('Ctrl Pts',(1.68365749299994,2.2,4.03687003199998));
#335531=CARTESIAN_POINT('Ctrl Pts',(1.68221660999994,12.2,4.03551098399999));
#335532=CARTESIAN_POINT('Ctrl Pts',(1.68221660999994,5.2,4.03551098399999));
#335533=CARTESIAN_POINT('Ctrl Pts',(1.68221660999994,2.2,4.03551098399999));
#335534=CARTESIAN_POINT('Ctrl Pts',(1.68078021899994,12.2,4.03415314999998));
#335535=CARTESIAN_POINT('Ctrl Pts',(1.68078021899994,5.2,4.03415314999998));
#335536=CARTESIAN_POINT('Ctrl Pts',(1.68078021899994,2.2,4.03415314999998));
#335537=CARTESIAN_POINT('Ctrl Pts',(1.67934831799994,12.2,4.03279653999999));
#335538=CARTESIAN_POINT('Ctrl Pts',(1.67934831799994,5.2,4.03279653999999));
#335539=CARTESIAN_POINT('Ctrl Pts',(1.67934831799994,2.2,4.03279653999999));
#335540=CARTESIAN_POINT('Ctrl Pts',(1.67792090699994,12.2,4.03144116699998));
#335541=CARTESIAN_POINT('Ctrl Pts',(1.67792090699994,5.2,4.03144116699998));
#335542=CARTESIAN_POINT('Ctrl Pts',(1.67792090699994,2.2,4.03144116699998));
#335543=CARTESIAN_POINT('Ctrl Pts',(1.67649798599994,12.2,4.03008703999999));
#335544=CARTESIAN_POINT('Ctrl Pts',(1.67649798599994,5.2,4.03008703999999));
#335545=CARTESIAN_POINT('Ctrl Pts',(1.67649798599994,2.2,4.03008703999999));
#335546=CARTESIAN_POINT('Ctrl Pts',(1.67507955399994,12.2,4.02873417099999));
#335547=CARTESIAN_POINT('Ctrl Pts',(1.67507955399994,5.2,4.02873417099999));
#335548=CARTESIAN_POINT('Ctrl Pts',(1.67507955399994,2.2,4.02873417099999));
#335549=CARTESIAN_POINT('Ctrl Pts',(1.67366561099994,12.2,4.02738257199999));
#335550=CARTESIAN_POINT('Ctrl Pts',(1.67366561099994,5.2,4.02738257199999));
#335551=CARTESIAN_POINT('Ctrl Pts',(1.67366561099994,2.2,4.02738257199999));
#335552=CARTESIAN_POINT('Ctrl Pts',(1.67225615599994,12.2,4.02603225199999));
#335553=CARTESIAN_POINT('Ctrl Pts',(1.67225615599994,5.2,4.02603225199999));
#335554=CARTESIAN_POINT('Ctrl Pts',(1.67225615599994,2.2,4.02603225199999));
#335555=CARTESIAN_POINT('Ctrl Pts',(1.67085118999994,12.2,4.02468322399999));
#335556=CARTESIAN_POINT('Ctrl Pts',(1.67085118999994,5.2,4.02468322399999));
#335557=CARTESIAN_POINT('Ctrl Pts',(1.67085118999994,2.2,4.02468322399999));
#335558=CARTESIAN_POINT('Ctrl Pts',(1.66945071199994,12.2,4.02333549799998));
#335559=CARTESIAN_POINT('Ctrl Pts',(1.66945071199994,5.2,4.02333549799998));
#335560=CARTESIAN_POINT('Ctrl Pts',(1.66945071199994,2.2,4.02333549799998));
#335561=CARTESIAN_POINT('Ctrl Pts',(1.66805472199994,12.2,4.02198908599999));
#335562=CARTESIAN_POINT('Ctrl Pts',(1.66805472199994,5.2,4.02198908599999));
#335563=CARTESIAN_POINT('Ctrl Pts',(1.66805472199994,2.2,4.02198908599999));
#335564=CARTESIAN_POINT('Ctrl Pts',(1.66666321699994,12.2,4.02064399699999));
#335565=CARTESIAN_POINT('Ctrl Pts',(1.66666321699994,5.2,4.02064399699999));
#335566=CARTESIAN_POINT('Ctrl Pts',(1.66666321699994,2.2,4.02064399699999));
#335567=CARTESIAN_POINT('Ctrl Pts',(1.66527619999994,12.2,4.01930024499999));
#335568=CARTESIAN_POINT('Ctrl Pts',(1.66527619999994,5.2,4.01930024499999));
#335569=CARTESIAN_POINT('Ctrl Pts',(1.66527619999994,2.2,4.01930024499999));
#335570=CARTESIAN_POINT('Ctrl Pts',(1.66389366899994,12.2,4.01795783999999));
#335571=CARTESIAN_POINT('Ctrl Pts',(1.66389366899994,5.2,4.01795783999999));
#335572=CARTESIAN_POINT('Ctrl Pts',(1.66389366899994,2.2,4.01795783999999));
#335573=CARTESIAN_POINT('Ctrl Pts',(1.66251562299994,12.2,4.01661679299998));
#335574=CARTESIAN_POINT('Ctrl Pts',(1.66251562299994,5.2,4.01661679299998));
#335575=CARTESIAN_POINT('Ctrl Pts',(1.66251562299994,2.2,4.01661679299998));
#335576=CARTESIAN_POINT('Ctrl Pts',(1.66114206199994,12.2,4.01527711499998));
#335577=CARTESIAN_POINT('Ctrl Pts',(1.66114206199994,5.2,4.01527711499998));
#335578=CARTESIAN_POINT('Ctrl Pts',(1.66114206199994,2.2,4.01527711499998));
#335579=CARTESIAN_POINT('Ctrl Pts',(1.65977298499994,12.2,4.01393881699998));
#335580=CARTESIAN_POINT('Ctrl Pts',(1.65977298499994,5.2,4.01393881699998));
#335581=CARTESIAN_POINT('Ctrl Pts',(1.65977298499994,2.2,4.01393881699998));
#335582=CARTESIAN_POINT('Ctrl Pts',(1.65840839199994,12.2,4.01260191099999));
#335583=CARTESIAN_POINT('Ctrl Pts',(1.65840839199994,5.2,4.01260191099999));
#335584=CARTESIAN_POINT('Ctrl Pts',(1.65840839199994,2.2,4.01260191099999));
#335585=CARTESIAN_POINT('Ctrl Pts',(1.65704828299994,12.2,4.01126640799998));
#335586=CARTESIAN_POINT('Ctrl Pts',(1.65704828299994,5.2,4.01126640799998));
#335587=CARTESIAN_POINT('Ctrl Pts',(1.65704828299994,2.2,4.01126640799998));
#335588=CARTESIAN_POINT('Ctrl Pts',(1.65569265599994,12.2,4.00993231999998));
#335589=CARTESIAN_POINT('Ctrl Pts',(1.65569265599994,5.2,4.00993231999998));
#335590=CARTESIAN_POINT('Ctrl Pts',(1.65569265599994,2.2,4.00993231999998));
#335591=CARTESIAN_POINT('Ctrl Pts',(1.65434151199994,12.2,4.00859965599999));
#335592=CARTESIAN_POINT('Ctrl Pts',(1.65434151199994,5.2,4.00859965599999));
#335593=CARTESIAN_POINT('Ctrl Pts',(1.65434151199994,2.2,4.00859965599999));
#335594=CARTESIAN_POINT('Ctrl Pts',(1.65299484899994,12.2,4.00726843099999));
#335595=CARTESIAN_POINT('Ctrl Pts',(1.65299484899994,5.2,4.00726843099999));
#335596=CARTESIAN_POINT('Ctrl Pts',(1.65299484899994,2.2,4.00726843099999));
#335597=CARTESIAN_POINT('Ctrl Pts',(1.65165266699994,12.2,4.00593865299999));
#335598=CARTESIAN_POINT('Ctrl Pts',(1.65165266699994,5.2,4.00593865299999));
#335599=CARTESIAN_POINT('Ctrl Pts',(1.65165266699994,2.2,4.00593865299999));
#335600=CARTESIAN_POINT('Ctrl Pts',(1.65031496599994,12.2,4.00461033499998));
#335601=CARTESIAN_POINT('Ctrl Pts',(1.65031496599994,5.2,4.00461033499998));
#335602=CARTESIAN_POINT('Ctrl Pts',(1.65031496599994,2.2,4.00461033499998));
#335603=CARTESIAN_POINT('Ctrl Pts',(1.64898174299994,12.2,4.00328348699999));
#335604=CARTESIAN_POINT('Ctrl Pts',(1.64898174299994,5.2,4.00328348699999));
#335605=CARTESIAN_POINT('Ctrl Pts',(1.64898174299994,2.2,4.00328348699999));
#335606=CARTESIAN_POINT('Ctrl Pts',(1.64765300099994,12.2,4.00195812199998));
#335607=CARTESIAN_POINT('Ctrl Pts',(1.64765300099994,5.2,4.00195812199998));
#335608=CARTESIAN_POINT('Ctrl Pts',(1.64765300099994,2.2,4.00195812199998));
#335609=CARTESIAN_POINT('Ctrl Pts',(1.64632873599994,12.2,4.00063424999999));
#335610=CARTESIAN_POINT('Ctrl Pts',(1.64632873599994,5.2,4.00063424999999));
#335611=CARTESIAN_POINT('Ctrl Pts',(1.64632873599994,2.2,4.00063424999999));
#335612=CARTESIAN_POINT('Ctrl Pts',(1.64500894899994,12.2,3.99931188399999));
#335613=CARTESIAN_POINT('Ctrl Pts',(1.64500894899994,5.2,3.99931188399999));
#335614=CARTESIAN_POINT('Ctrl Pts',(1.64500894899994,2.2,3.99931188399999));
#335615=CARTESIAN_POINT('Ctrl Pts',(1.64369363799994,12.2,3.99799103399998));
#335616=CARTESIAN_POINT('Ctrl Pts',(1.64369363799994,5.2,3.99799103399998));
#335617=CARTESIAN_POINT('Ctrl Pts',(1.64369363799994,2.2,3.99799103399998));
#335618=CARTESIAN_POINT('Ctrl Pts',(1.64238280299994,12.2,3.99667171299999));
#335619=CARTESIAN_POINT('Ctrl Pts',(1.64238280299994,5.2,3.99667171299999));
#335620=CARTESIAN_POINT('Ctrl Pts',(1.64238280299994,2.2,3.99667171299999));
#335621=CARTESIAN_POINT('Ctrl Pts',(1.64107644399994,12.2,3.99535393099999));
#335622=CARTESIAN_POINT('Ctrl Pts',(1.64107644399994,5.2,3.99535393099999));
#335623=CARTESIAN_POINT('Ctrl Pts',(1.64107644399994,2.2,3.99535393099999));
#335624=CARTESIAN_POINT('Ctrl Pts',(1.63977455999994,12.2,3.99403769999999));
#335625=CARTESIAN_POINT('Ctrl Pts',(1.63977455999994,5.2,3.99403769999999));
#335626=CARTESIAN_POINT('Ctrl Pts',(1.63977455999994,2.2,3.99403769999999));
#335627=CARTESIAN_POINT('Ctrl Pts',(1.63847714899994,12.2,3.99272303099998));
#335628=CARTESIAN_POINT('Ctrl Pts',(1.63847714899994,5.2,3.99272303099998));
#335629=CARTESIAN_POINT('Ctrl Pts',(1.63847714899994,2.2,3.99272303099998));
#335630=CARTESIAN_POINT('Ctrl Pts',(1.63718421099994,12.2,3.99140993699999));
#335631=CARTESIAN_POINT('Ctrl Pts',(1.63718421099994,5.2,3.99140993699999));
#335632=CARTESIAN_POINT('Ctrl Pts',(1.63718421099994,2.2,3.99140993699999));
#335633=CARTESIAN_POINT('Ctrl Pts',(1.63589574499994,12.2,3.99009842799998));
#335634=CARTESIAN_POINT('Ctrl Pts',(1.63589574499994,5.2,3.99009842799998));
#335635=CARTESIAN_POINT('Ctrl Pts',(1.63589574499994,2.2,3.99009842799998));
#335636=CARTESIAN_POINT('Ctrl Pts',(1.63461175099994,12.2,3.98878851599999));
#335637=CARTESIAN_POINT('Ctrl Pts',(1.63461175099994,5.2,3.98878851599999));
#335638=CARTESIAN_POINT('Ctrl Pts',(1.63461175099994,2.2,3.98878851599999));
#335639=CARTESIAN_POINT('Ctrl Pts',(1.63333222699994,12.2,3.98748021299999));
#335640=CARTESIAN_POINT('Ctrl Pts',(1.63333222699994,5.2,3.98748021299999));
#335641=CARTESIAN_POINT('Ctrl Pts',(1.63333222699994,2.2,3.98748021299999));
#335642=CARTESIAN_POINT('Ctrl Pts',(1.63205717199994,12.2,3.98617353099999));
#335643=CARTESIAN_POINT('Ctrl Pts',(1.63205717199994,5.2,3.98617353099999));
#335644=CARTESIAN_POINT('Ctrl Pts',(1.63205717199994,2.2,3.98617353099999));
#335645=CARTESIAN_POINT('Ctrl Pts',(1.63078658599994,12.2,3.98486848099999));
#335646=CARTESIAN_POINT('Ctrl Pts',(1.63078658599994,5.2,3.98486848099999));
#335647=CARTESIAN_POINT('Ctrl Pts',(1.63078658599994,2.2,3.98486848099999));
#335648=CARTESIAN_POINT('Ctrl Pts',(1.62952046699994,12.2,3.98356507399999));
#335649=CARTESIAN_POINT('Ctrl Pts',(1.62952046699994,5.2,3.98356507399999));
#335650=CARTESIAN_POINT('Ctrl Pts',(1.62952046699994,2.2,3.98356507399999));
#335651=CARTESIAN_POINT('Ctrl Pts',(1.62825881599994,12.2,3.98226332299998));
#335652=CARTESIAN_POINT('Ctrl Pts',(1.62825881599994,5.2,3.98226332299998));
#335653=CARTESIAN_POINT('Ctrl Pts',(1.62825881599994,2.2,3.98226332299998));
#335654=CARTESIAN_POINT('Ctrl Pts',(1.62700162999994,12.2,3.98096323799999));
#335655=CARTESIAN_POINT('Ctrl Pts',(1.62700162999994,5.2,3.98096323799999));
#335656=CARTESIAN_POINT('Ctrl Pts',(1.62700162999994,2.2,3.98096323799999));
#335657=CARTESIAN_POINT('Ctrl Pts',(1.62574890899994,12.2,3.97966483299999));
#335658=CARTESIAN_POINT('Ctrl Pts',(1.62574890899994,5.2,3.97966483299999));
#335659=CARTESIAN_POINT('Ctrl Pts',(1.62574890899994,2.2,3.97966483299999));
#335660=CARTESIAN_POINT('Ctrl Pts',(1.62450065199994,12.2,3.97836811799999));
#335661=CARTESIAN_POINT('Ctrl Pts',(1.62450065199994,5.2,3.97836811799999));
#335662=CARTESIAN_POINT('Ctrl Pts',(1.62450065199994,2.2,3.97836811799999));
#335663=CARTESIAN_POINT('Ctrl Pts',(1.62325685899994,12.2,3.97707310499998));
#335664=CARTESIAN_POINT('Ctrl Pts',(1.62325685899994,5.2,3.97707310499998));
#335665=CARTESIAN_POINT('Ctrl Pts',(1.62325685899994,2.2,3.97707310499998));
#335666=CARTESIAN_POINT('Ctrl Pts',(1.62201752599994,12.2,3.97577980599999));
#335667=CARTESIAN_POINT('Ctrl Pts',(1.62201752599994,5.2,3.97577980599999));
#335668=CARTESIAN_POINT('Ctrl Pts',(1.62201752599994,2.2,3.97577980599999));
#335669=CARTESIAN_POINT('Ctrl Pts',(1.62078265399994,12.2,3.97448823299998));
#335670=CARTESIAN_POINT('Ctrl Pts',(1.62078265399994,5.2,3.97448823299998));
#335671=CARTESIAN_POINT('Ctrl Pts',(1.62078265399994,2.2,3.97448823299998));
#335672=CARTESIAN_POINT('Ctrl Pts',(1.61955224199994,12.2,3.97319839699998));
#335673=CARTESIAN_POINT('Ctrl Pts',(1.61955224199994,5.2,3.97319839699998));
#335674=CARTESIAN_POINT('Ctrl Pts',(1.61955224199994,2.2,3.97319839699998));
#335675=CARTESIAN_POINT('Ctrl Pts',(1.61832628899994,12.2,3.97191031099998));
#335676=CARTESIAN_POINT('Ctrl Pts',(1.61832628899994,5.2,3.97191031099998));
#335677=CARTESIAN_POINT('Ctrl Pts',(1.61832628899994,2.2,3.97191031099998));
#335678=CARTESIAN_POINT('Ctrl Pts',(1.61710479299994,12.2,3.97062398599999));
#335679=CARTESIAN_POINT('Ctrl Pts',(1.61710479299994,5.2,3.97062398599999));
#335680=CARTESIAN_POINT('Ctrl Pts',(1.61710479299994,2.2,3.97062398599999));
#335681=CARTESIAN_POINT('Ctrl Pts',(1.61588775399994,12.2,3.96933943399999));
#335682=CARTESIAN_POINT('Ctrl Pts',(1.61588775399994,5.2,3.96933943399999));
#335683=CARTESIAN_POINT('Ctrl Pts',(1.61588775399994,2.2,3.96933943399999));
#335684=CARTESIAN_POINT('Ctrl Pts',(1.61467517099994,12.2,3.96805666699999));
#335685=CARTESIAN_POINT('Ctrl Pts',(1.61467517099994,5.2,3.96805666699999));
#335686=CARTESIAN_POINT('Ctrl Pts',(1.61467517099994,2.2,3.96805666699999));
#335687=CARTESIAN_POINT('Ctrl Pts',(1.61346704099994,12.2,3.96677569699998));
#335688=CARTESIAN_POINT('Ctrl Pts',(1.61346704099994,5.2,3.96677569699998));
#335689=CARTESIAN_POINT('Ctrl Pts',(1.61346704099994,2.2,3.96677569699998));
#335690=CARTESIAN_POINT('Ctrl Pts',(1.61226336499994,12.2,3.96549653599998));
#335691=CARTESIAN_POINT('Ctrl Pts',(1.61226336499994,5.2,3.96549653599998));
#335692=CARTESIAN_POINT('Ctrl Pts',(1.61226336499994,2.2,3.96549653599998));
#335693=CARTESIAN_POINT('Ctrl Pts',(1.61106413999994,12.2,3.96421919499998));
#335694=CARTESIAN_POINT('Ctrl Pts',(1.61106413999994,5.2,3.96421919499998));
#335695=CARTESIAN_POINT('Ctrl Pts',(1.61106413999994,2.2,3.96421919499998));
#335696=CARTESIAN_POINT('Ctrl Pts',(1.60986936499994,12.2,3.96294368699999));
#335697=CARTESIAN_POINT('Ctrl Pts',(1.60986936499994,5.2,3.96294368699999));
#335698=CARTESIAN_POINT('Ctrl Pts',(1.60986936499994,2.2,3.96294368699999));
#335699=CARTESIAN_POINT('Ctrl Pts',(1.60867904099994,12.2,3.96167002399999));
#335700=CARTESIAN_POINT('Ctrl Pts',(1.60867904099994,5.2,3.96167002399999));
#335701=CARTESIAN_POINT('Ctrl Pts',(1.60867904099994,2.2,3.96167002399999));
#335702=CARTESIAN_POINT('Ctrl Pts',(1.60749316499994,12.2,3.96039821699999));
#335703=CARTESIAN_POINT('Ctrl Pts',(1.60749316499994,5.2,3.96039821699999));
#335704=CARTESIAN_POINT('Ctrl Pts',(1.60749316499994,2.2,3.96039821699999));
#335705=CARTESIAN_POINT('Ctrl Pts',(1.60631173599994,12.2,3.95912827899998));
#335706=CARTESIAN_POINT('Ctrl Pts',(1.60631173599994,5.2,3.95912827899998));
#335707=CARTESIAN_POINT('Ctrl Pts',(1.60631173599994,2.2,3.95912827899998));
#335708=CARTESIAN_POINT('Ctrl Pts',(1.60513475099994,12.2,3.95786022099998));
#335709=CARTESIAN_POINT('Ctrl Pts',(1.60513475099994,5.2,3.95786022099998));
#335710=CARTESIAN_POINT('Ctrl Pts',(1.60513475099994,2.2,3.95786022099998));
#335711=CARTESIAN_POINT('Ctrl Pts',(1.60396221199994,12.2,3.95659405699998));
#335712=CARTESIAN_POINT('Ctrl Pts',(1.60396221199994,5.2,3.95659405699998));
#335713=CARTESIAN_POINT('Ctrl Pts',(1.60396221199994,2.2,3.95659405699998));
#335714=CARTESIAN_POINT('Ctrl Pts',(1.60279411499994,12.2,3.95532979699999));
#335715=CARTESIAN_POINT('Ctrl Pts',(1.60279411499994,5.2,3.95532979699999));
#335716=CARTESIAN_POINT('Ctrl Pts',(1.60279411499994,2.2,3.95532979699999));
#335717=CARTESIAN_POINT('Ctrl Pts',(1.60163045999994,12.2,3.95406745399999));
#335718=CARTESIAN_POINT('Ctrl Pts',(1.60163045999994,5.2,3.95406745399999));
#335719=CARTESIAN_POINT('Ctrl Pts',(1.60163045999994,2.2,3.95406745399999));
#335720=CARTESIAN_POINT('Ctrl Pts',(1.60047124599994,12.2,3.95280703999998));
#335721=CARTESIAN_POINT('Ctrl Pts',(1.60047124599994,5.2,3.95280703999998));
#335722=CARTESIAN_POINT('Ctrl Pts',(1.60047124599994,2.2,3.95280703999998));
#335723=CARTESIAN_POINT('Ctrl Pts',(1.59931646999994,12.2,3.95154856899998));
#335724=CARTESIAN_POINT('Ctrl Pts',(1.59931646999994,5.2,3.95154856899998));
#335725=CARTESIAN_POINT('Ctrl Pts',(1.59931646999994,2.2,3.95154856899998));
#335726=CARTESIAN_POINT('Ctrl Pts',(1.59816613199994,12.2,3.95029204999998));
#335727=CARTESIAN_POINT('Ctrl Pts',(1.59816613199994,5.2,3.95029204999998));
#335728=CARTESIAN_POINT('Ctrl Pts',(1.59816613199994,2.2,3.95029204999998));
#335729=CARTESIAN_POINT('Ctrl Pts',(1.59702023099994,12.2,3.94903749599998));
#335730=CARTESIAN_POINT('Ctrl Pts',(1.59702023099994,5.2,3.94903749599998));
#335731=CARTESIAN_POINT('Ctrl Pts',(1.59702023099994,2.2,3.94903749599998));
#335732=CARTESIAN_POINT('Ctrl Pts',(1.59587876399994,12.2,3.94778491999999));
#335733=CARTESIAN_POINT('Ctrl Pts',(1.59587876399994,5.2,3.94778491999999));
#335734=CARTESIAN_POINT('Ctrl Pts',(1.59587876399994,2.2,3.94778491999999));
#335735=CARTESIAN_POINT('Ctrl Pts',(1.59474173099994,12.2,3.94653433399998));
#335736=CARTESIAN_POINT('Ctrl Pts',(1.59474173099994,5.2,3.94653433399998));
#335737=CARTESIAN_POINT('Ctrl Pts',(1.59474173099994,2.2,3.94653433399998));
#335738=CARTESIAN_POINT('Ctrl Pts',(1.59360912799994,12.2,3.94528574999998));
#335739=CARTESIAN_POINT('Ctrl Pts',(1.59360912799994,5.2,3.94528574999998));
#335740=CARTESIAN_POINT('Ctrl Pts',(1.59360912799994,2.2,3.94528574999998));
#335741=CARTESIAN_POINT('Ctrl Pts',(1.59248095699994,12.2,3.94403918099999));
#335742=CARTESIAN_POINT('Ctrl Pts',(1.59248095699994,5.2,3.94403918099999));
#335743=CARTESIAN_POINT('Ctrl Pts',(1.59248095699994,2.2,3.94403918099999));
#335744=CARTESIAN_POINT('Ctrl Pts',(1.59135721499994,12.2,3.94279463799998));
#335745=CARTESIAN_POINT('Ctrl Pts',(1.59135721499994,5.2,3.94279463799998));
#335746=CARTESIAN_POINT('Ctrl Pts',(1.59135721499994,2.2,3.94279463799998));
#335747=CARTESIAN_POINT('Ctrl Pts',(1.59023789999994,12.2,3.94155213499998));
#335748=CARTESIAN_POINT('Ctrl Pts',(1.59023789999994,5.2,3.94155213499998));
#335749=CARTESIAN_POINT('Ctrl Pts',(1.59023789999994,2.2,3.94155213499998));
#335750=CARTESIAN_POINT('Ctrl Pts',(1.58912301099994,12.2,3.94031168199999));
#335751=CARTESIAN_POINT('Ctrl Pts',(1.58912301099994,5.2,3.94031168199999));
#335752=CARTESIAN_POINT('Ctrl Pts',(1.58912301099994,2.2,3.94031168199999));
#335753=CARTESIAN_POINT('Ctrl Pts',(1.58801254499994,12.2,3.93907329399998));
#335754=CARTESIAN_POINT('Ctrl Pts',(1.58801254499994,5.2,3.93907329399998));
#335755=CARTESIAN_POINT('Ctrl Pts',(1.58801254499994,2.2,3.93907329399998));
#335756=CARTESIAN_POINT('Ctrl Pts',(1.58690650299994,12.2,3.93783698099998));
#335757=CARTESIAN_POINT('Ctrl Pts',(1.58690650299994,5.2,3.93783698099998));
#335758=CARTESIAN_POINT('Ctrl Pts',(1.58690650299994,2.2,3.93783698099998));
#335759=CARTESIAN_POINT('Ctrl Pts',(1.58580488199994,12.2,3.93660275799999));
#335760=CARTESIAN_POINT('Ctrl Pts',(1.58580488199994,5.2,3.93660275799999));
#335761=CARTESIAN_POINT('Ctrl Pts',(1.58580488199994,2.2,3.93660275799999));
#335762=CARTESIAN_POINT('Ctrl Pts',(1.58470767999994,12.2,3.93537063399998));
#335763=CARTESIAN_POINT('Ctrl Pts',(1.58470767999994,5.2,3.93537063399998));
#335764=CARTESIAN_POINT('Ctrl Pts',(1.58470767999994,2.2,3.93537063399998));
#335765=CARTESIAN_POINT('Ctrl Pts',(1.58361489599994,12.2,3.93414062499998));
#335766=CARTESIAN_POINT('Ctrl Pts',(1.58361489599994,5.2,3.93414062499998));
#335767=CARTESIAN_POINT('Ctrl Pts',(1.58361489599994,2.2,3.93414062499998));
#335768=CARTESIAN_POINT('Ctrl Pts',(1.58252652799994,12.2,3.93291274099998));
#335769=CARTESIAN_POINT('Ctrl Pts',(1.58252652799994,5.2,3.93291274099998));
#335770=CARTESIAN_POINT('Ctrl Pts',(1.58252652799994,2.2,3.93291274099998));
#335771=CARTESIAN_POINT('Ctrl Pts',(1.58144257399994,12.2,3.93168699499999));
#335772=CARTESIAN_POINT('Ctrl Pts',(1.58144257399994,5.2,3.93168699499999));
#335773=CARTESIAN_POINT('Ctrl Pts',(1.58144257399994,2.2,3.93168699499999));
#335774=CARTESIAN_POINT('Ctrl Pts',(1.58036303299994,12.2,3.93046339999999));
#335775=CARTESIAN_POINT('Ctrl Pts',(1.58036303299994,5.2,3.93046339999999));
#335776=CARTESIAN_POINT('Ctrl Pts',(1.58036303299994,2.2,3.93046339999999));
#335777=CARTESIAN_POINT('Ctrl Pts',(1.57928790399994,12.2,3.92924196799999));
#335778=CARTESIAN_POINT('Ctrl Pts',(1.57928790399994,5.2,3.92924196799999));
#335779=CARTESIAN_POINT('Ctrl Pts',(1.57928790399994,2.2,3.92924196799999));
#335780=CARTESIAN_POINT('Ctrl Pts',(1.57821718299994,12.2,3.92802271199999));
#335781=CARTESIAN_POINT('Ctrl Pts',(1.57821718299994,5.2,3.92802271199999));
#335782=CARTESIAN_POINT('Ctrl Pts',(1.57821718299994,2.2,3.92802271199999));
#335783=CARTESIAN_POINT('Ctrl Pts',(1.57715086999994,12.2,3.92680564399999));
#335784=CARTESIAN_POINT('Ctrl Pts',(1.57715086999994,5.2,3.92680564399999));
#335785=CARTESIAN_POINT('Ctrl Pts',(1.57715086999994,2.2,3.92680564399999));
#335786=CARTESIAN_POINT('Ctrl Pts',(1.57608896299994,12.2,3.92559077799999));
#335787=CARTESIAN_POINT('Ctrl Pts',(1.57608896299994,5.2,3.92559077799999));
#335788=CARTESIAN_POINT('Ctrl Pts',(1.57608896299994,2.2,3.92559077799999));
#335789=CARTESIAN_POINT('Ctrl Pts',(1.57503145999994,12.2,3.92437812499999));
#335790=CARTESIAN_POINT('Ctrl Pts',(1.57503145999994,5.2,3.92437812499999));
#335791=CARTESIAN_POINT('Ctrl Pts',(1.57503145999994,2.2,3.92437812499999));
#335792=CARTESIAN_POINT('Ctrl Pts',(1.57397835999994,12.2,3.92316769799999));
#335793=CARTESIAN_POINT('Ctrl Pts',(1.57397835999994,5.2,3.92316769799999));
#335794=CARTESIAN_POINT('Ctrl Pts',(1.57397835999994,2.2,3.92316769799999));
#335795=CARTESIAN_POINT('Ctrl Pts',(1.57292965799994,12.2,3.92195950899998));
#335796=CARTESIAN_POINT('Ctrl Pts',(1.57292965799994,5.2,3.92195950899998));
#335797=CARTESIAN_POINT('Ctrl Pts',(1.57292965799994,2.2,3.92195950899998));
#335798=CARTESIAN_POINT('Ctrl Pts',(1.57188535699994,12.2,3.92075357199998));
#335799=CARTESIAN_POINT('Ctrl Pts',(1.57188535699994,5.2,3.92075357199998));
#335800=CARTESIAN_POINT('Ctrl Pts',(1.57188535699994,2.2,3.92075357199998));
#335801=CARTESIAN_POINT('Ctrl Pts',(1.57084544999994,12.2,3.91954989899999));
#335802=CARTESIAN_POINT('Ctrl Pts',(1.57084544999994,5.2,3.91954989899999));
#335803=CARTESIAN_POINT('Ctrl Pts',(1.57084544999994,2.2,3.91954989899999));
#335804=CARTESIAN_POINT('Ctrl Pts',(1.56980993999994,12.2,3.91834850299999));
#335805=CARTESIAN_POINT('Ctrl Pts',(1.56980993999994,5.2,3.91834850299999));
#335806=CARTESIAN_POINT('Ctrl Pts',(1.56980993999994,2.2,3.91834850299999));
#335807=CARTESIAN_POINT('Ctrl Pts',(1.56877882099994,12.2,3.91714939699998));
#335808=CARTESIAN_POINT('Ctrl Pts',(1.56877882099994,5.2,3.91714939699998));
#335809=CARTESIAN_POINT('Ctrl Pts',(1.56877882099994,2.2,3.91714939699998));
#335810=CARTESIAN_POINT('Ctrl Pts',(1.56775209299994,12.2,3.91595259199998));
#335811=CARTESIAN_POINT('Ctrl Pts',(1.56775209299994,5.2,3.91595259199998));
#335812=CARTESIAN_POINT('Ctrl Pts',(1.56775209299994,2.2,3.91595259199998));
#335813=CARTESIAN_POINT('Ctrl Pts',(1.56672975399994,12.2,3.91475810299998));
#335814=CARTESIAN_POINT('Ctrl Pts',(1.56672975399994,5.2,3.91475810299998));
#335815=CARTESIAN_POINT('Ctrl Pts',(1.56672975399994,2.2,3.91475810299998));
#335816=CARTESIAN_POINT('Ctrl Pts',(1.56571180199994,12.2,3.91356594199999));
#335817=CARTESIAN_POINT('Ctrl Pts',(1.56571180199994,5.2,3.91356594199999));
#335818=CARTESIAN_POINT('Ctrl Pts',(1.56571180199994,2.2,3.91356594199999));
#335819=CARTESIAN_POINT('Ctrl Pts',(1.56469823499994,12.2,3.91237612099999));
#335820=CARTESIAN_POINT('Ctrl Pts',(1.56469823499994,5.2,3.91237612099999));
#335821=CARTESIAN_POINT('Ctrl Pts',(1.56469823499994,2.2,3.91237612099999));
#335822=CARTESIAN_POINT('Ctrl Pts',(1.56368904999994,12.2,3.91118865499998));
#335823=CARTESIAN_POINT('Ctrl Pts',(1.56368904999994,5.2,3.91118865499998));
#335824=CARTESIAN_POINT('Ctrl Pts',(1.56368904999994,2.2,3.91118865499998));
#335825=CARTESIAN_POINT('Ctrl Pts',(1.56268424599994,12.2,3.91000355399999));
#335826=CARTESIAN_POINT('Ctrl Pts',(1.56268424599994,5.2,3.91000355399999));
#335827=CARTESIAN_POINT('Ctrl Pts',(1.56268424599994,2.2,3.91000355399999));
#335828=CARTESIAN_POINT('Ctrl Pts',(1.56168382199994,12.2,3.90882083299999));
#335829=CARTESIAN_POINT('Ctrl Pts',(1.56168382199994,5.2,3.90882083299999));
#335830=CARTESIAN_POINT('Ctrl Pts',(1.56168382199994,2.2,3.90882083299999));
#335831=CARTESIAN_POINT('Ctrl Pts',(1.56068777299994,12.2,3.90764050399999));
#335832=CARTESIAN_POINT('Ctrl Pts',(1.56068777299994,5.2,3.90764050399999));
#335833=CARTESIAN_POINT('Ctrl Pts',(1.56068777299994,2.2,3.90764050399999));
#335834=CARTESIAN_POINT('Ctrl Pts',(1.55969609799994,12.2,3.90646258099999));
#335835=CARTESIAN_POINT('Ctrl Pts',(1.55969609799994,5.2,3.90646258099999));
#335836=CARTESIAN_POINT('Ctrl Pts',(1.55969609799994,2.2,3.90646258099999));
#335837=CARTESIAN_POINT('Ctrl Pts',(1.55870879599994,12.2,3.90528707499998));
#335838=CARTESIAN_POINT('Ctrl Pts',(1.55870879599994,5.2,3.90528707499998));
#335839=CARTESIAN_POINT('Ctrl Pts',(1.55870879599994,2.2,3.90528707499998));
#335840=CARTESIAN_POINT('Ctrl Pts',(1.55772586499994,12.2,3.90411400099998));
#335841=CARTESIAN_POINT('Ctrl Pts',(1.55772586499994,5.2,3.90411400099998));
#335842=CARTESIAN_POINT('Ctrl Pts',(1.55772586499994,2.2,3.90411400099998));
#335843=CARTESIAN_POINT('Ctrl Pts',(1.55674730099994,12.2,3.90294336899998));
#335844=CARTESIAN_POINT('Ctrl Pts',(1.55674730099994,5.2,3.90294336899998));
#335845=CARTESIAN_POINT('Ctrl Pts',(1.55674730099994,2.2,3.90294336899998));
#335846=CARTESIAN_POINT('Ctrl Pts',(1.55577310299994,12.2,3.90177519699999));
#335847=CARTESIAN_POINT('Ctrl Pts',(1.55577310299994,5.2,3.90177519699999));
#335848=CARTESIAN_POINT('Ctrl Pts',(1.55577310299994,2.2,3.90177519699999));
#335849=CARTESIAN_POINT('Ctrl Pts',(1.55480326799994,12.2,3.90060949299999));
#335850=CARTESIAN_POINT('Ctrl Pts',(1.55480326799994,5.2,3.90060949299999));
#335851=CARTESIAN_POINT('Ctrl Pts',(1.55480326799994,2.2,3.90060949299999));
#335852=CARTESIAN_POINT('Ctrl Pts',(1.55383779599994,12.2,3.89944627299998));
#335853=CARTESIAN_POINT('Ctrl Pts',(1.55383779599994,5.2,3.89944627299998));
#335854=CARTESIAN_POINT('Ctrl Pts',(1.55383779599994,2.2,3.89944627299998));
#335855=CARTESIAN_POINT('Ctrl Pts',(1.55287668099994,12.2,3.89828554999998));
#335856=CARTESIAN_POINT('Ctrl Pts',(1.55287668099994,5.2,3.89828554999998));
#335857=CARTESIAN_POINT('Ctrl Pts',(1.55287668099994,2.2,3.89828554999998));
#335858=CARTESIAN_POINT('Ctrl Pts',(1.55191992399994,12.2,3.89712733499999));
#335859=CARTESIAN_POINT('Ctrl Pts',(1.55191992399994,5.2,3.89712733499999));
#335860=CARTESIAN_POINT('Ctrl Pts',(1.55191992399994,2.2,3.89712733499999));
#335861=CARTESIAN_POINT('Ctrl Pts',(1.55096752099994,12.2,3.89597164399999));
#335862=CARTESIAN_POINT('Ctrl Pts',(1.55096752099994,5.2,3.89597164399999));
#335863=CARTESIAN_POINT('Ctrl Pts',(1.55096752099994,2.2,3.89597164399999));
#335864=CARTESIAN_POINT('Ctrl Pts',(1.55001946899994,12.2,3.89481848799999));
#335865=CARTESIAN_POINT('Ctrl Pts',(1.55001946899994,5.2,3.89481848799999));
#335866=CARTESIAN_POINT('Ctrl Pts',(1.55001946899994,2.2,3.89481848799999));
#335867=CARTESIAN_POINT('Ctrl Pts',(1.54907576899994,12.2,3.89366788099998));
#335868=CARTESIAN_POINT('Ctrl Pts',(1.54907576899994,5.2,3.89366788099998));
#335869=CARTESIAN_POINT('Ctrl Pts',(1.54907576899994,2.2,3.89366788099998));
#335870=CARTESIAN_POINT('Ctrl Pts',(1.54813641499994,12.2,3.89251983599999));
#335871=CARTESIAN_POINT('Ctrl Pts',(1.54813641499994,5.2,3.89251983599999));
#335872=CARTESIAN_POINT('Ctrl Pts',(1.54813641499994,2.2,3.89251983599999));
#335873=CARTESIAN_POINT('Ctrl Pts',(1.54720140599994,12.2,3.89137436699999));
#335874=CARTESIAN_POINT('Ctrl Pts',(1.54720140599994,5.2,3.89137436699999));
#335875=CARTESIAN_POINT('Ctrl Pts',(1.54720140599994,2.2,3.89137436699999));
#335876=CARTESIAN_POINT('Ctrl Pts',(1.54627073899994,12.2,3.89023148599998));
#335877=CARTESIAN_POINT('Ctrl Pts',(1.54627073899994,5.2,3.89023148599998));
#335878=CARTESIAN_POINT('Ctrl Pts',(1.54627073899994,2.2,3.89023148599998));
#335879=CARTESIAN_POINT('Ctrl Pts',(1.54534441299994,12.2,3.88909120699999));
#335880=CARTESIAN_POINT('Ctrl Pts',(1.54534441299994,5.2,3.88909120699999));
#335881=CARTESIAN_POINT('Ctrl Pts',(1.54534441299994,2.2,3.88909120699999));
#335882=CARTESIAN_POINT('Ctrl Pts',(1.54442242499994,12.2,3.88795354299998));
#335883=CARTESIAN_POINT('Ctrl Pts',(1.54442242499994,5.2,3.88795354299998));
#335884=CARTESIAN_POINT('Ctrl Pts',(1.54442242499994,2.2,3.88795354299998));
#335885=CARTESIAN_POINT('Ctrl Pts',(1.54350476999994,12.2,3.88681850799999));
#335886=CARTESIAN_POINT('Ctrl Pts',(1.54350476999994,5.2,3.88681850799999));
#335887=CARTESIAN_POINT('Ctrl Pts',(1.54350476999994,2.2,3.88681850799999));
#335888=CARTESIAN_POINT('Ctrl Pts',(1.54259144899994,12.2,3.88568611499998));
#335889=CARTESIAN_POINT('Ctrl Pts',(1.54259144899994,5.2,3.88568611499998));
#335890=CARTESIAN_POINT('Ctrl Pts',(1.54259144899994,2.2,3.88568611499998));
#335891=CARTESIAN_POINT('Ctrl Pts',(1.54168245899994,12.2,3.88455637699998));
#335892=CARTESIAN_POINT('Ctrl Pts',(1.54168245899994,5.2,3.88455637699998));
#335893=CARTESIAN_POINT('Ctrl Pts',(1.54168245899994,2.2,3.88455637699998));
#335894=CARTESIAN_POINT('Ctrl Pts',(1.54077779499994,12.2,3.88342930899999));
#335895=CARTESIAN_POINT('Ctrl Pts',(1.54077779499994,5.2,3.88342930899999));
#335896=CARTESIAN_POINT('Ctrl Pts',(1.54077779499994,2.2,3.88342930899999));
#335897=CARTESIAN_POINT('Ctrl Pts',(1.53987745599994,12.2,3.88230492199998));
#335898=CARTESIAN_POINT('Ctrl Pts',(1.53987745599994,5.2,3.88230492199998));
#335899=CARTESIAN_POINT('Ctrl Pts',(1.53987745599994,2.2,3.88230492199998));
#335900=CARTESIAN_POINT('Ctrl Pts',(1.53898143999994,12.2,3.88118322999999));
#335901=CARTESIAN_POINT('Ctrl Pts',(1.53898143999994,5.2,3.88118322999999));
#335902=CARTESIAN_POINT('Ctrl Pts',(1.53898143999994,2.2,3.88118322999999));
#335903=CARTESIAN_POINT('Ctrl Pts',(1.53808974299994,12.2,3.88006424799999));
#335904=CARTESIAN_POINT('Ctrl Pts',(1.53808974299994,5.2,3.88006424799999));
#335905=CARTESIAN_POINT('Ctrl Pts',(1.53808974299994,2.2,3.88006424799999));
#335906=CARTESIAN_POINT('Ctrl Pts',(1.53720236299994,12.2,3.87894798699998));
#335907=CARTESIAN_POINT('Ctrl Pts',(1.53720236299994,5.2,3.87894798699998));
#335908=CARTESIAN_POINT('Ctrl Pts',(1.53720236299994,2.2,3.87894798699998));
#335909=CARTESIAN_POINT('Ctrl Pts',(1.53631929799994,12.2,3.87783446399999));
#335910=CARTESIAN_POINT('Ctrl Pts',(1.53631929799994,5.2,3.87783446399999));
#335911=CARTESIAN_POINT('Ctrl Pts',(1.53631929799994,2.2,3.87783446399999));
#335912=CARTESIAN_POINT('Ctrl Pts',(1.53544054399994,12.2,3.87672368899998));
#335913=CARTESIAN_POINT('Ctrl Pts',(1.53544054399994,5.2,3.87672368899998));
#335914=CARTESIAN_POINT('Ctrl Pts',(1.53544054399994,2.2,3.87672368899998));
#335915=CARTESIAN_POINT('Ctrl Pts',(1.53456609999994,12.2,3.87561567799998));
#335916=CARTESIAN_POINT('Ctrl Pts',(1.53456609999994,5.2,3.87561567799998));
#335917=CARTESIAN_POINT('Ctrl Pts',(1.53456609999994,2.2,3.87561567799998));
#335918=CARTESIAN_POINT('Ctrl Pts',(1.53369595999994,12.2,3.87451044399998));
#335919=CARTESIAN_POINT('Ctrl Pts',(1.53369595999994,5.2,3.87451044399998));
#335920=CARTESIAN_POINT('Ctrl Pts',(1.53369595999994,2.2,3.87451044399998));
#335921=CARTESIAN_POINT('Ctrl Pts',(1.53283012499994,12.2,3.87340800099999));
#335922=CARTESIAN_POINT('Ctrl Pts',(1.53283012499994,5.2,3.87340800099999));
#335923=CARTESIAN_POINT('Ctrl Pts',(1.53283012499994,2.2,3.87340800099999));
#335924=CARTESIAN_POINT('Ctrl Pts',(1.53196858999994,12.2,3.87230836099998));
#335925=CARTESIAN_POINT('Ctrl Pts',(1.53196858999994,5.2,3.87230836099998));
#335926=CARTESIAN_POINT('Ctrl Pts',(1.53196858999994,2.2,3.87230836099998));
#335927=CARTESIAN_POINT('Ctrl Pts',(1.53111135299994,12.2,3.87121153899999));
#335928=CARTESIAN_POINT('Ctrl Pts',(1.53111135299994,5.2,3.87121153899999));
#335929=CARTESIAN_POINT('Ctrl Pts',(1.53111135299994,2.2,3.87121153899999));
#335930=CARTESIAN_POINT('Ctrl Pts',(1.53025841199994,12.2,3.87011754799998));
#335931=CARTESIAN_POINT('Ctrl Pts',(1.53025841199994,5.2,3.87011754799998));
#335932=CARTESIAN_POINT('Ctrl Pts',(1.53025841199994,2.2,3.87011754799998));
#335933=CARTESIAN_POINT('Ctrl Pts',(1.52940976199994,12.2,3.86902640299999));
#335934=CARTESIAN_POINT('Ctrl Pts',(1.52940976199994,5.2,3.86902640299999));
#335935=CARTESIAN_POINT('Ctrl Pts',(1.52940976199994,2.2,3.86902640299999));
#335936=CARTESIAN_POINT('Ctrl Pts',(1.52856539999994,12.2,3.86793811599999));
#335937=CARTESIAN_POINT('Ctrl Pts',(1.52856539999994,5.2,3.86793811599999));
#335938=CARTESIAN_POINT('Ctrl Pts',(1.52856539999994,2.2,3.86793811599999));
#335939=CARTESIAN_POINT('Ctrl Pts',(1.52772532599994,12.2,3.86685270299999));
#335940=CARTESIAN_POINT('Ctrl Pts',(1.52772532599994,5.2,3.86685270299999));
#335941=CARTESIAN_POINT('Ctrl Pts',(1.52772532599994,2.2,3.86685270299999));
#335942=CARTESIAN_POINT('Ctrl Pts',(1.52688953499994,12.2,3.86577017499998));
#335943=CARTESIAN_POINT('Ctrl Pts',(1.52688953499994,5.2,3.86577017499998));
#335944=CARTESIAN_POINT('Ctrl Pts',(1.52688953499994,2.2,3.86577017499998));
#335945=CARTESIAN_POINT('Ctrl Pts',(1.52605802399994,12.2,3.86469054799999));
#335946=CARTESIAN_POINT('Ctrl Pts',(1.52605802399994,5.2,3.86469054799999));
#335947=CARTESIAN_POINT('Ctrl Pts',(1.52605802399994,2.2,3.86469054799999));
#335948=CARTESIAN_POINT('Ctrl Pts',(1.52523078999994,12.2,3.86361383599999));
#335949=CARTESIAN_POINT('Ctrl Pts',(1.52523078999994,5.2,3.86361383599999));
#335950=CARTESIAN_POINT('Ctrl Pts',(1.52523078999994,2.2,3.86361383599999));
#335951=CARTESIAN_POINT('Ctrl Pts',(1.52440782999994,12.2,3.86254005099998));
#335952=CARTESIAN_POINT('Ctrl Pts',(1.52440782999994,5.2,3.86254005099998));
#335953=CARTESIAN_POINT('Ctrl Pts',(1.52440782999994,2.2,3.86254005099998));
#335954=CARTESIAN_POINT('Ctrl Pts',(1.52358914199994,12.2,3.86146920799998));
#335955=CARTESIAN_POINT('Ctrl Pts',(1.52358914199994,5.2,3.86146920799998));
#335956=CARTESIAN_POINT('Ctrl Pts',(1.52358914199994,2.2,3.86146920799998));
#335957=CARTESIAN_POINT('Ctrl Pts',(1.52277472299994,12.2,3.86040132099998));
#335958=CARTESIAN_POINT('Ctrl Pts',(1.52277472299994,5.2,3.86040132099998));
#335959=CARTESIAN_POINT('Ctrl Pts',(1.52277472299994,2.2,3.86040132099998));
#335960=CARTESIAN_POINT('Ctrl Pts',(1.52196456699994,12.2,3.85933640399998));
#335961=CARTESIAN_POINT('Ctrl Pts',(1.52196456699994,5.2,3.85933640399998));
#335962=CARTESIAN_POINT('Ctrl Pts',(1.52196456699994,2.2,3.85933640399998));
#335963=CARTESIAN_POINT('Ctrl Pts',(1.52115867499994,12.2,3.85827446999999));
#335964=CARTESIAN_POINT('Ctrl Pts',(1.52115867499994,5.2,3.85827446999999));
#335965=CARTESIAN_POINT('Ctrl Pts',(1.52115867499994,2.2,3.85827446999999));
#335966=CARTESIAN_POINT('Ctrl Pts',(1.52035704199994,12.2,3.85721553499998));
#335967=CARTESIAN_POINT('Ctrl Pts',(1.52035704199994,5.2,3.85721553499998));
#335968=CARTESIAN_POINT('Ctrl Pts',(1.52035704199994,2.2,3.85721553499998));
#335969=CARTESIAN_POINT('Ctrl Pts',(1.51955966299994,12.2,3.85615961099998));
#335970=CARTESIAN_POINT('Ctrl Pts',(1.51955966299994,5.2,3.85615961099998));
#335971=CARTESIAN_POINT('Ctrl Pts',(1.51955966299994,2.2,3.85615961099998));
#335972=CARTESIAN_POINT('Ctrl Pts',(1.51876653699994,12.2,3.85510671399998));
#335973=CARTESIAN_POINT('Ctrl Pts',(1.51876653699994,5.2,3.85510671399998));
#335974=CARTESIAN_POINT('Ctrl Pts',(1.51876653699994,2.2,3.85510671399998));
#335975=CARTESIAN_POINT('Ctrl Pts',(1.51797765999994,12.2,3.85405685599999));
#335976=CARTESIAN_POINT('Ctrl Pts',(1.51797765999994,5.2,3.85405685599999));
#335977=CARTESIAN_POINT('Ctrl Pts',(1.51797765999994,2.2,3.85405685599999));
#335978=CARTESIAN_POINT('Ctrl Pts',(1.51719302999994,12.2,3.85301005199998));
#335979=CARTESIAN_POINT('Ctrl Pts',(1.51719302999994,5.2,3.85301005199998));
#335980=CARTESIAN_POINT('Ctrl Pts',(1.51719302999994,2.2,3.85301005199998));
#335981=CARTESIAN_POINT('Ctrl Pts',(1.51641264299994,12.2,3.85196631599998));
#335982=CARTESIAN_POINT('Ctrl Pts',(1.51641264299994,5.2,3.85196631599998));
#335983=CARTESIAN_POINT('Ctrl Pts',(1.51641264299994,2.2,3.85196631599998));
#335984=CARTESIAN_POINT('Ctrl Pts',(1.51563649399994,12.2,3.85092566399998));
#335985=CARTESIAN_POINT('Ctrl Pts',(1.51563649399994,5.2,3.85092566399998));
#335986=CARTESIAN_POINT('Ctrl Pts',(1.51563649399994,2.2,3.85092566399998));
#335987=CARTESIAN_POINT('Ctrl Pts',(1.51486458299994,12.2,3.84988810699999));
#335988=CARTESIAN_POINT('Ctrl Pts',(1.51486458299994,5.2,3.84988810699999));
#335989=CARTESIAN_POINT('Ctrl Pts',(1.51486458299994,2.2,3.84988810699999));
#335990=CARTESIAN_POINT('Ctrl Pts',(1.51409690299994,12.2,3.84885366199998));
#335991=CARTESIAN_POINT('Ctrl Pts',(1.51409690299994,5.2,3.84885366199998));
#335992=CARTESIAN_POINT('Ctrl Pts',(1.51409690299994,2.2,3.84885366199998));
#335993=CARTESIAN_POINT('Ctrl Pts',(1.51333345399994,12.2,3.84782234099998));
#335994=CARTESIAN_POINT('Ctrl Pts',(1.51333345399994,5.2,3.84782234099998));
#335995=CARTESIAN_POINT('Ctrl Pts',(1.51333345399994,2.2,3.84782234099998));
#335996=CARTESIAN_POINT('Ctrl Pts',(1.51257422899994,12.2,3.84679415999998));
#335997=CARTESIAN_POINT('Ctrl Pts',(1.51257422899994,5.2,3.84679415999998));
#335998=CARTESIAN_POINT('Ctrl Pts',(1.51257422899994,2.2,3.84679415999998));
#335999=CARTESIAN_POINT('Ctrl Pts',(1.51181922799994,12.2,3.84576913299998));
#336000=CARTESIAN_POINT('Ctrl Pts',(1.51181922799994,5.2,3.84576913299998));
#336001=CARTESIAN_POINT('Ctrl Pts',(1.51181922799994,2.2,3.84576913299998));
#336002=CARTESIAN_POINT('Ctrl Pts',(1.51106844599994,12.2,3.84474727399999));
#336003=CARTESIAN_POINT('Ctrl Pts',(1.51106844599994,5.2,3.84474727399999));
#336004=CARTESIAN_POINT('Ctrl Pts',(1.51106844599994,2.2,3.84474727399999));
#336005=CARTESIAN_POINT('Ctrl Pts',(1.51032187999994,12.2,3.84372859599999));
#336006=CARTESIAN_POINT('Ctrl Pts',(1.51032187999994,5.2,3.84372859599999));
#336007=CARTESIAN_POINT('Ctrl Pts',(1.51032187999994,2.2,3.84372859599999));
#336008=CARTESIAN_POINT('Ctrl Pts',(1.50957952599994,12.2,3.84271311599999));
#336009=CARTESIAN_POINT('Ctrl Pts',(1.50957952599994,5.2,3.84271311599999));
#336010=CARTESIAN_POINT('Ctrl Pts',(1.50957952599994,2.2,3.84271311599999));
#336011=CARTESIAN_POINT('Ctrl Pts',(1.50884137999994,12.2,3.84170084599998));
#336012=CARTESIAN_POINT('Ctrl Pts',(1.50884137999994,5.2,3.84170084599998));
#336013=CARTESIAN_POINT('Ctrl Pts',(1.50884137999994,2.2,3.84170084599998));
#336014=CARTESIAN_POINT('Ctrl Pts',(1.50810743899994,12.2,3.84069180299999));
#336015=CARTESIAN_POINT('Ctrl Pts',(1.50810743899994,5.2,3.84069180299999));
#336016=CARTESIAN_POINT('Ctrl Pts',(1.50810743899994,2.2,3.84069180299999));
#336017=CARTESIAN_POINT('Ctrl Pts',(1.50737770099994,12.2,3.83968599899998));
#336018=CARTESIAN_POINT('Ctrl Pts',(1.50737770099994,5.2,3.83968599899998));
#336019=CARTESIAN_POINT('Ctrl Pts',(1.50737770099994,2.2,3.83968599899998));
#336020=CARTESIAN_POINT('Ctrl Pts',(1.50665215899994,12.2,3.83868344999998));
#336021=CARTESIAN_POINT('Ctrl Pts',(1.50665215899994,5.2,3.83868344999998));
#336022=CARTESIAN_POINT('Ctrl Pts',(1.50665215899994,2.2,3.83868344999998));
#336023=CARTESIAN_POINT('Ctrl Pts',(1.50593081299994,12.2,3.83768416999998));
#336024=CARTESIAN_POINT('Ctrl Pts',(1.50593081299994,5.2,3.83768416999998));
#336025=CARTESIAN_POINT('Ctrl Pts',(1.50593081299994,2.2,3.83768416999998));
#336026=CARTESIAN_POINT('Ctrl Pts',(1.50521365599994,12.2,3.83668817499998));
#336027=CARTESIAN_POINT('Ctrl Pts',(1.50521365599994,5.2,3.83668817499998));
#336028=CARTESIAN_POINT('Ctrl Pts',(1.50521365599994,2.2,3.83668817499998));
#336029=CARTESIAN_POINT('Ctrl Pts',(1.50450068699994,12.2,3.83569547699998));
#336030=CARTESIAN_POINT('Ctrl Pts',(1.50450068699994,5.2,3.83569547699998));
#336031=CARTESIAN_POINT('Ctrl Pts',(1.50450068699994,2.2,3.83569547699998));
#336032=CARTESIAN_POINT('Ctrl Pts',(1.50379189999994,12.2,3.83470609099999));
#336033=CARTESIAN_POINT('Ctrl Pts',(1.50379189999994,5.2,3.83470609099999));
#336034=CARTESIAN_POINT('Ctrl Pts',(1.50379189999994,2.2,3.83470609099999));
#336035=CARTESIAN_POINT('Ctrl Pts',(1.50308729399994,12.2,3.83372003399998));
#336036=CARTESIAN_POINT('Ctrl Pts',(1.50308729399994,5.2,3.83372003399998));
#336037=CARTESIAN_POINT('Ctrl Pts',(1.50308729399994,2.2,3.83372003399998));
#336038=CARTESIAN_POINT('Ctrl Pts',(1.50238686199994,12.2,3.83273731799999));
#336039=CARTESIAN_POINT('Ctrl Pts',(1.50238686199994,5.2,3.83273731799999));
#336040=CARTESIAN_POINT('Ctrl Pts',(1.50238686199994,2.2,3.83273731799999));
#336041=CARTESIAN_POINT('Ctrl Pts',(1.50169060299994,12.2,3.83175795899999));
#336042=CARTESIAN_POINT('Ctrl Pts',(1.50169060299994,5.2,3.83175795899999));
#336043=CARTESIAN_POINT('Ctrl Pts',(1.50169060299994,2.2,3.83175795899999));
#336044=CARTESIAN_POINT('Ctrl Pts',(1.50099851099994,12.2,3.83078197199998));
#336045=CARTESIAN_POINT('Ctrl Pts',(1.50099851099994,5.2,3.83078197199998));
#336046=CARTESIAN_POINT('Ctrl Pts',(1.50099851099994,2.2,3.83078197199998));
#336047=CARTESIAN_POINT('Ctrl Pts',(1.50031058399994,12.2,3.82980937199999));
#336048=CARTESIAN_POINT('Ctrl Pts',(1.50031058399994,5.2,3.82980937199999));
#336049=CARTESIAN_POINT('Ctrl Pts',(1.50031058399994,2.2,3.82980937199999));
#336050=CARTESIAN_POINT('Ctrl Pts',(1.49962681699994,12.2,3.82884017099999));
#336051=CARTESIAN_POINT('Ctrl Pts',(1.49962681699994,5.2,3.82884017099999));
#336052=CARTESIAN_POINT('Ctrl Pts',(1.49962681699994,2.2,3.82884017099999));
#336053=CARTESIAN_POINT('Ctrl Pts',(1.49894720599994,12.2,3.82787438799999));
#336054=CARTESIAN_POINT('Ctrl Pts',(1.49894720599994,5.2,3.82787438799999));
#336055=CARTESIAN_POINT('Ctrl Pts',(1.49894720599994,2.2,3.82787438799999));
#336056=CARTESIAN_POINT('Ctrl Pts',(1.49827174799994,12.2,3.82691203499999));
#336057=CARTESIAN_POINT('Ctrl Pts',(1.49827174799994,5.2,3.82691203499999));
#336058=CARTESIAN_POINT('Ctrl Pts',(1.49827174799994,2.2,3.82691203499999));
#336059=CARTESIAN_POINT('Ctrl Pts',(1.49760043799994,12.2,3.82595312699999));
#336060=CARTESIAN_POINT('Ctrl Pts',(1.49760043799994,5.2,3.82595312699999));
#336061=CARTESIAN_POINT('Ctrl Pts',(1.49760043799994,2.2,3.82595312699999));
#336062=CARTESIAN_POINT('Ctrl Pts',(1.49693327199994,12.2,3.82499767999998));
#336063=CARTESIAN_POINT('Ctrl Pts',(1.49693327199994,5.2,3.82499767999998));
#336064=CARTESIAN_POINT('Ctrl Pts',(1.49693327199994,2.2,3.82499767999998));
#336065=CARTESIAN_POINT('Ctrl Pts',(1.49627024699994,12.2,3.82404570799999));
#336066=CARTESIAN_POINT('Ctrl Pts',(1.49627024699994,5.2,3.82404570799999));
#336067=CARTESIAN_POINT('Ctrl Pts',(1.49627024699994,2.2,3.82404570799999));
#336068=CARTESIAN_POINT('Ctrl Pts',(1.49561135799994,12.2,3.82309722799998));
#336069=CARTESIAN_POINT('Ctrl Pts',(1.49561135799994,5.2,3.82309722799998));
#336070=CARTESIAN_POINT('Ctrl Pts',(1.49561135799994,2.2,3.82309722799998));
#336071=CARTESIAN_POINT('Ctrl Pts',(1.49495660099994,12.2,3.82215225199998));
#336072=CARTESIAN_POINT('Ctrl Pts',(1.49495660099994,5.2,3.82215225199998));
#336073=CARTESIAN_POINT('Ctrl Pts',(1.49495660099994,2.2,3.82215225199998));
#336074=CARTESIAN_POINT('Ctrl Pts',(1.49430597199994,12.2,3.82121079699999));
#336075=CARTESIAN_POINT('Ctrl Pts',(1.49430597199994,5.2,3.82121079699999));
#336076=CARTESIAN_POINT('Ctrl Pts',(1.49430597199994,2.2,3.82121079699999));
#336077=CARTESIAN_POINT('Ctrl Pts',(1.49365946699994,12.2,3.82027287699999));
#336078=CARTESIAN_POINT('Ctrl Pts',(1.49365946699994,5.2,3.82027287699999));
#336079=CARTESIAN_POINT('Ctrl Pts',(1.49365946699994,2.2,3.82027287699999));
#336080=CARTESIAN_POINT('Ctrl Pts',(1.49301708199994,12.2,3.81933850799999));
#336081=CARTESIAN_POINT('Ctrl Pts',(1.49301708199994,5.2,3.81933850799999));
#336082=CARTESIAN_POINT('Ctrl Pts',(1.49301708199994,2.2,3.81933850799999));
#336083=CARTESIAN_POINT('Ctrl Pts',(1.49237881299994,12.2,3.81840770299998));
#336084=CARTESIAN_POINT('Ctrl Pts',(1.49237881299994,5.2,3.81840770299998));
#336085=CARTESIAN_POINT('Ctrl Pts',(1.49237881299994,2.2,3.81840770299998));
#336086=CARTESIAN_POINT('Ctrl Pts',(1.49174465499994,12.2,3.81748048099999));
#336087=CARTESIAN_POINT('Ctrl Pts',(1.49174465499994,5.2,3.81748048099999));
#336088=CARTESIAN_POINT('Ctrl Pts',(1.49174465499994,2.2,3.81748048099999));
#336089=CARTESIAN_POINT('Ctrl Pts',(1.49111460299994,12.2,3.81655685399998));
#336090=CARTESIAN_POINT('Ctrl Pts',(1.49111460299994,5.2,3.81655685399998));
#336091=CARTESIAN_POINT('Ctrl Pts',(1.49111460299994,2.2,3.81655685399998));
#336092=CARTESIAN_POINT('Ctrl Pts',(1.49048865599994,12.2,3.81563683899999));
#336093=CARTESIAN_POINT('Ctrl Pts',(1.49048865599994,5.2,3.81563683899999));
#336094=CARTESIAN_POINT('Ctrl Pts',(1.49048865599994,2.2,3.81563683899999));
#336095=CARTESIAN_POINT('Ctrl Pts',(1.48986680499994,12.2,3.81472044999998));
#336096=CARTESIAN_POINT('Ctrl Pts',(1.48986680499994,5.2,3.81472044999998));
#336097=CARTESIAN_POINT('Ctrl Pts',(1.48986680499994,2.2,3.81472044999998));
#336098=CARTESIAN_POINT('Ctrl Pts',(1.48924904999994,12.2,3.81380770199998));
#336099=CARTESIAN_POINT('Ctrl Pts',(1.48924904999994,5.2,3.81380770199998));
#336100=CARTESIAN_POINT('Ctrl Pts',(1.48924904999994,2.2,3.81380770199998));
#336101=CARTESIAN_POINT('Ctrl Pts',(1.48863538399994,12.2,3.81289861099999));
#336102=CARTESIAN_POINT('Ctrl Pts',(1.48863538399994,5.2,3.81289861099999));
#336103=CARTESIAN_POINT('Ctrl Pts',(1.48863538399994,2.2,3.81289861099999));
#336104=CARTESIAN_POINT('Ctrl Pts',(1.48802580299994,12.2,3.81199319299999));
#336105=CARTESIAN_POINT('Ctrl Pts',(1.48802580299994,5.2,3.81199319299999));
#336106=CARTESIAN_POINT('Ctrl Pts',(1.48802580299994,2.2,3.81199319299999));
#336107=CARTESIAN_POINT('Ctrl Pts',(1.48742030299994,12.2,3.81109146299998));
#336108=CARTESIAN_POINT('Ctrl Pts',(1.48742030299994,5.2,3.81109146299998));
#336109=CARTESIAN_POINT('Ctrl Pts',(1.48742030299994,2.2,3.81109146299998));
#336110=CARTESIAN_POINT('Ctrl Pts',(1.48681887899994,12.2,3.81019343499998));
#336111=CARTESIAN_POINT('Ctrl Pts',(1.48681887899994,5.2,3.81019343499998));
#336112=CARTESIAN_POINT('Ctrl Pts',(1.48681887899994,2.2,3.81019343499998));
#336113=CARTESIAN_POINT('Ctrl Pts',(1.48622152799994,12.2,3.80929912599999));
#336114=CARTESIAN_POINT('Ctrl Pts',(1.48622152799994,5.2,3.80929912599999));
#336115=CARTESIAN_POINT('Ctrl Pts',(1.48622152799994,2.2,3.80929912599999));
#336116=CARTESIAN_POINT('Ctrl Pts',(1.48562824299994,12.2,3.80840855199998));
#336117=CARTESIAN_POINT('Ctrl Pts',(1.48562824299994,5.2,3.80840855199998));
#336118=CARTESIAN_POINT('Ctrl Pts',(1.48562824299994,2.2,3.80840855199998));
#336119=CARTESIAN_POINT('Ctrl Pts',(1.48503902099994,12.2,3.80752172599998));
#336120=CARTESIAN_POINT('Ctrl Pts',(1.48503902099994,5.2,3.80752172599998));
#336121=CARTESIAN_POINT('Ctrl Pts',(1.48503902099994,2.2,3.80752172599998));
#336122=CARTESIAN_POINT('Ctrl Pts',(1.48445385799994,12.2,3.80663866499999));
#336123=CARTESIAN_POINT('Ctrl Pts',(1.48445385799994,5.2,3.80663866499999));
#336124=CARTESIAN_POINT('Ctrl Pts',(1.48445385799994,2.2,3.80663866499999));
#336125=CARTESIAN_POINT('Ctrl Pts',(1.48387274799994,12.2,3.80575938499998));
#336126=CARTESIAN_POINT('Ctrl Pts',(1.48387274799994,5.2,3.80575938499998));
#336127=CARTESIAN_POINT('Ctrl Pts',(1.48387274799994,2.2,3.80575938499998));
#336128=CARTESIAN_POINT('Ctrl Pts',(1.48329568599994,12.2,3.80488390099998));
#336129=CARTESIAN_POINT('Ctrl Pts',(1.48329568599994,5.2,3.80488390099998));
#336130=CARTESIAN_POINT('Ctrl Pts',(1.48329568599994,2.2,3.80488390099998));
#336131=CARTESIAN_POINT('Ctrl Pts',(1.48272266999994,12.2,3.80401222799998));
#336132=CARTESIAN_POINT('Ctrl Pts',(1.48272266999994,5.2,3.80401222799998));
#336133=CARTESIAN_POINT('Ctrl Pts',(1.48272266999994,2.2,3.80401222799998));
#336134=CARTESIAN_POINT('Ctrl Pts',(1.48215369199994,12.2,3.80314438299998));
#336135=CARTESIAN_POINT('Ctrl Pts',(1.48215369199994,5.2,3.80314438299998));
#336136=CARTESIAN_POINT('Ctrl Pts',(1.48215369199994,2.2,3.80314438299998));
#336137=CARTESIAN_POINT('Ctrl Pts',(1.48158874799994,12.2,3.80228038099998));
#336138=CARTESIAN_POINT('Ctrl Pts',(1.48158874799994,5.2,3.80228038099998));
#336139=CARTESIAN_POINT('Ctrl Pts',(1.48158874799994,2.2,3.80228038099998));
#336140=CARTESIAN_POINT('Ctrl Pts',(1.48102783599994,12.2,3.80142023799999));
#336141=CARTESIAN_POINT('Ctrl Pts',(1.48102783599994,5.2,3.80142023799999));
#336142=CARTESIAN_POINT('Ctrl Pts',(1.48102783599994,2.2,3.80142023799999));
#336143=CARTESIAN_POINT('Ctrl Pts',(1.48047094699994,12.2,3.80056396999999));
#336144=CARTESIAN_POINT('Ctrl Pts',(1.48047094699994,5.2,3.80056396999999));
#336145=CARTESIAN_POINT('Ctrl Pts',(1.48047094699994,2.2,3.80056396999999));
#336146=CARTESIAN_POINT('Ctrl Pts',(1.47991807899994,12.2,3.79971159099998));
#336147=CARTESIAN_POINT('Ctrl Pts',(1.47991807899994,5.2,3.79971159099998));
#336148=CARTESIAN_POINT('Ctrl Pts',(1.47991807899994,2.2,3.79971159099998));
#336149=CARTESIAN_POINT('Ctrl Pts',(1.47936922699994,12.2,3.79886311799999));
#336150=CARTESIAN_POINT('Ctrl Pts',(1.47936922699994,5.2,3.79886311799999));
#336151=CARTESIAN_POINT('Ctrl Pts',(1.47936922699994,2.2,3.79886311799999));
#336152=CARTESIAN_POINT('Ctrl Pts',(1.47882438399994,12.2,3.79801856699999));
#336153=CARTESIAN_POINT('Ctrl Pts',(1.47882438399994,5.2,3.79801856699999));
#336154=CARTESIAN_POINT('Ctrl Pts',(1.47882438399994,2.2,3.79801856699999));
#336155=CARTESIAN_POINT('Ctrl Pts',(1.47828354699994,12.2,3.79717795399999));
#336156=CARTESIAN_POINT('Ctrl Pts',(1.47828354699994,5.2,3.79717795399999));
#336157=CARTESIAN_POINT('Ctrl Pts',(1.47828354699994,2.2,3.79717795399999));
#336158=CARTESIAN_POINT('Ctrl Pts',(1.47774671099994,12.2,3.79634129599999));
#336159=CARTESIAN_POINT('Ctrl Pts',(1.47774671099994,5.2,3.79634129599999));
#336160=CARTESIAN_POINT('Ctrl Pts',(1.47774671099994,2.2,3.79634129599999));
#336161=CARTESIAN_POINT('Ctrl Pts',(1.47721387099994,12.2,3.79550860599998));
#336162=CARTESIAN_POINT('Ctrl Pts',(1.47721387099994,5.2,3.79550860599998));
#336163=CARTESIAN_POINT('Ctrl Pts',(1.47721387099994,2.2,3.79550860599998));
#336164=CARTESIAN_POINT('Ctrl Pts',(1.47668501999994,12.2,3.79467990299998));
#336165=CARTESIAN_POINT('Ctrl Pts',(1.47668501999994,5.2,3.79467990299998));
#336166=CARTESIAN_POINT('Ctrl Pts',(1.47668501999994,2.2,3.79467990299998));
#336167=CARTESIAN_POINT('Ctrl Pts',(1.47616015499994,12.2,3.79385519999998));
#336168=CARTESIAN_POINT('Ctrl Pts',(1.47616015499994,5.2,3.79385519999998));
#336169=CARTESIAN_POINT('Ctrl Pts',(1.47616015499994,2.2,3.79385519999998));
#336170=CARTESIAN_POINT('Ctrl Pts',(1.47563926899994,12.2,3.79303451599998));
#336171=CARTESIAN_POINT('Ctrl Pts',(1.47563926899994,5.2,3.79303451599998));
#336172=CARTESIAN_POINT('Ctrl Pts',(1.47563926899994,2.2,3.79303451599998));
#336173=CARTESIAN_POINT('Ctrl Pts',(1.47512235999994,12.2,3.79221786499999));
#336174=CARTESIAN_POINT('Ctrl Pts',(1.47512235999994,5.2,3.79221786499999));
#336175=CARTESIAN_POINT('Ctrl Pts',(1.47512235999994,2.2,3.79221786499999));
#336176=CARTESIAN_POINT('Ctrl Pts',(1.47460941899994,12.2,3.79140526399999));
#336177=CARTESIAN_POINT('Ctrl Pts',(1.47460941899994,5.2,3.79140526399999));
#336178=CARTESIAN_POINT('Ctrl Pts',(1.47460941899994,2.2,3.79140526399999));
#336179=CARTESIAN_POINT('Ctrl Pts',(1.47410044399994,12.2,3.79059672899999));
#336180=CARTESIAN_POINT('Ctrl Pts',(1.47410044399994,5.2,3.79059672899999));
#336181=CARTESIAN_POINT('Ctrl Pts',(1.47410044399994,2.2,3.79059672899999));
#336182=CARTESIAN_POINT('Ctrl Pts',(1.47359542799994,12.2,3.78979227699999));
#336183=CARTESIAN_POINT('Ctrl Pts',(1.47359542799994,5.2,3.78979227699999));
#336184=CARTESIAN_POINT('Ctrl Pts',(1.47359542799994,2.2,3.78979227699999));
#336185=CARTESIAN_POINT('Ctrl Pts',(1.47309436599994,12.2,3.78899192199999));
#336186=CARTESIAN_POINT('Ctrl Pts',(1.47309436599994,5.2,3.78899192199999));
#336187=CARTESIAN_POINT('Ctrl Pts',(1.47309436599994,2.2,3.78899192199999));
#336188=CARTESIAN_POINT('Ctrl Pts',(1.47259725299994,12.2,3.78819568399998));
#336189=CARTESIAN_POINT('Ctrl Pts',(1.47259725299994,5.2,3.78819568399998));
#336190=CARTESIAN_POINT('Ctrl Pts',(1.47259725299994,2.2,3.78819568399998));
#336191=CARTESIAN_POINT('Ctrl Pts',(1.47210408299994,12.2,3.78740357599998));
#336192=CARTESIAN_POINT('Ctrl Pts',(1.47210408299994,5.2,3.78740357599998));
#336193=CARTESIAN_POINT('Ctrl Pts',(1.47210408299994,2.2,3.78740357599998));
#336194=CARTESIAN_POINT('Ctrl Pts',(1.47161485199994,12.2,3.78661561499998));
#336195=CARTESIAN_POINT('Ctrl Pts',(1.47161485199994,5.2,3.78661561499998));
#336196=CARTESIAN_POINT('Ctrl Pts',(1.47161485199994,2.2,3.78661561499998));
#336197=CARTESIAN_POINT('Ctrl Pts',(1.47112955299994,12.2,3.78583181699998));
#336198=CARTESIAN_POINT('Ctrl Pts',(1.47112955299994,5.2,3.78583181699998));
#336199=CARTESIAN_POINT('Ctrl Pts',(1.47112955299994,2.2,3.78583181699998));
#336200=CARTESIAN_POINT('Ctrl Pts',(1.47064817999994,12.2,3.78505219999998));
#336201=CARTESIAN_POINT('Ctrl Pts',(1.47064817999994,5.2,3.78505219999998));
#336202=CARTESIAN_POINT('Ctrl Pts',(1.47064817999994,2.2,3.78505219999998));
#336203=CARTESIAN_POINT('Ctrl Pts',(1.47017072999994,12.2,3.78427677899998));
#336204=CARTESIAN_POINT('Ctrl Pts',(1.47017072999994,5.2,3.78427677899998));
#336205=CARTESIAN_POINT('Ctrl Pts',(1.47017072999994,2.2,3.78427677899998));
#336206=CARTESIAN_POINT('Ctrl Pts',(1.46969719599994,12.2,3.78350557199998));
#336207=CARTESIAN_POINT('Ctrl Pts',(1.46969719599994,5.2,3.78350557199998));
#336208=CARTESIAN_POINT('Ctrl Pts',(1.46969719599994,2.2,3.78350557199998));
#336209=CARTESIAN_POINT('Ctrl Pts',(1.46922757299994,12.2,3.78273859399999));
#336210=CARTESIAN_POINT('Ctrl Pts',(1.46922757299994,5.2,3.78273859399999));
#336211=CARTESIAN_POINT('Ctrl Pts',(1.46922757299994,2.2,3.78273859399999));
#336212=CARTESIAN_POINT('Ctrl Pts',(1.46876185499994,12.2,3.78197586199998));
#336213=CARTESIAN_POINT('Ctrl Pts',(1.46876185499994,5.2,3.78197586199998));
#336214=CARTESIAN_POINT('Ctrl Pts',(1.46876185499994,2.2,3.78197586199998));
#336215=CARTESIAN_POINT('Ctrl Pts',(1.46830003499994,12.2,3.78121739299999));
#336216=CARTESIAN_POINT('Ctrl Pts',(1.46830003499994,5.2,3.78121739299999));
#336217=CARTESIAN_POINT('Ctrl Pts',(1.46830003499994,2.2,3.78121739299999));
#336218=CARTESIAN_POINT('Ctrl Pts',(1.46784210999995,12.2,3.78046320299998));
#336219=CARTESIAN_POINT('Ctrl Pts',(1.46784210999995,5.2,3.78046320299998));
#336220=CARTESIAN_POINT('Ctrl Pts',(1.46784210999995,2.2,3.78046320299998));
#336221=CARTESIAN_POINT('Ctrl Pts',(1.46738807199994,12.2,3.77971330899998));
#336222=CARTESIAN_POINT('Ctrl Pts',(1.46738807199994,5.2,3.77971330899998));
#336223=CARTESIAN_POINT('Ctrl Pts',(1.46738807199994,2.2,3.77971330899998));
#336224=CARTESIAN_POINT('Ctrl Pts',(1.46693791799994,12.2,3.77896772699999));
#336225=CARTESIAN_POINT('Ctrl Pts',(1.46693791799994,5.2,3.77896772699999));
#336226=CARTESIAN_POINT('Ctrl Pts',(1.46693791799994,2.2,3.77896772699999));
#336227=CARTESIAN_POINT('Ctrl Pts',(1.46649163899994,12.2,3.77822647599999));
#336228=CARTESIAN_POINT('Ctrl Pts',(1.46649163899994,5.2,3.77822647599999));
#336229=CARTESIAN_POINT('Ctrl Pts',(1.46649163899994,2.2,3.77822647599999));
#336230=CARTESIAN_POINT('Ctrl Pts',(1.46604923099994,12.2,3.77748956899998));
#336231=CARTESIAN_POINT('Ctrl Pts',(1.46604923099994,5.2,3.77748956899998));
#336232=CARTESIAN_POINT('Ctrl Pts',(1.46604923099994,2.2,3.77748956899998));
#336233=CARTESIAN_POINT('Ctrl Pts',(1.46561068799994,12.2,3.77675702699998));
#336234=CARTESIAN_POINT('Ctrl Pts',(1.46561068799994,5.2,3.77675702699998));
#336235=CARTESIAN_POINT('Ctrl Pts',(1.46561068799994,2.2,3.77675702699998));
#336236=CARTESIAN_POINT('Ctrl Pts',(1.46517600399994,12.2,3.77602886399998));
#336237=CARTESIAN_POINT('Ctrl Pts',(1.46517600399994,5.2,3.77602886399998));
#336238=CARTESIAN_POINT('Ctrl Pts',(1.46517600399994,2.2,3.77602886399998));
#336239=CARTESIAN_POINT('Ctrl Pts',(1.46474517199994,12.2,3.77530509699999));
#336240=CARTESIAN_POINT('Ctrl Pts',(1.46474517199994,5.2,3.77530509699999));
#336241=CARTESIAN_POINT('Ctrl Pts',(1.46474517199994,2.2,3.77530509699999));
#336242=CARTESIAN_POINT('Ctrl Pts',(1.46431818799994,12.2,3.77458574399999));
#336243=CARTESIAN_POINT('Ctrl Pts',(1.46431818799994,5.2,3.77458574399999));
#336244=CARTESIAN_POINT('Ctrl Pts',(1.46431818799994,2.2,3.77458574399999));
#336245=CARTESIAN_POINT('Ctrl Pts',(1.46389504399994,12.2,3.77387082099998));
#336246=CARTESIAN_POINT('Ctrl Pts',(1.46389504399994,5.2,3.77387082099998));
#336247=CARTESIAN_POINT('Ctrl Pts',(1.46389504399994,2.2,3.77387082099998));
#336248=CARTESIAN_POINT('Ctrl Pts',(1.46347573699994,12.2,3.77316034699999));
#336249=CARTESIAN_POINT('Ctrl Pts',(1.46347573699994,5.2,3.77316034699999));
#336250=CARTESIAN_POINT('Ctrl Pts',(1.46347573699994,2.2,3.77316034699999));
#336251=CARTESIAN_POINT('Ctrl Pts',(1.46306025699994,12.2,3.77245433599998));
#336252=CARTESIAN_POINT('Ctrl Pts',(1.46306025699994,5.2,3.77245433599998));
#336253=CARTESIAN_POINT('Ctrl Pts',(1.46306025699994,2.2,3.77245433599998));
#336254=CARTESIAN_POINT('Ctrl Pts',(1.46264860099994,12.2,3.77175280699999));
#336255=CARTESIAN_POINT('Ctrl Pts',(1.46264860099994,5.2,3.77175280699999));
#336256=CARTESIAN_POINT('Ctrl Pts',(1.46264860099994,2.2,3.77175280699999));
#336257=CARTESIAN_POINT('Ctrl Pts',(1.46224076099994,12.2,3.77105577799998));
#336258=CARTESIAN_POINT('Ctrl Pts',(1.46224076099994,5.2,3.77105577799998));
#336259=CARTESIAN_POINT('Ctrl Pts',(1.46224076099994,2.2,3.77105577799998));
#336260=CARTESIAN_POINT('Ctrl Pts',(1.46183673199994,12.2,3.77036326399999));
#336261=CARTESIAN_POINT('Ctrl Pts',(1.46183673199994,5.2,3.77036326399999));
#336262=CARTESIAN_POINT('Ctrl Pts',(1.46183673199994,2.2,3.77036326399999));
#336263=CARTESIAN_POINT('Ctrl Pts',(1.46143650699994,12.2,3.76967528299998));
#336264=CARTESIAN_POINT('Ctrl Pts',(1.46143650699994,5.2,3.76967528299998));
#336265=CARTESIAN_POINT('Ctrl Pts',(1.46143650699994,2.2,3.76967528299998));
#336266=CARTESIAN_POINT('Ctrl Pts',(1.46104007999994,12.2,3.76899185199999));
#336267=CARTESIAN_POINT('Ctrl Pts',(1.46104007999994,5.2,3.76899185199999));
#336268=CARTESIAN_POINT('Ctrl Pts',(1.46104007999994,2.2,3.76899185199999));
#336269=CARTESIAN_POINT('Ctrl Pts',(1.46064744499994,12.2,3.76831298899998));
#336270=CARTESIAN_POINT('Ctrl Pts',(1.46064744499994,5.2,3.76831298899998));
#336271=CARTESIAN_POINT('Ctrl Pts',(1.46064744499994,2.2,3.76831298899998));
#336272=CARTESIAN_POINT('Ctrl Pts',(1.46025859499994,12.2,3.76763871099998));
#336273=CARTESIAN_POINT('Ctrl Pts',(1.46025859499994,5.2,3.76763871099998));
#336274=CARTESIAN_POINT('Ctrl Pts',(1.46025859499994,2.2,3.76763871099998));
#336275=CARTESIAN_POINT('Ctrl Pts',(1.45987352399994,12.2,3.76696903499998));
#336276=CARTESIAN_POINT('Ctrl Pts',(1.45987352399994,5.2,3.76696903499998));
#336277=CARTESIAN_POINT('Ctrl Pts',(1.45987352399994,2.2,3.76696903499998));
#336278=CARTESIAN_POINT('Ctrl Pts',(1.45949222599994,12.2,3.76630397899999));
#336279=CARTESIAN_POINT('Ctrl Pts',(1.45949222599994,5.2,3.76630397899999));
#336280=CARTESIAN_POINT('Ctrl Pts',(1.45949222599994,2.2,3.76630397899999));
#336281=CARTESIAN_POINT('Ctrl Pts',(1.45911469399994,12.2,3.76564355999999));
#336282=CARTESIAN_POINT('Ctrl Pts',(1.45911469399994,5.2,3.76564355999999));
#336283=CARTESIAN_POINT('Ctrl Pts',(1.45911469399994,2.2,3.76564355999999));
#336284=CARTESIAN_POINT('Ctrl Pts',(1.45874092099994,12.2,3.76498779599999));
#336285=CARTESIAN_POINT('Ctrl Pts',(1.45874092099994,5.2,3.76498779599999));
#336286=CARTESIAN_POINT('Ctrl Pts',(1.45874092099994,2.2,3.76498779599999));
#336287=CARTESIAN_POINT('Ctrl Pts',(1.45837090199994,12.2,3.76433670299999));
#336288=CARTESIAN_POINT('Ctrl Pts',(1.45837090199994,5.2,3.76433670299999));
#336289=CARTESIAN_POINT('Ctrl Pts',(1.45837090199994,2.2,3.76433670299999));
#336290=CARTESIAN_POINT('Ctrl Pts',(1.45800462899994,12.2,3.76369030099998));
#336291=CARTESIAN_POINT('Ctrl Pts',(1.45800462899994,5.2,3.76369030099998));
#336292=CARTESIAN_POINT('Ctrl Pts',(1.45800462899994,2.2,3.76369030099998));
#336293=CARTESIAN_POINT('Ctrl Pts',(1.45764209599994,12.2,3.76304860499998));
#336294=CARTESIAN_POINT('Ctrl Pts',(1.45764209599994,5.2,3.76304860499998));
#336295=CARTESIAN_POINT('Ctrl Pts',(1.45764209599994,2.2,3.76304860499998));
#336296=CARTESIAN_POINT('Ctrl Pts',(1.45728329599994,12.2,3.76241163399998));
#336297=CARTESIAN_POINT('Ctrl Pts',(1.45728329599994,5.2,3.76241163399998));
#336298=CARTESIAN_POINT('Ctrl Pts',(1.45728329599994,2.2,3.76241163399998));
#336299=CARTESIAN_POINT('Ctrl Pts',(1.45692822299994,12.2,3.76177940599998));
#336300=CARTESIAN_POINT('Ctrl Pts',(1.45692822299994,5.2,3.76177940599998));
#336301=CARTESIAN_POINT('Ctrl Pts',(1.45692822299994,2.2,3.76177940599998));
#336302=CARTESIAN_POINT('Ctrl Pts',(1.45657686999994,12.2,3.76115193799999));
#336303=CARTESIAN_POINT('Ctrl Pts',(1.45657686999994,5.2,3.76115193799999));
#336304=CARTESIAN_POINT('Ctrl Pts',(1.45657686999994,2.2,3.76115193799999));
#336305=CARTESIAN_POINT('Ctrl Pts',(1.45622922999994,12.2,3.76052924899999));
#336306=CARTESIAN_POINT('Ctrl Pts',(1.45622922999994,5.2,3.76052924899999));
#336307=CARTESIAN_POINT('Ctrl Pts',(1.45622922999994,2.2,3.76052924899999));
#336308=CARTESIAN_POINT('Ctrl Pts',(1.45588529499994,12.2,3.75991135499999));
#336309=CARTESIAN_POINT('Ctrl Pts',(1.45588529499994,5.2,3.75991135499999));
#336310=CARTESIAN_POINT('Ctrl Pts',(1.45588529499994,2.2,3.75991135499999));
#336311=CARTESIAN_POINT('Ctrl Pts',(1.45554505999994,12.2,3.75929827399998));
#336312=CARTESIAN_POINT('Ctrl Pts',(1.45554505999994,5.2,3.75929827399998));
#336313=CARTESIAN_POINT('Ctrl Pts',(1.45554505999994,2.2,3.75929827399998));
#336314=CARTESIAN_POINT('Ctrl Pts',(1.45520851699994,12.2,3.75869002599998));
#336315=CARTESIAN_POINT('Ctrl Pts',(1.45520851699994,5.2,3.75869002599998));
#336316=CARTESIAN_POINT('Ctrl Pts',(1.45520851699994,2.2,3.75869002599998));
#336317=CARTESIAN_POINT('Ctrl Pts',(1.45487566099994,12.2,3.75808662699999));
#336318=CARTESIAN_POINT('Ctrl Pts',(1.45487566099994,5.2,3.75808662699999));
#336319=CARTESIAN_POINT('Ctrl Pts',(1.45487566099994,2.2,3.75808662699999));
#336320=CARTESIAN_POINT('Ctrl Pts',(1.45454648199994,12.2,3.75748809499999));
#336321=CARTESIAN_POINT('Ctrl Pts',(1.45454648199994,5.2,3.75748809499999));
#336322=CARTESIAN_POINT('Ctrl Pts',(1.45454648199994,2.2,3.75748809499999));
#336323=CARTESIAN_POINT('Ctrl Pts',(1.45422097599994,12.2,3.75689444899999));
#336324=CARTESIAN_POINT('Ctrl Pts',(1.45422097599994,5.2,3.75689444899999));
#336325=CARTESIAN_POINT('Ctrl Pts',(1.45422097599994,2.2,3.75689444899999));
#336326=CARTESIAN_POINT('Ctrl Pts',(1.45389913299994,12.2,3.75630570599998));
#336327=CARTESIAN_POINT('Ctrl Pts',(1.45389913299994,5.2,3.75630570599998));
#336328=CARTESIAN_POINT('Ctrl Pts',(1.45389913299994,2.2,3.75630570599998));
#336329=CARTESIAN_POINT('Ctrl Pts',(1.45358094899994,12.2,3.75572188599998));
#336330=CARTESIAN_POINT('Ctrl Pts',(1.45358094899994,5.2,3.75572188599998));
#336331=CARTESIAN_POINT('Ctrl Pts',(1.45358094899994,2.2,3.75572188599998));
#336332=CARTESIAN_POINT('Ctrl Pts',(1.45326641399994,12.2,3.75514300499999));
#336333=CARTESIAN_POINT('Ctrl Pts',(1.45326641399994,5.2,3.75514300499999));
#336334=CARTESIAN_POINT('Ctrl Pts',(1.45326641399994,2.2,3.75514300499999));
#336335=CARTESIAN_POINT('Ctrl Pts',(1.45295552199994,12.2,3.75456908199999));
#336336=CARTESIAN_POINT('Ctrl Pts',(1.45295552199994,5.2,3.75456908199999));
#336337=CARTESIAN_POINT('Ctrl Pts',(1.45295552199994,2.2,3.75456908199999));
#336338=CARTESIAN_POINT('Ctrl Pts',(1.45264826499994,12.2,3.75400013499998));
#336339=CARTESIAN_POINT('Ctrl Pts',(1.45264826499994,5.2,3.75400013499998));
#336340=CARTESIAN_POINT('Ctrl Pts',(1.45264826499994,2.2,3.75400013499998));
#336341=CARTESIAN_POINT('Ctrl Pts',(1.45234463799994,12.2,3.75343618299999));
#336342=CARTESIAN_POINT('Ctrl Pts',(1.45234463799994,5.2,3.75343618299999));
#336343=CARTESIAN_POINT('Ctrl Pts',(1.45234463799994,2.2,3.75343618299999));
#336344=CARTESIAN_POINT('Ctrl Pts',(1.45204463099994,12.2,3.75287724399998));
#336345=CARTESIAN_POINT('Ctrl Pts',(1.45204463099994,5.2,3.75287724399998));
#336346=CARTESIAN_POINT('Ctrl Pts',(1.45204463099994,2.2,3.75287724399998));
#336347=CARTESIAN_POINT('Ctrl Pts',(1.45174823799994,12.2,3.75232333599998));
#336348=CARTESIAN_POINT('Ctrl Pts',(1.45174823799994,5.2,3.75232333599998));
#336349=CARTESIAN_POINT('Ctrl Pts',(1.45174823799994,2.2,3.75232333599998));
#336350=CARTESIAN_POINT('Ctrl Pts',(1.45145545199994,12.2,3.75177447799998));
#336351=CARTESIAN_POINT('Ctrl Pts',(1.45145545199994,5.2,3.75177447799998));
#336352=CARTESIAN_POINT('Ctrl Pts',(1.45145545199994,2.2,3.75177447799998));
#336353=CARTESIAN_POINT('Ctrl Pts',(1.45116626499994,12.2,3.75123068799999));
#336354=CARTESIAN_POINT('Ctrl Pts',(1.45116626499994,5.2,3.75123068799999));
#336355=CARTESIAN_POINT('Ctrl Pts',(1.45116626499994,2.2,3.75123068799999));
#336356=CARTESIAN_POINT('Ctrl Pts',(1.45088066799994,12.2,3.75069198499999));
#336357=CARTESIAN_POINT('Ctrl Pts',(1.45088066799994,5.2,3.75069198499999));
#336358=CARTESIAN_POINT('Ctrl Pts',(1.45088066799994,2.2,3.75069198499999));
#336359=CARTESIAN_POINT('Ctrl Pts',(1.45059865499995,12.2,3.75015838699999));
#336360=CARTESIAN_POINT('Ctrl Pts',(1.45059865499995,5.2,3.75015838699999));
#336361=CARTESIAN_POINT('Ctrl Pts',(1.45059865499995,2.2,3.75015838699999));
#336362=CARTESIAN_POINT('Ctrl Pts',(1.45032021899994,12.2,3.74962991299999));
#336363=CARTESIAN_POINT('Ctrl Pts',(1.45032021899994,5.2,3.74962991299999));
#336364=CARTESIAN_POINT('Ctrl Pts',(1.45032021899994,2.2,3.74962991299999));
#336365=CARTESIAN_POINT('Ctrl Pts',(1.45004535099994,12.2,3.74910658199998));
#336366=CARTESIAN_POINT('Ctrl Pts',(1.45004535099994,5.2,3.74910658199998));
#336367=CARTESIAN_POINT('Ctrl Pts',(1.45004535099994,2.2,3.74910658199998));
#336368=CARTESIAN_POINT('Ctrl Pts',(1.44977404499994,12.2,3.74858841099999));
#336369=CARTESIAN_POINT('Ctrl Pts',(1.44977404499994,5.2,3.74858841099999));
#336370=CARTESIAN_POINT('Ctrl Pts',(1.44977404499994,2.2,3.74858841099999));
#336371=CARTESIAN_POINT('Ctrl Pts',(1.44950629199994,12.2,3.74807542099998));
#336372=CARTESIAN_POINT('Ctrl Pts',(1.44950629199994,5.2,3.74807542099998));
#336373=CARTESIAN_POINT('Ctrl Pts',(1.44950629199994,2.2,3.74807542099998));
#336374=CARTESIAN_POINT('Ctrl Pts',(1.44924208299994,12.2,3.74756762899998));
#336375=CARTESIAN_POINT('Ctrl Pts',(1.44924208299994,5.2,3.74756762899998));
#336376=CARTESIAN_POINT('Ctrl Pts',(1.44924208299994,2.2,3.74756762899998));
#336377=CARTESIAN_POINT('Ctrl Pts',(1.44898141299994,12.2,3.74706505499999));
#336378=CARTESIAN_POINT('Ctrl Pts',(1.44898141299994,5.2,3.74706505499999));
#336379=CARTESIAN_POINT('Ctrl Pts',(1.44898141299994,2.2,3.74706505499999));
#336380=CARTESIAN_POINT('Ctrl Pts',(1.44872427199994,12.2,3.74656771799999));
#336381=CARTESIAN_POINT('Ctrl Pts',(1.44872427199994,5.2,3.74656771799999));
#336382=CARTESIAN_POINT('Ctrl Pts',(1.44872427199994,2.2,3.74656771799999));
#336383=CARTESIAN_POINT('Ctrl Pts',(1.44847065299994,12.2,3.74607563599999));
#336384=CARTESIAN_POINT('Ctrl Pts',(1.44847065299994,5.2,3.74607563599999));
#336385=CARTESIAN_POINT('Ctrl Pts',(1.44847065299994,2.2,3.74607563599999));
#336386=CARTESIAN_POINT('Ctrl Pts',(1.44822054799994,12.2,3.74558882799998));
#336387=CARTESIAN_POINT('Ctrl Pts',(1.44822054799994,5.2,3.74558882799998));
#336388=CARTESIAN_POINT('Ctrl Pts',(1.44822054799994,2.2,3.74558882799998));
#336389=CARTESIAN_POINT('Ctrl Pts',(1.44797394999994,12.2,3.74510731399998));
#336390=CARTESIAN_POINT('Ctrl Pts',(1.44797394999994,5.2,3.74510731399998));
#336391=CARTESIAN_POINT('Ctrl Pts',(1.44797394999994,2.2,3.74510731399998));
#336392=CARTESIAN_POINT('Ctrl Pts',(1.44773084699994,12.2,3.74463111299999));
#336393=CARTESIAN_POINT('Ctrl Pts',(1.44773084699994,5.2,3.74463111299999));
#336394=CARTESIAN_POINT('Ctrl Pts',(1.44773084699994,2.2,3.74463111299999));
#336395=CARTESIAN_POINT('Ctrl Pts',(1.44749123599994,12.2,3.74416024299999));
#336396=CARTESIAN_POINT('Ctrl Pts',(1.44749123599994,5.2,3.74416024299999));
#336397=CARTESIAN_POINT('Ctrl Pts',(1.44749123599994,2.2,3.74416024299999));
#336398=CARTESIAN_POINT('Ctrl Pts',(1.44725510599994,12.2,3.74369472399999));
#336399=CARTESIAN_POINT('Ctrl Pts',(1.44725510599994,5.2,3.74369472399999));
#336400=CARTESIAN_POINT('Ctrl Pts',(1.44725510599994,2.2,3.74369472399999));
#336401=CARTESIAN_POINT('Ctrl Pts',(1.44702244999994,12.2,3.74323457499998));
#336402=CARTESIAN_POINT('Ctrl Pts',(1.44702244999994,5.2,3.74323457499998));
#336403=CARTESIAN_POINT('Ctrl Pts',(1.44702244999994,2.2,3.74323457499998));
#336404=CARTESIAN_POINT('Ctrl Pts',(1.44679325699994,12.2,3.74277981599998));
#336405=CARTESIAN_POINT('Ctrl Pts',(1.44679325699994,5.2,3.74277981599998));
#336406=CARTESIAN_POINT('Ctrl Pts',(1.44679325699994,2.2,3.74277981599998));
#336407=CARTESIAN_POINT('Ctrl Pts',(1.44656752299994,12.2,3.74233046599999));
#336408=CARTESIAN_POINT('Ctrl Pts',(1.44656752299994,5.2,3.74233046599999));
#336409=CARTESIAN_POINT('Ctrl Pts',(1.44656752299994,2.2,3.74233046599999));
#336410=CARTESIAN_POINT('Ctrl Pts',(1.44634523599994,12.2,3.74188654299999));
#336411=CARTESIAN_POINT('Ctrl Pts',(1.44634523599994,5.2,3.74188654299999));
#336412=CARTESIAN_POINT('Ctrl Pts',(1.44634523599994,2.2,3.74188654299999));
#336413=CARTESIAN_POINT('Ctrl Pts',(1.44612638999994,12.2,3.74144806799999));
#336414=CARTESIAN_POINT('Ctrl Pts',(1.44612638999994,5.2,3.74144806799999));
#336415=CARTESIAN_POINT('Ctrl Pts',(1.44612638999994,2.2,3.74144806799999));
#336416=CARTESIAN_POINT('Ctrl Pts',(1.44591097499994,12.2,3.74101505999998));
#336417=CARTESIAN_POINT('Ctrl Pts',(1.44591097499994,5.2,3.74101505999998));
#336418=CARTESIAN_POINT('Ctrl Pts',(1.44591097499994,2.2,3.74101505999998));
#336419=CARTESIAN_POINT('Ctrl Pts',(1.44569898399994,12.2,3.74058753799999));
#336420=CARTESIAN_POINT('Ctrl Pts',(1.44569898399994,5.2,3.74058753799999));
#336421=CARTESIAN_POINT('Ctrl Pts',(1.44569898399994,2.2,3.74058753799999));
#336422=CARTESIAN_POINT('Ctrl Pts',(1.44549040799994,12.2,3.74016552299998));
#336423=CARTESIAN_POINT('Ctrl Pts',(1.44549040799994,5.2,3.74016552299998));
#336424=CARTESIAN_POINT('Ctrl Pts',(1.44549040799994,2.2,3.74016552299998));
#336425=CARTESIAN_POINT('Ctrl Pts',(1.44528523599994,12.2,3.73974903399999));
#336426=CARTESIAN_POINT('Ctrl Pts',(1.44528523599994,5.2,3.73974903399999));
#336427=CARTESIAN_POINT('Ctrl Pts',(1.44528523599994,2.2,3.73974903399999));
#336428=CARTESIAN_POINT('Ctrl Pts',(1.44508346299994,12.2,3.73933809099999));
#336429=CARTESIAN_POINT('Ctrl Pts',(1.44508346299994,5.2,3.73933809099999));
#336430=CARTESIAN_POINT('Ctrl Pts',(1.44508346299994,2.2,3.73933809099999));
#336431=CARTESIAN_POINT('Ctrl Pts',(1.44488507799994,12.2,3.73893271199999));
#336432=CARTESIAN_POINT('Ctrl Pts',(1.44488507799994,5.2,3.73893271199999));
#336433=CARTESIAN_POINT('Ctrl Pts',(1.44488507799994,2.2,3.73893271199999));
#336434=CARTESIAN_POINT('Ctrl Pts',(1.44469007399994,12.2,3.73853291899999));
#336435=CARTESIAN_POINT('Ctrl Pts',(1.44469007399994,5.2,3.73853291899999));
#336436=CARTESIAN_POINT('Ctrl Pts',(1.44469007399994,2.2,3.73853291899999));
#336437=CARTESIAN_POINT('Ctrl Pts',(1.44449844099994,12.2,3.73813872999998));
#336438=CARTESIAN_POINT('Ctrl Pts',(1.44449844099994,5.2,3.73813872999998));
#336439=CARTESIAN_POINT('Ctrl Pts',(1.44449844099994,2.2,3.73813872999998));
#336440=CARTESIAN_POINT('Ctrl Pts',(1.44431016899994,12.2,3.73775016699998));
#336441=CARTESIAN_POINT('Ctrl Pts',(1.44431016899994,5.2,3.73775016699998));
#336442=CARTESIAN_POINT('Ctrl Pts',(1.44431016899994,2.2,3.73775016699998));
#336443=CARTESIAN_POINT('Ctrl Pts',(1.44412525099994,12.2,3.73736724799999));
#336444=CARTESIAN_POINT('Ctrl Pts',(1.44412525099994,5.2,3.73736724799999));
#336445=CARTESIAN_POINT('Ctrl Pts',(1.44412525099994,2.2,3.73736724799999));
#336446=CARTESIAN_POINT('Ctrl Pts',(1.44394367899994,12.2,3.73698999399998));
#336447=CARTESIAN_POINT('Ctrl Pts',(1.44394367899994,5.2,3.73698999399998));
#336448=CARTESIAN_POINT('Ctrl Pts',(1.44394367899994,2.2,3.73698999399998));
#336449=CARTESIAN_POINT('Ctrl Pts',(1.44376544099994,12.2,3.73661842499998));
#336450=CARTESIAN_POINT('Ctrl Pts',(1.44376544099994,5.2,3.73661842499998));
#336451=CARTESIAN_POINT('Ctrl Pts',(1.44376544099994,2.2,3.73661842499998));
#336452=CARTESIAN_POINT('Ctrl Pts',(1.44359052999994,12.2,3.73625256099999));
#336453=CARTESIAN_POINT('Ctrl Pts',(1.44359052999994,5.2,3.73625256099999));
#336454=CARTESIAN_POINT('Ctrl Pts',(1.44359052999994,2.2,3.73625256099999));
#336455=CARTESIAN_POINT('Ctrl Pts',(1.44341893599994,12.2,3.73589242199999));
#336456=CARTESIAN_POINT('Ctrl Pts',(1.44341893599994,5.2,3.73589242199999));
#336457=CARTESIAN_POINT('Ctrl Pts',(1.44341893599994,2.2,3.73589242199999));
#336458=CARTESIAN_POINT('Ctrl Pts',(1.44325064999994,12.2,3.73553802799999));
#336459=CARTESIAN_POINT('Ctrl Pts',(1.44325064999994,5.2,3.73553802799999));
#336460=CARTESIAN_POINT('Ctrl Pts',(1.44325064999994,2.2,3.73553802799999));
#336461=CARTESIAN_POINT('Ctrl Pts',(1.44308566399994,12.2,3.73518940099999));
#336462=CARTESIAN_POINT('Ctrl Pts',(1.44308566399994,5.2,3.73518940099999));
#336463=CARTESIAN_POINT('Ctrl Pts',(1.44308566399994,2.2,3.73518940099999));
#336464=CARTESIAN_POINT('Ctrl Pts',(1.44292396699994,12.2,3.73484655899999));
#336465=CARTESIAN_POINT('Ctrl Pts',(1.44292396699994,5.2,3.73484655899999));
#336466=CARTESIAN_POINT('Ctrl Pts',(1.44292396699994,2.2,3.73484655899999));
#336467=CARTESIAN_POINT('Ctrl Pts',(1.44276555099994,12.2,3.73450952399998));
#336468=CARTESIAN_POINT('Ctrl Pts',(1.44276555099994,5.2,3.73450952399998));
#336469=CARTESIAN_POINT('Ctrl Pts',(1.44276555099994,2.2,3.73450952399998));
#336470=CARTESIAN_POINT('Ctrl Pts',(1.44261040599994,12.2,3.73417831599999));
#336471=CARTESIAN_POINT('Ctrl Pts',(1.44261040599994,5.2,3.73417831599999));
#336472=CARTESIAN_POINT('Ctrl Pts',(1.44261040599994,2.2,3.73417831599999));
#336473=CARTESIAN_POINT('Ctrl Pts',(1.44245852199994,12.2,3.73385295499999));
#336474=CARTESIAN_POINT('Ctrl Pts',(1.44245852199994,5.2,3.73385295499999));
#336475=CARTESIAN_POINT('Ctrl Pts',(1.44245852199994,2.2,3.73385295499999));
#336476=CARTESIAN_POINT('Ctrl Pts',(1.44230989099994,12.2,3.73353346199998));
#336477=CARTESIAN_POINT('Ctrl Pts',(1.44230989099994,5.2,3.73353346199998));
#336478=CARTESIAN_POINT('Ctrl Pts',(1.44230989099994,2.2,3.73353346199998));
#336479=CARTESIAN_POINT('Ctrl Pts',(1.44216450299994,12.2,3.73321985799999));
#336480=CARTESIAN_POINT('Ctrl Pts',(1.44216450299994,5.2,3.73321985799999));
#336481=CARTESIAN_POINT('Ctrl Pts',(1.44216450299994,2.2,3.73321985799999));
#336482=CARTESIAN_POINT('Ctrl Pts',(1.44202234599994,12.2,3.73291216299998));
#336483=CARTESIAN_POINT('Ctrl Pts',(1.44202234599994,5.2,3.73291216299998));
#336484=CARTESIAN_POINT('Ctrl Pts',(1.44202234599994,2.2,3.73291216299998));
#336485=CARTESIAN_POINT('Ctrl Pts',(1.44188341399994,12.2,3.73261039799999));
#336486=CARTESIAN_POINT('Ctrl Pts',(1.44188341399994,5.2,3.73261039799999));
#336487=CARTESIAN_POINT('Ctrl Pts',(1.44188341399994,2.2,3.73261039799999));
#336488=CARTESIAN_POINT('Ctrl Pts',(1.44174769599994,12.2,3.73231458499999));
#336489=CARTESIAN_POINT('Ctrl Pts',(1.44174769599994,5.2,3.73231458499999));
#336490=CARTESIAN_POINT('Ctrl Pts',(1.44174769599994,2.2,3.73231458499999));
#336491=CARTESIAN_POINT('Ctrl Pts',(1.44161518099994,12.2,3.73202474299998));
#336492=CARTESIAN_POINT('Ctrl Pts',(1.44161518099994,5.2,3.73202474299998));
#336493=CARTESIAN_POINT('Ctrl Pts',(1.44161518099994,2.2,3.73202474299998));
#336494=CARTESIAN_POINT('Ctrl Pts',(1.44148585999994,12.2,3.73174089299999));
#336495=CARTESIAN_POINT('Ctrl Pts',(1.44148585999994,5.2,3.73174089299999));
#336496=CARTESIAN_POINT('Ctrl Pts',(1.44148585999994,2.2,3.73174089299999));
#336497=CARTESIAN_POINT('Ctrl Pts',(1.44135972499994,12.2,3.73146305799998));
#336498=CARTESIAN_POINT('Ctrl Pts',(1.44135972499994,5.2,3.73146305799998));
#336499=CARTESIAN_POINT('Ctrl Pts',(1.44135972499994,2.2,3.73146305799998));
#336500=CARTESIAN_POINT('Ctrl Pts',(1.44123676199994,12.2,3.73119125799998));
#336501=CARTESIAN_POINT('Ctrl Pts',(1.44123676199994,5.2,3.73119125799998));
#336502=CARTESIAN_POINT('Ctrl Pts',(1.44123676199994,2.2,3.73119125799998));
#336503=CARTESIAN_POINT('Ctrl Pts',(1.44111696499994,12.2,3.73092551199999));
#336504=CARTESIAN_POINT('Ctrl Pts',(1.44111696499994,5.2,3.73092551199999));
#336505=CARTESIAN_POINT('Ctrl Pts',(1.44111696499994,2.2,3.73092551199999));
#336506=CARTESIAN_POINT('Ctrl Pts',(1.44100032099994,12.2,3.73066584399999));
#336507=CARTESIAN_POINT('Ctrl Pts',(1.44100032099994,5.2,3.73066584399999));
#336508=CARTESIAN_POINT('Ctrl Pts',(1.44100032099994,2.2,3.73066584399999));
#336509=CARTESIAN_POINT('Ctrl Pts',(1.44088682199994,12.2,3.73041227499999));
#336510=CARTESIAN_POINT('Ctrl Pts',(1.44088682199994,5.2,3.73041227499999));
#336511=CARTESIAN_POINT('Ctrl Pts',(1.44088682199994,2.2,3.73041227499999));
#336512=CARTESIAN_POINT('Ctrl Pts',(1.44077645799994,12.2,3.73016482399999));
#336513=CARTESIAN_POINT('Ctrl Pts',(1.44077645799994,5.2,3.73016482399999));
#336514=CARTESIAN_POINT('Ctrl Pts',(1.44077645799994,2.2,3.73016482399999));
#336515=CARTESIAN_POINT('Ctrl Pts',(1.44066921699994,12.2,3.72992351399999));
#336516=CARTESIAN_POINT('Ctrl Pts',(1.44066921699994,5.2,3.72992351399999));
#336517=CARTESIAN_POINT('Ctrl Pts',(1.44066921699994,2.2,3.72992351399999));
#336518=CARTESIAN_POINT('Ctrl Pts',(1.44056508899994,12.2,3.72968836699999));
#336519=CARTESIAN_POINT('Ctrl Pts',(1.44056508899994,5.2,3.72968836699999));
#336520=CARTESIAN_POINT('Ctrl Pts',(1.44056508899994,2.2,3.72968836699999));
#336521=CARTESIAN_POINT('Ctrl Pts',(1.44046406499994,12.2,3.72945940399998));
#336522=CARTESIAN_POINT('Ctrl Pts',(1.44046406499994,5.2,3.72945940399998));
#336523=CARTESIAN_POINT('Ctrl Pts',(1.44046406499994,2.2,3.72945940399998));
#336524=CARTESIAN_POINT('Ctrl Pts',(1.44036613299994,12.2,3.72923664599998));
#336525=CARTESIAN_POINT('Ctrl Pts',(1.44036613299994,5.2,3.72923664599998));
#336526=CARTESIAN_POINT('Ctrl Pts',(1.44036613299994,2.2,3.72923664599998));
#336527=CARTESIAN_POINT('Ctrl Pts',(1.44027128399994,12.2,3.72902011499999));
#336528=CARTESIAN_POINT('Ctrl Pts',(1.44027128399994,5.2,3.72902011499999));
#336529=CARTESIAN_POINT('Ctrl Pts',(1.44027128399994,2.2,3.72902011499999));
#336530=CARTESIAN_POINT('Ctrl Pts',(1.44017950699994,12.2,3.72880983299999));
#336531=CARTESIAN_POINT('Ctrl Pts',(1.44017950699994,5.2,3.72880983299999));
#336532=CARTESIAN_POINT('Ctrl Pts',(1.44017950699994,2.2,3.72880983299999));
#336533=CARTESIAN_POINT('Ctrl Pts',(1.44009079099994,12.2,3.72860581999999));
#336534=CARTESIAN_POINT('Ctrl Pts',(1.44009079099994,5.2,3.72860581999999));
#336535=CARTESIAN_POINT('Ctrl Pts',(1.44009079099994,2.2,3.72860581999999));
#336536=CARTESIAN_POINT('Ctrl Pts',(1.44000512699994,12.2,3.72840809899999));
#336537=CARTESIAN_POINT('Ctrl Pts',(1.44000512699994,5.2,3.72840809899999));
#336538=CARTESIAN_POINT('Ctrl Pts',(1.44000512699994,2.2,3.72840809899999));
#336539=CARTESIAN_POINT('Ctrl Pts',(1.43992250199994,12.2,3.72821669299999));
#336540=CARTESIAN_POINT('Ctrl Pts',(1.43992250199994,5.2,3.72821669299999));
#336541=CARTESIAN_POINT('Ctrl Pts',(1.43992250199994,2.2,3.72821669299999));
#336542=CARTESIAN_POINT('Ctrl Pts',(1.43984290599994,12.2,3.72803162199999));
#336543=CARTESIAN_POINT('Ctrl Pts',(1.43984290599994,5.2,3.72803162199999));
#336544=CARTESIAN_POINT('Ctrl Pts',(1.43984290599994,2.2,3.72803162199999));
#336545=CARTESIAN_POINT('Ctrl Pts',(1.43976632799994,12.2,3.72785290999998));
#336546=CARTESIAN_POINT('Ctrl Pts',(1.43976632799994,5.2,3.72785290999998));
#336547=CARTESIAN_POINT('Ctrl Pts',(1.43976632799994,2.2,3.72785290999998));
#336548=CARTESIAN_POINT('Ctrl Pts',(1.43969275699994,12.2,3.72768057899999));
#336549=CARTESIAN_POINT('Ctrl Pts',(1.43969275699994,5.2,3.72768057899999));
#336550=CARTESIAN_POINT('Ctrl Pts',(1.43969275699994,2.2,3.72768057899999));
#336551=CARTESIAN_POINT('Ctrl Pts',(1.43962218299994,12.2,3.72751464899999));
#336552=CARTESIAN_POINT('Ctrl Pts',(1.43962218299994,5.2,3.72751464899999));
#336553=CARTESIAN_POINT('Ctrl Pts',(1.43962218299994,2.2,3.72751464899999));
#336554=CARTESIAN_POINT('Ctrl Pts',(1.43955459499994,12.2,3.72735514399999));
#336555=CARTESIAN_POINT('Ctrl Pts',(1.43955459499994,5.2,3.72735514399999));
#336556=CARTESIAN_POINT('Ctrl Pts',(1.43955459499994,2.2,3.72735514399999));
#336557=CARTESIAN_POINT('Ctrl Pts',(1.43948998199994,12.2,3.72720208399999));
#336558=CARTESIAN_POINT('Ctrl Pts',(1.43948998199994,5.2,3.72720208399999));
#336559=CARTESIAN_POINT('Ctrl Pts',(1.43948998199994,2.2,3.72720208399999));
#336560=CARTESIAN_POINT('Ctrl Pts',(1.43942833299994,12.2,3.72705549099998));
#336561=CARTESIAN_POINT('Ctrl Pts',(1.43942833299994,5.2,3.72705549099998));
#336562=CARTESIAN_POINT('Ctrl Pts',(1.43942833299994,2.2,3.72705549099998));
#336563=CARTESIAN_POINT('Ctrl Pts',(1.43936963499994,12.2,3.72691538999998));
#336564=CARTESIAN_POINT('Ctrl Pts',(1.43936963499994,5.2,3.72691538999998));
#336565=CARTESIAN_POINT('Ctrl Pts',(1.43936963499994,2.2,3.72691538999998));
#336566=CARTESIAN_POINT('Ctrl Pts',(1.43931387899994,12.2,3.72678180299998));
#336567=CARTESIAN_POINT('Ctrl Pts',(1.43931387899994,5.2,3.72678180299998));
#336568=CARTESIAN_POINT('Ctrl Pts',(1.43931387899994,2.2,3.72678180299998));
#336569=CARTESIAN_POINT('Ctrl Pts',(1.43926105099994,12.2,3.72665475399998));
#336570=CARTESIAN_POINT('Ctrl Pts',(1.43926105099994,5.2,3.72665475399998));
#336571=CARTESIAN_POINT('Ctrl Pts',(1.43926105099994,2.2,3.72665475399998));
#336572=CARTESIAN_POINT('Ctrl Pts',(1.43921114099994,12.2,3.72653426499999));
#336573=CARTESIAN_POINT('Ctrl Pts',(1.43921114099994,5.2,3.72653426499999));
#336574=CARTESIAN_POINT('Ctrl Pts',(1.43921114099994,2.2,3.72653426499999));
#336575=CARTESIAN_POINT('Ctrl Pts',(1.43916413499994,12.2,3.72642036099998));
#336576=CARTESIAN_POINT('Ctrl Pts',(1.43916413499994,5.2,3.72642036099998));
#336577=CARTESIAN_POINT('Ctrl Pts',(1.43916413499994,2.2,3.72642036099998));
#336578=CARTESIAN_POINT('Ctrl Pts',(1.43912002499994,12.2,3.72631305999998));
#336579=CARTESIAN_POINT('Ctrl Pts',(1.43912002499994,5.2,3.72631305999998));
#336580=CARTESIAN_POINT('Ctrl Pts',(1.43912002499994,2.2,3.72631305999998));
#336581=CARTESIAN_POINT('Ctrl Pts',(1.43907880099994,12.2,3.72621238199999));
#336582=CARTESIAN_POINT('Ctrl Pts',(1.43907880099994,5.2,3.72621238199999));
#336583=CARTESIAN_POINT('Ctrl Pts',(1.43907880099994,2.2,3.72621238199999));
#336584=CARTESIAN_POINT('Ctrl Pts',(1.43904044999994,12.2,3.72611834999999));
#336585=CARTESIAN_POINT('Ctrl Pts',(1.43904044999994,5.2,3.72611834999999));
#336586=CARTESIAN_POINT('Ctrl Pts',(1.43904044999994,2.2,3.72611834999999));
#336587=CARTESIAN_POINT('Ctrl Pts',(1.43900496299994,12.2,3.72603098699999));
#336588=CARTESIAN_POINT('Ctrl Pts',(1.43900496299994,5.2,3.72603098699999));
#336589=CARTESIAN_POINT('Ctrl Pts',(1.43900496299994,2.2,3.72603098699999));
#336590=CARTESIAN_POINT('Ctrl Pts',(1.43897232399994,12.2,3.72595031699999));
#336591=CARTESIAN_POINT('Ctrl Pts',(1.43897232399994,5.2,3.72595031699999));
#336592=CARTESIAN_POINT('Ctrl Pts',(1.43897232399994,2.2,3.72595031699999));
#336593=CARTESIAN_POINT('Ctrl Pts',(1.43894251899994,12.2,3.72587637199998));
#336594=CARTESIAN_POINT('Ctrl Pts',(1.43894251899994,5.2,3.72587637199998));
#336595=CARTESIAN_POINT('Ctrl Pts',(1.43894251899994,2.2,3.72587637199998));
#336596=CARTESIAN_POINT('Ctrl Pts',(1.43891553299994,12.2,3.72580917999999));
#336597=CARTESIAN_POINT('Ctrl Pts',(1.43891553299994,5.2,3.72580917999999));
#336598=CARTESIAN_POINT('Ctrl Pts',(1.43891553299994,2.2,3.72580917999999));
#336599=CARTESIAN_POINT('Ctrl Pts',(1.43889135199994,12.2,3.72574876699999));
#336600=CARTESIAN_POINT('Ctrl Pts',(1.43889135199994,5.2,3.72574876699999));
#336601=CARTESIAN_POINT('Ctrl Pts',(1.43889135199994,2.2,3.72574876699999));
#336602=CARTESIAN_POINT('Ctrl Pts',(1.43886996799994,12.2,3.72569515099999));
#336603=CARTESIAN_POINT('Ctrl Pts',(1.43886996799994,5.2,3.72569515099999));
#336604=CARTESIAN_POINT('Ctrl Pts',(1.43886996799994,2.2,3.72569515099999));
#336605=CARTESIAN_POINT('Ctrl Pts',(1.43884938350029,12.2,3.72564333328053));
#336606=CARTESIAN_POINT('Ctrl Pts',(1.43884938350029,5.2,3.72564333328053));
#336607=CARTESIAN_POINT('Ctrl Pts',(1.43884938350029,2.2,3.72564333328053));
#336608=CARTESIAN_POINT('Ctrl Pts',(1.43883538351011,12.2,3.72560788388561));
#336609=CARTESIAN_POINT('Ctrl Pts',(1.43883538351011,5.2,3.72560788388561));
#336610=CARTESIAN_POINT('Ctrl Pts',(1.43883538351011,2.2,3.72560788388561));
#336611=CARTESIAN_POINT('Ctrl Pts',(1.43882621103565,12.2,3.72558451224687));
#336612=CARTESIAN_POINT('Ctrl Pts',(1.43882621103565,5.2,3.72558451224687));
#336613=CARTESIAN_POINT('Ctrl Pts',(1.43882621103565,2.2,3.72558451224687));
#336614=CARTESIAN_POINT('Ctrl Pts',(1.43882053151532,12.2,3.72556994107896));
#336615=CARTESIAN_POINT('Ctrl Pts',(1.43882053151532,5.2,3.72556994107896));
#336616=CARTESIAN_POINT('Ctrl Pts',(1.43882053151532,2.2,3.72556994107896));
#336617=CARTESIAN_POINT('Ctrl Pts',(1.43881701799994,12.2,3.72556094399998));
#336618=CARTESIAN_POINT('Ctrl Pts',(1.43881701799994,5.2,3.72556094399998));
#336619=CARTESIAN_POINT('Ctrl Pts',(1.43881701799994,2.2,3.72556094399998));
#336620=CARTESIAN_POINT('',(2.02484994999994,12.2,4.29679911999998));
#336621=CARTESIAN_POINT('Origin',(-5.66300478732629E-14,15.2,-1.77635683940025E-14));
#336622=CARTESIAN_POINT('',(2.32438124199994,12.2,4.14243308299999));
#336623=CARTESIAN_POINT('Ctrl Pts',(2.19921389299994,12.2,3.33366470799999));
#336624=CARTESIAN_POINT('Ctrl Pts',(2.19921389299994,5.2,3.33366470799999));
#336625=CARTESIAN_POINT('Ctrl Pts',(2.19921389299994,2.2,3.33366470799999));
#336626=CARTESIAN_POINT('Ctrl Pts',(2.19921763978639,12.2,3.33367043367347));
#336627=CARTESIAN_POINT('Ctrl Pts',(2.19921763978639,5.2,3.33367043367347));
#336628=CARTESIAN_POINT('Ctrl Pts',(2.19921763978639,2.2,3.33367043367347));
#336629=CARTESIAN_POINT('Ctrl Pts',(2.19922488336832,12.2,3.3336815089074));
#336630=CARTESIAN_POINT('Ctrl Pts',(2.19922488336832,5.2,3.3336815089074));
#336631=CARTESIAN_POINT('Ctrl Pts',(2.19922488336832,2.2,3.3336815089074));
#336632=CARTESIAN_POINT('Ctrl Pts',(2.19923563657748,12.2,3.33369793329671));
#336633=CARTESIAN_POINT('Ctrl Pts',(2.19923563657748,5.19999999999999,3.33369793329671));
#336634=CARTESIAN_POINT('Ctrl Pts',(2.19923563657748,2.2,3.33369793329671));
#336635=CARTESIAN_POINT('Ctrl Pts',(2.19924982935574,12.2,3.3337196857409));
#336636=CARTESIAN_POINT('Ctrl Pts',(2.19924982935574,5.19999999999999,3.3337196857409));
#336637=CARTESIAN_POINT('Ctrl Pts',(2.19924982935574,2.2,3.3337196857409));
#336638=CARTESIAN_POINT('Ctrl Pts',(2.19927450199994,12.2,3.33375771899998));
#336639=CARTESIAN_POINT('Ctrl Pts',(2.19927450199994,5.2,3.33375771899998));
#336640=CARTESIAN_POINT('Ctrl Pts',(2.19927450199994,2.2,3.33375771899998));
#336641=CARTESIAN_POINT('Ctrl Pts',(2.19930183199994,12.2,3.33380002299998));
#336642=CARTESIAN_POINT('Ctrl Pts',(2.19930183199994,5.2,3.33380002299998));
#336643=CARTESIAN_POINT('Ctrl Pts',(2.19930183199994,2.2,3.33380002299998));
#336644=CARTESIAN_POINT('Ctrl Pts',(2.19933308799994,12.2,3.33384855099998));
#336645=CARTESIAN_POINT('Ctrl Pts',(2.19933308799994,5.2,3.33384855099998));
#336646=CARTESIAN_POINT('Ctrl Pts',(2.19933308799994,2.2,3.33384855099998));
#336647=CARTESIAN_POINT('Ctrl Pts',(2.19936825899994,12.2,3.33390330099999));
#336648=CARTESIAN_POINT('Ctrl Pts',(2.19936825899994,5.2,3.33390330099999));
#336649=CARTESIAN_POINT('Ctrl Pts',(2.19936825899994,2.2,3.33390330099999));
#336650=CARTESIAN_POINT('Ctrl Pts',(2.19940732099994,12.2,3.33396426999998));
#336651=CARTESIAN_POINT('Ctrl Pts',(2.19940732099994,5.2,3.33396426999998));
#336652=CARTESIAN_POINT('Ctrl Pts',(2.19940732099994,2.2,3.33396426999998));
#336653=CARTESIAN_POINT('Ctrl Pts',(2.19945024699994,12.2,3.33403145199998));
#336654=CARTESIAN_POINT('Ctrl Pts',(2.19945024699994,5.2,3.33403145199998));
#336655=CARTESIAN_POINT('Ctrl Pts',(2.19945024699994,2.2,3.33403145199998));
#336656=CARTESIAN_POINT('Ctrl Pts',(2.19949700499994,12.2,3.33410484499999));
#336657=CARTESIAN_POINT('Ctrl Pts',(2.19949700499994,5.2,3.33410484499999));
#336658=CARTESIAN_POINT('Ctrl Pts',(2.19949700499994,2.2,3.33410484499999));
#336659=CARTESIAN_POINT('Ctrl Pts',(2.19954756299995,12.2,3.33418444299999));
#336660=CARTESIAN_POINT('Ctrl Pts',(2.19954756299995,5.2,3.33418444299999));
#336661=CARTESIAN_POINT('Ctrl Pts',(2.19954756299995,2.2,3.33418444299999));
#336662=CARTESIAN_POINT('Ctrl Pts',(2.19960188999994,12.2,3.33427024099999));
#336663=CARTESIAN_POINT('Ctrl Pts',(2.19960188999994,5.2,3.33427024099999));
#336664=CARTESIAN_POINT('Ctrl Pts',(2.19960188999994,2.2,3.33427024099999));
#336665=CARTESIAN_POINT('Ctrl Pts',(2.19965995999994,12.2,3.33436223599998));
#336666=CARTESIAN_POINT('Ctrl Pts',(2.19965995999994,5.2,3.33436223599998));
#336667=CARTESIAN_POINT('Ctrl Pts',(2.19965995999994,2.2,3.33436223599998));
#336668=CARTESIAN_POINT('Ctrl Pts',(2.19972175099994,12.2,3.33446042499999));
#336669=CARTESIAN_POINT('Ctrl Pts',(2.19972175099994,5.2,3.33446042499999));
#336670=CARTESIAN_POINT('Ctrl Pts',(2.19972175099994,2.2,3.33446042499999));
#336671=CARTESIAN_POINT('Ctrl Pts',(2.19978724099994,12.2,3.33456480399998));
#336672=CARTESIAN_POINT('Ctrl Pts',(2.19978724099994,5.2,3.33456480399998));
#336673=CARTESIAN_POINT('Ctrl Pts',(2.19978724099994,2.2,3.33456480399998));
#336674=CARTESIAN_POINT('Ctrl Pts',(2.19985640599994,12.2,3.33467536999999));
#336675=CARTESIAN_POINT('Ctrl Pts',(2.19985640599994,5.2,3.33467536999999));
#336676=CARTESIAN_POINT('Ctrl Pts',(2.19985640599994,2.2,3.33467536999999));
#336677=CARTESIAN_POINT('Ctrl Pts',(2.19992921999994,12.2,3.33479211899999));
#336678=CARTESIAN_POINT('Ctrl Pts',(2.19992921999994,5.2,3.33479211899999));
#336679=CARTESIAN_POINT('Ctrl Pts',(2.19992921999994,2.2,3.33479211899999));
#336680=CARTESIAN_POINT('Ctrl Pts',(2.20000566099994,12.2,3.33491504499998));
#336681=CARTESIAN_POINT('Ctrl Pts',(2.20000566099994,5.2,3.33491504499998));
#336682=CARTESIAN_POINT('Ctrl Pts',(2.20000566099994,2.2,3.33491504499998));
#336683=CARTESIAN_POINT('Ctrl Pts',(2.20008569999994,12.2,3.33504414799998));
#336684=CARTESIAN_POINT('Ctrl Pts',(2.20008569999994,5.2,3.33504414799998));
#336685=CARTESIAN_POINT('Ctrl Pts',(2.20008569999994,2.2,3.33504414799998));
#336686=CARTESIAN_POINT('Ctrl Pts',(2.20016931299994,12.2,3.33517942099999));
#336687=CARTESIAN_POINT('Ctrl Pts',(2.20016931299994,5.2,3.33517942099999));
#336688=CARTESIAN_POINT('Ctrl Pts',(2.20016931299994,2.2,3.33517942099999));
#336689=CARTESIAN_POINT('Ctrl Pts',(2.20025647299994,12.2,3.33532086199998));
#336690=CARTESIAN_POINT('Ctrl Pts',(2.20025647299994,5.2,3.33532086199998));
#336691=CARTESIAN_POINT('Ctrl Pts',(2.20025647299994,2.2,3.33532086199998));
#336692=CARTESIAN_POINT('Ctrl Pts',(2.20034715699994,12.2,3.33546846599998));
#336693=CARTESIAN_POINT('Ctrl Pts',(2.20034715699994,5.2,3.33546846599998));
#336694=CARTESIAN_POINT('Ctrl Pts',(2.20034715699994,2.2,3.33546846599998));
#336695=CARTESIAN_POINT('Ctrl Pts',(2.20044133899994,12.2,3.33562222799999));
#336696=CARTESIAN_POINT('Ctrl Pts',(2.20044133899994,5.2,3.33562222799999));
#336697=CARTESIAN_POINT('Ctrl Pts',(2.20044133899994,2.2,3.33562222799999));
#336698=CARTESIAN_POINT('Ctrl Pts',(2.20053899599994,12.2,3.33578214599999));
#336699=CARTESIAN_POINT('Ctrl Pts',(2.20053899599994,5.2,3.33578214599999));
#336700=CARTESIAN_POINT('Ctrl Pts',(2.20053899599994,2.2,3.33578214599999));
#336701=CARTESIAN_POINT('Ctrl Pts',(2.20064010499994,12.2,3.33594821699998));
#336702=CARTESIAN_POINT('Ctrl Pts',(2.20064010499994,5.2,3.33594821699998));
#336703=CARTESIAN_POINT('Ctrl Pts',(2.20064010499994,2.2,3.33594821699998));
#336704=CARTESIAN_POINT('Ctrl Pts',(2.20074464099994,12.2,3.33612043399999));
#336705=CARTESIAN_POINT('Ctrl Pts',(2.20074464099994,5.2,3.33612043399999));
#336706=CARTESIAN_POINT('Ctrl Pts',(2.20074464099994,2.2,3.33612043399999));
#336707=CARTESIAN_POINT('Ctrl Pts',(2.20085257799994,12.2,3.33629879499998));
#336708=CARTESIAN_POINT('Ctrl Pts',(2.20085257799994,5.2,3.33629879499998));
#336709=CARTESIAN_POINT('Ctrl Pts',(2.20085257799994,2.2,3.33629879499998));
#336710=CARTESIAN_POINT('Ctrl Pts',(2.20096389399994,12.2,3.33648329599999));
#336711=CARTESIAN_POINT('Ctrl Pts',(2.20096389399994,5.2,3.33648329599999));
#336712=CARTESIAN_POINT('Ctrl Pts',(2.20096389399994,2.2,3.33648329599999));
#336713=CARTESIAN_POINT('Ctrl Pts',(2.20107856499994,12.2,3.33667393299999));
#336714=CARTESIAN_POINT('Ctrl Pts',(2.20107856499994,5.2,3.33667393299999));
#336715=CARTESIAN_POINT('Ctrl Pts',(2.20107856499994,2.2,3.33667393299999));
#336716=CARTESIAN_POINT('Ctrl Pts',(2.20119656499994,12.2,3.33687070099998));
#336717=CARTESIAN_POINT('Ctrl Pts',(2.20119656499994,5.2,3.33687070099998));
#336718=CARTESIAN_POINT('Ctrl Pts',(2.20119656499994,2.2,3.33687070099998));
#336719=CARTESIAN_POINT('Ctrl Pts',(2.20131787099994,12.2,3.33707359699999));
#336720=CARTESIAN_POINT('Ctrl Pts',(2.20131787099994,5.2,3.33707359699999));
#336721=CARTESIAN_POINT('Ctrl Pts',(2.20131787099994,2.2,3.33707359699999));
#336722=CARTESIAN_POINT('Ctrl Pts',(2.20144245999994,12.2,3.33728261799998));
#336723=CARTESIAN_POINT('Ctrl Pts',(2.20144245999994,5.2,3.33728261799998));
#336724=CARTESIAN_POINT('Ctrl Pts',(2.20144245999994,2.2,3.33728261799998));
#336725=CARTESIAN_POINT('Ctrl Pts',(2.20157030699994,12.2,3.33749775599999));
#336726=CARTESIAN_POINT('Ctrl Pts',(2.20157030699994,5.2,3.33749775599999));
#336727=CARTESIAN_POINT('Ctrl Pts',(2.20157030699994,2.2,3.33749775599999));
#336728=CARTESIAN_POINT('Ctrl Pts',(2.20170139099995,12.2,3.33771901199999));
#336729=CARTESIAN_POINT('Ctrl Pts',(2.20170139099995,5.2,3.33771901199999));
#336730=CARTESIAN_POINT('Ctrl Pts',(2.20170139099995,2.2,3.33771901199999));
#336731=CARTESIAN_POINT('Ctrl Pts',(2.20183568599994,12.2,3.33794637799999));
#336732=CARTESIAN_POINT('Ctrl Pts',(2.20183568599994,5.2,3.33794637799999));
#336733=CARTESIAN_POINT('Ctrl Pts',(2.20183568599994,2.2,3.33794637799999));
#336734=CARTESIAN_POINT('Ctrl Pts',(2.20197316999994,12.2,3.33817985299999));
#336735=CARTESIAN_POINT('Ctrl Pts',(2.20197316999994,5.2,3.33817985299999));
#336736=CARTESIAN_POINT('Ctrl Pts',(2.20197316999994,2.2,3.33817985299999));
#336737=CARTESIAN_POINT('Ctrl Pts',(2.20211381899994,12.2,3.33841942999998));
#336738=CARTESIAN_POINT('Ctrl Pts',(2.20211381899994,5.2,3.33841942999998));
#336739=CARTESIAN_POINT('Ctrl Pts',(2.20211381899994,2.2,3.33841942999998));
#336740=CARTESIAN_POINT('Ctrl Pts',(2.20225760999994,12.2,3.33866510799999));
#336741=CARTESIAN_POINT('Ctrl Pts',(2.20225760999994,5.2,3.33866510799999));
#336742=CARTESIAN_POINT('Ctrl Pts',(2.20225760999994,2.2,3.33866510799999));
#336743=CARTESIAN_POINT('Ctrl Pts',(2.20240451999994,12.2,3.33891687999999));
#336744=CARTESIAN_POINT('Ctrl Pts',(2.20240451999994,5.2,3.33891687999999));
#336745=CARTESIAN_POINT('Ctrl Pts',(2.20240451999994,2.2,3.33891687999999));
#336746=CARTESIAN_POINT('Ctrl Pts',(2.20255452499994,12.2,3.33917474399998));
#336747=CARTESIAN_POINT('Ctrl Pts',(2.20255452499994,5.2,3.33917474399998));
#336748=CARTESIAN_POINT('Ctrl Pts',(2.20255452499994,2.2,3.33917474399998));
#336749=CARTESIAN_POINT('Ctrl Pts',(2.20270760299994,12.2,3.33943869499999));
#336750=CARTESIAN_POINT('Ctrl Pts',(2.20270760299994,5.2,3.33943869499999));
#336751=CARTESIAN_POINT('Ctrl Pts',(2.20270760299994,2.2,3.33943869499999));
#336752=CARTESIAN_POINT('Ctrl Pts',(2.20286373099994,12.2,3.33970872899998));
#336753=CARTESIAN_POINT('Ctrl Pts',(2.20286373099994,5.2,3.33970872899998));
#336754=CARTESIAN_POINT('Ctrl Pts',(2.20286373099994,2.2,3.33970872899998));
#336755=CARTESIAN_POINT('Ctrl Pts',(2.20302288599994,12.2,3.33998484099999));
#336756=CARTESIAN_POINT('Ctrl Pts',(2.20302288599994,5.2,3.33998484099999));
#336757=CARTESIAN_POINT('Ctrl Pts',(2.20302288599994,2.2,3.33998484099999));
#336758=CARTESIAN_POINT('Ctrl Pts',(2.20318504499994,12.2,3.34026702899998));
#336759=CARTESIAN_POINT('Ctrl Pts',(2.20318504499994,5.2,3.34026702899998));
#336760=CARTESIAN_POINT('Ctrl Pts',(2.20318504499994,2.2,3.34026702899998));
#336761=CARTESIAN_POINT('Ctrl Pts',(2.20335018599994,12.2,3.34055528599999));
#336762=CARTESIAN_POINT('Ctrl Pts',(2.20335018599994,5.2,3.34055528599999));
#336763=CARTESIAN_POINT('Ctrl Pts',(2.20335018599994,2.2,3.34055528599999));
#336764=CARTESIAN_POINT('Ctrl Pts',(2.20351828599994,12.2,3.34084961099999));
#336765=CARTESIAN_POINT('Ctrl Pts',(2.20351828599994,5.2,3.34084961099999));
#336766=CARTESIAN_POINT('Ctrl Pts',(2.20351828599994,2.2,3.34084961099999));
#336767=CARTESIAN_POINT('Ctrl Pts',(2.20368932299994,12.2,3.34114999699998));
#336768=CARTESIAN_POINT('Ctrl Pts',(2.20368932299994,5.2,3.34114999699998));
#336769=CARTESIAN_POINT('Ctrl Pts',(2.20368932299994,2.2,3.34114999699998));
#336770=CARTESIAN_POINT('Ctrl Pts',(2.20386327299994,12.2,3.34145644199998));
#336771=CARTESIAN_POINT('Ctrl Pts',(2.20386327299994,5.2,3.34145644199998));
#336772=CARTESIAN_POINT('Ctrl Pts',(2.20386327299994,2.2,3.34145644199998));
#336773=CARTESIAN_POINT('Ctrl Pts',(2.20404011499994,12.2,3.34176893899999));
#336774=CARTESIAN_POINT('Ctrl Pts',(2.20404011499994,5.2,3.34176893899999));
#336775=CARTESIAN_POINT('Ctrl Pts',(2.20404011499994,2.2,3.34176893899999));
#336776=CARTESIAN_POINT('Ctrl Pts',(2.20421982799994,12.2,3.34208748699999));
#336777=CARTESIAN_POINT('Ctrl Pts',(2.20421982799994,5.2,3.34208748699999));
#336778=CARTESIAN_POINT('Ctrl Pts',(2.20421982799994,2.2,3.34208748699999));
#336779=CARTESIAN_POINT('Ctrl Pts',(2.20440238699994,12.2,3.34241207999998));
#336780=CARTESIAN_POINT('Ctrl Pts',(2.20440238699994,5.2,3.34241207999998));
#336781=CARTESIAN_POINT('Ctrl Pts',(2.20440238699994,2.2,3.34241207999998));
#336782=CARTESIAN_POINT('Ctrl Pts',(2.20458777199994,12.2,3.34274271399998));
#336783=CARTESIAN_POINT('Ctrl Pts',(2.20458777199994,5.2,3.34274271399998));
#336784=CARTESIAN_POINT('Ctrl Pts',(2.20458777199994,2.2,3.34274271399998));
#336785=CARTESIAN_POINT('Ctrl Pts',(2.20477595999994,12.2,3.34307938399999));
#336786=CARTESIAN_POINT('Ctrl Pts',(2.20477595999994,5.2,3.34307938399999));
#336787=CARTESIAN_POINT('Ctrl Pts',(2.20477595999994,2.2,3.34307938399999));
#336788=CARTESIAN_POINT('Ctrl Pts',(2.20496692899994,12.2,3.34342208699999));
#336789=CARTESIAN_POINT('Ctrl Pts',(2.20496692899994,5.2,3.34342208699999));
#336790=CARTESIAN_POINT('Ctrl Pts',(2.20496692899994,2.2,3.34342208699999));
#336791=CARTESIAN_POINT('Ctrl Pts',(2.20516065799994,12.2,3.34377081999998));
#336792=CARTESIAN_POINT('Ctrl Pts',(2.20516065799994,5.2,3.34377081999998));
#336793=CARTESIAN_POINT('Ctrl Pts',(2.20516065799994,2.2,3.34377081999998));
#336794=CARTESIAN_POINT('Ctrl Pts',(2.20535712399994,12.2,3.34412557399999));
#336795=CARTESIAN_POINT('Ctrl Pts',(2.20535712399994,5.2,3.34412557399999));
#336796=CARTESIAN_POINT('Ctrl Pts',(2.20535712399994,2.2,3.34412557399999));
#336797=CARTESIAN_POINT('Ctrl Pts',(2.20555630599994,12.2,3.34448634899999));
#336798=CARTESIAN_POINT('Ctrl Pts',(2.20555630599994,5.2,3.34448634899999));
#336799=CARTESIAN_POINT('Ctrl Pts',(2.20555630599994,2.2,3.34448634899999));
#336800=CARTESIAN_POINT('Ctrl Pts',(2.20575818299994,12.2,3.34485313999998));
#336801=CARTESIAN_POINT('Ctrl Pts',(2.20575818299994,5.2,3.34485313999998));
#336802=CARTESIAN_POINT('Ctrl Pts',(2.20575818299994,2.2,3.34485313999998));
#336803=CARTESIAN_POINT('Ctrl Pts',(2.20596273199994,12.2,3.34522594199999));
#336804=CARTESIAN_POINT('Ctrl Pts',(2.20596273199994,5.2,3.34522594199999));
#336805=CARTESIAN_POINT('Ctrl Pts',(2.20596273199994,2.2,3.34522594199999));
#336806=CARTESIAN_POINT('Ctrl Pts',(2.20616993299994,12.2,3.34560474899998));
#336807=CARTESIAN_POINT('Ctrl Pts',(2.20616993299994,5.2,3.34560474899998));
#336808=CARTESIAN_POINT('Ctrl Pts',(2.20616993299994,2.2,3.34560474899998));
#336809=CARTESIAN_POINT('Ctrl Pts',(2.20637976299995,12.2,3.34598955999999));
#336810=CARTESIAN_POINT('Ctrl Pts',(2.20637976299995,5.2,3.34598955999999));
#336811=CARTESIAN_POINT('Ctrl Pts',(2.20637976299995,2.2,3.34598955999999));
#336812=CARTESIAN_POINT('Ctrl Pts',(2.20659220199994,12.2,3.34638036899998));
#336813=CARTESIAN_POINT('Ctrl Pts',(2.20659220199994,5.2,3.34638036899998));
#336814=CARTESIAN_POINT('Ctrl Pts',(2.20659220199994,2.2,3.34638036899998));
#336815=CARTESIAN_POINT('Ctrl Pts',(2.20680722799994,12.2,3.34677717099999));
#336816=CARTESIAN_POINT('Ctrl Pts',(2.20680722799994,5.2,3.34677717099999));
#336817=CARTESIAN_POINT('Ctrl Pts',(2.20680722799994,2.2,3.34677717099999));
#336818=CARTESIAN_POINT('Ctrl Pts',(2.20702481999994,12.2,3.34717996199998));
#336819=CARTESIAN_POINT('Ctrl Pts',(2.20702481999994,5.2,3.34717996199998));
#336820=CARTESIAN_POINT('Ctrl Pts',(2.20702481999994,2.2,3.34717996199998));
#336821=CARTESIAN_POINT('Ctrl Pts',(2.20724495699994,12.2,3.34758873899998));
#336822=CARTESIAN_POINT('Ctrl Pts',(2.20724495699994,5.2,3.34758873899998));
#336823=CARTESIAN_POINT('Ctrl Pts',(2.20724495699994,2.2,3.34758873899998));
#336824=CARTESIAN_POINT('Ctrl Pts',(2.20746761799994,12.2,3.34800349499999));
#336825=CARTESIAN_POINT('Ctrl Pts',(2.20746761799994,5.2,3.34800349499999));
#336826=CARTESIAN_POINT('Ctrl Pts',(2.20746761799994,2.2,3.34800349499999));
#336827=CARTESIAN_POINT('Ctrl Pts',(2.20769278099994,12.2,3.34842422799999));
#336828=CARTESIAN_POINT('Ctrl Pts',(2.20769278099994,5.2,3.34842422799999));
#336829=CARTESIAN_POINT('Ctrl Pts',(2.20769278099994,2.2,3.34842422799999));
#336830=CARTESIAN_POINT('Ctrl Pts',(2.20792042699994,12.2,3.34885093299999));
#336831=CARTESIAN_POINT('Ctrl Pts',(2.20792042699994,5.2,3.34885093299999));
#336832=CARTESIAN_POINT('Ctrl Pts',(2.20792042699994,2.2,3.34885093299999));
#336833=CARTESIAN_POINT('Ctrl Pts',(2.20815053399994,12.2,3.34928360399999));
#336834=CARTESIAN_POINT('Ctrl Pts',(2.20815053399994,5.2,3.34928360399999));
#336835=CARTESIAN_POINT('Ctrl Pts',(2.20815053399994,2.2,3.34928360399999));
#336836=CARTESIAN_POINT('Ctrl Pts',(2.20838308099994,12.2,3.34972223899998));
#336837=CARTESIAN_POINT('Ctrl Pts',(2.20838308099994,5.2,3.34972223899998));
#336838=CARTESIAN_POINT('Ctrl Pts',(2.20838308099994,2.2,3.34972223899998));
#336839=CARTESIAN_POINT('Ctrl Pts',(2.20861804799994,12.2,3.35016683099998));
#336840=CARTESIAN_POINT('Ctrl Pts',(2.20861804799994,5.2,3.35016683099998));
#336841=CARTESIAN_POINT('Ctrl Pts',(2.20861804799994,2.2,3.35016683099998));
#336842=CARTESIAN_POINT('Ctrl Pts',(2.20885541299995,12.2,3.35061737799998));
#336843=CARTESIAN_POINT('Ctrl Pts',(2.20885541299995,5.2,3.35061737799998));
#336844=CARTESIAN_POINT('Ctrl Pts',(2.20885541299995,2.2,3.35061737799998));
#336845=CARTESIAN_POINT('Ctrl Pts',(2.20909515699994,12.2,3.35107387499999));
#336846=CARTESIAN_POINT('Ctrl Pts',(2.20909515699994,5.2,3.35107387499999));
#336847=CARTESIAN_POINT('Ctrl Pts',(2.20909515699994,2.2,3.35107387499999));
#336848=CARTESIAN_POINT('Ctrl Pts',(2.20933725999994,12.2,3.35153631599999));
#336849=CARTESIAN_POINT('Ctrl Pts',(2.20933725999994,5.2,3.35153631599999));
#336850=CARTESIAN_POINT('Ctrl Pts',(2.20933725999994,2.2,3.35153631599999));
#336851=CARTESIAN_POINT('Ctrl Pts',(2.20958169899994,12.2,3.35200469699998));
#336852=CARTESIAN_POINT('Ctrl Pts',(2.20958169899994,5.2,3.35200469699998));
#336853=CARTESIAN_POINT('Ctrl Pts',(2.20958169899994,2.2,3.35200469699998));
#336854=CARTESIAN_POINT('Ctrl Pts',(2.20982845599994,12.2,3.35247901499999));
#336855=CARTESIAN_POINT('Ctrl Pts',(2.20982845599994,5.2,3.35247901499999));
#336856=CARTESIAN_POINT('Ctrl Pts',(2.20982845599994,2.2,3.35247901499999));
#336857=CARTESIAN_POINT('Ctrl Pts',(2.21007750999994,12.2,3.35295926399999));
#336858=CARTESIAN_POINT('Ctrl Pts',(2.21007750999994,5.2,3.35295926399999));
#336859=CARTESIAN_POINT('Ctrl Pts',(2.21007750999994,2.2,3.35295926399999));
#336860=CARTESIAN_POINT('Ctrl Pts',(2.21032883999994,12.2,3.35344543999998));
#336861=CARTESIAN_POINT('Ctrl Pts',(2.21032883999994,5.2,3.35344543999998));
#336862=CARTESIAN_POINT('Ctrl Pts',(2.21032883999994,2.2,3.35344543999998));
#336863=CARTESIAN_POINT('Ctrl Pts',(2.21058242699994,12.2,3.35393753899999));
#336864=CARTESIAN_POINT('Ctrl Pts',(2.21058242699994,5.2,3.35393753899999));
#336865=CARTESIAN_POINT('Ctrl Pts',(2.21058242699994,2.2,3.35393753899999));
#336866=CARTESIAN_POINT('Ctrl Pts',(2.21083824999994,12.2,3.35443555499998));
#336867=CARTESIAN_POINT('Ctrl Pts',(2.21083824999994,5.2,3.35443555499998));
#336868=CARTESIAN_POINT('Ctrl Pts',(2.21083824999994,2.2,3.35443555499998));
#336869=CARTESIAN_POINT('Ctrl Pts',(2.21109629099994,12.2,3.35493948499998));
#336870=CARTESIAN_POINT('Ctrl Pts',(2.21109629099994,5.2,3.35493948499998));
#336871=CARTESIAN_POINT('Ctrl Pts',(2.21109629099994,2.2,3.35493948499998));
#336872=CARTESIAN_POINT('Ctrl Pts',(2.21135652699994,12.2,3.35544932399999));
#336873=CARTESIAN_POINT('Ctrl Pts',(2.21135652699994,5.2,3.35544932399999));
#336874=CARTESIAN_POINT('Ctrl Pts',(2.21135652699994,2.2,3.35544932399999));
#336875=CARTESIAN_POINT('Ctrl Pts',(2.21161893999994,12.2,3.35596506599998));
#336876=CARTESIAN_POINT('Ctrl Pts',(2.21161893999994,5.2,3.35596506599998));
#336877=CARTESIAN_POINT('Ctrl Pts',(2.21161893999994,2.2,3.35596506599998));
#336878=CARTESIAN_POINT('Ctrl Pts',(2.21188350999994,12.2,3.35648670799999));
#336879=CARTESIAN_POINT('Ctrl Pts',(2.21188350999994,5.2,3.35648670799999));
#336880=CARTESIAN_POINT('Ctrl Pts',(2.21188350999994,2.2,3.35648670799999));
#336881=CARTESIAN_POINT('Ctrl Pts',(2.21215021599994,12.2,3.35701424599999));
#336882=CARTESIAN_POINT('Ctrl Pts',(2.21215021599994,5.2,3.35701424599999));
#336883=CARTESIAN_POINT('Ctrl Pts',(2.21215021599994,2.2,3.35701424599999));
#336884=CARTESIAN_POINT('Ctrl Pts',(2.21241903999994,12.2,3.35754767399998));
#336885=CARTESIAN_POINT('Ctrl Pts',(2.21241903999994,5.2,3.35754767399998));
#336886=CARTESIAN_POINT('Ctrl Pts',(2.21241903999994,2.2,3.35754767399998));
#336887=CARTESIAN_POINT('Ctrl Pts',(2.21268996199994,12.2,3.35808698699999));
#336888=CARTESIAN_POINT('Ctrl Pts',(2.21268996199994,5.2,3.35808698699999));
#336889=CARTESIAN_POINT('Ctrl Pts',(2.21268996199994,2.2,3.35808698699999));
#336890=CARTESIAN_POINT('Ctrl Pts',(2.21296296199994,12.2,3.35863218199999));
#336891=CARTESIAN_POINT('Ctrl Pts',(2.21296296199994,5.2,3.35863218199999));
#336892=CARTESIAN_POINT('Ctrl Pts',(2.21296296199994,2.2,3.35863218199999));
#336893=CARTESIAN_POINT('Ctrl Pts',(2.21323802099994,12.2,3.35918325299998));
#336894=CARTESIAN_POINT('Ctrl Pts',(2.21323802099994,5.2,3.35918325299998));
#336895=CARTESIAN_POINT('Ctrl Pts',(2.21323802099994,2.2,3.35918325299998));
#336896=CARTESIAN_POINT('Ctrl Pts',(2.21351511799994,12.2,3.35974019599998));
#336897=CARTESIAN_POINT('Ctrl Pts',(2.21351511799994,5.2,3.35974019599998));
#336898=CARTESIAN_POINT('Ctrl Pts',(2.21351511799994,2.2,3.35974019599998));
#336899=CARTESIAN_POINT('Ctrl Pts',(2.21379423599994,12.2,3.36030300699999));
#336900=CARTESIAN_POINT('Ctrl Pts',(2.21379423599994,5.2,3.36030300699999));
#336901=CARTESIAN_POINT('Ctrl Pts',(2.21379423599994,2.2,3.36030300699999));
#336902=CARTESIAN_POINT('Ctrl Pts',(2.21407535399994,12.2,3.36087167999998));
#336903=CARTESIAN_POINT('Ctrl Pts',(2.21407535399994,5.2,3.36087167999998));
#336904=CARTESIAN_POINT('Ctrl Pts',(2.21407535399994,2.2,3.36087167999998));
#336905=CARTESIAN_POINT('Ctrl Pts',(2.21435845399994,12.2,3.36144621199999));
#336906=CARTESIAN_POINT('Ctrl Pts',(2.21435845399994,5.2,3.36144621199999));
#336907=CARTESIAN_POINT('Ctrl Pts',(2.21435845399994,2.2,3.36144621199999));
#336908=CARTESIAN_POINT('Ctrl Pts',(2.21464351599994,12.2,3.36202659699998));
#336909=CARTESIAN_POINT('Ctrl Pts',(2.21464351599994,5.2,3.36202659699998));
#336910=CARTESIAN_POINT('Ctrl Pts',(2.21464351599994,2.2,3.36202659699998));
#336911=CARTESIAN_POINT('Ctrl Pts',(2.21493052099994,12.2,3.36261282999998));
#336912=CARTESIAN_POINT('Ctrl Pts',(2.21493052099994,5.2,3.36261282999998));
#336913=CARTESIAN_POINT('Ctrl Pts',(2.21493052099994,2.2,3.36261282999998));
#336914=CARTESIAN_POINT('Ctrl Pts',(2.21521944899994,12.2,3.36320490799999));
#336915=CARTESIAN_POINT('Ctrl Pts',(2.21521944899994,5.2,3.36320490799999));
#336916=CARTESIAN_POINT('Ctrl Pts',(2.21521944899994,2.2,3.36320490799999));
#336917=CARTESIAN_POINT('Ctrl Pts',(2.21551028299994,12.2,3.36380282399999));
#336918=CARTESIAN_POINT('Ctrl Pts',(2.21551028299994,5.2,3.36380282399999));
#336919=CARTESIAN_POINT('Ctrl Pts',(2.21551028299994,2.2,3.36380282399999));
#336920=CARTESIAN_POINT('Ctrl Pts',(2.21580300199994,12.2,3.36440657499999));
#336921=CARTESIAN_POINT('Ctrl Pts',(2.21580300199994,5.2,3.36440657499999));
#336922=CARTESIAN_POINT('Ctrl Pts',(2.21580300199994,2.2,3.36440657499999));
#336923=CARTESIAN_POINT('Ctrl Pts',(2.21609758899994,12.2,3.36501615599998));
#336924=CARTESIAN_POINT('Ctrl Pts',(2.21609758899994,5.2,3.36501615599998));
#336925=CARTESIAN_POINT('Ctrl Pts',(2.21609758899994,2.2,3.36501615599998));
#336926=CARTESIAN_POINT('Ctrl Pts',(2.21639402399994,12.2,3.36563156199999));
#336927=CARTESIAN_POINT('Ctrl Pts',(2.21639402399994,5.2,3.36563156199999));
#336928=CARTESIAN_POINT('Ctrl Pts',(2.21639402399994,2.2,3.36563156199999));
#336929=CARTESIAN_POINT('Ctrl Pts',(2.21669228799994,12.2,3.36625278899999));
#336930=CARTESIAN_POINT('Ctrl Pts',(2.21669228799994,5.2,3.36625278899999));
#336931=CARTESIAN_POINT('Ctrl Pts',(2.21669228799994,2.2,3.36625278899999));
#336932=CARTESIAN_POINT('Ctrl Pts',(2.21699236399994,12.2,3.36687983099999));
#336933=CARTESIAN_POINT('Ctrl Pts',(2.21699236399994,5.2,3.36687983099999));
#336934=CARTESIAN_POINT('Ctrl Pts',(2.21699236399994,2.2,3.36687983099999));
#336935=CARTESIAN_POINT('Ctrl Pts',(2.21729423199994,12.2,3.36751268399999));
#336936=CARTESIAN_POINT('Ctrl Pts',(2.21729423199994,5.2,3.36751268399999));
#336937=CARTESIAN_POINT('Ctrl Pts',(2.21729423199994,2.2,3.36751268399999));
#336938=CARTESIAN_POINT('Ctrl Pts',(2.21759787299994,12.2,3.36815134299999));
#336939=CARTESIAN_POINT('Ctrl Pts',(2.21759787299994,5.2,3.36815134299999));
#336940=CARTESIAN_POINT('Ctrl Pts',(2.21759787299994,2.2,3.36815134299999));
#336941=CARTESIAN_POINT('Ctrl Pts',(2.21790326999994,12.2,3.36879580399999));
#336942=CARTESIAN_POINT('Ctrl Pts',(2.21790326999994,5.2,3.36879580399999));
#336943=CARTESIAN_POINT('Ctrl Pts',(2.21790326999994,2.2,3.36879580399999));
#336944=CARTESIAN_POINT('Ctrl Pts',(2.21821040299994,12.2,3.36944606099999));
#336945=CARTESIAN_POINT('Ctrl Pts',(2.21821040299994,5.2,3.36944606099999));
#336946=CARTESIAN_POINT('Ctrl Pts',(2.21821040299994,2.2,3.36944606099999));
#336947=CARTESIAN_POINT('Ctrl Pts',(2.21851925399994,12.2,3.37010210999999));
#336948=CARTESIAN_POINT('Ctrl Pts',(2.21851925399994,5.2,3.37010210999999));
#336949=CARTESIAN_POINT('Ctrl Pts',(2.21851925399994,2.2,3.37010210999999));
#336950=CARTESIAN_POINT('Ctrl Pts',(2.21882980499994,12.2,3.37076394599999));
#336951=CARTESIAN_POINT('Ctrl Pts',(2.21882980499994,5.2,3.37076394599999));
#336952=CARTESIAN_POINT('Ctrl Pts',(2.21882980499994,2.2,3.37076394599999));
#336953=CARTESIAN_POINT('Ctrl Pts',(2.21914203899995,12.2,3.37143156299998));
#336954=CARTESIAN_POINT('Ctrl Pts',(2.21914203899995,5.2,3.37143156299998));
#336955=CARTESIAN_POINT('Ctrl Pts',(2.21914203899995,2.2,3.37143156299998));
#336956=CARTESIAN_POINT('Ctrl Pts',(2.21945593499994,12.2,3.37210495899999));
#336957=CARTESIAN_POINT('Ctrl Pts',(2.21945593499994,5.2,3.37210495899999));
#336958=CARTESIAN_POINT('Ctrl Pts',(2.21945593499994,2.2,3.37210495899999));
#336959=CARTESIAN_POINT('Ctrl Pts',(2.21977147599994,12.2,3.37278412699998));
#336960=CARTESIAN_POINT('Ctrl Pts',(2.21977147599994,5.2,3.37278412699998));
#336961=CARTESIAN_POINT('Ctrl Pts',(2.21977147599994,2.2,3.37278412699998));
#336962=CARTESIAN_POINT('Ctrl Pts',(2.22008864599994,12.2,3.37346906199999));
#336963=CARTESIAN_POINT('Ctrl Pts',(2.22008864599994,5.2,3.37346906199999));
#336964=CARTESIAN_POINT('Ctrl Pts',(2.22008864599994,2.2,3.37346906199999));
#336965=CARTESIAN_POINT('Ctrl Pts',(2.22040742299995,12.2,3.37415976099999));
#336966=CARTESIAN_POINT('Ctrl Pts',(2.22040742299995,5.2,3.37415976099999));
#336967=CARTESIAN_POINT('Ctrl Pts',(2.22040742299995,2.2,3.37415976099999));
#336968=CARTESIAN_POINT('Ctrl Pts',(2.22072779299994,12.2,3.37485621799999));
#336969=CARTESIAN_POINT('Ctrl Pts',(2.22072779299994,5.2,3.37485621799999));
#336970=CARTESIAN_POINT('Ctrl Pts',(2.22072779299994,2.2,3.37485621799999));
#336971=CARTESIAN_POINT('Ctrl Pts',(2.22104973399994,12.2,3.37555842699999));
#336972=CARTESIAN_POINT('Ctrl Pts',(2.22104973399994,5.2,3.37555842699999));
#336973=CARTESIAN_POINT('Ctrl Pts',(2.22104973399994,2.2,3.37555842699999));
#336974=CARTESIAN_POINT('Ctrl Pts',(2.22137323299994,12.2,3.37626638599998));
#336975=CARTESIAN_POINT('Ctrl Pts',(2.22137323299994,5.2,3.37626638599998));
#336976=CARTESIAN_POINT('Ctrl Pts',(2.22137323299994,2.2,3.37626638599998));
#336977=CARTESIAN_POINT('Ctrl Pts',(2.22169826699994,12.2,3.37698008699999));
#336978=CARTESIAN_POINT('Ctrl Pts',(2.22169826699994,5.2,3.37698008699999));
#336979=CARTESIAN_POINT('Ctrl Pts',(2.22169826699994,2.2,3.37698008699999));
#336980=CARTESIAN_POINT('Ctrl Pts',(2.22202482099994,12.2,3.37769952699999));
#336981=CARTESIAN_POINT('Ctrl Pts',(2.22202482099994,5.2,3.37769952699999));
#336982=CARTESIAN_POINT('Ctrl Pts',(2.22202482099994,2.2,3.37769952699999));
#336983=CARTESIAN_POINT('Ctrl Pts',(2.22235287899994,12.2,3.37842469999998));
#336984=CARTESIAN_POINT('Ctrl Pts',(2.22235287899994,5.2,3.37842469999998));
#336985=CARTESIAN_POINT('Ctrl Pts',(2.22235287899994,2.2,3.37842469999998));
#336986=CARTESIAN_POINT('Ctrl Pts',(2.22268241899994,12.2,3.37915560199999));
#336987=CARTESIAN_POINT('Ctrl Pts',(2.22268241899994,5.2,3.37915560199999));
#336988=CARTESIAN_POINT('Ctrl Pts',(2.22268241899994,2.2,3.37915560199999));
#336989=CARTESIAN_POINT('Ctrl Pts',(2.22301342599994,12.2,3.37989222799998));
#336990=CARTESIAN_POINT('Ctrl Pts',(2.22301342599994,5.2,3.37989222799998));
#336991=CARTESIAN_POINT('Ctrl Pts',(2.22301342599994,2.2,3.37989222799998));
#336992=CARTESIAN_POINT('Ctrl Pts',(2.22334588299994,12.2,3.38063457399999));
#336993=CARTESIAN_POINT('Ctrl Pts',(2.22334588299994,5.2,3.38063457399999));
#336994=CARTESIAN_POINT('Ctrl Pts',(2.22334588299994,2.2,3.38063457399999));
#336995=CARTESIAN_POINT('Ctrl Pts',(2.22367976999994,12.2,3.38138263299999));
#336996=CARTESIAN_POINT('Ctrl Pts',(2.22367976999994,5.2,3.38138263299999));
#336997=CARTESIAN_POINT('Ctrl Pts',(2.22367976999994,2.2,3.38138263299999));
#336998=CARTESIAN_POINT('Ctrl Pts',(2.22401507299994,12.2,3.38213640099998));
#336999=CARTESIAN_POINT('Ctrl Pts',(2.22401507299994,5.2,3.38213640099998));
#337000=CARTESIAN_POINT('Ctrl Pts',(2.22401507299994,2.2,3.38213640099998));
#337001=CARTESIAN_POINT('Ctrl Pts',(2.22435177099995,12.2,3.38289587299998));
#337002=CARTESIAN_POINT('Ctrl Pts',(2.22435177099995,5.2,3.38289587299998));
#337003=CARTESIAN_POINT('Ctrl Pts',(2.22435177099995,2.2,3.38289587299998));
#337004=CARTESIAN_POINT('Ctrl Pts',(2.22468984999994,12.2,3.38366104499999));
#337005=CARTESIAN_POINT('Ctrl Pts',(2.22468984999994,5.2,3.38366104499999));
#337006=CARTESIAN_POINT('Ctrl Pts',(2.22468984999994,2.2,3.38366104499999));
#337007=CARTESIAN_POINT('Ctrl Pts',(2.22502928999994,12.2,3.38443191099999));
#337008=CARTESIAN_POINT('Ctrl Pts',(2.22502928999994,5.2,3.38443191099999));
#337009=CARTESIAN_POINT('Ctrl Pts',(2.22502928999994,2.2,3.38443191099999));
#337010=CARTESIAN_POINT('Ctrl Pts',(2.22537007499994,12.2,3.38520846499998));
#337011=CARTESIAN_POINT('Ctrl Pts',(2.22537007499994,5.2,3.38520846499998));
#337012=CARTESIAN_POINT('Ctrl Pts',(2.22537007499994,2.2,3.38520846499998));
#337013=CARTESIAN_POINT('Ctrl Pts',(2.22571218799994,12.2,3.38599070399999));
#337014=CARTESIAN_POINT('Ctrl Pts',(2.22571218799994,5.2,3.38599070399999));
#337015=CARTESIAN_POINT('Ctrl Pts',(2.22571218799994,2.2,3.38599070399999));
#337016=CARTESIAN_POINT('Ctrl Pts',(2.22605561199994,12.2,3.38677862399998));
#337017=CARTESIAN_POINT('Ctrl Pts',(2.22605561199994,5.2,3.38677862399998));
#337018=CARTESIAN_POINT('Ctrl Pts',(2.22605561199994,2.2,3.38677862399998));
#337019=CARTESIAN_POINT('Ctrl Pts',(2.22640032799994,12.2,3.38757221599998));
#337020=CARTESIAN_POINT('Ctrl Pts',(2.22640032799994,5.2,3.38757221599998));
#337021=CARTESIAN_POINT('Ctrl Pts',(2.22640032799994,2.2,3.38757221599998));
#337022=CARTESIAN_POINT('Ctrl Pts',(2.22674632099995,12.2,3.38837147799998));
#337023=CARTESIAN_POINT('Ctrl Pts',(2.22674632099995,5.2,3.38837147799998));
#337024=CARTESIAN_POINT('Ctrl Pts',(2.22674632099995,2.2,3.38837147799998));
#337025=CARTESIAN_POINT('Ctrl Pts',(2.22709357399994,12.2,3.38917640399998));
#337026=CARTESIAN_POINT('Ctrl Pts',(2.22709357399994,5.2,3.38917640399998));
#337027=CARTESIAN_POINT('Ctrl Pts',(2.22709357399994,2.2,3.38917640399998));
#337028=CARTESIAN_POINT('Ctrl Pts',(2.22744206899994,12.2,3.38998698999998));
#337029=CARTESIAN_POINT('Ctrl Pts',(2.22744206899994,5.2,3.38998698999998));
#337030=CARTESIAN_POINT('Ctrl Pts',(2.22744206899994,2.2,3.38998698999998));
#337031=CARTESIAN_POINT('Ctrl Pts',(2.22779178999994,12.2,3.39080322999998));
#337032=CARTESIAN_POINT('Ctrl Pts',(2.22779178999994,5.2,3.39080322999998));
#337033=CARTESIAN_POINT('Ctrl Pts',(2.22779178999994,2.2,3.39080322999998));
#337034=CARTESIAN_POINT('Ctrl Pts',(2.22814272099995,12.2,3.39162511899998));
#337035=CARTESIAN_POINT('Ctrl Pts',(2.22814272099995,5.2,3.39162511899998));
#337036=CARTESIAN_POINT('Ctrl Pts',(2.22814272099995,2.2,3.39162511899998));
#337037=CARTESIAN_POINT('Ctrl Pts',(2.22849484199994,12.2,3.39245265299999));
#337038=CARTESIAN_POINT('Ctrl Pts',(2.22849484199994,5.2,3.39245265299999));
#337039=CARTESIAN_POINT('Ctrl Pts',(2.22849484199994,2.2,3.39245265299999));
#337040=CARTESIAN_POINT('Ctrl Pts',(2.22884813899995,12.2,3.39328582599999));
#337041=CARTESIAN_POINT('Ctrl Pts',(2.22884813899995,5.2,3.39328582599999));
#337042=CARTESIAN_POINT('Ctrl Pts',(2.22884813899995,2.2,3.39328582599999));
#337043=CARTESIAN_POINT('Ctrl Pts',(2.22920259499995,12.2,3.39412463199999));
#337044=CARTESIAN_POINT('Ctrl Pts',(2.22920259499995,5.2,3.39412463199999));
#337045=CARTESIAN_POINT('Ctrl Pts',(2.22920259499995,2.2,3.39412463199999));
#337046=CARTESIAN_POINT('Ctrl Pts',(2.22955819299994,12.2,3.39496906799998));
#337047=CARTESIAN_POINT('Ctrl Pts',(2.22955819299994,5.2,3.39496906799998));
#337048=CARTESIAN_POINT('Ctrl Pts',(2.22955819299994,2.2,3.39496906799998));
#337049=CARTESIAN_POINT('Ctrl Pts',(2.22991491599994,12.2,3.39581912699998));
#337050=CARTESIAN_POINT('Ctrl Pts',(2.22991491599994,5.2,3.39581912699998));
#337051=CARTESIAN_POINT('Ctrl Pts',(2.22991491599994,2.2,3.39581912699998));
#337052=CARTESIAN_POINT('Ctrl Pts',(2.23027274799994,12.2,3.39667480699998));
#337053=CARTESIAN_POINT('Ctrl Pts',(2.23027274799994,5.2,3.39667480699998));
#337054=CARTESIAN_POINT('Ctrl Pts',(2.23027274799994,2.2,3.39667480699998));
#337055=CARTESIAN_POINT('Ctrl Pts',(2.23063167299994,12.2,3.39753609899999));
#337056=CARTESIAN_POINT('Ctrl Pts',(2.23063167299994,5.2,3.39753609899999));
#337057=CARTESIAN_POINT('Ctrl Pts',(2.23063167299994,2.2,3.39753609899999));
#337058=CARTESIAN_POINT('Ctrl Pts',(2.23099167299994,12.2,3.39840300099999));
#337059=CARTESIAN_POINT('Ctrl Pts',(2.23099167299994,5.2,3.39840300099999));
#337060=CARTESIAN_POINT('Ctrl Pts',(2.23099167299994,2.2,3.39840300099999));
#337061=CARTESIAN_POINT('Ctrl Pts',(2.23135273399994,12.2,3.39927550499999));
#337062=CARTESIAN_POINT('Ctrl Pts',(2.23135273399994,5.2,3.39927550499999));
#337063=CARTESIAN_POINT('Ctrl Pts',(2.23135273399994,2.2,3.39927550499999));
#337064=CARTESIAN_POINT('Ctrl Pts',(2.23171483799994,12.2,3.40015360899999));
#337065=CARTESIAN_POINT('Ctrl Pts',(2.23171483799994,5.2,3.40015360899999));
#337066=CARTESIAN_POINT('Ctrl Pts',(2.23171483799994,2.2,3.40015360899999));
#337067=CARTESIAN_POINT('Ctrl Pts',(2.23207796799994,12.2,3.40103730699998));
#337068=CARTESIAN_POINT('Ctrl Pts',(2.23207796799994,5.2,3.40103730699998));
#337069=CARTESIAN_POINT('Ctrl Pts',(2.23207796799994,2.2,3.40103730699998));
#337070=CARTESIAN_POINT('Ctrl Pts',(2.23244210999994,12.2,3.40192659199998));
#337071=CARTESIAN_POINT('Ctrl Pts',(2.23244210999994,5.2,3.40192659199998));
#337072=CARTESIAN_POINT('Ctrl Pts',(2.23244210999994,2.2,3.40192659199998));
#337073=CARTESIAN_POINT('Ctrl Pts',(2.23280724699995,12.2,3.40282145999999));
#337074=CARTESIAN_POINT('Ctrl Pts',(2.23280724699995,5.2,3.40282145999999));
#337075=CARTESIAN_POINT('Ctrl Pts',(2.23280724699995,2.2,3.40282145999999));
#337076=CARTESIAN_POINT('Ctrl Pts',(2.23317336099994,12.2,3.40372190699998));
#337077=CARTESIAN_POINT('Ctrl Pts',(2.23317336099994,5.2,3.40372190699998));
#337078=CARTESIAN_POINT('Ctrl Pts',(2.23317336099994,2.2,3.40372190699998));
#337079=CARTESIAN_POINT('Ctrl Pts',(2.23354043899994,12.2,3.40462792699999));
#337080=CARTESIAN_POINT('Ctrl Pts',(2.23354043899994,5.2,3.40462792699999));
#337081=CARTESIAN_POINT('Ctrl Pts',(2.23354043899994,2.2,3.40462792699999));
#337082=CARTESIAN_POINT('Ctrl Pts',(2.23390846199994,12.2,3.40553951399999));
#337083=CARTESIAN_POINT('Ctrl Pts',(2.23390846199994,5.2,3.40553951399999));
#337084=CARTESIAN_POINT('Ctrl Pts',(2.23390846199994,2.2,3.40553951399999));
#337085=CARTESIAN_POINT('Ctrl Pts',(2.23427741599994,12.2,3.40645666299999));
#337086=CARTESIAN_POINT('Ctrl Pts',(2.23427741599994,5.2,3.40645666299999));
#337087=CARTESIAN_POINT('Ctrl Pts',(2.23427741599994,2.2,3.40645666299999));
#337088=CARTESIAN_POINT('Ctrl Pts',(2.23464728399994,12.2,3.40737937099998));
#337089=CARTESIAN_POINT('Ctrl Pts',(2.23464728399994,5.2,3.40737937099998));
#337090=CARTESIAN_POINT('Ctrl Pts',(2.23464728399994,2.2,3.40737937099998));
#337091=CARTESIAN_POINT('Ctrl Pts',(2.23501805199994,12.2,3.40830763099999));
#337092=CARTESIAN_POINT('Ctrl Pts',(2.23501805199994,5.2,3.40830763099999));
#337093=CARTESIAN_POINT('Ctrl Pts',(2.23501805199994,2.2,3.40830763099999));
#337094=CARTESIAN_POINT('Ctrl Pts',(2.23538970099994,12.2,3.40924143799998));
#337095=CARTESIAN_POINT('Ctrl Pts',(2.23538970099994,5.2,3.40924143799998));
#337096=CARTESIAN_POINT('Ctrl Pts',(2.23538970099994,2.2,3.40924143799998));
#337097=CARTESIAN_POINT('Ctrl Pts',(2.23576221699994,12.2,3.41018078599999));
#337098=CARTESIAN_POINT('Ctrl Pts',(2.23576221699994,5.2,3.41018078599999));
#337099=CARTESIAN_POINT('Ctrl Pts',(2.23576221699994,2.2,3.41018078599999));
#337100=CARTESIAN_POINT('Ctrl Pts',(2.23613558499994,12.2,3.41112567199998));
#337101=CARTESIAN_POINT('Ctrl Pts',(2.23613558499994,5.2,3.41112567199998));
#337102=CARTESIAN_POINT('Ctrl Pts',(2.23613558499994,2.2,3.41112567199998));
#337103=CARTESIAN_POINT('Ctrl Pts',(2.23650978899994,12.2,3.41207608999999));
#337104=CARTESIAN_POINT('Ctrl Pts',(2.23650978899994,5.2,3.41207608999999));
#337105=CARTESIAN_POINT('Ctrl Pts',(2.23650978899994,2.2,3.41207608999999));
#337106=CARTESIAN_POINT('Ctrl Pts',(2.23688481099994,12.2,3.41303203299999));
#337107=CARTESIAN_POINT('Ctrl Pts',(2.23688481099994,5.2,3.41303203299999));
#337108=CARTESIAN_POINT('Ctrl Pts',(2.23688481099994,2.2,3.41303203299999));
#337109=CARTESIAN_POINT('Ctrl Pts',(2.23726063799994,12.2,3.41399349799998));
#337110=CARTESIAN_POINT('Ctrl Pts',(2.23726063799994,5.2,3.41399349799998));
#337111=CARTESIAN_POINT('Ctrl Pts',(2.23726063799994,2.2,3.41399349799998));
#337112=CARTESIAN_POINT('Ctrl Pts',(2.23763725399994,12.2,3.41496047799998));
#337113=CARTESIAN_POINT('Ctrl Pts',(2.23763725399994,5.2,3.41496047799998));
#337114=CARTESIAN_POINT('Ctrl Pts',(2.23763725399994,2.2,3.41496047799998));
#337115=CARTESIAN_POINT('Ctrl Pts',(2.23801464299994,12.2,3.41593296899998));
#337116=CARTESIAN_POINT('Ctrl Pts',(2.23801464299994,5.2,3.41593296899998));
#337117=CARTESIAN_POINT('Ctrl Pts',(2.23801464299994,2.2,3.41593296899998));
#337118=CARTESIAN_POINT('Ctrl Pts',(2.23839278799994,12.2,3.41691096599998));
#337119=CARTESIAN_POINT('Ctrl Pts',(2.23839278799994,5.2,3.41691096599998));
#337120=CARTESIAN_POINT('Ctrl Pts',(2.23839278799994,2.2,3.41691096599998));
#337121=CARTESIAN_POINT('Ctrl Pts',(2.23877167599994,12.2,3.41789446399999));
#337122=CARTESIAN_POINT('Ctrl Pts',(2.23877167599994,5.2,3.41789446399999));
#337123=CARTESIAN_POINT('Ctrl Pts',(2.23877167599994,2.2,3.41789446399999));
#337124=CARTESIAN_POINT('Ctrl Pts',(2.23915129199994,12.2,3.41888345499999));
#337125=CARTESIAN_POINT('Ctrl Pts',(2.23915129199994,5.2,3.41888345499999));
#337126=CARTESIAN_POINT('Ctrl Pts',(2.23915129199994,2.2,3.41888345499999));
#337127=CARTESIAN_POINT('Ctrl Pts',(2.23953161699994,12.2,3.41987793699998));
#337128=CARTESIAN_POINT('Ctrl Pts',(2.23953161699994,5.2,3.41987793699998));
#337129=CARTESIAN_POINT('Ctrl Pts',(2.23953161699994,2.2,3.41987793699998));
#337130=CARTESIAN_POINT('Ctrl Pts',(2.23991263999994,12.2,3.42087790399999));
#337131=CARTESIAN_POINT('Ctrl Pts',(2.23991263999994,5.2,3.42087790399999));
#337132=CARTESIAN_POINT('Ctrl Pts',(2.23991263999994,2.2,3.42087790399999));
#337133=CARTESIAN_POINT('Ctrl Pts',(2.24029434299994,12.2,3.42188334899999));
#337134=CARTESIAN_POINT('Ctrl Pts',(2.24029434299994,5.2,3.42188334899999));
#337135=CARTESIAN_POINT('Ctrl Pts',(2.24029434299994,2.2,3.42188334899999));
#337136=CARTESIAN_POINT('Ctrl Pts',(2.24067671199994,12.2,3.42289426799999));
#337137=CARTESIAN_POINT('Ctrl Pts',(2.24067671199994,5.2,3.42289426799999));
#337138=CARTESIAN_POINT('Ctrl Pts',(2.24067671199994,2.2,3.42289426799999));
#337139=CARTESIAN_POINT('Ctrl Pts',(2.24105973099994,12.2,3.42391065599998));
#337140=CARTESIAN_POINT('Ctrl Pts',(2.24105973099994,5.2,3.42391065599998));
#337141=CARTESIAN_POINT('Ctrl Pts',(2.24105973099994,2.2,3.42391065599998));
#337142=CARTESIAN_POINT('Ctrl Pts',(2.24144338499995,12.2,3.42493250799999));
#337143=CARTESIAN_POINT('Ctrl Pts',(2.24144338499995,5.2,3.42493250799999));
#337144=CARTESIAN_POINT('Ctrl Pts',(2.24144338499995,2.2,3.42493250799999));
#337145=CARTESIAN_POINT('Ctrl Pts',(2.24182765899994,12.2,3.42595981699999));
#337146=CARTESIAN_POINT('Ctrl Pts',(2.24182765899994,5.2,3.42595981699999));
#337147=CARTESIAN_POINT('Ctrl Pts',(2.24182765899994,2.2,3.42595981699999));
#337148=CARTESIAN_POINT('Ctrl Pts',(2.24221253899994,12.2,3.42699257899999));
#337149=CARTESIAN_POINT('Ctrl Pts',(2.24221253899994,5.2,3.42699257899999));
#337150=CARTESIAN_POINT('Ctrl Pts',(2.24221253899994,2.2,3.42699257899999));
#337151=CARTESIAN_POINT('Ctrl Pts',(2.24259800899994,12.2,3.42803078999999));
#337152=CARTESIAN_POINT('Ctrl Pts',(2.24259800899994,5.2,3.42803078999999));
#337153=CARTESIAN_POINT('Ctrl Pts',(2.24259800899994,2.2,3.42803078999999));
#337154=CARTESIAN_POINT('Ctrl Pts',(2.24298405299994,12.2,3.42907444099998));
#337155=CARTESIAN_POINT('Ctrl Pts',(2.24298405299994,5.2,3.42907444099998));
#337156=CARTESIAN_POINT('Ctrl Pts',(2.24298405299994,2.2,3.42907444099998));
#337157=CARTESIAN_POINT('Ctrl Pts',(2.24337065799994,12.2,3.43012352999998));
#337158=CARTESIAN_POINT('Ctrl Pts',(2.24337065799994,5.2,3.43012352999998));
#337159=CARTESIAN_POINT('Ctrl Pts',(2.24337065799994,2.2,3.43012352999998));
#337160=CARTESIAN_POINT('Ctrl Pts',(2.24375780799994,12.2,3.43117804999999));
#337161=CARTESIAN_POINT('Ctrl Pts',(2.24375780799994,5.2,3.43117804999999));
#337162=CARTESIAN_POINT('Ctrl Pts',(2.24375780799994,2.2,3.43117804999999));
#337163=CARTESIAN_POINT('Ctrl Pts',(2.24414548899994,12.2,3.43223799699999));
#337164=CARTESIAN_POINT('Ctrl Pts',(2.24414548899994,5.2,3.43223799699999));
#337165=CARTESIAN_POINT('Ctrl Pts',(2.24414548899994,2.2,3.43223799699999));
#337166=CARTESIAN_POINT('Ctrl Pts',(2.24453368499994,12.2,3.43330336399998));
#337167=CARTESIAN_POINT('Ctrl Pts',(2.24453368499994,5.2,3.43330336399998));
#337168=CARTESIAN_POINT('Ctrl Pts',(2.24453368499994,2.2,3.43330336399998));
#337169=CARTESIAN_POINT('Ctrl Pts',(2.24492238299994,12.2,3.43437414699999));
#337170=CARTESIAN_POINT('Ctrl Pts',(2.24492238299994,5.2,3.43437414699999));
#337171=CARTESIAN_POINT('Ctrl Pts',(2.24492238299994,2.2,3.43437414699999));
#337172=CARTESIAN_POINT('Ctrl Pts',(2.24531156699994,12.2,3.43545033999998));
#337173=CARTESIAN_POINT('Ctrl Pts',(2.24531156699994,5.2,3.43545033999998));
#337174=CARTESIAN_POINT('Ctrl Pts',(2.24531156699994,2.2,3.43545033999998));
#337175=CARTESIAN_POINT('Ctrl Pts',(2.24570122199994,12.2,3.43653193799998));
#337176=CARTESIAN_POINT('Ctrl Pts',(2.24570122199994,5.2,3.43653193799998));
#337177=CARTESIAN_POINT('Ctrl Pts',(2.24570122199994,2.2,3.43653193799998));
#337178=CARTESIAN_POINT('Ctrl Pts',(2.24609133499994,12.2,3.43761893499998));
#337179=CARTESIAN_POINT('Ctrl Pts',(2.24609133499994,5.2,3.43761893499998));
#337180=CARTESIAN_POINT('Ctrl Pts',(2.24609133499994,2.2,3.43761893499998));
#337181=CARTESIAN_POINT('Ctrl Pts',(2.24648188999994,12.2,3.43871132799999));
#337182=CARTESIAN_POINT('Ctrl Pts',(2.24648188999994,5.2,3.43871132799999));
#337183=CARTESIAN_POINT('Ctrl Pts',(2.24648188999994,2.2,3.43871132799999));
#337184=CARTESIAN_POINT('Ctrl Pts',(2.24687287199994,12.2,3.43980910799999));
#337185=CARTESIAN_POINT('Ctrl Pts',(2.24687287199994,5.2,3.43980910799999));
#337186=CARTESIAN_POINT('Ctrl Pts',(2.24687287199994,2.2,3.43980910799999));
#337187=CARTESIAN_POINT('Ctrl Pts',(2.24726426799994,12.2,3.44091227099998));
#337188=CARTESIAN_POINT('Ctrl Pts',(2.24726426799994,5.2,3.44091227099998));
#337189=CARTESIAN_POINT('Ctrl Pts',(2.24726426799994,2.2,3.44091227099998));
#337190=CARTESIAN_POINT('Ctrl Pts',(2.24765606399994,12.2,3.44202081299999));
#337191=CARTESIAN_POINT('Ctrl Pts',(2.24765606399994,5.2,3.44202081299999));
#337192=CARTESIAN_POINT('Ctrl Pts',(2.24765606399994,2.2,3.44202081299999));
#337193=CARTESIAN_POINT('Ctrl Pts',(2.24804824299994,12.2,3.44313472599998));
#337194=CARTESIAN_POINT('Ctrl Pts',(2.24804824299994,5.2,3.44313472599998));
#337195=CARTESIAN_POINT('Ctrl Pts',(2.24804824299994,2.2,3.44313472599998));
#337196=CARTESIAN_POINT('Ctrl Pts',(2.24844079299995,12.2,3.44425400799998));
#337197=CARTESIAN_POINT('Ctrl Pts',(2.24844079299995,5.2,3.44425400799998));
#337198=CARTESIAN_POINT('Ctrl Pts',(2.24844079299995,2.2,3.44425400799998));
#337199=CARTESIAN_POINT('Ctrl Pts',(2.24883369799994,12.2,3.44537865099999));
#337200=CARTESIAN_POINT('Ctrl Pts',(2.24883369799994,5.2,3.44537865099999));
#337201=CARTESIAN_POINT('Ctrl Pts',(2.24883369799994,2.2,3.44537865099999));
#337202=CARTESIAN_POINT('Ctrl Pts',(2.24922694499994,12.2,3.44650864999998));
#337203=CARTESIAN_POINT('Ctrl Pts',(2.24922694499994,5.2,3.44650864999998));
#337204=CARTESIAN_POINT('Ctrl Pts',(2.24922694499994,2.2,3.44650864999998));
#337205=CARTESIAN_POINT('Ctrl Pts',(2.24962051999994,12.2,3.44764399999999));
#337206=CARTESIAN_POINT('Ctrl Pts',(2.24962051999994,5.2,3.44764399999999));
#337207=CARTESIAN_POINT('Ctrl Pts',(2.24962051999994,2.2,3.44764399999999));
#337208=CARTESIAN_POINT('Ctrl Pts',(2.25001440599994,12.2,3.44878469599998));
#337209=CARTESIAN_POINT('Ctrl Pts',(2.25001440599994,5.2,3.44878469599998));
#337210=CARTESIAN_POINT('Ctrl Pts',(2.25001440599994,2.2,3.44878469599998));
#337211=CARTESIAN_POINT('Ctrl Pts',(2.25040859199995,12.2,3.44993073199999));
#337212=CARTESIAN_POINT('Ctrl Pts',(2.25040859199995,5.2,3.44993073199999));
#337213=CARTESIAN_POINT('Ctrl Pts',(2.25040859199995,2.2,3.44993073199999));
#337214=CARTESIAN_POINT('Ctrl Pts',(2.25080306199994,12.2,3.45108210299998));
#337215=CARTESIAN_POINT('Ctrl Pts',(2.25080306199994,5.2,3.45108210299998));
#337216=CARTESIAN_POINT('Ctrl Pts',(2.25080306199994,2.2,3.45108210299998));
#337217=CARTESIAN_POINT('Ctrl Pts',(2.25119780399994,12.2,3.45223880199999));
#337218=CARTESIAN_POINT('Ctrl Pts',(2.25119780399994,5.2,3.45223880199999));
#337219=CARTESIAN_POINT('Ctrl Pts',(2.25119780399994,2.2,3.45223880199999));
#337220=CARTESIAN_POINT('Ctrl Pts',(2.25159280199994,12.2,3.45340082499998));
#337221=CARTESIAN_POINT('Ctrl Pts',(2.25159280199994,5.2,3.45340082499998));
#337222=CARTESIAN_POINT('Ctrl Pts',(2.25159280199994,2.2,3.45340082499998));
#337223=CARTESIAN_POINT('Ctrl Pts',(2.25198804199994,12.2,3.45456816699999));
#337224=CARTESIAN_POINT('Ctrl Pts',(2.25198804199994,5.2,3.45456816699999));
#337225=CARTESIAN_POINT('Ctrl Pts',(2.25198804199994,2.2,3.45456816699999));
#337226=CARTESIAN_POINT('Ctrl Pts',(2.25238351099994,12.2,3.45574082199998));
#337227=CARTESIAN_POINT('Ctrl Pts',(2.25238351099994,5.2,3.45574082199998));
#337228=CARTESIAN_POINT('Ctrl Pts',(2.25238351099994,2.2,3.45574082199998));
#337229=CARTESIAN_POINT('Ctrl Pts',(2.25277919399994,12.2,3.45691878299998));
#337230=CARTESIAN_POINT('Ctrl Pts',(2.25277919399994,5.2,3.45691878299998));
#337231=CARTESIAN_POINT('Ctrl Pts',(2.25277919399994,2.2,3.45691878299998));
#337232=CARTESIAN_POINT('Ctrl Pts',(2.25317507799994,12.2,3.45810204699998));
#337233=CARTESIAN_POINT('Ctrl Pts',(2.25317507799994,5.2,3.45810204699998));
#337234=CARTESIAN_POINT('Ctrl Pts',(2.25317507799994,2.2,3.45810204699998));
#337235=CARTESIAN_POINT('Ctrl Pts',(2.25357114899994,12.2,3.45929060799998));
#337236=CARTESIAN_POINT('Ctrl Pts',(2.25357114899994,5.2,3.45929060799998));
#337237=CARTESIAN_POINT('Ctrl Pts',(2.25357114899994,2.2,3.45929060799998));
#337238=CARTESIAN_POINT('Ctrl Pts',(2.25396739399994,12.2,3.46048445899999));
#337239=CARTESIAN_POINT('Ctrl Pts',(2.25396739399994,5.2,3.46048445899999));
#337240=CARTESIAN_POINT('Ctrl Pts',(2.25396739399994,2.2,3.46048445899999));
#337241=CARTESIAN_POINT('Ctrl Pts',(2.25436379699994,12.2,3.46168359599999));
#337242=CARTESIAN_POINT('Ctrl Pts',(2.25436379699994,5.2,3.46168359599999));
#337243=CARTESIAN_POINT('Ctrl Pts',(2.25436379699994,2.2,3.46168359599999));
#337244=CARTESIAN_POINT('Ctrl Pts',(2.25476034499994,12.2,3.46288801199999));
#337245=CARTESIAN_POINT('Ctrl Pts',(2.25476034499994,5.2,3.46288801199999));
#337246=CARTESIAN_POINT('Ctrl Pts',(2.25476034499994,2.2,3.46288801199999));
#337247=CARTESIAN_POINT('Ctrl Pts',(2.25515702499994,12.2,3.46409770399998));
#337248=CARTESIAN_POINT('Ctrl Pts',(2.25515702499994,5.2,3.46409770399998));
#337249=CARTESIAN_POINT('Ctrl Pts',(2.25515702499994,2.2,3.46409770399998));
#337250=CARTESIAN_POINT('Ctrl Pts',(2.25555382399994,12.2,3.46531266399998));
#337251=CARTESIAN_POINT('Ctrl Pts',(2.25555382399994,5.2,3.46531266399998));
#337252=CARTESIAN_POINT('Ctrl Pts',(2.25555382399994,2.2,3.46531266399998));
#337253=CARTESIAN_POINT('Ctrl Pts',(2.25595072699994,12.2,3.46653288799998));
#337254=CARTESIAN_POINT('Ctrl Pts',(2.25595072699994,5.2,3.46653288799998));
#337255=CARTESIAN_POINT('Ctrl Pts',(2.25595072699994,2.2,3.46653288799998));
#337256=CARTESIAN_POINT('Ctrl Pts',(2.25634771999994,12.2,3.46775836899998));
#337257=CARTESIAN_POINT('Ctrl Pts',(2.25634771999994,5.2,3.46775836899998));
#337258=CARTESIAN_POINT('Ctrl Pts',(2.25634771999994,2.2,3.46775836899998));
#337259=CARTESIAN_POINT('Ctrl Pts',(2.25674479099994,12.2,3.46898910299998));
#337260=CARTESIAN_POINT('Ctrl Pts',(2.25674479099994,5.2,3.46898910299998));
#337261=CARTESIAN_POINT('Ctrl Pts',(2.25674479099994,2.2,3.46898910299998));
#337262=CARTESIAN_POINT('Ctrl Pts',(2.25714192599995,12.2,3.47022508299998));
#337263=CARTESIAN_POINT('Ctrl Pts',(2.25714192599995,5.2,3.47022508299998));
#337264=CARTESIAN_POINT('Ctrl Pts',(2.25714192599995,2.2,3.47022508299998));
#337265=CARTESIAN_POINT('Ctrl Pts',(2.25753911099994,12.2,3.47146630599998));
#337266=CARTESIAN_POINT('Ctrl Pts',(2.25753911099994,5.2,3.47146630599998));
#337267=CARTESIAN_POINT('Ctrl Pts',(2.25753911099994,2.2,3.47146630599998));
#337268=CARTESIAN_POINT('Ctrl Pts',(2.25793633199994,12.2,3.47271276399999));
#337269=CARTESIAN_POINT('Ctrl Pts',(2.25793633199994,5.2,3.47271276399999));
#337270=CARTESIAN_POINT('Ctrl Pts',(2.25793633199994,2.2,3.47271276399999));
#337271=CARTESIAN_POINT('Ctrl Pts',(2.25833357799994,12.2,3.47396445199998));
#337272=CARTESIAN_POINT('Ctrl Pts',(2.25833357799994,5.2,3.47396445199998));
#337273=CARTESIAN_POINT('Ctrl Pts',(2.25833357799994,2.2,3.47396445199998));
#337274=CARTESIAN_POINT('Ctrl Pts',(2.25873083299994,12.2,3.47522136599999));
#337275=CARTESIAN_POINT('Ctrl Pts',(2.25873083299994,5.2,3.47522136599999));
#337276=CARTESIAN_POINT('Ctrl Pts',(2.25873083299994,2.2,3.47522136599999));
#337277=CARTESIAN_POINT('Ctrl Pts',(2.25912808499994,12.2,3.47648349699998));
#337278=CARTESIAN_POINT('Ctrl Pts',(2.25912808499994,5.2,3.47648349699998));
#337279=CARTESIAN_POINT('Ctrl Pts',(2.25912808499994,2.2,3.47648349699998));
#337280=CARTESIAN_POINT('Ctrl Pts',(2.25952531999994,12.2,3.47775084299998));
#337281=CARTESIAN_POINT('Ctrl Pts',(2.25952531999994,5.2,3.47775084299998));
#337282=CARTESIAN_POINT('Ctrl Pts',(2.25952531999994,2.2,3.47775084299998));
#337283=CARTESIAN_POINT('Ctrl Pts',(2.25992252599994,12.2,3.47902339799998));
#337284=CARTESIAN_POINT('Ctrl Pts',(2.25992252599994,5.2,3.47902339799998));
#337285=CARTESIAN_POINT('Ctrl Pts',(2.25992252599994,2.2,3.47902339799998));
#337286=CARTESIAN_POINT('Ctrl Pts',(2.26031968799994,12.2,3.48030115399999));
#337287=CARTESIAN_POINT('Ctrl Pts',(2.26031968799994,5.2,3.48030115399999));
#337288=CARTESIAN_POINT('Ctrl Pts',(2.26031968799994,2.2,3.48030115399999));
#337289=CARTESIAN_POINT('Ctrl Pts',(2.26071679399994,12.2,3.48158410699998));
#337290=CARTESIAN_POINT('Ctrl Pts',(2.26071679399994,5.2,3.48158410699998));
#337291=CARTESIAN_POINT('Ctrl Pts',(2.26071679399994,2.2,3.48158410699998));
#337292=CARTESIAN_POINT('Ctrl Pts',(2.26111382999994,12.2,3.48287225199999));
#337293=CARTESIAN_POINT('Ctrl Pts',(2.26111382999994,5.2,3.48287225199999));
#337294=CARTESIAN_POINT('Ctrl Pts',(2.26111382999994,2.2,3.48287225199999));
#337295=CARTESIAN_POINT('Ctrl Pts',(2.26151078499994,12.2,3.48416558199999));
#337296=CARTESIAN_POINT('Ctrl Pts',(2.26151078499994,5.2,3.48416558199999));
#337297=CARTESIAN_POINT('Ctrl Pts',(2.26151078499994,2.2,3.48416558199999));
#337298=CARTESIAN_POINT('Ctrl Pts',(2.26190764199994,12.2,3.48546409299999));
#337299=CARTESIAN_POINT('Ctrl Pts',(2.26190764199994,5.2,3.48546409299999));
#337300=CARTESIAN_POINT('Ctrl Pts',(2.26190764199994,2.2,3.48546409299999));
#337301=CARTESIAN_POINT('Ctrl Pts',(2.26230439099994,12.2,3.48676777799999));
#337302=CARTESIAN_POINT('Ctrl Pts',(2.26230439099994,5.2,3.48676777799999));
#337303=CARTESIAN_POINT('Ctrl Pts',(2.26230439099994,2.2,3.48676777799999));
#337304=CARTESIAN_POINT('Ctrl Pts',(2.26270101999994,12.2,3.48807663199998));
#337305=CARTESIAN_POINT('Ctrl Pts',(2.26270101999994,5.2,3.48807663199998));
#337306=CARTESIAN_POINT('Ctrl Pts',(2.26270101999994,2.2,3.48807663199998));
#337307=CARTESIAN_POINT('Ctrl Pts',(2.26309751299994,12.2,3.48939064899999));
#337308=CARTESIAN_POINT('Ctrl Pts',(2.26309751299994,5.2,3.48939064899999));
#337309=CARTESIAN_POINT('Ctrl Pts',(2.26309751299994,2.2,3.48939064899999));
#337310=CARTESIAN_POINT('Ctrl Pts',(2.26349385799994,12.2,3.49070982399999));
#337311=CARTESIAN_POINT('Ctrl Pts',(2.26349385799994,5.2,3.49070982399999));
#337312=CARTESIAN_POINT('Ctrl Pts',(2.26349385799994,2.2,3.49070982399999));
#337313=CARTESIAN_POINT('Ctrl Pts',(2.26389004199994,12.2,3.49203415199998));
#337314=CARTESIAN_POINT('Ctrl Pts',(2.26389004199994,5.2,3.49203415199998));
#337315=CARTESIAN_POINT('Ctrl Pts',(2.26389004199994,2.2,3.49203415199998));
#337316=CARTESIAN_POINT('Ctrl Pts',(2.26428605399994,12.2,3.49336362599999));
#337317=CARTESIAN_POINT('Ctrl Pts',(2.26428605399994,5.2,3.49336362599999));
#337318=CARTESIAN_POINT('Ctrl Pts',(2.26428605399994,2.2,3.49336362599999));
#337319=CARTESIAN_POINT('Ctrl Pts',(2.26468187899994,12.2,3.49469823999998));
#337320=CARTESIAN_POINT('Ctrl Pts',(2.26468187899994,5.2,3.49469823999998));
#337321=CARTESIAN_POINT('Ctrl Pts',(2.26468187899994,2.2,3.49469823999998));
#337322=CARTESIAN_POINT('Ctrl Pts',(2.26507750499994,12.2,3.49603798999999));
#337323=CARTESIAN_POINT('Ctrl Pts',(2.26507750499994,5.2,3.49603798999999));
#337324=CARTESIAN_POINT('Ctrl Pts',(2.26507750499994,2.2,3.49603798999999));
#337325=CARTESIAN_POINT('Ctrl Pts',(2.26547291799994,12.2,3.49738286999998));
#337326=CARTESIAN_POINT('Ctrl Pts',(2.26547291799994,5.2,3.49738286999998));
#337327=CARTESIAN_POINT('Ctrl Pts',(2.26547291799994,2.2,3.49738286999998));
#337328=CARTESIAN_POINT('Ctrl Pts',(2.26586810699994,12.2,3.49873287299998));
#337329=CARTESIAN_POINT('Ctrl Pts',(2.26586810699994,5.2,3.49873287299998));
#337330=CARTESIAN_POINT('Ctrl Pts',(2.26586810699994,2.2,3.49873287299998));
#337331=CARTESIAN_POINT('Ctrl Pts',(2.26626305999994,12.2,3.50008799499999));
#337332=CARTESIAN_POINT('Ctrl Pts',(2.26626305999994,5.2,3.50008799499999));
#337333=CARTESIAN_POINT('Ctrl Pts',(2.26626305999994,2.2,3.50008799499999));
#337334=CARTESIAN_POINT('Ctrl Pts',(2.26665776199994,12.2,3.50144822999999));
#337335=CARTESIAN_POINT('Ctrl Pts',(2.26665776199994,5.2,3.50144822999999));
#337336=CARTESIAN_POINT('Ctrl Pts',(2.26665776199994,2.2,3.50144822999999));
#337337=CARTESIAN_POINT('Ctrl Pts',(2.26705220099995,12.2,3.50281357199999));
#337338=CARTESIAN_POINT('Ctrl Pts',(2.26705220099995,5.2,3.50281357199999));
#337339=CARTESIAN_POINT('Ctrl Pts',(2.26705220099995,2.2,3.50281357199999));
#337340=CARTESIAN_POINT('Ctrl Pts',(2.26744636499994,12.2,3.50418401399998));
#337341=CARTESIAN_POINT('Ctrl Pts',(2.26744636499994,5.2,3.50418401399998));
#337342=CARTESIAN_POINT('Ctrl Pts',(2.26744636499994,2.2,3.50418401399998));
#337343=CARTESIAN_POINT('Ctrl Pts',(2.26784024099994,12.2,3.50555955299999));
#337344=CARTESIAN_POINT('Ctrl Pts',(2.26784024099994,5.2,3.50555955299999));
#337345=CARTESIAN_POINT('Ctrl Pts',(2.26784024099994,2.2,3.50555955299999));
#337346=CARTESIAN_POINT('Ctrl Pts',(2.26823381699994,12.2,3.50694018099999));
#337347=CARTESIAN_POINT('Ctrl Pts',(2.26823381699994,5.2,3.50694018099999));
#337348=CARTESIAN_POINT('Ctrl Pts',(2.26823381699994,2.2,3.50694018099999));
#337349=CARTESIAN_POINT('Ctrl Pts',(2.26862707899994,12.2,3.50832589399998));
#337350=CARTESIAN_POINT('Ctrl Pts',(2.26862707899994,5.2,3.50832589399998));
#337351=CARTESIAN_POINT('Ctrl Pts',(2.26862707899994,2.2,3.50832589399998));
#337352=CARTESIAN_POINT('Ctrl Pts',(2.26902001799994,12.2,3.50971668499999));
#337353=CARTESIAN_POINT('Ctrl Pts',(2.26902001799994,5.2,3.50971668499999));
#337354=CARTESIAN_POINT('Ctrl Pts',(2.26902001799994,2.2,3.50971668499999));
#337355=CARTESIAN_POINT('Ctrl Pts',(2.26941261799994,12.2,3.51111254999999));
#337356=CARTESIAN_POINT('Ctrl Pts',(2.26941261799994,5.2,3.51111254999999));
#337357=CARTESIAN_POINT('Ctrl Pts',(2.26941261799994,2.2,3.51111254999999));
#337358=CARTESIAN_POINT('Ctrl Pts',(2.26980486699994,12.2,3.51251348199998));
#337359=CARTESIAN_POINT('Ctrl Pts',(2.26980486699994,5.2,3.51251348199998));
#337360=CARTESIAN_POINT('Ctrl Pts',(2.26980486699994,2.2,3.51251348199998));
#337361=CARTESIAN_POINT('Ctrl Pts',(2.27019675399994,12.2,3.51391947499998));
#337362=CARTESIAN_POINT('Ctrl Pts',(2.27019675399994,5.2,3.51391947499998));
#337363=CARTESIAN_POINT('Ctrl Pts',(2.27019675399994,2.2,3.51391947499998));
#337364=CARTESIAN_POINT('Ctrl Pts',(2.27058826699994,12.2,3.51533052499998));
#337365=CARTESIAN_POINT('Ctrl Pts',(2.27058826699994,5.2,3.51533052499998));
#337366=CARTESIAN_POINT('Ctrl Pts',(2.27058826699994,2.2,3.51533052499998));
#337367=CARTESIAN_POINT('Ctrl Pts',(2.27097939199994,12.2,3.51674662399999));
#337368=CARTESIAN_POINT('Ctrl Pts',(2.27097939199994,5.2,3.51674662399999));
#337369=CARTESIAN_POINT('Ctrl Pts',(2.27097939199994,2.2,3.51674662399999));
#337370=CARTESIAN_POINT('Ctrl Pts',(2.27137011799994,12.2,3.51816776699999));
#337371=CARTESIAN_POINT('Ctrl Pts',(2.27137011799994,5.2,3.51816776699999));
#337372=CARTESIAN_POINT('Ctrl Pts',(2.27137011799994,2.2,3.51816776699999));
#337373=CARTESIAN_POINT('Ctrl Pts',(2.27176043199994,12.2,3.51959394999999));
#337374=CARTESIAN_POINT('Ctrl Pts',(2.27176043199994,5.2,3.51959394999999));
#337375=CARTESIAN_POINT('Ctrl Pts',(2.27176043199994,2.2,3.51959394999999));
#337376=CARTESIAN_POINT('Ctrl Pts',(2.27215032199994,12.2,3.52102516599999));
#337377=CARTESIAN_POINT('Ctrl Pts',(2.27215032199994,5.2,3.52102516599999));
#337378=CARTESIAN_POINT('Ctrl Pts',(2.27215032199994,2.2,3.52102516599999));
#337379=CARTESIAN_POINT('Ctrl Pts',(2.27253977599994,12.2,3.52246140899998));
#337380=CARTESIAN_POINT('Ctrl Pts',(2.27253977599994,5.2,3.52246140899998));
#337381=CARTESIAN_POINT('Ctrl Pts',(2.27253977599994,2.2,3.52246140899998));
#337382=CARTESIAN_POINT('Ctrl Pts',(2.27292878199994,12.2,3.52390267299998));
#337383=CARTESIAN_POINT('Ctrl Pts',(2.27292878199994,5.2,3.52390267299998));
#337384=CARTESIAN_POINT('Ctrl Pts',(2.27292878199994,2.2,3.52390267299998));
#337385=CARTESIAN_POINT('Ctrl Pts',(2.27331732799994,12.2,3.52534895399998));
#337386=CARTESIAN_POINT('Ctrl Pts',(2.27331732799994,5.2,3.52534895399998));
#337387=CARTESIAN_POINT('Ctrl Pts',(2.27331732799994,2.2,3.52534895399998));
#337388=CARTESIAN_POINT('Ctrl Pts',(2.27370540099994,12.2,3.52680024399999));
#337389=CARTESIAN_POINT('Ctrl Pts',(2.27370540099994,5.2,3.52680024399999));
#337390=CARTESIAN_POINT('Ctrl Pts',(2.27370540099994,2.2,3.52680024399999));
#337391=CARTESIAN_POINT('Ctrl Pts',(2.27409298999994,12.2,3.52825653899998));
#337392=CARTESIAN_POINT('Ctrl Pts',(2.27409298999994,5.2,3.52825653899998));
#337393=CARTESIAN_POINT('Ctrl Pts',(2.27409298999994,2.2,3.52825653899998));
#337394=CARTESIAN_POINT('Ctrl Pts',(2.27448008299994,12.2,3.52971783199998));
#337395=CARTESIAN_POINT('Ctrl Pts',(2.27448008299994,5.2,3.52971783199998));
#337396=CARTESIAN_POINT('Ctrl Pts',(2.27448008299994,2.2,3.52971783199998));
#337397=CARTESIAN_POINT('Ctrl Pts',(2.27486666599995,12.2,3.53118411799999));
#337398=CARTESIAN_POINT('Ctrl Pts',(2.27486666599995,5.2,3.53118411799999));
#337399=CARTESIAN_POINT('Ctrl Pts',(2.27486666599995,2.2,3.53118411799999));
#337400=CARTESIAN_POINT('Ctrl Pts',(2.27525272999994,12.2,3.53265539299999));
#337401=CARTESIAN_POINT('Ctrl Pts',(2.27525272999994,5.2,3.53265539299999));
#337402=CARTESIAN_POINT('Ctrl Pts',(2.27525272999994,2.2,3.53265539299999));
#337403=CARTESIAN_POINT('Ctrl Pts',(2.27563826199995,12.2,3.53413164699998));
#337404=CARTESIAN_POINT('Ctrl Pts',(2.27563826199995,5.2,3.53413164699998));
#337405=CARTESIAN_POINT('Ctrl Pts',(2.27563826199995,2.2,3.53413164699998));
#337406=CARTESIAN_POINT('Ctrl Pts',(2.27602324899994,12.2,3.53561287799998));
#337407=CARTESIAN_POINT('Ctrl Pts',(2.27602324899994,5.2,3.53561287799998));
#337408=CARTESIAN_POINT('Ctrl Pts',(2.27602324899994,2.2,3.53561287799998));
#337409=CARTESIAN_POINT('Ctrl Pts',(2.27640768099994,12.2,3.53709907799999));
#337410=CARTESIAN_POINT('Ctrl Pts',(2.27640768099994,5.2,3.53709907799999));
#337411=CARTESIAN_POINT('Ctrl Pts',(2.27640768099994,2.2,3.53709907799999));
#337412=CARTESIAN_POINT('Ctrl Pts',(2.27679154299994,12.2,3.53859024199998));
#337413=CARTESIAN_POINT('Ctrl Pts',(2.27679154299994,5.2,3.53859024199998));
#337414=CARTESIAN_POINT('Ctrl Pts',(2.27679154299994,2.2,3.53859024199998));
#337415=CARTESIAN_POINT('Ctrl Pts',(2.27717482699994,12.2,3.54008636499999));
#337416=CARTESIAN_POINT('Ctrl Pts',(2.27717482699994,5.2,3.54008636499999));
#337417=CARTESIAN_POINT('Ctrl Pts',(2.27717482699994,2.2,3.54008636499999));
#337418=CARTESIAN_POINT('Ctrl Pts',(2.27755751999994,12.2,3.54158743999999));
#337419=CARTESIAN_POINT('Ctrl Pts',(2.27755751999994,5.2,3.54158743999999));
#337420=CARTESIAN_POINT('Ctrl Pts',(2.27755751999994,2.2,3.54158743999999));
#337421=CARTESIAN_POINT('Ctrl Pts',(2.27793960899994,12.2,3.54309346199998));
#337422=CARTESIAN_POINT('Ctrl Pts',(2.27793960899994,5.2,3.54309346199998));
#337423=CARTESIAN_POINT('Ctrl Pts',(2.27793960899994,2.2,3.54309346199998));
#337424=CARTESIAN_POINT('Ctrl Pts',(2.27832108299994,12.2,3.54460442399999));
#337425=CARTESIAN_POINT('Ctrl Pts',(2.27832108299994,5.2,3.54460442399999));
#337426=CARTESIAN_POINT('Ctrl Pts',(2.27832108299994,2.2,3.54460442399999));
#337427=CARTESIAN_POINT('Ctrl Pts',(2.27870193199994,12.2,3.54612032199999));
#337428=CARTESIAN_POINT('Ctrl Pts',(2.27870193199994,5.2,3.54612032199999));
#337429=CARTESIAN_POINT('Ctrl Pts',(2.27870193199994,2.2,3.54612032199999));
#337430=CARTESIAN_POINT('Ctrl Pts',(2.27908214199994,12.2,3.54764114899999));
#337431=CARTESIAN_POINT('Ctrl Pts',(2.27908214199994,5.2,3.54764114899999));
#337432=CARTESIAN_POINT('Ctrl Pts',(2.27908214199994,2.2,3.54764114899999));
#337433=CARTESIAN_POINT('Ctrl Pts',(2.27946170199994,12.2,3.54916689899999));
#337434=CARTESIAN_POINT('Ctrl Pts',(2.27946170199994,5.2,3.54916689899999));
#337435=CARTESIAN_POINT('Ctrl Pts',(2.27946170199994,2.2,3.54916689899999));
#337436=CARTESIAN_POINT('Ctrl Pts',(2.27984059999994,12.2,3.55069756799999));
#337437=CARTESIAN_POINT('Ctrl Pts',(2.27984059999994,5.2,3.55069756799999));
#337438=CARTESIAN_POINT('Ctrl Pts',(2.27984059999994,2.2,3.55069756799999));
#337439=CARTESIAN_POINT('Ctrl Pts',(2.28021882599994,12.2,3.55223314899998));
#337440=CARTESIAN_POINT('Ctrl Pts',(2.28021882599994,5.2,3.55223314899998));
#337441=CARTESIAN_POINT('Ctrl Pts',(2.28021882599994,2.2,3.55223314899998));
#337442=CARTESIAN_POINT('Ctrl Pts',(2.28059636799994,12.2,3.55377363399998));
#337443=CARTESIAN_POINT('Ctrl Pts',(2.28059636799994,5.2,3.55377363399998));
#337444=CARTESIAN_POINT('Ctrl Pts',(2.28059636799994,2.2,3.55377363399998));
#337445=CARTESIAN_POINT('Ctrl Pts',(2.28097321299995,12.2,3.55531902099998));
#337446=CARTESIAN_POINT('Ctrl Pts',(2.28097321299995,5.2,3.55531902099998));
#337447=CARTESIAN_POINT('Ctrl Pts',(2.28097321299995,2.2,3.55531902099998));
#337448=CARTESIAN_POINT('Ctrl Pts',(2.28134935199995,12.2,3.55686930299999));
#337449=CARTESIAN_POINT('Ctrl Pts',(2.28134935199995,5.2,3.55686930299999));
#337450=CARTESIAN_POINT('Ctrl Pts',(2.28134935199995,2.2,3.55686930299999));
#337451=CARTESIAN_POINT('Ctrl Pts',(2.28172477199994,12.2,3.55842447199999));
#337452=CARTESIAN_POINT('Ctrl Pts',(2.28172477199994,5.2,3.55842447199999));
#337453=CARTESIAN_POINT('Ctrl Pts',(2.28172477199994,2.2,3.55842447199999));
#337454=CARTESIAN_POINT('Ctrl Pts',(2.28209946099994,12.2,3.55998452399999));
#337455=CARTESIAN_POINT('Ctrl Pts',(2.28209946099994,5.2,3.55998452399999));
#337456=CARTESIAN_POINT('Ctrl Pts',(2.28209946099994,2.2,3.55998452399999));
#337457=CARTESIAN_POINT('Ctrl Pts',(2.28247340999994,12.2,3.56154945399999));
#337458=CARTESIAN_POINT('Ctrl Pts',(2.28247340999994,5.2,3.56154945399999));
#337459=CARTESIAN_POINT('Ctrl Pts',(2.28247340999994,2.2,3.56154945399999));
#337460=CARTESIAN_POINT('Ctrl Pts',(2.28284660499994,12.2,3.56311925399999));
#337461=CARTESIAN_POINT('Ctrl Pts',(2.28284660499994,5.2,3.56311925399999));
#337462=CARTESIAN_POINT('Ctrl Pts',(2.28284660499994,2.2,3.56311925399999));
#337463=CARTESIAN_POINT('Ctrl Pts',(2.28321903599995,12.2,3.56469391999998));
#337464=CARTESIAN_POINT('Ctrl Pts',(2.28321903599995,5.2,3.56469391999998));
#337465=CARTESIAN_POINT('Ctrl Pts',(2.28321903599995,2.2,3.56469391999998));
#337466=CARTESIAN_POINT('Ctrl Pts',(2.28359069099994,12.2,3.56627344499999));
#337467=CARTESIAN_POINT('Ctrl Pts',(2.28359069099994,5.2,3.56627344499999));
#337468=CARTESIAN_POINT('Ctrl Pts',(2.28359069099994,2.2,3.56627344499999));
#337469=CARTESIAN_POINT('Ctrl Pts',(2.28396156099994,12.2,3.56785782399999));
#337470=CARTESIAN_POINT('Ctrl Pts',(2.28396156099994,5.2,3.56785782399999));
#337471=CARTESIAN_POINT('Ctrl Pts',(2.28396156099994,2.2,3.56785782399999));
#337472=CARTESIAN_POINT('Ctrl Pts',(2.28433163099994,12.2,3.56944704999999));
#337473=CARTESIAN_POINT('Ctrl Pts',(2.28433163099994,5.2,3.56944704999999));
#337474=CARTESIAN_POINT('Ctrl Pts',(2.28433163099994,2.2,3.56944704999999));
#337475=CARTESIAN_POINT('Ctrl Pts',(2.28470089299994,12.2,3.57104111799998));
#337476=CARTESIAN_POINT('Ctrl Pts',(2.28470089299994,5.2,3.57104111799998));
#337477=CARTESIAN_POINT('Ctrl Pts',(2.28470089299994,2.2,3.57104111799998));
#337478=CARTESIAN_POINT('Ctrl Pts',(2.28506933499994,12.2,3.57264002299999));
#337479=CARTESIAN_POINT('Ctrl Pts',(2.28506933499994,5.2,3.57264002299999));
#337480=CARTESIAN_POINT('Ctrl Pts',(2.28506933499994,2.2,3.57264002299999));
#337481=CARTESIAN_POINT('Ctrl Pts',(2.28543694599994,12.2,3.57424375699999));
#337482=CARTESIAN_POINT('Ctrl Pts',(2.28543694599994,5.2,3.57424375699999));
#337483=CARTESIAN_POINT('Ctrl Pts',(2.28543694599994,2.2,3.57424375699999));
#337484=CARTESIAN_POINT('Ctrl Pts',(2.28580371299994,12.2,3.57585231599998));
#337485=CARTESIAN_POINT('Ctrl Pts',(2.28580371299994,5.2,3.57585231599998));
#337486=CARTESIAN_POINT('Ctrl Pts',(2.28580371299994,2.2,3.57585231599998));
#337487=CARTESIAN_POINT('Ctrl Pts',(2.28616962799994,12.2,3.57746569199998));
#337488=CARTESIAN_POINT('Ctrl Pts',(2.28616962799994,5.2,3.57746569199998));
#337489=CARTESIAN_POINT('Ctrl Pts',(2.28616962799994,2.2,3.57746569199998));
#337490=CARTESIAN_POINT('Ctrl Pts',(2.28653467799994,12.2,3.57908388199998));
#337491=CARTESIAN_POINT('Ctrl Pts',(2.28653467799994,5.2,3.57908388199998));
#337492=CARTESIAN_POINT('Ctrl Pts',(2.28653467799994,2.2,3.57908388199998));
#337493=CARTESIAN_POINT('Ctrl Pts',(2.28689885199994,12.2,3.58070687699998));
#337494=CARTESIAN_POINT('Ctrl Pts',(2.28689885199994,5.2,3.58070687699998));
#337495=CARTESIAN_POINT('Ctrl Pts',(2.28689885199994,2.2,3.58070687699998));
#337496=CARTESIAN_POINT('Ctrl Pts',(2.28726213899995,12.2,3.58233467399998));
#337497=CARTESIAN_POINT('Ctrl Pts',(2.28726213899995,5.2,3.58233467399998));
#337498=CARTESIAN_POINT('Ctrl Pts',(2.28726213899995,2.2,3.58233467399998));
#337499=CARTESIAN_POINT('Ctrl Pts',(2.28762452899994,12.2,3.58396726599998));
#337500=CARTESIAN_POINT('Ctrl Pts',(2.28762452899994,5.2,3.58396726599998));
#337501=CARTESIAN_POINT('Ctrl Pts',(2.28762452899994,2.2,3.58396726599998));
#337502=CARTESIAN_POINT('Ctrl Pts',(2.28798600999994,12.2,3.58560464599999));
#337503=CARTESIAN_POINT('Ctrl Pts',(2.28798600999994,5.2,3.58560464599999));
#337504=CARTESIAN_POINT('Ctrl Pts',(2.28798600999994,2.2,3.58560464599999));
#337505=CARTESIAN_POINT('Ctrl Pts',(2.28834657299994,12.2,3.58724680899999));
#337506=CARTESIAN_POINT('Ctrl Pts',(2.28834657299994,5.2,3.58724680899999));
#337507=CARTESIAN_POINT('Ctrl Pts',(2.28834657299994,2.2,3.58724680899999));
#337508=CARTESIAN_POINT('Ctrl Pts',(2.28870620399994,12.2,3.58889374999999));
#337509=CARTESIAN_POINT('Ctrl Pts',(2.28870620399994,5.2,3.58889374999999));
#337510=CARTESIAN_POINT('Ctrl Pts',(2.28870620399994,2.2,3.58889374999999));
#337511=CARTESIAN_POINT('Ctrl Pts',(2.28906489399994,12.2,3.59054546099999));
#337512=CARTESIAN_POINT('Ctrl Pts',(2.28906489399994,5.2,3.59054546099999));
#337513=CARTESIAN_POINT('Ctrl Pts',(2.28906489399994,2.2,3.59054546099999));
#337514=CARTESIAN_POINT('Ctrl Pts',(2.28942263299994,12.2,3.59220193799998));
#337515=CARTESIAN_POINT('Ctrl Pts',(2.28942263299994,5.2,3.59220193799998));
#337516=CARTESIAN_POINT('Ctrl Pts',(2.28942263299994,2.2,3.59220193799998));
#337517=CARTESIAN_POINT('Ctrl Pts',(2.28977940899994,12.2,3.59386317399998));
#337518=CARTESIAN_POINT('Ctrl Pts',(2.28977940899994,5.2,3.59386317399998));
#337519=CARTESIAN_POINT('Ctrl Pts',(2.28977940899994,2.2,3.59386317399998));
#337520=CARTESIAN_POINT('Ctrl Pts',(2.29013521099994,12.2,3.59552916399998));
#337521=CARTESIAN_POINT('Ctrl Pts',(2.29013521099994,5.2,3.59552916399998));
#337522=CARTESIAN_POINT('Ctrl Pts',(2.29013521099994,2.2,3.59552916399998));
#337523=CARTESIAN_POINT('Ctrl Pts',(2.29049002999994,12.2,3.59719990199999));
#337524=CARTESIAN_POINT('Ctrl Pts',(2.29049002999994,5.2,3.59719990199999));
#337525=CARTESIAN_POINT('Ctrl Pts',(2.29049002999994,2.2,3.59719990199999));
#337526=CARTESIAN_POINT('Ctrl Pts',(2.29084385299994,12.2,3.59887538099999));
#337527=CARTESIAN_POINT('Ctrl Pts',(2.29084385299994,5.2,3.59887538099999));
#337528=CARTESIAN_POINT('Ctrl Pts',(2.29084385299994,2.2,3.59887538099999));
#337529=CARTESIAN_POINT('Ctrl Pts',(2.29119666999994,12.2,3.60055559599999));
#337530=CARTESIAN_POINT('Ctrl Pts',(2.29119666999994,5.2,3.60055559599999));
#337531=CARTESIAN_POINT('Ctrl Pts',(2.29119666999994,2.2,3.60055559599999));
#337532=CARTESIAN_POINT('Ctrl Pts',(2.29154847199994,12.2,3.60224053999998));
#337533=CARTESIAN_POINT('Ctrl Pts',(2.29154847199994,5.2,3.60224053999998));
#337534=CARTESIAN_POINT('Ctrl Pts',(2.29154847199994,2.2,3.60224053999998));
#337535=CARTESIAN_POINT('Ctrl Pts',(2.29189924599994,12.2,3.60393020899998));
#337536=CARTESIAN_POINT('Ctrl Pts',(2.29189924599994,5.2,3.60393020899998));
#337537=CARTESIAN_POINT('Ctrl Pts',(2.29189924599994,2.2,3.60393020899998));
#337538=CARTESIAN_POINT('Ctrl Pts',(2.29224898299994,12.2,3.60562459499998));
#337539=CARTESIAN_POINT('Ctrl Pts',(2.29224898299994,5.2,3.60562459499998));
#337540=CARTESIAN_POINT('Ctrl Pts',(2.29224898299994,2.2,3.60562459499998));
#337541=CARTESIAN_POINT('Ctrl Pts',(2.29259767199994,12.2,3.60732369299999));
#337542=CARTESIAN_POINT('Ctrl Pts',(2.29259767199994,5.2,3.60732369299999));
#337543=CARTESIAN_POINT('Ctrl Pts',(2.29259767199994,2.2,3.60732369299999));
#337544=CARTESIAN_POINT('Ctrl Pts',(2.29294530199994,12.2,3.60902749699999));
#337545=CARTESIAN_POINT('Ctrl Pts',(2.29294530199994,5.2,3.60902749699999));
#337546=CARTESIAN_POINT('Ctrl Pts',(2.29294530199994,2.2,3.60902749699999));
#337547=CARTESIAN_POINT('Ctrl Pts',(2.29329186299994,12.2,3.61073600099999));
#337548=CARTESIAN_POINT('Ctrl Pts',(2.29329186299994,5.2,3.61073600099999));
#337549=CARTESIAN_POINT('Ctrl Pts',(2.29329186299994,2.2,3.61073600099999));
#337550=CARTESIAN_POINT('Ctrl Pts',(2.29363734499994,12.2,3.61244919999999));
#337551=CARTESIAN_POINT('Ctrl Pts',(2.29363734499994,5.2,3.61244919999999));
#337552=CARTESIAN_POINT('Ctrl Pts',(2.29363734499994,2.2,3.61244919999999));
#337553=CARTESIAN_POINT('Ctrl Pts',(2.29398173699995,12.2,3.61416708599998));
#337554=CARTESIAN_POINT('Ctrl Pts',(2.29398173699995,5.2,3.61416708599998));
#337555=CARTESIAN_POINT('Ctrl Pts',(2.29398173699995,2.2,3.61416708599998));
#337556=CARTESIAN_POINT('Ctrl Pts',(2.29432502699995,12.2,3.61588965499998));
#337557=CARTESIAN_POINT('Ctrl Pts',(2.29432502699995,5.2,3.61588965499998));
#337558=CARTESIAN_POINT('Ctrl Pts',(2.29432502699995,2.2,3.61588965499998));
#337559=CARTESIAN_POINT('Ctrl Pts',(2.29466720699994,12.2,3.61761689899998));
#337560=CARTESIAN_POINT('Ctrl Pts',(2.29466720699994,5.2,3.61761689899998));
#337561=CARTESIAN_POINT('Ctrl Pts',(2.29466720699994,2.2,3.61761689899998));
#337562=CARTESIAN_POINT('Ctrl Pts',(2.29500826599994,12.2,3.61934881399999));
#337563=CARTESIAN_POINT('Ctrl Pts',(2.29500826599994,5.2,3.61934881399999));
#337564=CARTESIAN_POINT('Ctrl Pts',(2.29500826599994,2.2,3.61934881399999));
#337565=CARTESIAN_POINT('Ctrl Pts',(2.29534819299994,12.2,3.62108539299999));
#337566=CARTESIAN_POINT('Ctrl Pts',(2.29534819299994,5.2,3.62108539299999));
#337567=CARTESIAN_POINT('Ctrl Pts',(2.29534819299994,2.2,3.62108539299999));
#337568=CARTESIAN_POINT('Ctrl Pts',(2.29568697699994,12.2,3.62282663099998));
#337569=CARTESIAN_POINT('Ctrl Pts',(2.29568697699994,5.2,3.62282663099998));
#337570=CARTESIAN_POINT('Ctrl Pts',(2.29568697699994,2.2,3.62282663099998));
#337571=CARTESIAN_POINT('Ctrl Pts',(2.29602460999994,12.2,3.62457252099999));
#337572=CARTESIAN_POINT('Ctrl Pts',(2.29602460999994,5.2,3.62457252099999));
#337573=CARTESIAN_POINT('Ctrl Pts',(2.29602460999994,2.2,3.62457252099999));
#337574=CARTESIAN_POINT('Ctrl Pts',(2.29636107999994,12.2,3.62632305699999));
#337575=CARTESIAN_POINT('Ctrl Pts',(2.29636107999994,5.2,3.62632305699999));
#337576=CARTESIAN_POINT('Ctrl Pts',(2.29636107999994,2.2,3.62632305699999));
#337577=CARTESIAN_POINT('Ctrl Pts',(2.29669637699994,12.2,3.62807823299998));
#337578=CARTESIAN_POINT('Ctrl Pts',(2.29669637699994,5.2,3.62807823299998));
#337579=CARTESIAN_POINT('Ctrl Pts',(2.29669637699994,2.2,3.62807823299998));
#337580=CARTESIAN_POINT('Ctrl Pts',(2.29703049199994,12.2,3.62983804499999));
#337581=CARTESIAN_POINT('Ctrl Pts',(2.29703049199994,5.2,3.62983804499999));
#337582=CARTESIAN_POINT('Ctrl Pts',(2.29703049199994,2.2,3.62983804499999));
#337583=CARTESIAN_POINT('Ctrl Pts',(2.29736341199994,12.2,3.63160248399998));
#337584=CARTESIAN_POINT('Ctrl Pts',(2.29736341199994,5.2,3.63160248399998));
#337585=CARTESIAN_POINT('Ctrl Pts',(2.29736341199994,2.2,3.63160248399998));
#337586=CARTESIAN_POINT('Ctrl Pts',(2.29769512999995,12.2,3.63337154599999));
#337587=CARTESIAN_POINT('Ctrl Pts',(2.29769512999995,5.2,3.63337154599999));
#337588=CARTESIAN_POINT('Ctrl Pts',(2.29769512999995,2.2,3.63337154599999));
#337589=CARTESIAN_POINT('Ctrl Pts',(2.29802563399994,12.2,3.63514522399999));
#337590=CARTESIAN_POINT('Ctrl Pts',(2.29802563399994,5.2,3.63514522399999));
#337591=CARTESIAN_POINT('Ctrl Pts',(2.29802563399994,2.2,3.63514522399999));
#337592=CARTESIAN_POINT('Ctrl Pts',(2.29835491399994,12.2,3.63692351199998));
#337593=CARTESIAN_POINT('Ctrl Pts',(2.29835491399994,5.2,3.63692351199998));
#337594=CARTESIAN_POINT('Ctrl Pts',(2.29835491399994,2.2,3.63692351199998));
#337595=CARTESIAN_POINT('Ctrl Pts',(2.29868296099994,12.2,3.63870640499999));
#337596=CARTESIAN_POINT('Ctrl Pts',(2.29868296099994,5.2,3.63870640499999));
#337597=CARTESIAN_POINT('Ctrl Pts',(2.29868296099994,2.2,3.63870640499999));
#337598=CARTESIAN_POINT('Ctrl Pts',(2.29900976199994,12.2,3.64049389599998));
#337599=CARTESIAN_POINT('Ctrl Pts',(2.29900976199994,5.2,3.64049389599998));
#337600=CARTESIAN_POINT('Ctrl Pts',(2.29900976199994,2.2,3.64049389599998));
#337601=CARTESIAN_POINT('Ctrl Pts',(2.29933531199995,12.2,3.64228597899999));
#337602=CARTESIAN_POINT('Ctrl Pts',(2.29933531199995,5.2,3.64228597899999));
#337603=CARTESIAN_POINT('Ctrl Pts',(2.29933531199995,2.2,3.64228597899999));
#337604=CARTESIAN_POINT('Ctrl Pts',(2.29965959599994,12.2,3.64408264899998));
#337605=CARTESIAN_POINT('Ctrl Pts',(2.29965959599994,5.2,3.64408264899998));
#337606=CARTESIAN_POINT('Ctrl Pts',(2.29965959599994,2.2,3.64408264899998));
#337607=CARTESIAN_POINT('Ctrl Pts',(2.29998260699994,12.2,3.64588389899998));
#337608=CARTESIAN_POINT('Ctrl Pts',(2.29998260699994,5.2,3.64588389899998));
#337609=CARTESIAN_POINT('Ctrl Pts',(2.29998260699994,2.2,3.64588389899998));
#337610=CARTESIAN_POINT('Ctrl Pts',(2.30030433499994,12.2,3.64768972399999));
#337611=CARTESIAN_POINT('Ctrl Pts',(2.30030433499994,5.2,3.64768972399999));
#337612=CARTESIAN_POINT('Ctrl Pts',(2.30030433499994,2.2,3.64768972399999));
#337613=CARTESIAN_POINT('Ctrl Pts',(2.30062476699994,12.2,3.64950011699998));
#337614=CARTESIAN_POINT('Ctrl Pts',(2.30062476699994,5.2,3.64950011699998));
#337615=CARTESIAN_POINT('Ctrl Pts',(2.30062476699994,2.2,3.64950011699998));
#337616=CARTESIAN_POINT('Ctrl Pts',(2.30094389699994,12.2,3.65131507199998));
#337617=CARTESIAN_POINT('Ctrl Pts',(2.30094389699994,5.2,3.65131507199998));
#337618=CARTESIAN_POINT('Ctrl Pts',(2.30094389699994,2.2,3.65131507199998));
#337619=CARTESIAN_POINT('Ctrl Pts',(2.30126171299994,12.2,3.65313458299998));
#337620=CARTESIAN_POINT('Ctrl Pts',(2.30126171299994,5.2,3.65313458299998));
#337621=CARTESIAN_POINT('Ctrl Pts',(2.30126171299994,2.2,3.65313458299998));
#337622=CARTESIAN_POINT('Ctrl Pts',(2.30157820499994,12.2,3.65495864499999));
#337623=CARTESIAN_POINT('Ctrl Pts',(2.30157820499994,5.2,3.65495864499999));
#337624=CARTESIAN_POINT('Ctrl Pts',(2.30157820499994,2.2,3.65495864499999));
#337625=CARTESIAN_POINT('Ctrl Pts',(2.30189336399994,12.2,3.65678724999999));
#337626=CARTESIAN_POINT('Ctrl Pts',(2.30189336399994,5.2,3.65678724999999));
#337627=CARTESIAN_POINT('Ctrl Pts',(2.30189336399994,2.2,3.65678724999999));
#337628=CARTESIAN_POINT('Ctrl Pts',(2.30220717999994,12.2,3.65862039399998));
#337629=CARTESIAN_POINT('Ctrl Pts',(2.30220717999994,5.2,3.65862039399998));
#337630=CARTESIAN_POINT('Ctrl Pts',(2.30220717999994,2.2,3.65862039399998));
#337631=CARTESIAN_POINT('Ctrl Pts',(2.30251964299994,12.2,3.66045806999999));
#337632=CARTESIAN_POINT('Ctrl Pts',(2.30251964299994,5.2,3.66045806999999));
#337633=CARTESIAN_POINT('Ctrl Pts',(2.30251964299994,2.2,3.66045806999999));
#337634=CARTESIAN_POINT('Ctrl Pts',(2.30283074299994,12.2,3.66230027199999));
#337635=CARTESIAN_POINT('Ctrl Pts',(2.30283074299994,5.2,3.66230027199999));
#337636=CARTESIAN_POINT('Ctrl Pts',(2.30283074299994,2.2,3.66230027199999));
#337637=CARTESIAN_POINT('Ctrl Pts',(2.30314047099994,12.2,3.66414699399999));
#337638=CARTESIAN_POINT('Ctrl Pts',(2.30314047099994,5.2,3.66414699399999));
#337639=CARTESIAN_POINT('Ctrl Pts',(2.30314047099994,2.2,3.66414699399999));
#337640=CARTESIAN_POINT('Ctrl Pts',(2.30344881599994,12.2,3.66599822899998));
#337641=CARTESIAN_POINT('Ctrl Pts',(2.30344881599994,5.2,3.66599822899998));
#337642=CARTESIAN_POINT('Ctrl Pts',(2.30344881599994,2.2,3.66599822899998));
#337643=CARTESIAN_POINT('Ctrl Pts',(2.30375576999994,12.2,3.66785397299999));
#337644=CARTESIAN_POINT('Ctrl Pts',(2.30375576999994,5.2,3.66785397299999));
#337645=CARTESIAN_POINT('Ctrl Pts',(2.30375576999994,2.2,3.66785397299999));
#337646=CARTESIAN_POINT('Ctrl Pts',(2.30406132199994,12.2,3.66971421799998));
#337647=CARTESIAN_POINT('Ctrl Pts',(2.30406132199994,5.2,3.66971421799998));
#337648=CARTESIAN_POINT('Ctrl Pts',(2.30406132199994,2.2,3.66971421799998));
#337649=CARTESIAN_POINT('Ctrl Pts',(2.30436546299994,12.2,3.67157895999998));
#337650=CARTESIAN_POINT('Ctrl Pts',(2.30436546299994,5.2,3.67157895999998));
#337651=CARTESIAN_POINT('Ctrl Pts',(2.30436546299994,2.2,3.67157895999998));
#337652=CARTESIAN_POINT('Ctrl Pts',(2.30466818299994,12.2,3.67344819099999));
#337653=CARTESIAN_POINT('Ctrl Pts',(2.30466818299994,5.2,3.67344819099999));
#337654=CARTESIAN_POINT('Ctrl Pts',(2.30466818299994,2.2,3.67344819099999));
#337655=CARTESIAN_POINT('Ctrl Pts',(2.30496947299994,12.2,3.67532190499999));
#337656=CARTESIAN_POINT('Ctrl Pts',(2.30496947299994,5.2,3.67532190499999));
#337657=CARTESIAN_POINT('Ctrl Pts',(2.30496947299994,2.2,3.67532190499999));
#337658=CARTESIAN_POINT('Ctrl Pts',(2.30526932399994,12.2,3.67720009799999));
#337659=CARTESIAN_POINT('Ctrl Pts',(2.30526932399994,5.2,3.67720009799999));
#337660=CARTESIAN_POINT('Ctrl Pts',(2.30526932399994,2.2,3.67720009799999));
#337661=CARTESIAN_POINT('Ctrl Pts',(2.30556772399995,12.2,3.67908276099998));
#337662=CARTESIAN_POINT('Ctrl Pts',(2.30556772399995,5.2,3.67908276099998));
#337663=CARTESIAN_POINT('Ctrl Pts',(2.30556772399995,2.2,3.67908276099998));
#337664=CARTESIAN_POINT('Ctrl Pts',(2.30586466499994,12.2,3.68096988999999));
#337665=CARTESIAN_POINT('Ctrl Pts',(2.30586466499994,5.2,3.68096988999999));
#337666=CARTESIAN_POINT('Ctrl Pts',(2.30586466499994,2.2,3.68096988999999));
#337667=CARTESIAN_POINT('Ctrl Pts',(2.30616013899994,12.2,3.68286147899998));
#337668=CARTESIAN_POINT('Ctrl Pts',(2.30616013899994,5.2,3.68286147899998));
#337669=CARTESIAN_POINT('Ctrl Pts',(2.30616013899994,2.2,3.68286147899998));
#337670=CARTESIAN_POINT('Ctrl Pts',(2.30645413399994,12.2,3.68475751999998));
#337671=CARTESIAN_POINT('Ctrl Pts',(2.30645413399994,5.2,3.68475751999998));
#337672=CARTESIAN_POINT('Ctrl Pts',(2.30645413399994,2.2,3.68475751999998));
#337673=CARTESIAN_POINT('Ctrl Pts',(2.30674664199995,12.2,3.68665800899999));
#337674=CARTESIAN_POINT('Ctrl Pts',(2.30674664199995,5.2,3.68665800899999));
#337675=CARTESIAN_POINT('Ctrl Pts',(2.30674664199995,2.2,3.68665800899999));
#337676=CARTESIAN_POINT('Ctrl Pts',(2.30703765199994,12.2,3.68856293899999));
#337677=CARTESIAN_POINT('Ctrl Pts',(2.30703765199994,5.2,3.68856293899999));
#337678=CARTESIAN_POINT('Ctrl Pts',(2.30703765199994,2.2,3.68856293899999));
#337679=CARTESIAN_POINT('Ctrl Pts',(2.30732715699994,12.2,3.69047230399998));
#337680=CARTESIAN_POINT('Ctrl Pts',(2.30732715699994,5.2,3.69047230399998));
#337681=CARTESIAN_POINT('Ctrl Pts',(2.30732715699994,2.2,3.69047230399998));
#337682=CARTESIAN_POINT('Ctrl Pts',(2.30761514599994,12.2,3.69238609799999));
#337683=CARTESIAN_POINT('Ctrl Pts',(2.30761514599994,5.2,3.69238609799999));
#337684=CARTESIAN_POINT('Ctrl Pts',(2.30761514599994,2.2,3.69238609799999));
#337685=CARTESIAN_POINT('Ctrl Pts',(2.30790160999994,12.2,3.69430431499998));
#337686=CARTESIAN_POINT('Ctrl Pts',(2.30790160999994,5.2,3.69430431499998));
#337687=CARTESIAN_POINT('Ctrl Pts',(2.30790160999994,2.2,3.69430431499998));
#337688=CARTESIAN_POINT('Ctrl Pts',(2.30818653999994,12.2,3.69622694799999));
#337689=CARTESIAN_POINT('Ctrl Pts',(2.30818653999994,5.2,3.69622694799999));
#337690=CARTESIAN_POINT('Ctrl Pts',(2.30818653999994,2.2,3.69622694799999));
#337691=CARTESIAN_POINT('Ctrl Pts',(2.30846992599994,12.2,3.69815399199998));
#337692=CARTESIAN_POINT('Ctrl Pts',(2.30846992599994,5.2,3.69815399199998));
#337693=CARTESIAN_POINT('Ctrl Pts',(2.30846992599994,2.2,3.69815399199998));
#337694=CARTESIAN_POINT('Ctrl Pts',(2.30875175899994,12.2,3.70008544099999));
#337695=CARTESIAN_POINT('Ctrl Pts',(2.30875175899994,5.2,3.70008544099999));
#337696=CARTESIAN_POINT('Ctrl Pts',(2.30875175899994,2.2,3.70008544099999));
#337697=CARTESIAN_POINT('Ctrl Pts',(2.30903203099994,12.2,3.70202128799999));
#337698=CARTESIAN_POINT('Ctrl Pts',(2.30903203099994,5.2,3.70202128799999));
#337699=CARTESIAN_POINT('Ctrl Pts',(2.30903203099994,2.2,3.70202128799999));
#337700=CARTESIAN_POINT('Ctrl Pts',(2.30931073099994,12.2,3.70396152699998));
#337701=CARTESIAN_POINT('Ctrl Pts',(2.30931073099994,5.2,3.70396152699998));
#337702=CARTESIAN_POINT('Ctrl Pts',(2.30931073099994,2.2,3.70396152699998));
#337703=CARTESIAN_POINT('Ctrl Pts',(2.30958784999994,12.2,3.70590615299999));
#337704=CARTESIAN_POINT('Ctrl Pts',(2.30958784999994,5.2,3.70590615299999));
#337705=CARTESIAN_POINT('Ctrl Pts',(2.30958784999994,2.2,3.70590615299999));
#337706=CARTESIAN_POINT('Ctrl Pts',(2.30986337899994,12.2,3.70785515799999));
#337707=CARTESIAN_POINT('Ctrl Pts',(2.30986337899994,5.2,3.70785515799999));
#337708=CARTESIAN_POINT('Ctrl Pts',(2.30986337899994,2.2,3.70785515799999));
#337709=CARTESIAN_POINT('Ctrl Pts',(2.31013730899994,12.2,3.70980853799999));
#337710=CARTESIAN_POINT('Ctrl Pts',(2.31013730899994,5.2,3.70980853799999));
#337711=CARTESIAN_POINT('Ctrl Pts',(2.31013730899994,2.2,3.70980853799999));
#337712=CARTESIAN_POINT('Ctrl Pts',(2.31040963199994,12.2,3.71176628599999));
#337713=CARTESIAN_POINT('Ctrl Pts',(2.31040963199994,5.2,3.71176628599999));
#337714=CARTESIAN_POINT('Ctrl Pts',(2.31040963199994,2.2,3.71176628599999));
#337715=CARTESIAN_POINT('Ctrl Pts',(2.31068033599994,12.2,3.71372839499998));
#337716=CARTESIAN_POINT('Ctrl Pts',(2.31068033599994,5.2,3.71372839499998));
#337717=CARTESIAN_POINT('Ctrl Pts',(2.31068033599994,2.2,3.71372839499998));
#337718=CARTESIAN_POINT('Ctrl Pts',(2.31094941499994,12.2,3.71569485999999));
#337719=CARTESIAN_POINT('Ctrl Pts',(2.31094941499994,5.2,3.71569485999999));
#337720=CARTESIAN_POINT('Ctrl Pts',(2.31094941499994,2.2,3.71569485999999));
#337721=CARTESIAN_POINT('Ctrl Pts',(2.31121685899994,12.2,3.71766567399998));
#337722=CARTESIAN_POINT('Ctrl Pts',(2.31121685899994,5.2,3.71766567399998));
#337723=CARTESIAN_POINT('Ctrl Pts',(2.31121685899994,2.2,3.71766567399998));
#337724=CARTESIAN_POINT('Ctrl Pts',(2.31148265799995,12.2,3.71964083199998));
#337725=CARTESIAN_POINT('Ctrl Pts',(2.31148265799995,5.2,3.71964083199998));
#337726=CARTESIAN_POINT('Ctrl Pts',(2.31148265799995,2.2,3.71964083199998));
#337727=CARTESIAN_POINT('Ctrl Pts',(2.31174680299994,12.2,3.72162032699999));
#337728=CARTESIAN_POINT('Ctrl Pts',(2.31174680299994,5.2,3.72162032699999));
#337729=CARTESIAN_POINT('Ctrl Pts',(2.31174680299994,2.2,3.72162032699999));
#337730=CARTESIAN_POINT('Ctrl Pts',(2.31200928699994,12.2,3.72360415299998));
#337731=CARTESIAN_POINT('Ctrl Pts',(2.31200928699994,5.2,3.72360415299998));
#337732=CARTESIAN_POINT('Ctrl Pts',(2.31200928699994,2.2,3.72360415299998));
#337733=CARTESIAN_POINT('Ctrl Pts',(2.31227009899994,12.2,3.72559230399998));
#337734=CARTESIAN_POINT('Ctrl Pts',(2.31227009899994,5.2,3.72559230399998));
#337735=CARTESIAN_POINT('Ctrl Pts',(2.31227009899994,2.2,3.72559230399998));
#337736=CARTESIAN_POINT('Ctrl Pts',(2.31252923099994,12.2,3.72758477399999));
#337737=CARTESIAN_POINT('Ctrl Pts',(2.31252923099994,5.2,3.72758477399999));
#337738=CARTESIAN_POINT('Ctrl Pts',(2.31252923099994,2.2,3.72758477399999));
#337739=CARTESIAN_POINT('Ctrl Pts',(2.31278667299994,12.2,3.72958155599999));
#337740=CARTESIAN_POINT('Ctrl Pts',(2.31278667299994,5.2,3.72958155599999));
#337741=CARTESIAN_POINT('Ctrl Pts',(2.31278667299994,2.2,3.72958155599999));
#337742=CARTESIAN_POINT('Ctrl Pts',(2.31304241599994,12.2,3.73158264599999));
#337743=CARTESIAN_POINT('Ctrl Pts',(2.31304241599994,5.2,3.73158264599999));
#337744=CARTESIAN_POINT('Ctrl Pts',(2.31304241599994,2.2,3.73158264599999));
#337745=CARTESIAN_POINT('Ctrl Pts',(2.31329645199994,12.2,3.73358803499999));
#337746=CARTESIAN_POINT('Ctrl Pts',(2.31329645199994,5.2,3.73358803499999));
#337747=CARTESIAN_POINT('Ctrl Pts',(2.31329645199994,2.2,3.73358803499999));
#337748=CARTESIAN_POINT('Ctrl Pts',(2.31354877299994,12.2,3.73559771899998));
#337749=CARTESIAN_POINT('Ctrl Pts',(2.31354877299994,5.2,3.73559771899998));
#337750=CARTESIAN_POINT('Ctrl Pts',(2.31354877299994,2.2,3.73559771899998));
#337751=CARTESIAN_POINT('Ctrl Pts',(2.31379936899994,12.2,3.73761168999999));
#337752=CARTESIAN_POINT('Ctrl Pts',(2.31379936899994,5.2,3.73761168999999));
#337753=CARTESIAN_POINT('Ctrl Pts',(2.31379936899994,2.2,3.73761168999999));
#337754=CARTESIAN_POINT('Ctrl Pts',(2.31404823199994,12.2,3.73962994399999));
#337755=CARTESIAN_POINT('Ctrl Pts',(2.31404823199994,5.2,3.73962994399999));
#337756=CARTESIAN_POINT('Ctrl Pts',(2.31404823199994,2.2,3.73962994399999));
#337757=CARTESIAN_POINT('Ctrl Pts',(2.31429535099994,12.2,3.74165247399999));
#337758=CARTESIAN_POINT('Ctrl Pts',(2.31429535099994,5.2,3.74165247399999));
#337759=CARTESIAN_POINT('Ctrl Pts',(2.31429535099994,2.2,3.74165247399999));
#337760=CARTESIAN_POINT('Ctrl Pts',(2.31454071899994,12.2,3.74367927299998));
#337761=CARTESIAN_POINT('Ctrl Pts',(2.31454071899994,5.2,3.74367927299998));
#337762=CARTESIAN_POINT('Ctrl Pts',(2.31454071899994,2.2,3.74367927299998));
#337763=CARTESIAN_POINT('Ctrl Pts',(2.31478432699994,12.2,3.74571033499999));
#337764=CARTESIAN_POINT('Ctrl Pts',(2.31478432699994,5.2,3.74571033499999));
#337765=CARTESIAN_POINT('Ctrl Pts',(2.31478432699994,2.2,3.74571033499999));
#337766=CARTESIAN_POINT('Ctrl Pts',(2.31502616799994,12.2,3.74774565599999));
#337767=CARTESIAN_POINT('Ctrl Pts',(2.31502616799994,5.2,3.74774565599999));
#337768=CARTESIAN_POINT('Ctrl Pts',(2.31502616799994,2.2,3.74774565599999));
#337769=CARTESIAN_POINT('Ctrl Pts',(2.31526622999994,12.2,3.74978522699998));
#337770=CARTESIAN_POINT('Ctrl Pts',(2.31526622999994,5.2,3.74978522699998));
#337771=CARTESIAN_POINT('Ctrl Pts',(2.31526622999994,2.2,3.74978522699998));
#337772=CARTESIAN_POINT('Ctrl Pts',(2.31550450599994,12.2,3.75182904199999));
#337773=CARTESIAN_POINT('Ctrl Pts',(2.31550450599994,5.2,3.75182904199999));
#337774=CARTESIAN_POINT('Ctrl Pts',(2.31550450599994,2.2,3.75182904199999));
#337775=CARTESIAN_POINT('Ctrl Pts',(2.31574098699994,12.2,3.75387709699999));
#337776=CARTESIAN_POINT('Ctrl Pts',(2.31574098699994,5.2,3.75387709699999));
#337777=CARTESIAN_POINT('Ctrl Pts',(2.31574098699994,2.2,3.75387709699999));
#337778=CARTESIAN_POINT('Ctrl Pts',(2.31597566499994,12.2,3.75592938499998));
#337779=CARTESIAN_POINT('Ctrl Pts',(2.31597566499994,5.2,3.75592938499998));
#337780=CARTESIAN_POINT('Ctrl Pts',(2.31597566499994,2.2,3.75592938499998));
#337781=CARTESIAN_POINT('Ctrl Pts',(2.31620852999994,12.2,3.75798589899999));
#337782=CARTESIAN_POINT('Ctrl Pts',(2.31620852999994,5.2,3.75798589899999));
#337783=CARTESIAN_POINT('Ctrl Pts',(2.31620852999994,2.2,3.75798589899999));
#337784=CARTESIAN_POINT('Ctrl Pts',(2.31643957499994,12.2,3.76004663299998));
#337785=CARTESIAN_POINT('Ctrl Pts',(2.31643957499994,5.2,3.76004663299998));
#337786=CARTESIAN_POINT('Ctrl Pts',(2.31643957499994,2.2,3.76004663299998));
#337787=CARTESIAN_POINT('Ctrl Pts',(2.31666879099994,12.2,3.76211158199999));
#337788=CARTESIAN_POINT('Ctrl Pts',(2.31666879099994,5.2,3.76211158199999));
#337789=CARTESIAN_POINT('Ctrl Pts',(2.31666879099994,2.2,3.76211158199999));
#337790=CARTESIAN_POINT('Ctrl Pts',(2.31689616899994,12.2,3.76418073899998));
#337791=CARTESIAN_POINT('Ctrl Pts',(2.31689616899994,5.2,3.76418073899998));
#337792=CARTESIAN_POINT('Ctrl Pts',(2.31689616899994,2.2,3.76418073899998));
#337793=CARTESIAN_POINT('Ctrl Pts',(2.31712169999994,12.2,3.76625409599999));
#337794=CARTESIAN_POINT('Ctrl Pts',(2.31712169999994,5.2,3.76625409599999));
#337795=CARTESIAN_POINT('Ctrl Pts',(2.31712169999994,2.2,3.76625409599999));
#337796=CARTESIAN_POINT('Ctrl Pts',(2.31734537599994,12.2,3.76833164999999));
#337797=CARTESIAN_POINT('Ctrl Pts',(2.31734537599994,5.2,3.76833164999999));
#337798=CARTESIAN_POINT('Ctrl Pts',(2.31734537599994,2.2,3.76833164999999));
#337799=CARTESIAN_POINT('Ctrl Pts',(2.31756718999994,12.2,3.77041339299999));
#337800=CARTESIAN_POINT('Ctrl Pts',(2.31756718999994,5.2,3.77041339299999));
#337801=CARTESIAN_POINT('Ctrl Pts',(2.31756718999994,2.2,3.77041339299999));
#337802=CARTESIAN_POINT('Ctrl Pts',(2.31778713099994,12.2,3.77249931899998));
#337803=CARTESIAN_POINT('Ctrl Pts',(2.31778713099994,5.2,3.77249931899998));
#337804=CARTESIAN_POINT('Ctrl Pts',(2.31778713099994,2.2,3.77249931899998));
#337805=CARTESIAN_POINT('Ctrl Pts',(2.31800519199994,12.2,3.77458942199999));
#337806=CARTESIAN_POINT('Ctrl Pts',(2.31800519199994,5.2,3.77458942199999));
#337807=CARTESIAN_POINT('Ctrl Pts',(2.31800519199994,2.2,3.77458942199999));
#337808=CARTESIAN_POINT('Ctrl Pts',(2.31822136499995,12.2,3.77668369599998));
#337809=CARTESIAN_POINT('Ctrl Pts',(2.31822136499995,5.2,3.77668369599998));
#337810=CARTESIAN_POINT('Ctrl Pts',(2.31822136499995,2.2,3.77668369599998));
#337811=CARTESIAN_POINT('Ctrl Pts',(2.31843563999994,12.2,3.77878213499999));
#337812=CARTESIAN_POINT('Ctrl Pts',(2.31843563999994,5.2,3.77878213499999));
#337813=CARTESIAN_POINT('Ctrl Pts',(2.31843563999994,2.2,3.77878213499999));
#337814=CARTESIAN_POINT('Ctrl Pts',(2.31864800899995,12.2,3.78088473199998));
#337815=CARTESIAN_POINT('Ctrl Pts',(2.31864800899995,5.2,3.78088473199998));
#337816=CARTESIAN_POINT('Ctrl Pts',(2.31864800899995,2.2,3.78088473199998));
#337817=CARTESIAN_POINT('Ctrl Pts',(2.31885846499994,12.2,3.78299148099998));
#337818=CARTESIAN_POINT('Ctrl Pts',(2.31885846499994,5.2,3.78299148099998));
#337819=CARTESIAN_POINT('Ctrl Pts',(2.31885846499994,2.2,3.78299148099998));
#337820=CARTESIAN_POINT('Ctrl Pts',(2.31906699899994,12.2,3.78510237599999));
#337821=CARTESIAN_POINT('Ctrl Pts',(2.31906699899994,5.2,3.78510237599999));
#337822=CARTESIAN_POINT('Ctrl Pts',(2.31906699899994,2.2,3.78510237599999));
#337823=CARTESIAN_POINT('Ctrl Pts',(2.31927360099994,12.2,3.78721741099999));
#337824=CARTESIAN_POINT('Ctrl Pts',(2.31927360099994,5.2,3.78721741099999));
#337825=CARTESIAN_POINT('Ctrl Pts',(2.31927360099994,2.2,3.78721741099999));
#337826=CARTESIAN_POINT('Ctrl Pts',(2.31947826499994,12.2,3.78933657999998));
#337827=CARTESIAN_POINT('Ctrl Pts',(2.31947826499994,5.2,3.78933657999998));
#337828=CARTESIAN_POINT('Ctrl Pts',(2.31947826499994,2.2,3.78933657999998));
#337829=CARTESIAN_POINT('Ctrl Pts',(2.31968098099994,12.2,3.79145987599999));
#337830=CARTESIAN_POINT('Ctrl Pts',(2.31968098099994,5.2,3.79145987599999));
#337831=CARTESIAN_POINT('Ctrl Pts',(2.31968098099994,2.2,3.79145987599999));
#337832=CARTESIAN_POINT('Ctrl Pts',(2.31988174199994,12.2,3.79358729299998));
#337833=CARTESIAN_POINT('Ctrl Pts',(2.31988174199994,5.2,3.79358729299998));
#337834=CARTESIAN_POINT('Ctrl Pts',(2.31988174199994,2.2,3.79358729299998));
#337835=CARTESIAN_POINT('Ctrl Pts',(2.32008053999994,12.2,3.79571882499998));
#337836=CARTESIAN_POINT('Ctrl Pts',(2.32008053999994,5.2,3.79571882499998));
#337837=CARTESIAN_POINT('Ctrl Pts',(2.32008053999994,2.2,3.79571882499998));
#337838=CARTESIAN_POINT('Ctrl Pts',(2.32027736599994,12.2,3.79785446599998));
#337839=CARTESIAN_POINT('Ctrl Pts',(2.32027736599994,5.2,3.79785446599998));
#337840=CARTESIAN_POINT('Ctrl Pts',(2.32027736599994,2.2,3.79785446599998));
#337841=CARTESIAN_POINT('Ctrl Pts',(2.32047221099994,12.2,3.79999420999999));
#337842=CARTESIAN_POINT('Ctrl Pts',(2.32047221099994,5.2,3.79999420999999));
#337843=CARTESIAN_POINT('Ctrl Pts',(2.32047221099994,2.2,3.79999420999999));
#337844=CARTESIAN_POINT('Ctrl Pts',(2.32066506899994,12.2,3.80213804899999));
#337845=CARTESIAN_POINT('Ctrl Pts',(2.32066506899994,5.2,3.80213804899999));
#337846=CARTESIAN_POINT('Ctrl Pts',(2.32066506899994,2.2,3.80213804899999));
#337847=CARTESIAN_POINT('Ctrl Pts',(2.32085592999994,12.2,3.80428597799998));
#337848=CARTESIAN_POINT('Ctrl Pts',(2.32085592999994,5.2,3.80428597799998));
#337849=CARTESIAN_POINT('Ctrl Pts',(2.32085592999994,2.2,3.80428597799998));
#337850=CARTESIAN_POINT('Ctrl Pts',(2.32104478499994,12.2,3.80643799199999));
#337851=CARTESIAN_POINT('Ctrl Pts',(2.32104478499994,5.2,3.80643799199999));
#337852=CARTESIAN_POINT('Ctrl Pts',(2.32104478499994,2.2,3.80643799199999));
#337853=CARTESIAN_POINT('Ctrl Pts',(2.32123162999994,12.2,3.80859408399999));
#337854=CARTESIAN_POINT('Ctrl Pts',(2.32123162999994,5.2,3.80859408399999));
#337855=CARTESIAN_POINT('Ctrl Pts',(2.32123162999994,2.2,3.80859408399999));
#337856=CARTESIAN_POINT('Ctrl Pts',(2.32141645199994,12.2,3.81075424599998));
#337857=CARTESIAN_POINT('Ctrl Pts',(2.32141645199994,5.2,3.81075424599998));
#337858=CARTESIAN_POINT('Ctrl Pts',(2.32141645199994,2.2,3.81075424599998));
#337859=CARTESIAN_POINT('Ctrl Pts',(2.32159924599994,12.2,3.81291847499998));
#337860=CARTESIAN_POINT('Ctrl Pts',(2.32159924599994,5.2,3.81291847499998));
#337861=CARTESIAN_POINT('Ctrl Pts',(2.32159924599994,2.2,3.81291847499998));
#337862=CARTESIAN_POINT('Ctrl Pts',(2.32178000199994,12.2,3.81508676099998));
#337863=CARTESIAN_POINT('Ctrl Pts',(2.32178000199994,5.2,3.81508676099998));
#337864=CARTESIAN_POINT('Ctrl Pts',(2.32178000199994,2.2,3.81508676099998));
#337865=CARTESIAN_POINT('Ctrl Pts',(2.32195871499994,12.2,3.81725910099998));
#337866=CARTESIAN_POINT('Ctrl Pts',(2.32195871499994,5.2,3.81725910099998));
#337867=CARTESIAN_POINT('Ctrl Pts',(2.32195871499994,2.2,3.81725910099998));
#337868=CARTESIAN_POINT('Ctrl Pts',(2.32213537299994,12.2,3.81943548699999));
#337869=CARTESIAN_POINT('Ctrl Pts',(2.32213537299994,5.2,3.81943548699999));
#337870=CARTESIAN_POINT('Ctrl Pts',(2.32213537299994,2.2,3.81943548699999));
#337871=CARTESIAN_POINT('Ctrl Pts',(2.32230997199994,12.2,3.82161591299998));
#337872=CARTESIAN_POINT('Ctrl Pts',(2.32230997199994,5.2,3.82161591299998));
#337873=CARTESIAN_POINT('Ctrl Pts',(2.32230997199994,2.2,3.82161591299998));
#337874=CARTESIAN_POINT('Ctrl Pts',(2.32248249999994,12.2,3.82380037299999));
#337875=CARTESIAN_POINT('Ctrl Pts',(2.32248249999994,5.2,3.82380037299999));
#337876=CARTESIAN_POINT('Ctrl Pts',(2.32248249999994,2.2,3.82380037299999));
#337877=CARTESIAN_POINT('Ctrl Pts',(2.32265295199995,12.2,3.82598886199998));
#337878=CARTESIAN_POINT('Ctrl Pts',(2.32265295199995,5.2,3.82598886199998));
#337879=CARTESIAN_POINT('Ctrl Pts',(2.32265295199995,2.2,3.82598886199998));
#337880=CARTESIAN_POINT('Ctrl Pts',(2.32282131999995,12.2,3.82818137199998));
#337881=CARTESIAN_POINT('Ctrl Pts',(2.32282131999995,5.2,3.82818137199998));
#337882=CARTESIAN_POINT('Ctrl Pts',(2.32282131999995,2.2,3.82818137199998));
#337883=CARTESIAN_POINT('Ctrl Pts',(2.32298759399994,12.2,3.83037789599998));
#337884=CARTESIAN_POINT('Ctrl Pts',(2.32298759399994,5.2,3.83037789599998));
#337885=CARTESIAN_POINT('Ctrl Pts',(2.32298759399994,2.2,3.83037789599998));
#337886=CARTESIAN_POINT('Ctrl Pts',(2.32315176699994,12.2,3.83257843099998));
#337887=CARTESIAN_POINT('Ctrl Pts',(2.32315176699994,5.2,3.83257843099998));
#337888=CARTESIAN_POINT('Ctrl Pts',(2.32315176699994,2.2,3.83257843099998));
#337889=CARTESIAN_POINT('Ctrl Pts',(2.32331383199994,12.2,3.83478296699998));
#337890=CARTESIAN_POINT('Ctrl Pts',(2.32331383199994,5.2,3.83478296699998));
#337891=CARTESIAN_POINT('Ctrl Pts',(2.32331383199994,2.2,3.83478296699998));
#337892=CARTESIAN_POINT('Ctrl Pts',(2.32347378099994,12.2,3.83699150099999));
#337893=CARTESIAN_POINT('Ctrl Pts',(2.32347378099994,5.2,3.83699150099999));
#337894=CARTESIAN_POINT('Ctrl Pts',(2.32347378099994,2.2,3.83699150099999));
#337895=CARTESIAN_POINT('Ctrl Pts',(2.32363160599994,12.2,3.83920402399998));
#337896=CARTESIAN_POINT('Ctrl Pts',(2.32363160599994,5.2,3.83920402399998));
#337897=CARTESIAN_POINT('Ctrl Pts',(2.32363160599994,2.2,3.83920402399998));
#337898=CARTESIAN_POINT('Ctrl Pts',(2.32378729899994,12.2,3.84142053199999));
#337899=CARTESIAN_POINT('Ctrl Pts',(2.32378729899994,5.2,3.84142053199999));
#337900=CARTESIAN_POINT('Ctrl Pts',(2.32378729899994,2.2,3.84142053199999));
#337901=CARTESIAN_POINT('Ctrl Pts',(2.32394085099994,12.2,3.84364101799999));
#337902=CARTESIAN_POINT('Ctrl Pts',(2.32394085099994,5.2,3.84364101799999));
#337903=CARTESIAN_POINT('Ctrl Pts',(2.32394085099994,2.2,3.84364101799999));
#337904=CARTESIAN_POINT('Ctrl Pts',(2.32409225599994,12.2,3.84586547499998));
#337905=CARTESIAN_POINT('Ctrl Pts',(2.32409225599994,5.2,3.84586547499998));
#337906=CARTESIAN_POINT('Ctrl Pts',(2.32409225599994,2.2,3.84586547499998));
#337907=CARTESIAN_POINT('Ctrl Pts',(2.32424150599994,12.2,3.84809389699999));
#337908=CARTESIAN_POINT('Ctrl Pts',(2.32424150599994,5.2,3.84809389699999));
#337909=CARTESIAN_POINT('Ctrl Pts',(2.32424150599994,2.2,3.84809389699999));
#337910=CARTESIAN_POINT('Ctrl Pts',(2.32438859199994,12.2,3.85032627899999));
#337911=CARTESIAN_POINT('Ctrl Pts',(2.32438859199994,5.2,3.85032627899999));
#337912=CARTESIAN_POINT('Ctrl Pts',(2.32438859199994,2.2,3.85032627899999));
#337913=CARTESIAN_POINT('Ctrl Pts',(2.32453350799994,12.2,3.85256261199999));
#337914=CARTESIAN_POINT('Ctrl Pts',(2.32453350799994,5.2,3.85256261199999));
#337915=CARTESIAN_POINT('Ctrl Pts',(2.32453350799994,2.2,3.85256261199999));
#337916=CARTESIAN_POINT('Ctrl Pts',(2.32467624499994,12.2,3.85480289399998));
#337917=CARTESIAN_POINT('Ctrl Pts',(2.32467624499994,5.2,3.85480289399998));
#337918=CARTESIAN_POINT('Ctrl Pts',(2.32467624499994,2.2,3.85480289399998));
#337919=CARTESIAN_POINT('Ctrl Pts',(2.32481679599994,12.2,3.85704711399999));
#337920=CARTESIAN_POINT('Ctrl Pts',(2.32481679599994,5.2,3.85704711399999));
#337921=CARTESIAN_POINT('Ctrl Pts',(2.32481679599994,2.2,3.85704711399999));
#337922=CARTESIAN_POINT('Ctrl Pts',(2.32495515299994,12.2,3.85929526899999));
#337923=CARTESIAN_POINT('Ctrl Pts',(2.32495515299994,5.2,3.85929526899999));
#337924=CARTESIAN_POINT('Ctrl Pts',(2.32495515299994,2.2,3.85929526899999));
#337925=CARTESIAN_POINT('Ctrl Pts',(2.32509130799994,12.2,3.86154735199998));
#337926=CARTESIAN_POINT('Ctrl Pts',(2.32509130799994,5.2,3.86154735199998));
#337927=CARTESIAN_POINT('Ctrl Pts',(2.32509130799994,2.2,3.86154735199998));
#337928=CARTESIAN_POINT('Ctrl Pts',(2.32522525399994,12.2,3.86380335599998));
#337929=CARTESIAN_POINT('Ctrl Pts',(2.32522525399994,5.2,3.86380335599998));
#337930=CARTESIAN_POINT('Ctrl Pts',(2.32522525399994,2.2,3.86380335599998));
#337931=CARTESIAN_POINT('Ctrl Pts',(2.32535698399994,12.2,3.86606327499998));
#337932=CARTESIAN_POINT('Ctrl Pts',(2.32535698399994,5.2,3.86606327499998));
#337933=CARTESIAN_POINT('Ctrl Pts',(2.32535698399994,2.2,3.86606327499998));
#337934=CARTESIAN_POINT('Ctrl Pts',(2.32548648899995,12.2,3.86832710299998));
#337935=CARTESIAN_POINT('Ctrl Pts',(2.32548648899995,5.2,3.86832710299998));
#337936=CARTESIAN_POINT('Ctrl Pts',(2.32548648899995,2.2,3.86832710299998));
#337937=CARTESIAN_POINT('Ctrl Pts',(2.32561376299994,12.2,3.87059483399998));
#337938=CARTESIAN_POINT('Ctrl Pts',(2.32561376299994,5.2,3.87059483399998));
#337939=CARTESIAN_POINT('Ctrl Pts',(2.32561376299994,2.2,3.87059483399998));
#337940=CARTESIAN_POINT('Ctrl Pts',(2.32573879599994,12.2,3.87286646099999));
#337941=CARTESIAN_POINT('Ctrl Pts',(2.32573879599994,5.2,3.87286646099999));
#337942=CARTESIAN_POINT('Ctrl Pts',(2.32573879599994,2.2,3.87286646099999));
#337943=CARTESIAN_POINT('Ctrl Pts',(2.32586158399994,12.2,3.87514197799998));
#337944=CARTESIAN_POINT('Ctrl Pts',(2.32586158399994,5.2,3.87514197799998));
#337945=CARTESIAN_POINT('Ctrl Pts',(2.32586158399994,2.2,3.87514197799998));
#337946=CARTESIAN_POINT('Ctrl Pts',(2.32598211699994,12.2,3.87742137899998));
#337947=CARTESIAN_POINT('Ctrl Pts',(2.32598211699994,5.2,3.87742137899998));
#337948=CARTESIAN_POINT('Ctrl Pts',(2.32598211699994,2.2,3.87742137899998));
#337949=CARTESIAN_POINT('Ctrl Pts',(2.32610038699994,12.2,3.87970465699999));
#337950=CARTESIAN_POINT('Ctrl Pts',(2.32610038699994,5.2,3.87970465699999));
#337951=CARTESIAN_POINT('Ctrl Pts',(2.32610038699994,2.2,3.87970465699999));
#337952=CARTESIAN_POINT('Ctrl Pts',(2.32621638899994,12.2,3.88199180699999));
#337953=CARTESIAN_POINT('Ctrl Pts',(2.32621638899994,5.2,3.88199180699999));
#337954=CARTESIAN_POINT('Ctrl Pts',(2.32621638899994,2.2,3.88199180699999));
#337955=CARTESIAN_POINT('Ctrl Pts',(2.32633011299994,12.2,3.88428282199998));
#337956=CARTESIAN_POINT('Ctrl Pts',(2.32633011299994,5.2,3.88428282199998));
#337957=CARTESIAN_POINT('Ctrl Pts',(2.32633011299994,2.2,3.88428282199998));
#337958=CARTESIAN_POINT('Ctrl Pts',(2.32644155199994,12.2,3.88657769599998));
#337959=CARTESIAN_POINT('Ctrl Pts',(2.32644155199994,5.2,3.88657769599998));
#337960=CARTESIAN_POINT('Ctrl Pts',(2.32644155199994,2.2,3.88657769599998));
#337961=CARTESIAN_POINT('Ctrl Pts',(2.32655070199994,12.2,3.88887642099998));
#337962=CARTESIAN_POINT('Ctrl Pts',(2.32655070199994,5.2,3.88887642099998));
#337963=CARTESIAN_POINT('Ctrl Pts',(2.32655070199994,2.2,3.88887642099998));
#337964=CARTESIAN_POINT('Ctrl Pts',(2.32665754999994,12.2,3.89117899199999));
#337965=CARTESIAN_POINT('Ctrl Pts',(2.32665754999994,5.2,3.89117899199999));
#337966=CARTESIAN_POINT('Ctrl Pts',(2.32665754999994,2.2,3.89117899199999));
#337967=CARTESIAN_POINT('Ctrl Pts',(2.32676209299994,12.2,3.89348540499999));
#337968=CARTESIAN_POINT('Ctrl Pts',(2.32676209299994,5.2,3.89348540499999));
#337969=CARTESIAN_POINT('Ctrl Pts',(2.32676209299994,2.2,3.89348540499999));
#337970=CARTESIAN_POINT('Ctrl Pts',(2.32686432199994,12.2,3.89579564899999));
#337971=CARTESIAN_POINT('Ctrl Pts',(2.32686432199994,5.2,3.89579564899999));
#337972=CARTESIAN_POINT('Ctrl Pts',(2.32686432199994,2.2,3.89579564899999));
#337973=CARTESIAN_POINT('Ctrl Pts',(2.32696422899994,12.2,3.89810972199999));
#337974=CARTESIAN_POINT('Ctrl Pts',(2.32696422899994,5.2,3.89810972199999));
#337975=CARTESIAN_POINT('Ctrl Pts',(2.32696422899994,2.2,3.89810972199999));
#337976=CARTESIAN_POINT('Ctrl Pts',(2.32706180899994,12.2,3.90042761499998));
#337977=CARTESIAN_POINT('Ctrl Pts',(2.32706180899994,5.2,3.90042761499998));
#337978=CARTESIAN_POINT('Ctrl Pts',(2.32706180899994,2.2,3.90042761499998));
#337979=CARTESIAN_POINT('Ctrl Pts',(2.32715705299994,12.2,3.90274932299998));
#337980=CARTESIAN_POINT('Ctrl Pts',(2.32715705299994,5.2,3.90274932299998));
#337981=CARTESIAN_POINT('Ctrl Pts',(2.32715705299994,2.2,3.90274932299998));
#337982=CARTESIAN_POINT('Ctrl Pts',(2.32724995299994,12.2,3.90507483899999));
#337983=CARTESIAN_POINT('Ctrl Pts',(2.32724995299994,5.2,3.90507483899999));
#337984=CARTESIAN_POINT('Ctrl Pts',(2.32724995299994,2.2,3.90507483899999));
#337985=CARTESIAN_POINT('Ctrl Pts',(2.32734050299995,12.2,3.90740415699998));
#337986=CARTESIAN_POINT('Ctrl Pts',(2.32734050299995,5.2,3.90740415699998));
#337987=CARTESIAN_POINT('Ctrl Pts',(2.32734050299995,2.2,3.90740415699998));
#337988=CARTESIAN_POINT('Ctrl Pts',(2.32742869599994,12.2,3.90973727099999));
#337989=CARTESIAN_POINT('Ctrl Pts',(2.32742869599994,5.2,3.90973727099999));
#337990=CARTESIAN_POINT('Ctrl Pts',(2.32742869599994,2.2,3.90973727099999));
#337991=CARTESIAN_POINT('Ctrl Pts',(2.32751452399994,12.2,3.91207417399999));
#337992=CARTESIAN_POINT('Ctrl Pts',(2.32751452399994,5.2,3.91207417399999));
#337993=CARTESIAN_POINT('Ctrl Pts',(2.32751452399994,2.2,3.91207417399999));
#337994=CARTESIAN_POINT('Ctrl Pts',(2.32759797899994,12.2,3.91441486099998));
#337995=CARTESIAN_POINT('Ctrl Pts',(2.32759797899994,5.2,3.91441486099998));
#337996=CARTESIAN_POINT('Ctrl Pts',(2.32759797899994,2.2,3.91441486099998));
#337997=CARTESIAN_POINT('Ctrl Pts',(2.32767905599994,12.2,3.91675932499999));
#337998=CARTESIAN_POINT('Ctrl Pts',(2.32767905599994,5.2,3.91675932499999));
#337999=CARTESIAN_POINT('Ctrl Pts',(2.32767905599994,2.2,3.91675932499999));
#338000=CARTESIAN_POINT('Ctrl Pts',(2.32775774599994,12.2,3.91910755799999));
#338001=CARTESIAN_POINT('Ctrl Pts',(2.32775774599994,5.2,3.91910755799999));
#338002=CARTESIAN_POINT('Ctrl Pts',(2.32775774599994,2.2,3.91910755799999));
#338003=CARTESIAN_POINT('Ctrl Pts',(2.32783404299994,12.2,3.92145955599998));
#338004=CARTESIAN_POINT('Ctrl Pts',(2.32783404299994,5.2,3.92145955599998));
#338005=CARTESIAN_POINT('Ctrl Pts',(2.32783404299994,2.2,3.92145955599998));
#338006=CARTESIAN_POINT('Ctrl Pts',(2.32790793899994,12.2,3.92381531299999));
#338007=CARTESIAN_POINT('Ctrl Pts',(2.32790793899994,5.2,3.92381531299999));
#338008=CARTESIAN_POINT('Ctrl Pts',(2.32790793899994,2.2,3.92381531299999));
#338009=CARTESIAN_POINT('Ctrl Pts',(2.32797942799994,12.2,3.92617481999999));
#338010=CARTESIAN_POINT('Ctrl Pts',(2.32797942799994,5.2,3.92617481999999));
#338011=CARTESIAN_POINT('Ctrl Pts',(2.32797942799994,2.2,3.92617481999999));
#338012=CARTESIAN_POINT('Ctrl Pts',(2.32804850099994,12.2,3.92853807299999));
#338013=CARTESIAN_POINT('Ctrl Pts',(2.32804850099994,5.2,3.92853807299999));
#338014=CARTESIAN_POINT('Ctrl Pts',(2.32804850099994,2.2,3.92853807299999));
#338015=CARTESIAN_POINT('Ctrl Pts',(2.32811515299994,12.2,3.93090506499998));
#338016=CARTESIAN_POINT('Ctrl Pts',(2.32811515299994,5.2,3.93090506499998));
#338017=CARTESIAN_POINT('Ctrl Pts',(2.32811515299994,2.2,3.93090506499998));
#338018=CARTESIAN_POINT('Ctrl Pts',(2.32817937599994,12.2,3.93327578999998));
#338019=CARTESIAN_POINT('Ctrl Pts',(2.32817937599994,5.2,3.93327578999998));
#338020=CARTESIAN_POINT('Ctrl Pts',(2.32817937599994,2.2,3.93327578999998));
#338021=CARTESIAN_POINT('Ctrl Pts',(2.32824116199994,12.2,3.93565023999999));
#338022=CARTESIAN_POINT('Ctrl Pts',(2.32824116199994,5.2,3.93565023999999));
#338023=CARTESIAN_POINT('Ctrl Pts',(2.32824116199994,2.2,3.93565023999999));
#338024=CARTESIAN_POINT('Ctrl Pts',(2.32830050599994,12.2,3.93802841199999));
#338025=CARTESIAN_POINT('Ctrl Pts',(2.32830050599994,5.2,3.93802841199999));
#338026=CARTESIAN_POINT('Ctrl Pts',(2.32830050599994,2.2,3.93802841199999));
#338027=CARTESIAN_POINT('Ctrl Pts',(2.32835739899994,12.2,3.94041029599999));
#338028=CARTESIAN_POINT('Ctrl Pts',(2.32835739899994,5.2,3.94041029599999));
#338029=CARTESIAN_POINT('Ctrl Pts',(2.32835739899994,2.2,3.94041029599999));
#338030=CARTESIAN_POINT('Ctrl Pts',(2.32841183599994,12.2,3.94279588799999));
#338031=CARTESIAN_POINT('Ctrl Pts',(2.32841183599994,5.2,3.94279588799999));
#338032=CARTESIAN_POINT('Ctrl Pts',(2.32841183599994,2.2,3.94279588799999));
#338033=CARTESIAN_POINT('Ctrl Pts',(2.32846380899994,12.2,3.94518518199998));
#338034=CARTESIAN_POINT('Ctrl Pts',(2.32846380899994,5.2,3.94518518199998));
#338035=CARTESIAN_POINT('Ctrl Pts',(2.32846380899994,2.2,3.94518518199998));
#338036=CARTESIAN_POINT('Ctrl Pts',(2.32851330999994,12.2,3.94757816999999));
#338037=CARTESIAN_POINT('Ctrl Pts',(2.32851330999994,5.2,3.94757816999999));
#338038=CARTESIAN_POINT('Ctrl Pts',(2.32851330999994,2.2,3.94757816999999));
#338039=CARTESIAN_POINT('Ctrl Pts',(2.32856033299994,12.2,3.94997484599998));
#338040=CARTESIAN_POINT('Ctrl Pts',(2.32856033299994,5.2,3.94997484599998));
#338041=CARTESIAN_POINT('Ctrl Pts',(2.32856033299994,2.2,3.94997484599998));
#338042=CARTESIAN_POINT('Ctrl Pts',(2.32860487199994,12.2,3.95237520499998));
#338043=CARTESIAN_POINT('Ctrl Pts',(2.32860487199994,5.2,3.95237520499998));
#338044=CARTESIAN_POINT('Ctrl Pts',(2.32860487199994,2.2,3.95237520499998));
#338045=CARTESIAN_POINT('Ctrl Pts',(2.32864691899994,12.2,3.95477923899998));
#338046=CARTESIAN_POINT('Ctrl Pts',(2.32864691899994,5.2,3.95477923899998));
#338047=CARTESIAN_POINT('Ctrl Pts',(2.32864691899994,2.2,3.95477923899998));
#338048=CARTESIAN_POINT('Ctrl Pts',(2.32868646699994,12.2,3.95718694299998));
#338049=CARTESIAN_POINT('Ctrl Pts',(2.32868646699994,5.2,3.95718694299998));
#338050=CARTESIAN_POINT('Ctrl Pts',(2.32868646699994,2.2,3.95718694299998));
#338051=CARTESIAN_POINT('Ctrl Pts',(2.32872350999994,12.2,3.95959830999999));
#338052=CARTESIAN_POINT('Ctrl Pts',(2.32872350999994,5.2,3.95959830999999));
#338053=CARTESIAN_POINT('Ctrl Pts',(2.32872350999994,2.2,3.95959830999999));
#338054=CARTESIAN_POINT('Ctrl Pts',(2.32875804099994,12.2,3.96201333399999));
#338055=CARTESIAN_POINT('Ctrl Pts',(2.32875804099994,5.2,3.96201333399999));
#338056=CARTESIAN_POINT('Ctrl Pts',(2.32875804099994,2.2,3.96201333399999));
#338057=CARTESIAN_POINT('Ctrl Pts',(2.32879005199994,12.2,3.96443200799999));
#338058=CARTESIAN_POINT('Ctrl Pts',(2.32879005199994,5.2,3.96443200799999));
#338059=CARTESIAN_POINT('Ctrl Pts',(2.32879005199994,2.2,3.96443200799999));
#338060=CARTESIAN_POINT('Ctrl Pts',(2.32881953799994,12.2,3.96685432699999));
#338061=CARTESIAN_POINT('Ctrl Pts',(2.32881953799994,5.2,3.96685432699999));
#338062=CARTESIAN_POINT('Ctrl Pts',(2.32881953799994,2.2,3.96685432699999));
#338063=CARTESIAN_POINT('Ctrl Pts',(2.32884649099994,12.2,3.96928028299998));
#338064=CARTESIAN_POINT('Ctrl Pts',(2.32884649099994,5.2,3.96928028299998));
#338065=CARTESIAN_POINT('Ctrl Pts',(2.32884649099994,2.2,3.96928028299998));
#338066=CARTESIAN_POINT('Ctrl Pts',(2.32887090299994,12.2,3.97170987099998));
#338067=CARTESIAN_POINT('Ctrl Pts',(2.32887090299994,5.2,3.97170987099998));
#338068=CARTESIAN_POINT('Ctrl Pts',(2.32887090299994,2.2,3.97170987099998));
#338069=CARTESIAN_POINT('Ctrl Pts',(2.32889277099994,12.2,3.97414308499999));
#338070=CARTESIAN_POINT('Ctrl Pts',(2.32889277099994,5.2,3.97414308499999));
#338071=CARTESIAN_POINT('Ctrl Pts',(2.32889277099994,2.2,3.97414308499999));
#338072=CARTESIAN_POINT('Ctrl Pts',(2.32891208399994,12.2,3.97657991599999));
#338073=CARTESIAN_POINT('Ctrl Pts',(2.32891208399994,5.2,3.97657991599999));
#338074=CARTESIAN_POINT('Ctrl Pts',(2.32891208399994,2.2,3.97657991599999));
#338075=CARTESIAN_POINT('Ctrl Pts',(2.32892883899994,12.2,3.97902035999999));
#338076=CARTESIAN_POINT('Ctrl Pts',(2.32892883899994,5.2,3.97902035999999));
#338077=CARTESIAN_POINT('Ctrl Pts',(2.32892883899994,2.2,3.97902035999999));
#338078=CARTESIAN_POINT('Ctrl Pts',(2.32894302699994,12.2,3.98146441099998));
#338079=CARTESIAN_POINT('Ctrl Pts',(2.32894302699994,5.2,3.98146441099998));
#338080=CARTESIAN_POINT('Ctrl Pts',(2.32894302699994,2.2,3.98146441099998));
#338081=CARTESIAN_POINT('Ctrl Pts',(2.32895464099994,12.2,3.98391206199998));
#338082=CARTESIAN_POINT('Ctrl Pts',(2.32895464099994,5.2,3.98391206199998));
#338083=CARTESIAN_POINT('Ctrl Pts',(2.32895464099994,2.2,3.98391206199998));
#338084=CARTESIAN_POINT('Ctrl Pts',(2.32896367499994,12.2,3.98636330599999));
#338085=CARTESIAN_POINT('Ctrl Pts',(2.32896367499994,5.2,3.98636330599999));
#338086=CARTESIAN_POINT('Ctrl Pts',(2.32896367499994,2.2,3.98636330599999));
#338087=CARTESIAN_POINT('Ctrl Pts',(2.32897012299994,12.2,3.98881813699998));
#338088=CARTESIAN_POINT('Ctrl Pts',(2.32897012299994,5.2,3.98881813699998));
#338089=CARTESIAN_POINT('Ctrl Pts',(2.32897012299994,2.2,3.98881813699998));
#338090=CARTESIAN_POINT('Ctrl Pts',(2.32897397899994,12.2,3.99127654899999));
#338091=CARTESIAN_POINT('Ctrl Pts',(2.32897397899994,5.2,3.99127654899999));
#338092=CARTESIAN_POINT('Ctrl Pts',(2.32897397899994,2.2,3.99127654899999));
#338093=CARTESIAN_POINT('Ctrl Pts',(2.32897523399994,12.2,3.99373853499998));
#338094=CARTESIAN_POINT('Ctrl Pts',(2.32897523399994,5.2,3.99373853499998));
#338095=CARTESIAN_POINT('Ctrl Pts',(2.32897523399994,2.2,3.99373853499998));
#338096=CARTESIAN_POINT('Ctrl Pts',(2.32897388199994,12.2,3.99620408999999));
#338097=CARTESIAN_POINT('Ctrl Pts',(2.32897388199994,5.2,3.99620408999999));
#338098=CARTESIAN_POINT('Ctrl Pts',(2.32897388199994,2.2,3.99620408999999));
#338099=CARTESIAN_POINT('Ctrl Pts',(2.32896991899994,12.2,3.99867320599999));
#338100=CARTESIAN_POINT('Ctrl Pts',(2.32896991899994,5.2,3.99867320599999));
#338101=CARTESIAN_POINT('Ctrl Pts',(2.32896991899994,2.2,3.99867320599999));
#338102=CARTESIAN_POINT('Ctrl Pts',(2.32896333499994,12.2,4.00114587899999));
#338103=CARTESIAN_POINT('Ctrl Pts',(2.32896333499994,5.2,4.00114587899999));
#338104=CARTESIAN_POINT('Ctrl Pts',(2.32896333499994,2.2,4.00114587899999));
#338105=CARTESIAN_POINT('Ctrl Pts',(2.32895412499994,12.2,4.00362209899999));
#338106=CARTESIAN_POINT('Ctrl Pts',(2.32895412499994,5.2,4.00362209899999));
#338107=CARTESIAN_POINT('Ctrl Pts',(2.32895412499994,2.2,4.00362209899999));
#338108=CARTESIAN_POINT('Ctrl Pts',(2.32894228399994,12.2,4.00610186299998));
#338109=CARTESIAN_POINT('Ctrl Pts',(2.32894228399994,5.2,4.00610186299998));
#338110=CARTESIAN_POINT('Ctrl Pts',(2.32894228399994,2.2,4.00610186299998));
#338111=CARTESIAN_POINT('Ctrl Pts',(2.32892780199994,12.2,4.00858516399998));
#338112=CARTESIAN_POINT('Ctrl Pts',(2.32892780199994,5.2,4.00858516399998));
#338113=CARTESIAN_POINT('Ctrl Pts',(2.32892780199994,2.2,4.00858516399998));
#338114=CARTESIAN_POINT('Ctrl Pts',(2.32891067499994,12.2,4.01107199399998));
#338115=CARTESIAN_POINT('Ctrl Pts',(2.32891067499994,5.2,4.01107199399998));
#338116=CARTESIAN_POINT('Ctrl Pts',(2.32891067499994,2.2,4.01107199399998));
#338117=CARTESIAN_POINT('Ctrl Pts',(2.32889089599994,12.2,4.01356234799999));
#338118=CARTESIAN_POINT('Ctrl Pts',(2.32889089599994,5.2,4.01356234799999));
#338119=CARTESIAN_POINT('Ctrl Pts',(2.32889089599994,2.2,4.01356234799999));
#338120=CARTESIAN_POINT('Ctrl Pts',(2.32886845899994,12.2,4.01605621899999));
#338121=CARTESIAN_POINT('Ctrl Pts',(2.32886845899994,5.2,4.01605621899999));
#338122=CARTESIAN_POINT('Ctrl Pts',(2.32886845899994,2.2,4.01605621899999));
#338123=CARTESIAN_POINT('Ctrl Pts',(2.32884335599994,12.2,4.01855360199999));
#338124=CARTESIAN_POINT('Ctrl Pts',(2.32884335599994,5.2,4.01855360199999));
#338125=CARTESIAN_POINT('Ctrl Pts',(2.32884335599994,2.2,4.01855360199999));
#338126=CARTESIAN_POINT('Ctrl Pts',(2.32881558199994,12.2,4.02105448799999));
#338127=CARTESIAN_POINT('Ctrl Pts',(2.32881558199994,5.2,4.02105448799999));
#338128=CARTESIAN_POINT('Ctrl Pts',(2.32881558199994,2.2,4.02105448799999));
#338129=CARTESIAN_POINT('Ctrl Pts',(2.32878512999994,12.2,4.02355887399998));
#338130=CARTESIAN_POINT('Ctrl Pts',(2.32878512999994,5.2,4.02355887399998));
#338131=CARTESIAN_POINT('Ctrl Pts',(2.32878512999994,2.2,4.02355887399998));
#338132=CARTESIAN_POINT('Ctrl Pts',(2.32875199399994,12.2,4.02606675199999));
#338133=CARTESIAN_POINT('Ctrl Pts',(2.32875199399994,5.2,4.02606675199999));
#338134=CARTESIAN_POINT('Ctrl Pts',(2.32875199399994,2.2,4.02606675199999));
#338135=CARTESIAN_POINT('Ctrl Pts',(2.32871616699994,12.2,4.02857811499998));
#338136=CARTESIAN_POINT('Ctrl Pts',(2.32871616699994,5.2,4.02857811499998));
#338137=CARTESIAN_POINT('Ctrl Pts',(2.32871616699994,2.2,4.02857811499998));
#338138=CARTESIAN_POINT('Ctrl Pts',(2.32867764299994,12.2,4.03109295699998));
#338139=CARTESIAN_POINT('Ctrl Pts',(2.32867764299994,5.2,4.03109295699998));
#338140=CARTESIAN_POINT('Ctrl Pts',(2.32867764299994,2.2,4.03109295699998));
#338141=CARTESIAN_POINT('Ctrl Pts',(2.32863641599994,12.2,4.03361127299998));
#338142=CARTESIAN_POINT('Ctrl Pts',(2.32863641599994,5.2,4.03361127299998));
#338143=CARTESIAN_POINT('Ctrl Pts',(2.32863641599994,2.2,4.03361127299998));
#338144=CARTESIAN_POINT('Ctrl Pts',(2.32859247799994,12.2,4.03613305399999));
#338145=CARTESIAN_POINT('Ctrl Pts',(2.32859247799994,5.2,4.03613305399999));
#338146=CARTESIAN_POINT('Ctrl Pts',(2.32859247799994,2.2,4.03613305399999));
#338147=CARTESIAN_POINT('Ctrl Pts',(2.32854582499994,12.2,4.03865829699999));
#338148=CARTESIAN_POINT('Ctrl Pts',(2.32854582499994,5.2,4.03865829699999));
#338149=CARTESIAN_POINT('Ctrl Pts',(2.32854582499994,2.2,4.03865829699999));
#338150=CARTESIAN_POINT('Ctrl Pts',(2.32849644899995,12.2,4.04118699199999));
#338151=CARTESIAN_POINT('Ctrl Pts',(2.32849644899995,5.2,4.04118699199999));
#338152=CARTESIAN_POINT('Ctrl Pts',(2.32849644899995,2.2,4.04118699199999));
#338153=CARTESIAN_POINT('Ctrl Pts',(2.32844434499994,12.2,4.04371913499999));
#338154=CARTESIAN_POINT('Ctrl Pts',(2.32844434499994,5.2,4.04371913499999));
#338155=CARTESIAN_POINT('Ctrl Pts',(2.32844434499994,2.2,4.04371913499999));
#338156=CARTESIAN_POINT('Ctrl Pts',(2.32838950599994,12.2,4.04625471999999));
#338157=CARTESIAN_POINT('Ctrl Pts',(2.32838950599994,5.2,4.04625471999999));
#338158=CARTESIAN_POINT('Ctrl Pts',(2.32838950599994,2.2,4.04625471999999));
#338159=CARTESIAN_POINT('Ctrl Pts',(2.32833192599994,12.2,4.04879373899998));
#338160=CARTESIAN_POINT('Ctrl Pts',(2.32833192599994,5.2,4.04879373899998));
#338161=CARTESIAN_POINT('Ctrl Pts',(2.32833192599994,2.2,4.04879373899998));
#338162=CARTESIAN_POINT('Ctrl Pts',(2.32827159799994,12.2,4.05133618699999));
#338163=CARTESIAN_POINT('Ctrl Pts',(2.32827159799994,5.2,4.05133618699999));
#338164=CARTESIAN_POINT('Ctrl Pts',(2.32827159799994,2.2,4.05133618699999));
#338165=CARTESIAN_POINT('Ctrl Pts',(2.32820851699994,12.2,4.05388205699998));
#338166=CARTESIAN_POINT('Ctrl Pts',(2.32820851699994,5.2,4.05388205699998));
#338167=CARTESIAN_POINT('Ctrl Pts',(2.32820851699994,2.2,4.05388205699998));
#338168=CARTESIAN_POINT('Ctrl Pts',(2.32814267599994,12.2,4.05643134199998));
#338169=CARTESIAN_POINT('Ctrl Pts',(2.32814267599994,5.2,4.05643134199998));
#338170=CARTESIAN_POINT('Ctrl Pts',(2.32814267599994,2.2,4.05643134199998));
#338171=CARTESIAN_POINT('Ctrl Pts',(2.32807406899994,12.2,4.05898403699998));
#338172=CARTESIAN_POINT('Ctrl Pts',(2.32807406899994,5.2,4.05898403699998));
#338173=CARTESIAN_POINT('Ctrl Pts',(2.32807406899994,2.2,4.05898403699998));
#338174=CARTESIAN_POINT('Ctrl Pts',(2.32800268999994,12.2,4.06154013499999));
#338175=CARTESIAN_POINT('Ctrl Pts',(2.32800268999994,5.2,4.06154013499999));
#338176=CARTESIAN_POINT('Ctrl Pts',(2.32800268999994,2.2,4.06154013499999));
#338177=CARTESIAN_POINT('Ctrl Pts',(2.32792853199994,12.2,4.06409962899998));
#338178=CARTESIAN_POINT('Ctrl Pts',(2.32792853199994,5.2,4.06409962899998));
#338179=CARTESIAN_POINT('Ctrl Pts',(2.32792853199994,2.2,4.06409962899998));
#338180=CARTESIAN_POINT('Ctrl Pts',(2.32785158999994,12.2,4.06666251299999));
#338181=CARTESIAN_POINT('Ctrl Pts',(2.32785158999994,5.2,4.06666251299999));
#338182=CARTESIAN_POINT('Ctrl Pts',(2.32785158999994,2.2,4.06666251299999));
#338183=CARTESIAN_POINT('Ctrl Pts',(2.32777185699994,12.2,4.06922878199998));
#338184=CARTESIAN_POINT('Ctrl Pts',(2.32777185699994,5.2,4.06922878199998));
#338185=CARTESIAN_POINT('Ctrl Pts',(2.32777185699994,2.2,4.06922878199998));
#338186=CARTESIAN_POINT('Ctrl Pts',(2.32768932599994,12.2,4.07179842699998));
#338187=CARTESIAN_POINT('Ctrl Pts',(2.32768932599994,5.2,4.07179842699998));
#338188=CARTESIAN_POINT('Ctrl Pts',(2.32768932599994,2.2,4.07179842699998));
#338189=CARTESIAN_POINT('Ctrl Pts',(2.32760399399994,12.2,4.07437144399999));
#338190=CARTESIAN_POINT('Ctrl Pts',(2.32760399399994,5.2,4.07437144399999));
#338191=CARTESIAN_POINT('Ctrl Pts',(2.32760399399994,2.2,4.07437144399999));
#338192=CARTESIAN_POINT('Ctrl Pts',(2.32751585199995,12.2,4.07694782499998));
#338193=CARTESIAN_POINT('Ctrl Pts',(2.32751585199995,5.2,4.07694782499998));
#338194=CARTESIAN_POINT('Ctrl Pts',(2.32751585199995,2.2,4.07694782499998));
#338195=CARTESIAN_POINT('Ctrl Pts',(2.32742489599994,12.2,4.07952756599999));
#338196=CARTESIAN_POINT('Ctrl Pts',(2.32742489599994,5.2,4.07952756599999));
#338197=CARTESIAN_POINT('Ctrl Pts',(2.32742489599994,2.2,4.07952756599999));
#338198=CARTESIAN_POINT('Ctrl Pts',(2.32733111999994,12.2,4.08211065799998));
#338199=CARTESIAN_POINT('Ctrl Pts',(2.32733111999994,5.2,4.08211065799998));
#338200=CARTESIAN_POINT('Ctrl Pts',(2.32733111999994,2.2,4.08211065799998));
#338201=CARTESIAN_POINT('Ctrl Pts',(2.32723451599994,12.2,4.08469709699999));
#338202=CARTESIAN_POINT('Ctrl Pts',(2.32723451599994,5.2,4.08469709699999));
#338203=CARTESIAN_POINT('Ctrl Pts',(2.32723451599994,2.2,4.08469709699999));
#338204=CARTESIAN_POINT('Ctrl Pts',(2.32713507999994,12.2,4.08728687499998));
#338205=CARTESIAN_POINT('Ctrl Pts',(2.32713507999994,5.2,4.08728687499998));
#338206=CARTESIAN_POINT('Ctrl Pts',(2.32713507999994,2.2,4.08728687499998));
#338207=CARTESIAN_POINT('Ctrl Pts',(2.32703280399994,12.2,4.08987998599999));
#338208=CARTESIAN_POINT('Ctrl Pts',(2.32703280399994,5.2,4.08987998599999));
#338209=CARTESIAN_POINT('Ctrl Pts',(2.32703280399994,2.2,4.08987998599999));
#338210=CARTESIAN_POINT('Ctrl Pts',(2.32692768299994,12.2,4.09247642199999));
#338211=CARTESIAN_POINT('Ctrl Pts',(2.32692768299994,5.2,4.09247642199999));
#338212=CARTESIAN_POINT('Ctrl Pts',(2.32692768299994,2.2,4.09247642199999));
#338213=CARTESIAN_POINT('Ctrl Pts',(2.32681970999994,12.2,4.09507617799999));
#338214=CARTESIAN_POINT('Ctrl Pts',(2.32681970999994,5.2,4.09507617799999));
#338215=CARTESIAN_POINT('Ctrl Pts',(2.32681970999994,2.2,4.09507617799999));
#338216=CARTESIAN_POINT('Ctrl Pts',(2.32670887999994,12.2,4.09767924799999));
#338217=CARTESIAN_POINT('Ctrl Pts',(2.32670887999994,5.2,4.09767924799999));
#338218=CARTESIAN_POINT('Ctrl Pts',(2.32670887999994,2.2,4.09767924799999));
#338219=CARTESIAN_POINT('Ctrl Pts',(2.32659518599994,12.2,4.10028562499999));
#338220=CARTESIAN_POINT('Ctrl Pts',(2.32659518599994,5.2,4.10028562499999));
#338221=CARTESIAN_POINT('Ctrl Pts',(2.32659518599994,2.2,4.10028562499999));
#338222=CARTESIAN_POINT('Ctrl Pts',(2.32647862299994,12.2,4.10289530199999));
#338223=CARTESIAN_POINT('Ctrl Pts',(2.32647862299994,5.2,4.10289530199999));
#338224=CARTESIAN_POINT('Ctrl Pts',(2.32647862299994,2.2,4.10289530199999));
#338225=CARTESIAN_POINT('Ctrl Pts',(2.32635918599994,12.2,4.10550827399998));
#338226=CARTESIAN_POINT('Ctrl Pts',(2.32635918599994,5.2,4.10550827399998));
#338227=CARTESIAN_POINT('Ctrl Pts',(2.32635918599994,2.2,4.10550827399998));
#338228=CARTESIAN_POINT('Ctrl Pts',(2.32623686999994,12.2,4.10812453699998));
#338229=CARTESIAN_POINT('Ctrl Pts',(2.32623686999994,5.2,4.10812453699998));
#338230=CARTESIAN_POINT('Ctrl Pts',(2.32623686999994,2.2,4.10812453699998));
#338231=CARTESIAN_POINT('Ctrl Pts',(2.32611166899995,12.2,4.11074408199998));
#338232=CARTESIAN_POINT('Ctrl Pts',(2.32611166899995,5.2,4.11074408199998));
#338233=CARTESIAN_POINT('Ctrl Pts',(2.32611166899995,2.2,4.11074408199998));
#338234=CARTESIAN_POINT('Ctrl Pts',(2.32598357799994,12.2,4.11336690499999));
#338235=CARTESIAN_POINT('Ctrl Pts',(2.32598357799994,5.2,4.11336690499999));
#338236=CARTESIAN_POINT('Ctrl Pts',(2.32598357799994,2.2,4.11336690499999));
#338237=CARTESIAN_POINT('Ctrl Pts',(2.32585258899995,12.2,4.11599299899999));
#338238=CARTESIAN_POINT('Ctrl Pts',(2.32585258899995,5.2,4.11599299899999));
#338239=CARTESIAN_POINT('Ctrl Pts',(2.32585258899995,2.2,4.11599299899999));
#338240=CARTESIAN_POINT('Ctrl Pts',(2.32571869499994,12.2,4.11862235399998));
#338241=CARTESIAN_POINT('Ctrl Pts',(2.32571869499994,5.2,4.11862235399998));
#338242=CARTESIAN_POINT('Ctrl Pts',(2.32571869499994,2.2,4.11862235399998));
#338243=CARTESIAN_POINT('Ctrl Pts',(2.32558188999994,12.2,4.12125496399998));
#338244=CARTESIAN_POINT('Ctrl Pts',(2.32558188999994,5.2,4.12125496399998));
#338245=CARTESIAN_POINT('Ctrl Pts',(2.32558188999994,2.2,4.12125496399998));
#338246=CARTESIAN_POINT('Ctrl Pts',(2.32544216699994,12.2,4.12389081999999));
#338247=CARTESIAN_POINT('Ctrl Pts',(2.32544216699994,5.2,4.12389081999999));
#338248=CARTESIAN_POINT('Ctrl Pts',(2.32544216699994,2.2,4.12389081999999));
#338249=CARTESIAN_POINT('Ctrl Pts',(2.32529951799994,12.2,4.12652991599998));
#338250=CARTESIAN_POINT('Ctrl Pts',(2.32529951799994,5.2,4.12652991599998));
#338251=CARTESIAN_POINT('Ctrl Pts',(2.32529951799994,2.2,4.12652991599998));
#338252=CARTESIAN_POINT('Ctrl Pts',(2.32515393799994,12.2,4.12917224599998));
#338253=CARTESIAN_POINT('Ctrl Pts',(2.32515393799994,5.2,4.12917224599998));
#338254=CARTESIAN_POINT('Ctrl Pts',(2.32515393799994,2.2,4.12917224599998));
#338255=CARTESIAN_POINT('Ctrl Pts',(2.32500542299994,12.2,4.13181780399999));
#338256=CARTESIAN_POINT('Ctrl Pts',(2.32500542299994,5.2,4.13181780399999));
#338257=CARTESIAN_POINT('Ctrl Pts',(2.32500542299994,2.2,4.13181780399999));
#338258=CARTESIAN_POINT('Ctrl Pts',(2.32485396999994,12.2,4.13446658699999));
#338259=CARTESIAN_POINT('Ctrl Pts',(2.32485396999994,5.2,4.13446658699999));
#338260=CARTESIAN_POINT('Ctrl Pts',(2.32485396999994,2.2,4.13446658699999));
#338261=CARTESIAN_POINT('Ctrl Pts',(2.3246995789955,12.2,4.1371185950763));
#338262=CARTESIAN_POINT('Ctrl Pts',(2.3246995789955,5.2,4.1371185950763));
#338263=CARTESIAN_POINT('Ctrl Pts',(2.3246995789955,2.2,4.1371185950763));
#338264=CARTESIAN_POINT('Ctrl Pts',(2.32457371399089,12.2,4.1392427791528));
#338265=CARTESIAN_POINT('Ctrl Pts',(2.32457371399089,5.2,4.1392427791528));
#338266=CARTESIAN_POINT('Ctrl Pts',(2.32457371399089,2.2,4.1392427791528));
#338267=CARTESIAN_POINT('Ctrl Pts',(2.32447799198617,12.2,4.14083736722942));
#338268=CARTESIAN_POINT('Ctrl Pts',(2.32447799198617,5.2,4.14083736722942));
#338269=CARTESIAN_POINT('Ctrl Pts',(2.32447799198617,2.2,4.14083736722942));
#338270=CARTESIAN_POINT('Ctrl Pts',(2.32441358898141,12.2,4.14190107030607));
#338271=CARTESIAN_POINT('Ctrl Pts',(2.32441358898141,5.2,4.14190107030607));
#338272=CARTESIAN_POINT('Ctrl Pts',(2.32441358898141,2.2,4.14190107030607));
#338273=CARTESIAN_POINT('Ctrl Pts',(2.32438124099994,12.2,4.14243308299999));
#338274=CARTESIAN_POINT('Ctrl Pts',(2.32438124099994,5.2,4.14243308299999));
#338275=CARTESIAN_POINT('Ctrl Pts',(2.32438124099994,2.2,4.14243308299999));
#338276=CARTESIAN_POINT('Origin',(2.68745007499994,15.2,2.95418363899999));
#338277=CARTESIAN_POINT('',(2.43934748299994,2.2,2.68145648099999));
#338278=CARTESIAN_POINT('',(2.68748460699994,12.2,2.95422159799998));
#338279=CARTESIAN_POINT('Origin',(-5.66300478732629E-14,15.2,-1.77635683940025E-14));
#338280=CARTESIAN_POINT('',(3.25496455399994,12.2,2.31410196199999));
#338281=CARTESIAN_POINT('',(2.95444430699995,12.2,2.10044848399999));
#338282=CARTESIAN_POINT('Ctrl Pts',(3.44029922199995,12.2,3.27518568399999));
#338283=CARTESIAN_POINT('Ctrl Pts',(3.44029922199995,5.2,3.27518568399999));
#338284=CARTESIAN_POINT('Ctrl Pts',(3.44029922199995,2.2,3.27518568399999));
#338285=CARTESIAN_POINT('Ctrl Pts',(3.43977569199994,12.2,3.27508567799998));
#338286=CARTESIAN_POINT('Ctrl Pts',(3.43977569199994,5.2,3.27508567799998));
#338287=CARTESIAN_POINT('Ctrl Pts',(3.43977569199994,2.2,3.27508567799998));
#338288=CARTESIAN_POINT('Ctrl Pts',(3.43872901899994,12.2,3.27488545899998));
#338289=CARTESIAN_POINT('Ctrl Pts',(3.43872901899994,5.2,3.27488545899998));
#338290=CARTESIAN_POINT('Ctrl Pts',(3.43872901899994,2.2,3.27488545899998));
#338291=CARTESIAN_POINT('Ctrl Pts',(3.43716016399994,12.2,3.27458451299999));
#338292=CARTESIAN_POINT('Ctrl Pts',(3.43716016399994,5.2,3.27458451299999));
#338293=CARTESIAN_POINT('Ctrl Pts',(3.43716016399994,2.2,3.27458451299999));
#338294=CARTESIAN_POINT('Ctrl Pts',(3.43507066699994,12.2,3.27418202199999));
#338295=CARTESIAN_POINT('Ctrl Pts',(3.43507066699994,5.2,3.27418202199999));
#338296=CARTESIAN_POINT('Ctrl Pts',(3.43507066699994,2.2,3.27418202199999));
#338297=CARTESIAN_POINT('Ctrl Pts',(3.43246264299994,12.2,3.27367685499999));
#338298=CARTESIAN_POINT('Ctrl Pts',(3.43246264299994,5.2,3.27367685499999));
#338299=CARTESIAN_POINT('Ctrl Pts',(3.43246264299994,2.2,3.27367685499999));
#338300=CARTESIAN_POINT('Ctrl Pts',(3.42985846999994,12.2,3.27316963499998));
#338301=CARTESIAN_POINT('Ctrl Pts',(3.42985846999994,5.2,3.27316963499998));
#338302=CARTESIAN_POINT('Ctrl Pts',(3.42985846999994,2.2,3.27316963499998));
#338303=CARTESIAN_POINT('Ctrl Pts',(3.42725814699994,12.2,3.27266036499999));
#338304=CARTESIAN_POINT('Ctrl Pts',(3.42725814699994,5.2,3.27266036499999));
#338305=CARTESIAN_POINT('Ctrl Pts',(3.42725814699994,2.2,3.27266036499999));
#338306=CARTESIAN_POINT('Ctrl Pts',(3.42466167799994,12.2,3.27214904799998));
#338307=CARTESIAN_POINT('Ctrl Pts',(3.42466167799994,5.2,3.27214904799998));
#338308=CARTESIAN_POINT('Ctrl Pts',(3.42466167799994,2.2,3.27214904799998));
#338309=CARTESIAN_POINT('Ctrl Pts',(3.42206906499994,12.2,3.27163568999998));
#338310=CARTESIAN_POINT('Ctrl Pts',(3.42206906499994,5.2,3.27163568999998));
#338311=CARTESIAN_POINT('Ctrl Pts',(3.42206906499994,2.2,3.27163568999998));
#338312=CARTESIAN_POINT('Ctrl Pts',(3.41948031499994,12.2,3.27112029599999));
#338313=CARTESIAN_POINT('Ctrl Pts',(3.41948031499994,5.2,3.27112029599999));
#338314=CARTESIAN_POINT('Ctrl Pts',(3.41948031499994,2.2,3.27112029599999));
#338315=CARTESIAN_POINT('Ctrl Pts',(3.41689542999994,12.2,3.27060287499998));
#338316=CARTESIAN_POINT('Ctrl Pts',(3.41689542999994,5.2,3.27060287499998));
#338317=CARTESIAN_POINT('Ctrl Pts',(3.41689542999994,2.2,3.27060287499998));
#338318=CARTESIAN_POINT('Ctrl Pts',(3.41431441799994,12.2,3.27008343699998));
#338319=CARTESIAN_POINT('Ctrl Pts',(3.41431441799994,5.2,3.27008343699998));
#338320=CARTESIAN_POINT('Ctrl Pts',(3.41431441799994,2.2,3.27008343699998));
#338321=CARTESIAN_POINT('Ctrl Pts',(3.41173728499994,12.2,3.26956198899998));
#338322=CARTESIAN_POINT('Ctrl Pts',(3.41173728499994,5.2,3.26956198899998));
#338323=CARTESIAN_POINT('Ctrl Pts',(3.41173728499994,2.2,3.26956198899998));
#338324=CARTESIAN_POINT('Ctrl Pts',(3.40916403599994,12.2,3.26903854199998));
#338325=CARTESIAN_POINT('Ctrl Pts',(3.40916403599994,5.2,3.26903854199998));
#338326=CARTESIAN_POINT('Ctrl Pts',(3.40916403599994,2.2,3.26903854199998));
#338327=CARTESIAN_POINT('Ctrl Pts',(3.40659467599994,12.2,3.26851310199999));
#338328=CARTESIAN_POINT('Ctrl Pts',(3.40659467599994,5.2,3.26851310199999));
#338329=CARTESIAN_POINT('Ctrl Pts',(3.40659467599994,2.2,3.26851310199999));
#338330=CARTESIAN_POINT('Ctrl Pts',(3.40402921099995,12.2,3.26798567699999));
#338331=CARTESIAN_POINT('Ctrl Pts',(3.40402921099995,5.2,3.26798567699999));
#338332=CARTESIAN_POINT('Ctrl Pts',(3.40402921099995,2.2,3.26798567699999));
#338333=CARTESIAN_POINT('Ctrl Pts',(3.40146764399994,12.2,3.26745627399998));
#338334=CARTESIAN_POINT('Ctrl Pts',(3.40146764399994,5.2,3.26745627399998));
#338335=CARTESIAN_POINT('Ctrl Pts',(3.40146764399994,2.2,3.26745627399998));
#338336=CARTESIAN_POINT('Ctrl Pts',(3.39890997999994,12.2,3.26692490099998));
#338337=CARTESIAN_POINT('Ctrl Pts',(3.39890997999994,5.2,3.26692490099998));
#338338=CARTESIAN_POINT('Ctrl Pts',(3.39890997999994,2.2,3.26692490099998));
#338339=CARTESIAN_POINT('Ctrl Pts',(3.39635622399994,12.2,3.26639156099999));
#338340=CARTESIAN_POINT('Ctrl Pts',(3.39635622399994,5.2,3.26639156099999));
#338341=CARTESIAN_POINT('Ctrl Pts',(3.39635622399994,2.2,3.26639156099999));
#338342=CARTESIAN_POINT('Ctrl Pts',(3.39380637899994,12.2,3.26585626399999));
#338343=CARTESIAN_POINT('Ctrl Pts',(3.39380637899994,5.2,3.26585626399999));
#338344=CARTESIAN_POINT('Ctrl Pts',(3.39380637899994,2.2,3.26585626399999));
#338345=CARTESIAN_POINT('Ctrl Pts',(3.39126044899994,12.2,3.26531901499998));
#338346=CARTESIAN_POINT('Ctrl Pts',(3.39126044899994,5.2,3.26531901499998));
#338347=CARTESIAN_POINT('Ctrl Pts',(3.39126044899994,2.2,3.26531901499998));
#338348=CARTESIAN_POINT('Ctrl Pts',(3.38871844099994,12.2,3.26477982299998));
#338349=CARTESIAN_POINT('Ctrl Pts',(3.38871844099994,5.2,3.26477982299998));
#338350=CARTESIAN_POINT('Ctrl Pts',(3.38871844099994,2.2,3.26477982299998));
#338351=CARTESIAN_POINT('Ctrl Pts',(3.38618035899994,12.2,3.26423869499998));
#338352=CARTESIAN_POINT('Ctrl Pts',(3.38618035899994,5.2,3.26423869499998));
#338353=CARTESIAN_POINT('Ctrl Pts',(3.38618035899994,2.2,3.26423869499998));
#338354=CARTESIAN_POINT('Ctrl Pts',(3.38364620599994,12.2,3.26369563699998));
#338355=CARTESIAN_POINT('Ctrl Pts',(3.38364620599994,5.2,3.26369563699998));
#338356=CARTESIAN_POINT('Ctrl Pts',(3.38364620599994,2.2,3.26369563699998));
#338357=CARTESIAN_POINT('Ctrl Pts',(3.38111598999994,12.2,3.26315065999999));
#338358=CARTESIAN_POINT('Ctrl Pts',(3.38111598999994,5.2,3.26315065999999));
#338359=CARTESIAN_POINT('Ctrl Pts',(3.38111598999994,2.2,3.26315065999999));
#338360=CARTESIAN_POINT('Ctrl Pts',(3.37858971299994,12.2,3.26260376899998));
#338361=CARTESIAN_POINT('Ctrl Pts',(3.37858971299994,5.2,3.26260376899998));
#338362=CARTESIAN_POINT('Ctrl Pts',(3.37858971299994,2.2,3.26260376899998));
#338363=CARTESIAN_POINT('Ctrl Pts',(3.37606738299994,12.2,3.26205497299998));
#338364=CARTESIAN_POINT('Ctrl Pts',(3.37606738299994,5.2,3.26205497299998));
#338365=CARTESIAN_POINT('Ctrl Pts',(3.37606738299994,2.2,3.26205497299998));
#338366=CARTESIAN_POINT('Ctrl Pts',(3.37354899999994,12.2,3.26150427799998));
#338367=CARTESIAN_POINT('Ctrl Pts',(3.37354899999994,5.2,3.26150427799998));
#338368=CARTESIAN_POINT('Ctrl Pts',(3.37354899999994,2.2,3.26150427799998));
#338369=CARTESIAN_POINT('Ctrl Pts',(3.37103457299994,12.2,3.26095169299998));
#338370=CARTESIAN_POINT('Ctrl Pts',(3.37103457299994,5.2,3.26095169299998));
#338371=CARTESIAN_POINT('Ctrl Pts',(3.37103457299994,2.2,3.26095169299998));
#338372=CARTESIAN_POINT('Ctrl Pts',(3.36852410399994,12.2,3.26039722299999));
#338373=CARTESIAN_POINT('Ctrl Pts',(3.36852410399994,5.2,3.26039722299999));
#338374=CARTESIAN_POINT('Ctrl Pts',(3.36852410399994,2.2,3.26039722299999));
#338375=CARTESIAN_POINT('Ctrl Pts',(3.36601759899994,12.2,3.25984087699998));
#338376=CARTESIAN_POINT('Ctrl Pts',(3.36601759899994,5.2,3.25984087699998));
#338377=CARTESIAN_POINT('Ctrl Pts',(3.36601759899994,2.2,3.25984087699998));
#338378=CARTESIAN_POINT('Ctrl Pts',(3.36351506199994,12.2,3.25928266199998));
#338379=CARTESIAN_POINT('Ctrl Pts',(3.36351506199994,5.2,3.25928266199998));
#338380=CARTESIAN_POINT('Ctrl Pts',(3.36351506199994,2.2,3.25928266199998));
#338381=CARTESIAN_POINT('Ctrl Pts',(3.36101649699994,12.2,3.25872258599999));
#338382=CARTESIAN_POINT('Ctrl Pts',(3.36101649699994,5.2,3.25872258599999));
#338383=CARTESIAN_POINT('Ctrl Pts',(3.36101649699994,2.2,3.25872258599999));
#338384=CARTESIAN_POINT('Ctrl Pts',(3.35852190999995,12.2,3.25816065699998));
#338385=CARTESIAN_POINT('Ctrl Pts',(3.35852190999995,5.2,3.25816065699998));
#338386=CARTESIAN_POINT('Ctrl Pts',(3.35852190999995,2.2,3.25816065699998));
#338387=CARTESIAN_POINT('Ctrl Pts',(3.35603130399994,12.2,3.25759688099998));
#338388=CARTESIAN_POINT('Ctrl Pts',(3.35603130399994,5.2,3.25759688099998));
#338389=CARTESIAN_POINT('Ctrl Pts',(3.35603130399994,2.2,3.25759688099998));
#338390=CARTESIAN_POINT('Ctrl Pts',(3.35354468599995,12.2,3.25703126499998));
#338391=CARTESIAN_POINT('Ctrl Pts',(3.35354468599995,5.2,3.25703126499998));
#338392=CARTESIAN_POINT('Ctrl Pts',(3.35354468599995,2.2,3.25703126499998));
#338393=CARTESIAN_POINT('Ctrl Pts',(3.35106205899995,12.2,3.25646381999999));
#338394=CARTESIAN_POINT('Ctrl Pts',(3.35106205899995,5.2,3.25646381999999));
#338395=CARTESIAN_POINT('Ctrl Pts',(3.35106205899995,2.2,3.25646381999999));
#338396=CARTESIAN_POINT('Ctrl Pts',(3.34858342799994,12.2,3.25589455099998));
#338397=CARTESIAN_POINT('Ctrl Pts',(3.34858342799994,5.2,3.25589455099998));
#338398=CARTESIAN_POINT('Ctrl Pts',(3.34858342799994,2.2,3.25589455099998));
#338399=CARTESIAN_POINT('Ctrl Pts',(3.34610879699994,12.2,3.25532346499998));
#338400=CARTESIAN_POINT('Ctrl Pts',(3.34610879699994,5.2,3.25532346499998));
#338401=CARTESIAN_POINT('Ctrl Pts',(3.34610879699994,2.2,3.25532346499998));
#338402=CARTESIAN_POINT('Ctrl Pts',(3.34363817199994,12.2,3.25475057199998));
#338403=CARTESIAN_POINT('Ctrl Pts',(3.34363817199994,5.2,3.25475057199998));
#338404=CARTESIAN_POINT('Ctrl Pts',(3.34363817199994,2.2,3.25475057199998));
#338405=CARTESIAN_POINT('Ctrl Pts',(3.34117155699994,12.2,3.25417587899998));
#338406=CARTESIAN_POINT('Ctrl Pts',(3.34117155699994,5.2,3.25417587899998));
#338407=CARTESIAN_POINT('Ctrl Pts',(3.34117155699994,2.2,3.25417587899998));
#338408=CARTESIAN_POINT('Ctrl Pts',(3.33870895599994,12.2,3.25359939099998));
#338409=CARTESIAN_POINT('Ctrl Pts',(3.33870895599994,5.2,3.25359939099998));
#338410=CARTESIAN_POINT('Ctrl Pts',(3.33870895599994,2.2,3.25359939099998));
#338411=CARTESIAN_POINT('Ctrl Pts',(3.33625037399994,12.2,3.25302111999999));
#338412=CARTESIAN_POINT('Ctrl Pts',(3.33625037399994,5.2,3.25302111999999));
#338413=CARTESIAN_POINT('Ctrl Pts',(3.33625037399994,2.2,3.25302111999999));
#338414=CARTESIAN_POINT('Ctrl Pts',(3.33379581499994,12.2,3.25244106999998));
#338415=CARTESIAN_POINT('Ctrl Pts',(3.33379581499994,5.2,3.25244106999998));
#338416=CARTESIAN_POINT('Ctrl Pts',(3.33379581499994,2.2,3.25244106999998));
#338417=CARTESIAN_POINT('Ctrl Pts',(3.33134528499994,12.2,3.25185924999998));
#338418=CARTESIAN_POINT('Ctrl Pts',(3.33134528499994,5.2,3.25185924999998));
#338419=CARTESIAN_POINT('Ctrl Pts',(3.33134528499994,2.2,3.25185924999998));
#338420=CARTESIAN_POINT('Ctrl Pts',(3.32889878899994,12.2,3.25127566799999));
#338421=CARTESIAN_POINT('Ctrl Pts',(3.32889878899994,5.2,3.25127566799999));
#338422=CARTESIAN_POINT('Ctrl Pts',(3.32889878899994,2.2,3.25127566799999));
#338423=CARTESIAN_POINT('Ctrl Pts',(3.32645632899994,12.2,3.25069033099999));
#338424=CARTESIAN_POINT('Ctrl Pts',(3.32645632899994,5.2,3.25069033099999));
#338425=CARTESIAN_POINT('Ctrl Pts',(3.32645632899994,2.2,3.25069033099999));
#338426=CARTESIAN_POINT('Ctrl Pts',(3.32401791099994,12.2,3.25010324799998));
#338427=CARTESIAN_POINT('Ctrl Pts',(3.32401791099994,5.2,3.25010324799998));
#338428=CARTESIAN_POINT('Ctrl Pts',(3.32401791099994,2.2,3.25010324799998));
#338429=CARTESIAN_POINT('Ctrl Pts',(3.32158353999994,12.2,3.24951442599998));
#338430=CARTESIAN_POINT('Ctrl Pts',(3.32158353999994,5.2,3.24951442599998));
#338431=CARTESIAN_POINT('Ctrl Pts',(3.32158353999994,2.2,3.24951442599998));
#338432=CARTESIAN_POINT('Ctrl Pts',(3.31915322099994,12.2,3.24892387199998));
#338433=CARTESIAN_POINT('Ctrl Pts',(3.31915322099994,5.2,3.24892387199998));
#338434=CARTESIAN_POINT('Ctrl Pts',(3.31915322099994,2.2,3.24892387199998));
#338435=CARTESIAN_POINT('Ctrl Pts',(3.31672695699994,12.2,3.24833159499998));
#338436=CARTESIAN_POINT('Ctrl Pts',(3.31672695699994,5.2,3.24833159499998));
#338437=CARTESIAN_POINT('Ctrl Pts',(3.31672695699994,2.2,3.24833159499998));
#338438=CARTESIAN_POINT('Ctrl Pts',(3.31430475199994,12.2,3.24773760199999));
#338439=CARTESIAN_POINT('Ctrl Pts',(3.31430475199994,5.2,3.24773760199999));
#338440=CARTESIAN_POINT('Ctrl Pts',(3.31430475199994,2.2,3.24773760199999));
#338441=CARTESIAN_POINT('Ctrl Pts',(3.31188661399994,12.2,3.24714190199998));
#338442=CARTESIAN_POINT('Ctrl Pts',(3.31188661399994,5.2,3.24714190199998));
#338443=CARTESIAN_POINT('Ctrl Pts',(3.31188661399994,2.2,3.24714190199998));
#338444=CARTESIAN_POINT('Ctrl Pts',(3.30947254399995,12.2,3.24654450099998));
#338445=CARTESIAN_POINT('Ctrl Pts',(3.30947254399995,5.2,3.24654450099998));
#338446=CARTESIAN_POINT('Ctrl Pts',(3.30947254399995,2.2,3.24654450099998));
#338447=CARTESIAN_POINT('Ctrl Pts',(3.30706254899995,12.2,3.24594540799998));
#338448=CARTESIAN_POINT('Ctrl Pts',(3.30706254899995,5.2,3.24594540799998));
#338449=CARTESIAN_POINT('Ctrl Pts',(3.30706254899995,2.2,3.24594540799998));
#338450=CARTESIAN_POINT('Ctrl Pts',(3.30465663199994,12.2,3.24534463199999));
#338451=CARTESIAN_POINT('Ctrl Pts',(3.30465663199994,5.2,3.24534463199999));
#338452=CARTESIAN_POINT('Ctrl Pts',(3.30465663199994,2.2,3.24534463199999));
#338453=CARTESIAN_POINT('Ctrl Pts',(3.30225479899994,12.2,3.24474217799998));
#338454=CARTESIAN_POINT('Ctrl Pts',(3.30225479899994,5.2,3.24474217799998));
#338455=CARTESIAN_POINT('Ctrl Pts',(3.30225479899994,2.2,3.24474217799998));
#338456=CARTESIAN_POINT('Ctrl Pts',(3.29985705299995,12.2,3.24413805699999));
#338457=CARTESIAN_POINT('Ctrl Pts',(3.29985705299995,5.2,3.24413805699999));
#338458=CARTESIAN_POINT('Ctrl Pts',(3.29985705299995,2.2,3.24413805699999));
#338459=CARTESIAN_POINT('Ctrl Pts',(3.29746339799994,12.2,3.24353227399998));
#338460=CARTESIAN_POINT('Ctrl Pts',(3.29746339799994,5.2,3.24353227399998));
#338461=CARTESIAN_POINT('Ctrl Pts',(3.29746339799994,2.2,3.24353227399998));
#338462=CARTESIAN_POINT('Ctrl Pts',(3.29507384099994,12.2,3.24292483899999));
#338463=CARTESIAN_POINT('Ctrl Pts',(3.29507384099994,5.2,3.24292483899999));
#338464=CARTESIAN_POINT('Ctrl Pts',(3.29507384099994,2.2,3.24292483899999));
#338465=CARTESIAN_POINT('Ctrl Pts',(3.29268838499994,12.2,3.24231575899999));
#338466=CARTESIAN_POINT('Ctrl Pts',(3.29268838499994,5.2,3.24231575899999));
#338467=CARTESIAN_POINT('Ctrl Pts',(3.29268838499994,2.2,3.24231575899999));
#338468=CARTESIAN_POINT('Ctrl Pts',(3.29030703499994,12.2,3.24170504199999));
#338469=CARTESIAN_POINT('Ctrl Pts',(3.29030703499994,5.2,3.24170504199999));
#338470=CARTESIAN_POINT('Ctrl Pts',(3.29030703499994,2.2,3.24170504199999));
#338471=CARTESIAN_POINT('Ctrl Pts',(3.28792979399994,12.2,3.24109269699999));
#338472=CARTESIAN_POINT('Ctrl Pts',(3.28792979399994,5.2,3.24109269699999));
#338473=CARTESIAN_POINT('Ctrl Pts',(3.28792979399994,2.2,3.24109269699999));
#338474=CARTESIAN_POINT('Ctrl Pts',(3.28555666899994,12.2,3.24047873199999));
#338475=CARTESIAN_POINT('Ctrl Pts',(3.28555666899994,5.2,3.24047873199999));
#338476=CARTESIAN_POINT('Ctrl Pts',(3.28555666899994,2.2,3.24047873199999));
#338477=CARTESIAN_POINT('Ctrl Pts',(3.28318766199994,12.2,3.23986315299998));
#338478=CARTESIAN_POINT('Ctrl Pts',(3.28318766199994,5.2,3.23986315299998));
#338479=CARTESIAN_POINT('Ctrl Pts',(3.28318766199994,2.2,3.23986315299998));
#338480=CARTESIAN_POINT('Ctrl Pts',(3.28082277999994,12.2,3.23924596999999));
#338481=CARTESIAN_POINT('Ctrl Pts',(3.28082277999994,5.2,3.23924596999999));
#338482=CARTESIAN_POINT('Ctrl Pts',(3.28082277999994,2.2,3.23924596999999));
#338483=CARTESIAN_POINT('Ctrl Pts',(3.27846202599994,12.2,3.23862718999998));
#338484=CARTESIAN_POINT('Ctrl Pts',(3.27846202599994,5.2,3.23862718999998));
#338485=CARTESIAN_POINT('Ctrl Pts',(3.27846202599994,2.2,3.23862718999998));
#338486=CARTESIAN_POINT('Ctrl Pts',(3.27610540399994,12.2,3.23800682099999));
#338487=CARTESIAN_POINT('Ctrl Pts',(3.27610540399994,5.2,3.23800682099999));
#338488=CARTESIAN_POINT('Ctrl Pts',(3.27610540399994,2.2,3.23800682099999));
#338489=CARTESIAN_POINT('Ctrl Pts',(3.27375291999994,12.2,3.23738487199999));
#338490=CARTESIAN_POINT('Ctrl Pts',(3.27375291999994,5.2,3.23738487199999));
#338491=CARTESIAN_POINT('Ctrl Pts',(3.27375291999994,2.2,3.23738487199999));
#338492=CARTESIAN_POINT('Ctrl Pts',(3.27140457599994,12.2,3.23676135099999));
#338493=CARTESIAN_POINT('Ctrl Pts',(3.27140457599994,5.2,3.23676135099999));
#338494=CARTESIAN_POINT('Ctrl Pts',(3.27140457599994,2.2,3.23676135099999));
#338495=CARTESIAN_POINT('Ctrl Pts',(3.26906037999994,12.2,3.23613626499998));
#338496=CARTESIAN_POINT('Ctrl Pts',(3.26906037999994,5.2,3.23613626499998));
#338497=CARTESIAN_POINT('Ctrl Pts',(3.26906037999994,2.2,3.23613626499998));
#338498=CARTESIAN_POINT('Ctrl Pts',(3.26672033299995,12.2,3.23550962299999));
#338499=CARTESIAN_POINT('Ctrl Pts',(3.26672033299995,5.2,3.23550962299999));
#338500=CARTESIAN_POINT('Ctrl Pts',(3.26672033299995,2.2,3.23550962299999));
#338501=CARTESIAN_POINT('Ctrl Pts',(3.26438444199994,12.2,3.23488143299999));
#338502=CARTESIAN_POINT('Ctrl Pts',(3.26438444199994,5.2,3.23488143299999));
#338503=CARTESIAN_POINT('Ctrl Pts',(3.26438444199994,2.2,3.23488143299999));
#338504=CARTESIAN_POINT('Ctrl Pts',(3.26205271099994,12.2,3.23425170299998));
#338505=CARTESIAN_POINT('Ctrl Pts',(3.26205271099994,5.2,3.23425170299998));
#338506=CARTESIAN_POINT('Ctrl Pts',(3.26205271099994,2.2,3.23425170299998));
#338507=CARTESIAN_POINT('Ctrl Pts',(3.25972514299994,12.2,3.23362044099999));
#338508=CARTESIAN_POINT('Ctrl Pts',(3.25972514299994,5.2,3.23362044099999));
#338509=CARTESIAN_POINT('Ctrl Pts',(3.25972514299994,2.2,3.23362044099999));
#338510=CARTESIAN_POINT('Ctrl Pts',(3.25740174399994,12.2,3.23298765599999));
#338511=CARTESIAN_POINT('Ctrl Pts',(3.25740174399994,5.2,3.23298765599999));
#338512=CARTESIAN_POINT('Ctrl Pts',(3.25740174399994,2.2,3.23298765599999));
#338513=CARTESIAN_POINT('Ctrl Pts',(3.25508251599994,12.2,3.23235335699999));
#338514=CARTESIAN_POINT('Ctrl Pts',(3.25508251599994,5.2,3.23235335699999));
#338515=CARTESIAN_POINT('Ctrl Pts',(3.25508251599994,2.2,3.23235335699999));
#338516=CARTESIAN_POINT('Ctrl Pts',(3.25276746699994,12.2,3.23171754899998));
#338517=CARTESIAN_POINT('Ctrl Pts',(3.25276746699994,5.2,3.23171754899998));
#338518=CARTESIAN_POINT('Ctrl Pts',(3.25276746699994,2.2,3.23171754899998));
#338519=CARTESIAN_POINT('Ctrl Pts',(3.25045659899994,12.2,3.23108024299999));
#338520=CARTESIAN_POINT('Ctrl Pts',(3.25045659899994,5.2,3.23108024299999));
#338521=CARTESIAN_POINT('Ctrl Pts',(3.25045659899994,2.2,3.23108024299999));
#338522=CARTESIAN_POINT('Ctrl Pts',(3.24814991699995,12.2,3.23044144699999));
#338523=CARTESIAN_POINT('Ctrl Pts',(3.24814991699995,5.2,3.23044144699999));
#338524=CARTESIAN_POINT('Ctrl Pts',(3.24814991699995,2.2,3.23044144699999));
#338525=CARTESIAN_POINT('Ctrl Pts',(3.24584742499994,12.2,3.22980116799998));
#338526=CARTESIAN_POINT('Ctrl Pts',(3.24584742499994,5.2,3.22980116799998));
#338527=CARTESIAN_POINT('Ctrl Pts',(3.24584742499994,2.2,3.22980116799998));
#338528=CARTESIAN_POINT('Ctrl Pts',(3.24354912899994,12.2,3.22915941499998));
#338529=CARTESIAN_POINT('Ctrl Pts',(3.24354912899994,5.2,3.22915941499998));
#338530=CARTESIAN_POINT('Ctrl Pts',(3.24354912899994,2.2,3.22915941499998));
#338531=CARTESIAN_POINT('Ctrl Pts',(3.24125503199994,12.2,3.22851619699998));
#338532=CARTESIAN_POINT('Ctrl Pts',(3.24125503199994,5.2,3.22851619699998));
#338533=CARTESIAN_POINT('Ctrl Pts',(3.24125503199994,2.2,3.22851619699998));
#338534=CARTESIAN_POINT('Ctrl Pts',(3.23896513799995,12.2,3.22787152099998));
#338535=CARTESIAN_POINT('Ctrl Pts',(3.23896513799995,5.2,3.22787152099998));
#338536=CARTESIAN_POINT('Ctrl Pts',(3.23896513799995,2.2,3.22787152099998));
#338537=CARTESIAN_POINT('Ctrl Pts',(3.23667945299994,12.2,3.22722539699999));
#338538=CARTESIAN_POINT('Ctrl Pts',(3.23667945299994,5.2,3.22722539699999));
#338539=CARTESIAN_POINT('Ctrl Pts',(3.23667945299994,2.2,3.22722539699999));
#338540=CARTESIAN_POINT('Ctrl Pts',(3.23439797999994,12.2,3.22657783099999));
#338541=CARTESIAN_POINT('Ctrl Pts',(3.23439797999994,5.2,3.22657783099999));
#338542=CARTESIAN_POINT('Ctrl Pts',(3.23439797999994,2.2,3.22657783099999));
#338543=CARTESIAN_POINT('Ctrl Pts',(3.23212072399994,12.2,3.22592883399999));
#338544=CARTESIAN_POINT('Ctrl Pts',(3.23212072399994,5.2,3.22592883399999));
#338545=CARTESIAN_POINT('Ctrl Pts',(3.23212072399994,2.2,3.22592883399999));
#338546=CARTESIAN_POINT('Ctrl Pts',(3.22984768899994,12.2,3.22527841199998));
#338547=CARTESIAN_POINT('Ctrl Pts',(3.22984768899994,5.2,3.22527841199998));
#338548=CARTESIAN_POINT('Ctrl Pts',(3.22984768899994,2.2,3.22527841199998));
#338549=CARTESIAN_POINT('Ctrl Pts',(3.22757887999995,12.2,3.22462657599999));
#338550=CARTESIAN_POINT('Ctrl Pts',(3.22757887999995,5.2,3.22462657599999));
#338551=CARTESIAN_POINT('Ctrl Pts',(3.22757887999995,2.2,3.22462657599999));
#338552=CARTESIAN_POINT('Ctrl Pts',(3.22531429999994,12.2,3.22397333299998));
#338553=CARTESIAN_POINT('Ctrl Pts',(3.22531429999994,5.2,3.22397333299998));
#338554=CARTESIAN_POINT('Ctrl Pts',(3.22531429999994,2.2,3.22397333299998));
#338555=CARTESIAN_POINT('Ctrl Pts',(3.22305395499995,12.2,3.22331869099998));
#338556=CARTESIAN_POINT('Ctrl Pts',(3.22305395499995,5.2,3.22331869099998));
#338557=CARTESIAN_POINT('Ctrl Pts',(3.22305395499995,2.2,3.22331869099998));
#338558=CARTESIAN_POINT('Ctrl Pts',(3.22079784899994,12.2,3.22266265899999));
#338559=CARTESIAN_POINT('Ctrl Pts',(3.22079784899994,5.2,3.22266265899999));
#338560=CARTESIAN_POINT('Ctrl Pts',(3.22079784899994,2.2,3.22266265899999));
#338561=CARTESIAN_POINT('Ctrl Pts',(3.21854598499994,12.2,3.22200524599998));
#338562=CARTESIAN_POINT('Ctrl Pts',(3.21854598499994,5.2,3.22200524599998));
#338563=CARTESIAN_POINT('Ctrl Pts',(3.21854598499994,2.2,3.22200524599998));
#338564=CARTESIAN_POINT('Ctrl Pts',(3.21629836899994,12.2,3.22134645899999));
#338565=CARTESIAN_POINT('Ctrl Pts',(3.21629836899994,5.2,3.22134645899999));
#338566=CARTESIAN_POINT('Ctrl Pts',(3.21629836899994,2.2,3.22134645899999));
#338567=CARTESIAN_POINT('Ctrl Pts',(3.21405500399994,12.2,3.22068630799999));
#338568=CARTESIAN_POINT('Ctrl Pts',(3.21405500399994,5.2,3.22068630799999));
#338569=CARTESIAN_POINT('Ctrl Pts',(3.21405500399994,2.2,3.22068630799999));
#338570=CARTESIAN_POINT('Ctrl Pts',(3.21181589499994,12.2,3.22002480099999));
#338571=CARTESIAN_POINT('Ctrl Pts',(3.21181589499994,5.2,3.22002480099999));
#338572=CARTESIAN_POINT('Ctrl Pts',(3.21181589499994,2.2,3.22002480099999));
#338573=CARTESIAN_POINT('Ctrl Pts',(3.20958104699994,12.2,3.21936194599999));
#338574=CARTESIAN_POINT('Ctrl Pts',(3.20958104699994,5.2,3.21936194599999));
#338575=CARTESIAN_POINT('Ctrl Pts',(3.20958104699994,2.2,3.21936194599999));
#338576=CARTESIAN_POINT('Ctrl Pts',(3.20735046399995,12.2,3.21869775299999));
#338577=CARTESIAN_POINT('Ctrl Pts',(3.20735046399995,5.2,3.21869775299999));
#338578=CARTESIAN_POINT('Ctrl Pts',(3.20735046399995,2.2,3.21869775299999));
#338579=CARTESIAN_POINT('Ctrl Pts',(3.20512414899994,12.2,3.21803222899998));
#338580=CARTESIAN_POINT('Ctrl Pts',(3.20512414899994,5.2,3.21803222899998));
#338581=CARTESIAN_POINT('Ctrl Pts',(3.20512414899994,2.2,3.21803222899998));
#338582=CARTESIAN_POINT('Ctrl Pts',(3.20290210799994,12.2,3.21736538499999));
#338583=CARTESIAN_POINT('Ctrl Pts',(3.20290210799994,5.2,3.21736538499999));
#338584=CARTESIAN_POINT('Ctrl Pts',(3.20290210799994,2.2,3.21736538499999));
#338585=CARTESIAN_POINT('Ctrl Pts',(3.20068434399994,12.2,3.21669722699998));
#338586=CARTESIAN_POINT('Ctrl Pts',(3.20068434399994,5.2,3.21669722699998));
#338587=CARTESIAN_POINT('Ctrl Pts',(3.20068434399994,2.2,3.21669722699998));
#338588=CARTESIAN_POINT('Ctrl Pts',(3.19847086099994,12.2,3.21602776399998));
#338589=CARTESIAN_POINT('Ctrl Pts',(3.19847086099994,5.2,3.21602776399998));
#338590=CARTESIAN_POINT('Ctrl Pts',(3.19847086099994,2.2,3.21602776399998));
#338591=CARTESIAN_POINT('Ctrl Pts',(3.19626166499994,12.2,3.21535700599998));
#338592=CARTESIAN_POINT('Ctrl Pts',(3.19626166499994,5.2,3.21535700599998));
#338593=CARTESIAN_POINT('Ctrl Pts',(3.19626166499994,2.2,3.21535700599998));
#338594=CARTESIAN_POINT('Ctrl Pts',(3.19405675999994,12.2,3.21468495999999));
#338595=CARTESIAN_POINT('Ctrl Pts',(3.19405675999994,5.2,3.21468495999999));
#338596=CARTESIAN_POINT('Ctrl Pts',(3.19405675999994,2.2,3.21468495999999));
#338597=CARTESIAN_POINT('Ctrl Pts',(3.19185614899994,12.2,3.21401163799998));
#338598=CARTESIAN_POINT('Ctrl Pts',(3.19185614899994,5.2,3.21401163799998));
#338599=CARTESIAN_POINT('Ctrl Pts',(3.19185614899994,2.2,3.21401163799998));
#338600=CARTESIAN_POINT('Ctrl Pts',(3.18965983699994,12.2,3.21333704399999));
#338601=CARTESIAN_POINT('Ctrl Pts',(3.18965983699994,5.2,3.21333704399999));
#338602=CARTESIAN_POINT('Ctrl Pts',(3.18965983699994,2.2,3.21333704399999));
#338603=CARTESIAN_POINT('Ctrl Pts',(3.18746782799994,12.2,3.21266118999999));
#338604=CARTESIAN_POINT('Ctrl Pts',(3.18746782799994,5.2,3.21266118999999));
#338605=CARTESIAN_POINT('Ctrl Pts',(3.18746782799994,2.2,3.21266118999999));
#338606=CARTESIAN_POINT('Ctrl Pts',(3.18528012699994,12.2,3.21198408399999));
#338607=CARTESIAN_POINT('Ctrl Pts',(3.18528012699994,5.2,3.21198408399999));
#338608=CARTESIAN_POINT('Ctrl Pts',(3.18528012699994,2.2,3.21198408399999));
#338609=CARTESIAN_POINT('Ctrl Pts',(3.18309673699994,12.2,3.21130573399999));
#338610=CARTESIAN_POINT('Ctrl Pts',(3.18309673699994,5.2,3.21130573399999));
#338611=CARTESIAN_POINT('Ctrl Pts',(3.18309673699994,2.2,3.21130573399999));
#338612=CARTESIAN_POINT('Ctrl Pts',(3.18091766399994,12.2,3.21062614999998));
#338613=CARTESIAN_POINT('Ctrl Pts',(3.18091766399994,5.2,3.21062614999998));
#338614=CARTESIAN_POINT('Ctrl Pts',(3.18091766399994,2.2,3.21062614999998));
#338615=CARTESIAN_POINT('Ctrl Pts',(3.17874290899995,12.2,3.20994534099999));
#338616=CARTESIAN_POINT('Ctrl Pts',(3.17874290899995,5.2,3.20994534099999));
#338617=CARTESIAN_POINT('Ctrl Pts',(3.17874290899995,2.2,3.20994534099999));
#338618=CARTESIAN_POINT('Ctrl Pts',(3.17657247999994,12.2,3.20926331399999));
#338619=CARTESIAN_POINT('Ctrl Pts',(3.17657247999994,5.2,3.20926331399999));
#338620=CARTESIAN_POINT('Ctrl Pts',(3.17657247999994,2.2,3.20926331399999));
#338621=CARTESIAN_POINT('Ctrl Pts',(3.17440637999994,12.2,3.20858007899999));
#338622=CARTESIAN_POINT('Ctrl Pts',(3.17440637999994,5.2,3.20858007899999));
#338623=CARTESIAN_POINT('Ctrl Pts',(3.17440637999994,2.2,3.20858007899999));
#338624=CARTESIAN_POINT('Ctrl Pts',(3.17224461299995,12.2,3.20789564499999));
#338625=CARTESIAN_POINT('Ctrl Pts',(3.17224461299995,5.2,3.20789564499999));
#338626=CARTESIAN_POINT('Ctrl Pts',(3.17224461299995,2.2,3.20789564499999));
#338627=CARTESIAN_POINT('Ctrl Pts',(3.17008718199994,12.2,3.20721002099998));
#338628=CARTESIAN_POINT('Ctrl Pts',(3.17008718199994,5.2,3.20721002099998));
#338629=CARTESIAN_POINT('Ctrl Pts',(3.17008718199994,2.2,3.20721002099998));
#338630=CARTESIAN_POINT('Ctrl Pts',(3.16793409199994,12.2,3.20652321499999));
#338631=CARTESIAN_POINT('Ctrl Pts',(3.16793409199994,5.2,3.20652321499999));
#338632=CARTESIAN_POINT('Ctrl Pts',(3.16793409199994,2.2,3.20652321499999));
#338633=CARTESIAN_POINT('Ctrl Pts',(3.16578534799994,12.2,3.20583523599999));
#338634=CARTESIAN_POINT('Ctrl Pts',(3.16578534799994,5.2,3.20583523599999));
#338635=CARTESIAN_POINT('Ctrl Pts',(3.16578534799994,2.2,3.20583523599999));
#338636=CARTESIAN_POINT('Ctrl Pts',(3.16364095399994,12.2,3.20514609399999));
#338637=CARTESIAN_POINT('Ctrl Pts',(3.16364095399994,5.2,3.20514609399999));
#338638=CARTESIAN_POINT('Ctrl Pts',(3.16364095399994,2.2,3.20514609399999));
#338639=CARTESIAN_POINT('Ctrl Pts',(3.16150091399995,12.2,3.20445579799999));
#338640=CARTESIAN_POINT('Ctrl Pts',(3.16150091399995,5.2,3.20445579799999));
#338641=CARTESIAN_POINT('Ctrl Pts',(3.16150091399995,2.2,3.20445579799999));
#338642=CARTESIAN_POINT('Ctrl Pts',(3.15936523199994,12.2,3.20376435599999));
#338643=CARTESIAN_POINT('Ctrl Pts',(3.15936523199994,5.2,3.20376435599999));
#338644=CARTESIAN_POINT('Ctrl Pts',(3.15936523199994,2.2,3.20376435599999));
#338645=CARTESIAN_POINT('Ctrl Pts',(3.15723391199994,12.2,3.20307177699998));
#338646=CARTESIAN_POINT('Ctrl Pts',(3.15723391199994,5.2,3.20307177699998));
#338647=CARTESIAN_POINT('Ctrl Pts',(3.15723391199994,2.2,3.20307177699998));
#338648=CARTESIAN_POINT('Ctrl Pts',(3.15510695899994,12.2,3.20237806899998));
#338649=CARTESIAN_POINT('Ctrl Pts',(3.15510695899994,5.2,3.20237806899998));
#338650=CARTESIAN_POINT('Ctrl Pts',(3.15510695899994,2.2,3.20237806899998));
#338651=CARTESIAN_POINT('Ctrl Pts',(3.15298437499994,12.2,3.20168324399998));
#338652=CARTESIAN_POINT('Ctrl Pts',(3.15298437499994,5.2,3.20168324399998));
#338653=CARTESIAN_POINT('Ctrl Pts',(3.15298437499994,2.2,3.20168324399998));
#338654=CARTESIAN_POINT('Ctrl Pts',(3.15086616699995,12.2,3.20098730899999));
#338655=CARTESIAN_POINT('Ctrl Pts',(3.15086616699995,5.2,3.20098730899999));
#338656=CARTESIAN_POINT('Ctrl Pts',(3.15086616699995,2.2,3.20098730899999));
#338657=CARTESIAN_POINT('Ctrl Pts',(3.14875233699994,12.2,3.20029027299999));
#338658=CARTESIAN_POINT('Ctrl Pts',(3.14875233699994,5.2,3.20029027299999));
#338659=CARTESIAN_POINT('Ctrl Pts',(3.14875233699994,2.2,3.20029027299999));
#338660=CARTESIAN_POINT('Ctrl Pts',(3.14664288999994,12.2,3.19959214699999));
#338661=CARTESIAN_POINT('Ctrl Pts',(3.14664288999994,5.2,3.19959214699999));
#338662=CARTESIAN_POINT('Ctrl Pts',(3.14664288999994,2.2,3.19959214699999));
#338663=CARTESIAN_POINT('Ctrl Pts',(3.14453782999994,12.2,3.19889293699998));
#338664=CARTESIAN_POINT('Ctrl Pts',(3.14453782999994,5.2,3.19889293699998));
#338665=CARTESIAN_POINT('Ctrl Pts',(3.14453782999994,2.2,3.19889293699998));
#338666=CARTESIAN_POINT('Ctrl Pts',(3.14243716299994,12.2,3.19819265399998));
#338667=CARTESIAN_POINT('Ctrl Pts',(3.14243716299994,5.2,3.19819265399998));
#338668=CARTESIAN_POINT('Ctrl Pts',(3.14243716299994,2.2,3.19819265399998));
#338669=CARTESIAN_POINT('Ctrl Pts',(3.14034088999994,12.2,3.19749130699999));
#338670=CARTESIAN_POINT('Ctrl Pts',(3.14034088999994,5.2,3.19749130699999));
#338671=CARTESIAN_POINT('Ctrl Pts',(3.14034088999994,2.2,3.19749130699999));
#338672=CARTESIAN_POINT('Ctrl Pts',(3.13824901599994,12.2,3.19678890499999));
#338673=CARTESIAN_POINT('Ctrl Pts',(3.13824901599994,5.2,3.19678890499999));
#338674=CARTESIAN_POINT('Ctrl Pts',(3.13824901599994,2.2,3.19678890499999));
#338675=CARTESIAN_POINT('Ctrl Pts',(3.13616154599994,12.2,3.19608545799999));
#338676=CARTESIAN_POINT('Ctrl Pts',(3.13616154599994,5.2,3.19608545799999));
#338677=CARTESIAN_POINT('Ctrl Pts',(3.13616154599994,2.2,3.19608545799999));
#338678=CARTESIAN_POINT('Ctrl Pts',(3.13407848399994,12.2,3.19538097399998));
#338679=CARTESIAN_POINT('Ctrl Pts',(3.13407848399994,5.2,3.19538097399998));
#338680=CARTESIAN_POINT('Ctrl Pts',(3.13407848399994,2.2,3.19538097399998));
#338681=CARTESIAN_POINT('Ctrl Pts',(3.13199983299994,12.2,3.19467546199999));
#338682=CARTESIAN_POINT('Ctrl Pts',(3.13199983299994,5.2,3.19467546199999));
#338683=CARTESIAN_POINT('Ctrl Pts',(3.13199983299994,2.2,3.19467546199999));
#338684=CARTESIAN_POINT('Ctrl Pts',(3.12992559899994,12.2,3.19396893199999));
#338685=CARTESIAN_POINT('Ctrl Pts',(3.12992559899994,5.2,3.19396893199999));
#338686=CARTESIAN_POINT('Ctrl Pts',(3.12992559899994,2.2,3.19396893199999));
#338687=CARTESIAN_POINT('Ctrl Pts',(3.12785578499994,12.2,3.19326139299999));
#338688=CARTESIAN_POINT('Ctrl Pts',(3.12785578499994,5.2,3.19326139299999));
#338689=CARTESIAN_POINT('Ctrl Pts',(3.12785578499994,2.2,3.19326139299999));
#338690=CARTESIAN_POINT('Ctrl Pts',(3.12579039399994,12.2,3.19255285499998));
#338691=CARTESIAN_POINT('Ctrl Pts',(3.12579039399994,5.2,3.19255285499998));
#338692=CARTESIAN_POINT('Ctrl Pts',(3.12579039399994,2.2,3.19255285499998));
#338693=CARTESIAN_POINT('Ctrl Pts',(3.12372943099994,12.2,3.19184332599999));
#338694=CARTESIAN_POINT('Ctrl Pts',(3.12372943099994,5.2,3.19184332599999));
#338695=CARTESIAN_POINT('Ctrl Pts',(3.12372943099994,2.2,3.19184332599999));
#338696=CARTESIAN_POINT('Ctrl Pts',(3.12167290099994,12.2,3.19113281599999));
#338697=CARTESIAN_POINT('Ctrl Pts',(3.12167290099994,5.2,3.19113281599999));
#338698=CARTESIAN_POINT('Ctrl Pts',(3.12167290099994,2.2,3.19113281599999));
#338699=CARTESIAN_POINT('Ctrl Pts',(3.11962080699994,12.2,3.19042133399999));
#338700=CARTESIAN_POINT('Ctrl Pts',(3.11962080699994,5.2,3.19042133399999));
#338701=CARTESIAN_POINT('Ctrl Pts',(3.11962080699994,2.2,3.19042133399999));
#338702=CARTESIAN_POINT('Ctrl Pts',(3.11757315299994,12.2,3.18970889099998));
#338703=CARTESIAN_POINT('Ctrl Pts',(3.11757315299994,5.2,3.18970889099998));
#338704=CARTESIAN_POINT('Ctrl Pts',(3.11757315299994,2.2,3.18970889099998));
#338705=CARTESIAN_POINT('Ctrl Pts',(3.11552994399994,12.2,3.18899549399998));
#338706=CARTESIAN_POINT('Ctrl Pts',(3.11552994399994,5.2,3.18899549399998));
#338707=CARTESIAN_POINT('Ctrl Pts',(3.11552994399994,2.2,3.18899549399998));
#338708=CARTESIAN_POINT('Ctrl Pts',(3.11349118199994,12.2,3.18828115299999));
#338709=CARTESIAN_POINT('Ctrl Pts',(3.11349118199994,5.2,3.18828115299999));
#338710=CARTESIAN_POINT('Ctrl Pts',(3.11349118199994,2.2,3.18828115299999));
#338711=CARTESIAN_POINT('Ctrl Pts',(3.11145687399994,12.2,3.18756587899999));
#338712=CARTESIAN_POINT('Ctrl Pts',(3.11145687399994,5.2,3.18756587899999));
#338713=CARTESIAN_POINT('Ctrl Pts',(3.11145687399994,2.2,3.18756587899999));
#338714=CARTESIAN_POINT('Ctrl Pts',(3.10942702099994,12.2,3.18684967899999));
#338715=CARTESIAN_POINT('Ctrl Pts',(3.10942702099994,5.2,3.18684967899999));
#338716=CARTESIAN_POINT('Ctrl Pts',(3.10942702099994,2.2,3.18684967899999));
#338717=CARTESIAN_POINT('Ctrl Pts',(3.10740162899994,12.2,3.18613256399999));
#338718=CARTESIAN_POINT('Ctrl Pts',(3.10740162899994,5.2,3.18613256399999));
#338719=CARTESIAN_POINT('Ctrl Pts',(3.10740162899994,2.2,3.18613256399999));
#338720=CARTESIAN_POINT('Ctrl Pts',(3.10538070199994,12.2,3.18541454299999));
#338721=CARTESIAN_POINT('Ctrl Pts',(3.10538070199994,5.2,3.18541454299999));
#338722=CARTESIAN_POINT('Ctrl Pts',(3.10538070199994,2.2,3.18541454299999));
#338723=CARTESIAN_POINT('Ctrl Pts',(3.10336424299994,12.2,3.18469562499998));
#338724=CARTESIAN_POINT('Ctrl Pts',(3.10336424299994,5.2,3.18469562499998));
#338725=CARTESIAN_POINT('Ctrl Pts',(3.10336424299994,2.2,3.18469562499998));
#338726=CARTESIAN_POINT('Ctrl Pts',(3.10135225599995,12.2,3.18397582199999));
#338727=CARTESIAN_POINT('Ctrl Pts',(3.10135225599995,5.2,3.18397582199999));
#338728=CARTESIAN_POINT('Ctrl Pts',(3.10135225599995,2.2,3.18397582199999));
#338729=CARTESIAN_POINT('Ctrl Pts',(3.09934474499994,12.2,3.18325513999999));
#338730=CARTESIAN_POINT('Ctrl Pts',(3.09934474499994,5.2,3.18325513999999));
#338731=CARTESIAN_POINT('Ctrl Pts',(3.09934474499994,2.2,3.18325513999999));
#338732=CARTESIAN_POINT('Ctrl Pts',(3.09734171599994,12.2,3.18253358999999));
#338733=CARTESIAN_POINT('Ctrl Pts',(3.09734171599994,5.2,3.18253358999999));
#338734=CARTESIAN_POINT('Ctrl Pts',(3.09734171599994,2.2,3.18253358999999));
#338735=CARTESIAN_POINT('Ctrl Pts',(3.09534316999994,12.2,3.18181118299999));
#338736=CARTESIAN_POINT('Ctrl Pts',(3.09534316999994,5.2,3.18181118299999));
#338737=CARTESIAN_POINT('Ctrl Pts',(3.09534316999994,2.2,3.18181118299999));
#338738=CARTESIAN_POINT('Ctrl Pts',(3.09334911199994,12.2,3.18108792599999));
#338739=CARTESIAN_POINT('Ctrl Pts',(3.09334911199994,5.2,3.18108792599999));
#338740=CARTESIAN_POINT('Ctrl Pts',(3.09334911199994,2.2,3.18108792599999));
#338741=CARTESIAN_POINT('Ctrl Pts',(3.09135954699994,12.2,3.18036382999999));
#338742=CARTESIAN_POINT('Ctrl Pts',(3.09135954699994,5.2,3.18036382999999));
#338743=CARTESIAN_POINT('Ctrl Pts',(3.09135954699994,2.2,3.18036382999999));
#338744=CARTESIAN_POINT('Ctrl Pts',(3.08937447799994,12.2,3.17963890499998));
#338745=CARTESIAN_POINT('Ctrl Pts',(3.08937447799994,5.2,3.17963890499998));
#338746=CARTESIAN_POINT('Ctrl Pts',(3.08937447799994,2.2,3.17963890499998));
#338747=CARTESIAN_POINT('Ctrl Pts',(3.08739390899994,12.2,3.17891316099999));
#338748=CARTESIAN_POINT('Ctrl Pts',(3.08739390899994,5.2,3.17891316099999));
#338749=CARTESIAN_POINT('Ctrl Pts',(3.08739390899994,2.2,3.17891316099999));
#338750=CARTESIAN_POINT('Ctrl Pts',(3.08541784499994,12.2,3.17818660599999));
#338751=CARTESIAN_POINT('Ctrl Pts',(3.08541784499994,5.2,3.17818660599999));
#338752=CARTESIAN_POINT('Ctrl Pts',(3.08541784499994,2.2,3.17818660599999));
#338753=CARTESIAN_POINT('Ctrl Pts',(3.08344628799994,12.2,3.17745925099998));
#338754=CARTESIAN_POINT('Ctrl Pts',(3.08344628799994,5.2,3.17745925099998));
#338755=CARTESIAN_POINT('Ctrl Pts',(3.08344628799994,2.2,3.17745925099998));
#338756=CARTESIAN_POINT('Ctrl Pts',(3.08147924299994,12.2,3.17673110399999));
#338757=CARTESIAN_POINT('Ctrl Pts',(3.08147924299994,5.2,3.17673110399999));
#338758=CARTESIAN_POINT('Ctrl Pts',(3.08147924299994,2.2,3.17673110399999));
#338759=CARTESIAN_POINT('Ctrl Pts',(3.07951671499994,12.2,3.17600217599999));
#338760=CARTESIAN_POINT('Ctrl Pts',(3.07951671499994,5.2,3.17600217599999));
#338761=CARTESIAN_POINT('Ctrl Pts',(3.07951671499994,2.2,3.17600217599999));
#338762=CARTESIAN_POINT('Ctrl Pts',(3.07755870499994,12.2,3.17527247699999));
#338763=CARTESIAN_POINT('Ctrl Pts',(3.07755870499994,5.2,3.17527247699999));
#338764=CARTESIAN_POINT('Ctrl Pts',(3.07755870499994,2.2,3.17527247699999));
#338765=CARTESIAN_POINT('Ctrl Pts',(3.07560521899994,12.2,3.17454201799999));
#338766=CARTESIAN_POINT('Ctrl Pts',(3.07560521899994,5.2,3.17454201799999));
#338767=CARTESIAN_POINT('Ctrl Pts',(3.07560521899994,2.2,3.17454201799999));
#338768=CARTESIAN_POINT('Ctrl Pts',(3.07365626099994,12.2,3.17381080499998));
#338769=CARTESIAN_POINT('Ctrl Pts',(3.07365626099994,5.2,3.17381080499998));
#338770=CARTESIAN_POINT('Ctrl Pts',(3.07365626099994,2.2,3.17381080499998));
#338771=CARTESIAN_POINT('Ctrl Pts',(3.07171183499995,12.2,3.17307885099999));
#338772=CARTESIAN_POINT('Ctrl Pts',(3.07171183499995,5.2,3.17307885099999));
#338773=CARTESIAN_POINT('Ctrl Pts',(3.07171183499995,2.2,3.17307885099999));
#338774=CARTESIAN_POINT('Ctrl Pts',(3.06977194399995,12.2,3.17234616499999));
#338775=CARTESIAN_POINT('Ctrl Pts',(3.06977194399995,5.2,3.17234616499999));
#338776=CARTESIAN_POINT('Ctrl Pts',(3.06977194399995,2.2,3.17234616499999));
#338777=CARTESIAN_POINT('Ctrl Pts',(3.06783659099994,12.2,3.17161275499998));
#338778=CARTESIAN_POINT('Ctrl Pts',(3.06783659099994,5.2,3.17161275499998));
#338779=CARTESIAN_POINT('Ctrl Pts',(3.06783659099994,2.2,3.17161275499998));
#338780=CARTESIAN_POINT('Ctrl Pts',(3.06590578199994,12.2,3.17087863499999));
#338781=CARTESIAN_POINT('Ctrl Pts',(3.06590578199994,5.2,3.17087863499999));
#338782=CARTESIAN_POINT('Ctrl Pts',(3.06590578199994,2.2,3.17087863499999));
#338783=CARTESIAN_POINT('Ctrl Pts',(3.06397951999994,12.2,3.17014381099998));
#338784=CARTESIAN_POINT('Ctrl Pts',(3.06397951999994,5.2,3.17014381099998));
#338785=CARTESIAN_POINT('Ctrl Pts',(3.06397951999994,2.2,3.17014381099998));
#338786=CARTESIAN_POINT('Ctrl Pts',(3.06205780799994,12.2,3.16940829399999));
#338787=CARTESIAN_POINT('Ctrl Pts',(3.06205780799994,5.2,3.16940829399999));
#338788=CARTESIAN_POINT('Ctrl Pts',(3.06205780799994,2.2,3.16940829399999));
#338789=CARTESIAN_POINT('Ctrl Pts',(3.06014065099995,12.2,3.16867209499998));
#338790=CARTESIAN_POINT('Ctrl Pts',(3.06014065099995,5.2,3.16867209499998));
#338791=CARTESIAN_POINT('Ctrl Pts',(3.06014065099995,2.2,3.16867209499998));
#338792=CARTESIAN_POINT('Ctrl Pts',(3.05822805299994,12.2,3.16793522299999));
#338793=CARTESIAN_POINT('Ctrl Pts',(3.05822805299994,5.2,3.16793522299999));
#338794=CARTESIAN_POINT('Ctrl Pts',(3.05822805299994,2.2,3.16793522299999));
#338795=CARTESIAN_POINT('Ctrl Pts',(3.05632001699994,12.2,3.16719768799998));
#338796=CARTESIAN_POINT('Ctrl Pts',(3.05632001699994,5.2,3.16719768799998));
#338797=CARTESIAN_POINT('Ctrl Pts',(3.05632001699994,2.2,3.16719768799998));
#338798=CARTESIAN_POINT('Ctrl Pts',(3.05441654599994,12.2,3.16645949999998));
#338799=CARTESIAN_POINT('Ctrl Pts',(3.05441654599994,5.2,3.16645949999998));
#338800=CARTESIAN_POINT('Ctrl Pts',(3.05441654599994,2.2,3.16645949999998));
#338801=CARTESIAN_POINT('Ctrl Pts',(3.05251764599995,12.2,3.16572066899998));
#338802=CARTESIAN_POINT('Ctrl Pts',(3.05251764599995,5.2,3.16572066899998));
#338803=CARTESIAN_POINT('Ctrl Pts',(3.05251764599995,2.2,3.16572066899998));
#338804=CARTESIAN_POINT('Ctrl Pts',(3.05062331899994,12.2,3.16498120599999));
#338805=CARTESIAN_POINT('Ctrl Pts',(3.05062331899994,5.2,3.16498120599999));
#338806=CARTESIAN_POINT('Ctrl Pts',(3.05062331899994,2.2,3.16498120599999));
#338807=CARTESIAN_POINT('Ctrl Pts',(3.04873356899994,12.2,3.16424111899998));
#338808=CARTESIAN_POINT('Ctrl Pts',(3.04873356899994,5.2,3.16424111899998));
#338809=CARTESIAN_POINT('Ctrl Pts',(3.04873356899994,2.2,3.16424111899998));
#338810=CARTESIAN_POINT('Ctrl Pts',(3.04684840199994,12.2,3.16350042099998));
#338811=CARTESIAN_POINT('Ctrl Pts',(3.04684840199994,5.2,3.16350042099998));
#338812=CARTESIAN_POINT('Ctrl Pts',(3.04684840199994,2.2,3.16350042099998));
#338813=CARTESIAN_POINT('Ctrl Pts',(3.04496781799994,12.2,3.16275911799998));
#338814=CARTESIAN_POINT('Ctrl Pts',(3.04496781799994,5.2,3.16275911799998));
#338815=CARTESIAN_POINT('Ctrl Pts',(3.04496781799994,2.2,3.16275911799998));
#338816=CARTESIAN_POINT('Ctrl Pts',(3.04309182299995,12.2,3.16201722499999));
#338817=CARTESIAN_POINT('Ctrl Pts',(3.04309182299995,5.2,3.16201722499999));
#338818=CARTESIAN_POINT('Ctrl Pts',(3.04309182299995,2.2,3.16201722499999));
#338819=CARTESIAN_POINT('Ctrl Pts',(3.04122042199995,12.2,3.16127474799998));
#338820=CARTESIAN_POINT('Ctrl Pts',(3.04122042199995,5.2,3.16127474799998));
#338821=CARTESIAN_POINT('Ctrl Pts',(3.04122042199995,2.2,3.16127474799998));
#338822=CARTESIAN_POINT('Ctrl Pts',(3.03935361599994,12.2,3.16053169999999));
#338823=CARTESIAN_POINT('Ctrl Pts',(3.03935361599994,5.2,3.16053169999999));
#338824=CARTESIAN_POINT('Ctrl Pts',(3.03935361599994,2.2,3.16053169999999));
#338825=CARTESIAN_POINT('Ctrl Pts',(3.03749140999995,12.2,3.15978808799999));
#338826=CARTESIAN_POINT('Ctrl Pts',(3.03749140999995,5.2,3.15978808799999));
#338827=CARTESIAN_POINT('Ctrl Pts',(3.03749140999995,2.2,3.15978808799999));
#338828=CARTESIAN_POINT('Ctrl Pts',(3.03563380799994,12.2,3.15904392599998));
#338829=CARTESIAN_POINT('Ctrl Pts',(3.03563380799994,5.2,3.15904392599998));
#338830=CARTESIAN_POINT('Ctrl Pts',(3.03563380799994,2.2,3.15904392599998));
#338831=CARTESIAN_POINT('Ctrl Pts',(3.03378081399994,12.2,3.15829922099999));
#338832=CARTESIAN_POINT('Ctrl Pts',(3.03378081399994,5.2,3.15829922099999));
#338833=CARTESIAN_POINT('Ctrl Pts',(3.03378081399994,2.2,3.15829922099999));
#338834=CARTESIAN_POINT('Ctrl Pts',(3.03193242999994,12.2,3.15755398499999));
#338835=CARTESIAN_POINT('Ctrl Pts',(3.03193242999994,5.2,3.15755398499999));
#338836=CARTESIAN_POINT('Ctrl Pts',(3.03193242999994,2.2,3.15755398499999));
#338837=CARTESIAN_POINT('Ctrl Pts',(3.03008866199994,12.2,3.15680822899999));
#338838=CARTESIAN_POINT('Ctrl Pts',(3.03008866199994,5.2,3.15680822899999));
#338839=CARTESIAN_POINT('Ctrl Pts',(3.03008866199994,2.2,3.15680822899999));
#338840=CARTESIAN_POINT('Ctrl Pts',(3.02824951199994,12.2,3.15606196099999));
#338841=CARTESIAN_POINT('Ctrl Pts',(3.02824951199994,5.2,3.15606196099999));
#338842=CARTESIAN_POINT('Ctrl Pts',(3.02824951199994,2.2,3.15606196099999));
#338843=CARTESIAN_POINT('Ctrl Pts',(3.02641498399994,12.2,3.15531519299999));
#338844=CARTESIAN_POINT('Ctrl Pts',(3.02641498399994,5.2,3.15531519299999));
#338845=CARTESIAN_POINT('Ctrl Pts',(3.02641498399994,2.2,3.15531519299999));
#338846=CARTESIAN_POINT('Ctrl Pts',(3.02458508299994,12.2,3.15456793499998));
#338847=CARTESIAN_POINT('Ctrl Pts',(3.02458508299994,5.2,3.15456793499998));
#338848=CARTESIAN_POINT('Ctrl Pts',(3.02458508299994,2.2,3.15456793499998));
#338849=CARTESIAN_POINT('Ctrl Pts',(3.02275981199994,12.2,3.15382019599999));
#338850=CARTESIAN_POINT('Ctrl Pts',(3.02275981199994,5.2,3.15382019599999));
#338851=CARTESIAN_POINT('Ctrl Pts',(3.02275981199994,2.2,3.15382019599999));
#338852=CARTESIAN_POINT('Ctrl Pts',(3.02093917299994,12.2,3.15307198799999));
#338853=CARTESIAN_POINT('Ctrl Pts',(3.02093917299994,5.2,3.15307198799999));
#338854=CARTESIAN_POINT('Ctrl Pts',(3.02093917299994,2.2,3.15307198799999));
#338855=CARTESIAN_POINT('Ctrl Pts',(3.01912317099994,12.2,3.15232332099999));
#338856=CARTESIAN_POINT('Ctrl Pts',(3.01912317099994,5.2,3.15232332099999));
#338857=CARTESIAN_POINT('Ctrl Pts',(3.01912317099994,2.2,3.15232332099999));
#338858=CARTESIAN_POINT('Ctrl Pts',(3.01731180999994,12.2,3.15157420499999));
#338859=CARTESIAN_POINT('Ctrl Pts',(3.01731180999994,5.2,3.15157420499999));
#338860=CARTESIAN_POINT('Ctrl Pts',(3.01731180999994,2.2,3.15157420499999));
#338861=CARTESIAN_POINT('Ctrl Pts',(3.01550509399994,12.2,3.15082465099999));
#338862=CARTESIAN_POINT('Ctrl Pts',(3.01550509399994,5.2,3.15082465099999));
#338863=CARTESIAN_POINT('Ctrl Pts',(3.01550509399994,2.2,3.15082465099999));
#338864=CARTESIAN_POINT('Ctrl Pts',(3.01370302499994,12.2,3.15007466999998));
#338865=CARTESIAN_POINT('Ctrl Pts',(3.01370302499994,5.2,3.15007466999998));
#338866=CARTESIAN_POINT('Ctrl Pts',(3.01370302499994,2.2,3.15007466999998));
#338867=CARTESIAN_POINT('Ctrl Pts',(3.01190560799995,12.2,3.14932426999999));
#338868=CARTESIAN_POINT('Ctrl Pts',(3.01190560799995,5.2,3.14932426999999));
#338869=CARTESIAN_POINT('Ctrl Pts',(3.01190560799995,2.2,3.14932426999999));
#338870=CARTESIAN_POINT('Ctrl Pts',(3.01011284599995,12.2,3.14857346399998));
#338871=CARTESIAN_POINT('Ctrl Pts',(3.01011284599995,5.2,3.14857346399998));
#338872=CARTESIAN_POINT('Ctrl Pts',(3.01011284599995,2.2,3.14857346399998));
#338873=CARTESIAN_POINT('Ctrl Pts',(3.00832474399995,12.2,3.14782226199998));
#338874=CARTESIAN_POINT('Ctrl Pts',(3.00832474399995,5.2,3.14782226199998));
#338875=CARTESIAN_POINT('Ctrl Pts',(3.00832474399995,2.2,3.14782226199998));
#338876=CARTESIAN_POINT('Ctrl Pts',(3.00654130299994,12.2,3.14707067499998));
#338877=CARTESIAN_POINT('Ctrl Pts',(3.00654130299994,5.2,3.14707067499998));
#338878=CARTESIAN_POINT('Ctrl Pts',(3.00654130299994,2.2,3.14707067499998));
#338879=CARTESIAN_POINT('Ctrl Pts',(3.00476252899994,12.2,3.14631871099999));
#338880=CARTESIAN_POINT('Ctrl Pts',(3.00476252899994,5.2,3.14631871099999));
#338881=CARTESIAN_POINT('Ctrl Pts',(3.00476252899994,2.2,3.14631871099999));
#338882=CARTESIAN_POINT('Ctrl Pts',(3.00298842299994,12.2,3.14556638299998));
#338883=CARTESIAN_POINT('Ctrl Pts',(3.00298842299994,5.2,3.14556638299998));
#338884=CARTESIAN_POINT('Ctrl Pts',(3.00298842299994,2.2,3.14556638299998));
#338885=CARTESIAN_POINT('Ctrl Pts',(3.00121899199994,12.2,3.14481370199999));
#338886=CARTESIAN_POINT('Ctrl Pts',(3.00121899199994,5.2,3.14481370199999));
#338887=CARTESIAN_POINT('Ctrl Pts',(3.00121899199994,2.2,3.14481370199999));
#338888=CARTESIAN_POINT('Ctrl Pts',(2.99945423699994,12.2,3.14406067699998));
#338889=CARTESIAN_POINT('Ctrl Pts',(2.99945423699994,5.2,3.14406067699998));
#338890=CARTESIAN_POINT('Ctrl Pts',(2.99945423699994,2.2,3.14406067699998));
#338891=CARTESIAN_POINT('Ctrl Pts',(2.99769416199994,12.2,3.14330731899998));
#338892=CARTESIAN_POINT('Ctrl Pts',(2.99769416199994,5.2,3.14330731899998));
#338893=CARTESIAN_POINT('Ctrl Pts',(2.99769416199994,2.2,3.14330731899998));
#338894=CARTESIAN_POINT('Ctrl Pts',(2.99593877199994,12.2,3.14255363899999));
#338895=CARTESIAN_POINT('Ctrl Pts',(2.99593877199994,5.2,3.14255363899999));
#338896=CARTESIAN_POINT('Ctrl Pts',(2.99593877199994,2.2,3.14255363899999));
#338897=CARTESIAN_POINT('Ctrl Pts',(2.99418806799994,12.2,3.14179964699999));
#338898=CARTESIAN_POINT('Ctrl Pts',(2.99418806799994,5.2,3.14179964699999));
#338899=CARTESIAN_POINT('Ctrl Pts',(2.99418806799994,2.2,3.14179964699999));
#338900=CARTESIAN_POINT('Ctrl Pts',(2.99244205499994,12.2,3.14104535499999));
#338901=CARTESIAN_POINT('Ctrl Pts',(2.99244205499994,5.2,3.14104535499999));
#338902=CARTESIAN_POINT('Ctrl Pts',(2.99244205499994,2.2,3.14104535499999));
#338903=CARTESIAN_POINT('Ctrl Pts',(2.99070073699994,12.2,3.14029077499999));
#338904=CARTESIAN_POINT('Ctrl Pts',(2.99070073699994,5.2,3.14029077499999));
#338905=CARTESIAN_POINT('Ctrl Pts',(2.99070073699994,2.2,3.14029077499999));
#338906=CARTESIAN_POINT('Ctrl Pts',(2.98896411699995,12.2,3.13953591399999));
#338907=CARTESIAN_POINT('Ctrl Pts',(2.98896411699995,5.2,3.13953591399999));
#338908=CARTESIAN_POINT('Ctrl Pts',(2.98896411699995,2.2,3.13953591399999));
#338909=CARTESIAN_POINT('Ctrl Pts',(2.98723219799994,12.2,3.13878078399998));
#338910=CARTESIAN_POINT('Ctrl Pts',(2.98723219799994,5.2,3.13878078399998));
#338911=CARTESIAN_POINT('Ctrl Pts',(2.98723219799994,2.2,3.13878078399998));
#338912=CARTESIAN_POINT('Ctrl Pts',(2.98550498499994,12.2,3.13802539799998));
#338913=CARTESIAN_POINT('Ctrl Pts',(2.98550498499994,5.2,3.13802539799998));
#338914=CARTESIAN_POINT('Ctrl Pts',(2.98550498499994,2.2,3.13802539799998));
#338915=CARTESIAN_POINT('Ctrl Pts',(2.98378247999994,12.2,3.13726976499999));
#338916=CARTESIAN_POINT('Ctrl Pts',(2.98378247999994,5.2,3.13726976499999));
#338917=CARTESIAN_POINT('Ctrl Pts',(2.98378247999994,2.2,3.13726976499999));
#338918=CARTESIAN_POINT('Ctrl Pts',(2.98206468699994,12.2,3.13651389599999));
#338919=CARTESIAN_POINT('Ctrl Pts',(2.98206468699994,5.2,3.13651389599999));
#338920=CARTESIAN_POINT('Ctrl Pts',(2.98206468699994,2.2,3.13651389599999));
#338921=CARTESIAN_POINT('Ctrl Pts',(2.98035160799994,12.2,3.13575780299999));
#338922=CARTESIAN_POINT('Ctrl Pts',(2.98035160799994,5.2,3.13575780299999));
#338923=CARTESIAN_POINT('Ctrl Pts',(2.98035160799994,2.2,3.13575780299999));
#338924=CARTESIAN_POINT('Ctrl Pts',(2.97864324999995,12.2,3.13500149499998));
#338925=CARTESIAN_POINT('Ctrl Pts',(2.97864324999995,5.2,3.13500149499998));
#338926=CARTESIAN_POINT('Ctrl Pts',(2.97864324999995,2.2,3.13500149499998));
#338927=CARTESIAN_POINT('Ctrl Pts',(2.97693961299994,12.2,3.13424498399999));
#338928=CARTESIAN_POINT('Ctrl Pts',(2.97693961299994,5.2,3.13424498399999));
#338929=CARTESIAN_POINT('Ctrl Pts',(2.97693961299994,2.2,3.13424498399999));
#338930=CARTESIAN_POINT('Ctrl Pts',(2.97524070299994,12.2,3.13348828099999));
#338931=CARTESIAN_POINT('Ctrl Pts',(2.97524070299994,5.2,3.13348828099999));
#338932=CARTESIAN_POINT('Ctrl Pts',(2.97524070299994,2.2,3.13348828099999));
#338933=CARTESIAN_POINT('Ctrl Pts',(2.97354652199994,12.2,3.13273139699999));
#338934=CARTESIAN_POINT('Ctrl Pts',(2.97354652199994,5.2,3.13273139699999));
#338935=CARTESIAN_POINT('Ctrl Pts',(2.97354652199994,2.2,3.13273139699999));
#338936=CARTESIAN_POINT('Ctrl Pts',(2.97185707199994,12.2,3.13197434399999));
#338937=CARTESIAN_POINT('Ctrl Pts',(2.97185707199994,5.2,3.13197434399999));
#338938=CARTESIAN_POINT('Ctrl Pts',(2.97185707199994,2.2,3.13197434399999));
#338939=CARTESIAN_POINT('Ctrl Pts',(2.97017235999995,12.2,3.13121713099999));
#338940=CARTESIAN_POINT('Ctrl Pts',(2.97017235999995,5.2,3.13121713099999));
#338941=CARTESIAN_POINT('Ctrl Pts',(2.97017235999995,2.2,3.13121713099999));
#338942=CARTESIAN_POINT('Ctrl Pts',(2.96849238699994,12.2,3.13045976999998));
#338943=CARTESIAN_POINT('Ctrl Pts',(2.96849238699994,5.2,3.13045976999998));
#338944=CARTESIAN_POINT('Ctrl Pts',(2.96849238699994,2.2,3.13045976999998));
#338945=CARTESIAN_POINT('Ctrl Pts',(2.96681715699994,12.2,3.12970227099999));
#338946=CARTESIAN_POINT('Ctrl Pts',(2.96681715699994,5.2,3.12970227099999));
#338947=CARTESIAN_POINT('Ctrl Pts',(2.96681715699994,2.2,3.12970227099999));
#338948=CARTESIAN_POINT('Ctrl Pts',(2.96514667299994,12.2,3.12894464799999));
#338949=CARTESIAN_POINT('Ctrl Pts',(2.96514667299994,5.2,3.12894464799999));
#338950=CARTESIAN_POINT('Ctrl Pts',(2.96514667299994,2.2,3.12894464799999));
#338951=CARTESIAN_POINT('Ctrl Pts',(2.96348093899995,12.2,3.12818690899999));
#338952=CARTESIAN_POINT('Ctrl Pts',(2.96348093899995,5.2,3.12818690899999));
#338953=CARTESIAN_POINT('Ctrl Pts',(2.96348093899995,2.2,3.12818690899999));
#338954=CARTESIAN_POINT('Ctrl Pts',(2.96181995799994,12.2,3.12742906699999));
#338955=CARTESIAN_POINT('Ctrl Pts',(2.96181995799994,5.2,3.12742906699999));
#338956=CARTESIAN_POINT('Ctrl Pts',(2.96181995799994,2.2,3.12742906699999));
#338957=CARTESIAN_POINT('Ctrl Pts',(2.96016373299994,12.2,3.12667113199999));
#338958=CARTESIAN_POINT('Ctrl Pts',(2.96016373299994,5.2,3.12667113199999));
#338959=CARTESIAN_POINT('Ctrl Pts',(2.96016373299994,2.2,3.12667113199999));
#338960=CARTESIAN_POINT('Ctrl Pts',(2.95851226799994,12.2,3.12591311699999));
#338961=CARTESIAN_POINT('Ctrl Pts',(2.95851226799994,5.2,3.12591311699999));
#338962=CARTESIAN_POINT('Ctrl Pts',(2.95851226799994,2.2,3.12591311699999));
#338963=CARTESIAN_POINT('Ctrl Pts',(2.95686556599994,12.2,3.12515503099998));
#338964=CARTESIAN_POINT('Ctrl Pts',(2.95686556599994,5.2,3.12515503099998));
#338965=CARTESIAN_POINT('Ctrl Pts',(2.95686556599994,2.2,3.12515503099998));
#338966=CARTESIAN_POINT('Ctrl Pts',(2.95522362999994,12.2,3.12439688599999));
#338967=CARTESIAN_POINT('Ctrl Pts',(2.95522362999994,5.2,3.12439688599999));
#338968=CARTESIAN_POINT('Ctrl Pts',(2.95522362999994,2.2,3.12439688599999));
#338969=CARTESIAN_POINT('Ctrl Pts',(2.95358646499994,12.2,3.12363869399999));
#338970=CARTESIAN_POINT('Ctrl Pts',(2.95358646499994,5.2,3.12363869399999));
#338971=CARTESIAN_POINT('Ctrl Pts',(2.95358646499994,2.2,3.12363869399999));
#338972=CARTESIAN_POINT('Ctrl Pts',(2.95195407199994,12.2,3.12288046599999));
#338973=CARTESIAN_POINT('Ctrl Pts',(2.95195407199994,5.2,3.12288046599999));
#338974=CARTESIAN_POINT('Ctrl Pts',(2.95195407199994,2.2,3.12288046599999));
#338975=CARTESIAN_POINT('Ctrl Pts',(2.95032645599994,12.2,3.12212221199999));
#338976=CARTESIAN_POINT('Ctrl Pts',(2.95032645599994,5.2,3.12212221199999));
#338977=CARTESIAN_POINT('Ctrl Pts',(2.95032645599994,2.2,3.12212221199999));
#338978=CARTESIAN_POINT('Ctrl Pts',(2.94870361999994,12.2,3.12136394499999));
#338979=CARTESIAN_POINT('Ctrl Pts',(2.94870361999994,5.2,3.12136394499999));
#338980=CARTESIAN_POINT('Ctrl Pts',(2.94870361999994,2.2,3.12136394499999));
#338981=CARTESIAN_POINT('Ctrl Pts',(2.94708556599995,12.2,3.12060567599998));
#338982=CARTESIAN_POINT('Ctrl Pts',(2.94708556599995,5.2,3.12060567599998));
#338983=CARTESIAN_POINT('Ctrl Pts',(2.94708556599995,2.2,3.12060567599998));
#338984=CARTESIAN_POINT('Ctrl Pts',(2.94547229899994,12.2,3.11984741699998));
#338985=CARTESIAN_POINT('Ctrl Pts',(2.94547229899994,5.2,3.11984741699998));
#338986=CARTESIAN_POINT('Ctrl Pts',(2.94547229899994,2.2,3.11984741699998));
#338987=CARTESIAN_POINT('Ctrl Pts',(2.94386382099994,12.2,3.11908917699999));
#338988=CARTESIAN_POINT('Ctrl Pts',(2.94386382099994,5.2,3.11908917699999));
#338989=CARTESIAN_POINT('Ctrl Pts',(2.94386382099994,2.2,3.11908917699999));
#338990=CARTESIAN_POINT('Ctrl Pts',(2.94226013599994,12.2,3.11833096999998));
#338991=CARTESIAN_POINT('Ctrl Pts',(2.94226013599994,5.2,3.11833096999998));
#338992=CARTESIAN_POINT('Ctrl Pts',(2.94226013599994,2.2,3.11833096999998));
#338993=CARTESIAN_POINT('Ctrl Pts',(2.94066124799994,12.2,3.11757280599998));
#338994=CARTESIAN_POINT('Ctrl Pts',(2.94066124799994,5.2,3.11757280599998));
#338995=CARTESIAN_POINT('Ctrl Pts',(2.94066124799994,2.2,3.11757280599998));
#338996=CARTESIAN_POINT('Ctrl Pts',(2.93906715799995,12.2,3.11681469799999));
#338997=CARTESIAN_POINT('Ctrl Pts',(2.93906715799995,5.2,3.11681469799999));
#338998=CARTESIAN_POINT('Ctrl Pts',(2.93906715799995,2.2,3.11681469799999));
#338999=CARTESIAN_POINT('Ctrl Pts',(2.93747787099994,12.2,3.11605665499999));
#339000=CARTESIAN_POINT('Ctrl Pts',(2.93747787099994,5.2,3.11605665499999));
#339001=CARTESIAN_POINT('Ctrl Pts',(2.93747787099994,2.2,3.11605665499999));
#339002=CARTESIAN_POINT('Ctrl Pts',(2.93589338999994,12.2,3.11529869099999));
#339003=CARTESIAN_POINT('Ctrl Pts',(2.93589338999994,5.2,3.11529869099999));
#339004=CARTESIAN_POINT('Ctrl Pts',(2.93589338999994,2.2,3.11529869099999));
#339005=CARTESIAN_POINT('Ctrl Pts',(2.93431371699994,12.2,3.11454081699999));
#339006=CARTESIAN_POINT('Ctrl Pts',(2.93431371699994,5.2,3.11454081699999));
#339007=CARTESIAN_POINT('Ctrl Pts',(2.93431371699994,2.2,3.11454081699999));
#339008=CARTESIAN_POINT('Ctrl Pts',(2.93273885699994,12.2,3.11378304199999));
#339009=CARTESIAN_POINT('Ctrl Pts',(2.93273885699994,5.2,3.11378304199999));
#339010=CARTESIAN_POINT('Ctrl Pts',(2.93273885699994,2.2,3.11378304199999));
#339011=CARTESIAN_POINT('Ctrl Pts',(2.93116881199994,12.2,3.11302538199998));
#339012=CARTESIAN_POINT('Ctrl Pts',(2.93116881199994,5.2,3.11302538199998));
#339013=CARTESIAN_POINT('Ctrl Pts',(2.93116881199994,2.2,3.11302538199998));
#339014=CARTESIAN_POINT('Ctrl Pts',(2.92960358599994,12.2,3.11226784599998));
#339015=CARTESIAN_POINT('Ctrl Pts',(2.92960358599994,5.2,3.11226784599998));
#339016=CARTESIAN_POINT('Ctrl Pts',(2.92960358599994,2.2,3.11226784599998));
#339017=CARTESIAN_POINT('Ctrl Pts',(2.92804318099994,12.2,3.11151044499999));
#339018=CARTESIAN_POINT('Ctrl Pts',(2.92804318099994,5.2,3.11151044499999));
#339019=CARTESIAN_POINT('Ctrl Pts',(2.92804318099994,2.2,3.11151044499999));
#339020=CARTESIAN_POINT('Ctrl Pts',(2.92648760099994,12.2,3.11075319299999));
#339021=CARTESIAN_POINT('Ctrl Pts',(2.92648760099994,5.2,3.11075319299999));
#339022=CARTESIAN_POINT('Ctrl Pts',(2.92648760099994,2.2,3.11075319299999));
#339023=CARTESIAN_POINT('Ctrl Pts',(2.92493684899994,12.2,3.10999609999998));
#339024=CARTESIAN_POINT('Ctrl Pts',(2.92493684899994,5.2,3.10999609999998));
#339025=CARTESIAN_POINT('Ctrl Pts',(2.92493684899994,2.2,3.10999609999998));
#339026=CARTESIAN_POINT('Ctrl Pts',(2.92339092799994,12.2,3.10923917799999));
#339027=CARTESIAN_POINT('Ctrl Pts',(2.92339092799994,5.2,3.10923917799999));
#339028=CARTESIAN_POINT('Ctrl Pts',(2.92339092799994,2.2,3.10923917799999));
#339029=CARTESIAN_POINT('Ctrl Pts',(2.92184984099995,12.2,3.10848243799998));
#339030=CARTESIAN_POINT('Ctrl Pts',(2.92184984099995,5.2,3.10848243799998));
#339031=CARTESIAN_POINT('Ctrl Pts',(2.92184984099995,2.2,3.10848243799998));
#339032=CARTESIAN_POINT('Ctrl Pts',(2.92031359299994,12.2,3.10772589399999));
#339033=CARTESIAN_POINT('Ctrl Pts',(2.92031359299994,5.2,3.10772589399999));
#339034=CARTESIAN_POINT('Ctrl Pts',(2.92031359299994,2.2,3.10772589399999));
#339035=CARTESIAN_POINT('Ctrl Pts',(2.91878218399995,12.2,3.10696955699999));
#339036=CARTESIAN_POINT('Ctrl Pts',(2.91878218399995,5.2,3.10696955699999));
#339037=CARTESIAN_POINT('Ctrl Pts',(2.91878218399995,2.2,3.10696955699999));
#339038=CARTESIAN_POINT('Ctrl Pts',(2.91725561899994,12.2,3.10621343799999));
#339039=CARTESIAN_POINT('Ctrl Pts',(2.91725561899994,5.2,3.10621343799999));
#339040=CARTESIAN_POINT('Ctrl Pts',(2.91725561899994,2.2,3.10621343799999));
#339041=CARTESIAN_POINT('Ctrl Pts',(2.91573389999995,12.2,3.10545754899999));
#339042=CARTESIAN_POINT('Ctrl Pts',(2.91573389999995,5.2,3.10545754899999));
#339043=CARTESIAN_POINT('Ctrl Pts',(2.91573389999995,2.2,3.10545754899999));
#339044=CARTESIAN_POINT('Ctrl Pts',(2.91421703099994,12.2,3.10470190199998));
#339045=CARTESIAN_POINT('Ctrl Pts',(2.91421703099994,5.2,3.10470190199998));
#339046=CARTESIAN_POINT('Ctrl Pts',(2.91421703099994,2.2,3.10470190199998));
#339047=CARTESIAN_POINT('Ctrl Pts',(2.91270501499994,12.2,3.10394650799999));
#339048=CARTESIAN_POINT('Ctrl Pts',(2.91270501499994,5.2,3.10394650799999));
#339049=CARTESIAN_POINT('Ctrl Pts',(2.91270501499994,2.2,3.10394650799999));
#339050=CARTESIAN_POINT('Ctrl Pts',(2.91119785499995,12.2,3.10319138199999));
#339051=CARTESIAN_POINT('Ctrl Pts',(2.91119785499995,5.2,3.10319138199999));
#339052=CARTESIAN_POINT('Ctrl Pts',(2.91119785499995,2.2,3.10319138199999));
#339053=CARTESIAN_POINT('Ctrl Pts',(2.90969555299994,12.2,3.10243653299998));
#339054=CARTESIAN_POINT('Ctrl Pts',(2.90969555299994,5.2,3.10243653299998));
#339055=CARTESIAN_POINT('Ctrl Pts',(2.90969555299994,2.2,3.10243653299998));
#339056=CARTESIAN_POINT('Ctrl Pts',(2.90819811399994,12.2,3.10168197399998));
#339057=CARTESIAN_POINT('Ctrl Pts',(2.90819811399994,5.2,3.10168197399998));
#339058=CARTESIAN_POINT('Ctrl Pts',(2.90819811399994,2.2,3.10168197399998));
#339059=CARTESIAN_POINT('Ctrl Pts',(2.90670553999994,12.2,3.10092771799999));
#339060=CARTESIAN_POINT('Ctrl Pts',(2.90670553999994,5.2,3.10092771799999));
#339061=CARTESIAN_POINT('Ctrl Pts',(2.90670553999994,2.2,3.10092771799999));
#339062=CARTESIAN_POINT('Ctrl Pts',(2.90521783399994,12.2,3.10017377499998));
#339063=CARTESIAN_POINT('Ctrl Pts',(2.90521783399994,5.2,3.10017377499998));
#339064=CARTESIAN_POINT('Ctrl Pts',(2.90521783399994,2.2,3.10017377499998));
#339065=CARTESIAN_POINT('Ctrl Pts',(2.90373499899995,12.2,3.09942015899999));
#339066=CARTESIAN_POINT('Ctrl Pts',(2.90373499899995,5.2,3.09942015899999));
#339067=CARTESIAN_POINT('Ctrl Pts',(2.90373499899995,2.2,3.09942015899999));
#339068=CARTESIAN_POINT('Ctrl Pts',(2.90225703699994,12.2,3.09866687999998));
#339069=CARTESIAN_POINT('Ctrl Pts',(2.90225703699994,5.2,3.09866687999998));
#339070=CARTESIAN_POINT('Ctrl Pts',(2.90225703699994,2.2,3.09866687999998));
#339071=CARTESIAN_POINT('Ctrl Pts',(2.90078395299994,12.2,3.09791395199999));
#339072=CARTESIAN_POINT('Ctrl Pts',(2.90078395299994,5.2,3.09791395199999));
#339073=CARTESIAN_POINT('Ctrl Pts',(2.90078395299994,2.2,3.09791395199999));
#339074=CARTESIAN_POINT('Ctrl Pts',(2.89931574799994,12.2,3.09716138599998));
#339075=CARTESIAN_POINT('Ctrl Pts',(2.89931574799994,5.2,3.09716138599998));
#339076=CARTESIAN_POINT('Ctrl Pts',(2.89931574799994,2.2,3.09716138599998));
#339077=CARTESIAN_POINT('Ctrl Pts',(2.89785242599994,12.2,3.09640919499999));
#339078=CARTESIAN_POINT('Ctrl Pts',(2.89785242599994,5.2,3.09640919499999));
#339079=CARTESIAN_POINT('Ctrl Pts',(2.89785242599994,2.2,3.09640919499999));
#339080=CARTESIAN_POINT('Ctrl Pts',(2.89639399099994,12.2,3.09565739199999));
#339081=CARTESIAN_POINT('Ctrl Pts',(2.89639399099994,5.2,3.09565739199999));
#339082=CARTESIAN_POINT('Ctrl Pts',(2.89639399099994,2.2,3.09565739199999));
#339083=CARTESIAN_POINT('Ctrl Pts',(2.89494044399994,12.2,3.09490598699998));
#339084=CARTESIAN_POINT('Ctrl Pts',(2.89494044399994,5.2,3.09490598699998));
#339085=CARTESIAN_POINT('Ctrl Pts',(2.89494044399994,2.2,3.09490598699998));
#339086=CARTESIAN_POINT('Ctrl Pts',(2.89349178899994,12.2,3.09415499399999));
#339087=CARTESIAN_POINT('Ctrl Pts',(2.89349178899994,5.2,3.09415499399999));
#339088=CARTESIAN_POINT('Ctrl Pts',(2.89349178899994,2.2,3.09415499399999));
#339089=CARTESIAN_POINT('Ctrl Pts',(2.89204802899994,12.2,3.09340442399999));
#339090=CARTESIAN_POINT('Ctrl Pts',(2.89204802899994,5.2,3.09340442399999));
#339091=CARTESIAN_POINT('Ctrl Pts',(2.89204802899994,2.2,3.09340442399999));
#339092=CARTESIAN_POINT('Ctrl Pts',(2.89060916499994,12.2,3.09265429099998));
#339093=CARTESIAN_POINT('Ctrl Pts',(2.89060916499994,5.2,3.09265429099998));
#339094=CARTESIAN_POINT('Ctrl Pts',(2.89060916499994,2.2,3.09265429099998));
#339095=CARTESIAN_POINT('Ctrl Pts',(2.88917520199994,12.2,3.09190460599999));
#339096=CARTESIAN_POINT('Ctrl Pts',(2.88917520199994,5.2,3.09190460599999));
#339097=CARTESIAN_POINT('Ctrl Pts',(2.88917520199994,2.2,3.09190460599999));
#339098=CARTESIAN_POINT('Ctrl Pts',(2.88774614299995,12.2,3.09115538099999));
#339099=CARTESIAN_POINT('Ctrl Pts',(2.88774614299995,5.2,3.09115538099999));
#339100=CARTESIAN_POINT('Ctrl Pts',(2.88774614299995,2.2,3.09115538099999));
#339101=CARTESIAN_POINT('Ctrl Pts',(2.88632198899994,12.2,3.09040662899999));
#339102=CARTESIAN_POINT('Ctrl Pts',(2.88632198899994,5.2,3.09040662899999));
#339103=CARTESIAN_POINT('Ctrl Pts',(2.88632198899994,2.2,3.09040662899999));
#339104=CARTESIAN_POINT('Ctrl Pts',(2.88490274499994,12.2,3.08965836399998));
#339105=CARTESIAN_POINT('Ctrl Pts',(2.88490274499994,5.2,3.08965836399998));
#339106=CARTESIAN_POINT('Ctrl Pts',(2.88490274499994,2.2,3.08965836399998));
#339107=CARTESIAN_POINT('Ctrl Pts',(2.88348841299995,12.2,3.08891059699998));
#339108=CARTESIAN_POINT('Ctrl Pts',(2.88348841299995,5.2,3.08891059699998));
#339109=CARTESIAN_POINT('Ctrl Pts',(2.88348841299995,2.2,3.08891059699998));
#339110=CARTESIAN_POINT('Ctrl Pts',(2.88207899499994,12.2,3.08816333899999));
#339111=CARTESIAN_POINT('Ctrl Pts',(2.88207899499994,5.2,3.08816333899999));
#339112=CARTESIAN_POINT('Ctrl Pts',(2.88207899499994,2.2,3.08816333899999));
#339113=CARTESIAN_POINT('Ctrl Pts',(2.88067449499994,12.2,3.08741660499999));
#339114=CARTESIAN_POINT('Ctrl Pts',(2.88067449499994,5.2,3.08741660499999));
#339115=CARTESIAN_POINT('Ctrl Pts',(2.88067449499994,2.2,3.08741660499999));
#339116=CARTESIAN_POINT('Ctrl Pts',(2.87927491499994,12.2,3.08667040599998));
#339117=CARTESIAN_POINT('Ctrl Pts',(2.87927491499994,5.2,3.08667040599998));
#339118=CARTESIAN_POINT('Ctrl Pts',(2.87927491499994,2.2,3.08667040599998));
#339119=CARTESIAN_POINT('Ctrl Pts',(2.87788025899995,12.2,3.08592475599998));
#339120=CARTESIAN_POINT('Ctrl Pts',(2.87788025899995,5.2,3.08592475599998));
#339121=CARTESIAN_POINT('Ctrl Pts',(2.87788025899995,2.2,3.08592475599998));
#339122=CARTESIAN_POINT('Ctrl Pts',(2.87649052899994,12.2,3.08517966499998));
#339123=CARTESIAN_POINT('Ctrl Pts',(2.87649052899994,5.2,3.08517966499998));
#339124=CARTESIAN_POINT('Ctrl Pts',(2.87649052899994,2.2,3.08517966499998));
#339125=CARTESIAN_POINT('Ctrl Pts',(2.87510572599994,12.2,3.08443514899999));
#339126=CARTESIAN_POINT('Ctrl Pts',(2.87510572599994,5.2,3.08443514899999));
#339127=CARTESIAN_POINT('Ctrl Pts',(2.87510572599994,2.2,3.08443514899999));
#339128=CARTESIAN_POINT('Ctrl Pts',(2.87372585599994,12.2,3.08369121799998));
#339129=CARTESIAN_POINT('Ctrl Pts',(2.87372585599994,5.2,3.08369121799998));
#339130=CARTESIAN_POINT('Ctrl Pts',(2.87372585599994,2.2,3.08369121799998));
#339131=CARTESIAN_POINT('Ctrl Pts',(2.87235091999994,12.2,3.08294788699998));
#339132=CARTESIAN_POINT('Ctrl Pts',(2.87235091999994,5.2,3.08294788699998));
#339133=CARTESIAN_POINT('Ctrl Pts',(2.87235091999994,2.2,3.08294788699998));
#339134=CARTESIAN_POINT('Ctrl Pts',(2.87098092099995,12.2,3.08220516599999));
#339135=CARTESIAN_POINT('Ctrl Pts',(2.87098092099995,5.2,3.08220516599999));
#339136=CARTESIAN_POINT('Ctrl Pts',(2.87098092099995,2.2,3.08220516599999));
#339137=CARTESIAN_POINT('Ctrl Pts',(2.86961586199994,12.2,3.08146307099998));
#339138=CARTESIAN_POINT('Ctrl Pts',(2.86961586199994,5.2,3.08146307099998));
#339139=CARTESIAN_POINT('Ctrl Pts',(2.86961586199994,2.2,3.08146307099998));
#339140=CARTESIAN_POINT('Ctrl Pts',(2.86825574499994,12.2,3.08072161099999));
#339141=CARTESIAN_POINT('Ctrl Pts',(2.86825574499994,5.2,3.08072161099999));
#339142=CARTESIAN_POINT('Ctrl Pts',(2.86825574499994,2.2,3.08072161099999));
#339143=CARTESIAN_POINT('Ctrl Pts',(2.86690057399994,12.2,3.07998080199999));
#339144=CARTESIAN_POINT('Ctrl Pts',(2.86690057399994,5.2,3.07998080199999));
#339145=CARTESIAN_POINT('Ctrl Pts',(2.86690057399994,2.2,3.07998080199999));
#339146=CARTESIAN_POINT('Ctrl Pts',(2.86555034999994,12.2,3.07924065399998));
#339147=CARTESIAN_POINT('Ctrl Pts',(2.86555034999994,5.2,3.07924065399998));
#339148=CARTESIAN_POINT('Ctrl Pts',(2.86555034999994,2.2,3.07924065399998));
#339149=CARTESIAN_POINT('Ctrl Pts',(2.86420507699995,12.2,3.07850118299999));
#339150=CARTESIAN_POINT('Ctrl Pts',(2.86420507699995,5.2,3.07850118299999));
#339151=CARTESIAN_POINT('Ctrl Pts',(2.86420507699995,2.2,3.07850118299999));
#339152=CARTESIAN_POINT('Ctrl Pts',(2.86286475699994,12.2,3.07776239899999));
#339153=CARTESIAN_POINT('Ctrl Pts',(2.86286475699994,5.2,3.07776239899999));
#339154=CARTESIAN_POINT('Ctrl Pts',(2.86286475699994,2.2,3.07776239899999));
#339155=CARTESIAN_POINT('Ctrl Pts',(2.86152939299994,12.2,3.07702431599999));
#339156=CARTESIAN_POINT('Ctrl Pts',(2.86152939299994,5.2,3.07702431599999));
#339157=CARTESIAN_POINT('Ctrl Pts',(2.86152939299994,2.2,3.07702431599999));
#339158=CARTESIAN_POINT('Ctrl Pts',(2.86019898699994,12.2,3.07628694799998));
#339159=CARTESIAN_POINT('Ctrl Pts',(2.86019898699994,5.2,3.07628694799998));
#339160=CARTESIAN_POINT('Ctrl Pts',(2.86019898699994,2.2,3.07628694799998));
#339161=CARTESIAN_POINT('Ctrl Pts',(2.85887354299994,12.2,3.07555030699999));
#339162=CARTESIAN_POINT('Ctrl Pts',(2.85887354299994,5.2,3.07555030699999));
#339163=CARTESIAN_POINT('Ctrl Pts',(2.85887354299994,2.2,3.07555030699999));
#339164=CARTESIAN_POINT('Ctrl Pts',(2.85755306199994,12.2,3.07481440599998));
#339165=CARTESIAN_POINT('Ctrl Pts',(2.85755306199994,5.2,3.07481440599998));
#339166=CARTESIAN_POINT('Ctrl Pts',(2.85755306199994,2.2,3.07481440599998));
#339167=CARTESIAN_POINT('Ctrl Pts',(2.85623754899994,12.2,3.07407925799998));
#339168=CARTESIAN_POINT('Ctrl Pts',(2.85623754899994,5.2,3.07407925799998));
#339169=CARTESIAN_POINT('Ctrl Pts',(2.85623754899994,2.2,3.07407925799998));
#339170=CARTESIAN_POINT('Ctrl Pts',(2.85492700399995,12.2,3.07334487499999));
#339171=CARTESIAN_POINT('Ctrl Pts',(2.85492700399995,5.2,3.07334487499999));
#339172=CARTESIAN_POINT('Ctrl Pts',(2.85492700399995,2.2,3.07334487499999));
#339173=CARTESIAN_POINT('Ctrl Pts',(2.85362142999994,12.2,3.07261127299999));
#339174=CARTESIAN_POINT('Ctrl Pts',(2.85362142999994,5.2,3.07261127299999));
#339175=CARTESIAN_POINT('Ctrl Pts',(2.85362142999994,2.2,3.07261127299999));
#339176=CARTESIAN_POINT('Ctrl Pts',(2.85232083099995,12.2,3.07187846199999));
#339177=CARTESIAN_POINT('Ctrl Pts',(2.85232083099995,5.2,3.07187846199999));
#339178=CARTESIAN_POINT('Ctrl Pts',(2.85232083099995,2.2,3.07187846199999));
#339179=CARTESIAN_POINT('Ctrl Pts',(2.85102520899994,12.2,3.07114645799999));
#339180=CARTESIAN_POINT('Ctrl Pts',(2.85102520899994,5.2,3.07114645799999));
#339181=CARTESIAN_POINT('Ctrl Pts',(2.85102520899994,2.2,3.07114645799999));
#339182=CARTESIAN_POINT('Ctrl Pts',(2.84973456599994,12.2,3.07041527099998));
#339183=CARTESIAN_POINT('Ctrl Pts',(2.84973456599994,5.2,3.07041527099998));
#339184=CARTESIAN_POINT('Ctrl Pts',(2.84973456599994,2.2,3.07041527099998));
#339185=CARTESIAN_POINT('Ctrl Pts',(2.84844890399994,12.2,3.06968491699998));
#339186=CARTESIAN_POINT('Ctrl Pts',(2.84844890399994,5.2,3.06968491699998));
#339187=CARTESIAN_POINT('Ctrl Pts',(2.84844890399994,2.2,3.06968491699998));
#339188=CARTESIAN_POINT('Ctrl Pts',(2.84716822699994,12.2,3.06895540799999));
#339189=CARTESIAN_POINT('Ctrl Pts',(2.84716822699994,5.2,3.06895540799999));
#339190=CARTESIAN_POINT('Ctrl Pts',(2.84716822699994,2.2,3.06895540799999));
#339191=CARTESIAN_POINT('Ctrl Pts',(2.84589253799994,12.2,3.06822675799998));
#339192=CARTESIAN_POINT('Ctrl Pts',(2.84589253799994,5.2,3.06822675799998));
#339193=CARTESIAN_POINT('Ctrl Pts',(2.84589253799994,2.2,3.06822675799998));
#339194=CARTESIAN_POINT('Ctrl Pts',(2.84462183699994,12.2,3.06749897899999));
#339195=CARTESIAN_POINT('Ctrl Pts',(2.84462183699994,5.2,3.06749897899999));
#339196=CARTESIAN_POINT('Ctrl Pts',(2.84462183699994,2.2,3.06749897899999));
#339197=CARTESIAN_POINT('Ctrl Pts',(2.84335612799994,12.2,3.06677208499998));
#339198=CARTESIAN_POINT('Ctrl Pts',(2.84335612799994,5.2,3.06677208499998));
#339199=CARTESIAN_POINT('Ctrl Pts',(2.84335612799994,2.2,3.06677208499998));
#339200=CARTESIAN_POINT('Ctrl Pts',(2.84209541399994,12.2,3.06604608899999));
#339201=CARTESIAN_POINT('Ctrl Pts',(2.84209541399994,5.2,3.06604608899999));
#339202=CARTESIAN_POINT('Ctrl Pts',(2.84209541399994,2.2,3.06604608899999));
#339203=CARTESIAN_POINT('Ctrl Pts',(2.84083969699994,12.2,3.06532100499999));
#339204=CARTESIAN_POINT('Ctrl Pts',(2.84083969699994,5.2,3.06532100499999));
#339205=CARTESIAN_POINT('Ctrl Pts',(2.84083969699994,2.2,3.06532100499999));
#339206=CARTESIAN_POINT('Ctrl Pts',(2.83958897899995,12.2,3.06459684699998));
#339207=CARTESIAN_POINT('Ctrl Pts',(2.83958897899995,5.2,3.06459684699998));
#339208=CARTESIAN_POINT('Ctrl Pts',(2.83958897899995,2.2,3.06459684699998));
#339209=CARTESIAN_POINT('Ctrl Pts',(2.83834326299994,12.2,3.06387362699999));
#339210=CARTESIAN_POINT('Ctrl Pts',(2.83834326299994,5.2,3.06387362699999));
#339211=CARTESIAN_POINT('Ctrl Pts',(2.83834326299994,2.2,3.06387362699999));
#339212=CARTESIAN_POINT('Ctrl Pts',(2.83710254999994,12.2,3.06315135899998));
#339213=CARTESIAN_POINT('Ctrl Pts',(2.83710254999994,5.2,3.06315135899998));
#339214=CARTESIAN_POINT('Ctrl Pts',(2.83710254999994,2.2,3.06315135899998));
#339215=CARTESIAN_POINT('Ctrl Pts',(2.83586684499994,12.2,3.06243005699999));
#339216=CARTESIAN_POINT('Ctrl Pts',(2.83586684499994,5.2,3.06243005699999));
#339217=CARTESIAN_POINT('Ctrl Pts',(2.83586684499994,2.2,3.06243005699999));
#339218=CARTESIAN_POINT('Ctrl Pts',(2.83463614899994,12.2,3.06170973399999));
#339219=CARTESIAN_POINT('Ctrl Pts',(2.83463614899994,5.2,3.06170973399999));
#339220=CARTESIAN_POINT('Ctrl Pts',(2.83463614899994,2.2,3.06170973399999));
#339221=CARTESIAN_POINT('Ctrl Pts',(2.83341046299994,12.2,3.06099040399998));
#339222=CARTESIAN_POINT('Ctrl Pts',(2.83341046299994,5.2,3.06099040399998));
#339223=CARTESIAN_POINT('Ctrl Pts',(2.83341046299994,2.2,3.06099040399998));
#339224=CARTESIAN_POINT('Ctrl Pts',(2.83218979199995,12.2,3.06027208099999));
#339225=CARTESIAN_POINT('Ctrl Pts',(2.83218979199995,5.2,3.06027208099999));
#339226=CARTESIAN_POINT('Ctrl Pts',(2.83218979199995,2.2,3.06027208099999));
#339227=CARTESIAN_POINT('Ctrl Pts',(2.83097413699994,12.2,3.05955477799999));
#339228=CARTESIAN_POINT('Ctrl Pts',(2.83097413699994,5.2,3.05955477799999));
#339229=CARTESIAN_POINT('Ctrl Pts',(2.83097413699994,2.2,3.05955477799999));
#339230=CARTESIAN_POINT('Ctrl Pts',(2.82976349999994,12.2,3.05883850699999));
#339231=CARTESIAN_POINT('Ctrl Pts',(2.82976349999994,5.2,3.05883850699999));
#339232=CARTESIAN_POINT('Ctrl Pts',(2.82976349999994,2.2,3.05883850699999));
#339233=CARTESIAN_POINT('Ctrl Pts',(2.82855788499994,12.2,3.05812328499999));
#339234=CARTESIAN_POINT('Ctrl Pts',(2.82855788499994,5.2,3.05812328499999));
#339235=CARTESIAN_POINT('Ctrl Pts',(2.82855788499994,2.2,3.05812328499999));
#339236=CARTESIAN_POINT('Ctrl Pts',(2.82735729199994,12.2,3.05740912399998));
#339237=CARTESIAN_POINT('Ctrl Pts',(2.82735729199994,5.2,3.05740912399998));
#339238=CARTESIAN_POINT('Ctrl Pts',(2.82735729199994,2.2,3.05740912399998));
#339239=CARTESIAN_POINT('Ctrl Pts',(2.82616172399994,12.2,3.05669603699998));
#339240=CARTESIAN_POINT('Ctrl Pts',(2.82616172399994,5.2,3.05669603699998));
#339241=CARTESIAN_POINT('Ctrl Pts',(2.82616172399994,2.2,3.05669603699998));
#339242=CARTESIAN_POINT('Ctrl Pts',(2.82497118399994,12.2,3.05598403999999));
#339243=CARTESIAN_POINT('Ctrl Pts',(2.82497118399994,5.2,3.05598403999999));
#339244=CARTESIAN_POINT('Ctrl Pts',(2.82497118399994,2.2,3.05598403999999));
#339245=CARTESIAN_POINT('Ctrl Pts',(2.82378567499994,12.2,3.05527314499999));
#339246=CARTESIAN_POINT('Ctrl Pts',(2.82378567499994,5.2,3.05527314499999));
#339247=CARTESIAN_POINT('Ctrl Pts',(2.82378567499994,2.2,3.05527314499999));
#339248=CARTESIAN_POINT('Ctrl Pts',(2.82260519599994,12.2,3.05456336699999));
#339249=CARTESIAN_POINT('Ctrl Pts',(2.82260519599994,5.2,3.05456336699999));
#339250=CARTESIAN_POINT('Ctrl Pts',(2.82260519599994,2.2,3.05456336699999));
#339251=CARTESIAN_POINT('Ctrl Pts',(2.82142975399994,12.2,3.05385471799998));
#339252=CARTESIAN_POINT('Ctrl Pts',(2.82142975399994,5.2,3.05385471799998));
#339253=CARTESIAN_POINT('Ctrl Pts',(2.82142975399994,2.2,3.05385471799998));
#339254=CARTESIAN_POINT('Ctrl Pts',(2.82025934699994,12.2,3.05314721399998));
#339255=CARTESIAN_POINT('Ctrl Pts',(2.82025934699994,5.2,3.05314721399998));
#339256=CARTESIAN_POINT('Ctrl Pts',(2.82025934699994,2.2,3.05314721399998));
#339257=CARTESIAN_POINT('Ctrl Pts',(2.81909397999994,12.2,3.05244086899998));
#339258=CARTESIAN_POINT('Ctrl Pts',(2.81909397999994,5.2,3.05244086899998));
#339259=CARTESIAN_POINT('Ctrl Pts',(2.81909397999994,2.2,3.05244086899998));
#339260=CARTESIAN_POINT('Ctrl Pts',(2.81793365499994,12.2,3.05173569499999));
#339261=CARTESIAN_POINT('Ctrl Pts',(2.81793365499994,5.2,3.05173569499999));
#339262=CARTESIAN_POINT('Ctrl Pts',(2.81793365499994,2.2,3.05173569499999));
#339263=CARTESIAN_POINT('Ctrl Pts',(2.81677837199994,12.2,3.05103170699999));
#339264=CARTESIAN_POINT('Ctrl Pts',(2.81677837199994,5.2,3.05103170699999));
#339265=CARTESIAN_POINT('Ctrl Pts',(2.81677837199994,2.2,3.05103170699999));
#339266=CARTESIAN_POINT('Ctrl Pts',(2.81562813499994,12.2,3.05032892099998));
#339267=CARTESIAN_POINT('Ctrl Pts',(2.81562813499994,5.2,3.05032892099998));
#339268=CARTESIAN_POINT('Ctrl Pts',(2.81562813499994,2.2,3.05032892099998));
#339269=CARTESIAN_POINT('Ctrl Pts',(2.81448294599994,12.2,3.04962734799999));
#339270=CARTESIAN_POINT('Ctrl Pts',(2.81448294599994,5.2,3.04962734799999));
#339271=CARTESIAN_POINT('Ctrl Pts',(2.81448294599994,2.2,3.04962734799999));
#339272=CARTESIAN_POINT('Ctrl Pts',(2.81334280599994,12.2,3.04892700399999));
#339273=CARTESIAN_POINT('Ctrl Pts',(2.81334280599994,5.2,3.04892700399999));
#339274=CARTESIAN_POINT('Ctrl Pts',(2.81334280599994,2.2,3.04892700399999));
#339275=CARTESIAN_POINT('Ctrl Pts',(2.81220771899994,12.2,3.04822790299998));
#339276=CARTESIAN_POINT('Ctrl Pts',(2.81220771899994,5.2,3.04822790299998));
#339277=CARTESIAN_POINT('Ctrl Pts',(2.81220771899994,2.2,3.04822790299998));
#339278=CARTESIAN_POINT('Ctrl Pts',(2.81107768699994,12.2,3.04753005899999));
#339279=CARTESIAN_POINT('Ctrl Pts',(2.81107768699994,5.2,3.04753005899999));
#339280=CARTESIAN_POINT('Ctrl Pts',(2.81107768699994,2.2,3.04753005899999));
#339281=CARTESIAN_POINT('Ctrl Pts',(2.80995270899994,12.2,3.04683348499999));
#339282=CARTESIAN_POINT('Ctrl Pts',(2.80995270899994,5.2,3.04683348499999));
#339283=CARTESIAN_POINT('Ctrl Pts',(2.80995270899994,2.2,3.04683348499999));
#339284=CARTESIAN_POINT('Ctrl Pts',(2.80883279199994,12.2,3.04613819699998));
#339285=CARTESIAN_POINT('Ctrl Pts',(2.80883279199994,5.2,3.04613819699998));
#339286=CARTESIAN_POINT('Ctrl Pts',(2.80883279199994,2.2,3.04613819699998));
#339287=CARTESIAN_POINT('Ctrl Pts',(2.80771793299994,12.2,3.04544420899998));
#339288=CARTESIAN_POINT('Ctrl Pts',(2.80771793299994,5.2,3.04544420899998));
#339289=CARTESIAN_POINT('Ctrl Pts',(2.80771793299994,2.2,3.04544420899998));
#339290=CARTESIAN_POINT('Ctrl Pts',(2.80660813799994,12.2,3.04475153399999));
#339291=CARTESIAN_POINT('Ctrl Pts',(2.80660813799994,5.2,3.04475153399999));
#339292=CARTESIAN_POINT('Ctrl Pts',(2.80660813799994,2.2,3.04475153399999));
#339293=CARTESIAN_POINT('Ctrl Pts',(2.80550340799994,12.2,3.04406018899999));
#339294=CARTESIAN_POINT('Ctrl Pts',(2.80550340799994,5.2,3.04406018899999));
#339295=CARTESIAN_POINT('Ctrl Pts',(2.80550340799994,2.2,3.04406018899999));
#339296=CARTESIAN_POINT('Ctrl Pts',(2.80440374399994,12.2,3.04337018599998));
#339297=CARTESIAN_POINT('Ctrl Pts',(2.80440374399994,5.2,3.04337018599998));
#339298=CARTESIAN_POINT('Ctrl Pts',(2.80440374399994,2.2,3.04337018599998));
#339299=CARTESIAN_POINT('Ctrl Pts',(2.80330914799995,12.2,3.04268154099999));
#339300=CARTESIAN_POINT('Ctrl Pts',(2.80330914799995,5.2,3.04268154099999));
#339301=CARTESIAN_POINT('Ctrl Pts',(2.80330914799995,2.2,3.04268154099999));
#339302=CARTESIAN_POINT('Ctrl Pts',(2.80221962399994,12.2,3.04199426699999));
#339303=CARTESIAN_POINT('Ctrl Pts',(2.80221962399994,5.2,3.04199426699999));
#339304=CARTESIAN_POINT('Ctrl Pts',(2.80221962399994,2.2,3.04199426699999));
#339305=CARTESIAN_POINT('Ctrl Pts',(2.80113517299994,12.2,3.04130837799998));
#339306=CARTESIAN_POINT('Ctrl Pts',(2.80113517299994,5.2,3.04130837799998));
#339307=CARTESIAN_POINT('Ctrl Pts',(2.80113517299994,2.2,3.04130837799998));
#339308=CARTESIAN_POINT('Ctrl Pts',(2.80005579499994,12.2,3.04062389199999));
#339309=CARTESIAN_POINT('Ctrl Pts',(2.80005579499994,5.2,3.04062389199999));
#339310=CARTESIAN_POINT('Ctrl Pts',(2.80005579499994,2.2,3.04062389199999));
#339311=CARTESIAN_POINT('Ctrl Pts',(2.79898149599994,12.2,3.03994081999999));
#339312=CARTESIAN_POINT('Ctrl Pts',(2.79898149599994,5.2,3.03994081999999));
#339313=CARTESIAN_POINT('Ctrl Pts',(2.79898149599994,2.2,3.03994081999999));
#339314=CARTESIAN_POINT('Ctrl Pts',(2.79791227399994,12.2,3.03925917799998));
#339315=CARTESIAN_POINT('Ctrl Pts',(2.79791227399994,5.2,3.03925917799998));
#339316=CARTESIAN_POINT('Ctrl Pts',(2.79791227399994,2.2,3.03925917799998));
#339317=CARTESIAN_POINT('Ctrl Pts',(2.79684813299995,12.2,3.03857898099999));
#339318=CARTESIAN_POINT('Ctrl Pts',(2.79684813299995,5.2,3.03857898099999));
#339319=CARTESIAN_POINT('Ctrl Pts',(2.79684813299995,2.2,3.03857898099999));
#339320=CARTESIAN_POINT('Ctrl Pts',(2.79578907399994,12.2,3.03790024299998));
#339321=CARTESIAN_POINT('Ctrl Pts',(2.79578907399994,5.2,3.03790024299998));
#339322=CARTESIAN_POINT('Ctrl Pts',(2.79578907399994,2.2,3.03790024299998));
#339323=CARTESIAN_POINT('Ctrl Pts',(2.79473510099994,12.2,3.03722297899998));
#339324=CARTESIAN_POINT('Ctrl Pts',(2.79473510099994,5.2,3.03722297899998));
#339325=CARTESIAN_POINT('Ctrl Pts',(2.79473510099994,2.2,3.03722297899998));
#339326=CARTESIAN_POINT('Ctrl Pts',(2.79368621299994,12.2,3.03654720399999));
#339327=CARTESIAN_POINT('Ctrl Pts',(2.79368621299994,5.2,3.03654720399999));
#339328=CARTESIAN_POINT('Ctrl Pts',(2.79368621299994,2.2,3.03654720399999));
#339329=CARTESIAN_POINT('Ctrl Pts',(2.79264241399994,12.2,3.03587293199998));
#339330=CARTESIAN_POINT('Ctrl Pts',(2.79264241399994,5.2,3.03587293199998));
#339331=CARTESIAN_POINT('Ctrl Pts',(2.79264241399994,2.2,3.03587293199998));
#339332=CARTESIAN_POINT('Ctrl Pts',(2.79160370399994,12.2,3.03520017899999));
#339333=CARTESIAN_POINT('Ctrl Pts',(2.79160370399994,5.2,3.03520017899999));
#339334=CARTESIAN_POINT('Ctrl Pts',(2.79160370399994,2.2,3.03520017899999));
#339335=CARTESIAN_POINT('Ctrl Pts',(2.79057008599994,12.2,3.03452895899999));
#339336=CARTESIAN_POINT('Ctrl Pts',(2.79057008599994,5.2,3.03452895899999));
#339337=CARTESIAN_POINT('Ctrl Pts',(2.79057008599994,2.2,3.03452895899999));
#339338=CARTESIAN_POINT('Ctrl Pts',(2.78954156299994,12.2,3.03385928599998));
#339339=CARTESIAN_POINT('Ctrl Pts',(2.78954156299994,5.2,3.03385928599998));
#339340=CARTESIAN_POINT('Ctrl Pts',(2.78954156299994,2.2,3.03385928599998));
#339341=CARTESIAN_POINT('Ctrl Pts',(2.78851813399994,12.2,3.03319117699999));
#339342=CARTESIAN_POINT('Ctrl Pts',(2.78851813399994,5.2,3.03319117699999));
#339343=CARTESIAN_POINT('Ctrl Pts',(2.78851813399994,2.2,3.03319117699999));
#339344=CARTESIAN_POINT('Ctrl Pts',(2.78749980299994,12.2,3.03252464699998));
#339345=CARTESIAN_POINT('Ctrl Pts',(2.78749980299994,5.2,3.03252464699998));
#339346=CARTESIAN_POINT('Ctrl Pts',(2.78749980299994,2.2,3.03252464699998));
#339347=CARTESIAN_POINT('Ctrl Pts',(2.78648657199994,12.2,3.03185970799999));
#339348=CARTESIAN_POINT('Ctrl Pts',(2.78648657199994,5.2,3.03185970799999));
#339349=CARTESIAN_POINT('Ctrl Pts',(2.78648657199994,2.2,3.03185970799999));
#339350=CARTESIAN_POINT('Ctrl Pts',(2.78547844199994,12.2,3.03119637799998));
#339351=CARTESIAN_POINT('Ctrl Pts',(2.78547844199994,5.2,3.03119637799998));
#339352=CARTESIAN_POINT('Ctrl Pts',(2.78547844199994,2.2,3.03119637799998));
#339353=CARTESIAN_POINT('Ctrl Pts',(2.78447541399995,12.2,3.03053467099998));
#339354=CARTESIAN_POINT('Ctrl Pts',(2.78447541399995,5.2,3.03053467099998));
#339355=CARTESIAN_POINT('Ctrl Pts',(2.78447541399995,2.2,3.03053467099998));
#339356=CARTESIAN_POINT('Ctrl Pts',(2.78347749099995,12.2,3.02987460199999));
#339357=CARTESIAN_POINT('Ctrl Pts',(2.78347749099995,5.2,3.02987460199999));
#339358=CARTESIAN_POINT('Ctrl Pts',(2.78347749099995,2.2,3.02987460199999));
#339359=CARTESIAN_POINT('Ctrl Pts',(2.78248467399994,12.2,3.02921618799999));
#339360=CARTESIAN_POINT('Ctrl Pts',(2.78248467399994,5.2,3.02921618799999));
#339361=CARTESIAN_POINT('Ctrl Pts',(2.78248467399994,2.2,3.02921618799999));
#339362=CARTESIAN_POINT('Ctrl Pts',(2.78149696399994,12.2,3.02855943999998));
#339363=CARTESIAN_POINT('Ctrl Pts',(2.78149696399994,5.2,3.02855943999998));
#339364=CARTESIAN_POINT('Ctrl Pts',(2.78149696399994,2.2,3.02855943999998));
#339365=CARTESIAN_POINT('Ctrl Pts',(2.78051436499994,12.2,3.02790437799998));
#339366=CARTESIAN_POINT('Ctrl Pts',(2.78051436499994,5.2,3.02790437799998));
#339367=CARTESIAN_POINT('Ctrl Pts',(2.78051436499994,2.2,3.02790437799998));
#339368=CARTESIAN_POINT('Ctrl Pts',(2.77953687699994,12.2,3.02725101399999));
#339369=CARTESIAN_POINT('Ctrl Pts',(2.77953687699994,5.2,3.02725101399999));
#339370=CARTESIAN_POINT('Ctrl Pts',(2.77953687699994,2.2,3.02725101399999));
#339371=CARTESIAN_POINT('Ctrl Pts',(2.77856450199994,12.2,3.02659936399999));
#339372=CARTESIAN_POINT('Ctrl Pts',(2.77856450199994,5.2,3.02659936399999));
#339373=CARTESIAN_POINT('Ctrl Pts',(2.77856450199994,2.2,3.02659936399999));
#339374=CARTESIAN_POINT('Ctrl Pts',(2.77759723999994,12.2,3.02594944399999));
#339375=CARTESIAN_POINT('Ctrl Pts',(2.77759723999994,5.2,3.02594944399999));
#339376=CARTESIAN_POINT('Ctrl Pts',(2.77759723999994,2.2,3.02594944399999));
#339377=CARTESIAN_POINT('Ctrl Pts',(2.77663509599994,12.2,3.02530126999999));
#339378=CARTESIAN_POINT('Ctrl Pts',(2.77663509599994,5.2,3.02530126999999));
#339379=CARTESIAN_POINT('Ctrl Pts',(2.77663509599994,2.2,3.02530126999999));
#339380=CARTESIAN_POINT('Ctrl Pts',(2.77567806899994,12.2,3.02465485599999));
#339381=CARTESIAN_POINT('Ctrl Pts',(2.77567806899994,5.2,3.02465485599999));
#339382=CARTESIAN_POINT('Ctrl Pts',(2.77567806899994,2.2,3.02465485599999));
#339383=CARTESIAN_POINT('Ctrl Pts',(2.77472616299994,12.2,3.02401021799999));
#339384=CARTESIAN_POINT('Ctrl Pts',(2.77472616299994,5.2,3.02401021799999));
#339385=CARTESIAN_POINT('Ctrl Pts',(2.77472616299994,2.2,3.02401021799999));
#339386=CARTESIAN_POINT('Ctrl Pts',(2.77377937599995,12.2,3.02336737099999));
#339387=CARTESIAN_POINT('Ctrl Pts',(2.77377937599995,5.2,3.02336737099999));
#339388=CARTESIAN_POINT('Ctrl Pts',(2.77377937599995,2.2,3.02336737099999));
#339389=CARTESIAN_POINT('Ctrl Pts',(2.77283771299994,12.2,3.02272633199999));
#339390=CARTESIAN_POINT('Ctrl Pts',(2.77283771299994,5.2,3.02272633199999));
#339391=CARTESIAN_POINT('Ctrl Pts',(2.77283771299994,2.2,3.02272633199999));
#339392=CARTESIAN_POINT('Ctrl Pts',(2.77190117299994,12.2,3.02208711399999));
#339393=CARTESIAN_POINT('Ctrl Pts',(2.77190117299994,5.2,3.02208711399999));
#339394=CARTESIAN_POINT('Ctrl Pts',(2.77190117299994,2.2,3.02208711399999));
#339395=CARTESIAN_POINT('Ctrl Pts',(2.77096975999994,12.2,3.02144973499999));
#339396=CARTESIAN_POINT('Ctrl Pts',(2.77096975999994,5.2,3.02144973499999));
#339397=CARTESIAN_POINT('Ctrl Pts',(2.77096975999994,2.2,3.02144973499999));
#339398=CARTESIAN_POINT('Ctrl Pts',(2.77004347399994,12.2,3.02081421099999));
#339399=CARTESIAN_POINT('Ctrl Pts',(2.77004347399994,5.2,3.02081421099999));
#339400=CARTESIAN_POINT('Ctrl Pts',(2.77004347399994,2.2,3.02081421099999));
#339401=CARTESIAN_POINT('Ctrl Pts',(2.76912231599994,12.2,3.02018055499998));
#339402=CARTESIAN_POINT('Ctrl Pts',(2.76912231599994,5.2,3.02018055499998));
#339403=CARTESIAN_POINT('Ctrl Pts',(2.76912231599994,2.2,3.02018055499998));
#339404=CARTESIAN_POINT('Ctrl Pts',(2.76820628899995,12.2,3.01954878399999));
#339405=CARTESIAN_POINT('Ctrl Pts',(2.76820628899995,5.2,3.01954878399999));
#339406=CARTESIAN_POINT('Ctrl Pts',(2.76820628899995,2.2,3.01954878399999));
#339407=CARTESIAN_POINT('Ctrl Pts',(2.76729539299994,12.2,3.01891891499999));
#339408=CARTESIAN_POINT('Ctrl Pts',(2.76729539299994,5.2,3.01891891499999));
#339409=CARTESIAN_POINT('Ctrl Pts',(2.76729539299994,2.2,3.01891891499999));
#339410=CARTESIAN_POINT('Ctrl Pts',(2.76638963099994,12.2,3.01829096199998));
#339411=CARTESIAN_POINT('Ctrl Pts',(2.76638963099994,5.2,3.01829096199998));
#339412=CARTESIAN_POINT('Ctrl Pts',(2.76638963099994,2.2,3.01829096199998));
#339413=CARTESIAN_POINT('Ctrl Pts',(2.76548900299994,12.2,3.01766494299999));
#339414=CARTESIAN_POINT('Ctrl Pts',(2.76548900299994,5.2,3.01766494299999));
#339415=CARTESIAN_POINT('Ctrl Pts',(2.76548900299994,2.2,3.01766494299999));
#339416=CARTESIAN_POINT('Ctrl Pts',(2.76459351099994,12.2,3.01704087099999));
#339417=CARTESIAN_POINT('Ctrl Pts',(2.76459351099994,5.2,3.01704087099999));
#339418=CARTESIAN_POINT('Ctrl Pts',(2.76459351099994,2.2,3.01704087099999));
#339419=CARTESIAN_POINT('Ctrl Pts',(2.76370315599994,12.2,3.01641876399999));
#339420=CARTESIAN_POINT('Ctrl Pts',(2.76370315599994,5.2,3.01641876399999));
#339421=CARTESIAN_POINT('Ctrl Pts',(2.76370315599994,2.2,3.01641876399999));
#339422=CARTESIAN_POINT('Ctrl Pts',(2.76281793999994,12.2,3.01579863699998));
#339423=CARTESIAN_POINT('Ctrl Pts',(2.76281793999994,5.2,3.01579863699998));
#339424=CARTESIAN_POINT('Ctrl Pts',(2.76281793999994,2.2,3.01579863699998));
#339425=CARTESIAN_POINT('Ctrl Pts',(2.76193786499995,12.2,3.01518050799999));
#339426=CARTESIAN_POINT('Ctrl Pts',(2.76193786499995,5.2,3.01518050799999));
#339427=CARTESIAN_POINT('Ctrl Pts',(2.76193786499995,2.2,3.01518050799999));
#339428=CARTESIAN_POINT('Ctrl Pts',(2.76106292999994,12.2,3.01456438999999));
#339429=CARTESIAN_POINT('Ctrl Pts',(2.76106292999994,5.2,3.01456438999999));
#339430=CARTESIAN_POINT('Ctrl Pts',(2.76106292999994,2.2,3.01456438999999));
#339431=CARTESIAN_POINT('Ctrl Pts',(2.76019313899994,12.2,3.01395030099999));
#339432=CARTESIAN_POINT('Ctrl Pts',(2.76019313899994,5.2,3.01395030099999));
#339433=CARTESIAN_POINT('Ctrl Pts',(2.76019313899994,2.2,3.01395030099999));
#339434=CARTESIAN_POINT('Ctrl Pts',(2.75932849199994,12.2,3.01333825799999));
#339435=CARTESIAN_POINT('Ctrl Pts',(2.75932849199994,5.2,3.01333825799999));
#339436=CARTESIAN_POINT('Ctrl Pts',(2.75932849199994,2.2,3.01333825799999));
#339437=CARTESIAN_POINT('Ctrl Pts',(2.75846898999994,12.2,3.01272827399998));
#339438=CARTESIAN_POINT('Ctrl Pts',(2.75846898999994,5.2,3.01272827399998));
#339439=CARTESIAN_POINT('Ctrl Pts',(2.75846898999994,2.2,3.01272827399998));
#339440=CARTESIAN_POINT('Ctrl Pts',(2.75761463499994,12.2,3.01212036899998));
#339441=CARTESIAN_POINT('Ctrl Pts',(2.75761463499994,5.2,3.01212036899998));
#339442=CARTESIAN_POINT('Ctrl Pts',(2.75761463499994,2.2,3.01212036899998));
#339443=CARTESIAN_POINT('Ctrl Pts',(2.75676542799994,12.2,3.01151455599998));
#339444=CARTESIAN_POINT('Ctrl Pts',(2.75676542799994,5.2,3.01151455599998));
#339445=CARTESIAN_POINT('Ctrl Pts',(2.75676542799994,2.2,3.01151455599998));
#339446=CARTESIAN_POINT('Ctrl Pts',(2.75592137099995,12.2,3.01091085199998));
#339447=CARTESIAN_POINT('Ctrl Pts',(2.75592137099995,5.2,3.01091085199998));
#339448=CARTESIAN_POINT('Ctrl Pts',(2.75592137099995,2.2,3.01091085199998));
#339449=CARTESIAN_POINT('Ctrl Pts',(2.75508246399994,12.2,3.01030927599999));
#339450=CARTESIAN_POINT('Ctrl Pts',(2.75508246399994,5.2,3.01030927599999));
#339451=CARTESIAN_POINT('Ctrl Pts',(2.75508246399994,2.2,3.01030927599999));
#339452=CARTESIAN_POINT('Ctrl Pts',(2.75424870799994,12.2,3.00970984099998));
#339453=CARTESIAN_POINT('Ctrl Pts',(2.75424870799994,5.2,3.00970984099998));
#339454=CARTESIAN_POINT('Ctrl Pts',(2.75424870799994,2.2,3.00970984099998));
#339455=CARTESIAN_POINT('Ctrl Pts',(2.75342010599994,12.2,3.00911256499998));
#339456=CARTESIAN_POINT('Ctrl Pts',(2.75342010599994,5.2,3.00911256499998));
#339457=CARTESIAN_POINT('Ctrl Pts',(2.75342010599994,2.2,3.00911256499998));
#339458=CARTESIAN_POINT('Ctrl Pts',(2.75259665699994,12.2,3.00851746499998));
#339459=CARTESIAN_POINT('Ctrl Pts',(2.75259665699994,5.2,3.00851746499998));
#339460=CARTESIAN_POINT('Ctrl Pts',(2.75259665699994,2.2,3.00851746499998));
#339461=CARTESIAN_POINT('Ctrl Pts',(2.75177836299994,12.2,3.00792455699998));
#339462=CARTESIAN_POINT('Ctrl Pts',(2.75177836299994,5.2,3.00792455699998));
#339463=CARTESIAN_POINT('Ctrl Pts',(2.75177836299994,2.2,3.00792455699998));
#339464=CARTESIAN_POINT('Ctrl Pts',(2.75096522599994,12.2,3.00733385699999));
#339465=CARTESIAN_POINT('Ctrl Pts',(2.75096522599994,5.2,3.00733385699999));
#339466=CARTESIAN_POINT('Ctrl Pts',(2.75096522599994,2.2,3.00733385699999));
#339467=CARTESIAN_POINT('Ctrl Pts',(2.75015724699994,12.2,3.00674538099998));
#339468=CARTESIAN_POINT('Ctrl Pts',(2.75015724699994,5.2,3.00674538099998));
#339469=CARTESIAN_POINT('Ctrl Pts',(2.75015724699994,2.2,3.00674538099998));
#339470=CARTESIAN_POINT('Ctrl Pts',(2.74935442599994,12.2,3.00615914699998));
#339471=CARTESIAN_POINT('Ctrl Pts',(2.74935442599994,5.2,3.00615914699998));
#339472=CARTESIAN_POINT('Ctrl Pts',(2.74935442599994,2.2,3.00615914699998));
#339473=CARTESIAN_POINT('Ctrl Pts',(2.74855676399994,12.2,3.00557517099998));
#339474=CARTESIAN_POINT('Ctrl Pts',(2.74855676399994,5.2,3.00557517099998));
#339475=CARTESIAN_POINT('Ctrl Pts',(2.74855676399994,2.2,3.00557517099998));
#339476=CARTESIAN_POINT('Ctrl Pts',(2.74776426299994,12.2,3.00499347099999));
#339477=CARTESIAN_POINT('Ctrl Pts',(2.74776426299994,5.2,3.00499347099999));
#339478=CARTESIAN_POINT('Ctrl Pts',(2.74776426299994,2.2,3.00499347099999));
#339479=CARTESIAN_POINT('Ctrl Pts',(2.74697692399994,12.2,3.00441406299999));
#339480=CARTESIAN_POINT('Ctrl Pts',(2.74697692399994,5.2,3.00441406299999));
#339481=CARTESIAN_POINT('Ctrl Pts',(2.74697692399994,2.2,3.00441406299999));
#339482=CARTESIAN_POINT('Ctrl Pts',(2.74619474799994,12.2,3.00383696199999));
#339483=CARTESIAN_POINT('Ctrl Pts',(2.74619474799994,5.2,3.00383696199999));
#339484=CARTESIAN_POINT('Ctrl Pts',(2.74619474799994,2.2,3.00383696199999));
#339485=CARTESIAN_POINT('Ctrl Pts',(2.74541773599994,12.2,3.00326218699999));
#339486=CARTESIAN_POINT('Ctrl Pts',(2.74541773599994,5.2,3.00326218699999));
#339487=CARTESIAN_POINT('Ctrl Pts',(2.74541773599994,2.2,3.00326218699999));
#339488=CARTESIAN_POINT('Ctrl Pts',(2.74464588799994,12.2,3.00268975499999));
#339489=CARTESIAN_POINT('Ctrl Pts',(2.74464588799994,5.2,3.00268975499999));
#339490=CARTESIAN_POINT('Ctrl Pts',(2.74464588799994,2.2,3.00268975499999));
#339491=CARTESIAN_POINT('Ctrl Pts',(2.74387920599994,12.2,3.00211968199999));
#339492=CARTESIAN_POINT('Ctrl Pts',(2.74387920599994,5.2,3.00211968199999));
#339493=CARTESIAN_POINT('Ctrl Pts',(2.74387920599994,2.2,3.00211968199999));
#339494=CARTESIAN_POINT('Ctrl Pts',(2.74311768999994,12.2,3.00155198599998));
#339495=CARTESIAN_POINT('Ctrl Pts',(2.74311768999994,5.2,3.00155198599998));
#339496=CARTESIAN_POINT('Ctrl Pts',(2.74311768999994,2.2,3.00155198599998));
#339497=CARTESIAN_POINT('Ctrl Pts',(2.74236134299994,12.2,3.00098668199999));
#339498=CARTESIAN_POINT('Ctrl Pts',(2.74236134299994,5.2,3.00098668199999));
#339499=CARTESIAN_POINT('Ctrl Pts',(2.74236134299994,2.2,3.00098668199999));
#339500=CARTESIAN_POINT('Ctrl Pts',(2.74161016399994,12.2,3.00042378899998));
#339501=CARTESIAN_POINT('Ctrl Pts',(2.74161016399994,5.2,3.00042378899998));
#339502=CARTESIAN_POINT('Ctrl Pts',(2.74161016399994,2.2,3.00042378899998));
#339503=CARTESIAN_POINT('Ctrl Pts',(2.74086415499994,12.2,2.99986332399998));
#339504=CARTESIAN_POINT('Ctrl Pts',(2.74086415499994,5.2,2.99986332399998));
#339505=CARTESIAN_POINT('Ctrl Pts',(2.74086415499994,2.2,2.99986332399998));
#339506=CARTESIAN_POINT('Ctrl Pts',(2.74012331499994,12.2,2.99930530299999));
#339507=CARTESIAN_POINT('Ctrl Pts',(2.74012331499994,5.2,2.99930530299999));
#339508=CARTESIAN_POINT('Ctrl Pts',(2.74012331499994,2.2,2.99930530299999));
#339509=CARTESIAN_POINT('Ctrl Pts',(2.73938764699994,12.2,2.99874974399999));
#339510=CARTESIAN_POINT('Ctrl Pts',(2.73938764699994,5.2,2.99874974399999));
#339511=CARTESIAN_POINT('Ctrl Pts',(2.73938764699994,2.2,2.99874974399999));
#339512=CARTESIAN_POINT('Ctrl Pts',(2.73865715199994,12.2,2.99819666399999));
#339513=CARTESIAN_POINT('Ctrl Pts',(2.73865715199994,5.2,2.99819666399999));
#339514=CARTESIAN_POINT('Ctrl Pts',(2.73865715199994,2.2,2.99819666399999));
#339515=CARTESIAN_POINT('Ctrl Pts',(2.73793182799994,12.2,2.99764608099998));
#339516=CARTESIAN_POINT('Ctrl Pts',(2.73793182799994,5.2,2.99764608099998));
#339517=CARTESIAN_POINT('Ctrl Pts',(2.73793182799994,2.2,2.99764608099998));
#339518=CARTESIAN_POINT('Ctrl Pts',(2.73721167799994,12.2,2.99709801099999));
#339519=CARTESIAN_POINT('Ctrl Pts',(2.73721167799994,5.2,2.99709801099999));
#339520=CARTESIAN_POINT('Ctrl Pts',(2.73721167799994,2.2,2.99709801099999));
#339521=CARTESIAN_POINT('Ctrl Pts',(2.73649670299994,12.2,2.99655247299999));
#339522=CARTESIAN_POINT('Ctrl Pts',(2.73649670299994,5.2,2.99655247299999));
#339523=CARTESIAN_POINT('Ctrl Pts',(2.73649670299994,2.2,2.99655247299999));
#339524=CARTESIAN_POINT('Ctrl Pts',(2.73578690299995,12.2,2.99600948399998));
#339525=CARTESIAN_POINT('Ctrl Pts',(2.73578690299995,5.2,2.99600948399998));
#339526=CARTESIAN_POINT('Ctrl Pts',(2.73578690299995,2.2,2.99600948399998));
#339527=CARTESIAN_POINT('Ctrl Pts',(2.73508227899995,12.2,2.99546906099999));
#339528=CARTESIAN_POINT('Ctrl Pts',(2.73508227899995,5.2,2.99546906099999));
#339529=CARTESIAN_POINT('Ctrl Pts',(2.73508227899995,2.2,2.99546906099999));
#339530=CARTESIAN_POINT('Ctrl Pts',(2.73438283199994,12.2,2.99493122099998));
#339531=CARTESIAN_POINT('Ctrl Pts',(2.73438283199994,5.2,2.99493122099998));
#339532=CARTESIAN_POINT('Ctrl Pts',(2.73438283199994,2.2,2.99493122099998));
#339533=CARTESIAN_POINT('Ctrl Pts',(2.73368856099995,12.2,2.99439598299998));
#339534=CARTESIAN_POINT('Ctrl Pts',(2.73368856099995,5.2,2.99439598299998));
#339535=CARTESIAN_POINT('Ctrl Pts',(2.73368856099995,2.2,2.99439598299998));
#339536=CARTESIAN_POINT('Ctrl Pts',(2.73299946899995,12.2,2.99386336399999));
#339537=CARTESIAN_POINT('Ctrl Pts',(2.73299946899995,5.2,2.99386336399999));
#339538=CARTESIAN_POINT('Ctrl Pts',(2.73299946899995,2.2,2.99386336399999));
#339539=CARTESIAN_POINT('Ctrl Pts',(2.73231555499994,12.2,2.99333338199999));
#339540=CARTESIAN_POINT('Ctrl Pts',(2.73231555499994,5.2,2.99333338199999));
#339541=CARTESIAN_POINT('Ctrl Pts',(2.73231555499994,2.2,2.99333338199999));
#339542=CARTESIAN_POINT('Ctrl Pts',(2.73163682099994,12.2,2.99280605399999));
#339543=CARTESIAN_POINT('Ctrl Pts',(2.73163682099994,5.2,2.99280605399999));
#339544=CARTESIAN_POINT('Ctrl Pts',(2.73163682099994,2.2,2.99280605399999));
#339545=CARTESIAN_POINT('Ctrl Pts',(2.73096326699994,12.2,2.99228139699999));
#339546=CARTESIAN_POINT('Ctrl Pts',(2.73096326699994,5.2,2.99228139699999));
#339547=CARTESIAN_POINT('Ctrl Pts',(2.73096326699994,2.2,2.99228139699999));
#339548=CARTESIAN_POINT('Ctrl Pts',(2.73029489299994,12.2,2.99175943199998));
#339549=CARTESIAN_POINT('Ctrl Pts',(2.73029489299994,5.2,2.99175943199998));
#339550=CARTESIAN_POINT('Ctrl Pts',(2.73029489299994,2.2,2.99175943199998));
#339551=CARTESIAN_POINT('Ctrl Pts',(2.72963169999994,12.2,2.99124017399999));
#339552=CARTESIAN_POINT('Ctrl Pts',(2.72963169999994,5.2,2.99124017399999));
#339553=CARTESIAN_POINT('Ctrl Pts',(2.72963169999994,2.2,2.99124017399999));
#339554=CARTESIAN_POINT('Ctrl Pts',(2.72897368899994,12.2,2.99072364099998));
#339555=CARTESIAN_POINT('Ctrl Pts',(2.72897368899994,5.2,2.99072364099998));
#339556=CARTESIAN_POINT('Ctrl Pts',(2.72897368899994,2.2,2.99072364099998));
#339557=CARTESIAN_POINT('Ctrl Pts',(2.72832085899994,12.2,2.99020985299999));
#339558=CARTESIAN_POINT('Ctrl Pts',(2.72832085899994,5.2,2.99020985299999));
#339559=CARTESIAN_POINT('Ctrl Pts',(2.72832085899994,2.2,2.99020985299999));
#339560=CARTESIAN_POINT('Ctrl Pts',(2.72767321299995,12.2,2.98969882599998));
#339561=CARTESIAN_POINT('Ctrl Pts',(2.72767321299995,5.2,2.98969882599998));
#339562=CARTESIAN_POINT('Ctrl Pts',(2.72767321299995,2.2,2.98969882599998));
#339563=CARTESIAN_POINT('Ctrl Pts',(2.72703074999994,12.2,2.98919057999999));
#339564=CARTESIAN_POINT('Ctrl Pts',(2.72703074999994,5.2,2.98919057999999));
#339565=CARTESIAN_POINT('Ctrl Pts',(2.72703074999994,2.2,2.98919057999999));
#339566=CARTESIAN_POINT('Ctrl Pts',(2.72639347099994,12.2,2.98868513199999));
#339567=CARTESIAN_POINT('Ctrl Pts',(2.72639347099994,5.2,2.98868513199999));
#339568=CARTESIAN_POINT('Ctrl Pts',(2.72639347099994,2.2,2.98868513199999));
#339569=CARTESIAN_POINT('Ctrl Pts',(2.72576137499994,12.2,2.98818249999999));
#339570=CARTESIAN_POINT('Ctrl Pts',(2.72576137499994,5.2,2.98818249999999));
#339571=CARTESIAN_POINT('Ctrl Pts',(2.72576137499994,2.2,2.98818249999999));
#339572=CARTESIAN_POINT('Ctrl Pts',(2.72513446399994,12.2,2.98768270099998));
#339573=CARTESIAN_POINT('Ctrl Pts',(2.72513446399994,5.2,2.98768270099998));
#339574=CARTESIAN_POINT('Ctrl Pts',(2.72513446399994,2.2,2.98768270099998));
#339575=CARTESIAN_POINT('Ctrl Pts',(2.72451273799994,12.2,2.98718575599998));
#339576=CARTESIAN_POINT('Ctrl Pts',(2.72451273799994,5.2,2.98718575599998));
#339577=CARTESIAN_POINT('Ctrl Pts',(2.72451273799994,2.2,2.98718575599998));
#339578=CARTESIAN_POINT('Ctrl Pts',(2.72389619799994,12.2,2.98669168199999));
#339579=CARTESIAN_POINT('Ctrl Pts',(2.72389619799994,5.2,2.98669168199999));
#339580=CARTESIAN_POINT('Ctrl Pts',(2.72389619799994,2.2,2.98669168199999));
#339581=CARTESIAN_POINT('Ctrl Pts',(2.72328484299994,12.2,2.98620049699998));
#339582=CARTESIAN_POINT('Ctrl Pts',(2.72328484299994,5.2,2.98620049699998));
#339583=CARTESIAN_POINT('Ctrl Pts',(2.72328484299994,2.2,2.98620049699998));
#339584=CARTESIAN_POINT('Ctrl Pts',(2.72267867399994,12.2,2.98571222099999));
#339585=CARTESIAN_POINT('Ctrl Pts',(2.72267867399994,5.2,2.98571222099999));
#339586=CARTESIAN_POINT('Ctrl Pts',(2.72267867399994,2.2,2.98571222099999));
#339587=CARTESIAN_POINT('Ctrl Pts',(2.72207768999994,12.2,2.98522686999998));
#339588=CARTESIAN_POINT('Ctrl Pts',(2.72207768999994,5.2,2.98522686999998));
#339589=CARTESIAN_POINT('Ctrl Pts',(2.72207768999994,2.2,2.98522686999998));
#339590=CARTESIAN_POINT('Ctrl Pts',(2.72148189399994,12.2,2.98474446399998));
#339591=CARTESIAN_POINT('Ctrl Pts',(2.72148189399994,5.2,2.98474446399998));
#339592=CARTESIAN_POINT('Ctrl Pts',(2.72148189399994,2.2,2.98474446399998));
#339593=CARTESIAN_POINT('Ctrl Pts',(2.72089128599994,12.2,2.98426502199998));
#339594=CARTESIAN_POINT('Ctrl Pts',(2.72089128599994,5.2,2.98426502199998));
#339595=CARTESIAN_POINT('Ctrl Pts',(2.72089128599994,2.2,2.98426502199998));
#339596=CARTESIAN_POINT('Ctrl Pts',(2.72030586299994,12.2,2.98378856299998));
#339597=CARTESIAN_POINT('Ctrl Pts',(2.72030586299994,5.2,2.98378856299998));
#339598=CARTESIAN_POINT('Ctrl Pts',(2.72030586299994,2.2,2.98378856299998));
#339599=CARTESIAN_POINT('Ctrl Pts',(2.71972562899994,12.2,2.98331510299998));
#339600=CARTESIAN_POINT('Ctrl Pts',(2.71972562899994,5.2,2.98331510299998));
#339601=CARTESIAN_POINT('Ctrl Pts',(2.71972562899994,2.2,2.98331510299998));
#339602=CARTESIAN_POINT('Ctrl Pts',(2.71915058199995,12.2,2.98284466299998));
#339603=CARTESIAN_POINT('Ctrl Pts',(2.71915058199995,5.2,2.98284466299998));
#339604=CARTESIAN_POINT('Ctrl Pts',(2.71915058199995,2.2,2.98284466299998));
#339605=CARTESIAN_POINT('Ctrl Pts',(2.71858072299994,12.2,2.98237726199999));
#339606=CARTESIAN_POINT('Ctrl Pts',(2.71858072299994,5.2,2.98237726199999));
#339607=CARTESIAN_POINT('Ctrl Pts',(2.71858072299994,2.2,2.98237726199999));
#339608=CARTESIAN_POINT('Ctrl Pts',(2.71801605199995,12.2,2.98191291799998));
#339609=CARTESIAN_POINT('Ctrl Pts',(2.71801605199995,5.2,2.98191291799998));
#339610=CARTESIAN_POINT('Ctrl Pts',(2.71801605199995,2.2,2.98191291799998));
#339611=CARTESIAN_POINT('Ctrl Pts',(2.71745656899995,12.2,2.98145165099999));
#339612=CARTESIAN_POINT('Ctrl Pts',(2.71745656899995,5.2,2.98145165099999));
#339613=CARTESIAN_POINT('Ctrl Pts',(2.71745656899995,2.2,2.98145165099999));
#339614=CARTESIAN_POINT('Ctrl Pts',(2.71690227399994,12.2,2.98099347799998));
#339615=CARTESIAN_POINT('Ctrl Pts',(2.71690227399994,5.2,2.98099347799998));
#339616=CARTESIAN_POINT('Ctrl Pts',(2.71690227399994,2.2,2.98099347799998));
#339617=CARTESIAN_POINT('Ctrl Pts',(2.71635316699995,12.2,2.98053841899999));
#339618=CARTESIAN_POINT('Ctrl Pts',(2.71635316699995,5.2,2.98053841899999));
#339619=CARTESIAN_POINT('Ctrl Pts',(2.71635316699995,2.2,2.98053841899999));
#339620=CARTESIAN_POINT('Ctrl Pts',(2.71580924999994,12.2,2.98008649399998));
#339621=CARTESIAN_POINT('Ctrl Pts',(2.71580924999994,5.2,2.98008649399998));
#339622=CARTESIAN_POINT('Ctrl Pts',(2.71580924999994,2.2,2.98008649399998));
#339623=CARTESIAN_POINT('Ctrl Pts',(2.71527051999994,12.2,2.97963772099998));
#339624=CARTESIAN_POINT('Ctrl Pts',(2.71527051999994,5.2,2.97963772099998));
#339625=CARTESIAN_POINT('Ctrl Pts',(2.71527051999994,2.2,2.97963772099998));
#339626=CARTESIAN_POINT('Ctrl Pts',(2.71473697799994,12.2,2.97919211899998));
#339627=CARTESIAN_POINT('Ctrl Pts',(2.71473697799994,5.2,2.97919211899998));
#339628=CARTESIAN_POINT('Ctrl Pts',(2.71473697799994,2.2,2.97919211899998));
#339629=CARTESIAN_POINT('Ctrl Pts',(2.71420862599994,12.2,2.97874970699999));
#339630=CARTESIAN_POINT('Ctrl Pts',(2.71420862599994,5.2,2.97874970699999));
#339631=CARTESIAN_POINT('Ctrl Pts',(2.71420862599994,2.2,2.97874970699999));
#339632=CARTESIAN_POINT('Ctrl Pts',(2.71368546199994,12.2,2.97831050599999));
#339633=CARTESIAN_POINT('Ctrl Pts',(2.71368546199994,5.2,2.97831050599999));
#339634=CARTESIAN_POINT('Ctrl Pts',(2.71368546199994,2.2,2.97831050599999));
#339635=CARTESIAN_POINT('Ctrl Pts',(2.71316748599994,12.2,2.97787453299998));
#339636=CARTESIAN_POINT('Ctrl Pts',(2.71316748599994,5.2,2.97787453299998));
#339637=CARTESIAN_POINT('Ctrl Pts',(2.71316748599994,2.2,2.97787453299998));
#339638=CARTESIAN_POINT('Ctrl Pts',(2.71265469899994,12.2,2.97744181099999));
#339639=CARTESIAN_POINT('Ctrl Pts',(2.71265469899994,5.2,2.97744181099999));
#339640=CARTESIAN_POINT('Ctrl Pts',(2.71265469899994,2.2,2.97744181099999));
#339641=CARTESIAN_POINT('Ctrl Pts',(2.71214709999994,12.2,2.97701235599998));
#339642=CARTESIAN_POINT('Ctrl Pts',(2.71214709999994,5.2,2.97701235599998));
#339643=CARTESIAN_POINT('Ctrl Pts',(2.71214709999994,2.2,2.97701235599998));
#339644=CARTESIAN_POINT('Ctrl Pts',(2.71164468899994,12.2,2.97658618899998));
#339645=CARTESIAN_POINT('Ctrl Pts',(2.71164468899994,5.2,2.97658618899998));
#339646=CARTESIAN_POINT('Ctrl Pts',(2.71164468899994,2.2,2.97658618899998));
#339647=CARTESIAN_POINT('Ctrl Pts',(2.71114746499994,12.2,2.97616332799999));
#339648=CARTESIAN_POINT('Ctrl Pts',(2.71114746499994,5.2,2.97616332799999));
#339649=CARTESIAN_POINT('Ctrl Pts',(2.71114746499994,2.2,2.97616332799999));
#339650=CARTESIAN_POINT('Ctrl Pts',(2.71065543099994,12.2,2.97574379499999));
#339651=CARTESIAN_POINT('Ctrl Pts',(2.71065543099994,5.2,2.97574379499999));
#339652=CARTESIAN_POINT('Ctrl Pts',(2.71065543099994,2.2,2.97574379499999));
#339653=CARTESIAN_POINT('Ctrl Pts',(2.71016858299994,12.2,2.97532760899998));
#339654=CARTESIAN_POINT('Ctrl Pts',(2.71016858299994,5.2,2.97532760899998));
#339655=CARTESIAN_POINT('Ctrl Pts',(2.71016858299994,2.2,2.97532760899998));
#339656=CARTESIAN_POINT('Ctrl Pts',(2.70968692299994,12.2,2.97491478899998));
#339657=CARTESIAN_POINT('Ctrl Pts',(2.70968692299994,5.2,2.97491478899998));
#339658=CARTESIAN_POINT('Ctrl Pts',(2.70968692299994,2.2,2.97491478899998));
#339659=CARTESIAN_POINT('Ctrl Pts',(2.70921044999994,12.2,2.97450535399998));
#339660=CARTESIAN_POINT('Ctrl Pts',(2.70921044999994,5.2,2.97450535399998));
#339661=CARTESIAN_POINT('Ctrl Pts',(2.70921044999994,2.2,2.97450535399998));
#339662=CARTESIAN_POINT('Ctrl Pts',(2.70873916399994,12.2,2.97409932599999));
#339663=CARTESIAN_POINT('Ctrl Pts',(2.70873916399994,5.2,2.97409932599999));
#339664=CARTESIAN_POINT('Ctrl Pts',(2.70873916399994,2.2,2.97409932599999));
#339665=CARTESIAN_POINT('Ctrl Pts',(2.70827306599994,12.2,2.97369672399999));
#339666=CARTESIAN_POINT('Ctrl Pts',(2.70827306599994,5.2,2.97369672399999));
#339667=CARTESIAN_POINT('Ctrl Pts',(2.70827306599994,2.2,2.97369672399999));
#339668=CARTESIAN_POINT('Ctrl Pts',(2.70781215299994,12.2,2.97329756699998));
#339669=CARTESIAN_POINT('Ctrl Pts',(2.70781215299994,5.2,2.97329756699998));
#339670=CARTESIAN_POINT('Ctrl Pts',(2.70781215299994,2.2,2.97329756699998));
#339671=CARTESIAN_POINT('Ctrl Pts',(2.70735642699994,12.2,2.97290187599998));
#339672=CARTESIAN_POINT('Ctrl Pts',(2.70735642699994,5.2,2.97290187599998));
#339673=CARTESIAN_POINT('Ctrl Pts',(2.70735642699994,2.2,2.97290187599998));
#339674=CARTESIAN_POINT('Ctrl Pts',(2.70690588599994,12.2,2.97250967099998));
#339675=CARTESIAN_POINT('Ctrl Pts',(2.70690588599994,5.2,2.97250967099998));
#339676=CARTESIAN_POINT('Ctrl Pts',(2.70690588599994,2.2,2.97250967099998));
#339677=CARTESIAN_POINT('Ctrl Pts',(2.70646052999994,12.2,2.97212097299998));
#339678=CARTESIAN_POINT('Ctrl Pts',(2.70646052999994,5.2,2.97212097299998));
#339679=CARTESIAN_POINT('Ctrl Pts',(2.70646052999994,2.2,2.97212097299998));
#339680=CARTESIAN_POINT('Ctrl Pts',(2.70602035899994,12.2,2.97173580099999));
#339681=CARTESIAN_POINT('Ctrl Pts',(2.70602035899994,5.2,2.97173580099999));
#339682=CARTESIAN_POINT('Ctrl Pts',(2.70602035899994,2.2,2.97173580099999));
#339683=CARTESIAN_POINT('Ctrl Pts',(2.70558537299994,12.2,2.97135417599999));
#339684=CARTESIAN_POINT('Ctrl Pts',(2.70558537299994,5.2,2.97135417599999));
#339685=CARTESIAN_POINT('Ctrl Pts',(2.70558537299994,2.2,2.97135417599999));
#339686=CARTESIAN_POINT('Ctrl Pts',(2.70515557099994,12.2,2.97097611699999));
#339687=CARTESIAN_POINT('Ctrl Pts',(2.70515557099994,5.2,2.97097611699999));
#339688=CARTESIAN_POINT('Ctrl Pts',(2.70515557099994,2.2,2.97097611699999));
#339689=CARTESIAN_POINT('Ctrl Pts',(2.70473095299995,12.2,2.97060164499998));
#339690=CARTESIAN_POINT('Ctrl Pts',(2.70473095299995,5.2,2.97060164499998));
#339691=CARTESIAN_POINT('Ctrl Pts',(2.70473095299995,2.2,2.97060164499998));
#339692=CARTESIAN_POINT('Ctrl Pts',(2.70431151699994,12.2,2.97023078199998));
#339693=CARTESIAN_POINT('Ctrl Pts',(2.70431151699994,5.2,2.97023078199998));
#339694=CARTESIAN_POINT('Ctrl Pts',(2.70431151699994,2.2,2.97023078199998));
#339695=CARTESIAN_POINT('Ctrl Pts',(2.70389726299994,12.2,2.96986354699998));
#339696=CARTESIAN_POINT('Ctrl Pts',(2.70389726299994,5.2,2.96986354699998));
#339697=CARTESIAN_POINT('Ctrl Pts',(2.70389726299994,2.2,2.96986354699998));
#339698=CARTESIAN_POINT('Ctrl Pts',(2.70348819199994,12.2,2.96949996099999));
#339699=CARTESIAN_POINT('Ctrl Pts',(2.70348819199994,5.2,2.96949996099999));
#339700=CARTESIAN_POINT('Ctrl Pts',(2.70348819199994,2.2,2.96949996099999));
#339701=CARTESIAN_POINT('Ctrl Pts',(2.70308430199994,12.2,2.96914004499998));
#339702=CARTESIAN_POINT('Ctrl Pts',(2.70308430199994,5.2,2.96914004499998));
#339703=CARTESIAN_POINT('Ctrl Pts',(2.70308430199994,2.2,2.96914004499998));
#339704=CARTESIAN_POINT('Ctrl Pts',(2.70268559399995,12.2,2.96878381799999));
#339705=CARTESIAN_POINT('Ctrl Pts',(2.70268559399995,5.2,2.96878381799999));
#339706=CARTESIAN_POINT('Ctrl Pts',(2.70268559399995,2.2,2.96878381799999));
#339707=CARTESIAN_POINT('Ctrl Pts',(2.70229206499994,12.2,2.96843130299998));
#339708=CARTESIAN_POINT('Ctrl Pts',(2.70229206499994,5.2,2.96843130299998));
#339709=CARTESIAN_POINT('Ctrl Pts',(2.70229206499994,2.2,2.96843130299998));
#339710=CARTESIAN_POINT('Ctrl Pts',(2.70190371499994,12.2,2.96808251899999));
#339711=CARTESIAN_POINT('Ctrl Pts',(2.70190371499994,5.2,2.96808251899999));
#339712=CARTESIAN_POINT('Ctrl Pts',(2.70190371499994,2.2,2.96808251899999));
#339713=CARTESIAN_POINT('Ctrl Pts',(2.70152054299994,12.2,2.96773748899999));
#339714=CARTESIAN_POINT('Ctrl Pts',(2.70152054299994,5.2,2.96773748899999));
#339715=CARTESIAN_POINT('Ctrl Pts',(2.70152054299994,2.2,2.96773748899999));
#339716=CARTESIAN_POINT('Ctrl Pts',(2.70114255199994,12.2,2.96739623199999));
#339717=CARTESIAN_POINT('Ctrl Pts',(2.70114255199994,5.2,2.96739623199999));
#339718=CARTESIAN_POINT('Ctrl Pts',(2.70114255199994,2.2,2.96739623199999));
#339719=CARTESIAN_POINT('Ctrl Pts',(2.70076973599994,12.2,2.96705876999999));
#339720=CARTESIAN_POINT('Ctrl Pts',(2.70076973599994,5.2,2.96705876999999));
#339721=CARTESIAN_POINT('Ctrl Pts',(2.70076973599994,2.2,2.96705876999999));
#339722=CARTESIAN_POINT('Ctrl Pts',(2.70040209599994,12.2,2.96672512299998));
#339723=CARTESIAN_POINT('Ctrl Pts',(2.70040209599994,5.2,2.96672512299998));
#339724=CARTESIAN_POINT('Ctrl Pts',(2.70040209599994,2.2,2.96672512299998));
#339725=CARTESIAN_POINT('Ctrl Pts',(2.70003963199994,12.2,2.96639531499999));
#339726=CARTESIAN_POINT('Ctrl Pts',(2.70003963199994,5.2,2.96639531499999));
#339727=CARTESIAN_POINT('Ctrl Pts',(2.70003963199994,2.2,2.96639531499999));
#339728=CARTESIAN_POINT('Ctrl Pts',(2.69968234399995,12.2,2.96606936399999));
#339729=CARTESIAN_POINT('Ctrl Pts',(2.69968234399995,5.2,2.96606936399999));
#339730=CARTESIAN_POINT('Ctrl Pts',(2.69968234399995,2.2,2.96606936399999));
#339731=CARTESIAN_POINT('Ctrl Pts',(2.69933022999994,12.2,2.96574729199998));
#339732=CARTESIAN_POINT('Ctrl Pts',(2.69933022999994,5.2,2.96574729199998));
#339733=CARTESIAN_POINT('Ctrl Pts',(2.69933022999994,2.2,2.96574729199998));
#339734=CARTESIAN_POINT('Ctrl Pts',(2.69898328799994,12.2,2.96542912099999));
#339735=CARTESIAN_POINT('Ctrl Pts',(2.69898328799994,5.2,2.96542912099999));
#339736=CARTESIAN_POINT('Ctrl Pts',(2.69898328799994,2.2,2.96542912099999));
#339737=CARTESIAN_POINT('Ctrl Pts',(2.69864151899994,12.2,2.96511487199999));
#339738=CARTESIAN_POINT('Ctrl Pts',(2.69864151899994,5.2,2.96511487199999));
#339739=CARTESIAN_POINT('Ctrl Pts',(2.69864151899994,2.2,2.96511487199999));
#339740=CARTESIAN_POINT('Ctrl Pts',(2.69830492099994,12.2,2.96480456799999));
#339741=CARTESIAN_POINT('Ctrl Pts',(2.69830492099994,5.2,2.96480456799999));
#339742=CARTESIAN_POINT('Ctrl Pts',(2.69830492099994,2.2,2.96480456799999));
#339743=CARTESIAN_POINT('Ctrl Pts',(2.69797349399994,12.2,2.96449822799998));
#339744=CARTESIAN_POINT('Ctrl Pts',(2.69797349399994,5.2,2.96449822799998));
#339745=CARTESIAN_POINT('Ctrl Pts',(2.69797349399994,2.2,2.96449822799998));
#339746=CARTESIAN_POINT('Ctrl Pts',(2.69764723399994,12.2,2.96419587599999));
#339747=CARTESIAN_POINT('Ctrl Pts',(2.69764723399994,5.2,2.96419587599999));
#339748=CARTESIAN_POINT('Ctrl Pts',(2.69764723399994,2.2,2.96419587599999));
#339749=CARTESIAN_POINT('Ctrl Pts',(2.69732614499994,12.2,2.96389753299999));
#339750=CARTESIAN_POINT('Ctrl Pts',(2.69732614499994,5.2,2.96389753299999));
#339751=CARTESIAN_POINT('Ctrl Pts',(2.69732614499994,2.2,2.96389753299999));
#339752=CARTESIAN_POINT('Ctrl Pts',(2.69701022099994,12.2,2.96360321899999));
#339753=CARTESIAN_POINT('Ctrl Pts',(2.69701022099994,5.2,2.96360321899999));
#339754=CARTESIAN_POINT('Ctrl Pts',(2.69701022099994,2.2,2.96360321899999));
#339755=CARTESIAN_POINT('Ctrl Pts',(2.69669946499994,12.2,2.96331295699999));
#339756=CARTESIAN_POINT('Ctrl Pts',(2.69669946499994,5.2,2.96331295699999));
#339757=CARTESIAN_POINT('Ctrl Pts',(2.69669946499994,2.2,2.96331295699999));
#339758=CARTESIAN_POINT('Ctrl Pts',(2.69639387299994,12.2,2.96302676999999));
#339759=CARTESIAN_POINT('Ctrl Pts',(2.69639387299994,5.2,2.96302676999999));
#339760=CARTESIAN_POINT('Ctrl Pts',(2.69639387299994,2.2,2.96302676999999));
#339761=CARTESIAN_POINT('Ctrl Pts',(2.69609344499994,12.2,2.96274467999999));
#339762=CARTESIAN_POINT('Ctrl Pts',(2.69609344499994,5.2,2.96274467999999));
#339763=CARTESIAN_POINT('Ctrl Pts',(2.69609344499994,2.2,2.96274467999999));
#339764=CARTESIAN_POINT('Ctrl Pts',(2.69579818099994,12.2,2.96246670699999));
#339765=CARTESIAN_POINT('Ctrl Pts',(2.69579818099994,5.2,2.96246670699999));
#339766=CARTESIAN_POINT('Ctrl Pts',(2.69579818099994,2.2,2.96246670699999));
#339767=CARTESIAN_POINT('Ctrl Pts',(2.69550807599995,12.2,2.96219287399998));
#339768=CARTESIAN_POINT('Ctrl Pts',(2.69550807599995,5.2,2.96219287399998));
#339769=CARTESIAN_POINT('Ctrl Pts',(2.69550807599995,2.2,2.96219287399998));
#339770=CARTESIAN_POINT('Ctrl Pts',(2.69522313299994,12.2,2.96192320399999));
#339771=CARTESIAN_POINT('Ctrl Pts',(2.69522313299994,5.2,2.96192320399999));
#339772=CARTESIAN_POINT('Ctrl Pts',(2.69522313299994,2.2,2.96192320399999));
#339773=CARTESIAN_POINT('Ctrl Pts',(2.69494334899994,12.2,2.96165771799998));
#339774=CARTESIAN_POINT('Ctrl Pts',(2.69494334899994,5.2,2.96165771799998));
#339775=CARTESIAN_POINT('Ctrl Pts',(2.69494334899994,2.2,2.96165771799998));
#339776=CARTESIAN_POINT('Ctrl Pts',(2.69466872299994,12.2,2.96139643899998));
#339777=CARTESIAN_POINT('Ctrl Pts',(2.69466872299994,5.2,2.96139643899998));
#339778=CARTESIAN_POINT('Ctrl Pts',(2.69466872299994,2.2,2.96139643899998));
#339779=CARTESIAN_POINT('Ctrl Pts',(2.69439925299995,12.2,2.96113938999999));
#339780=CARTESIAN_POINT('Ctrl Pts',(2.69439925299995,5.2,2.96113938999999));
#339781=CARTESIAN_POINT('Ctrl Pts',(2.69439925299995,2.2,2.96113938999999));
#339782=CARTESIAN_POINT('Ctrl Pts',(2.69413493799994,12.2,2.96088659199999));
#339783=CARTESIAN_POINT('Ctrl Pts',(2.69413493799994,5.2,2.96088659199999));
#339784=CARTESIAN_POINT('Ctrl Pts',(2.69413493799994,2.2,2.96088659199999));
#339785=CARTESIAN_POINT('Ctrl Pts',(2.69387577699994,12.2,2.96063806999998));
#339786=CARTESIAN_POINT('Ctrl Pts',(2.69387577699994,5.2,2.96063806999998));
#339787=CARTESIAN_POINT('Ctrl Pts',(2.69387577699994,2.2,2.96063806999998));
#339788=CARTESIAN_POINT('Ctrl Pts',(2.69362176799994,12.2,2.96039384299998));
#339789=CARTESIAN_POINT('Ctrl Pts',(2.69362176799994,5.2,2.96039384299998));
#339790=CARTESIAN_POINT('Ctrl Pts',(2.69362176799994,2.2,2.96039384299998));
#339791=CARTESIAN_POINT('Ctrl Pts',(2.69337290999994,12.2,2.96015393599999));
#339792=CARTESIAN_POINT('Ctrl Pts',(2.69337290999994,5.2,2.96015393599999));
#339793=CARTESIAN_POINT('Ctrl Pts',(2.69337290999994,2.2,2.96015393599999));
#339794=CARTESIAN_POINT('Ctrl Pts',(2.69312920199994,12.2,2.95991837199999));
#339795=CARTESIAN_POINT('Ctrl Pts',(2.69312920199994,5.2,2.95991837199999));
#339796=CARTESIAN_POINT('Ctrl Pts',(2.69312920199994,2.2,2.95991837199999));
#339797=CARTESIAN_POINT('Ctrl Pts',(2.69289064099994,12.2,2.95968717299999));
#339798=CARTESIAN_POINT('Ctrl Pts',(2.69289064099994,5.2,2.95968717299999));
#339799=CARTESIAN_POINT('Ctrl Pts',(2.69289064099994,2.2,2.95968717299999));
#339800=CARTESIAN_POINT('Ctrl Pts',(2.69265722699994,12.2,2.95946036199998));
#339801=CARTESIAN_POINT('Ctrl Pts',(2.69265722699994,5.2,2.95946036199998));
#339802=CARTESIAN_POINT('Ctrl Pts',(2.69265722699994,2.2,2.95946036199998));
#339803=CARTESIAN_POINT('Ctrl Pts',(2.69242895799994,12.2,2.95923796299999));
#339804=CARTESIAN_POINT('Ctrl Pts',(2.69242895799994,5.2,2.95923796299999));
#339805=CARTESIAN_POINT('Ctrl Pts',(2.69242895799994,2.2,2.95923796299999));
#339806=CARTESIAN_POINT('Ctrl Pts',(2.69220583199994,12.2,2.95901999699999));
#339807=CARTESIAN_POINT('Ctrl Pts',(2.69220583199994,5.2,2.95901999699999));
#339808=CARTESIAN_POINT('Ctrl Pts',(2.69220583199994,2.2,2.95901999699999));
#339809=CARTESIAN_POINT('Ctrl Pts',(2.69198784799995,12.2,2.95880648799999));
#339810=CARTESIAN_POINT('Ctrl Pts',(2.69198784799995,5.2,2.95880648799999));
#339811=CARTESIAN_POINT('Ctrl Pts',(2.69198784799995,2.2,2.95880648799999));
#339812=CARTESIAN_POINT('Ctrl Pts',(2.69177500299994,12.2,2.95859746099998));
#339813=CARTESIAN_POINT('Ctrl Pts',(2.69177500299994,5.2,2.95859746099998));
#339814=CARTESIAN_POINT('Ctrl Pts',(2.69177500299994,2.2,2.95859746099998));
#339815=CARTESIAN_POINT('Ctrl Pts',(2.69156729699994,12.2,2.95839293699999));
#339816=CARTESIAN_POINT('Ctrl Pts',(2.69156729699994,5.2,2.95839293699999));
#339817=CARTESIAN_POINT('Ctrl Pts',(2.69156729699994,2.2,2.95839293699999));
#339818=CARTESIAN_POINT('Ctrl Pts',(2.69136472799994,12.2,2.95819293999998));
#339819=CARTESIAN_POINT('Ctrl Pts',(2.69136472799994,5.2,2.95819293999998));
#339820=CARTESIAN_POINT('Ctrl Pts',(2.69136472799994,2.2,2.95819293999998));
#339821=CARTESIAN_POINT('Ctrl Pts',(2.69116729299994,12.2,2.95799749299999));
#339822=CARTESIAN_POINT('Ctrl Pts',(2.69116729299994,5.2,2.95799749299999));
#339823=CARTESIAN_POINT('Ctrl Pts',(2.69116729299994,2.2,2.95799749299999));
#339824=CARTESIAN_POINT('Ctrl Pts',(2.69097499199995,12.2,2.95780662099999));
#339825=CARTESIAN_POINT('Ctrl Pts',(2.69097499199995,5.2,2.95780662099999));
#339826=CARTESIAN_POINT('Ctrl Pts',(2.69097499199995,2.2,2.95780662099999));
#339827=CARTESIAN_POINT('Ctrl Pts',(2.69078782199994,12.2,2.95762034699998));
#339828=CARTESIAN_POINT('Ctrl Pts',(2.69078782199994,5.2,2.95762034699998));
#339829=CARTESIAN_POINT('Ctrl Pts',(2.69078782199994,2.2,2.95762034699998));
#339830=CARTESIAN_POINT('Ctrl Pts',(2.69060577999995,12.2,2.95743869399999));
#339831=CARTESIAN_POINT('Ctrl Pts',(2.69060577999995,5.2,2.95743869399999));
#339832=CARTESIAN_POINT('Ctrl Pts',(2.69060577999995,2.2,2.95743869399999));
#339833=CARTESIAN_POINT('Ctrl Pts',(2.69042886699994,12.2,2.95726168599998));
#339834=CARTESIAN_POINT('Ctrl Pts',(2.69042886699994,5.2,2.95726168599998));
#339835=CARTESIAN_POINT('Ctrl Pts',(2.69042886699994,2.2,2.95726168599998));
#339836=CARTESIAN_POINT('Ctrl Pts',(2.69025707999994,12.2,2.95708934699999));
#339837=CARTESIAN_POINT('Ctrl Pts',(2.69025707999994,5.2,2.95708934699999));
#339838=CARTESIAN_POINT('Ctrl Pts',(2.69025707999994,2.2,2.95708934699999));
#339839=CARTESIAN_POINT('Ctrl Pts',(2.69009041599995,12.2,2.95692170099999));
#339840=CARTESIAN_POINT('Ctrl Pts',(2.69009041599995,5.2,2.95692170099999));
#339841=CARTESIAN_POINT('Ctrl Pts',(2.69009041599995,2.2,2.95692170099999));
#339842=CARTESIAN_POINT('Ctrl Pts',(2.68992887199994,12.2,2.95675877199999));
#339843=CARTESIAN_POINT('Ctrl Pts',(2.68992887199994,5.2,2.95675877199999));
#339844=CARTESIAN_POINT('Ctrl Pts',(2.68992887199994,2.2,2.95675877199999));
#339845=CARTESIAN_POINT('Ctrl Pts',(2.68977244999994,12.2,2.95660058499998));
#339846=CARTESIAN_POINT('Ctrl Pts',(2.68977244999994,5.2,2.95660058499998));
#339847=CARTESIAN_POINT('Ctrl Pts',(2.68977244999994,2.2,2.95660058499998));
#339848=CARTESIAN_POINT('Ctrl Pts',(2.68962114499995,12.2,2.95644716099999));
#339849=CARTESIAN_POINT('Ctrl Pts',(2.68962114499995,5.2,2.95644716099999));
#339850=CARTESIAN_POINT('Ctrl Pts',(2.68962114499995,2.2,2.95644716099999));
#339851=CARTESIAN_POINT('Ctrl Pts',(2.68947495599994,12.2,2.95629852799999));
#339852=CARTESIAN_POINT('Ctrl Pts',(2.68947495599994,5.2,2.95629852799999));
#339853=CARTESIAN_POINT('Ctrl Pts',(2.68947495599994,2.2,2.95629852799999));
#339854=CARTESIAN_POINT('Ctrl Pts',(2.68933387899994,12.2,2.95615470799999));
#339855=CARTESIAN_POINT('Ctrl Pts',(2.68933387899994,5.2,2.95615470799999));
#339856=CARTESIAN_POINT('Ctrl Pts',(2.68933387899994,2.2,2.95615470799999));
#339857=CARTESIAN_POINT('Ctrl Pts',(2.68919791499994,12.2,2.95601572699999));
#339858=CARTESIAN_POINT('Ctrl Pts',(2.68919791499994,5.2,2.95601572699999));
#339859=CARTESIAN_POINT('Ctrl Pts',(2.68919791499994,2.2,2.95601572699999));
#339860=CARTESIAN_POINT('Ctrl Pts',(2.68906705899994,12.2,2.95588160999999));
#339861=CARTESIAN_POINT('Ctrl Pts',(2.68906705899994,5.2,2.95588160999999));
#339862=CARTESIAN_POINT('Ctrl Pts',(2.68906705899994,2.2,2.95588160999999));
#339863=CARTESIAN_POINT('Ctrl Pts',(2.68894130999994,12.2,2.95575237899998));
#339864=CARTESIAN_POINT('Ctrl Pts',(2.68894130999994,5.2,2.95575237899998));
#339865=CARTESIAN_POINT('Ctrl Pts',(2.68894130999994,2.2,2.95575237899998));
#339866=CARTESIAN_POINT('Ctrl Pts',(2.68882066599994,12.2,2.95562805999998));
#339867=CARTESIAN_POINT('Ctrl Pts',(2.68882066599994,5.2,2.95562805999998));
#339868=CARTESIAN_POINT('Ctrl Pts',(2.68882066599994,2.2,2.95562805999998));
#339869=CARTESIAN_POINT('Ctrl Pts',(2.68870512299995,12.2,2.95550867699998));
#339870=CARTESIAN_POINT('Ctrl Pts',(2.68870512299995,5.2,2.95550867699998));
#339871=CARTESIAN_POINT('Ctrl Pts',(2.68870512299995,2.2,2.95550867699998));
#339872=CARTESIAN_POINT('Ctrl Pts',(2.68859468199994,12.2,2.95539425399999));
#339873=CARTESIAN_POINT('Ctrl Pts',(2.68859468199994,5.2,2.95539425399999));
#339874=CARTESIAN_POINT('Ctrl Pts',(2.68859468199994,2.2,2.95539425399999));
#339875=CARTESIAN_POINT('Ctrl Pts',(2.68848933799994,12.2,2.95528481599998));
#339876=CARTESIAN_POINT('Ctrl Pts',(2.68848933799994,5.2,2.95528481599998));
#339877=CARTESIAN_POINT('Ctrl Pts',(2.68848933799994,2.2,2.95528481599998));
#339878=CARTESIAN_POINT('Ctrl Pts',(2.68838908999995,12.2,2.95518039199998));
#339879=CARTESIAN_POINT('Ctrl Pts',(2.68838908999995,5.2,2.95518039199998));
#339880=CARTESIAN_POINT('Ctrl Pts',(2.68838908999995,2.2,2.95518039199998));
#339881=CARTESIAN_POINT('Ctrl Pts',(2.68829393399994,12.2,2.95508100599999));
#339882=CARTESIAN_POINT('Ctrl Pts',(2.68829393399994,5.2,2.95508100599999));
#339883=CARTESIAN_POINT('Ctrl Pts',(2.68829393399994,2.2,2.95508100599999));
#339884=CARTESIAN_POINT('Ctrl Pts',(2.68820386799994,12.2,2.95498668399999));
#339885=CARTESIAN_POINT('Ctrl Pts',(2.68820386799994,5.2,2.95498668399999));
#339886=CARTESIAN_POINT('Ctrl Pts',(2.68820386799994,2.2,2.95498668399999));
#339887=CARTESIAN_POINT('Ctrl Pts',(2.68811888899994,12.2,2.95489745099999));
#339888=CARTESIAN_POINT('Ctrl Pts',(2.68811888899994,5.2,2.95489745099999));
#339889=CARTESIAN_POINT('Ctrl Pts',(2.68811888899994,2.2,2.95489745099999));
#339890=CARTESIAN_POINT('Ctrl Pts',(2.68803899599994,12.2,2.95481332999999));
#339891=CARTESIAN_POINT('Ctrl Pts',(2.68803899599994,5.2,2.95481332999999));
#339892=CARTESIAN_POINT('Ctrl Pts',(2.68803899599994,2.2,2.95481332999999));
#339893=CARTESIAN_POINT('Ctrl Pts',(2.68796418699994,12.2,2.95473434299999));
#339894=CARTESIAN_POINT('Ctrl Pts',(2.68796418699994,5.2,2.95473434299999));
#339895=CARTESIAN_POINT('Ctrl Pts',(2.68796418699994,2.2,2.95473434299999));
#339896=CARTESIAN_POINT('Ctrl Pts',(2.68789445799994,12.2,2.95466051499999));
#339897=CARTESIAN_POINT('Ctrl Pts',(2.68789445799994,5.2,2.95466051499999));
#339898=CARTESIAN_POINT('Ctrl Pts',(2.68789445799994,2.2,2.95466051499999));
#339899=CARTESIAN_POINT('Ctrl Pts',(2.68782980799994,12.2,2.95459186999998));
#339900=CARTESIAN_POINT('Ctrl Pts',(2.68782980799994,5.2,2.95459186999998));
#339901=CARTESIAN_POINT('Ctrl Pts',(2.68782980799994,2.2,2.95459186999998));
#339902=CARTESIAN_POINT('Ctrl Pts',(2.68777023099994,12.2,2.95452843899999));
#339903=CARTESIAN_POINT('Ctrl Pts',(2.68777023099994,5.2,2.95452843899999));
#339904=CARTESIAN_POINT('Ctrl Pts',(2.68777023099994,2.2,2.95452843899999));
#339905=CARTESIAN_POINT('Ctrl Pts',(2.68771572699994,12.2,2.95447025399999));
#339906=CARTESIAN_POINT('Ctrl Pts',(2.68771572699994,5.2,2.95447025399999));
#339907=CARTESIAN_POINT('Ctrl Pts',(2.68771572699994,2.2,2.95447025399999));
#339908=CARTESIAN_POINT('Ctrl Pts',(2.68766629099995,12.2,2.95441734799999));
#339909=CARTESIAN_POINT('Ctrl Pts',(2.68766629099995,5.2,2.95441734799999));
#339910=CARTESIAN_POINT('Ctrl Pts',(2.68766629099995,2.2,2.95441734799999));
#339911=CARTESIAN_POINT('Ctrl Pts',(2.68762191999994,12.2,2.95436974999999));
#339912=CARTESIAN_POINT('Ctrl Pts',(2.68762191999994,5.2,2.95436974999999));
#339913=CARTESIAN_POINT('Ctrl Pts',(2.68762191999994,2.2,2.95436974999999));
#339914=CARTESIAN_POINT('Ctrl Pts',(2.68758261099994,12.2,2.95432747899999));
#339915=CARTESIAN_POINT('Ctrl Pts',(2.68758261099994,5.2,2.95432747899999));
#339916=CARTESIAN_POINT('Ctrl Pts',(2.68758261099994,2.2,2.95432747899999));
#339917=CARTESIAN_POINT('Ctrl Pts',(2.68754469767605,12.2,2.95428659655369));
#339918=CARTESIAN_POINT('Ctrl Pts',(2.68754469767605,5.2,2.95428659655369));
#339919=CARTESIAN_POINT('Ctrl Pts',(2.68754469767605,2.2,2.95428659655369));
#339920=CARTESIAN_POINT('Ctrl Pts',(2.68751883712808,12.2,2.9542585984447));
#339921=CARTESIAN_POINT('Ctrl Pts',(2.68751883712808,5.2,2.9542585984447));
#339922=CARTESIAN_POINT('Ctrl Pts',(2.68751883712808,2.2,2.9542585984447));
#339923=CARTESIAN_POINT('Ctrl Pts',(2.68750184158111,12.2,2.95424011739526));
#339924=CARTESIAN_POINT('Ctrl Pts',(2.68750184158111,5.2,2.95424011739526));
#339925=CARTESIAN_POINT('Ctrl Pts',(2.68750184158111,2.2,2.95424011739526));
#339926=CARTESIAN_POINT('Ctrl Pts',(2.68749128112236,12.2,2.95422858071313));
#339927=CARTESIAN_POINT('Ctrl Pts',(2.68749128112236,5.2,2.95422858071313));
#339928=CARTESIAN_POINT('Ctrl Pts',(2.68749128112236,2.2,2.95422858071313));
#339929=CARTESIAN_POINT('Ctrl Pts',(2.68748475499994,12.2,2.95422146199999));
#339930=CARTESIAN_POINT('Ctrl Pts',(2.68748475499994,5.2,2.95422146199999));
#339931=CARTESIAN_POINT('Ctrl Pts',(2.68748475499994,2.2,2.95422146199999));
#339932=CARTESIAN_POINT('',(3.44029922199995,12.2,3.27518568399999));
#339933=CARTESIAN_POINT('Origin',(-5.66300478732629E-14,15.2,-1.77635683940025E-14));
#339934=CARTESIAN_POINT('',(3.66384038699994,12.2,3.02304045899999));
#339935=CARTESIAN_POINT('Ctrl Pts',(3.25496447599994,12.2,2.31410207099998));
#339936=CARTESIAN_POINT('Ctrl Pts',(3.25496447599994,5.2,2.31410207099998));
#339937=CARTESIAN_POINT('Ctrl Pts',(3.25496447599994,2.2,2.31410207099998));
#339938=CARTESIAN_POINT('Ctrl Pts',(3.25497003667146,12.2,2.31410605776463));
#339939=CARTESIAN_POINT('Ctrl Pts',(3.25497003667146,5.2,2.31410605776463));
#339940=CARTESIAN_POINT('Ctrl Pts',(3.25497003667146,2.2,2.31410605776463));
#339941=CARTESIAN_POINT('Ctrl Pts',(3.25498079470201,12.2,2.31411376555869));
#339942=CARTESIAN_POINT('Ctrl Pts',(3.25498079470201,5.2,2.31411376555869));
#339943=CARTESIAN_POINT('Ctrl Pts',(3.25498079470201,2.2,2.31411376555869));
#339944=CARTESIAN_POINT('Ctrl Pts',(3.25499674313561,12.2,2.31412520718679));
#339945=CARTESIAN_POINT('Ctrl Pts',(3.25499674313561,5.19999999999999,2.31412520718679));
#339946=CARTESIAN_POINT('Ctrl Pts',(3.25499674313561,2.2,2.31412520718679));
#339947=CARTESIAN_POINT('Ctrl Pts',(3.25501789589991,12.2,2.31414031259025));
#339948=CARTESIAN_POINT('Ctrl Pts',(3.25501789589991,5.19999999999999,2.31414031259025));
#339949=CARTESIAN_POINT('Ctrl Pts',(3.25501789589991,2.2,2.31414031259025));
#339950=CARTESIAN_POINT('Ctrl Pts',(3.25505458999995,12.2,2.31416690699998));
#339951=CARTESIAN_POINT('Ctrl Pts',(3.25505458999995,5.2,2.31416690699998));
#339952=CARTESIAN_POINT('Ctrl Pts',(3.25505458999995,2.2,2.31416690699998));
#339953=CARTESIAN_POINT('Ctrl Pts',(3.25509535799994,12.2,2.31419648199998));
#339954=CARTESIAN_POINT('Ctrl Pts',(3.25509535799994,5.2,2.31419648199998));
#339955=CARTESIAN_POINT('Ctrl Pts',(3.25509535799994,2.2,2.31419648199998));
#339956=CARTESIAN_POINT('Ctrl Pts',(3.25514203299994,12.2,2.31423044199999));
#339957=CARTESIAN_POINT('Ctrl Pts',(3.25514203299994,5.2,2.31423044199999));
#339958=CARTESIAN_POINT('Ctrl Pts',(3.25514203299994,2.2,2.31423044199999));
#339959=CARTESIAN_POINT('Ctrl Pts',(3.25519460599994,12.2,2.31426878999998));
#339960=CARTESIAN_POINT('Ctrl Pts',(3.25519460599994,5.2,2.31426878999998));
#339961=CARTESIAN_POINT('Ctrl Pts',(3.25519460599994,2.2,2.31426878999998));
#339962=CARTESIAN_POINT('Ctrl Pts',(3.25525305499994,12.2,2.31431152999999));
#339963=CARTESIAN_POINT('Ctrl Pts',(3.25525305499994,5.2,2.31431152999999));
#339964=CARTESIAN_POINT('Ctrl Pts',(3.25525305499994,2.2,2.31431152999999));
#339965=CARTESIAN_POINT('Ctrl Pts',(3.25531735199994,12.2,2.31435866999998));
#339966=CARTESIAN_POINT('Ctrl Pts',(3.25531735199994,5.2,2.31435866999998));
#339967=CARTESIAN_POINT('Ctrl Pts',(3.25531735199994,2.2,2.31435866999998));
#339968=CARTESIAN_POINT('Ctrl Pts',(3.25538746499995,12.2,2.31441021399998));
#339969=CARTESIAN_POINT('Ctrl Pts',(3.25538746499995,5.2,2.31441021399998));
#339970=CARTESIAN_POINT('Ctrl Pts',(3.25538746499995,2.2,2.31441021399998));
#339971=CARTESIAN_POINT('Ctrl Pts',(3.25546336299994,12.2,2.31446617399999));
#339972=CARTESIAN_POINT('Ctrl Pts',(3.25546336299994,5.2,2.31446617399999));
#339973=CARTESIAN_POINT('Ctrl Pts',(3.25546336299994,2.2,2.31446617399999));
#339974=CARTESIAN_POINT('Ctrl Pts',(3.25554501499994,12.2,2.31452655399998));
#339975=CARTESIAN_POINT('Ctrl Pts',(3.25554501499994,5.2,2.31452655399998));
#339976=CARTESIAN_POINT('Ctrl Pts',(3.25554501499994,2.2,2.31452655399998));
#339977=CARTESIAN_POINT('Ctrl Pts',(3.25563239699994,12.2,2.31459135899998));
#339978=CARTESIAN_POINT('Ctrl Pts',(3.25563239699994,5.2,2.31459135899998));
#339979=CARTESIAN_POINT('Ctrl Pts',(3.25563239699994,2.2,2.31459135899998));
#339980=CARTESIAN_POINT('Ctrl Pts',(3.25572548599995,12.2,2.31466059599999));
#339981=CARTESIAN_POINT('Ctrl Pts',(3.25572548599995,5.2,2.31466059599999));
#339982=CARTESIAN_POINT('Ctrl Pts',(3.25572548599995,2.2,2.31466059599999));
#339983=CARTESIAN_POINT('Ctrl Pts',(3.25582425799994,12.2,2.31473426899999));
#339984=CARTESIAN_POINT('Ctrl Pts',(3.25582425799994,5.2,2.31473426899999));
#339985=CARTESIAN_POINT('Ctrl Pts',(3.25582425799994,2.2,2.31473426899999));
#339986=CARTESIAN_POINT('Ctrl Pts',(3.25592869299994,12.2,2.31481238299999));
#339987=CARTESIAN_POINT('Ctrl Pts',(3.25592869299994,5.2,2.31481238299999));
#339988=CARTESIAN_POINT('Ctrl Pts',(3.25592869299994,2.2,2.31481238299999));
#339989=CARTESIAN_POINT('Ctrl Pts',(3.25603876599994,12.2,2.31489494399999));
#339990=CARTESIAN_POINT('Ctrl Pts',(3.25603876599994,5.2,2.31489494399999));
#339991=CARTESIAN_POINT('Ctrl Pts',(3.25603876599994,2.2,2.31489494399999));
#339992=CARTESIAN_POINT('Ctrl Pts',(3.25615445099994,12.2,2.31498195699999));
#339993=CARTESIAN_POINT('Ctrl Pts',(3.25615445099994,5.2,2.31498195699999));
#339994=CARTESIAN_POINT('Ctrl Pts',(3.25615445099994,2.2,2.31498195699999));
#339995=CARTESIAN_POINT('Ctrl Pts',(3.25627572299994,12.2,2.31507342799999));
#339996=CARTESIAN_POINT('Ctrl Pts',(3.25627572299994,5.2,2.31507342799999));
#339997=CARTESIAN_POINT('Ctrl Pts',(3.25627572299994,2.2,2.31507342799999));
#339998=CARTESIAN_POINT('Ctrl Pts',(3.25640255599994,12.2,2.31516936199998));
#339999=CARTESIAN_POINT('Ctrl Pts',(3.25640255599994,5.2,2.31516936199998));
#340000=CARTESIAN_POINT('Ctrl Pts',(3.25640255599994,2.2,2.31516936199998));
#340001=CARTESIAN_POINT('Ctrl Pts',(3.25653492399995,12.2,2.31526976599998));
#340002=CARTESIAN_POINT('Ctrl Pts',(3.25653492399995,5.2,2.31526976599998));
#340003=CARTESIAN_POINT('Ctrl Pts',(3.25653492399995,2.2,2.31526976599998));
#340004=CARTESIAN_POINT('Ctrl Pts',(3.25667280399994,12.2,2.31537464299999));
#340005=CARTESIAN_POINT('Ctrl Pts',(3.25667280399994,5.2,2.31537464299999));
#340006=CARTESIAN_POINT('Ctrl Pts',(3.25667280399994,2.2,2.31537464299999));
#340007=CARTESIAN_POINT('Ctrl Pts',(3.25681617199994,12.2,2.31548399999999));
#340008=CARTESIAN_POINT('Ctrl Pts',(3.25681617199994,5.2,2.31548399999999));
#340009=CARTESIAN_POINT('Ctrl Pts',(3.25681617199994,2.2,2.31548399999999));
#340010=CARTESIAN_POINT('Ctrl Pts',(3.25696500399994,12.2,2.31559784099999));
#340011=CARTESIAN_POINT('Ctrl Pts',(3.25696500399994,5.2,2.31559784099999));
#340012=CARTESIAN_POINT('Ctrl Pts',(3.25696500399994,2.2,2.31559784099999));
#340013=CARTESIAN_POINT('Ctrl Pts',(3.25711927599994,12.2,2.31571617199998));
#340014=CARTESIAN_POINT('Ctrl Pts',(3.25711927599994,5.2,2.31571617199998));
#340015=CARTESIAN_POINT('Ctrl Pts',(3.25711927599994,2.2,2.31571617199998));
#340016=CARTESIAN_POINT('Ctrl Pts',(3.25727896499994,12.2,2.31583899699999));
#340017=CARTESIAN_POINT('Ctrl Pts',(3.25727896499994,5.2,2.31583899699999));
#340018=CARTESIAN_POINT('Ctrl Pts',(3.25727896499994,2.2,2.31583899699999));
#340019=CARTESIAN_POINT('Ctrl Pts',(3.25744404599994,12.2,2.31596632299999));
#340020=CARTESIAN_POINT('Ctrl Pts',(3.25744404599994,5.2,2.31596632299999));
#340021=CARTESIAN_POINT('Ctrl Pts',(3.25744404599994,2.2,2.31596632299999));
#340022=CARTESIAN_POINT('Ctrl Pts',(3.25761449399995,12.2,2.31609815299999));
#340023=CARTESIAN_POINT('Ctrl Pts',(3.25761449399995,5.2,2.31609815299999));
#340024=CARTESIAN_POINT('Ctrl Pts',(3.25761449399995,2.2,2.31609815299999));
#340025=CARTESIAN_POINT('Ctrl Pts',(3.25779028699994,12.2,2.31623449299999));
#340026=CARTESIAN_POINT('Ctrl Pts',(3.25779028699994,5.2,2.31623449299999));
#340027=CARTESIAN_POINT('Ctrl Pts',(3.25779028699994,2.2,2.31623449299999));
#340028=CARTESIAN_POINT('Ctrl Pts',(3.25797139899994,12.2,2.31637534699999));
#340029=CARTESIAN_POINT('Ctrl Pts',(3.25797139899994,5.2,2.31637534699999));
#340030=CARTESIAN_POINT('Ctrl Pts',(3.25797139899994,2.2,2.31637534699999));
#340031=CARTESIAN_POINT('Ctrl Pts',(3.25815780899994,12.2,2.31652072099998));
#340032=CARTESIAN_POINT('Ctrl Pts',(3.25815780899994,5.2,2.31652072099998));
#340033=CARTESIAN_POINT('Ctrl Pts',(3.25815780899994,2.2,2.31652072099998));
#340034=CARTESIAN_POINT('Ctrl Pts',(3.25834949099994,12.2,2.31667061999998));
#340035=CARTESIAN_POINT('Ctrl Pts',(3.25834949099994,5.2,2.31667061999998));
#340036=CARTESIAN_POINT('Ctrl Pts',(3.25834949099994,2.2,2.31667061999998));
#340037=CARTESIAN_POINT('Ctrl Pts',(3.25854642299995,12.2,2.31682504699998));
#340038=CARTESIAN_POINT('Ctrl Pts',(3.25854642299995,5.2,2.31682504699998));
#340039=CARTESIAN_POINT('Ctrl Pts',(3.25854642299995,2.2,2.31682504699998));
#340040=CARTESIAN_POINT('Ctrl Pts',(3.25874858199994,12.2,2.31698400899999));
#340041=CARTESIAN_POINT('Ctrl Pts',(3.25874858199994,5.2,2.31698400899999));
#340042=CARTESIAN_POINT('Ctrl Pts',(3.25874858199994,2.2,2.31698400899999));
#340043=CARTESIAN_POINT('Ctrl Pts',(3.25895594299995,12.2,2.31714750899998));
#340044=CARTESIAN_POINT('Ctrl Pts',(3.25895594299995,5.2,2.31714750899998));
#340045=CARTESIAN_POINT('Ctrl Pts',(3.25895594299995,2.2,2.31714750899998));
#340046=CARTESIAN_POINT('Ctrl Pts',(3.25916848299994,12.2,2.31731555299998));
#340047=CARTESIAN_POINT('Ctrl Pts',(3.25916848299994,5.2,2.31731555299998));
#340048=CARTESIAN_POINT('Ctrl Pts',(3.25916848299994,2.2,2.31731555299998));
#340049=CARTESIAN_POINT('Ctrl Pts',(3.25938617999994,12.2,2.31748814399999));
#340050=CARTESIAN_POINT('Ctrl Pts',(3.25938617999994,5.2,2.31748814399999));
#340051=CARTESIAN_POINT('Ctrl Pts',(3.25938617999994,2.2,2.31748814399999));
#340052=CARTESIAN_POINT('Ctrl Pts',(3.25960900999994,12.2,2.31766528799998));
#340053=CARTESIAN_POINT('Ctrl Pts',(3.25960900999994,5.2,2.31766528799998));
#340054=CARTESIAN_POINT('Ctrl Pts',(3.25960900999994,2.2,2.31766528799998));
#340055=CARTESIAN_POINT('Ctrl Pts',(3.25983694999994,12.2,2.31784698899999));
#340056=CARTESIAN_POINT('Ctrl Pts',(3.25983694999994,5.2,2.31784698899999));
#340057=CARTESIAN_POINT('Ctrl Pts',(3.25983694999994,2.2,2.31784698899999));
#340058=CARTESIAN_POINT('Ctrl Pts',(3.26006997599994,12.2,2.31803325099999));
#340059=CARTESIAN_POINT('Ctrl Pts',(3.26006997599994,5.2,2.31803325099999));
#340060=CARTESIAN_POINT('Ctrl Pts',(3.26006997599994,2.2,2.31803325099999));
#340061=CARTESIAN_POINT('Ctrl Pts',(3.26030806799994,12.2,2.31822407999998));
#340062=CARTESIAN_POINT('Ctrl Pts',(3.26030806799994,5.2,2.31822407999998));
#340063=CARTESIAN_POINT('Ctrl Pts',(3.26030806799994,2.2,2.31822407999998));
#340064=CARTESIAN_POINT('Ctrl Pts',(3.26055119999995,12.2,2.31841947899999));
#340065=CARTESIAN_POINT('Ctrl Pts',(3.26055119999995,5.2,2.31841947899999));
#340066=CARTESIAN_POINT('Ctrl Pts',(3.26055119999995,2.2,2.31841947899999));
#340067=CARTESIAN_POINT('Ctrl Pts',(3.26079935099994,12.2,2.31861945399999));
#340068=CARTESIAN_POINT('Ctrl Pts',(3.26079935099994,5.2,2.31861945399999));
#340069=CARTESIAN_POINT('Ctrl Pts',(3.26079935099994,2.2,2.31861945399999));
#340070=CARTESIAN_POINT('Ctrl Pts',(3.26105249699994,12.2,2.31882400699998));
#340071=CARTESIAN_POINT('Ctrl Pts',(3.26105249699994,5.2,2.31882400699998));
#340072=CARTESIAN_POINT('Ctrl Pts',(3.26105249699994,2.2,2.31882400699998));
#340073=CARTESIAN_POINT('Ctrl Pts',(3.26131061799994,12.2,2.31903314399998));
#340074=CARTESIAN_POINT('Ctrl Pts',(3.26131061799994,5.2,2.31903314399998));
#340075=CARTESIAN_POINT('Ctrl Pts',(3.26131061799994,2.2,2.31903314399998));
#340076=CARTESIAN_POINT('Ctrl Pts',(3.26157368799994,12.2,2.31924686699998));
#340077=CARTESIAN_POINT('Ctrl Pts',(3.26157368799994,5.2,2.31924686699998));
#340078=CARTESIAN_POINT('Ctrl Pts',(3.26157368799994,2.2,2.31924686699998));
#340079=CARTESIAN_POINT('Ctrl Pts',(3.26184168799994,12.2,2.31946518399999));
#340080=CARTESIAN_POINT('Ctrl Pts',(3.26184168799994,5.2,2.31946518399999));
#340081=CARTESIAN_POINT('Ctrl Pts',(3.26184168799994,2.2,2.31946518399999));
#340082=CARTESIAN_POINT('Ctrl Pts',(3.26211459199994,12.2,2.31968809699998));
#340083=CARTESIAN_POINT('Ctrl Pts',(3.26211459199994,5.2,2.31968809699998));
#340084=CARTESIAN_POINT('Ctrl Pts',(3.26211459199994,2.2,2.31968809699998));
#340085=CARTESIAN_POINT('Ctrl Pts',(3.26239237999994,12.2,2.31991560899999));
#340086=CARTESIAN_POINT('Ctrl Pts',(3.26239237999994,5.2,2.31991560899999));
#340087=CARTESIAN_POINT('Ctrl Pts',(3.26239237999994,2.2,2.31991560899999));
#340088=CARTESIAN_POINT('Ctrl Pts',(3.26267502899994,12.2,2.32014772599999));
#340089=CARTESIAN_POINT('Ctrl Pts',(3.26267502899994,5.2,2.32014772599999));
#340090=CARTESIAN_POINT('Ctrl Pts',(3.26267502899994,2.2,2.32014772599999));
#340091=CARTESIAN_POINT('Ctrl Pts',(3.26296251699994,12.2,2.32038445199999));
#340092=CARTESIAN_POINT('Ctrl Pts',(3.26296251699994,5.2,2.32038445199999));
#340093=CARTESIAN_POINT('Ctrl Pts',(3.26296251699994,2.2,2.32038445199999));
#340094=CARTESIAN_POINT('Ctrl Pts',(3.26325482199994,12.2,2.32062579099999));
#340095=CARTESIAN_POINT('Ctrl Pts',(3.26325482199994,5.2,2.32062579099999));
#340096=CARTESIAN_POINT('Ctrl Pts',(3.26325482199994,2.2,2.32062579099999));
#340097=CARTESIAN_POINT('Ctrl Pts',(3.26355192099994,12.2,2.32087174499998));
#340098=CARTESIAN_POINT('Ctrl Pts',(3.26355192099994,5.2,2.32087174499998));
#340099=CARTESIAN_POINT('Ctrl Pts',(3.26355192099994,2.2,2.32087174499998));
#340100=CARTESIAN_POINT('Ctrl Pts',(3.26385379399994,12.2,2.32112232099999));
#340101=CARTESIAN_POINT('Ctrl Pts',(3.26385379399994,5.2,2.32112232099999));
#340102=CARTESIAN_POINT('Ctrl Pts',(3.26385379399994,2.2,2.32112232099999));
#340103=CARTESIAN_POINT('Ctrl Pts',(3.26416041699995,12.2,2.32137751999999));
#340104=CARTESIAN_POINT('Ctrl Pts',(3.26416041699995,5.2,2.32137751999999));
#340105=CARTESIAN_POINT('Ctrl Pts',(3.26416041699995,2.2,2.32137751999999));
#340106=CARTESIAN_POINT('Ctrl Pts',(3.26447176799994,12.2,2.32163734799999));
#340107=CARTESIAN_POINT('Ctrl Pts',(3.26447176799994,5.2,2.32163734799999));
#340108=CARTESIAN_POINT('Ctrl Pts',(3.26447176799994,2.2,2.32163734799999));
#340109=CARTESIAN_POINT('Ctrl Pts',(3.26478782799994,12.2,2.32190180699998));
#340110=CARTESIAN_POINT('Ctrl Pts',(3.26478782799994,5.2,2.32190180699998));
#340111=CARTESIAN_POINT('Ctrl Pts',(3.26478782799994,2.2,2.32190180699998));
#340112=CARTESIAN_POINT('Ctrl Pts',(3.26510857199994,12.2,2.32217090299998));
#340113=CARTESIAN_POINT('Ctrl Pts',(3.26510857199994,5.2,2.32217090299998));
#340114=CARTESIAN_POINT('Ctrl Pts',(3.26510857199994,2.2,2.32217090299998));
#340115=CARTESIAN_POINT('Ctrl Pts',(3.26543397999994,12.2,2.32244463899999));
#340116=CARTESIAN_POINT('Ctrl Pts',(3.26543397999994,5.2,2.32244463899999));
#340117=CARTESIAN_POINT('Ctrl Pts',(3.26543397999994,2.2,2.32244463899999));
#340118=CARTESIAN_POINT('Ctrl Pts',(3.26576402999994,12.2,2.32272301699998));
#340119=CARTESIAN_POINT('Ctrl Pts',(3.26576402999994,5.2,2.32272301699998));
#340120=CARTESIAN_POINT('Ctrl Pts',(3.26576402999994,2.2,2.32272301699998));
#340121=CARTESIAN_POINT('Ctrl Pts',(3.26609869999994,12.2,2.32300604199999));
#340122=CARTESIAN_POINT('Ctrl Pts',(3.26609869999994,5.2,2.32300604199999));
#340123=CARTESIAN_POINT('Ctrl Pts',(3.26609869999994,2.2,2.32300604199999));
#340124=CARTESIAN_POINT('Ctrl Pts',(3.26643796999994,12.2,2.32329371799999));
#340125=CARTESIAN_POINT('Ctrl Pts',(3.26643796999994,5.2,2.32329371799999));
#340126=CARTESIAN_POINT('Ctrl Pts',(3.26643796999994,2.2,2.32329371799999));
#340127=CARTESIAN_POINT('Ctrl Pts',(3.26678181699994,12.2,2.32358604899999));
#340128=CARTESIAN_POINT('Ctrl Pts',(3.26678181699994,5.2,2.32358604899999));
#340129=CARTESIAN_POINT('Ctrl Pts',(3.26678181699994,2.2,2.32358604899999));
#340130=CARTESIAN_POINT('Ctrl Pts',(3.26713022099994,12.2,2.32388303699999));
#340131=CARTESIAN_POINT('Ctrl Pts',(3.26713022099994,5.2,2.32388303699999));
#340132=CARTESIAN_POINT('Ctrl Pts',(3.26713022099994,2.2,2.32388303699999));
#340133=CARTESIAN_POINT('Ctrl Pts',(3.26748315999994,12.2,2.32418468699999));
#340134=CARTESIAN_POINT('Ctrl Pts',(3.26748315999994,5.2,2.32418468699999));
#340135=CARTESIAN_POINT('Ctrl Pts',(3.26748315999994,2.2,2.32418468699999));
#340136=CARTESIAN_POINT('Ctrl Pts',(3.26784061199994,12.2,2.32449100199998));
#340137=CARTESIAN_POINT('Ctrl Pts',(3.26784061199994,5.2,2.32449100199998));
#340138=CARTESIAN_POINT('Ctrl Pts',(3.26784061199994,2.2,2.32449100199998));
#340139=CARTESIAN_POINT('Ctrl Pts',(3.26820255799994,12.2,2.32480198599998));
#340140=CARTESIAN_POINT('Ctrl Pts',(3.26820255799994,5.2,2.32480198599998));
#340141=CARTESIAN_POINT('Ctrl Pts',(3.26820255799994,2.2,2.32480198599998));
#340142=CARTESIAN_POINT('Ctrl Pts',(3.26856897399994,12.2,2.32511764099999));
#340143=CARTESIAN_POINT('Ctrl Pts',(3.26856897399994,5.2,2.32511764099999));
#340144=CARTESIAN_POINT('Ctrl Pts',(3.26856897399994,2.2,2.32511764099999));
#340145=CARTESIAN_POINT('Ctrl Pts',(3.26893984099994,12.2,2.32543797099999));
#340146=CARTESIAN_POINT('Ctrl Pts',(3.26893984099994,5.2,2.32543797099999));
#340147=CARTESIAN_POINT('Ctrl Pts',(3.26893984099994,2.2,2.32543797099999));
#340148=CARTESIAN_POINT('Ctrl Pts',(3.26931513799994,12.2,2.32576297999998));
#340149=CARTESIAN_POINT('Ctrl Pts',(3.26931513799994,5.2,2.32576297999998));
#340150=CARTESIAN_POINT('Ctrl Pts',(3.26931513799994,2.2,2.32576297999998));
#340151=CARTESIAN_POINT('Ctrl Pts',(3.26969484299994,12.2,2.32609266999999));
#340152=CARTESIAN_POINT('Ctrl Pts',(3.26969484299994,5.2,2.32609266999999));
#340153=CARTESIAN_POINT('Ctrl Pts',(3.26969484299994,2.2,2.32609266999999));
#340154=CARTESIAN_POINT('Ctrl Pts',(3.27007893599994,12.2,2.32642704699999));
#340155=CARTESIAN_POINT('Ctrl Pts',(3.27007893599994,5.2,2.32642704699999));
#340156=CARTESIAN_POINT('Ctrl Pts',(3.27007893599994,2.2,2.32642704699999));
#340157=CARTESIAN_POINT('Ctrl Pts',(3.27046739699994,12.2,2.32676611099999));
#340158=CARTESIAN_POINT('Ctrl Pts',(3.27046739699994,5.2,2.32676611099999));
#340159=CARTESIAN_POINT('Ctrl Pts',(3.27046739699994,2.2,2.32676611099999));
#340160=CARTESIAN_POINT('Ctrl Pts',(3.27086020299994,12.2,2.32710986699999));
#340161=CARTESIAN_POINT('Ctrl Pts',(3.27086020299994,5.2,2.32710986699999));
#340162=CARTESIAN_POINT('Ctrl Pts',(3.27086020299994,2.2,2.32710986699999));
#340163=CARTESIAN_POINT('Ctrl Pts',(3.27125733499994,12.2,2.32745831799999));
#340164=CARTESIAN_POINT('Ctrl Pts',(3.27125733499994,5.2,2.32745831799999));
#340165=CARTESIAN_POINT('Ctrl Pts',(3.27125733499994,2.2,2.32745831799999));
#340166=CARTESIAN_POINT('Ctrl Pts',(3.27165877199994,12.2,2.32781146799999));
#340167=CARTESIAN_POINT('Ctrl Pts',(3.27165877199994,5.2,2.32781146799999));
#340168=CARTESIAN_POINT('Ctrl Pts',(3.27165877199994,2.2,2.32781146799999));
#340169=CARTESIAN_POINT('Ctrl Pts',(3.27206449399994,12.2,2.32816931799999));
#340170=CARTESIAN_POINT('Ctrl Pts',(3.27206449399994,5.2,2.32816931799999));
#340171=CARTESIAN_POINT('Ctrl Pts',(3.27206449399994,2.2,2.32816931799999));
#340172=CARTESIAN_POINT('Ctrl Pts',(3.27247447999994,12.2,2.32853187299999));
#340173=CARTESIAN_POINT('Ctrl Pts',(3.27247447999994,5.2,2.32853187299999));
#340174=CARTESIAN_POINT('Ctrl Pts',(3.27247447999994,2.2,2.32853187299999));
#340175=CARTESIAN_POINT('Ctrl Pts',(3.27288870899994,12.2,2.32889913399998));
#340176=CARTESIAN_POINT('Ctrl Pts',(3.27288870899994,5.2,2.32889913399998));
#340177=CARTESIAN_POINT('Ctrl Pts',(3.27288870899994,2.2,2.32889913399998));
#340178=CARTESIAN_POINT('Ctrl Pts',(3.27330716099994,12.2,2.32927110699999));
#340179=CARTESIAN_POINT('Ctrl Pts',(3.27330716099994,5.2,2.32927110699999));
#340180=CARTESIAN_POINT('Ctrl Pts',(3.27330716099994,2.2,2.32927110699999));
#340181=CARTESIAN_POINT('Ctrl Pts',(3.27372981699994,12.2,2.32964779199999));
#340182=CARTESIAN_POINT('Ctrl Pts',(3.27372981699994,5.2,2.32964779199999));
#340183=CARTESIAN_POINT('Ctrl Pts',(3.27372981699994,2.2,2.32964779199999));
#340184=CARTESIAN_POINT('Ctrl Pts',(3.27415665499994,12.2,2.33002919399999));
#340185=CARTESIAN_POINT('Ctrl Pts',(3.27415665499994,5.2,2.33002919399999));
#340186=CARTESIAN_POINT('Ctrl Pts',(3.27415665499994,2.2,2.33002919399999));
#340187=CARTESIAN_POINT('Ctrl Pts',(3.27458765499994,12.2,2.33041531599998));
#340188=CARTESIAN_POINT('Ctrl Pts',(3.27458765499994,5.2,2.33041531599998));
#340189=CARTESIAN_POINT('Ctrl Pts',(3.27458765499994,2.2,2.33041531599998));
#340190=CARTESIAN_POINT('Ctrl Pts',(3.27502279799994,12.2,2.33080615899999));
#340191=CARTESIAN_POINT('Ctrl Pts',(3.27502279799994,5.2,2.33080615899999));
#340192=CARTESIAN_POINT('Ctrl Pts',(3.27502279799994,2.2,2.33080615899999));
#340193=CARTESIAN_POINT('Ctrl Pts',(3.27546206299994,12.2,2.33120172699998));
#340194=CARTESIAN_POINT('Ctrl Pts',(3.27546206299994,5.2,2.33120172699998));
#340195=CARTESIAN_POINT('Ctrl Pts',(3.27546206299994,2.2,2.33120172699998));
#340196=CARTESIAN_POINT('Ctrl Pts',(3.27590543099994,12.2,2.33160202399999));
#340197=CARTESIAN_POINT('Ctrl Pts',(3.27590543099994,5.2,2.33160202399999));
#340198=CARTESIAN_POINT('Ctrl Pts',(3.27590543099994,2.2,2.33160202399999));
#340199=CARTESIAN_POINT('Ctrl Pts',(3.27635287999994,12.2,2.33200705099998));
#340200=CARTESIAN_POINT('Ctrl Pts',(3.27635287999994,5.2,2.33200705099998));
#340201=CARTESIAN_POINT('Ctrl Pts',(3.27635287999994,2.2,2.33200705099998));
#340202=CARTESIAN_POINT('Ctrl Pts',(3.27680439199994,12.2,2.33241680999999));
#340203=CARTESIAN_POINT('Ctrl Pts',(3.27680439199994,5.2,2.33241680999999));
#340204=CARTESIAN_POINT('Ctrl Pts',(3.27680439199994,2.2,2.33241680999999));
#340205=CARTESIAN_POINT('Ctrl Pts',(3.27725994699994,12.2,2.33283130599999));
#340206=CARTESIAN_POINT('Ctrl Pts',(3.27725994699994,5.2,2.33283130599999));
#340207=CARTESIAN_POINT('Ctrl Pts',(3.27725994699994,2.2,2.33283130599999));
#340208=CARTESIAN_POINT('Ctrl Pts',(3.27771952399994,12.2,2.33325054099998));
#340209=CARTESIAN_POINT('Ctrl Pts',(3.27771952399994,5.2,2.33325054099998));
#340210=CARTESIAN_POINT('Ctrl Pts',(3.27771952399994,2.2,2.33325054099998));
#340211=CARTESIAN_POINT('Ctrl Pts',(3.27818310399994,12.2,2.33367451799999));
#340212=CARTESIAN_POINT('Ctrl Pts',(3.27818310399994,5.2,2.33367451799999));
#340213=CARTESIAN_POINT('Ctrl Pts',(3.27818310399994,2.2,2.33367451799999));
#340214=CARTESIAN_POINT('Ctrl Pts',(3.27865066799994,12.2,2.33410323899998));
#340215=CARTESIAN_POINT('Ctrl Pts',(3.27865066799994,5.2,2.33410323899998));
#340216=CARTESIAN_POINT('Ctrl Pts',(3.27865066799994,2.2,2.33410323899998));
#340217=CARTESIAN_POINT('Ctrl Pts',(3.27912219499995,12.2,2.33453670599999));
#340218=CARTESIAN_POINT('Ctrl Pts',(3.27912219499995,5.2,2.33453670599999));
#340219=CARTESIAN_POINT('Ctrl Pts',(3.27912219499995,2.2,2.33453670599999));
#340220=CARTESIAN_POINT('Ctrl Pts',(3.27959766499994,12.2,2.33497492199998));
#340221=CARTESIAN_POINT('Ctrl Pts',(3.27959766499994,5.2,2.33497492199998));
#340222=CARTESIAN_POINT('Ctrl Pts',(3.27959766499994,2.2,2.33497492199998));
#340223=CARTESIAN_POINT('Ctrl Pts',(3.28007706199994,12.2,2.33541788999998));
#340224=CARTESIAN_POINT('Ctrl Pts',(3.28007706199994,5.2,2.33541788999998));
#340225=CARTESIAN_POINT('Ctrl Pts',(3.28007706199994,2.2,2.33541788999998));
#340226=CARTESIAN_POINT('Ctrl Pts',(3.28056036299994,12.2,2.33586561299999));
#340227=CARTESIAN_POINT('Ctrl Pts',(3.28056036299994,5.2,2.33586561299999));
#340228=CARTESIAN_POINT('Ctrl Pts',(3.28056036299994,2.2,2.33586561299999));
#340229=CARTESIAN_POINT('Ctrl Pts',(3.28104754899994,12.2,2.33631809299998));
#340230=CARTESIAN_POINT('Ctrl Pts',(3.28104754899994,5.2,2.33631809299998));
#340231=CARTESIAN_POINT('Ctrl Pts',(3.28104754899994,2.2,2.33631809299998));
#340232=CARTESIAN_POINT('Ctrl Pts',(3.28153860199994,12.2,2.33677533199999));
#340233=CARTESIAN_POINT('Ctrl Pts',(3.28153860199994,5.2,2.33677533199999));
#340234=CARTESIAN_POINT('Ctrl Pts',(3.28153860199994,2.2,2.33677533199999));
#340235=CARTESIAN_POINT('Ctrl Pts',(3.28203350199994,12.2,2.33723733099998));
#340236=CARTESIAN_POINT('Ctrl Pts',(3.28203350199994,5.2,2.33723733099998));
#340237=CARTESIAN_POINT('Ctrl Pts',(3.28203350199994,2.2,2.33723733099998));
#340238=CARTESIAN_POINT('Ctrl Pts',(3.28253222999995,12.2,2.33770409699999));
#340239=CARTESIAN_POINT('Ctrl Pts',(3.28253222999995,5.2,2.33770409699999));
#340240=CARTESIAN_POINT('Ctrl Pts',(3.28253222999995,2.2,2.33770409699999));
#340241=CARTESIAN_POINT('Ctrl Pts',(3.28303476599995,12.2,2.33817562699999));
#340242=CARTESIAN_POINT('Ctrl Pts',(3.28303476599995,5.2,2.33817562699999));
#340243=CARTESIAN_POINT('Ctrl Pts',(3.28303476599995,2.2,2.33817562699999));
#340244=CARTESIAN_POINT('Ctrl Pts',(3.28354109199994,12.2,2.33865192699998));
#340245=CARTESIAN_POINT('Ctrl Pts',(3.28354109199994,5.2,2.33865192699998));
#340246=CARTESIAN_POINT('Ctrl Pts',(3.28354109199994,2.2,2.33865192699998));
#340247=CARTESIAN_POINT('Ctrl Pts',(3.28405118799994,12.2,2.33913299699998));
#340248=CARTESIAN_POINT('Ctrl Pts',(3.28405118799994,5.2,2.33913299699998));
#340249=CARTESIAN_POINT('Ctrl Pts',(3.28405118799994,2.2,2.33913299699998));
#340250=CARTESIAN_POINT('Ctrl Pts',(3.28456503599994,12.2,2.33961884099998));
#340251=CARTESIAN_POINT('Ctrl Pts',(3.28456503599994,5.2,2.33961884099998));
#340252=CARTESIAN_POINT('Ctrl Pts',(3.28456503599994,2.2,2.33961884099998));
#340253=CARTESIAN_POINT('Ctrl Pts',(3.28508261599994,12.2,2.34010946099998));
#340254=CARTESIAN_POINT('Ctrl Pts',(3.28508261599994,5.2,2.34010946099998));
#340255=CARTESIAN_POINT('Ctrl Pts',(3.28508261599994,2.2,2.34010946099998));
#340256=CARTESIAN_POINT('Ctrl Pts',(3.28560390899994,12.2,2.34060485799999));
#340257=CARTESIAN_POINT('Ctrl Pts',(3.28560390899994,5.2,2.34060485799999));
#340258=CARTESIAN_POINT('Ctrl Pts',(3.28560390899994,2.2,2.34060485799999));
#340259=CARTESIAN_POINT('Ctrl Pts',(3.28612889699994,12.2,2.34110503599998));
#340260=CARTESIAN_POINT('Ctrl Pts',(3.28612889699994,5.2,2.34110503599998));
#340261=CARTESIAN_POINT('Ctrl Pts',(3.28612889699994,2.2,2.34110503599998));
#340262=CARTESIAN_POINT('Ctrl Pts',(3.28665755999995,12.2,2.34160999499998));
#340263=CARTESIAN_POINT('Ctrl Pts',(3.28665755999995,5.2,2.34160999499998));
#340264=CARTESIAN_POINT('Ctrl Pts',(3.28665755999995,2.2,2.34160999499998));
#340265=CARTESIAN_POINT('Ctrl Pts',(3.28718987999994,12.2,2.34211973899999));
#340266=CARTESIAN_POINT('Ctrl Pts',(3.28718987999994,5.2,2.34211973899999));
#340267=CARTESIAN_POINT('Ctrl Pts',(3.28718987999994,2.2,2.34211973899999));
#340268=CARTESIAN_POINT('Ctrl Pts',(3.28772583699994,12.2,2.34263426899998));
#340269=CARTESIAN_POINT('Ctrl Pts',(3.28772583699994,5.2,2.34263426899998));
#340270=CARTESIAN_POINT('Ctrl Pts',(3.28772583699994,2.2,2.34263426899998));
#340271=CARTESIAN_POINT('Ctrl Pts',(3.28826541599994,12.2,2.34315358699998));
#340272=CARTESIAN_POINT('Ctrl Pts',(3.28826541599994,5.2,2.34315358699998));
#340273=CARTESIAN_POINT('Ctrl Pts',(3.28826541599994,2.2,2.34315358699998));
#340274=CARTESIAN_POINT('Ctrl Pts',(3.28880859399994,12.2,2.34367769699999));
#340275=CARTESIAN_POINT('Ctrl Pts',(3.28880859399994,5.2,2.34367769699999));
#340276=CARTESIAN_POINT('Ctrl Pts',(3.28880859399994,2.2,2.34367769699999));
#340277=CARTESIAN_POINT('Ctrl Pts',(3.28935535399994,12.2,2.34420659699999));
#340278=CARTESIAN_POINT('Ctrl Pts',(3.28935535399994,5.2,2.34420659699999));
#340279=CARTESIAN_POINT('Ctrl Pts',(3.28935535399994,2.2,2.34420659699999));
#340280=CARTESIAN_POINT('Ctrl Pts',(3.28990567899994,12.2,2.34474029299998));
#340281=CARTESIAN_POINT('Ctrl Pts',(3.28990567899994,5.2,2.34474029299998));
#340282=CARTESIAN_POINT('Ctrl Pts',(3.28990567899994,2.2,2.34474029299998));
#340283=CARTESIAN_POINT('Ctrl Pts',(3.29045954899994,12.2,2.34527878499998));
#340284=CARTESIAN_POINT('Ctrl Pts',(3.29045954899994,5.2,2.34527878499998));
#340285=CARTESIAN_POINT('Ctrl Pts',(3.29045954899994,2.2,2.34527878499998));
#340286=CARTESIAN_POINT('Ctrl Pts',(3.29101694499994,12.2,2.34582207599999));
#340287=CARTESIAN_POINT('Ctrl Pts',(3.29101694499994,5.2,2.34582207599999));
#340288=CARTESIAN_POINT('Ctrl Pts',(3.29101694499994,2.2,2.34582207599999));
#340289=CARTESIAN_POINT('Ctrl Pts',(3.29157784999994,12.2,2.34637016699998));
#340290=CARTESIAN_POINT('Ctrl Pts',(3.29157784999994,5.2,2.34637016699998));
#340291=CARTESIAN_POINT('Ctrl Pts',(3.29157784999994,2.2,2.34637016699998));
#340292=CARTESIAN_POINT('Ctrl Pts',(3.29214224399994,12.2,2.34692305899999));
#340293=CARTESIAN_POINT('Ctrl Pts',(3.29214224399994,5.2,2.34692305899999));
#340294=CARTESIAN_POINT('Ctrl Pts',(3.29214224399994,2.2,2.34692305899999));
#340295=CARTESIAN_POINT('Ctrl Pts',(3.29271011099994,12.2,2.34748075599999));
#340296=CARTESIAN_POINT('Ctrl Pts',(3.29271011099994,5.2,2.34748075599999));
#340297=CARTESIAN_POINT('Ctrl Pts',(3.29271011099994,2.2,2.34748075599999));
#340298=CARTESIAN_POINT('Ctrl Pts',(3.29328143099994,12.2,2.34804325699999));
#340299=CARTESIAN_POINT('Ctrl Pts',(3.29328143099994,5.2,2.34804325699999));
#340300=CARTESIAN_POINT('Ctrl Pts',(3.29328143099994,2.2,2.34804325699999));
#340301=CARTESIAN_POINT('Ctrl Pts',(3.29385618599995,12.2,2.34861056699998));
#340302=CARTESIAN_POINT('Ctrl Pts',(3.29385618599995,5.2,2.34861056699998));
#340303=CARTESIAN_POINT('Ctrl Pts',(3.29385618599995,2.2,2.34861056699998));
#340304=CARTESIAN_POINT('Ctrl Pts',(3.29443435799994,12.2,2.34918268699998));
#340305=CARTESIAN_POINT('Ctrl Pts',(3.29443435799994,5.2,2.34918268699998));
#340306=CARTESIAN_POINT('Ctrl Pts',(3.29443435799994,2.2,2.34918268699998));
#340307=CARTESIAN_POINT('Ctrl Pts',(3.29501592899994,12.2,2.34975961699998));
#340308=CARTESIAN_POINT('Ctrl Pts',(3.29501592899994,5.2,2.34975961699998));
#340309=CARTESIAN_POINT('Ctrl Pts',(3.29501592899994,2.2,2.34975961699998));
#340310=CARTESIAN_POINT('Ctrl Pts',(3.29560088099994,12.2,2.35034135999998));
#340311=CARTESIAN_POINT('Ctrl Pts',(3.29560088099994,5.2,2.35034135999998));
#340312=CARTESIAN_POINT('Ctrl Pts',(3.29560088099994,2.2,2.35034135999998));
#340313=CARTESIAN_POINT('Ctrl Pts',(3.29618919699994,12.2,2.35092791599998));
#340314=CARTESIAN_POINT('Ctrl Pts',(3.29618919699994,5.2,2.35092791599998));
#340315=CARTESIAN_POINT('Ctrl Pts',(3.29618919699994,2.2,2.35092791599998));
#340316=CARTESIAN_POINT('Ctrl Pts',(3.29678085799994,12.2,2.35151928999999));
#340317=CARTESIAN_POINT('Ctrl Pts',(3.29678085799994,5.2,2.35151928999999));
#340318=CARTESIAN_POINT('Ctrl Pts',(3.29678085799994,2.2,2.35151928999999));
#340319=CARTESIAN_POINT('Ctrl Pts',(3.29737584499994,12.2,2.35211548099999));
#340320=CARTESIAN_POINT('Ctrl Pts',(3.29737584499994,5.2,2.35211548099999));
#340321=CARTESIAN_POINT('Ctrl Pts',(3.29737584499994,2.2,2.35211548099999));
#340322=CARTESIAN_POINT('Ctrl Pts',(3.29797414199994,12.2,2.35271649099998));
#340323=CARTESIAN_POINT('Ctrl Pts',(3.29797414199994,5.2,2.35271649099998));
#340324=CARTESIAN_POINT('Ctrl Pts',(3.29797414199994,2.2,2.35271649099998));
#340325=CARTESIAN_POINT('Ctrl Pts',(3.29857572899994,12.2,2.35332232199998));
#340326=CARTESIAN_POINT('Ctrl Pts',(3.29857572899994,5.2,2.35332232199998));
#340327=CARTESIAN_POINT('Ctrl Pts',(3.29857572899994,2.2,2.35332232199998));
#340328=CARTESIAN_POINT('Ctrl Pts',(3.29918059199994,12.2,2.35393297499999));
#340329=CARTESIAN_POINT('Ctrl Pts',(3.29918059199994,5.2,2.35393297499999));
#340330=CARTESIAN_POINT('Ctrl Pts',(3.29918059199994,2.2,2.35393297499999));
#340331=CARTESIAN_POINT('Ctrl Pts',(3.29978870899994,12.2,2.35454845199998));
#340332=CARTESIAN_POINT('Ctrl Pts',(3.29978870899994,5.2,2.35454845199998));
#340333=CARTESIAN_POINT('Ctrl Pts',(3.29978870899994,2.2,2.35454845199998));
#340334=CARTESIAN_POINT('Ctrl Pts',(3.30040006499994,12.2,2.35516875499999));
#340335=CARTESIAN_POINT('Ctrl Pts',(3.30040006499994,5.2,2.35516875499999));
#340336=CARTESIAN_POINT('Ctrl Pts',(3.30040006499994,2.2,2.35516875499999));
#340337=CARTESIAN_POINT('Ctrl Pts',(3.30101464199994,12.2,2.35579388399999));
#340338=CARTESIAN_POINT('Ctrl Pts',(3.30101464199994,5.2,2.35579388399999));
#340339=CARTESIAN_POINT('Ctrl Pts',(3.30101464199994,2.2,2.35579388399999));
#340340=CARTESIAN_POINT('Ctrl Pts',(3.30163242099994,12.2,2.35642384199998));
#340341=CARTESIAN_POINT('Ctrl Pts',(3.30163242099994,5.2,2.35642384199998));
#340342=CARTESIAN_POINT('Ctrl Pts',(3.30163242099994,2.2,2.35642384199998));
#340343=CARTESIAN_POINT('Ctrl Pts',(3.30225338599994,12.2,2.35705862899999));
#340344=CARTESIAN_POINT('Ctrl Pts',(3.30225338599994,5.2,2.35705862899999));
#340345=CARTESIAN_POINT('Ctrl Pts',(3.30225338599994,2.2,2.35705862899999));
#340346=CARTESIAN_POINT('Ctrl Pts',(3.30287751899994,12.2,2.35769824699998));
#340347=CARTESIAN_POINT('Ctrl Pts',(3.30287751899994,5.2,2.35769824699998));
#340348=CARTESIAN_POINT('Ctrl Pts',(3.30287751899994,2.2,2.35769824699998));
#340349=CARTESIAN_POINT('Ctrl Pts',(3.30350480199994,12.2,2.35834269899998));
#340350=CARTESIAN_POINT('Ctrl Pts',(3.30350480199994,5.2,2.35834269899998));
#340351=CARTESIAN_POINT('Ctrl Pts',(3.30350480199994,2.2,2.35834269899998));
#340352=CARTESIAN_POINT('Ctrl Pts',(3.30413521799994,12.2,2.35899198299999));
#340353=CARTESIAN_POINT('Ctrl Pts',(3.30413521799994,5.2,2.35899198299999));
#340354=CARTESIAN_POINT('Ctrl Pts',(3.30413521799994,2.2,2.35899198299999));
#340355=CARTESIAN_POINT('Ctrl Pts',(3.30476875099994,12.2,2.35964610299998));
#340356=CARTESIAN_POINT('Ctrl Pts',(3.30476875099994,5.2,2.35964610299998));
#340357=CARTESIAN_POINT('Ctrl Pts',(3.30476875099994,2.2,2.35964610299998));
#340358=CARTESIAN_POINT('Ctrl Pts',(3.30540538099994,12.2,2.36030505899999));
#340359=CARTESIAN_POINT('Ctrl Pts',(3.30540538099994,5.2,2.36030505899999));
#340360=CARTESIAN_POINT('Ctrl Pts',(3.30540538099994,2.2,2.36030505899999));
#340361=CARTESIAN_POINT('Ctrl Pts',(3.30604509299994,12.2,2.36096885299999));
#340362=CARTESIAN_POINT('Ctrl Pts',(3.30604509299994,5.2,2.36096885299999));
#340363=CARTESIAN_POINT('Ctrl Pts',(3.30604509299994,2.2,2.36096885299999));
#340364=CARTESIAN_POINT('Ctrl Pts',(3.30668786899994,12.2,2.36163748599999));
#340365=CARTESIAN_POINT('Ctrl Pts',(3.30668786899994,5.2,2.36163748599999));
#340366=CARTESIAN_POINT('Ctrl Pts',(3.30668786899994,2.2,2.36163748599999));
#340367=CARTESIAN_POINT('Ctrl Pts',(3.30733368999995,12.2,2.36231095899999));
#340368=CARTESIAN_POINT('Ctrl Pts',(3.30733368999995,5.2,2.36231095899999));
#340369=CARTESIAN_POINT('Ctrl Pts',(3.30733368999995,2.2,2.36231095899999));
#340370=CARTESIAN_POINT('Ctrl Pts',(3.30798254199994,12.2,2.36298927299998));
#340371=CARTESIAN_POINT('Ctrl Pts',(3.30798254199994,5.2,2.36298927299998));
#340372=CARTESIAN_POINT('Ctrl Pts',(3.30798254199994,2.2,2.36298927299998));
#340373=CARTESIAN_POINT('Ctrl Pts',(3.30863440599994,12.2,2.36367242999999));
#340374=CARTESIAN_POINT('Ctrl Pts',(3.30863440599994,5.2,2.36367242999999));
#340375=CARTESIAN_POINT('Ctrl Pts',(3.30863440599994,2.2,2.36367242999999));
#340376=CARTESIAN_POINT('Ctrl Pts',(3.30928926599994,12.2,2.36436042899999));
#340377=CARTESIAN_POINT('Ctrl Pts',(3.30928926599994,5.2,2.36436042899999));
#340378=CARTESIAN_POINT('Ctrl Pts',(3.30928926599994,2.2,2.36436042899999));
#340379=CARTESIAN_POINT('Ctrl Pts',(3.30994710299994,12.2,2.36505327499999));
#340380=CARTESIAN_POINT('Ctrl Pts',(3.30994710299994,5.2,2.36505327499999));
#340381=CARTESIAN_POINT('Ctrl Pts',(3.30994710299994,2.2,2.36505327499999));
#340382=CARTESIAN_POINT('Ctrl Pts',(3.31060790199994,12.2,2.36575096499998));
#340383=CARTESIAN_POINT('Ctrl Pts',(3.31060790199994,5.2,2.36575096499998));
#340384=CARTESIAN_POINT('Ctrl Pts',(3.31060790199994,2.2,2.36575096499998));
#340385=CARTESIAN_POINT('Ctrl Pts',(3.31127164499994,12.2,2.36645350299998));
#340386=CARTESIAN_POINT('Ctrl Pts',(3.31127164499994,5.2,2.36645350299998));
#340387=CARTESIAN_POINT('Ctrl Pts',(3.31127164499994,2.2,2.36645350299998));
#340388=CARTESIAN_POINT('Ctrl Pts',(3.31193831499994,12.2,2.36716088899998));
#340389=CARTESIAN_POINT('Ctrl Pts',(3.31193831499994,5.2,2.36716088899998));
#340390=CARTESIAN_POINT('Ctrl Pts',(3.31193831499994,2.2,2.36716088899998));
#340391=CARTESIAN_POINT('Ctrl Pts',(3.31260789699994,12.2,2.36787312299998));
#340392=CARTESIAN_POINT('Ctrl Pts',(3.31260789699994,5.2,2.36787312299998));
#340393=CARTESIAN_POINT('Ctrl Pts',(3.31260789699994,2.2,2.36787312299998));
#340394=CARTESIAN_POINT('Ctrl Pts',(3.31328037199994,12.2,2.36859020799999));
#340395=CARTESIAN_POINT('Ctrl Pts',(3.31328037199994,5.2,2.36859020799999));
#340396=CARTESIAN_POINT('Ctrl Pts',(3.31328037199994,2.2,2.36859020799999));
#340397=CARTESIAN_POINT('Ctrl Pts',(3.31395572399994,12.2,2.36931214299998));
#340398=CARTESIAN_POINT('Ctrl Pts',(3.31395572399994,5.2,2.36931214299998));
#340399=CARTESIAN_POINT('Ctrl Pts',(3.31395572399994,2.2,2.36931214299998));
#340400=CARTESIAN_POINT('Ctrl Pts',(3.31463393699994,12.2,2.37003892999999));
#340401=CARTESIAN_POINT('Ctrl Pts',(3.31463393699994,5.2,2.37003892999999));
#340402=CARTESIAN_POINT('Ctrl Pts',(3.31463393699994,2.2,2.37003892999999));
#340403=CARTESIAN_POINT('Ctrl Pts',(3.31531499199994,12.2,2.37077056999999));
#340404=CARTESIAN_POINT('Ctrl Pts',(3.31531499199994,5.2,2.37077056999999));
#340405=CARTESIAN_POINT('Ctrl Pts',(3.31531499199994,2.2,2.37077056999999));
#340406=CARTESIAN_POINT('Ctrl Pts',(3.31599887599995,12.2,2.37150706399999));
#340407=CARTESIAN_POINT('Ctrl Pts',(3.31599887599995,5.2,2.37150706399999));
#340408=CARTESIAN_POINT('Ctrl Pts',(3.31599887599995,2.2,2.37150706399999));
#340409=CARTESIAN_POINT('Ctrl Pts',(3.31668556899994,12.2,2.37224841199998));
#340410=CARTESIAN_POINT('Ctrl Pts',(3.31668556899994,5.2,2.37224841199998));
#340411=CARTESIAN_POINT('Ctrl Pts',(3.31668556899994,2.2,2.37224841199998));
#340412=CARTESIAN_POINT('Ctrl Pts',(3.31737505599994,12.2,2.37299461599999));
#340413=CARTESIAN_POINT('Ctrl Pts',(3.31737505599994,5.2,2.37299461599999));
#340414=CARTESIAN_POINT('Ctrl Pts',(3.31737505599994,2.2,2.37299461599999));
#340415=CARTESIAN_POINT('Ctrl Pts',(3.31806731999994,12.2,2.37374567499998));
#340416=CARTESIAN_POINT('Ctrl Pts',(3.31806731999994,5.2,2.37374567499998));
#340417=CARTESIAN_POINT('Ctrl Pts',(3.31806731999994,2.2,2.37374567499998));
#340418=CARTESIAN_POINT('Ctrl Pts',(3.31876234499994,12.2,2.37450159199999));
#340419=CARTESIAN_POINT('Ctrl Pts',(3.31876234499994,5.2,2.37450159199999));
#340420=CARTESIAN_POINT('Ctrl Pts',(3.31876234499994,2.2,2.37450159199999));
#340421=CARTESIAN_POINT('Ctrl Pts',(3.31946011499994,12.2,2.37526236699999));
#340422=CARTESIAN_POINT('Ctrl Pts',(3.31946011499994,5.2,2.37526236699999));
#340423=CARTESIAN_POINT('Ctrl Pts',(3.31946011499994,2.2,2.37526236699999));
#340424=CARTESIAN_POINT('Ctrl Pts',(3.32016061199994,12.2,2.37602799999999));
#340425=CARTESIAN_POINT('Ctrl Pts',(3.32016061199994,5.2,2.37602799999999));
#340426=CARTESIAN_POINT('Ctrl Pts',(3.32016061199994,2.2,2.37602799999999));
#340427=CARTESIAN_POINT('Ctrl Pts',(3.32086381999994,12.2,2.37679849299998));
#340428=CARTESIAN_POINT('Ctrl Pts',(3.32086381999994,5.2,2.37679849299998));
#340429=CARTESIAN_POINT('Ctrl Pts',(3.32086381999994,2.2,2.37679849299998));
#340430=CARTESIAN_POINT('Ctrl Pts',(3.32156972399994,12.2,2.37757384599998));
#340431=CARTESIAN_POINT('Ctrl Pts',(3.32156972399994,5.2,2.37757384599998));
#340432=CARTESIAN_POINT('Ctrl Pts',(3.32156972399994,2.2,2.37757384599998));
#340433=CARTESIAN_POINT('Ctrl Pts',(3.32227830699994,12.2,2.37835405899999));
#340434=CARTESIAN_POINT('Ctrl Pts',(3.32227830699994,5.2,2.37835405899999));
#340435=CARTESIAN_POINT('Ctrl Pts',(3.32227830699994,2.2,2.37835405899999));
#340436=CARTESIAN_POINT('Ctrl Pts',(3.32298955199994,12.2,2.37913913399999));
#340437=CARTESIAN_POINT('Ctrl Pts',(3.32298955199994,5.2,2.37913913399999));
#340438=CARTESIAN_POINT('Ctrl Pts',(3.32298955199994,2.2,2.37913913399999));
#340439=CARTESIAN_POINT('Ctrl Pts',(3.32370344499994,12.2,2.37992907099999));
#340440=CARTESIAN_POINT('Ctrl Pts',(3.32370344499994,5.2,2.37992907099999));
#340441=CARTESIAN_POINT('Ctrl Pts',(3.32370344499994,2.2,2.37992907099999));
#340442=CARTESIAN_POINT('Ctrl Pts',(3.32441996699994,12.2,2.38072386999999));
#340443=CARTESIAN_POINT('Ctrl Pts',(3.32441996699994,5.2,2.38072386999999));
#340444=CARTESIAN_POINT('Ctrl Pts',(3.32441996699994,2.2,2.38072386999999));
#340445=CARTESIAN_POINT('Ctrl Pts',(3.32513910199994,12.2,2.38152353399999));
#340446=CARTESIAN_POINT('Ctrl Pts',(3.32513910199994,5.2,2.38152353399999));
#340447=CARTESIAN_POINT('Ctrl Pts',(3.32513910199994,2.2,2.38152353399999));
#340448=CARTESIAN_POINT('Ctrl Pts',(3.32586083699994,12.2,2.38232805999999));
#340449=CARTESIAN_POINT('Ctrl Pts',(3.32586083699994,5.2,2.38232805999999));
#340450=CARTESIAN_POINT('Ctrl Pts',(3.32586083699994,2.2,2.38232805999999));
#340451=CARTESIAN_POINT('Ctrl Pts',(3.32658515399994,12.2,2.38313745099998));
#340452=CARTESIAN_POINT('Ctrl Pts',(3.32658515399994,5.2,2.38313745099998));
#340453=CARTESIAN_POINT('Ctrl Pts',(3.32658515399994,2.2,2.38313745099998));
#340454=CARTESIAN_POINT('Ctrl Pts',(3.32731203599994,12.2,2.38395170799999));
#340455=CARTESIAN_POINT('Ctrl Pts',(3.32731203599994,5.2,2.38395170799999));
#340456=CARTESIAN_POINT('Ctrl Pts',(3.32731203599994,2.2,2.38395170799999));
#340457=CARTESIAN_POINT('Ctrl Pts',(3.32804146799994,12.2,2.38477082899998));
#340458=CARTESIAN_POINT('Ctrl Pts',(3.32804146799994,5.2,2.38477082899998));
#340459=CARTESIAN_POINT('Ctrl Pts',(3.32804146799994,2.2,2.38477082899998));
#340460=CARTESIAN_POINT('Ctrl Pts',(3.32877343399994,12.2,2.38559481699999));
#340461=CARTESIAN_POINT('Ctrl Pts',(3.32877343399994,5.2,2.38559481699999));
#340462=CARTESIAN_POINT('Ctrl Pts',(3.32877343399994,2.2,2.38559481699999));
#340463=CARTESIAN_POINT('Ctrl Pts',(3.32950791799994,12.2,2.38642367099998));
#340464=CARTESIAN_POINT('Ctrl Pts',(3.32950791799994,5.2,2.38642367099998));
#340465=CARTESIAN_POINT('Ctrl Pts',(3.32950791799994,2.2,2.38642367099998));
#340466=CARTESIAN_POINT('Ctrl Pts',(3.33024490499994,12.2,2.38725739199998));
#340467=CARTESIAN_POINT('Ctrl Pts',(3.33024490499994,5.2,2.38725739199998));
#340468=CARTESIAN_POINT('Ctrl Pts',(3.33024490499994,2.2,2.38725739199998));
#340469=CARTESIAN_POINT('Ctrl Pts',(3.33098437699994,12.2,2.38809598099999));
#340470=CARTESIAN_POINT('Ctrl Pts',(3.33098437699994,5.2,2.38809598099999));
#340471=CARTESIAN_POINT('Ctrl Pts',(3.33098437699994,2.2,2.38809598099999));
#340472=CARTESIAN_POINT('Ctrl Pts',(3.33172632099994,12.2,2.38893943699999));
#340473=CARTESIAN_POINT('Ctrl Pts',(3.33172632099994,5.2,2.38893943699999));
#340474=CARTESIAN_POINT('Ctrl Pts',(3.33172632099994,2.2,2.38893943699999));
#340475=CARTESIAN_POINT('Ctrl Pts',(3.33247071999994,12.2,2.38978775999998));
#340476=CARTESIAN_POINT('Ctrl Pts',(3.33247071999994,5.2,2.38978775999998));
#340477=CARTESIAN_POINT('Ctrl Pts',(3.33247071999994,2.2,2.38978775999998));
#340478=CARTESIAN_POINT('Ctrl Pts',(3.33321755799994,12.2,2.39064095399999));
#340479=CARTESIAN_POINT('Ctrl Pts',(3.33321755799994,5.2,2.39064095399999));
#340480=CARTESIAN_POINT('Ctrl Pts',(3.33321755799994,2.2,2.39064095399999));
#340481=CARTESIAN_POINT('Ctrl Pts',(3.33396681799994,12.2,2.39149901499999));
#340482=CARTESIAN_POINT('Ctrl Pts',(3.33396681799994,5.2,2.39149901499999));
#340483=CARTESIAN_POINT('Ctrl Pts',(3.33396681799994,2.2,2.39149901499999));
#340484=CARTESIAN_POINT('Ctrl Pts',(3.33471848799994,12.2,2.39236194599999));
#340485=CARTESIAN_POINT('Ctrl Pts',(3.33471848799994,5.2,2.39236194599999));
#340486=CARTESIAN_POINT('Ctrl Pts',(3.33471848799994,2.2,2.39236194599999));
#340487=CARTESIAN_POINT('Ctrl Pts',(3.33547254899994,12.2,2.39322974699999));
#340488=CARTESIAN_POINT('Ctrl Pts',(3.33547254899994,5.2,2.39322974699999));
#340489=CARTESIAN_POINT('Ctrl Pts',(3.33547254899994,2.2,2.39322974699999));
#340490=CARTESIAN_POINT('Ctrl Pts',(3.33622898699995,12.2,2.39410241599998));
#340491=CARTESIAN_POINT('Ctrl Pts',(3.33622898699995,5.2,2.39410241599998));
#340492=CARTESIAN_POINT('Ctrl Pts',(3.33622898699995,2.2,2.39410241599998));
#340493=CARTESIAN_POINT('Ctrl Pts',(3.33698778599994,12.2,2.39497995699999));
#340494=CARTESIAN_POINT('Ctrl Pts',(3.33698778599994,5.2,2.39497995699999));
#340495=CARTESIAN_POINT('Ctrl Pts',(3.33698778599994,2.2,2.39497995699999));
#340496=CARTESIAN_POINT('Ctrl Pts',(3.33774892999994,12.2,2.39586236699999));
#340497=CARTESIAN_POINT('Ctrl Pts',(3.33774892999994,5.2,2.39586236699999));
#340498=CARTESIAN_POINT('Ctrl Pts',(3.33774892999994,2.2,2.39586236699999));
#340499=CARTESIAN_POINT('Ctrl Pts',(3.33851240499994,12.2,2.39674964699999));
#340500=CARTESIAN_POINT('Ctrl Pts',(3.33851240499994,5.2,2.39674964699999));
#340501=CARTESIAN_POINT('Ctrl Pts',(3.33851240499994,2.2,2.39674964699999));
#340502=CARTESIAN_POINT('Ctrl Pts',(3.33927819399995,12.2,2.39764179899999));
#340503=CARTESIAN_POINT('Ctrl Pts',(3.33927819399995,5.2,2.39764179899999));
#340504=CARTESIAN_POINT('Ctrl Pts',(3.33927819399995,2.2,2.39764179899999));
#340505=CARTESIAN_POINT('Ctrl Pts',(3.34004628199994,12.2,2.39853882099998));
#340506=CARTESIAN_POINT('Ctrl Pts',(3.34004628199994,5.2,2.39853882099998));
#340507=CARTESIAN_POINT('Ctrl Pts',(3.34004628199994,2.2,2.39853882099998));
#340508=CARTESIAN_POINT('Ctrl Pts',(3.34081665599995,12.2,2.39944071499998));
#340509=CARTESIAN_POINT('Ctrl Pts',(3.34081665599995,5.2,2.39944071499998));
#340510=CARTESIAN_POINT('Ctrl Pts',(3.34081665599995,2.2,2.39944071499998));
#340511=CARTESIAN_POINT('Ctrl Pts',(3.34158929699994,12.2,2.40034747899998));
#340512=CARTESIAN_POINT('Ctrl Pts',(3.34158929699994,5.2,2.40034747899998));
#340513=CARTESIAN_POINT('Ctrl Pts',(3.34158929699994,2.2,2.40034747899998));
#340514=CARTESIAN_POINT('Ctrl Pts',(3.34236419099994,12.2,2.40125911499998));
#340515=CARTESIAN_POINT('Ctrl Pts',(3.34236419099994,5.2,2.40125911499998));
#340516=CARTESIAN_POINT('Ctrl Pts',(3.34236419099994,2.2,2.40125911499998));
#340517=CARTESIAN_POINT('Ctrl Pts',(3.34314132399995,12.2,2.40217562199999));
#340518=CARTESIAN_POINT('Ctrl Pts',(3.34314132399995,5.2,2.40217562199999));
#340519=CARTESIAN_POINT('Ctrl Pts',(3.34314132399995,2.2,2.40217562199999));
#340520=CARTESIAN_POINT('Ctrl Pts',(3.34392067899994,12.2,2.40309700199998));
#340521=CARTESIAN_POINT('Ctrl Pts',(3.34392067899994,5.2,2.40309700199998));
#340522=CARTESIAN_POINT('Ctrl Pts',(3.34392067899994,2.2,2.40309700199998));
#340523=CARTESIAN_POINT('Ctrl Pts',(3.34470224199995,12.2,2.40402325199998));
#340524=CARTESIAN_POINT('Ctrl Pts',(3.34470224199995,5.2,2.40402325199998));
#340525=CARTESIAN_POINT('Ctrl Pts',(3.34470224199995,2.2,2.40402325199998));
#340526=CARTESIAN_POINT('Ctrl Pts',(3.34548599799994,12.2,2.40495437299998));
#340527=CARTESIAN_POINT('Ctrl Pts',(3.34548599799994,5.2,2.40495437299998));
#340528=CARTESIAN_POINT('Ctrl Pts',(3.34548599799994,2.2,2.40495437299998));
#340529=CARTESIAN_POINT('Ctrl Pts',(3.34627193199994,12.2,2.40589036699999));
#340530=CARTESIAN_POINT('Ctrl Pts',(3.34627193199994,5.2,2.40589036699999));
#340531=CARTESIAN_POINT('Ctrl Pts',(3.34627193199994,2.2,2.40589036699999));
#340532=CARTESIAN_POINT('Ctrl Pts',(3.34706002699994,12.2,2.40683123199998));
#340533=CARTESIAN_POINT('Ctrl Pts',(3.34706002699994,5.2,2.40683123199998));
#340534=CARTESIAN_POINT('Ctrl Pts',(3.34706002699994,2.2,2.40683123199998));
#340535=CARTESIAN_POINT('Ctrl Pts',(3.34785027099994,12.2,2.40777696799999));
#340536=CARTESIAN_POINT('Ctrl Pts',(3.34785027099994,5.2,2.40777696799999));
#340537=CARTESIAN_POINT('Ctrl Pts',(3.34785027099994,2.2,2.40777696799999));
#340538=CARTESIAN_POINT('Ctrl Pts',(3.34864264599994,12.2,2.40872757599998));
#340539=CARTESIAN_POINT('Ctrl Pts',(3.34864264599994,5.2,2.40872757599998));
#340540=CARTESIAN_POINT('Ctrl Pts',(3.34864264599994,2.2,2.40872757599998));
#340541=CARTESIAN_POINT('Ctrl Pts',(3.34943713899994,12.2,2.40968305499998));
#340542=CARTESIAN_POINT('Ctrl Pts',(3.34943713899994,5.2,2.40968305499998));
#340543=CARTESIAN_POINT('Ctrl Pts',(3.34943713899994,2.2,2.40968305499998));
#340544=CARTESIAN_POINT('Ctrl Pts',(3.35023373399994,12.2,2.41064340599999));
#340545=CARTESIAN_POINT('Ctrl Pts',(3.35023373399994,5.2,2.41064340599999));
#340546=CARTESIAN_POINT('Ctrl Pts',(3.35023373399994,2.2,2.41064340599999));
#340547=CARTESIAN_POINT('Ctrl Pts',(3.35103241699994,12.2,2.41160862899999));
#340548=CARTESIAN_POINT('Ctrl Pts',(3.35103241699994,5.2,2.41160862899999));
#340549=CARTESIAN_POINT('Ctrl Pts',(3.35103241699994,2.2,2.41160862899999));
#340550=CARTESIAN_POINT('Ctrl Pts',(3.35183317199995,12.2,2.41257872199999));
#340551=CARTESIAN_POINT('Ctrl Pts',(3.35183317199995,5.2,2.41257872199999));
#340552=CARTESIAN_POINT('Ctrl Pts',(3.35183317199995,2.2,2.41257872199999));
#340553=CARTESIAN_POINT('Ctrl Pts',(3.35263598499994,12.2,2.41355368599999));
#340554=CARTESIAN_POINT('Ctrl Pts',(3.35263598499994,5.2,2.41355368599999));
#340555=CARTESIAN_POINT('Ctrl Pts',(3.35263598499994,2.2,2.41355368599999));
#340556=CARTESIAN_POINT('Ctrl Pts',(3.35344084099995,12.2,2.41453352099998));
#340557=CARTESIAN_POINT('Ctrl Pts',(3.35344084099995,5.2,2.41453352099998));
#340558=CARTESIAN_POINT('Ctrl Pts',(3.35344084099995,2.2,2.41453352099998));
#340559=CARTESIAN_POINT('Ctrl Pts',(3.35424772499994,12.2,2.41551822699999));
#340560=CARTESIAN_POINT('Ctrl Pts',(3.35424772499994,5.2,2.41551822699999));
#340561=CARTESIAN_POINT('Ctrl Pts',(3.35424772499994,2.2,2.41551822699999));
#340562=CARTESIAN_POINT('Ctrl Pts',(3.35505662299994,12.2,2.41650780399999));
#340563=CARTESIAN_POINT('Ctrl Pts',(3.35505662299994,5.2,2.41650780399999));
#340564=CARTESIAN_POINT('Ctrl Pts',(3.35505662299994,2.2,2.41650780399999));
#340565=CARTESIAN_POINT('Ctrl Pts',(3.35586751999994,12.2,2.41750225099998));
#340566=CARTESIAN_POINT('Ctrl Pts',(3.35586751999994,5.2,2.41750225099998));
#340567=CARTESIAN_POINT('Ctrl Pts',(3.35586751999994,2.2,2.41750225099998));
#340568=CARTESIAN_POINT('Ctrl Pts',(3.35668039999995,12.2,2.41850156699999));
#340569=CARTESIAN_POINT('Ctrl Pts',(3.35668039999995,5.2,2.41850156699999));
#340570=CARTESIAN_POINT('Ctrl Pts',(3.35668039999995,2.2,2.41850156699999));
#340571=CARTESIAN_POINT('Ctrl Pts',(3.35749524999994,12.2,2.41950575399999));
#340572=CARTESIAN_POINT('Ctrl Pts',(3.35749524999994,5.2,2.41950575399999));
#340573=CARTESIAN_POINT('Ctrl Pts',(3.35749524999994,2.2,2.41950575399999));
#340574=CARTESIAN_POINT('Ctrl Pts',(3.35831205499994,12.2,2.42051480999999));
#340575=CARTESIAN_POINT('Ctrl Pts',(3.35831205499994,5.2,2.42051480999999));
#340576=CARTESIAN_POINT('Ctrl Pts',(3.35831205499994,2.2,2.42051480999999));
#340577=CARTESIAN_POINT('Ctrl Pts',(3.35913079999994,12.2,2.42152873599998));
#340578=CARTESIAN_POINT('Ctrl Pts',(3.35913079999994,5.2,2.42152873599998));
#340579=CARTESIAN_POINT('Ctrl Pts',(3.35913079999994,2.2,2.42152873599998));
#340580=CARTESIAN_POINT('Ctrl Pts',(3.35995147099994,12.2,2.42254753099999));
#340581=CARTESIAN_POINT('Ctrl Pts',(3.35995147099994,5.2,2.42254753099999));
#340582=CARTESIAN_POINT('Ctrl Pts',(3.35995147099994,2.2,2.42254753099999));
#340583=CARTESIAN_POINT('Ctrl Pts',(3.36077405299994,12.2,2.42357119399998));
#340584=CARTESIAN_POINT('Ctrl Pts',(3.36077405299994,5.2,2.42357119399998));
#340585=CARTESIAN_POINT('Ctrl Pts',(3.36077405299994,2.2,2.42357119399998));
#340586=CARTESIAN_POINT('Ctrl Pts',(3.36159853199994,12.2,2.42459972499999));
#340587=CARTESIAN_POINT('Ctrl Pts',(3.36159853199994,5.2,2.42459972499999));
#340588=CARTESIAN_POINT('Ctrl Pts',(3.36159853199994,2.2,2.42459972499999));
#340589=CARTESIAN_POINT('Ctrl Pts',(3.36242489299994,12.2,2.42563312399999));
#340590=CARTESIAN_POINT('Ctrl Pts',(3.36242489299994,5.2,2.42563312399999));
#340591=CARTESIAN_POINT('Ctrl Pts',(3.36242489299994,2.2,2.42563312399999));
#340592=CARTESIAN_POINT('Ctrl Pts',(3.36325312199994,12.2,2.42667139099999));
#340593=CARTESIAN_POINT('Ctrl Pts',(3.36325312199994,5.2,2.42667139099999));
#340594=CARTESIAN_POINT('Ctrl Pts',(3.36325312199994,2.2,2.42667139099999));
#340595=CARTESIAN_POINT('Ctrl Pts',(3.36408320499994,12.2,2.42771452499999));
#340596=CARTESIAN_POINT('Ctrl Pts',(3.36408320499994,5.2,2.42771452499999));
#340597=CARTESIAN_POINT('Ctrl Pts',(3.36408320499994,2.2,2.42771452499999));
#340598=CARTESIAN_POINT('Ctrl Pts',(3.36491512599994,12.2,2.42876252599999));
#340599=CARTESIAN_POINT('Ctrl Pts',(3.36491512599994,5.2,2.42876252599999));
#340600=CARTESIAN_POINT('Ctrl Pts',(3.36491512599994,2.2,2.42876252599999));
#340601=CARTESIAN_POINT('Ctrl Pts',(3.36574887299995,12.2,2.42981539299999));
#340602=CARTESIAN_POINT('Ctrl Pts',(3.36574887299995,5.2,2.42981539299999));
#340603=CARTESIAN_POINT('Ctrl Pts',(3.36574887299995,2.2,2.42981539299999));
#340604=CARTESIAN_POINT('Ctrl Pts',(3.36658442999994,12.2,2.43087312599998));
#340605=CARTESIAN_POINT('Ctrl Pts',(3.36658442999994,5.2,2.43087312599998));
#340606=CARTESIAN_POINT('Ctrl Pts',(3.36658442999994,2.2,2.43087312599998));
#340607=CARTESIAN_POINT('Ctrl Pts',(3.36742178299994,12.2,2.43193572399999));
#340608=CARTESIAN_POINT('Ctrl Pts',(3.36742178299994,5.2,2.43193572399999));
#340609=CARTESIAN_POINT('Ctrl Pts',(3.36742178299994,2.2,2.43193572399999));
#340610=CARTESIAN_POINT('Ctrl Pts',(3.36826091899994,12.2,2.43300318699998));
#340611=CARTESIAN_POINT('Ctrl Pts',(3.36826091899994,5.2,2.43300318699998));
#340612=CARTESIAN_POINT('Ctrl Pts',(3.36826091899994,2.2,2.43300318699998));
#340613=CARTESIAN_POINT('Ctrl Pts',(3.36910182099994,12.2,2.43407551499998));
#340614=CARTESIAN_POINT('Ctrl Pts',(3.36910182099994,5.2,2.43407551499998));
#340615=CARTESIAN_POINT('Ctrl Pts',(3.36910182099994,2.2,2.43407551499998));
#340616=CARTESIAN_POINT('Ctrl Pts',(3.36994447899994,12.2,2.43515270699999));
#340617=CARTESIAN_POINT('Ctrl Pts',(3.36994447899994,5.2,2.43515270699999));
#340618=CARTESIAN_POINT('Ctrl Pts',(3.36994447899994,2.2,2.43515270699999));
#340619=CARTESIAN_POINT('Ctrl Pts',(3.37078887499994,12.2,2.43623476199998));
#340620=CARTESIAN_POINT('Ctrl Pts',(3.37078887499994,5.2,2.43623476199998));
#340621=CARTESIAN_POINT('Ctrl Pts',(3.37078887499994,2.2,2.43623476199998));
#340622=CARTESIAN_POINT('Ctrl Pts',(3.37163499699995,12.2,2.43732167999998));
#340623=CARTESIAN_POINT('Ctrl Pts',(3.37163499699995,5.2,2.43732167999998));
#340624=CARTESIAN_POINT('Ctrl Pts',(3.37163499699995,2.2,2.43732167999998));
#340625=CARTESIAN_POINT('Ctrl Pts',(3.37248283099994,12.2,2.43841345999999));
#340626=CARTESIAN_POINT('Ctrl Pts',(3.37248283099994,5.2,2.43841345999999));
#340627=CARTESIAN_POINT('Ctrl Pts',(3.37248283099994,2.2,2.43841345999999));
#340628=CARTESIAN_POINT('Ctrl Pts',(3.37333236099994,12.2,2.43951010199999));
#340629=CARTESIAN_POINT('Ctrl Pts',(3.37333236099994,5.2,2.43951010199999));
#340630=CARTESIAN_POINT('Ctrl Pts',(3.37333236099994,2.2,2.43951010199999));
#340631=CARTESIAN_POINT('Ctrl Pts',(3.37418357599995,12.2,2.44061160399998));
#340632=CARTESIAN_POINT('Ctrl Pts',(3.37418357599995,5.2,2.44061160399998));
#340633=CARTESIAN_POINT('Ctrl Pts',(3.37418357599995,2.2,2.44061160399998));
#340634=CARTESIAN_POINT('Ctrl Pts',(3.37503645899994,12.2,2.44171796699998));
#340635=CARTESIAN_POINT('Ctrl Pts',(3.37503645899994,5.2,2.44171796699998));
#340636=CARTESIAN_POINT('Ctrl Pts',(3.37503645899994,2.2,2.44171796699998));
#340637=CARTESIAN_POINT('Ctrl Pts',(3.37589099799994,12.2,2.44282918999998));
#340638=CARTESIAN_POINT('Ctrl Pts',(3.37589099799994,5.2,2.44282918999998));
#340639=CARTESIAN_POINT('Ctrl Pts',(3.37589099799994,2.2,2.44282918999998));
#340640=CARTESIAN_POINT('Ctrl Pts',(3.37674717799994,12.2,2.44394527199999));
#340641=CARTESIAN_POINT('Ctrl Pts',(3.37674717799994,5.2,2.44394527199999));
#340642=CARTESIAN_POINT('Ctrl Pts',(3.37674717799994,2.2,2.44394527199999));
#340643=CARTESIAN_POINT('Ctrl Pts',(3.37760498599994,12.2,2.44506621199999));
#340644=CARTESIAN_POINT('Ctrl Pts',(3.37760498599994,5.2,2.44506621199999));
#340645=CARTESIAN_POINT('Ctrl Pts',(3.37760498599994,2.2,2.44506621199999));
#340646=CARTESIAN_POINT('Ctrl Pts',(3.37846440799995,12.2,2.44619201099999));
#340647=CARTESIAN_POINT('Ctrl Pts',(3.37846440799995,5.2,2.44619201099999));
#340648=CARTESIAN_POINT('Ctrl Pts',(3.37846440799995,2.2,2.44619201099999));
#340649=CARTESIAN_POINT('Ctrl Pts',(3.37932542999994,12.2,2.44732266599998));
#340650=CARTESIAN_POINT('Ctrl Pts',(3.37932542999994,5.2,2.44732266599998));
#340651=CARTESIAN_POINT('Ctrl Pts',(3.37932542999994,2.2,2.44732266599998));
#340652=CARTESIAN_POINT('Ctrl Pts',(3.38018803799994,12.2,2.44845817699999));
#340653=CARTESIAN_POINT('Ctrl Pts',(3.38018803799994,5.2,2.44845817699999));
#340654=CARTESIAN_POINT('Ctrl Pts',(3.38018803799994,2.2,2.44845817699999));
#340655=CARTESIAN_POINT('Ctrl Pts',(3.38105221899994,12.2,2.44959854399998));
#340656=CARTESIAN_POINT('Ctrl Pts',(3.38105221899994,5.2,2.44959854399998));
#340657=CARTESIAN_POINT('Ctrl Pts',(3.38105221899994,2.2,2.44959854399998));
#340658=CARTESIAN_POINT('Ctrl Pts',(3.38191795799994,12.2,2.45074376599998));
#340659=CARTESIAN_POINT('Ctrl Pts',(3.38191795799994,5.2,2.45074376599998));
#340660=CARTESIAN_POINT('Ctrl Pts',(3.38191795799994,2.2,2.45074376599998));
#340661=CARTESIAN_POINT('Ctrl Pts',(3.38278524199994,12.2,2.45189384199998));
#340662=CARTESIAN_POINT('Ctrl Pts',(3.38278524199994,5.2,2.45189384199998));
#340663=CARTESIAN_POINT('Ctrl Pts',(3.38278524199994,2.2,2.45189384199998));
#340664=CARTESIAN_POINT('Ctrl Pts',(3.38365405699995,12.2,2.45304877099999));
#340665=CARTESIAN_POINT('Ctrl Pts',(3.38365405699995,5.2,2.45304877099999));
#340666=CARTESIAN_POINT('Ctrl Pts',(3.38365405699995,2.2,2.45304877099999));
#340667=CARTESIAN_POINT('Ctrl Pts',(3.38452438999994,12.2,2.45420855199999));
#340668=CARTESIAN_POINT('Ctrl Pts',(3.38452438999994,5.2,2.45420855199999));
#340669=CARTESIAN_POINT('Ctrl Pts',(3.38452438999994,2.2,2.45420855199999));
#340670=CARTESIAN_POINT('Ctrl Pts',(3.38539622699995,12.2,2.45537318499998));
#340671=CARTESIAN_POINT('Ctrl Pts',(3.38539622699995,5.2,2.45537318499998));
#340672=CARTESIAN_POINT('Ctrl Pts',(3.38539622699995,2.2,2.45537318499998));
#340673=CARTESIAN_POINT('Ctrl Pts',(3.38626955399994,12.2,2.45654266899999));
#340674=CARTESIAN_POINT('Ctrl Pts',(3.38626955399994,5.2,2.45654266899999));
#340675=CARTESIAN_POINT('Ctrl Pts',(3.38626955399994,2.2,2.45654266899999));
#340676=CARTESIAN_POINT('Ctrl Pts',(3.38714435899994,12.2,2.45771700299999));
#340677=CARTESIAN_POINT('Ctrl Pts',(3.38714435899994,5.2,2.45771700299999));
#340678=CARTESIAN_POINT('Ctrl Pts',(3.38714435899994,2.2,2.45771700299999));
#340679=CARTESIAN_POINT('Ctrl Pts',(3.38802062599994,12.2,2.45889618499999));
#340680=CARTESIAN_POINT('Ctrl Pts',(3.38802062599994,5.2,2.45889618499999));
#340681=CARTESIAN_POINT('Ctrl Pts',(3.38802062599994,2.2,2.45889618499999));
#340682=CARTESIAN_POINT('Ctrl Pts',(3.38889834299994,12.2,2.46008021599998));
#340683=CARTESIAN_POINT('Ctrl Pts',(3.38889834299994,5.2,2.46008021599998));
#340684=CARTESIAN_POINT('Ctrl Pts',(3.38889834299994,2.2,2.46008021599998));
#340685=CARTESIAN_POINT('Ctrl Pts',(3.38977749699994,12.2,2.46126909299999));
#340686=CARTESIAN_POINT('Ctrl Pts',(3.38977749699994,5.2,2.46126909299999));
#340687=CARTESIAN_POINT('Ctrl Pts',(3.38977749699994,2.2,2.46126909299999));
#340688=CARTESIAN_POINT('Ctrl Pts',(3.39065807299994,12.2,2.46246281799999));
#340689=CARTESIAN_POINT('Ctrl Pts',(3.39065807299994,5.2,2.46246281799999));
#340690=CARTESIAN_POINT('Ctrl Pts',(3.39065807299994,2.2,2.46246281799999));
#340691=CARTESIAN_POINT('Ctrl Pts',(3.39154005999994,12.2,2.46366138699998));
#340692=CARTESIAN_POINT('Ctrl Pts',(3.39154005999994,5.2,2.46366138699998));
#340693=CARTESIAN_POINT('Ctrl Pts',(3.39154005999994,2.2,2.46366138699998));
#340694=CARTESIAN_POINT('Ctrl Pts',(3.39242344199994,12.2,2.46486480199999));
#340695=CARTESIAN_POINT('Ctrl Pts',(3.39242344199994,5.2,2.46486480199999));
#340696=CARTESIAN_POINT('Ctrl Pts',(3.39242344199994,2.2,2.46486480199999));
#340697=CARTESIAN_POINT('Ctrl Pts',(3.39330820699994,12.2,2.46607305899998));
#340698=CARTESIAN_POINT('Ctrl Pts',(3.39330820699994,5.2,2.46607305899998));
#340699=CARTESIAN_POINT('Ctrl Pts',(3.39330820699994,2.2,2.46607305899998));
#340700=CARTESIAN_POINT('Ctrl Pts',(3.39419434099994,12.2,2.46728615799999));
#340701=CARTESIAN_POINT('Ctrl Pts',(3.39419434099994,5.2,2.46728615799999));
#340702=CARTESIAN_POINT('Ctrl Pts',(3.39419434099994,2.2,2.46728615799999));
#340703=CARTESIAN_POINT('Ctrl Pts',(3.39508183099994,12.2,2.46850409999999));
#340704=CARTESIAN_POINT('Ctrl Pts',(3.39508183099994,5.2,2.46850409999999));
#340705=CARTESIAN_POINT('Ctrl Pts',(3.39508183099994,2.2,2.46850409999999));
#340706=CARTESIAN_POINT('Ctrl Pts',(3.39597066499994,12.2,2.46972688099999));
#340707=CARTESIAN_POINT('Ctrl Pts',(3.39597066499994,5.2,2.46972688099999));
#340708=CARTESIAN_POINT('Ctrl Pts',(3.39597066499994,2.2,2.46972688099999));
#340709=CARTESIAN_POINT('Ctrl Pts',(3.39686082699994,12.2,2.47095450299998));
#340710=CARTESIAN_POINT('Ctrl Pts',(3.39686082699994,5.2,2.47095450299998));
#340711=CARTESIAN_POINT('Ctrl Pts',(3.39686082699994,2.2,2.47095450299998));
#340712=CARTESIAN_POINT('Ctrl Pts',(3.39775230599995,12.2,2.47218696199998));
#340713=CARTESIAN_POINT('Ctrl Pts',(3.39775230599995,5.2,2.47218696199998));
#340714=CARTESIAN_POINT('Ctrl Pts',(3.39775230599995,2.2,2.47218696199998));
#340715=CARTESIAN_POINT('Ctrl Pts',(3.39864508699995,12.2,2.47342425899999));
#340716=CARTESIAN_POINT('Ctrl Pts',(3.39864508699995,5.2,2.47342425899999));
#340717=CARTESIAN_POINT('Ctrl Pts',(3.39864508699995,2.2,2.47342425899999));
#340718=CARTESIAN_POINT('Ctrl Pts',(3.39953915999994,12.2,2.47466639199998));
#340719=CARTESIAN_POINT('Ctrl Pts',(3.39953915999994,5.2,2.47466639199998));
#340720=CARTESIAN_POINT('Ctrl Pts',(3.39953915999994,2.2,2.47466639199998));
#340721=CARTESIAN_POINT('Ctrl Pts',(3.40043450899994,12.2,2.47591335999999));
#340722=CARTESIAN_POINT('Ctrl Pts',(3.40043450899994,5.2,2.47591335999999));
#340723=CARTESIAN_POINT('Ctrl Pts',(3.40043450899994,2.2,2.47591335999999));
#340724=CARTESIAN_POINT('Ctrl Pts',(3.40133112099994,12.2,2.47716516099998));
#340725=CARTESIAN_POINT('Ctrl Pts',(3.40133112099994,5.2,2.47716516099998));
#340726=CARTESIAN_POINT('Ctrl Pts',(3.40133112099994,2.2,2.47716516099998));
#340727=CARTESIAN_POINT('Ctrl Pts',(3.40222898499994,12.2,2.47842179599999));
#340728=CARTESIAN_POINT('Ctrl Pts',(3.40222898499994,5.2,2.47842179599999));
#340729=CARTESIAN_POINT('Ctrl Pts',(3.40222898499994,2.2,2.47842179599999));
#340730=CARTESIAN_POINT('Ctrl Pts',(3.40312808599994,12.2,2.47968326199998));
#340731=CARTESIAN_POINT('Ctrl Pts',(3.40312808599994,5.2,2.47968326199998));
#340732=CARTESIAN_POINT('Ctrl Pts',(3.40312808599994,2.2,2.47968326199998));
#340733=CARTESIAN_POINT('Ctrl Pts',(3.40402841099994,12.2,2.48094955899998));
#340734=CARTESIAN_POINT('Ctrl Pts',(3.40402841099994,5.2,2.48094955899998));
#340735=CARTESIAN_POINT('Ctrl Pts',(3.40402841099994,2.2,2.48094955899998));
#340736=CARTESIAN_POINT('Ctrl Pts',(3.40492994799994,12.2,2.48222068499998));
#340737=CARTESIAN_POINT('Ctrl Pts',(3.40492994799994,5.2,2.48222068499998));
#340738=CARTESIAN_POINT('Ctrl Pts',(3.40492994799994,2.2,2.48222068499998));
#340739=CARTESIAN_POINT('Ctrl Pts',(3.40583268299994,12.2,2.48349663999999));
#340740=CARTESIAN_POINT('Ctrl Pts',(3.40583268299994,5.2,2.48349663999999));
#340741=CARTESIAN_POINT('Ctrl Pts',(3.40583268299994,2.2,2.48349663999999));
#340742=CARTESIAN_POINT('Ctrl Pts',(3.40673660499994,12.2,2.48477742199999));
#340743=CARTESIAN_POINT('Ctrl Pts',(3.40673660499994,5.2,2.48477742199999));
#340744=CARTESIAN_POINT('Ctrl Pts',(3.40673660499994,2.2,2.48477742199999));
#340745=CARTESIAN_POINT('Ctrl Pts',(3.40764169899994,12.2,2.48606302799999));
#340746=CARTESIAN_POINT('Ctrl Pts',(3.40764169899994,5.2,2.48606302799999));
#340747=CARTESIAN_POINT('Ctrl Pts',(3.40764169899994,2.2,2.48606302799999));
#340748=CARTESIAN_POINT('Ctrl Pts',(3.40854795299995,12.2,2.48735345999999));
#340749=CARTESIAN_POINT('Ctrl Pts',(3.40854795299995,5.2,2.48735345999999));
#340750=CARTESIAN_POINT('Ctrl Pts',(3.40854795299995,2.2,2.48735345999999));
#340751=CARTESIAN_POINT('Ctrl Pts',(3.40945535399995,12.2,2.48864871499999));
#340752=CARTESIAN_POINT('Ctrl Pts',(3.40945535399995,5.2,2.48864871499999));
#340753=CARTESIAN_POINT('Ctrl Pts',(3.40945535399995,2.2,2.48864871499999));
#340754=CARTESIAN_POINT('Ctrl Pts',(3.41036388799994,12.2,2.48994879199999));
#340755=CARTESIAN_POINT('Ctrl Pts',(3.41036388799994,5.2,2.48994879199999));
#340756=CARTESIAN_POINT('Ctrl Pts',(3.41036388799994,2.2,2.48994879199999));
#340757=CARTESIAN_POINT('Ctrl Pts',(3.41127354499994,12.2,2.49125368899998));
#340758=CARTESIAN_POINT('Ctrl Pts',(3.41127354499994,5.2,2.49125368899998));
#340759=CARTESIAN_POINT('Ctrl Pts',(3.41127354499994,2.2,2.49125368899998));
#340760=CARTESIAN_POINT('Ctrl Pts',(3.41218430899994,12.2,2.49256340699999));
#340761=CARTESIAN_POINT('Ctrl Pts',(3.41218430899994,5.2,2.49256340699999));
#340762=CARTESIAN_POINT('Ctrl Pts',(3.41218430899994,2.2,2.49256340699999));
#340763=CARTESIAN_POINT('Ctrl Pts',(3.41309616999995,12.2,2.49387794199999));
#340764=CARTESIAN_POINT('Ctrl Pts',(3.41309616999995,5.2,2.49387794199999));
#340765=CARTESIAN_POINT('Ctrl Pts',(3.41309616999995,2.2,2.49387794199999));
#340766=CARTESIAN_POINT('Ctrl Pts',(3.41400911399994,12.2,2.49519729399999));
#340767=CARTESIAN_POINT('Ctrl Pts',(3.41400911399994,5.2,2.49519729399999));
#340768=CARTESIAN_POINT('Ctrl Pts',(3.41400911399994,2.2,2.49519729399999));
#340769=CARTESIAN_POINT('Ctrl Pts',(3.41492312799994,12.2,2.49652146199999));
#340770=CARTESIAN_POINT('Ctrl Pts',(3.41492312799994,5.2,2.49652146199999));
#340771=CARTESIAN_POINT('Ctrl Pts',(3.41492312799994,2.2,2.49652146199999));
#340772=CARTESIAN_POINT('Ctrl Pts',(3.41583819899994,12.2,2.49785044399999));
#340773=CARTESIAN_POINT('Ctrl Pts',(3.41583819899994,5.2,2.49785044399999));
#340774=CARTESIAN_POINT('Ctrl Pts',(3.41583819899994,2.2,2.49785044399999));
#340775=CARTESIAN_POINT('Ctrl Pts',(3.41675431499994,12.2,2.49918423799999));
#340776=CARTESIAN_POINT('Ctrl Pts',(3.41675431499994,5.2,2.49918423799999));
#340777=CARTESIAN_POINT('Ctrl Pts',(3.41675431499994,2.2,2.49918423799999));
#340778=CARTESIAN_POINT('Ctrl Pts',(3.41767146399994,12.2,2.50052284399998));
#340779=CARTESIAN_POINT('Ctrl Pts',(3.41767146399994,5.2,2.50052284399998));
#340780=CARTESIAN_POINT('Ctrl Pts',(3.41767146399994,2.2,2.50052284399998));
#340781=CARTESIAN_POINT('Ctrl Pts',(3.41858963299994,12.2,2.50186625899998));
#340782=CARTESIAN_POINT('Ctrl Pts',(3.41858963299994,5.2,2.50186625899998));
#340783=CARTESIAN_POINT('Ctrl Pts',(3.41858963299994,2.2,2.50186625899998));
#340784=CARTESIAN_POINT('Ctrl Pts',(3.41950880899994,12.2,2.50321448399998));
#340785=CARTESIAN_POINT('Ctrl Pts',(3.41950880899994,5.2,2.50321448399998));
#340786=CARTESIAN_POINT('Ctrl Pts',(3.41950880899994,2.2,2.50321448399998));
#340787=CARTESIAN_POINT('Ctrl Pts',(3.42042897899994,12.2,2.50456751499998));
#340788=CARTESIAN_POINT('Ctrl Pts',(3.42042897899994,5.2,2.50456751499998));
#340789=CARTESIAN_POINT('Ctrl Pts',(3.42042897899994,2.2,2.50456751499998));
#340790=CARTESIAN_POINT('Ctrl Pts',(3.42135013199994,12.2,2.50592535199999));
#340791=CARTESIAN_POINT('Ctrl Pts',(3.42135013199994,5.2,2.50592535199999));
#340792=CARTESIAN_POINT('Ctrl Pts',(3.42135013199994,2.2,2.50592535199999));
#340793=CARTESIAN_POINT('Ctrl Pts',(3.42227225299994,12.2,2.50728799399998));
#340794=CARTESIAN_POINT('Ctrl Pts',(3.42227225299994,5.2,2.50728799399998));
#340795=CARTESIAN_POINT('Ctrl Pts',(3.42227225299994,2.2,2.50728799399998));
#340796=CARTESIAN_POINT('Ctrl Pts',(3.42319533199994,12.2,2.50865543899998));
#340797=CARTESIAN_POINT('Ctrl Pts',(3.42319533199994,5.2,2.50865543899998));
#340798=CARTESIAN_POINT('Ctrl Pts',(3.42319533199994,2.2,2.50865543899998));
#340799=CARTESIAN_POINT('Ctrl Pts',(3.42411935599995,12.2,2.51002768399999));
#340800=CARTESIAN_POINT('Ctrl Pts',(3.42411935599995,5.2,2.51002768399999));
#340801=CARTESIAN_POINT('Ctrl Pts',(3.42411935599995,2.2,2.51002768399999));
#340802=CARTESIAN_POINT('Ctrl Pts',(3.42504431299994,12.2,2.51140472999998));
#340803=CARTESIAN_POINT('Ctrl Pts',(3.42504431299994,5.2,2.51140472999998));
#340804=CARTESIAN_POINT('Ctrl Pts',(3.42504431299994,2.2,2.51140472999998));
#340805=CARTESIAN_POINT('Ctrl Pts',(3.42597018799994,12.2,2.51278657299999));
#340806=CARTESIAN_POINT('Ctrl Pts',(3.42597018799994,5.2,2.51278657299999));
#340807=CARTESIAN_POINT('Ctrl Pts',(3.42597018799994,2.2,2.51278657299999));
#340808=CARTESIAN_POINT('Ctrl Pts',(3.42689697199994,12.2,2.51417321299999));
#340809=CARTESIAN_POINT('Ctrl Pts',(3.42689697199994,5.2,2.51417321299999));
#340810=CARTESIAN_POINT('Ctrl Pts',(3.42689697199994,2.2,2.51417321299999));
#340811=CARTESIAN_POINT('Ctrl Pts',(3.42782465099994,12.2,2.51556464999998));
#340812=CARTESIAN_POINT('Ctrl Pts',(3.42782465099994,5.2,2.51556464999998));
#340813=CARTESIAN_POINT('Ctrl Pts',(3.42782465099994,2.2,2.51556464999998));
#340814=CARTESIAN_POINT('Ctrl Pts',(3.42875321299994,12.2,2.51696087899998));
#340815=CARTESIAN_POINT('Ctrl Pts',(3.42875321299994,5.2,2.51696087899998));
#340816=CARTESIAN_POINT('Ctrl Pts',(3.42875321299994,2.2,2.51696087899998));
#340817=CARTESIAN_POINT('Ctrl Pts',(3.42968264399994,12.2,2.51836190099999));
#340818=CARTESIAN_POINT('Ctrl Pts',(3.42968264399994,5.2,2.51836190099999));
#340819=CARTESIAN_POINT('Ctrl Pts',(3.42968264399994,2.2,2.51836190099999));
#340820=CARTESIAN_POINT('Ctrl Pts',(3.43061293499995,12.2,2.51976771299999));
#340821=CARTESIAN_POINT('Ctrl Pts',(3.43061293499995,5.2,2.51976771299999));
#340822=CARTESIAN_POINT('Ctrl Pts',(3.43061293499995,2.2,2.51976771299999));
#340823=CARTESIAN_POINT('Ctrl Pts',(3.43154406999994,12.2,2.52117831499999));
#340824=CARTESIAN_POINT('Ctrl Pts',(3.43154406999994,5.2,2.52117831499999));
#340825=CARTESIAN_POINT('Ctrl Pts',(3.43154406999994,2.2,2.52117831499999));
#340826=CARTESIAN_POINT('Ctrl Pts',(3.43247603999994,12.2,2.52259370399998));
#340827=CARTESIAN_POINT('Ctrl Pts',(3.43247603999994,5.2,2.52259370399998));
#340828=CARTESIAN_POINT('Ctrl Pts',(3.43247603999994,2.2,2.52259370399998));
#340829=CARTESIAN_POINT('Ctrl Pts',(3.43340883199994,12.2,2.52401387799999));
#340830=CARTESIAN_POINT('Ctrl Pts',(3.43340883199994,5.2,2.52401387799999));
#340831=CARTESIAN_POINT('Ctrl Pts',(3.43340883199994,2.2,2.52401387799999));
#340832=CARTESIAN_POINT('Ctrl Pts',(3.43434243299995,12.2,2.52543883599999));
#340833=CARTESIAN_POINT('Ctrl Pts',(3.43434243299995,5.2,2.52543883599999));
#340834=CARTESIAN_POINT('Ctrl Pts',(3.43434243299995,2.2,2.52543883599999));
#340835=CARTESIAN_POINT('Ctrl Pts',(3.43527682999994,12.2,2.52686857799999));
#340836=CARTESIAN_POINT('Ctrl Pts',(3.43527682999994,5.2,2.52686857799999));
#340837=CARTESIAN_POINT('Ctrl Pts',(3.43527682999994,2.2,2.52686857799999));
#340838=CARTESIAN_POINT('Ctrl Pts',(3.43621201299994,12.2,2.52830309999998));
#340839=CARTESIAN_POINT('Ctrl Pts',(3.43621201299994,5.2,2.52830309999998));
#340840=CARTESIAN_POINT('Ctrl Pts',(3.43621201299994,2.2,2.52830309999998));
#340841=CARTESIAN_POINT('Ctrl Pts',(3.43714796899994,12.2,2.52974240099999));
#340842=CARTESIAN_POINT('Ctrl Pts',(3.43714796899994,5.2,2.52974240099999));
#340843=CARTESIAN_POINT('Ctrl Pts',(3.43714796899994,2.2,2.52974240099999));
#340844=CARTESIAN_POINT('Ctrl Pts',(3.43808468699994,12.2,2.53118647999998));
#340845=CARTESIAN_POINT('Ctrl Pts',(3.43808468699994,5.2,2.53118647999998));
#340846=CARTESIAN_POINT('Ctrl Pts',(3.43808468699994,2.2,2.53118647999998));
#340847=CARTESIAN_POINT('Ctrl Pts',(3.43902215299994,12.2,2.53263533399998));
#340848=CARTESIAN_POINT('Ctrl Pts',(3.43902215299994,5.2,2.53263533399998));
#340849=CARTESIAN_POINT('Ctrl Pts',(3.43902215299994,2.2,2.53263533399998));
#340850=CARTESIAN_POINT('Ctrl Pts',(3.43996035499994,12.2,2.53408896199999));
#340851=CARTESIAN_POINT('Ctrl Pts',(3.43996035499994,5.2,2.53408896199999));
#340852=CARTESIAN_POINT('Ctrl Pts',(3.43996035499994,2.2,2.53408896199999));
#340853=CARTESIAN_POINT('Ctrl Pts',(3.44089928299995,12.2,2.53554736299999));
#340854=CARTESIAN_POINT('Ctrl Pts',(3.44089928299995,5.2,2.53554736299999));
#340855=CARTESIAN_POINT('Ctrl Pts',(3.44089928299995,2.2,2.53554736299999));
#340856=CARTESIAN_POINT('Ctrl Pts',(3.44183892399994,12.2,2.53701053499999));
#340857=CARTESIAN_POINT('Ctrl Pts',(3.44183892399994,5.2,2.53701053499999));
#340858=CARTESIAN_POINT('Ctrl Pts',(3.44183892399994,2.2,2.53701053499999));
#340859=CARTESIAN_POINT('Ctrl Pts',(3.44277926599994,12.2,2.53847847499999));
#340860=CARTESIAN_POINT('Ctrl Pts',(3.44277926599994,5.2,2.53847847499999));
#340861=CARTESIAN_POINT('Ctrl Pts',(3.44277926599994,2.2,2.53847847499999));
#340862=CARTESIAN_POINT('Ctrl Pts',(3.44372029599994,12.2,2.53995118299999));
#340863=CARTESIAN_POINT('Ctrl Pts',(3.44372029599994,5.2,2.53995118299999));
#340864=CARTESIAN_POINT('Ctrl Pts',(3.44372029599994,2.2,2.53995118299999));
#340865=CARTESIAN_POINT('Ctrl Pts',(3.44466200399994,12.2,2.54142865499999));
#340866=CARTESIAN_POINT('Ctrl Pts',(3.44466200399994,5.2,2.54142865499999));
#340867=CARTESIAN_POINT('Ctrl Pts',(3.44466200399994,2.2,2.54142865499999));
#340868=CARTESIAN_POINT('Ctrl Pts',(3.44560437599994,12.2,2.54291089099999));
#340869=CARTESIAN_POINT('Ctrl Pts',(3.44560437599994,5.2,2.54291089099999));
#340870=CARTESIAN_POINT('Ctrl Pts',(3.44560437599994,2.2,2.54291089099999));
#340871=CARTESIAN_POINT('Ctrl Pts',(3.44654740199994,12.2,2.54439788899998));
#340872=CARTESIAN_POINT('Ctrl Pts',(3.44654740199994,5.2,2.54439788899998));
#340873=CARTESIAN_POINT('Ctrl Pts',(3.44654740199994,2.2,2.54439788899998));
#340874=CARTESIAN_POINT('Ctrl Pts',(3.44749106999994,12.2,2.54588964799999));
#340875=CARTESIAN_POINT('Ctrl Pts',(3.44749106999994,5.2,2.54588964799999));
#340876=CARTESIAN_POINT('Ctrl Pts',(3.44749106999994,2.2,2.54588964799999));
#340877=CARTESIAN_POINT('Ctrl Pts',(3.44843536699994,12.2,2.54738616399998));
#340878=CARTESIAN_POINT('Ctrl Pts',(3.44843536699994,5.2,2.54738616399998));
#340879=CARTESIAN_POINT('Ctrl Pts',(3.44843536699994,2.2,2.54738616399998));
#340880=CARTESIAN_POINT('Ctrl Pts',(3.44938028199994,12.2,2.54888743599999));
#340881=CARTESIAN_POINT('Ctrl Pts',(3.44938028199994,5.2,2.54888743599999));
#340882=CARTESIAN_POINT('Ctrl Pts',(3.44938028199994,2.2,2.54888743599999));
#340883=CARTESIAN_POINT('Ctrl Pts',(3.45032580399995,12.2,2.55039346299998));
#340884=CARTESIAN_POINT('Ctrl Pts',(3.45032580399995,5.2,2.55039346299998));
#340885=CARTESIAN_POINT('Ctrl Pts',(3.45032580399995,2.2,2.55039346299998));
#340886=CARTESIAN_POINT('Ctrl Pts',(3.45127191899994,12.2,2.55190424299998));
#340887=CARTESIAN_POINT('Ctrl Pts',(3.45127191899994,5.2,2.55190424299998));
#340888=CARTESIAN_POINT('Ctrl Pts',(3.45127191899994,2.2,2.55190424299998));
#340889=CARTESIAN_POINT('Ctrl Pts',(3.45221861799994,12.2,2.55341977199999));
#340890=CARTESIAN_POINT('Ctrl Pts',(3.45221861799994,5.2,2.55341977199999));
#340891=CARTESIAN_POINT('Ctrl Pts',(3.45221861799994,2.2,2.55341977199999));
#340892=CARTESIAN_POINT('Ctrl Pts',(3.45316588699994,12.2,2.55494005199999));
#340893=CARTESIAN_POINT('Ctrl Pts',(3.45316588699994,5.2,2.55494005199999));
#340894=CARTESIAN_POINT('Ctrl Pts',(3.45316588699994,2.2,2.55494005199999));
#340895=CARTESIAN_POINT('Ctrl Pts',(3.45411371499994,12.2,2.55646507699999));
#340896=CARTESIAN_POINT('Ctrl Pts',(3.45411371499994,5.2,2.55646507699999));
#340897=CARTESIAN_POINT('Ctrl Pts',(3.45411371499994,2.2,2.55646507699999));
#340898=CARTESIAN_POINT('Ctrl Pts',(3.45506209099995,12.2,2.55799484799999));
#340899=CARTESIAN_POINT('Ctrl Pts',(3.45506209099995,5.2,2.55799484799999));
#340900=CARTESIAN_POINT('Ctrl Pts',(3.45506209099995,2.2,2.55799484799999));
#340901=CARTESIAN_POINT('Ctrl Pts',(3.45601100299994,12.2,2.55952936199999));
#340902=CARTESIAN_POINT('Ctrl Pts',(3.45601100299994,5.2,2.55952936199999));
#340903=CARTESIAN_POINT('Ctrl Pts',(3.45601100299994,2.2,2.55952936199999));
#340904=CARTESIAN_POINT('Ctrl Pts',(3.45696043999994,12.2,2.56106861699998));
#340905=CARTESIAN_POINT('Ctrl Pts',(3.45696043999994,5.2,2.56106861699998));
#340906=CARTESIAN_POINT('Ctrl Pts',(3.45696043999994,2.2,2.56106861699998));
#340907=CARTESIAN_POINT('Ctrl Pts',(3.45791038899995,12.2,2.56261261099999));
#340908=CARTESIAN_POINT('Ctrl Pts',(3.45791038899995,5.2,2.56261261099999));
#340909=CARTESIAN_POINT('Ctrl Pts',(3.45791038899995,2.2,2.56261261099999));
#340910=CARTESIAN_POINT('Ctrl Pts',(3.45886083999994,12.2,2.56416134199998));
#340911=CARTESIAN_POINT('Ctrl Pts',(3.45886083999994,5.2,2.56416134199998));
#340912=CARTESIAN_POINT('Ctrl Pts',(3.45886083999994,2.2,2.56416134199998));
#340913=CARTESIAN_POINT('Ctrl Pts',(3.45981177999994,12.2,2.56571480799998));
#340914=CARTESIAN_POINT('Ctrl Pts',(3.45981177999994,5.2,2.56571480799998));
#340915=CARTESIAN_POINT('Ctrl Pts',(3.45981177999994,2.2,2.56571480799998));
#340916=CARTESIAN_POINT('Ctrl Pts',(3.46076319899994,12.2,2.56727300699998));
#340917=CARTESIAN_POINT('Ctrl Pts',(3.46076319899994,5.2,2.56727300699998));
#340918=CARTESIAN_POINT('Ctrl Pts',(3.46076319899994,2.2,2.56727300699998));
#340919=CARTESIAN_POINT('Ctrl Pts',(3.46171508399994,12.2,2.56883593899998));
#340920=CARTESIAN_POINT('Ctrl Pts',(3.46171508399994,5.2,2.56883593899998));
#340921=CARTESIAN_POINT('Ctrl Pts',(3.46171508399994,2.2,2.56883593899998));
#340922=CARTESIAN_POINT('Ctrl Pts',(3.46266742399994,12.2,2.57040359899998));
#340923=CARTESIAN_POINT('Ctrl Pts',(3.46266742399994,5.2,2.57040359899998));
#340924=CARTESIAN_POINT('Ctrl Pts',(3.46266742399994,2.2,2.57040359899998));
#340925=CARTESIAN_POINT('Ctrl Pts',(3.46362020899994,12.2,2.57197598599999));
#340926=CARTESIAN_POINT('Ctrl Pts',(3.46362020899994,5.2,2.57197598599999));
#340927=CARTESIAN_POINT('Ctrl Pts',(3.46362020899994,2.2,2.57197598599999));
#340928=CARTESIAN_POINT('Ctrl Pts',(3.46457342599995,12.2,2.57355309899998));
#340929=CARTESIAN_POINT('Ctrl Pts',(3.46457342599995,5.2,2.57355309899998));
#340930=CARTESIAN_POINT('Ctrl Pts',(3.46457342599995,2.2,2.57355309899998));
#340931=CARTESIAN_POINT('Ctrl Pts',(3.46552706299994,12.2,2.57513493299999));
#340932=CARTESIAN_POINT('Ctrl Pts',(3.46552706299994,5.2,2.57513493299999));
#340933=CARTESIAN_POINT('Ctrl Pts',(3.46552706299994,2.2,2.57513493299999));
#340934=CARTESIAN_POINT('Ctrl Pts',(3.46648111099995,12.2,2.57672148999998));
#340935=CARTESIAN_POINT('Ctrl Pts',(3.46648111099995,5.2,2.57672148999998));
#340936=CARTESIAN_POINT('Ctrl Pts',(3.46648111099995,2.2,2.57672148999998));
#340937=CARTESIAN_POINT('Ctrl Pts',(3.46743555599994,12.2,2.57831276599998));
#340938=CARTESIAN_POINT('Ctrl Pts',(3.46743555599994,5.2,2.57831276599998));
#340939=CARTESIAN_POINT('Ctrl Pts',(3.46743555599994,2.2,2.57831276599998));
#340940=CARTESIAN_POINT('Ctrl Pts',(3.46839038799994,12.2,2.57990875799998));
#340941=CARTESIAN_POINT('Ctrl Pts',(3.46839038799994,5.2,2.57990875799998));
#340942=CARTESIAN_POINT('Ctrl Pts',(3.46839038799994,2.2,2.57990875799998));
#340943=CARTESIAN_POINT('Ctrl Pts',(3.46934559599994,12.2,2.58150946499998));
#340944=CARTESIAN_POINT('Ctrl Pts',(3.46934559599994,5.2,2.58150946499998));
#340945=CARTESIAN_POINT('Ctrl Pts',(3.46934559599994,2.2,2.58150946499998));
#340946=CARTESIAN_POINT('Ctrl Pts',(3.47030116899994,12.2,2.58311488399999));
#340947=CARTESIAN_POINT('Ctrl Pts',(3.47030116899994,5.2,2.58311488399999));
#340948=CARTESIAN_POINT('Ctrl Pts',(3.47030116899994,2.2,2.58311488399999));
#340949=CARTESIAN_POINT('Ctrl Pts',(3.47125709399994,12.2,2.58472501499998));
#340950=CARTESIAN_POINT('Ctrl Pts',(3.47125709399994,5.2,2.58472501499998));
#340951=CARTESIAN_POINT('Ctrl Pts',(3.47125709399994,2.2,2.58472501499998));
#340952=CARTESIAN_POINT('Ctrl Pts',(3.47221336199994,12.2,2.58633985299999));
#340953=CARTESIAN_POINT('Ctrl Pts',(3.47221336199994,5.2,2.58633985299999));
#340954=CARTESIAN_POINT('Ctrl Pts',(3.47221336199994,2.2,2.58633985299999));
#340955=CARTESIAN_POINT('Ctrl Pts',(3.47316995899994,12.2,2.58795939899999));
#340956=CARTESIAN_POINT('Ctrl Pts',(3.47316995899994,5.2,2.58795939899999));
#340957=CARTESIAN_POINT('Ctrl Pts',(3.47316995899994,2.2,2.58795939899999));
#340958=CARTESIAN_POINT('Ctrl Pts',(3.47412687699994,12.2,2.58958364799999));
#340959=CARTESIAN_POINT('Ctrl Pts',(3.47412687699994,5.2,2.58958364799999));
#340960=CARTESIAN_POINT('Ctrl Pts',(3.47412687699994,2.2,2.58958364799999));
#340961=CARTESIAN_POINT('Ctrl Pts',(3.47508410099994,12.2,2.59121259899998));
#340962=CARTESIAN_POINT('Ctrl Pts',(3.47508410099994,5.2,2.59121259899998));
#340963=CARTESIAN_POINT('Ctrl Pts',(3.47508410099994,2.2,2.59121259899998));
#340964=CARTESIAN_POINT('Ctrl Pts',(3.47604162499994,12.2,2.59284624899998));
#340965=CARTESIAN_POINT('Ctrl Pts',(3.47604162499994,5.2,2.59284624899998));
#340966=CARTESIAN_POINT('Ctrl Pts',(3.47604162499994,2.2,2.59284624899998));
#340967=CARTESIAN_POINT('Ctrl Pts',(3.47699943199994,12.2,2.59448459699998));
#340968=CARTESIAN_POINT('Ctrl Pts',(3.47699943199994,5.2,2.59448459699998));
#340969=CARTESIAN_POINT('Ctrl Pts',(3.47699943199994,2.2,2.59448459699998));
#340970=CARTESIAN_POINT('Ctrl Pts',(3.47795751599994,12.2,2.59612764199999));
#340971=CARTESIAN_POINT('Ctrl Pts',(3.47795751599994,5.2,2.59612764199999));
#340972=CARTESIAN_POINT('Ctrl Pts',(3.47795751599994,2.2,2.59612764199999));
#340973=CARTESIAN_POINT('Ctrl Pts',(3.47891586199994,12.2,2.59777537799999));
#340974=CARTESIAN_POINT('Ctrl Pts',(3.47891586199994,5.2,2.59777537799999));
#340975=CARTESIAN_POINT('Ctrl Pts',(3.47891586199994,2.2,2.59777537799999));
#340976=CARTESIAN_POINT('Ctrl Pts',(3.47987446199994,12.2,2.59942780599999));
#340977=CARTESIAN_POINT('Ctrl Pts',(3.47987446199994,5.2,2.59942780599999));
#340978=CARTESIAN_POINT('Ctrl Pts',(3.47987446199994,2.2,2.59942780599999));
#340979=CARTESIAN_POINT('Ctrl Pts',(3.48083330299994,12.2,2.60108492199999));
#340980=CARTESIAN_POINT('Ctrl Pts',(3.48083330299994,5.2,2.60108492199999));
#340981=CARTESIAN_POINT('Ctrl Pts',(3.48083330299994,2.2,2.60108492199999));
#340982=CARTESIAN_POINT('Ctrl Pts',(3.48179237399994,12.2,2.60274672499998));
#340983=CARTESIAN_POINT('Ctrl Pts',(3.48179237399994,5.2,2.60274672499998));
#340984=CARTESIAN_POINT('Ctrl Pts',(3.48179237399994,2.2,2.60274672499998));
#340985=CARTESIAN_POINT('Ctrl Pts',(3.48275166499994,12.2,2.60441321199998));
#340986=CARTESIAN_POINT('Ctrl Pts',(3.48275166499994,5.2,2.60441321199998));
#340987=CARTESIAN_POINT('Ctrl Pts',(3.48275166499994,2.2,2.60441321199998));
#340988=CARTESIAN_POINT('Ctrl Pts',(3.48371116499994,12.2,2.60608438099998));
#340989=CARTESIAN_POINT('Ctrl Pts',(3.48371116499994,5.2,2.60608438099998));
#340990=CARTESIAN_POINT('Ctrl Pts',(3.48371116499994,2.2,2.60608438099998));
#340991=CARTESIAN_POINT('Ctrl Pts',(3.48467086199994,12.2,2.60776022999998));
#340992=CARTESIAN_POINT('Ctrl Pts',(3.48467086199994,5.2,2.60776022999998));
#340993=CARTESIAN_POINT('Ctrl Pts',(3.48467086199994,2.2,2.60776022999998));
#340994=CARTESIAN_POINT('Ctrl Pts',(3.48563074599994,12.2,2.60944075599999));
#340995=CARTESIAN_POINT('Ctrl Pts',(3.48563074599994,5.2,2.60944075599999));
#340996=CARTESIAN_POINT('Ctrl Pts',(3.48563074599994,2.2,2.60944075599999));
#340997=CARTESIAN_POINT('Ctrl Pts',(3.48659080599994,12.2,2.61112595699998));
#340998=CARTESIAN_POINT('Ctrl Pts',(3.48659080599994,5.2,2.61112595699998));
#340999=CARTESIAN_POINT('Ctrl Pts',(3.48659080599994,2.2,2.61112595699998));
#341000=CARTESIAN_POINT('Ctrl Pts',(3.48755102999994,12.2,2.61281583099999));
#341001=CARTESIAN_POINT('Ctrl Pts',(3.48755102999994,5.2,2.61281583099999));
#341002=CARTESIAN_POINT('Ctrl Pts',(3.48755102999994,2.2,2.61281583099999));
#341003=CARTESIAN_POINT('Ctrl Pts',(3.48851140799994,12.2,2.61451037499998));
#341004=CARTESIAN_POINT('Ctrl Pts',(3.48851140799994,5.2,2.61451037499998));
#341005=CARTESIAN_POINT('Ctrl Pts',(3.48851140799994,2.2,2.61451037499998));
#341006=CARTESIAN_POINT('Ctrl Pts',(3.48947192999994,12.2,2.61620958799998));
#341007=CARTESIAN_POINT('Ctrl Pts',(3.48947192999994,5.2,2.61620958799998));
#341008=CARTESIAN_POINT('Ctrl Pts',(3.48947192999994,2.2,2.61620958799998));
#341009=CARTESIAN_POINT('Ctrl Pts',(3.49043258299994,12.2,2.61791346599999));
#341010=CARTESIAN_POINT('Ctrl Pts',(3.49043258299994,5.2,2.61791346599999));
#341011=CARTESIAN_POINT('Ctrl Pts',(3.49043258299994,2.2,2.61791346599999));
#341012=CARTESIAN_POINT('Ctrl Pts',(3.49139335899994,12.2,2.61962200699998));
#341013=CARTESIAN_POINT('Ctrl Pts',(3.49139335899994,5.2,2.61962200699998));
#341014=CARTESIAN_POINT('Ctrl Pts',(3.49139335899994,2.2,2.61962200699998));
#341015=CARTESIAN_POINT('Ctrl Pts',(3.49235424499994,12.2,2.62133520899998));
#341016=CARTESIAN_POINT('Ctrl Pts',(3.49235424499994,5.2,2.62133520899998));
#341017=CARTESIAN_POINT('Ctrl Pts',(3.49235424499994,2.2,2.62133520899998));
#341018=CARTESIAN_POINT('Ctrl Pts',(3.49331522999994,12.2,2.62305306999998));
#341019=CARTESIAN_POINT('Ctrl Pts',(3.49331522999994,5.2,2.62305306999998));
#341020=CARTESIAN_POINT('Ctrl Pts',(3.49331522999994,2.2,2.62305306999998));
#341021=CARTESIAN_POINT('Ctrl Pts',(3.49427630399994,12.2,2.62477558799999));
#341022=CARTESIAN_POINT('Ctrl Pts',(3.49427630399994,5.2,2.62477558799999));
#341023=CARTESIAN_POINT('Ctrl Pts',(3.49427630399994,2.2,2.62477558799999));
#341024=CARTESIAN_POINT('Ctrl Pts',(3.49523745799994,12.2,2.62650275899999));
#341025=CARTESIAN_POINT('Ctrl Pts',(3.49523745799994,5.2,2.62650275899999));
#341026=CARTESIAN_POINT('Ctrl Pts',(3.49523745799994,2.2,2.62650275899999));
#341027=CARTESIAN_POINT('Ctrl Pts',(3.49619867799994,12.2,2.62823458099999));
#341028=CARTESIAN_POINT('Ctrl Pts',(3.49619867799994,5.2,2.62823458099999));
#341029=CARTESIAN_POINT('Ctrl Pts',(3.49619867799994,2.2,2.62823458099999));
#341030=CARTESIAN_POINT('Ctrl Pts',(3.49715995499994,12.2,2.62997105199998));
#341031=CARTESIAN_POINT('Ctrl Pts',(3.49715995499994,5.2,2.62997105199998));
#341032=CARTESIAN_POINT('Ctrl Pts',(3.49715995499994,2.2,2.62997105199998));
#341033=CARTESIAN_POINT('Ctrl Pts',(3.49812127999995,12.2,2.63171216999999));
#341034=CARTESIAN_POINT('Ctrl Pts',(3.49812127999995,5.2,2.63171216999999));
#341035=CARTESIAN_POINT('Ctrl Pts',(3.49812127999995,2.2,2.63171216999999));
#341036=CARTESIAN_POINT('Ctrl Pts',(3.49908263899994,12.2,2.63345793199999));
#341037=CARTESIAN_POINT('Ctrl Pts',(3.49908263899994,5.2,2.63345793199999));
#341038=CARTESIAN_POINT('Ctrl Pts',(3.49908263899994,2.2,2.63345793199999));
#341039=CARTESIAN_POINT('Ctrl Pts',(3.50004402399994,12.2,2.63520833499998));
#341040=CARTESIAN_POINT('Ctrl Pts',(3.50004402399994,5.2,2.63520833499998));
#341041=CARTESIAN_POINT('Ctrl Pts',(3.50004402399994,2.2,2.63520833499998));
#341042=CARTESIAN_POINT('Ctrl Pts',(3.50100542299994,12.2,2.63696337799999));
#341043=CARTESIAN_POINT('Ctrl Pts',(3.50100542299994,5.2,2.63696337799999));
#341044=CARTESIAN_POINT('Ctrl Pts',(3.50100542299994,2.2,2.63696337799999));
#341045=CARTESIAN_POINT('Ctrl Pts',(3.50196682599994,12.2,2.63872305799998));
#341046=CARTESIAN_POINT('Ctrl Pts',(3.50196682599994,5.2,2.63872305799998));
#341047=CARTESIAN_POINT('Ctrl Pts',(3.50196682599994,2.2,2.63872305799998));
#341048=CARTESIAN_POINT('Ctrl Pts',(3.50292822099994,12.2,2.64048737199998));
#341049=CARTESIAN_POINT('Ctrl Pts',(3.50292822099994,5.2,2.64048737199998));
#341050=CARTESIAN_POINT('Ctrl Pts',(3.50292822099994,2.2,2.64048737199998));
#341051=CARTESIAN_POINT('Ctrl Pts',(3.50388959899994,12.2,2.64225631699999));
#341052=CARTESIAN_POINT('Ctrl Pts',(3.50388959899994,5.2,2.64225631699999));
#341053=CARTESIAN_POINT('Ctrl Pts',(3.50388959899994,2.2,2.64225631699999));
#341054=CARTESIAN_POINT('Ctrl Pts',(3.50485095099994,12.2,2.64402989199999));
#341055=CARTESIAN_POINT('Ctrl Pts',(3.50485095099994,5.2,2.64402989199999));
#341056=CARTESIAN_POINT('Ctrl Pts',(3.50485095099994,2.2,2.64402989199999));
#341057=CARTESIAN_POINT('Ctrl Pts',(3.50581226299994,12.2,2.64580809299999));
#341058=CARTESIAN_POINT('Ctrl Pts',(3.50581226299994,5.2,2.64580809299999));
#341059=CARTESIAN_POINT('Ctrl Pts',(3.50581226299994,2.2,2.64580809299999));
#341060=CARTESIAN_POINT('Ctrl Pts',(3.50677352599994,12.2,2.64759091899998));
#341061=CARTESIAN_POINT('Ctrl Pts',(3.50677352599994,5.2,2.64759091899998));
#341062=CARTESIAN_POINT('Ctrl Pts',(3.50677352599994,2.2,2.64759091899998));
#341063=CARTESIAN_POINT('Ctrl Pts',(3.50773473099994,12.2,2.64937836699998));
#341064=CARTESIAN_POINT('Ctrl Pts',(3.50773473099994,5.2,2.64937836699998));
#341065=CARTESIAN_POINT('Ctrl Pts',(3.50773473099994,2.2,2.64937836699998));
#341066=CARTESIAN_POINT('Ctrl Pts',(3.50869586499994,12.2,2.65117043299998));
#341067=CARTESIAN_POINT('Ctrl Pts',(3.50869586499994,5.2,2.65117043299998));
#341068=CARTESIAN_POINT('Ctrl Pts',(3.50869586499994,2.2,2.65117043299998));
#341069=CARTESIAN_POINT('Ctrl Pts',(3.50965691899995,12.2,2.65296711499998));
#341070=CARTESIAN_POINT('Ctrl Pts',(3.50965691899995,5.2,2.65296711499998));
#341071=CARTESIAN_POINT('Ctrl Pts',(3.50965691899995,2.2,2.65296711499998));
#341072=CARTESIAN_POINT('Ctrl Pts',(3.51061788199994,12.2,2.65476841099999));
#341073=CARTESIAN_POINT('Ctrl Pts',(3.51061788199994,5.2,2.65476841099999));
#341074=CARTESIAN_POINT('Ctrl Pts',(3.51061788199994,2.2,2.65476841099999));
#341075=CARTESIAN_POINT('Ctrl Pts',(3.51157874499994,12.2,2.65657431999998));
#341076=CARTESIAN_POINT('Ctrl Pts',(3.51157874499994,5.2,2.65657431999998));
#341077=CARTESIAN_POINT('Ctrl Pts',(3.51157874499994,2.2,2.65657431999998));
#341078=CARTESIAN_POINT('Ctrl Pts',(3.51253949599994,12.2,2.65838483699999));
#341079=CARTESIAN_POINT('Ctrl Pts',(3.51253949599994,5.2,2.65838483699999));
#341080=CARTESIAN_POINT('Ctrl Pts',(3.51253949599994,2.2,2.65838483699999));
#341081=CARTESIAN_POINT('Ctrl Pts',(3.51350012599994,12.2,2.66019995999999));
#341082=CARTESIAN_POINT('Ctrl Pts',(3.51350012599994,5.2,2.66019995999999));
#341083=CARTESIAN_POINT('Ctrl Pts',(3.51350012599994,2.2,2.66019995999999));
#341084=CARTESIAN_POINT('Ctrl Pts',(3.51446062299994,12.2,2.66201968599999));
#341085=CARTESIAN_POINT('Ctrl Pts',(3.51446062299994,5.2,2.66201968599999));
#341086=CARTESIAN_POINT('Ctrl Pts',(3.51446062299994,2.2,2.66201968599999));
#341087=CARTESIAN_POINT('Ctrl Pts',(3.51542097799994,12.2,2.66384401299998));
#341088=CARTESIAN_POINT('Ctrl Pts',(3.51542097799994,5.2,2.66384401299998));
#341089=CARTESIAN_POINT('Ctrl Pts',(3.51542097799994,2.2,2.66384401299998));
#341090=CARTESIAN_POINT('Ctrl Pts',(3.51638117999994,12.2,2.66567293999999));
#341091=CARTESIAN_POINT('Ctrl Pts',(3.51638117999994,5.2,2.66567293999999));
#341092=CARTESIAN_POINT('Ctrl Pts',(3.51638117999994,2.2,2.66567293999999));
#341093=CARTESIAN_POINT('Ctrl Pts',(3.51734121999994,12.2,2.66750645999998));
#341094=CARTESIAN_POINT('Ctrl Pts',(3.51734121999994,5.2,2.66750645999998));
#341095=CARTESIAN_POINT('Ctrl Pts',(3.51734121999994,2.2,2.66750645999998));
#341096=CARTESIAN_POINT('Ctrl Pts',(3.51830108599994,12.2,2.66934457499998));
#341097=CARTESIAN_POINT('Ctrl Pts',(3.51830108599994,5.2,2.66934457499998));
#341098=CARTESIAN_POINT('Ctrl Pts',(3.51830108599994,2.2,2.66934457499998));
#341099=CARTESIAN_POINT('Ctrl Pts',(3.51926076799994,12.2,2.67118727999998));
#341100=CARTESIAN_POINT('Ctrl Pts',(3.51926076799994,5.2,2.67118727999998));
#341101=CARTESIAN_POINT('Ctrl Pts',(3.51926076799994,2.2,2.67118727999998));
#341102=CARTESIAN_POINT('Ctrl Pts',(3.52022025699994,12.2,2.67303457199999));
#341103=CARTESIAN_POINT('Ctrl Pts',(3.52022025699994,5.2,2.67303457199999));
#341104=CARTESIAN_POINT('Ctrl Pts',(3.52022025699994,2.2,2.67303457199999));
#341105=CARTESIAN_POINT('Ctrl Pts',(3.52117954299994,12.2,2.67488644999998));
#341106=CARTESIAN_POINT('Ctrl Pts',(3.52117954299994,5.2,2.67488644999998));
#341107=CARTESIAN_POINT('Ctrl Pts',(3.52117954299994,2.2,2.67488644999998));
#341108=CARTESIAN_POINT('Ctrl Pts',(3.52213861299994,12.2,2.67674290999998));
#341109=CARTESIAN_POINT('Ctrl Pts',(3.52213861299994,5.2,2.67674290999998));
#341110=CARTESIAN_POINT('Ctrl Pts',(3.52213861299994,2.2,2.67674290999998));
#341111=CARTESIAN_POINT('Ctrl Pts',(3.52309746099994,12.2,2.67860394899999));
#341112=CARTESIAN_POINT('Ctrl Pts',(3.52309746099994,5.2,2.67860394899999));
#341113=CARTESIAN_POINT('Ctrl Pts',(3.52309746099994,2.2,2.67860394899999));
#341114=CARTESIAN_POINT('Ctrl Pts',(3.52405607299994,12.2,2.68046956499998));
#341115=CARTESIAN_POINT('Ctrl Pts',(3.52405607299994,5.2,2.68046956499998));
#341116=CARTESIAN_POINT('Ctrl Pts',(3.52405607299994,2.2,2.68046956499998));
#341117=CARTESIAN_POINT('Ctrl Pts',(3.52501444199994,12.2,2.68233975599999));
#341118=CARTESIAN_POINT('Ctrl Pts',(3.52501444199994,5.2,2.68233975599999));
#341119=CARTESIAN_POINT('Ctrl Pts',(3.52501444199994,2.2,2.68233975599999));
#341120=CARTESIAN_POINT('Ctrl Pts',(3.52597255499994,12.2,2.68421451799998));
#341121=CARTESIAN_POINT('Ctrl Pts',(3.52597255499994,5.2,2.68421451799998));
#341122=CARTESIAN_POINT('Ctrl Pts',(3.52597255499994,2.2,2.68421451799998));
#341123=CARTESIAN_POINT('Ctrl Pts',(3.52693040399994,12.2,2.68609384799999));
#341124=CARTESIAN_POINT('Ctrl Pts',(3.52693040399994,5.2,2.68609384799999));
#341125=CARTESIAN_POINT('Ctrl Pts',(3.52693040399994,2.2,2.68609384799999));
#341126=CARTESIAN_POINT('Ctrl Pts',(3.52788797899994,12.2,2.68797774499999));
#341127=CARTESIAN_POINT('Ctrl Pts',(3.52788797899994,5.2,2.68797774499999));
#341128=CARTESIAN_POINT('Ctrl Pts',(3.52788797899994,2.2,2.68797774499999));
#341129=CARTESIAN_POINT('Ctrl Pts',(3.52884526799994,12.2,2.68986620399998));
#341130=CARTESIAN_POINT('Ctrl Pts',(3.52884526799994,5.2,2.68986620399998));
#341131=CARTESIAN_POINT('Ctrl Pts',(3.52884526799994,2.2,2.68986620399998));
#341132=CARTESIAN_POINT('Ctrl Pts',(3.52980226299994,12.2,2.69175922499999));
#341133=CARTESIAN_POINT('Ctrl Pts',(3.52980226299994,5.2,2.69175922499999));
#341134=CARTESIAN_POINT('Ctrl Pts',(3.52980226299994,2.2,2.69175922499999));
#341135=CARTESIAN_POINT('Ctrl Pts',(3.53075895299995,12.2,2.69365680299998));
#341136=CARTESIAN_POINT('Ctrl Pts',(3.53075895299995,5.2,2.69365680299998));
#341137=CARTESIAN_POINT('Ctrl Pts',(3.53075895299995,2.2,2.69365680299998));
#341138=CARTESIAN_POINT('Ctrl Pts',(3.53171532799994,12.2,2.69555893499999));
#341139=CARTESIAN_POINT('Ctrl Pts',(3.53171532799994,5.2,2.69555893499999));
#341140=CARTESIAN_POINT('Ctrl Pts',(3.53171532799994,2.2,2.69555893499999));
#341141=CARTESIAN_POINT('Ctrl Pts',(3.53267137899994,12.2,2.69746561999998));
#341142=CARTESIAN_POINT('Ctrl Pts',(3.53267137899994,5.2,2.69746561999998));
#341143=CARTESIAN_POINT('Ctrl Pts',(3.53267137899994,2.2,2.69746561999998));
#341144=CARTESIAN_POINT('Ctrl Pts',(3.53362709499994,12.2,2.69937685399999));
#341145=CARTESIAN_POINT('Ctrl Pts',(3.53362709499994,5.2,2.69937685399999));
#341146=CARTESIAN_POINT('Ctrl Pts',(3.53362709499994,2.2,2.69937685399999));
#341147=CARTESIAN_POINT('Ctrl Pts',(3.53458246599994,12.2,2.70129263399999));
#341148=CARTESIAN_POINT('Ctrl Pts',(3.53458246599994,5.2,2.70129263399999));
#341149=CARTESIAN_POINT('Ctrl Pts',(3.53458246599994,2.2,2.70129263399999));
#341150=CARTESIAN_POINT('Ctrl Pts',(3.53553748299994,12.2,2.70321295899999));
#341151=CARTESIAN_POINT('Ctrl Pts',(3.53553748299994,5.2,2.70321295899999));
#341152=CARTESIAN_POINT('Ctrl Pts',(3.53553748299994,2.2,2.70321295899999));
#341153=CARTESIAN_POINT('Ctrl Pts',(3.53649213599994,12.2,2.70513782399998));
#341154=CARTESIAN_POINT('Ctrl Pts',(3.53649213599994,5.2,2.70513782399998));
#341155=CARTESIAN_POINT('Ctrl Pts',(3.53649213599994,2.2,2.70513782399998));
#341156=CARTESIAN_POINT('Ctrl Pts',(3.53744641399994,12.2,2.70706722699998));
#341157=CARTESIAN_POINT('Ctrl Pts',(3.53744641399994,5.2,2.70706722699998));
#341158=CARTESIAN_POINT('Ctrl Pts',(3.53744641399994,2.2,2.70706722699998));
#341159=CARTESIAN_POINT('Ctrl Pts',(3.53840030899994,12.2,2.70900116499998));
#341160=CARTESIAN_POINT('Ctrl Pts',(3.53840030899994,5.2,2.70900116499998));
#341161=CARTESIAN_POINT('Ctrl Pts',(3.53840030899994,2.2,2.70900116499998));
#341162=CARTESIAN_POINT('Ctrl Pts',(3.53935380899994,12.2,2.71093963499998));
#341163=CARTESIAN_POINT('Ctrl Pts',(3.53935380899994,5.2,2.71093963499998));
#341164=CARTESIAN_POINT('Ctrl Pts',(3.53935380899994,2.2,2.71093963499998));
#341165=CARTESIAN_POINT('Ctrl Pts',(3.54030690499994,12.2,2.71288263399998));
#341166=CARTESIAN_POINT('Ctrl Pts',(3.54030690499994,5.2,2.71288263399998));
#341167=CARTESIAN_POINT('Ctrl Pts',(3.54030690499994,2.2,2.71288263399998));
#341168=CARTESIAN_POINT('Ctrl Pts',(3.54125958799994,12.2,2.71483016099998));
#341169=CARTESIAN_POINT('Ctrl Pts',(3.54125958799994,5.2,2.71483016099998));
#341170=CARTESIAN_POINT('Ctrl Pts',(3.54125958799994,2.2,2.71483016099998));
#341171=CARTESIAN_POINT('Ctrl Pts',(3.54221184699994,12.2,2.71678220999998));
#341172=CARTESIAN_POINT('Ctrl Pts',(3.54221184699994,5.2,2.71678220999998));
#341173=CARTESIAN_POINT('Ctrl Pts',(3.54221184699994,2.2,2.71678220999998));
#341174=CARTESIAN_POINT('Ctrl Pts',(3.54316367399994,12.2,2.71873878099999));
#341175=CARTESIAN_POINT('Ctrl Pts',(3.54316367399994,5.2,2.71873878099999));
#341176=CARTESIAN_POINT('Ctrl Pts',(3.54316367399994,2.2,2.71873878099999));
#341177=CARTESIAN_POINT('Ctrl Pts',(3.54411505699994,12.2,2.72069986899999));
#341178=CARTESIAN_POINT('Ctrl Pts',(3.54411505699994,5.2,2.72069986899999));
#341179=CARTESIAN_POINT('Ctrl Pts',(3.54411505699994,2.2,2.72069986899999));
#341180=CARTESIAN_POINT('Ctrl Pts',(3.54506598799994,12.2,2.72266547199998));
#341181=CARTESIAN_POINT('Ctrl Pts',(3.54506598799994,5.2,2.72266547199998));
#341182=CARTESIAN_POINT('Ctrl Pts',(3.54506598799994,2.2,2.72266547199998));
#341183=CARTESIAN_POINT('Ctrl Pts',(3.54601645599994,12.2,2.72463558699998));
#341184=CARTESIAN_POINT('Ctrl Pts',(3.54601645599994,5.2,2.72463558699998));
#341185=CARTESIAN_POINT('Ctrl Pts',(3.54601645599994,2.2,2.72463558699998));
#341186=CARTESIAN_POINT('Ctrl Pts',(3.54696645299994,12.2,2.72661021099999));
#341187=CARTESIAN_POINT('Ctrl Pts',(3.54696645299994,5.2,2.72661021099999));
#341188=CARTESIAN_POINT('Ctrl Pts',(3.54696645299994,2.2,2.72661021099999));
#341189=CARTESIAN_POINT('Ctrl Pts',(3.54791596799994,12.2,2.72858934099999));
#341190=CARTESIAN_POINT('Ctrl Pts',(3.54791596799994,5.2,2.72858934099999));
#341191=CARTESIAN_POINT('Ctrl Pts',(3.54791596799994,2.2,2.72858934099999));
#341192=CARTESIAN_POINT('Ctrl Pts',(3.54886499099994,12.2,2.73057297399999));
#341193=CARTESIAN_POINT('Ctrl Pts',(3.54886499099994,5.2,2.73057297399999));
#341194=CARTESIAN_POINT('Ctrl Pts',(3.54886499099994,2.2,2.73057297399999));
#341195=CARTESIAN_POINT('Ctrl Pts',(3.54981351399994,12.2,2.73256110699998));
#341196=CARTESIAN_POINT('Ctrl Pts',(3.54981351399994,5.2,2.73256110699998));
#341197=CARTESIAN_POINT('Ctrl Pts',(3.54981351399994,2.2,2.73256110699998));
#341198=CARTESIAN_POINT('Ctrl Pts',(3.55076152599994,12.2,2.73455373799998));
#341199=CARTESIAN_POINT('Ctrl Pts',(3.55076152599994,5.2,2.73455373799998));
#341200=CARTESIAN_POINT('Ctrl Pts',(3.55076152599994,2.2,2.73455373799998));
#341201=CARTESIAN_POINT('Ctrl Pts',(3.55170901699994,12.2,2.73655086199999));
#341202=CARTESIAN_POINT('Ctrl Pts',(3.55170901699994,5.2,2.73655086199999));
#341203=CARTESIAN_POINT('Ctrl Pts',(3.55170901699994,2.2,2.73655086199999));
#341204=CARTESIAN_POINT('Ctrl Pts',(3.55265597999994,12.2,2.73855247899998));
#341205=CARTESIAN_POINT('Ctrl Pts',(3.55265597999994,5.2,2.73855247899998));
#341206=CARTESIAN_POINT('Ctrl Pts',(3.55265597999994,2.2,2.73855247899998));
#341207=CARTESIAN_POINT('Ctrl Pts',(3.55360240199994,12.2,2.74055858299998));
#341208=CARTESIAN_POINT('Ctrl Pts',(3.55360240199994,5.2,2.74055858299998));
#341209=CARTESIAN_POINT('Ctrl Pts',(3.55360240199994,2.2,2.74055858299998));
#341210=CARTESIAN_POINT('Ctrl Pts',(3.55454827599994,12.2,2.74256917199998));
#341211=CARTESIAN_POINT('Ctrl Pts',(3.55454827599994,5.2,2.74256917199998));
#341212=CARTESIAN_POINT('Ctrl Pts',(3.55454827599994,2.2,2.74256917199998));
#341213=CARTESIAN_POINT('Ctrl Pts',(3.55549359199994,12.2,2.74458424399998));
#341214=CARTESIAN_POINT('Ctrl Pts',(3.55549359199994,5.2,2.74458424399998));
#341215=CARTESIAN_POINT('Ctrl Pts',(3.55549359199994,2.2,2.74458424399998));
#341216=CARTESIAN_POINT('Ctrl Pts',(3.55643833899994,12.2,2.74660379399998));
#341217=CARTESIAN_POINT('Ctrl Pts',(3.55643833899994,5.2,2.74660379399998));
#341218=CARTESIAN_POINT('Ctrl Pts',(3.55643833899994,2.2,2.74660379399998));
#341219=CARTESIAN_POINT('Ctrl Pts',(3.55738250899994,12.2,2.74862782199998));
#341220=CARTESIAN_POINT('Ctrl Pts',(3.55738250899994,5.2,2.74862782199998));
#341221=CARTESIAN_POINT('Ctrl Pts',(3.55738250899994,2.2,2.74862782199998));
#341222=CARTESIAN_POINT('Ctrl Pts',(3.55832609299994,12.2,2.75065632199999));
#341223=CARTESIAN_POINT('Ctrl Pts',(3.55832609299994,5.2,2.75065632199999));
#341224=CARTESIAN_POINT('Ctrl Pts',(3.55832609299994,2.2,2.75065632199999));
#341225=CARTESIAN_POINT('Ctrl Pts',(3.55926907899994,12.2,2.75268929099998));
#341226=CARTESIAN_POINT('Ctrl Pts',(3.55926907899994,5.2,2.75268929099998));
#341227=CARTESIAN_POINT('Ctrl Pts',(3.55926907899994,2.2,2.75268929099998));
#341228=CARTESIAN_POINT('Ctrl Pts',(3.56021145999994,12.2,2.75472672799999));
#341229=CARTESIAN_POINT('Ctrl Pts',(3.56021145999994,5.2,2.75472672799999));
#341230=CARTESIAN_POINT('Ctrl Pts',(3.56021145999994,2.2,2.75472672799999));
#341231=CARTESIAN_POINT('Ctrl Pts',(3.56115322699994,12.2,2.75676862799998));
#341232=CARTESIAN_POINT('Ctrl Pts',(3.56115322699994,5.2,2.75676862799998));
#341233=CARTESIAN_POINT('Ctrl Pts',(3.56115322699994,2.2,2.75676862799998));
#341234=CARTESIAN_POINT('Ctrl Pts',(3.56209436799994,12.2,2.75881499099999));
#341235=CARTESIAN_POINT('Ctrl Pts',(3.56209436799994,5.2,2.75881499099999));
#341236=CARTESIAN_POINT('Ctrl Pts',(3.56209436799994,2.2,2.75881499099999));
#341237=CARTESIAN_POINT('Ctrl Pts',(3.56303487499994,12.2,2.76086580999999));
#341238=CARTESIAN_POINT('Ctrl Pts',(3.56303487499994,5.2,2.76086580999999));
#341239=CARTESIAN_POINT('Ctrl Pts',(3.56303487499994,2.2,2.76086580999999));
#341240=CARTESIAN_POINT('Ctrl Pts',(3.56397473899994,12.2,2.76292108399999));
#341241=CARTESIAN_POINT('Ctrl Pts',(3.56397473899994,5.2,2.76292108399999));
#341242=CARTESIAN_POINT('Ctrl Pts',(3.56397473899994,2.2,2.76292108399999));
#341243=CARTESIAN_POINT('Ctrl Pts',(3.56491394999995,12.2,2.76498080999998));
#341244=CARTESIAN_POINT('Ctrl Pts',(3.56491394999995,5.2,2.76498080999998));
#341245=CARTESIAN_POINT('Ctrl Pts',(3.56491394999995,2.2,2.76498080999998));
#341246=CARTESIAN_POINT('Ctrl Pts',(3.56585249999994,12.2,2.76704498399998));
#341247=CARTESIAN_POINT('Ctrl Pts',(3.56585249999994,5.2,2.76704498399998));
#341248=CARTESIAN_POINT('Ctrl Pts',(3.56585249999994,2.2,2.76704498399998));
#341249=CARTESIAN_POINT('Ctrl Pts',(3.56679037699994,12.2,2.76911360399998));
#341250=CARTESIAN_POINT('Ctrl Pts',(3.56679037699994,5.2,2.76911360399998));
#341251=CARTESIAN_POINT('Ctrl Pts',(3.56679037699994,2.2,2.76911360399998));
#341252=CARTESIAN_POINT('Ctrl Pts',(3.56772757399995,12.2,2.77118666499998));
#341253=CARTESIAN_POINT('Ctrl Pts',(3.56772757399995,5.2,2.77118666499998));
#341254=CARTESIAN_POINT('Ctrl Pts',(3.56772757399995,2.2,2.77118666499998));
#341255=CARTESIAN_POINT('Ctrl Pts',(3.56866408199994,12.2,2.77326416599998));
#341256=CARTESIAN_POINT('Ctrl Pts',(3.56866408199994,5.2,2.77326416599998));
#341257=CARTESIAN_POINT('Ctrl Pts',(3.56866408199994,2.2,2.77326416599998));
#341258=CARTESIAN_POINT('Ctrl Pts',(3.56959988899994,12.2,2.77534610199999));
#341259=CARTESIAN_POINT('Ctrl Pts',(3.56959988899994,5.2,2.77534610199999));
#341260=CARTESIAN_POINT('Ctrl Pts',(3.56959988899994,2.2,2.77534610199999));
#341261=CARTESIAN_POINT('Ctrl Pts',(3.57053498799994,12.2,2.77743247199999));
#341262=CARTESIAN_POINT('Ctrl Pts',(3.57053498799994,5.2,2.77743247199999));
#341263=CARTESIAN_POINT('Ctrl Pts',(3.57053498799994,2.2,2.77743247199999));
#341264=CARTESIAN_POINT('Ctrl Pts',(3.57146936999994,12.2,2.77952327099998));
#341265=CARTESIAN_POINT('Ctrl Pts',(3.57146936999994,5.2,2.77952327099998));
#341266=CARTESIAN_POINT('Ctrl Pts',(3.57146936999994,2.2,2.77952327099998));
#341267=CARTESIAN_POINT('Ctrl Pts',(3.57240302499994,12.2,2.78161849699998));
#341268=CARTESIAN_POINT('Ctrl Pts',(3.57240302499994,5.2,2.78161849699998));
#341269=CARTESIAN_POINT('Ctrl Pts',(3.57240302499994,2.2,2.78161849699998));
#341270=CARTESIAN_POINT('Ctrl Pts',(3.57333594399994,12.2,2.78371814599998));
#341271=CARTESIAN_POINT('Ctrl Pts',(3.57333594399994,5.2,2.78371814599998));
#341272=CARTESIAN_POINT('Ctrl Pts',(3.57333594399994,2.2,2.78371814599998));
#341273=CARTESIAN_POINT('Ctrl Pts',(3.57426811699994,12.2,2.78582221499998));
#341274=CARTESIAN_POINT('Ctrl Pts',(3.57426811699994,5.2,2.78582221499998));
#341275=CARTESIAN_POINT('Ctrl Pts',(3.57426811699994,2.2,2.78582221499998));
#341276=CARTESIAN_POINT('Ctrl Pts',(3.57519953599994,12.2,2.78793069999999));
#341277=CARTESIAN_POINT('Ctrl Pts',(3.57519953599994,5.2,2.78793069999999));
#341278=CARTESIAN_POINT('Ctrl Pts',(3.57519953599994,2.2,2.78793069999999));
#341279=CARTESIAN_POINT('Ctrl Pts',(3.57613019099994,12.2,2.79004359899999));
#341280=CARTESIAN_POINT('Ctrl Pts',(3.57613019099994,5.2,2.79004359899999));
#341281=CARTESIAN_POINT('Ctrl Pts',(3.57613019099994,2.2,2.79004359899999));
#341282=CARTESIAN_POINT('Ctrl Pts',(3.57706007399994,12.2,2.79216090999999));
#341283=CARTESIAN_POINT('Ctrl Pts',(3.57706007399994,5.2,2.79216090999999));
#341284=CARTESIAN_POINT('Ctrl Pts',(3.57706007399994,2.2,2.79216090999999));
#341285=CARTESIAN_POINT('Ctrl Pts',(3.57798917399994,12.2,2.79428262799998));
#341286=CARTESIAN_POINT('Ctrl Pts',(3.57798917399994,5.2,2.79428262799998));
#341287=CARTESIAN_POINT('Ctrl Pts',(3.57798917399994,2.2,2.79428262799998));
#341288=CARTESIAN_POINT('Ctrl Pts',(3.57891748399994,12.2,2.79640874799998));
#341289=CARTESIAN_POINT('Ctrl Pts',(3.57891748399994,5.2,2.79640874799998));
#341290=CARTESIAN_POINT('Ctrl Pts',(3.57891748399994,2.2,2.79640874799998));
#341291=CARTESIAN_POINT('Ctrl Pts',(3.57984499299994,12.2,2.79853926999999));
#341292=CARTESIAN_POINT('Ctrl Pts',(3.57984499299994,5.2,2.79853926999999));
#341293=CARTESIAN_POINT('Ctrl Pts',(3.57984499299994,2.2,2.79853926999999));
#341294=CARTESIAN_POINT('Ctrl Pts',(3.58077169299994,12.2,2.80067419099999));
#341295=CARTESIAN_POINT('Ctrl Pts',(3.58077169299994,5.2,2.80067419099999));
#341296=CARTESIAN_POINT('Ctrl Pts',(3.58077169299994,2.2,2.80067419099999));
#341297=CARTESIAN_POINT('Ctrl Pts',(3.58169757499994,12.2,2.80281350399999));
#341298=CARTESIAN_POINT('Ctrl Pts',(3.58169757499994,5.2,2.80281350399999));
#341299=CARTESIAN_POINT('Ctrl Pts',(3.58169757499994,2.2,2.80281350399999));
#341300=CARTESIAN_POINT('Ctrl Pts',(3.58262263099994,12.2,2.80495720899999));
#341301=CARTESIAN_POINT('Ctrl Pts',(3.58262263099994,5.2,2.80495720899999));
#341302=CARTESIAN_POINT('Ctrl Pts',(3.58262263099994,2.2,2.80495720899999));
#341303=CARTESIAN_POINT('Ctrl Pts',(3.58354684999994,12.2,2.80710530299999));
#341304=CARTESIAN_POINT('Ctrl Pts',(3.58354684999994,5.2,2.80710530299999));
#341305=CARTESIAN_POINT('Ctrl Pts',(3.58354684999994,2.2,2.80710530299999));
#341306=CARTESIAN_POINT('Ctrl Pts',(3.58447022299994,12.2,2.80925777999999));
#341307=CARTESIAN_POINT('Ctrl Pts',(3.58447022299994,5.2,2.80925777999999));
#341308=CARTESIAN_POINT('Ctrl Pts',(3.58447022299994,2.2,2.80925777999999));
#341309=CARTESIAN_POINT('Ctrl Pts',(3.58539274299994,12.2,2.81141463799998));
#341310=CARTESIAN_POINT('Ctrl Pts',(3.58539274299994,5.2,2.81141463799998));
#341311=CARTESIAN_POINT('Ctrl Pts',(3.58539274299994,2.2,2.81141463799998));
#341312=CARTESIAN_POINT('Ctrl Pts',(3.58631439899994,12.2,2.81357587599998));
#341313=CARTESIAN_POINT('Ctrl Pts',(3.58631439899994,5.2,2.81357587599998));
#341314=CARTESIAN_POINT('Ctrl Pts',(3.58631439899994,2.2,2.81357587599998));
#341315=CARTESIAN_POINT('Ctrl Pts',(3.58723518399994,12.2,2.81574148699999));
#341316=CARTESIAN_POINT('Ctrl Pts',(3.58723518399994,5.2,2.81574148699999));
#341317=CARTESIAN_POINT('Ctrl Pts',(3.58723518399994,2.2,2.81574148699999));
#341318=CARTESIAN_POINT('Ctrl Pts',(3.58815508699994,12.2,2.81791146899998));
#341319=CARTESIAN_POINT('Ctrl Pts',(3.58815508699994,5.2,2.81791146899998));
#341320=CARTESIAN_POINT('Ctrl Pts',(3.58815508699994,2.2,2.81791146899998));
#341321=CARTESIAN_POINT('Ctrl Pts',(3.58907410099994,12.2,2.82008581999998));
#341322=CARTESIAN_POINT('Ctrl Pts',(3.58907410099994,5.2,2.82008581999998));
#341323=CARTESIAN_POINT('Ctrl Pts',(3.58907410099994,2.2,2.82008581999998));
#341324=CARTESIAN_POINT('Ctrl Pts',(3.58999221499994,12.2,2.82226453499998));
#341325=CARTESIAN_POINT('Ctrl Pts',(3.58999221499994,5.2,2.82226453499998));
#341326=CARTESIAN_POINT('Ctrl Pts',(3.58999221499994,2.2,2.82226453499998));
#341327=CARTESIAN_POINT('Ctrl Pts',(3.59090942199995,12.2,2.82444761199999));
#341328=CARTESIAN_POINT('Ctrl Pts',(3.59090942199995,5.2,2.82444761199999));
#341329=CARTESIAN_POINT('Ctrl Pts',(3.59090942199995,2.2,2.82444761199999));
#341330=CARTESIAN_POINT('Ctrl Pts',(3.59182571199994,12.2,2.82663504699999));
#341331=CARTESIAN_POINT('Ctrl Pts',(3.59182571199994,5.2,2.82663504699999));
#341332=CARTESIAN_POINT('Ctrl Pts',(3.59182571199994,2.2,2.82663504699999));
#341333=CARTESIAN_POINT('Ctrl Pts',(3.59274107699994,12.2,2.82882683699999));
#341334=CARTESIAN_POINT('Ctrl Pts',(3.59274107699994,5.2,2.82882683699999));
#341335=CARTESIAN_POINT('Ctrl Pts',(3.59274107699994,2.2,2.82882683699999));
#341336=CARTESIAN_POINT('Ctrl Pts',(3.59365550899994,12.2,2.83102297799999));
#341337=CARTESIAN_POINT('Ctrl Pts',(3.59365550899994,5.2,2.83102297799999));
#341338=CARTESIAN_POINT('Ctrl Pts',(3.59365550899994,2.2,2.83102297799999));
#341339=CARTESIAN_POINT('Ctrl Pts',(3.59456899599994,12.2,2.83322346799999));
#341340=CARTESIAN_POINT('Ctrl Pts',(3.59456899599994,5.2,2.83322346799999));
#341341=CARTESIAN_POINT('Ctrl Pts',(3.59456899599994,2.2,2.83322346799999));
#341342=CARTESIAN_POINT('Ctrl Pts',(3.59548153099994,12.2,2.83542830099999));
#341343=CARTESIAN_POINT('Ctrl Pts',(3.59548153099994,5.2,2.83542830099999));
#341344=CARTESIAN_POINT('Ctrl Pts',(3.59548153099994,2.2,2.83542830099999));
#341345=CARTESIAN_POINT('Ctrl Pts',(3.59639310699994,12.2,2.83763747599998));
#341346=CARTESIAN_POINT('Ctrl Pts',(3.59639310699994,5.2,2.83763747599998));
#341347=CARTESIAN_POINT('Ctrl Pts',(3.59639310699994,2.2,2.83763747599998));
#341348=CARTESIAN_POINT('Ctrl Pts',(3.59730371299994,12.2,2.83985098799998));
#341349=CARTESIAN_POINT('Ctrl Pts',(3.59730371299994,5.2,2.83985098799998));
#341350=CARTESIAN_POINT('Ctrl Pts',(3.59730371299994,2.2,2.83985098799998));
#341351=CARTESIAN_POINT('Ctrl Pts',(3.59821333999994,12.2,2.84206883599998));
#341352=CARTESIAN_POINT('Ctrl Pts',(3.59821333999994,5.2,2.84206883599998));
#341353=CARTESIAN_POINT('Ctrl Pts',(3.59821333999994,2.2,2.84206883599998));
#341354=CARTESIAN_POINT('Ctrl Pts',(3.59912197999994,12.2,2.84429101499998));
#341355=CARTESIAN_POINT('Ctrl Pts',(3.59912197999994,5.2,2.84429101499998));
#341356=CARTESIAN_POINT('Ctrl Pts',(3.59912197999994,2.2,2.84429101499998));
#341357=CARTESIAN_POINT('Ctrl Pts',(3.60002962499994,12.2,2.84651751999998));
#341358=CARTESIAN_POINT('Ctrl Pts',(3.60002962499994,5.2,2.84651751999998));
#341359=CARTESIAN_POINT('Ctrl Pts',(3.60002962499994,2.2,2.84651751999998));
#341360=CARTESIAN_POINT('Ctrl Pts',(3.60093626599994,12.2,2.84874835199999));
#341361=CARTESIAN_POINT('Ctrl Pts',(3.60093626599994,5.2,2.84874835199999));
#341362=CARTESIAN_POINT('Ctrl Pts',(3.60093626599994,2.2,2.84874835199999));
#341363=CARTESIAN_POINT('Ctrl Pts',(3.60184189399994,12.2,2.85098350199998));
#341364=CARTESIAN_POINT('Ctrl Pts',(3.60184189399994,5.2,2.85098350199998));
#341365=CARTESIAN_POINT('Ctrl Pts',(3.60184189399994,2.2,2.85098350199998));
#341366=CARTESIAN_POINT('Ctrl Pts',(3.60274650099994,12.2,2.85322297199999));
#341367=CARTESIAN_POINT('Ctrl Pts',(3.60274650099994,5.2,2.85322297199999));
#341368=CARTESIAN_POINT('Ctrl Pts',(3.60274650099994,2.2,2.85322297199999));
#341369=CARTESIAN_POINT('Ctrl Pts',(3.60365007599994,12.2,2.85546675399999));
#341370=CARTESIAN_POINT('Ctrl Pts',(3.60365007599994,5.2,2.85546675399999));
#341371=CARTESIAN_POINT('Ctrl Pts',(3.60365007599994,2.2,2.85546675399999));
#341372=CARTESIAN_POINT('Ctrl Pts',(3.60455261199994,12.2,2.85771484799999));
#341373=CARTESIAN_POINT('Ctrl Pts',(3.60455261199994,5.2,2.85771484799999));
#341374=CARTESIAN_POINT('Ctrl Pts',(3.60455261199994,2.2,2.85771484799999));
#341375=CARTESIAN_POINT('Ctrl Pts',(3.60545410099994,12.2,2.85996724799999));
#341376=CARTESIAN_POINT('Ctrl Pts',(3.60545410099994,5.2,2.85996724799999));
#341377=CARTESIAN_POINT('Ctrl Pts',(3.60545410099994,2.2,2.85996724799999));
#341378=CARTESIAN_POINT('Ctrl Pts',(3.60635453499994,12.2,2.86222395299998));
#341379=CARTESIAN_POINT('Ctrl Pts',(3.60635453499994,5.2,2.86222395299998));
#341380=CARTESIAN_POINT('Ctrl Pts',(3.60635453499994,2.2,2.86222395299998));
#341381=CARTESIAN_POINT('Ctrl Pts',(3.60725390299994,12.2,2.86448495699998));
#341382=CARTESIAN_POINT('Ctrl Pts',(3.60725390299994,5.2,2.86448495699998));
#341383=CARTESIAN_POINT('Ctrl Pts',(3.60725390299994,2.2,2.86448495699998));
#341384=CARTESIAN_POINT('Ctrl Pts',(3.60815219799994,12.2,2.86675025799998));
#341385=CARTESIAN_POINT('Ctrl Pts',(3.60815219799994,5.2,2.86675025799998));
#341386=CARTESIAN_POINT('Ctrl Pts',(3.60815219799994,2.2,2.86675025799998));
#341387=CARTESIAN_POINT('Ctrl Pts',(3.60904941099994,12.2,2.86901985299998));
#341388=CARTESIAN_POINT('Ctrl Pts',(3.60904941099994,5.2,2.86901985299998));
#341389=CARTESIAN_POINT('Ctrl Pts',(3.60904941099994,2.2,2.86901985299998));
#341390=CARTESIAN_POINT('Ctrl Pts',(3.60994553399994,12.2,2.87129373699998));
#341391=CARTESIAN_POINT('Ctrl Pts',(3.60994553399994,5.2,2.87129373699998));
#341392=CARTESIAN_POINT('Ctrl Pts',(3.60994553399994,2.2,2.87129373699998));
#341393=CARTESIAN_POINT('Ctrl Pts',(3.61084055699994,12.2,2.87357190699999));
#341394=CARTESIAN_POINT('Ctrl Pts',(3.61084055699994,5.2,2.87357190699999));
#341395=CARTESIAN_POINT('Ctrl Pts',(3.61084055699994,2.2,2.87357190699999));
#341396=CARTESIAN_POINT('Ctrl Pts',(3.61173447299994,12.2,2.87585435999999));
#341397=CARTESIAN_POINT('Ctrl Pts',(3.61173447299994,5.2,2.87585435999999));
#341398=CARTESIAN_POINT('Ctrl Pts',(3.61173447299994,2.2,2.87585435999999));
#341399=CARTESIAN_POINT('Ctrl Pts',(3.61262727299994,12.2,2.87814109199999));
#341400=CARTESIAN_POINT('Ctrl Pts',(3.61262727299994,5.2,2.87814109199999));
#341401=CARTESIAN_POINT('Ctrl Pts',(3.61262727299994,2.2,2.87814109199999));
#341402=CARTESIAN_POINT('Ctrl Pts',(3.61351894799994,12.2,2.88043210099998));
#341403=CARTESIAN_POINT('Ctrl Pts',(3.61351894799994,5.2,2.88043210099998));
#341404=CARTESIAN_POINT('Ctrl Pts',(3.61351894799994,2.2,2.88043210099998));
#341405=CARTESIAN_POINT('Ctrl Pts',(3.61440949099994,12.2,2.88272738199999));
#341406=CARTESIAN_POINT('Ctrl Pts',(3.61440949099994,5.2,2.88272738199999));
#341407=CARTESIAN_POINT('Ctrl Pts',(3.61440949099994,2.2,2.88272738199999));
#341408=CARTESIAN_POINT('Ctrl Pts',(3.61529889299994,12.2,2.88502693099999));
#341409=CARTESIAN_POINT('Ctrl Pts',(3.61529889299994,5.2,2.88502693099999));
#341410=CARTESIAN_POINT('Ctrl Pts',(3.61529889299994,2.2,2.88502693099999));
#341411=CARTESIAN_POINT('Ctrl Pts',(3.61618714399994,12.2,2.88733074599998));
#341412=CARTESIAN_POINT('Ctrl Pts',(3.61618714399994,5.2,2.88733074599998));
#341413=CARTESIAN_POINT('Ctrl Pts',(3.61618714399994,2.2,2.88733074599998));
#341414=CARTESIAN_POINT('Ctrl Pts',(3.61707423799994,12.2,2.88963882199998));
#341415=CARTESIAN_POINT('Ctrl Pts',(3.61707423799994,5.2,2.88963882199998));
#341416=CARTESIAN_POINT('Ctrl Pts',(3.61707423799994,2.2,2.88963882199998));
#341417=CARTESIAN_POINT('Ctrl Pts',(3.61796016399994,12.2,2.89195115599998));
#341418=CARTESIAN_POINT('Ctrl Pts',(3.61796016399994,5.2,2.89195115599998));
#341419=CARTESIAN_POINT('Ctrl Pts',(3.61796016399994,2.2,2.89195115599998));
#341420=CARTESIAN_POINT('Ctrl Pts',(3.61884491599994,12.2,2.89426774499999));
#341421=CARTESIAN_POINT('Ctrl Pts',(3.61884491599994,5.2,2.89426774499999));
#341422=CARTESIAN_POINT('Ctrl Pts',(3.61884491599994,2.2,2.89426774499999));
#341423=CARTESIAN_POINT('Ctrl Pts',(3.61972848299994,12.2,2.89658858399999));
#341424=CARTESIAN_POINT('Ctrl Pts',(3.61972848299994,5.2,2.89658858399999));
#341425=CARTESIAN_POINT('Ctrl Pts',(3.61972848299994,2.2,2.89658858399999));
#341426=CARTESIAN_POINT('Ctrl Pts',(3.62061085999994,12.2,2.89891367199999));
#341427=CARTESIAN_POINT('Ctrl Pts',(3.62061085999994,5.2,2.89891367199999));
#341428=CARTESIAN_POINT('Ctrl Pts',(3.62061085999994,2.2,2.89891367199999));
#341429=CARTESIAN_POINT('Ctrl Pts',(3.62149203599994,12.2,2.90124300299999));
#341430=CARTESIAN_POINT('Ctrl Pts',(3.62149203599994,5.2,2.90124300299999));
#341431=CARTESIAN_POINT('Ctrl Pts',(3.62149203599994,2.2,2.90124300299999));
#341432=CARTESIAN_POINT('Ctrl Pts',(3.62237200399994,12.2,2.90357657399999));
#341433=CARTESIAN_POINT('Ctrl Pts',(3.62237200399994,5.2,2.90357657399999));
#341434=CARTESIAN_POINT('Ctrl Pts',(3.62237200399994,2.2,2.90357657399999));
#341435=CARTESIAN_POINT('Ctrl Pts',(3.62325075499994,12.2,2.90591438199999));
#341436=CARTESIAN_POINT('Ctrl Pts',(3.62325075499994,5.2,2.90591438199999));
#341437=CARTESIAN_POINT('Ctrl Pts',(3.62325075499994,2.2,2.90591438199999));
#341438=CARTESIAN_POINT('Ctrl Pts',(3.62412828099994,12.2,2.90825642199999));
#341439=CARTESIAN_POINT('Ctrl Pts',(3.62412828099994,5.2,2.90825642199999));
#341440=CARTESIAN_POINT('Ctrl Pts',(3.62412828099994,2.2,2.90825642199999));
#341441=CARTESIAN_POINT('Ctrl Pts',(3.62500457299994,12.2,2.91060269299999));
#341442=CARTESIAN_POINT('Ctrl Pts',(3.62500457299994,5.2,2.91060269299999));
#341443=CARTESIAN_POINT('Ctrl Pts',(3.62500457299994,2.2,2.91060269299999));
#341444=CARTESIAN_POINT('Ctrl Pts',(3.62587962499994,12.2,2.91295318899999));
#341445=CARTESIAN_POINT('Ctrl Pts',(3.62587962499994,5.2,2.91295318899999));
#341446=CARTESIAN_POINT('Ctrl Pts',(3.62587962499994,2.2,2.91295318899999));
#341447=CARTESIAN_POINT('Ctrl Pts',(3.62675342599994,12.2,2.91530790699999));
#341448=CARTESIAN_POINT('Ctrl Pts',(3.62675342599994,5.2,2.91530790699999));
#341449=CARTESIAN_POINT('Ctrl Pts',(3.62675342599994,2.2,2.91530790699999));
#341450=CARTESIAN_POINT('Ctrl Pts',(3.62762596899994,12.2,2.91766684499999));
#341451=CARTESIAN_POINT('Ctrl Pts',(3.62762596899994,5.2,2.91766684499999));
#341452=CARTESIAN_POINT('Ctrl Pts',(3.62762596899994,2.2,2.91766684499999));
#341453=CARTESIAN_POINT('Ctrl Pts',(3.62849724599994,12.2,2.92002999699999));
#341454=CARTESIAN_POINT('Ctrl Pts',(3.62849724599994,5.2,2.92002999699999));
#341455=CARTESIAN_POINT('Ctrl Pts',(3.62849724599994,2.2,2.92002999699999));
#341456=CARTESIAN_POINT('Ctrl Pts',(3.62936724899994,12.2,2.92239736099998));
#341457=CARTESIAN_POINT('Ctrl Pts',(3.62936724899994,5.2,2.92239736099998));
#341458=CARTESIAN_POINT('Ctrl Pts',(3.62936724899994,2.2,2.92239736099998));
#341459=CARTESIAN_POINT('Ctrl Pts',(3.63023596899994,12.2,2.92476893199999));
#341460=CARTESIAN_POINT('Ctrl Pts',(3.63023596899994,5.2,2.92476893199999));
#341461=CARTESIAN_POINT('Ctrl Pts',(3.63023596899994,2.2,2.92476893199999));
#341462=CARTESIAN_POINT('Ctrl Pts',(3.63110339699994,12.2,2.92714470699998));
#341463=CARTESIAN_POINT('Ctrl Pts',(3.63110339699994,5.2,2.92714470699998));
#341464=CARTESIAN_POINT('Ctrl Pts',(3.63110339699994,2.2,2.92714470699998));
#341465=CARTESIAN_POINT('Ctrl Pts',(3.63196952799994,12.2,2.92952468299998));
#341466=CARTESIAN_POINT('Ctrl Pts',(3.63196952799994,5.2,2.92952468299998));
#341467=CARTESIAN_POINT('Ctrl Pts',(3.63196952799994,2.2,2.92952468299998));
#341468=CARTESIAN_POINT('Ctrl Pts',(3.63283434999994,12.2,2.93190885499998));
#341469=CARTESIAN_POINT('Ctrl Pts',(3.63283434999994,5.2,2.93190885499998));
#341470=CARTESIAN_POINT('Ctrl Pts',(3.63283434999994,2.2,2.93190885499998));
#341471=CARTESIAN_POINT('Ctrl Pts',(3.63369785799994,12.2,2.93429721999999));
#341472=CARTESIAN_POINT('Ctrl Pts',(3.63369785799994,5.2,2.93429721999999));
#341473=CARTESIAN_POINT('Ctrl Pts',(3.63369785799994,2.2,2.93429721999999));
#341474=CARTESIAN_POINT('Ctrl Pts',(3.63456004199994,12.2,2.93668977499999));
#341475=CARTESIAN_POINT('Ctrl Pts',(3.63456004199994,5.2,2.93668977499999));
#341476=CARTESIAN_POINT('Ctrl Pts',(3.63456004199994,2.2,2.93668977499999));
#341477=CARTESIAN_POINT('Ctrl Pts',(3.63542089399994,12.2,2.93908651499999));
#341478=CARTESIAN_POINT('Ctrl Pts',(3.63542089399994,5.2,2.93908651499999));
#341479=CARTESIAN_POINT('Ctrl Pts',(3.63542089399994,2.2,2.93908651499999));
#341480=CARTESIAN_POINT('Ctrl Pts',(3.63628040899994,12.2,2.94148743699999));
#341481=CARTESIAN_POINT('Ctrl Pts',(3.63628040899994,5.2,2.94148743699999));
#341482=CARTESIAN_POINT('Ctrl Pts',(3.63628040899994,2.2,2.94148743699999));
#341483=CARTESIAN_POINT('Ctrl Pts',(3.63713857299994,12.2,2.94389253799999));
#341484=CARTESIAN_POINT('Ctrl Pts',(3.63713857299994,5.2,2.94389253799999));
#341485=CARTESIAN_POINT('Ctrl Pts',(3.63713857299994,2.2,2.94389253799999));
#341486=CARTESIAN_POINT('Ctrl Pts',(3.63799538399994,12.2,2.94630181399998));
#341487=CARTESIAN_POINT('Ctrl Pts',(3.63799538399994,5.2,2.94630181399998));
#341488=CARTESIAN_POINT('Ctrl Pts',(3.63799538399994,2.2,2.94630181399998));
#341489=CARTESIAN_POINT('Ctrl Pts',(3.63885082999994,12.2,2.94871525999999));
#341490=CARTESIAN_POINT('Ctrl Pts',(3.63885082999994,5.2,2.94871525999999));
#341491=CARTESIAN_POINT('Ctrl Pts',(3.63885082999994,2.2,2.94871525999999));
#341492=CARTESIAN_POINT('Ctrl Pts',(3.63970490299994,12.2,2.95113287299999));
#341493=CARTESIAN_POINT('Ctrl Pts',(3.63970490299994,5.2,2.95113287299999));
#341494=CARTESIAN_POINT('Ctrl Pts',(3.63970490299994,2.2,2.95113287299999));
#341495=CARTESIAN_POINT('Ctrl Pts',(3.64055759799994,12.2,2.95355464999999));
#341496=CARTESIAN_POINT('Ctrl Pts',(3.64055759799994,5.2,2.95355464999999));
#341497=CARTESIAN_POINT('Ctrl Pts',(3.64055759799994,2.2,2.95355464999999));
#341498=CARTESIAN_POINT('Ctrl Pts',(3.64140890399994,12.2,2.95598058599998));
#341499=CARTESIAN_POINT('Ctrl Pts',(3.64140890399994,5.2,2.95598058599998));
#341500=CARTESIAN_POINT('Ctrl Pts',(3.64140890399994,2.2,2.95598058599998));
#341501=CARTESIAN_POINT('Ctrl Pts',(3.64225881399994,12.2,2.95841067899998));
#341502=CARTESIAN_POINT('Ctrl Pts',(3.64225881399994,5.2,2.95841067899998));
#341503=CARTESIAN_POINT('Ctrl Pts',(3.64225881399994,2.2,2.95841067899998));
#341504=CARTESIAN_POINT('Ctrl Pts',(3.64310732199994,12.2,2.96084492299999));
#341505=CARTESIAN_POINT('Ctrl Pts',(3.64310732199994,5.2,2.96084492299999));
#341506=CARTESIAN_POINT('Ctrl Pts',(3.64310732199994,2.2,2.96084492299999));
#341507=CARTESIAN_POINT('Ctrl Pts',(3.64395441699994,12.2,2.96328331599998));
#341508=CARTESIAN_POINT('Ctrl Pts',(3.64395441699994,5.2,2.96328331599998));
#341509=CARTESIAN_POINT('Ctrl Pts',(3.64395441699994,2.2,2.96328331599998));
#341510=CARTESIAN_POINT('Ctrl Pts',(3.64480009299994,12.2,2.96572585499998));
#341511=CARTESIAN_POINT('Ctrl Pts',(3.64480009299994,5.2,2.96572585499998));
#341512=CARTESIAN_POINT('Ctrl Pts',(3.64480009299994,2.2,2.96572585499998));
#341513=CARTESIAN_POINT('Ctrl Pts',(3.64564434199994,12.2,2.96817253399999));
#341514=CARTESIAN_POINT('Ctrl Pts',(3.64564434199994,5.2,2.96817253399999));
#341515=CARTESIAN_POINT('Ctrl Pts',(3.64564434199994,2.2,2.96817253399999));
#341516=CARTESIAN_POINT('Ctrl Pts',(3.64648715699994,12.2,2.97062334999998));
#341517=CARTESIAN_POINT('Ctrl Pts',(3.64648715699994,5.2,2.97062334999998));
#341518=CARTESIAN_POINT('Ctrl Pts',(3.64648715699994,2.2,2.97062334999998));
#341519=CARTESIAN_POINT('Ctrl Pts',(3.64732852699994,12.2,2.97307830099999));
#341520=CARTESIAN_POINT('Ctrl Pts',(3.64732852699994,5.2,2.97307830099999));
#341521=CARTESIAN_POINT('Ctrl Pts',(3.64732852699994,2.2,2.97307830099999));
#341522=CARTESIAN_POINT('Ctrl Pts',(3.64816844599994,12.2,2.97553737999999));
#341523=CARTESIAN_POINT('Ctrl Pts',(3.64816844599994,5.2,2.97553737999999));
#341524=CARTESIAN_POINT('Ctrl Pts',(3.64816844599994,2.2,2.97553737999999));
#341525=CARTESIAN_POINT('Ctrl Pts',(3.64900690399994,12.2,2.97800058399999));
#341526=CARTESIAN_POINT('Ctrl Pts',(3.64900690399994,5.2,2.97800058399999));
#341527=CARTESIAN_POINT('Ctrl Pts',(3.64900690399994,2.2,2.97800058399999));
#341528=CARTESIAN_POINT('Ctrl Pts',(3.64984389599994,12.2,2.98046791099999));
#341529=CARTESIAN_POINT('Ctrl Pts',(3.64984389599994,5.2,2.98046791099999));
#341530=CARTESIAN_POINT('Ctrl Pts',(3.64984389599994,2.2,2.98046791099999));
#341531=CARTESIAN_POINT('Ctrl Pts',(3.65067941099994,12.2,2.98293935599999));
#341532=CARTESIAN_POINT('Ctrl Pts',(3.65067941099994,5.2,2.98293935599999));
#341533=CARTESIAN_POINT('Ctrl Pts',(3.65067941099994,2.2,2.98293935599999));
#341534=CARTESIAN_POINT('Ctrl Pts',(3.65151344299994,12.2,2.98541491399998));
#341535=CARTESIAN_POINT('Ctrl Pts',(3.65151344299994,5.2,2.98541491399998));
#341536=CARTESIAN_POINT('Ctrl Pts',(3.65151344299994,2.2,2.98541491399998));
#341537=CARTESIAN_POINT('Ctrl Pts',(3.65234598699994,12.2,2.98789458399998));
#341538=CARTESIAN_POINT('Ctrl Pts',(3.65234598699994,5.2,2.98789458399998));
#341539=CARTESIAN_POINT('Ctrl Pts',(3.65234598699994,2.2,2.98789458399998));
#341540=CARTESIAN_POINT('Ctrl Pts',(3.65317703299994,12.2,2.99037836199999));
#341541=CARTESIAN_POINT('Ctrl Pts',(3.65317703299994,5.2,2.99037836199999));
#341542=CARTESIAN_POINT('Ctrl Pts',(3.65317703299994,2.2,2.99037836199999));
#341543=CARTESIAN_POINT('Ctrl Pts',(3.65400657599994,12.2,2.99286624399999));
#341544=CARTESIAN_POINT('Ctrl Pts',(3.65400657599994,5.2,2.99286624399999));
#341545=CARTESIAN_POINT('Ctrl Pts',(3.65400657599994,2.2,2.99286624399999));
#341546=CARTESIAN_POINT('Ctrl Pts',(3.65483460699994,12.2,2.99535822499998));
#341547=CARTESIAN_POINT('Ctrl Pts',(3.65483460699994,5.2,2.99535822499998));
#341548=CARTESIAN_POINT('Ctrl Pts',(3.65483460699994,2.2,2.99535822499998));
#341549=CARTESIAN_POINT('Ctrl Pts',(3.65566111799994,12.2,2.99785430299998));
#341550=CARTESIAN_POINT('Ctrl Pts',(3.65566111799994,5.2,2.99785430299998));
#341551=CARTESIAN_POINT('Ctrl Pts',(3.65566111799994,2.2,2.99785430299998));
#341552=CARTESIAN_POINT('Ctrl Pts',(3.65648609799994,12.2,3.00035447199999));
#341553=CARTESIAN_POINT('Ctrl Pts',(3.65648609799994,5.2,3.00035447199999));
#341554=CARTESIAN_POINT('Ctrl Pts',(3.65648609799994,2.2,3.00035447199999));
#341555=CARTESIAN_POINT('Ctrl Pts',(3.65730953999994,12.2,3.00285872699998));
#341556=CARTESIAN_POINT('Ctrl Pts',(3.65730953999994,5.2,3.00285872699998));
#341557=CARTESIAN_POINT('Ctrl Pts',(3.65730953999994,2.2,3.00285872699998));
#341558=CARTESIAN_POINT('Ctrl Pts',(3.65813143199994,12.2,3.00536706399999));
#341559=CARTESIAN_POINT('Ctrl Pts',(3.65813143199994,5.2,3.00536706399999));
#341560=CARTESIAN_POINT('Ctrl Pts',(3.65813143199994,2.2,3.00536706399999));
#341561=CARTESIAN_POINT('Ctrl Pts',(3.65895176799994,12.2,3.00787947899998));
#341562=CARTESIAN_POINT('Ctrl Pts',(3.65895176799994,5.2,3.00787947899998));
#341563=CARTESIAN_POINT('Ctrl Pts',(3.65895176799994,2.2,3.00787947899998));
#341564=CARTESIAN_POINT('Ctrl Pts',(3.65977053899994,12.2,3.01039596699999));
#341565=CARTESIAN_POINT('Ctrl Pts',(3.65977053899994,5.2,3.01039596699999));
#341566=CARTESIAN_POINT('Ctrl Pts',(3.65977053899994,2.2,3.01039596699999));
#341567=CARTESIAN_POINT('Ctrl Pts',(3.66058773799994,12.2,3.01291652599998));
#341568=CARTESIAN_POINT('Ctrl Pts',(3.66058773799994,5.2,3.01291652599998));
#341569=CARTESIAN_POINT('Ctrl Pts',(3.66058773799994,2.2,3.01291652599998));
#341570=CARTESIAN_POINT('Ctrl Pts',(3.66140336299994,12.2,3.01544115399999));
#341571=CARTESIAN_POINT('Ctrl Pts',(3.66140336299994,5.2,3.01544115399999));
#341572=CARTESIAN_POINT('Ctrl Pts',(3.66140336299994,2.2,3.01544115399999));
#341573=CARTESIAN_POINT('Ctrl Pts',(3.66221741303907,12.2,3.01796985012154));
#341574=CARTESIAN_POINT('Ctrl Pts',(3.66221741303907,5.2,3.01796985012154));
#341575=CARTESIAN_POINT('Ctrl Pts',(3.66221741303907,2.2,3.01796985012154));
#341576=CARTESIAN_POINT('Ctrl Pts',(3.66286739107805,12.2,3.01999606024348));
#341577=CARTESIAN_POINT('Ctrl Pts',(3.66286739107805,5.2,3.01999606024348));
#341578=CARTESIAN_POINT('Ctrl Pts',(3.66286739107805,2.2,3.01999606024348));
#341579=CARTESIAN_POINT('Ctrl Pts',(3.66335416511694,12.2,3.02151754936566));
#341580=CARTESIAN_POINT('Ctrl Pts',(3.66335416511694,5.2,3.02151754936566));
#341581=CARTESIAN_POINT('Ctrl Pts',(3.66335416511694,2.2,3.02151754936566));
#341582=CARTESIAN_POINT('Ctrl Pts',(3.66367836615578,12.2,3.02253268748795));
#341583=CARTESIAN_POINT('Ctrl Pts',(3.66367836615578,5.2,3.02253268748795));
#341584=CARTESIAN_POINT('Ctrl Pts',(3.66367836615578,2.2,3.02253268748795));
#341585=CARTESIAN_POINT('Ctrl Pts',(3.66384038699994,12.2,3.02304045999998));
#341586=CARTESIAN_POINT('Ctrl Pts',(3.66384038699994,5.2,3.02304045999998));
#341587=CARTESIAN_POINT('Ctrl Pts',(3.66384038699994,2.2,3.02304045999998));
#341588=CARTESIAN_POINT('Origin',(-5.66300478732629E-14,15.2,-1.77635683940025E-14));
#341589=CARTESIAN_POINT('',(3.24327759199994,2.2,1.61918975399999));
#341590=CARTESIAN_POINT('Origin',(3.57314678299994,15.2,1.78387526099999));
#341591=CARTESIAN_POINT('',(3.57319269599994,12.2,1.78389818299999));
#341592=CARTESIAN_POINT('Ctrl Pts',(4.39111701799995,12.2,1.81124027399999));
#341593=CARTESIAN_POINT('Ctrl Pts',(4.39111701799995,5.2,1.81124027399999));
#341594=CARTESIAN_POINT('Ctrl Pts',(4.39111701799995,2.2,1.81124027399999));
#341595=CARTESIAN_POINT('Ctrl Pts',(4.39059271499994,12.2,1.81133614099998));
#341596=CARTESIAN_POINT('Ctrl Pts',(4.39059271499994,5.2,1.81133614099998));
#341597=CARTESIAN_POINT('Ctrl Pts',(4.39059271499994,2.2,1.81133614099998));
#341598=CARTESIAN_POINT('Ctrl Pts',(4.38954439399994,12.2,1.81152754399998));
#341599=CARTESIAN_POINT('Ctrl Pts',(4.38954439399994,5.2,1.81152754399998));
#341600=CARTESIAN_POINT('Ctrl Pts',(4.38954439399994,2.2,1.81152754399998));
#341601=CARTESIAN_POINT('Ctrl Pts',(4.38797276699994,12.2,1.81181365699999));
#341602=CARTESIAN_POINT('Ctrl Pts',(4.38797276699994,5.2,1.81181365699999));
#341603=CARTESIAN_POINT('Ctrl Pts',(4.38797276699994,2.2,1.81181365699999));
#341604=CARTESIAN_POINT('Ctrl Pts',(4.38587897099994,12.2,1.81219315899999));
#341605=CARTESIAN_POINT('Ctrl Pts',(4.38587897099994,5.2,1.81219315899999));
#341606=CARTESIAN_POINT('Ctrl Pts',(4.38587897099994,2.2,1.81219315899999));
#341607=CARTESIAN_POINT('Ctrl Pts',(4.38326457499994,12.2,1.81266423099999));
#341608=CARTESIAN_POINT('Ctrl Pts',(4.38326457499994,5.2,1.81266423099999));
#341609=CARTESIAN_POINT('Ctrl Pts',(4.38326457499994,2.2,1.81266423099999));
#341610=CARTESIAN_POINT('Ctrl Pts',(4.38065302599994,12.2,1.81313199799999));
#341611=CARTESIAN_POINT('Ctrl Pts',(4.38065302599994,5.2,1.81313199799999));
#341612=CARTESIAN_POINT('Ctrl Pts',(4.38065302599994,2.2,1.81313199799999));
#341613=CARTESIAN_POINT('Ctrl Pts',(4.37804432799994,12.2,1.81359646299999));
#341614=CARTESIAN_POINT('Ctrl Pts',(4.37804432799994,5.2,1.81359646299999));
#341615=CARTESIAN_POINT('Ctrl Pts',(4.37804432799994,2.2,1.81359646299999));
#341616=CARTESIAN_POINT('Ctrl Pts',(4.37543848299994,12.2,1.81405762699999));
#341617=CARTESIAN_POINT('Ctrl Pts',(4.37543848299994,5.2,1.81405762699999));
#341618=CARTESIAN_POINT('Ctrl Pts',(4.37543848299994,2.2,1.81405762699999));
#341619=CARTESIAN_POINT('Ctrl Pts',(4.37283549799994,12.2,1.81451549399998));
#341620=CARTESIAN_POINT('Ctrl Pts',(4.37283549799994,5.2,1.81451549399998));
#341621=CARTESIAN_POINT('Ctrl Pts',(4.37283549799994,2.2,1.81451549399998));
#341622=CARTESIAN_POINT('Ctrl Pts',(4.37023537799995,12.2,1.81497006899999));
#341623=CARTESIAN_POINT('Ctrl Pts',(4.37023537799995,5.2,1.81497006899999));
#341624=CARTESIAN_POINT('Ctrl Pts',(4.37023537799995,2.2,1.81497006899999));
#341625=CARTESIAN_POINT('Ctrl Pts',(4.36763813199994,12.2,1.81542135599999));
#341626=CARTESIAN_POINT('Ctrl Pts',(4.36763813199994,5.2,1.81542135599999));
#341627=CARTESIAN_POINT('Ctrl Pts',(4.36763813199994,2.2,1.81542135599999));
#341628=CARTESIAN_POINT('Ctrl Pts',(4.36504376699994,12.2,1.81586936299999));
#341629=CARTESIAN_POINT('Ctrl Pts',(4.36504376699994,5.2,1.81586936299999));
#341630=CARTESIAN_POINT('Ctrl Pts',(4.36504376699994,2.2,1.81586936299999));
#341631=CARTESIAN_POINT('Ctrl Pts',(4.36245229199994,12.2,1.81631409599999));
#341632=CARTESIAN_POINT('Ctrl Pts',(4.36245229199994,5.2,1.81631409599999));
#341633=CARTESIAN_POINT('Ctrl Pts',(4.36245229199994,2.2,1.81631409599999));
#341634=CARTESIAN_POINT('Ctrl Pts',(4.35986371899994,12.2,1.81675555999998));
#341635=CARTESIAN_POINT('Ctrl Pts',(4.35986371899994,5.2,1.81675555999998));
#341636=CARTESIAN_POINT('Ctrl Pts',(4.35986371899994,2.2,1.81675555999998));
#341637=CARTESIAN_POINT('Ctrl Pts',(4.35727805099994,12.2,1.81719376199998));
#341638=CARTESIAN_POINT('Ctrl Pts',(4.35727805099994,5.2,1.81719376199998));
#341639=CARTESIAN_POINT('Ctrl Pts',(4.35727805099994,2.2,1.81719376199998));
#341640=CARTESIAN_POINT('Ctrl Pts',(4.35469529799995,12.2,1.81762870599998));
#341641=CARTESIAN_POINT('Ctrl Pts',(4.35469529799995,5.2,1.81762870599998));
#341642=CARTESIAN_POINT('Ctrl Pts',(4.35469529799995,2.2,1.81762870599998));
#341643=CARTESIAN_POINT('Ctrl Pts',(4.35211546599994,12.2,1.81806039799998));
#341644=CARTESIAN_POINT('Ctrl Pts',(4.35211546599994,5.2,1.81806039799998));
#341645=CARTESIAN_POINT('Ctrl Pts',(4.35211546599994,2.2,1.81806039799998));
#341646=CARTESIAN_POINT('Ctrl Pts',(4.34953856099995,12.2,1.81848884099999));
#341647=CARTESIAN_POINT('Ctrl Pts',(4.34953856099995,5.2,1.81848884099999));
#341648=CARTESIAN_POINT('Ctrl Pts',(4.34953856099995,2.2,1.81848884099999));
#341649=CARTESIAN_POINT('Ctrl Pts',(4.34696458899994,12.2,1.81891403999999));
#341650=CARTESIAN_POINT('Ctrl Pts',(4.34696458899994,5.2,1.81891403999999));
#341651=CARTESIAN_POINT('Ctrl Pts',(4.34696458899994,2.2,1.81891403999999));
#341652=CARTESIAN_POINT('Ctrl Pts',(4.34439355799995,12.2,1.81933599999998));
#341653=CARTESIAN_POINT('Ctrl Pts',(4.34439355799995,5.2,1.81933599999998));
#341654=CARTESIAN_POINT('Ctrl Pts',(4.34439355799995,2.2,1.81933599999998));
#341655=CARTESIAN_POINT('Ctrl Pts',(4.34182547399994,12.2,1.81975472699999));
#341656=CARTESIAN_POINT('Ctrl Pts',(4.34182547399994,5.2,1.81975472699999));
#341657=CARTESIAN_POINT('Ctrl Pts',(4.34182547399994,2.2,1.81975472699999));
#341658=CARTESIAN_POINT('Ctrl Pts',(4.33926034299995,12.2,1.82017022399998));
#341659=CARTESIAN_POINT('Ctrl Pts',(4.33926034299995,5.2,1.82017022399998));
#341660=CARTESIAN_POINT('Ctrl Pts',(4.33926034299995,2.2,1.82017022399998));
#341661=CARTESIAN_POINT('Ctrl Pts',(4.33669817299995,12.2,1.82058249799999));
#341662=CARTESIAN_POINT('Ctrl Pts',(4.33669817299995,5.2,1.82058249799999));
#341663=CARTESIAN_POINT('Ctrl Pts',(4.33669817299995,2.2,1.82058249799999));
#341664=CARTESIAN_POINT('Ctrl Pts',(4.33413897099994,12.2,1.82099155399999));
#341665=CARTESIAN_POINT('Ctrl Pts',(4.33413897099994,5.2,1.82099155399999));
#341666=CARTESIAN_POINT('Ctrl Pts',(4.33413897099994,2.2,1.82099155399999));
#341667=CARTESIAN_POINT('Ctrl Pts',(4.33158274699994,12.2,1.82139739699998));
#341668=CARTESIAN_POINT('Ctrl Pts',(4.33158274699994,5.2,1.82139739699998));
#341669=CARTESIAN_POINT('Ctrl Pts',(4.33158274699994,2.2,1.82139739699998));
#341670=CARTESIAN_POINT('Ctrl Pts',(4.32902950299995,12.2,1.82180003299999));
#341671=CARTESIAN_POINT('Ctrl Pts',(4.32902950299995,5.2,1.82180003299999));
#341672=CARTESIAN_POINT('Ctrl Pts',(4.32902950299995,2.2,1.82180003299999));
#341673=CARTESIAN_POINT('Ctrl Pts',(4.32647925199994,12.2,1.82219946699998));
#341674=CARTESIAN_POINT('Ctrl Pts',(4.32647925199994,5.2,1.82219946699998));
#341675=CARTESIAN_POINT('Ctrl Pts',(4.32647925199994,2.2,1.82219946699998));
#341676=CARTESIAN_POINT('Ctrl Pts',(4.32393199699994,12.2,1.82259570299999));
#341677=CARTESIAN_POINT('Ctrl Pts',(4.32393199699994,5.2,1.82259570299999));
#341678=CARTESIAN_POINT('Ctrl Pts',(4.32393199699994,2.2,1.82259570299999));
#341679=CARTESIAN_POINT('Ctrl Pts',(4.32138774599994,12.2,1.82298874899999));
#341680=CARTESIAN_POINT('Ctrl Pts',(4.32138774599994,5.2,1.82298874899999));
#341681=CARTESIAN_POINT('Ctrl Pts',(4.32138774599994,2.2,1.82298874899999));
#341682=CARTESIAN_POINT('Ctrl Pts',(4.31884650699994,12.2,1.82337860699999));
#341683=CARTESIAN_POINT('Ctrl Pts',(4.31884650699994,5.2,1.82337860699999));
#341684=CARTESIAN_POINT('Ctrl Pts',(4.31884650699994,2.2,1.82337860699999));
#341685=CARTESIAN_POINT('Ctrl Pts',(4.31630828499994,12.2,1.82376528399999));
#341686=CARTESIAN_POINT('Ctrl Pts',(4.31630828499994,5.2,1.82376528399999));
#341687=CARTESIAN_POINT('Ctrl Pts',(4.31630828499994,2.2,1.82376528399999));
#341688=CARTESIAN_POINT('Ctrl Pts',(4.31377308699994,12.2,1.82414878599999));
#341689=CARTESIAN_POINT('Ctrl Pts',(4.31377308699994,5.2,1.82414878599999));
#341690=CARTESIAN_POINT('Ctrl Pts',(4.31377308699994,2.2,1.82414878599999));
#341691=CARTESIAN_POINT('Ctrl Pts',(4.31124092199994,12.2,1.82452911599999));
#341692=CARTESIAN_POINT('Ctrl Pts',(4.31124092199994,5.2,1.82452911599999));
#341693=CARTESIAN_POINT('Ctrl Pts',(4.31124092199994,2.2,1.82452911599999));
#341694=CARTESIAN_POINT('Ctrl Pts',(4.30871179599994,12.2,1.82490628099998));
#341695=CARTESIAN_POINT('Ctrl Pts',(4.30871179599994,5.2,1.82490628099998));
#341696=CARTESIAN_POINT('Ctrl Pts',(4.30871179599994,2.2,1.82490628099998));
#341697=CARTESIAN_POINT('Ctrl Pts',(4.30618571699994,12.2,1.82528028499998));
#341698=CARTESIAN_POINT('Ctrl Pts',(4.30618571699994,5.2,1.82528028499998));
#341699=CARTESIAN_POINT('Ctrl Pts',(4.30618571699994,2.2,1.82528028499998));
#341700=CARTESIAN_POINT('Ctrl Pts',(4.30366269099994,12.2,1.82565113499999));
#341701=CARTESIAN_POINT('Ctrl Pts',(4.30366269099994,5.2,1.82565113499999));
#341702=CARTESIAN_POINT('Ctrl Pts',(4.30366269099994,2.2,1.82565113499999));
#341703=CARTESIAN_POINT('Ctrl Pts',(4.30114272499994,12.2,1.82601883599999));
#341704=CARTESIAN_POINT('Ctrl Pts',(4.30114272499994,5.2,1.82601883599999));
#341705=CARTESIAN_POINT('Ctrl Pts',(4.30114272499994,2.2,1.82601883599999));
#341706=CARTESIAN_POINT('Ctrl Pts',(4.29862582699994,12.2,1.82638339399999));
#341707=CARTESIAN_POINT('Ctrl Pts',(4.29862582699994,5.2,1.82638339399999));
#341708=CARTESIAN_POINT('Ctrl Pts',(4.29862582699994,2.2,1.82638339399999));
#341709=CARTESIAN_POINT('Ctrl Pts',(4.29611200199994,12.2,1.82674481199999));
#341710=CARTESIAN_POINT('Ctrl Pts',(4.29611200199994,5.2,1.82674481199999));
#341711=CARTESIAN_POINT('Ctrl Pts',(4.29611200199994,2.2,1.82674481199999));
#341712=CARTESIAN_POINT('Ctrl Pts',(4.29360125999994,12.2,1.82710309799999));
#341713=CARTESIAN_POINT('Ctrl Pts',(4.29360125999994,5.2,1.82710309799999));
#341714=CARTESIAN_POINT('Ctrl Pts',(4.29360125999994,2.2,1.82710309799999));
#341715=CARTESIAN_POINT('Ctrl Pts',(4.29109360699994,12.2,1.82745825599998));
#341716=CARTESIAN_POINT('Ctrl Pts',(4.29109360699994,5.2,1.82745825599998));
#341717=CARTESIAN_POINT('Ctrl Pts',(4.29109360699994,2.2,1.82745825599998));
#341718=CARTESIAN_POINT('Ctrl Pts',(4.28858904899994,12.2,1.82781029199999));
#341719=CARTESIAN_POINT('Ctrl Pts',(4.28858904899994,5.2,1.82781029199999));
#341720=CARTESIAN_POINT('Ctrl Pts',(4.28858904899994,2.2,1.82781029199999));
#341721=CARTESIAN_POINT('Ctrl Pts',(4.28608759299994,12.2,1.82815921199999));
#341722=CARTESIAN_POINT('Ctrl Pts',(4.28608759299994,5.2,1.82815921199999));
#341723=CARTESIAN_POINT('Ctrl Pts',(4.28608759299994,2.2,1.82815921199999));
#341724=CARTESIAN_POINT('Ctrl Pts',(4.28358924799995,12.2,1.82850502099999));
#341725=CARTESIAN_POINT('Ctrl Pts',(4.28358924799995,5.2,1.82850502099999));
#341726=CARTESIAN_POINT('Ctrl Pts',(4.28358924799995,2.2,1.82850502099999));
#341727=CARTESIAN_POINT('Ctrl Pts',(4.28109401899994,12.2,1.82884772299999));
#341728=CARTESIAN_POINT('Ctrl Pts',(4.28109401899994,5.2,1.82884772299999));
#341729=CARTESIAN_POINT('Ctrl Pts',(4.28109401899994,2.2,1.82884772299999));
#341730=CARTESIAN_POINT('Ctrl Pts',(4.27860191399995,12.2,1.82918732499999));
#341731=CARTESIAN_POINT('Ctrl Pts',(4.27860191399995,5.2,1.82918732499999));
#341732=CARTESIAN_POINT('Ctrl Pts',(4.27860191399995,2.2,1.82918732499999));
#341733=CARTESIAN_POINT('Ctrl Pts',(4.27611294099994,12.2,1.82952383399998));
#341734=CARTESIAN_POINT('Ctrl Pts',(4.27611294099994,5.2,1.82952383399998));
#341735=CARTESIAN_POINT('Ctrl Pts',(4.27611294099994,2.2,1.82952383399998));
#341736=CARTESIAN_POINT('Ctrl Pts',(4.27362710499995,12.2,1.82985725299998));
#341737=CARTESIAN_POINT('Ctrl Pts',(4.27362710499995,5.2,1.82985725299998));
#341738=CARTESIAN_POINT('Ctrl Pts',(4.27362710499995,2.2,1.82985725299998));
#341739=CARTESIAN_POINT('Ctrl Pts',(4.27114441499994,12.2,1.83018758799999));
#341740=CARTESIAN_POINT('Ctrl Pts',(4.27114441499994,5.2,1.83018758799999));
#341741=CARTESIAN_POINT('Ctrl Pts',(4.27114441499994,2.2,1.83018758799999));
#341742=CARTESIAN_POINT('Ctrl Pts',(4.26866487599994,12.2,1.83051484599998));
#341743=CARTESIAN_POINT('Ctrl Pts',(4.26866487599994,5.2,1.83051484599998));
#341744=CARTESIAN_POINT('Ctrl Pts',(4.26866487599994,2.2,1.83051484599998));
#341745=CARTESIAN_POINT('Ctrl Pts',(4.26618849699994,12.2,1.83083903299998));
#341746=CARTESIAN_POINT('Ctrl Pts',(4.26618849699994,5.2,1.83083903299998));
#341747=CARTESIAN_POINT('Ctrl Pts',(4.26618849699994,2.2,1.83083903299998));
#341748=CARTESIAN_POINT('Ctrl Pts',(4.26371528399994,12.2,1.83116015199999));
#341749=CARTESIAN_POINT('Ctrl Pts',(4.26371528399994,5.2,1.83116015199999));
#341750=CARTESIAN_POINT('Ctrl Pts',(4.26371528399994,2.2,1.83116015199999));
#341751=CARTESIAN_POINT('Ctrl Pts',(4.26124524499994,12.2,1.83147820999999));
#341752=CARTESIAN_POINT('Ctrl Pts',(4.26124524499994,5.2,1.83147820999999));
#341753=CARTESIAN_POINT('Ctrl Pts',(4.26124524499994,2.2,1.83147820999999));
#341754=CARTESIAN_POINT('Ctrl Pts',(4.25877838699994,12.2,1.83179321299999));
#341755=CARTESIAN_POINT('Ctrl Pts',(4.25877838699994,5.2,1.83179321299999));
#341756=CARTESIAN_POINT('Ctrl Pts',(4.25877838699994,2.2,1.83179321299999));
#341757=CARTESIAN_POINT('Ctrl Pts',(4.25631471599995,12.2,1.83210516699999));
#341758=CARTESIAN_POINT('Ctrl Pts',(4.25631471599995,5.2,1.83210516699999));
#341759=CARTESIAN_POINT('Ctrl Pts',(4.25631471599995,2.2,1.83210516699999));
#341760=CARTESIAN_POINT('Ctrl Pts',(4.25385423899994,12.2,1.83241407499999));
#341761=CARTESIAN_POINT('Ctrl Pts',(4.25385423899994,5.2,1.83241407499999));
#341762=CARTESIAN_POINT('Ctrl Pts',(4.25385423899994,2.2,1.83241407499999));
#341763=CARTESIAN_POINT('Ctrl Pts',(4.25139696499994,12.2,1.83271994799998));
#341764=CARTESIAN_POINT('Ctrl Pts',(4.25139696499994,5.2,1.83271994799998));
#341765=CARTESIAN_POINT('Ctrl Pts',(4.25139696499994,2.2,1.83271994799998));
#341766=CARTESIAN_POINT('Ctrl Pts',(4.24894289999994,12.2,1.83302278599998));
#341767=CARTESIAN_POINT('Ctrl Pts',(4.24894289999994,5.2,1.83302278599998));
#341768=CARTESIAN_POINT('Ctrl Pts',(4.24894289999994,2.2,1.83302278599998));
#341769=CARTESIAN_POINT('Ctrl Pts',(4.24649204999994,12.2,1.83332259799998));
#341770=CARTESIAN_POINT('Ctrl Pts',(4.24649204999994,5.2,1.83332259799998));
#341771=CARTESIAN_POINT('Ctrl Pts',(4.24649204999994,2.2,1.83332259799998));
#341772=CARTESIAN_POINT('Ctrl Pts',(4.24404442299994,12.2,1.83361938999999));
#341773=CARTESIAN_POINT('Ctrl Pts',(4.24404442299994,5.2,1.83361938999999));
#341774=CARTESIAN_POINT('Ctrl Pts',(4.24404442299994,2.2,1.83361938999999));
#341775=CARTESIAN_POINT('Ctrl Pts',(4.24160002599994,12.2,1.83391316599999));
#341776=CARTESIAN_POINT('Ctrl Pts',(4.24160002599994,5.2,1.83391316599999));
#341777=CARTESIAN_POINT('Ctrl Pts',(4.24160002599994,2.2,1.83391316599999));
#341778=CARTESIAN_POINT('Ctrl Pts',(4.23915886699994,12.2,1.83420393299999));
#341779=CARTESIAN_POINT('Ctrl Pts',(4.23915886699994,5.2,1.83420393299999));
#341780=CARTESIAN_POINT('Ctrl Pts',(4.23915886699994,2.2,1.83420393299999));
#341781=CARTESIAN_POINT('Ctrl Pts',(4.23672095199994,12.2,1.83449169599998));
#341782=CARTESIAN_POINT('Ctrl Pts',(4.23672095199994,5.2,1.83449169599998));
#341783=CARTESIAN_POINT('Ctrl Pts',(4.23672095199994,2.2,1.83449169599998));
#341784=CARTESIAN_POINT('Ctrl Pts',(4.23428628799994,12.2,1.83477646199998));
#341785=CARTESIAN_POINT('Ctrl Pts',(4.23428628799994,5.2,1.83477646199998));
#341786=CARTESIAN_POINT('Ctrl Pts',(4.23428628799994,2.2,1.83477646199998));
#341787=CARTESIAN_POINT('Ctrl Pts',(4.23185488199994,12.2,1.83505823599999));
#341788=CARTESIAN_POINT('Ctrl Pts',(4.23185488199994,5.2,1.83505823599999));
#341789=CARTESIAN_POINT('Ctrl Pts',(4.23185488199994,2.2,1.83505823599999));
#341790=CARTESIAN_POINT('Ctrl Pts',(4.22942674399994,12.2,1.83533702299998));
#341791=CARTESIAN_POINT('Ctrl Pts',(4.22942674399994,5.2,1.83533702299998));
#341792=CARTESIAN_POINT('Ctrl Pts',(4.22942674399994,2.2,1.83533702299998));
#341793=CARTESIAN_POINT('Ctrl Pts',(4.22700187599994,12.2,1.83561283099999));
#341794=CARTESIAN_POINT('Ctrl Pts',(4.22700187599994,5.2,1.83561283099999));
#341795=CARTESIAN_POINT('Ctrl Pts',(4.22700187599994,2.2,1.83561283099999));
#341796=CARTESIAN_POINT('Ctrl Pts',(4.22458028899994,12.2,1.83588566399999));
#341797=CARTESIAN_POINT('Ctrl Pts',(4.22458028899994,5.2,1.83588566399999));
#341798=CARTESIAN_POINT('Ctrl Pts',(4.22458028899994,2.2,1.83588566399999));
#341799=CARTESIAN_POINT('Ctrl Pts',(4.22216198899994,12.2,1.83615552999999));
#341800=CARTESIAN_POINT('Ctrl Pts',(4.22216198899994,5.2,1.83615552999999));
#341801=CARTESIAN_POINT('Ctrl Pts',(4.22216198899994,2.2,1.83615552999999));
#341802=CARTESIAN_POINT('Ctrl Pts',(4.21974698199994,12.2,1.83642243199999));
#341803=CARTESIAN_POINT('Ctrl Pts',(4.21974698199994,5.2,1.83642243199999));
#341804=CARTESIAN_POINT('Ctrl Pts',(4.21974698199994,2.2,1.83642243199999));
#341805=CARTESIAN_POINT('Ctrl Pts',(4.21733527599994,12.2,1.83668637899999));
#341806=CARTESIAN_POINT('Ctrl Pts',(4.21733527599994,5.2,1.83668637899999));
#341807=CARTESIAN_POINT('Ctrl Pts',(4.21733527599994,2.2,1.83668637899999));
#341808=CARTESIAN_POINT('Ctrl Pts',(4.21492687899994,12.2,1.83694737499998));
#341809=CARTESIAN_POINT('Ctrl Pts',(4.21492687899994,5.2,1.83694737499998));
#341810=CARTESIAN_POINT('Ctrl Pts',(4.21492687899994,2.2,1.83694737499998));
#341811=CARTESIAN_POINT('Ctrl Pts',(4.21252179699994,12.2,1.83720542699998));
#341812=CARTESIAN_POINT('Ctrl Pts',(4.21252179699994,5.2,1.83720542699998));
#341813=CARTESIAN_POINT('Ctrl Pts',(4.21252179699994,2.2,1.83720542699998));
#341814=CARTESIAN_POINT('Ctrl Pts',(4.21012003699994,12.2,1.83746053999998));
#341815=CARTESIAN_POINT('Ctrl Pts',(4.21012003699994,5.2,1.83746053999998));
#341816=CARTESIAN_POINT('Ctrl Pts',(4.21012003699994,2.2,1.83746053999998));
#341817=CARTESIAN_POINT('Ctrl Pts',(4.20772160699994,12.2,1.83771271999999));
#341818=CARTESIAN_POINT('Ctrl Pts',(4.20772160699994,5.2,1.83771271999999));
#341819=CARTESIAN_POINT('Ctrl Pts',(4.20772160699994,2.2,1.83771271999999));
#341820=CARTESIAN_POINT('Ctrl Pts',(4.20532651299994,12.2,1.83796197499999));
#341821=CARTESIAN_POINT('Ctrl Pts',(4.20532651299994,5.2,1.83796197499999));
#341822=CARTESIAN_POINT('Ctrl Pts',(4.20532651299994,2.2,1.83796197499999));
#341823=CARTESIAN_POINT('Ctrl Pts',(4.20293476299994,12.2,1.83820830899998));
#341824=CARTESIAN_POINT('Ctrl Pts',(4.20293476299994,5.2,1.83820830899998));
#341825=CARTESIAN_POINT('Ctrl Pts',(4.20293476299994,2.2,1.83820830899998));
#341826=CARTESIAN_POINT('Ctrl Pts',(4.20054636399994,12.2,1.83845172799999));
#341827=CARTESIAN_POINT('Ctrl Pts',(4.20054636399994,5.2,1.83845172799999));
#341828=CARTESIAN_POINT('Ctrl Pts',(4.20054636399994,2.2,1.83845172799999));
#341829=CARTESIAN_POINT('Ctrl Pts',(4.19816132099994,12.2,1.83869223899999));
#341830=CARTESIAN_POINT('Ctrl Pts',(4.19816132099994,5.2,1.83869223899999));
#341831=CARTESIAN_POINT('Ctrl Pts',(4.19816132099994,2.2,1.83869223899999));
#341832=CARTESIAN_POINT('Ctrl Pts',(4.19577964499994,12.2,1.83892984999999));
#341833=CARTESIAN_POINT('Ctrl Pts',(4.19577964499994,5.2,1.83892984999999));
#341834=CARTESIAN_POINT('Ctrl Pts',(4.19577964499994,2.2,1.83892984999999));
#341835=CARTESIAN_POINT('Ctrl Pts',(4.19340133999994,12.2,1.83916456299999));
#341836=CARTESIAN_POINT('Ctrl Pts',(4.19340133999994,5.2,1.83916456299999));
#341837=CARTESIAN_POINT('Ctrl Pts',(4.19340133999994,2.2,1.83916456299999));
#341838=CARTESIAN_POINT('Ctrl Pts',(4.19102641499994,12.2,1.83939638699998));
#341839=CARTESIAN_POINT('Ctrl Pts',(4.19102641499994,5.2,1.83939638699998));
#341840=CARTESIAN_POINT('Ctrl Pts',(4.19102641499994,2.2,1.83939638699998));
#341841=CARTESIAN_POINT('Ctrl Pts',(4.18865487599995,12.2,1.83962532699999));
#341842=CARTESIAN_POINT('Ctrl Pts',(4.18865487599995,5.2,1.83962532699999));
#341843=CARTESIAN_POINT('Ctrl Pts',(4.18865487599995,2.2,1.83962532699999));
#341844=CARTESIAN_POINT('Ctrl Pts',(4.18628672999994,12.2,1.83985138999998));
#341845=CARTESIAN_POINT('Ctrl Pts',(4.18628672999994,5.2,1.83985138999998));
#341846=CARTESIAN_POINT('Ctrl Pts',(4.18628672999994,2.2,1.83985138999998));
#341847=CARTESIAN_POINT('Ctrl Pts',(4.18392198399994,12.2,1.84007458199998));
#341848=CARTESIAN_POINT('Ctrl Pts',(4.18392198399994,5.2,1.84007458199998));
#341849=CARTESIAN_POINT('Ctrl Pts',(4.18392198399994,2.2,1.84007458199998));
#341850=CARTESIAN_POINT('Ctrl Pts',(4.18156064699994,12.2,1.84029490799999));
#341851=CARTESIAN_POINT('Ctrl Pts',(4.18156064699994,5.2,1.84029490799999));
#341852=CARTESIAN_POINT('Ctrl Pts',(4.18156064699994,2.2,1.84029490799999));
#341853=CARTESIAN_POINT('Ctrl Pts',(4.17920272399994,12.2,1.84051237599999));
#341854=CARTESIAN_POINT('Ctrl Pts',(4.17920272399994,5.2,1.84051237599999));
#341855=CARTESIAN_POINT('Ctrl Pts',(4.17920272399994,2.2,1.84051237599999));
#341856=CARTESIAN_POINT('Ctrl Pts',(4.17684822299994,12.2,1.84072699099998));
#341857=CARTESIAN_POINT('Ctrl Pts',(4.17684822299994,5.2,1.84072699099998));
#341858=CARTESIAN_POINT('Ctrl Pts',(4.17684822299994,2.2,1.84072699099998));
#341859=CARTESIAN_POINT('Ctrl Pts',(4.17449715099994,12.2,1.84093875999999));
#341860=CARTESIAN_POINT('Ctrl Pts',(4.17449715099994,5.2,1.84093875999999));
#341861=CARTESIAN_POINT('Ctrl Pts',(4.17449715099994,2.2,1.84093875999999));
#341862=CARTESIAN_POINT('Ctrl Pts',(4.17214951399994,12.2,1.84114768899999));
#341863=CARTESIAN_POINT('Ctrl Pts',(4.17214951399994,5.2,1.84114768899999));
#341864=CARTESIAN_POINT('Ctrl Pts',(4.17214951399994,2.2,1.84114768899999));
#341865=CARTESIAN_POINT('Ctrl Pts',(4.16980532099995,12.2,1.84135378499999));
#341866=CARTESIAN_POINT('Ctrl Pts',(4.16980532099995,5.2,1.84135378499999));
#341867=CARTESIAN_POINT('Ctrl Pts',(4.16980532099995,2.2,1.84135378499999));
#341868=CARTESIAN_POINT('Ctrl Pts',(4.16746457899994,12.2,1.84155705199998));
#341869=CARTESIAN_POINT('Ctrl Pts',(4.16746457899994,5.2,1.84155705199998));
#341870=CARTESIAN_POINT('Ctrl Pts',(4.16746457899994,2.2,1.84155705199998));
#341871=CARTESIAN_POINT('Ctrl Pts',(4.16512729299995,12.2,1.84175749999998));
#341872=CARTESIAN_POINT('Ctrl Pts',(4.16512729299995,5.2,1.84175749999998));
#341873=CARTESIAN_POINT('Ctrl Pts',(4.16512729299995,2.2,1.84175749999998));
#341874=CARTESIAN_POINT('Ctrl Pts',(4.16279347199994,12.2,1.84195513199999));
#341875=CARTESIAN_POINT('Ctrl Pts',(4.16279347199994,5.2,1.84195513199999));
#341876=CARTESIAN_POINT('Ctrl Pts',(4.16279347199994,2.2,1.84195513199999));
#341877=CARTESIAN_POINT('Ctrl Pts',(4.16046312299994,12.2,1.84214995599998));
#341878=CARTESIAN_POINT('Ctrl Pts',(4.16046312299994,5.2,1.84214995599998));
#341879=CARTESIAN_POINT('Ctrl Pts',(4.16046312299994,2.2,1.84214995599998));
#341880=CARTESIAN_POINT('Ctrl Pts',(4.15813625299995,12.2,1.84234197899999));
#341881=CARTESIAN_POINT('Ctrl Pts',(4.15813625299995,5.2,1.84234197899999));
#341882=CARTESIAN_POINT('Ctrl Pts',(4.15813625299995,2.2,1.84234197899999));
#341883=CARTESIAN_POINT('Ctrl Pts',(4.15581286799994,12.2,1.84253120599998));
#341884=CARTESIAN_POINT('Ctrl Pts',(4.15581286799994,5.2,1.84253120599998));
#341885=CARTESIAN_POINT('Ctrl Pts',(4.15581286799994,2.2,1.84253120599998));
#341886=CARTESIAN_POINT('Ctrl Pts',(4.15349297599994,12.2,1.84271764399998));
#341887=CARTESIAN_POINT('Ctrl Pts',(4.15349297599994,5.2,1.84271764399998));
#341888=CARTESIAN_POINT('Ctrl Pts',(4.15349297599994,2.2,1.84271764399998));
#341889=CARTESIAN_POINT('Ctrl Pts',(4.15117658499994,12.2,1.84290129899999));
#341890=CARTESIAN_POINT('Ctrl Pts',(4.15117658499994,5.2,1.84290129899999));
#341891=CARTESIAN_POINT('Ctrl Pts',(4.15117658499994,2.2,1.84290129899999));
#341892=CARTESIAN_POINT('Ctrl Pts',(4.14886370099994,12.2,1.84308217899999));
#341893=CARTESIAN_POINT('Ctrl Pts',(4.14886370099994,5.2,1.84308217899999));
#341894=CARTESIAN_POINT('Ctrl Pts',(4.14886370099994,2.2,1.84308217899999));
#341895=CARTESIAN_POINT('Ctrl Pts',(4.14655433099994,12.2,1.84326028799998));
#341896=CARTESIAN_POINT('Ctrl Pts',(4.14655433099994,5.2,1.84326028799998));
#341897=CARTESIAN_POINT('Ctrl Pts',(4.14655433099994,2.2,1.84326028799998));
#341898=CARTESIAN_POINT('Ctrl Pts',(4.14424848299995,12.2,1.84343563499999));
#341899=CARTESIAN_POINT('Ctrl Pts',(4.14424848299995,5.2,1.84343563499999));
#341900=CARTESIAN_POINT('Ctrl Pts',(4.14424848299995,2.2,1.84343563499999));
#341901=CARTESIAN_POINT('Ctrl Pts',(4.14194616299994,12.2,1.84360822599999));
#341902=CARTESIAN_POINT('Ctrl Pts',(4.14194616299994,5.2,1.84360822599999));
#341903=CARTESIAN_POINT('Ctrl Pts',(4.14194616299994,2.2,1.84360822599999));
#341904=CARTESIAN_POINT('Ctrl Pts',(4.13964737899994,12.2,1.84377806599999));
#341905=CARTESIAN_POINT('Ctrl Pts',(4.13964737899994,5.2,1.84377806599999));
#341906=CARTESIAN_POINT('Ctrl Pts',(4.13964737899994,2.2,1.84377806599999));
#341907=CARTESIAN_POINT('Ctrl Pts',(4.13735213799994,12.2,1.84394516299998));
#341908=CARTESIAN_POINT('Ctrl Pts',(4.13735213799994,5.2,1.84394516299998));
#341909=CARTESIAN_POINT('Ctrl Pts',(4.13735213799994,2.2,1.84394516299998));
#341910=CARTESIAN_POINT('Ctrl Pts',(4.13506044699994,12.2,1.84410952299999));
#341911=CARTESIAN_POINT('Ctrl Pts',(4.13506044699994,5.2,1.84410952299999));
#341912=CARTESIAN_POINT('Ctrl Pts',(4.13506044699994,2.2,1.84410952299999));
#341913=CARTESIAN_POINT('Ctrl Pts',(4.13277231299995,12.2,1.84427115299998));
#341914=CARTESIAN_POINT('Ctrl Pts',(4.13277231299995,5.2,1.84427115299998));
#341915=CARTESIAN_POINT('Ctrl Pts',(4.13277231299995,2.2,1.84427115299998));
#341916=CARTESIAN_POINT('Ctrl Pts',(4.13048774299994,12.2,1.84443005899999));
#341917=CARTESIAN_POINT('Ctrl Pts',(4.13048774299994,5.2,1.84443005899999));
#341918=CARTESIAN_POINT('Ctrl Pts',(4.13048774299994,2.2,1.84443005899999));
#341919=CARTESIAN_POINT('Ctrl Pts',(4.12820674499994,12.2,1.84458624799999));
#341920=CARTESIAN_POINT('Ctrl Pts',(4.12820674499994,5.2,1.84458624799999));
#341921=CARTESIAN_POINT('Ctrl Pts',(4.12820674499994,2.2,1.84458624799999));
#341922=CARTESIAN_POINT('Ctrl Pts',(4.12592932499994,12.2,1.84473972799998));
#341923=CARTESIAN_POINT('Ctrl Pts',(4.12592932499994,5.2,1.84473972799998));
#341924=CARTESIAN_POINT('Ctrl Pts',(4.12592932499994,2.2,1.84473972799998));
#341925=CARTESIAN_POINT('Ctrl Pts',(4.12365549099994,12.2,1.84489050299999));
#341926=CARTESIAN_POINT('Ctrl Pts',(4.12365549099994,5.2,1.84489050299999));
#341927=CARTESIAN_POINT('Ctrl Pts',(4.12365549099994,2.2,1.84489050299999));
#341928=CARTESIAN_POINT('Ctrl Pts',(4.12138524999994,12.2,1.84503858199998));
#341929=CARTESIAN_POINT('Ctrl Pts',(4.12138524999994,5.2,1.84503858199998));
#341930=CARTESIAN_POINT('Ctrl Pts',(4.12138524999994,2.2,1.84503858199998));
#341931=CARTESIAN_POINT('Ctrl Pts',(4.11911860799994,12.2,1.84518396999998));
#341932=CARTESIAN_POINT('Ctrl Pts',(4.11911860799994,5.2,1.84518396999998));
#341933=CARTESIAN_POINT('Ctrl Pts',(4.11911860799994,2.2,1.84518396999998));
#341934=CARTESIAN_POINT('Ctrl Pts',(4.11685557399994,12.2,1.84532667399999));
#341935=CARTESIAN_POINT('Ctrl Pts',(4.11685557399994,5.2,1.84532667399999));
#341936=CARTESIAN_POINT('Ctrl Pts',(4.11685557399994,2.2,1.84532667399999));
#341937=CARTESIAN_POINT('Ctrl Pts',(4.11459615299994,12.2,1.84546670299999));
#341938=CARTESIAN_POINT('Ctrl Pts',(4.11459615299994,5.2,1.84546670299999));
#341939=CARTESIAN_POINT('Ctrl Pts',(4.11459615299994,2.2,1.84546670299999));
#341940=CARTESIAN_POINT('Ctrl Pts',(4.11234035499994,12.2,1.84560406099999));
#341941=CARTESIAN_POINT('Ctrl Pts',(4.11234035499994,5.2,1.84560406099999));
#341942=CARTESIAN_POINT('Ctrl Pts',(4.11234035499994,2.2,1.84560406099999));
#341943=CARTESIAN_POINT('Ctrl Pts',(4.11008818399995,12.2,1.84573875499999));
#341944=CARTESIAN_POINT('Ctrl Pts',(4.11008818399995,5.2,1.84573875499999));
#341945=CARTESIAN_POINT('Ctrl Pts',(4.11008818399995,2.2,1.84573875499999));
#341946=CARTESIAN_POINT('Ctrl Pts',(4.10783964999994,12.2,1.84587079399999));
#341947=CARTESIAN_POINT('Ctrl Pts',(4.10783964999994,5.2,1.84587079399999));
#341948=CARTESIAN_POINT('Ctrl Pts',(4.10783964999994,2.2,1.84587079399999));
#341949=CARTESIAN_POINT('Ctrl Pts',(4.10559475699994,12.2,1.84600018399999));
#341950=CARTESIAN_POINT('Ctrl Pts',(4.10559475699994,5.2,1.84600018399999));
#341951=CARTESIAN_POINT('Ctrl Pts',(4.10559475699994,2.2,1.84600018399999));
#341952=CARTESIAN_POINT('Ctrl Pts',(4.10335351499994,12.2,1.84612693099998));
#341953=CARTESIAN_POINT('Ctrl Pts',(4.10335351499994,5.2,1.84612693099998));
#341954=CARTESIAN_POINT('Ctrl Pts',(4.10335351499994,2.2,1.84612693099998));
#341955=CARTESIAN_POINT('Ctrl Pts',(4.10111592999994,12.2,1.84625104099998));
#341956=CARTESIAN_POINT('Ctrl Pts',(4.10111592999994,5.2,1.84625104099998));
#341957=CARTESIAN_POINT('Ctrl Pts',(4.10111592999994,2.2,1.84625104099998));
#341958=CARTESIAN_POINT('Ctrl Pts',(4.09888200799994,12.2,1.84637252299999));
#341959=CARTESIAN_POINT('Ctrl Pts',(4.09888200799994,5.2,1.84637252299999));
#341960=CARTESIAN_POINT('Ctrl Pts',(4.09888200799994,2.2,1.84637252299999));
#341961=CARTESIAN_POINT('Ctrl Pts',(4.09665175899994,12.2,1.84649138299998));
#341962=CARTESIAN_POINT('Ctrl Pts',(4.09665175899994,5.2,1.84649138299998));
#341963=CARTESIAN_POINT('Ctrl Pts',(4.09665175899994,2.2,1.84649138299998));
#341964=CARTESIAN_POINT('Ctrl Pts',(4.09442518799994,12.2,1.84660762799998));
#341965=CARTESIAN_POINT('Ctrl Pts',(4.09442518799994,5.2,1.84660762799998));
#341966=CARTESIAN_POINT('Ctrl Pts',(4.09442518799994,2.2,1.84660762799998));
#341967=CARTESIAN_POINT('Ctrl Pts',(4.09220230199994,12.2,1.84672126599999));
#341968=CARTESIAN_POINT('Ctrl Pts',(4.09220230199994,5.2,1.84672126599999));
#341969=CARTESIAN_POINT('Ctrl Pts',(4.09220230199994,2.2,1.84672126599999));
#341970=CARTESIAN_POINT('Ctrl Pts',(4.08998310899995,12.2,1.84683230099999));
#341971=CARTESIAN_POINT('Ctrl Pts',(4.08998310899995,5.2,1.84683230099999));
#341972=CARTESIAN_POINT('Ctrl Pts',(4.08998310899995,2.2,1.84683230099999));
#341973=CARTESIAN_POINT('Ctrl Pts',(4.08776761599994,12.2,1.84694074299999));
#341974=CARTESIAN_POINT('Ctrl Pts',(4.08776761599994,5.2,1.84694074299999));
#341975=CARTESIAN_POINT('Ctrl Pts',(4.08776761599994,2.2,1.84694074299999));
#341976=CARTESIAN_POINT('Ctrl Pts',(4.08555582999994,12.2,1.84704659699999));
#341977=CARTESIAN_POINT('Ctrl Pts',(4.08555582999994,5.2,1.84704659699999));
#341978=CARTESIAN_POINT('Ctrl Pts',(4.08555582999994,2.2,1.84704659699999));
#341979=CARTESIAN_POINT('Ctrl Pts',(4.08334775699995,12.2,1.84714987299999));
#341980=CARTESIAN_POINT('Ctrl Pts',(4.08334775699995,5.2,1.84714987299999));
#341981=CARTESIAN_POINT('Ctrl Pts',(4.08334775699995,2.2,1.84714987299999));
#341982=CARTESIAN_POINT('Ctrl Pts',(4.08114340699994,12.2,1.84725057399998));
#341983=CARTESIAN_POINT('Ctrl Pts',(4.08114340699994,5.2,1.84725057399998));
#341984=CARTESIAN_POINT('Ctrl Pts',(4.08114340699994,2.2,1.84725057399998));
#341985=CARTESIAN_POINT('Ctrl Pts',(4.07894278499994,12.2,1.84734870999999));
#341986=CARTESIAN_POINT('Ctrl Pts',(4.07894278499994,5.2,1.84734870999999));
#341987=CARTESIAN_POINT('Ctrl Pts',(4.07894278499994,2.2,1.84734870999999));
#341988=CARTESIAN_POINT('Ctrl Pts',(4.07674589799994,12.2,1.84744428699998));
#341989=CARTESIAN_POINT('Ctrl Pts',(4.07674589799994,5.2,1.84744428699998));
#341990=CARTESIAN_POINT('Ctrl Pts',(4.07674589799994,2.2,1.84744428699998));
#341991=CARTESIAN_POINT('Ctrl Pts',(4.07455275399994,12.2,1.84753731199998));
#341992=CARTESIAN_POINT('Ctrl Pts',(4.07455275399994,5.2,1.84753731199998));
#341993=CARTESIAN_POINT('Ctrl Pts',(4.07455275399994,2.2,1.84753731199998));
#341994=CARTESIAN_POINT('Ctrl Pts',(4.07236335899994,12.2,1.84762779199998));
#341995=CARTESIAN_POINT('Ctrl Pts',(4.07236335899994,5.2,1.84762779199998));
#341996=CARTESIAN_POINT('Ctrl Pts',(4.07236335899994,2.2,1.84762779199998));
#341997=CARTESIAN_POINT('Ctrl Pts',(4.07017772299994,12.2,1.84771573499999));
#341998=CARTESIAN_POINT('Ctrl Pts',(4.07017772299994,5.2,1.84771573499999));
#341999=CARTESIAN_POINT('Ctrl Pts',(4.07017772299994,2.2,1.84771573499999));
#342000=CARTESIAN_POINT('Ctrl Pts',(4.06799584999994,12.2,1.84780114799999));
#342001=CARTESIAN_POINT('Ctrl Pts',(4.06799584999994,5.2,1.84780114799999));
#342002=CARTESIAN_POINT('Ctrl Pts',(4.06799584999994,2.2,1.84780114799999));
#342003=CARTESIAN_POINT('Ctrl Pts',(4.06581774699994,12.2,1.84788403799999));
#342004=CARTESIAN_POINT('Ctrl Pts',(4.06581774699994,5.2,1.84788403799999));
#342005=CARTESIAN_POINT('Ctrl Pts',(4.06581774699994,2.2,1.84788403799999));
#342006=CARTESIAN_POINT('Ctrl Pts',(4.06364342499994,12.2,1.84796441199999));
#342007=CARTESIAN_POINT('Ctrl Pts',(4.06364342499994,5.2,1.84796441199999));
#342008=CARTESIAN_POINT('Ctrl Pts',(4.06364342499994,2.2,1.84796441199999));
#342009=CARTESIAN_POINT('Ctrl Pts',(4.06147288699994,12.2,1.84804227599999));
#342010=CARTESIAN_POINT('Ctrl Pts',(4.06147288699994,5.2,1.84804227599999));
#342011=CARTESIAN_POINT('Ctrl Pts',(4.06147288699994,2.2,1.84804227599999));
#342012=CARTESIAN_POINT('Ctrl Pts',(4.05930614299994,12.2,1.84811763999999));
#342013=CARTESIAN_POINT('Ctrl Pts',(4.05930614299994,5.2,1.84811763999999));
#342014=CARTESIAN_POINT('Ctrl Pts',(4.05930614299994,2.2,1.84811763999999));
#342015=CARTESIAN_POINT('Ctrl Pts',(4.05714319699995,12.2,1.84819050899999));
#342016=CARTESIAN_POINT('Ctrl Pts',(4.05714319699995,5.2,1.84819050899999));
#342017=CARTESIAN_POINT('Ctrl Pts',(4.05714319699995,2.2,1.84819050899999));
#342018=CARTESIAN_POINT('Ctrl Pts',(4.05498405999994,12.2,1.84826089199999));
#342019=CARTESIAN_POINT('Ctrl Pts',(4.05498405999994,5.2,1.84826089199999));
#342020=CARTESIAN_POINT('Ctrl Pts',(4.05498405999994,2.2,1.84826089199999));
#342021=CARTESIAN_POINT('Ctrl Pts',(4.05282873699994,12.2,1.84832879599998));
#342022=CARTESIAN_POINT('Ctrl Pts',(4.05282873699994,5.2,1.84832879599998));
#342023=CARTESIAN_POINT('Ctrl Pts',(4.05282873699994,2.2,1.84832879599998));
#342024=CARTESIAN_POINT('Ctrl Pts',(4.05067723499995,12.2,1.84839422599998));
#342025=CARTESIAN_POINT('Ctrl Pts',(4.05067723499995,5.2,1.84839422599998));
#342026=CARTESIAN_POINT('Ctrl Pts',(4.05067723499995,2.2,1.84839422599998));
#342027=CARTESIAN_POINT('Ctrl Pts',(4.04852955999994,12.2,1.84845719299998));
#342028=CARTESIAN_POINT('Ctrl Pts',(4.04852955999994,5.2,1.84845719299998));
#342029=CARTESIAN_POINT('Ctrl Pts',(4.04852955999994,2.2,1.84845719299998));
#342030=CARTESIAN_POINT('Ctrl Pts',(4.04638572299994,12.2,1.84851770099999));
#342031=CARTESIAN_POINT('Ctrl Pts',(4.04638572299994,5.2,1.84851770099999));
#342032=CARTESIAN_POINT('Ctrl Pts',(4.04638572299994,2.2,1.84851770099999));
#342033=CARTESIAN_POINT('Ctrl Pts',(4.04424572799994,12.2,1.84857575999999));
#342034=CARTESIAN_POINT('Ctrl Pts',(4.04424572799994,5.2,1.84857575999999));
#342035=CARTESIAN_POINT('Ctrl Pts',(4.04424572799994,2.2,1.84857575999999));
#342036=CARTESIAN_POINT('Ctrl Pts',(4.04210958299995,12.2,1.84863137599999));
#342037=CARTESIAN_POINT('Ctrl Pts',(4.04210958299995,5.2,1.84863137599999));
#342038=CARTESIAN_POINT('Ctrl Pts',(4.04210958299995,2.2,1.84863137599999));
#342039=CARTESIAN_POINT('Ctrl Pts',(4.03997729399994,12.2,1.84868455699998));
#342040=CARTESIAN_POINT('Ctrl Pts',(4.03997729399994,5.2,1.84868455699998));
#342041=CARTESIAN_POINT('Ctrl Pts',(4.03997729399994,2.2,1.84868455699998));
#342042=CARTESIAN_POINT('Ctrl Pts',(4.03784887099994,12.2,1.84873531099999));
#342043=CARTESIAN_POINT('Ctrl Pts',(4.03784887099994,5.2,1.84873531099999));
#342044=CARTESIAN_POINT('Ctrl Pts',(4.03784887099994,2.2,1.84873531099999));
#342045=CARTESIAN_POINT('Ctrl Pts',(4.03572431899994,12.2,1.84878364299998));
#342046=CARTESIAN_POINT('Ctrl Pts',(4.03572431899994,5.2,1.84878364299998));
#342047=CARTESIAN_POINT('Ctrl Pts',(4.03572431899994,2.2,1.84878364299998));
#342048=CARTESIAN_POINT('Ctrl Pts',(4.03360364499994,12.2,1.84882956299999));
#342049=CARTESIAN_POINT('Ctrl Pts',(4.03360364499994,5.2,1.84882956299999));
#342050=CARTESIAN_POINT('Ctrl Pts',(4.03360364499994,2.2,1.84882956299999));
#342051=CARTESIAN_POINT('Ctrl Pts',(4.03148685699994,12.2,1.84887307799999));
#342052=CARTESIAN_POINT('Ctrl Pts',(4.03148685699994,5.2,1.84887307799999));
#342053=CARTESIAN_POINT('Ctrl Pts',(4.03148685699994,2.2,1.84887307799999));
#342054=CARTESIAN_POINT('Ctrl Pts',(4.02937396299994,12.2,1.84891419499999));
#342055=CARTESIAN_POINT('Ctrl Pts',(4.02937396299994,5.2,1.84891419499999));
#342056=CARTESIAN_POINT('Ctrl Pts',(4.02937396299994,2.2,1.84891419499999));
#342057=CARTESIAN_POINT('Ctrl Pts',(4.02726496799994,12.2,1.84895292199998));
#342058=CARTESIAN_POINT('Ctrl Pts',(4.02726496799994,5.2,1.84895292199998));
#342059=CARTESIAN_POINT('Ctrl Pts',(4.02726496799994,2.2,1.84895292199998));
#342060=CARTESIAN_POINT('Ctrl Pts',(4.02515988099994,12.2,1.84898926699999));
#342061=CARTESIAN_POINT('Ctrl Pts',(4.02515988099994,5.2,1.84898926699999));
#342062=CARTESIAN_POINT('Ctrl Pts',(4.02515988099994,2.2,1.84898926699999));
#342063=CARTESIAN_POINT('Ctrl Pts',(4.02305870799994,12.2,1.84902323599998));
#342064=CARTESIAN_POINT('Ctrl Pts',(4.02305870799994,5.2,1.84902323599998));
#342065=CARTESIAN_POINT('Ctrl Pts',(4.02305870799994,2.2,1.84902323599998));
#342066=CARTESIAN_POINT('Ctrl Pts',(4.02096145599994,12.2,1.84905483799998));
#342067=CARTESIAN_POINT('Ctrl Pts',(4.02096145599994,5.2,1.84905483799998));
#342068=CARTESIAN_POINT('Ctrl Pts',(4.02096145599994,2.2,1.84905483799998));
#342069=CARTESIAN_POINT('Ctrl Pts',(4.01886813399994,12.2,1.84908408199998));
#342070=CARTESIAN_POINT('Ctrl Pts',(4.01886813399994,5.2,1.84908408199998));
#342071=CARTESIAN_POINT('Ctrl Pts',(4.01886813399994,2.2,1.84908408199998));
#342072=CARTESIAN_POINT('Ctrl Pts',(4.01677874699994,12.2,1.84911097199999));
#342073=CARTESIAN_POINT('Ctrl Pts',(4.01677874699994,5.2,1.84911097199999));
#342074=CARTESIAN_POINT('Ctrl Pts',(4.01677874699994,2.2,1.84911097199999));
#342075=CARTESIAN_POINT('Ctrl Pts',(4.01469330299994,12.2,1.84913551799998));
#342076=CARTESIAN_POINT('Ctrl Pts',(4.01469330299994,5.2,1.84913551799998));
#342077=CARTESIAN_POINT('Ctrl Pts',(4.01469330299994,2.2,1.84913551799998));
#342078=CARTESIAN_POINT('Ctrl Pts',(4.01261180999995,12.2,1.84915772799998));
#342079=CARTESIAN_POINT('Ctrl Pts',(4.01261180999995,5.2,1.84915772799998));
#342080=CARTESIAN_POINT('Ctrl Pts',(4.01261180999995,2.2,1.84915772799998));
#342081=CARTESIAN_POINT('Ctrl Pts',(4.01053427299995,12.2,1.84917760899999));
#342082=CARTESIAN_POINT('Ctrl Pts',(4.01053427299995,5.2,1.84917760899999));
#342083=CARTESIAN_POINT('Ctrl Pts',(4.01053427299995,2.2,1.84917760899999));
#342084=CARTESIAN_POINT('Ctrl Pts',(4.00846070199994,12.2,1.84919516899999));
#342085=CARTESIAN_POINT('Ctrl Pts',(4.00846070199994,5.2,1.84919516899999));
#342086=CARTESIAN_POINT('Ctrl Pts',(4.00846070199994,2.2,1.84919516899999));
#342087=CARTESIAN_POINT('Ctrl Pts',(4.00639110199995,12.2,1.84921041499999));
#342088=CARTESIAN_POINT('Ctrl Pts',(4.00639110199995,5.2,1.84921041499999));
#342089=CARTESIAN_POINT('Ctrl Pts',(4.00639110199995,2.2,1.84921041499999));
#342090=CARTESIAN_POINT('Ctrl Pts',(4.00432548099994,12.2,1.84922335699999));
#342091=CARTESIAN_POINT('Ctrl Pts',(4.00432548099994,5.2,1.84922335699999));
#342092=CARTESIAN_POINT('Ctrl Pts',(4.00432548099994,2.2,1.84922335699999));
#342093=CARTESIAN_POINT('Ctrl Pts',(4.00226384599994,12.2,1.84923399999999));
#342094=CARTESIAN_POINT('Ctrl Pts',(4.00226384599994,5.2,1.84923399999999));
#342095=CARTESIAN_POINT('Ctrl Pts',(4.00226384599994,2.2,1.84923399999999));
#342096=CARTESIAN_POINT('Ctrl Pts',(4.00020620399994,12.2,1.84924235299999));
#342097=CARTESIAN_POINT('Ctrl Pts',(4.00020620399994,5.2,1.84924235299999));
#342098=CARTESIAN_POINT('Ctrl Pts',(4.00020620399994,2.2,1.84924235299999));
#342099=CARTESIAN_POINT('Ctrl Pts',(3.99815256199994,12.2,1.84924842499999));
#342100=CARTESIAN_POINT('Ctrl Pts',(3.99815256199994,5.2,1.84924842499999));
#342101=CARTESIAN_POINT('Ctrl Pts',(3.99815256199994,2.2,1.84924842499999));
#342102=CARTESIAN_POINT('Ctrl Pts',(3.99610292899994,12.2,1.84925222199999));
#342103=CARTESIAN_POINT('Ctrl Pts',(3.99610292899994,5.2,1.84925222199999));
#342104=CARTESIAN_POINT('Ctrl Pts',(3.99610292899994,2.2,1.84925222199999));
#342105=CARTESIAN_POINT('Ctrl Pts',(3.99405730999994,12.2,1.84925375299999));
#342106=CARTESIAN_POINT('Ctrl Pts',(3.99405730999994,5.2,1.84925375299999));
#342107=CARTESIAN_POINT('Ctrl Pts',(3.99405730999994,2.2,1.84925375299999));
#342108=CARTESIAN_POINT('Ctrl Pts',(3.99201571199994,12.2,1.84925302699999));
#342109=CARTESIAN_POINT('Ctrl Pts',(3.99201571199994,5.2,1.84925302699999));
#342110=CARTESIAN_POINT('Ctrl Pts',(3.99201571199994,2.2,1.84925302699999));
#342111=CARTESIAN_POINT('Ctrl Pts',(3.98997814399995,12.2,1.84925004999998));
#342112=CARTESIAN_POINT('Ctrl Pts',(3.98997814399995,5.2,1.84925004999998));
#342113=CARTESIAN_POINT('Ctrl Pts',(3.98997814399995,2.2,1.84925004999998));
#342114=CARTESIAN_POINT('Ctrl Pts',(3.98794461099994,12.2,1.84924482999998));
#342115=CARTESIAN_POINT('Ctrl Pts',(3.98794461099994,5.2,1.84924482999998));
#342116=CARTESIAN_POINT('Ctrl Pts',(3.98794461099994,2.2,1.84924482999998));
#342117=CARTESIAN_POINT('Ctrl Pts',(3.98591512199994,12.2,1.84923737699998));
#342118=CARTESIAN_POINT('Ctrl Pts',(3.98591512199994,5.2,1.84923737699998));
#342119=CARTESIAN_POINT('Ctrl Pts',(3.98591512199994,2.2,1.84923737699998));
#342120=CARTESIAN_POINT('Ctrl Pts',(3.98388968399995,12.2,1.84922769599998));
#342121=CARTESIAN_POINT('Ctrl Pts',(3.98388968399995,5.2,1.84922769599998));
#342122=CARTESIAN_POINT('Ctrl Pts',(3.98388968399995,2.2,1.84922769599998));
#342123=CARTESIAN_POINT('Ctrl Pts',(3.98186830299994,12.2,1.84921579899999));
#342124=CARTESIAN_POINT('Ctrl Pts',(3.98186830299994,5.2,1.84921579899999));
#342125=CARTESIAN_POINT('Ctrl Pts',(3.98186830299994,2.2,1.84921579899999));
#342126=CARTESIAN_POINT('Ctrl Pts',(3.97985098799994,12.2,1.84920168999998));
#342127=CARTESIAN_POINT('Ctrl Pts',(3.97985098799994,5.2,1.84920168999998));
#342128=CARTESIAN_POINT('Ctrl Pts',(3.97985098799994,2.2,1.84920168999998));
#342129=CARTESIAN_POINT('Ctrl Pts',(3.97783774399994,12.2,1.84918537999998));
#342130=CARTESIAN_POINT('Ctrl Pts',(3.97783774399994,5.2,1.84918537999998));
#342131=CARTESIAN_POINT('Ctrl Pts',(3.97783774399994,2.2,1.84918537999998));
#342132=CARTESIAN_POINT('Ctrl Pts',(3.97582857899994,12.2,1.84916687499999));
#342133=CARTESIAN_POINT('Ctrl Pts',(3.97582857899994,5.2,1.84916687499999));
#342134=CARTESIAN_POINT('Ctrl Pts',(3.97582857899994,2.2,1.84916687499999));
#342135=CARTESIAN_POINT('Ctrl Pts',(3.97382350099994,12.2,1.84914618499999));
#342136=CARTESIAN_POINT('Ctrl Pts',(3.97382350099994,5.2,1.84914618499999));
#342137=CARTESIAN_POINT('Ctrl Pts',(3.97382350099994,2.2,1.84914618499999));
#342138=CARTESIAN_POINT('Ctrl Pts',(3.97182251499994,12.2,1.84912331799998));
#342139=CARTESIAN_POINT('Ctrl Pts',(3.97182251499994,5.2,1.84912331799998));
#342140=CARTESIAN_POINT('Ctrl Pts',(3.97182251499994,2.2,1.84912331799998));
#342141=CARTESIAN_POINT('Ctrl Pts',(3.96982563199994,12.2,1.84909827999999));
#342142=CARTESIAN_POINT('Ctrl Pts',(3.96982563199994,5.2,1.84909827999999));
#342143=CARTESIAN_POINT('Ctrl Pts',(3.96982563199994,2.2,1.84909827999999));
#342144=CARTESIAN_POINT('Ctrl Pts',(3.96783285499994,12.2,1.84907108099999));
#342145=CARTESIAN_POINT('Ctrl Pts',(3.96783285499994,5.2,1.84907108099999));
#342146=CARTESIAN_POINT('Ctrl Pts',(3.96783285499994,2.2,1.84907108099999));
#342147=CARTESIAN_POINT('Ctrl Pts',(3.96584419399994,12.2,1.84904172999998));
#342148=CARTESIAN_POINT('Ctrl Pts',(3.96584419399994,5.2,1.84904172999998));
#342149=CARTESIAN_POINT('Ctrl Pts',(3.96584419399994,2.2,1.84904172999998));
#342150=CARTESIAN_POINT('Ctrl Pts',(3.96385965499995,12.2,1.84901023299998));
#342151=CARTESIAN_POINT('Ctrl Pts',(3.96385965499995,5.2,1.84901023299998));
#342152=CARTESIAN_POINT('Ctrl Pts',(3.96385965499995,2.2,1.84901023299998));
#342153=CARTESIAN_POINT('Ctrl Pts',(3.96187924499994,12.2,1.84897660099999));
#342154=CARTESIAN_POINT('Ctrl Pts',(3.96187924499994,5.2,1.84897660099999));
#342155=CARTESIAN_POINT('Ctrl Pts',(3.96187924499994,2.2,1.84897660099999));
#342156=CARTESIAN_POINT('Ctrl Pts',(3.95990297199994,12.2,1.84894083999998));
#342157=CARTESIAN_POINT('Ctrl Pts',(3.95990297199994,5.2,1.84894083999998));
#342158=CARTESIAN_POINT('Ctrl Pts',(3.95990297199994,2.2,1.84894083999998));
#342159=CARTESIAN_POINT('Ctrl Pts',(3.95793084199994,12.2,1.84890295799998));
#342160=CARTESIAN_POINT('Ctrl Pts',(3.95793084199994,5.2,1.84890295799998));
#342161=CARTESIAN_POINT('Ctrl Pts',(3.95793084199994,2.2,1.84890295799998));
#342162=CARTESIAN_POINT('Ctrl Pts',(3.95596286399994,12.2,1.84886296599998));
#342163=CARTESIAN_POINT('Ctrl Pts',(3.95596286399994,5.2,1.84886296599998));
#342164=CARTESIAN_POINT('Ctrl Pts',(3.95596286399994,2.2,1.84886296599998));
#342165=CARTESIAN_POINT('Ctrl Pts',(3.95399904299994,12.2,1.84882086999998));
#342166=CARTESIAN_POINT('Ctrl Pts',(3.95399904299994,5.2,1.84882086999998));
#342167=CARTESIAN_POINT('Ctrl Pts',(3.95399904299994,2.2,1.84882086999998));
#342168=CARTESIAN_POINT('Ctrl Pts',(3.95203938799995,12.2,1.84877667999999));
#342169=CARTESIAN_POINT('Ctrl Pts',(3.95203938799995,5.2,1.84877667999999));
#342170=CARTESIAN_POINT('Ctrl Pts',(3.95203938799995,2.2,1.84877667999999));
#342171=CARTESIAN_POINT('Ctrl Pts',(3.95008390499994,12.2,1.84873040199999));
#342172=CARTESIAN_POINT('Ctrl Pts',(3.95008390499994,5.2,1.84873040199999));
#342173=CARTESIAN_POINT('Ctrl Pts',(3.95008390499994,2.2,1.84873040199999));
#342174=CARTESIAN_POINT('Ctrl Pts',(3.94813260099994,12.2,1.84868204799999));
#342175=CARTESIAN_POINT('Ctrl Pts',(3.94813260099994,5.2,1.84868204799999));
#342176=CARTESIAN_POINT('Ctrl Pts',(3.94813260099994,2.2,1.84868204799999));
#342177=CARTESIAN_POINT('Ctrl Pts',(3.94618548399994,12.2,1.84863162399999));
#342178=CARTESIAN_POINT('Ctrl Pts',(3.94618548399994,5.2,1.84863162399999));
#342179=CARTESIAN_POINT('Ctrl Pts',(3.94618548399994,2.2,1.84863162399999));
#342180=CARTESIAN_POINT('Ctrl Pts',(3.94424256099994,12.2,1.84857913799998));
#342181=CARTESIAN_POINT('Ctrl Pts',(3.94424256099994,5.2,1.84857913799998));
#342182=CARTESIAN_POINT('Ctrl Pts',(3.94424256099994,2.2,1.84857913799998));
#342183=CARTESIAN_POINT('Ctrl Pts',(3.94230383899994,12.2,1.84852459999998));
#342184=CARTESIAN_POINT('Ctrl Pts',(3.94230383899994,5.2,1.84852459999998));
#342185=CARTESIAN_POINT('Ctrl Pts',(3.94230383899994,2.2,1.84852459999998));
#342186=CARTESIAN_POINT('Ctrl Pts',(3.94036932599994,12.2,1.84846801799999));
#342187=CARTESIAN_POINT('Ctrl Pts',(3.94036932599994,5.2,1.84846801799999));
#342188=CARTESIAN_POINT('Ctrl Pts',(3.94036932599994,2.2,1.84846801799999));
#342189=CARTESIAN_POINT('Ctrl Pts',(3.93843902799994,12.2,1.84840940099999));
#342190=CARTESIAN_POINT('Ctrl Pts',(3.93843902799994,5.2,1.84840940099999));
#342191=CARTESIAN_POINT('Ctrl Pts',(3.93843902799994,2.2,1.84840940099999));
#342192=CARTESIAN_POINT('Ctrl Pts',(3.93651295199994,12.2,1.84834875699998));
#342193=CARTESIAN_POINT('Ctrl Pts',(3.93651295199994,5.2,1.84834875699998));
#342194=CARTESIAN_POINT('Ctrl Pts',(3.93651295199994,2.2,1.84834875699998));
#342195=CARTESIAN_POINT('Ctrl Pts',(3.93459110599994,12.2,1.84828609399998));
#342196=CARTESIAN_POINT('Ctrl Pts',(3.93459110599994,5.2,1.84828609399998));
#342197=CARTESIAN_POINT('Ctrl Pts',(3.93459110599994,2.2,1.84828609399998));
#342198=CARTESIAN_POINT('Ctrl Pts',(3.93267349599994,12.2,1.84822142199998));
#342199=CARTESIAN_POINT('Ctrl Pts',(3.93267349599994,5.2,1.84822142199998));
#342200=CARTESIAN_POINT('Ctrl Pts',(3.93267349599994,2.2,1.84822142199998));
#342201=CARTESIAN_POINT('Ctrl Pts',(3.93076013199994,12.2,1.84815474899999));
#342202=CARTESIAN_POINT('Ctrl Pts',(3.93076013199994,5.2,1.84815474899999));
#342203=CARTESIAN_POINT('Ctrl Pts',(3.93076013199994,2.2,1.84815474899999));
#342204=CARTESIAN_POINT('Ctrl Pts',(3.92885101799994,12.2,1.84808608399999));
#342205=CARTESIAN_POINT('Ctrl Pts',(3.92885101799994,5.2,1.84808608399999));
#342206=CARTESIAN_POINT('Ctrl Pts',(3.92885101799994,2.2,1.84808608399999));
#342207=CARTESIAN_POINT('Ctrl Pts',(3.92694616199994,12.2,1.84801543499999));
#342208=CARTESIAN_POINT('Ctrl Pts',(3.92694616199994,5.2,1.84801543499999));
#342209=CARTESIAN_POINT('Ctrl Pts',(3.92694616199994,2.2,1.84801543499999));
#342210=CARTESIAN_POINT('Ctrl Pts',(3.92504557199994,12.2,1.84794281199999));
#342211=CARTESIAN_POINT('Ctrl Pts',(3.92504557199994,5.2,1.84794281199999));
#342212=CARTESIAN_POINT('Ctrl Pts',(3.92504557199994,2.2,1.84794281199999));
#342213=CARTESIAN_POINT('Ctrl Pts',(3.92314925599994,12.2,1.84786822199999));
#342214=CARTESIAN_POINT('Ctrl Pts',(3.92314925599994,5.2,1.84786822199999));
#342215=CARTESIAN_POINT('Ctrl Pts',(3.92314925599994,2.2,1.84786822199999));
#342216=CARTESIAN_POINT('Ctrl Pts',(3.92125721899994,12.2,1.84779167499999));
#342217=CARTESIAN_POINT('Ctrl Pts',(3.92125721899994,5.2,1.84779167499999));
#342218=CARTESIAN_POINT('Ctrl Pts',(3.92125721899994,2.2,1.84779167499999));
#342219=CARTESIAN_POINT('Ctrl Pts',(3.91936946799994,12.2,1.84771317899999));
#342220=CARTESIAN_POINT('Ctrl Pts',(3.91936946799994,5.2,1.84771317899999));
#342221=CARTESIAN_POINT('Ctrl Pts',(3.91936946799994,2.2,1.84771317899999));
#342222=CARTESIAN_POINT('Ctrl Pts',(3.91748601299994,12.2,1.84763274399999));
#342223=CARTESIAN_POINT('Ctrl Pts',(3.91748601299994,5.2,1.84763274399999));
#342224=CARTESIAN_POINT('Ctrl Pts',(3.91748601299994,2.2,1.84763274399999));
#342225=CARTESIAN_POINT('Ctrl Pts',(3.91560685799994,12.2,1.84755037699999));
#342226=CARTESIAN_POINT('Ctrl Pts',(3.91560685799994,5.2,1.84755037699999));
#342227=CARTESIAN_POINT('Ctrl Pts',(3.91560685799994,2.2,1.84755037699999));
#342228=CARTESIAN_POINT('Ctrl Pts',(3.91373201199994,12.2,1.84746608899998));
#342229=CARTESIAN_POINT('Ctrl Pts',(3.91373201199994,5.2,1.84746608899998));
#342230=CARTESIAN_POINT('Ctrl Pts',(3.91373201199994,2.2,1.84746608899998));
#342231=CARTESIAN_POINT('Ctrl Pts',(3.91186148299994,12.2,1.84737988799998));
#342232=CARTESIAN_POINT('Ctrl Pts',(3.91186148299994,5.2,1.84737988799998));
#342233=CARTESIAN_POINT('Ctrl Pts',(3.91186148299994,2.2,1.84737988799998));
#342234=CARTESIAN_POINT('Ctrl Pts',(3.90999527499994,12.2,1.84729178299999));
#342235=CARTESIAN_POINT('Ctrl Pts',(3.90999527499994,5.2,1.84729178299999));
#342236=CARTESIAN_POINT('Ctrl Pts',(3.90999527499994,2.2,1.84729178299999));
#342237=CARTESIAN_POINT('Ctrl Pts',(3.90813339899994,12.2,1.84720178199999));
#342238=CARTESIAN_POINT('Ctrl Pts',(3.90813339899994,5.2,1.84720178199999));
#342239=CARTESIAN_POINT('Ctrl Pts',(3.90813339899994,2.2,1.84720178199999));
#342240=CARTESIAN_POINT('Ctrl Pts',(3.90627585999994,12.2,1.84710989499999));
#342241=CARTESIAN_POINT('Ctrl Pts',(3.90627585999994,5.2,1.84710989499999));
#342242=CARTESIAN_POINT('Ctrl Pts',(3.90627585999994,2.2,1.84710989499999));
#342243=CARTESIAN_POINT('Ctrl Pts',(3.90442266399994,12.2,1.84701613099998));
#342244=CARTESIAN_POINT('Ctrl Pts',(3.90442266399994,5.2,1.84701613099998));
#342245=CARTESIAN_POINT('Ctrl Pts',(3.90442266399994,2.2,1.84701613099998));
#342246=CARTESIAN_POINT('Ctrl Pts',(3.90257382099994,12.2,1.84692049799999));
#342247=CARTESIAN_POINT('Ctrl Pts',(3.90257382099994,5.2,1.84692049799999));
#342248=CARTESIAN_POINT('Ctrl Pts',(3.90257382099994,2.2,1.84692049799999));
#342249=CARTESIAN_POINT('Ctrl Pts',(3.90072933599994,12.2,1.84682300599999));
#342250=CARTESIAN_POINT('Ctrl Pts',(3.90072933599994,5.2,1.84682300599999));
#342251=CARTESIAN_POINT('Ctrl Pts',(3.90072933599994,2.2,1.84682300599999));
#342252=CARTESIAN_POINT('Ctrl Pts',(3.89888921699994,12.2,1.84672366499999));
#342253=CARTESIAN_POINT('Ctrl Pts',(3.89888921699994,5.2,1.84672366499999));
#342254=CARTESIAN_POINT('Ctrl Pts',(3.89888921699994,2.2,1.84672366499999));
#342255=CARTESIAN_POINT('Ctrl Pts',(3.89705347199994,12.2,1.84662248199999));
#342256=CARTESIAN_POINT('Ctrl Pts',(3.89705347199994,5.2,1.84662248199999));
#342257=CARTESIAN_POINT('Ctrl Pts',(3.89705347199994,2.2,1.84662248199999));
#342258=CARTESIAN_POINT('Ctrl Pts',(3.89522210699994,12.2,1.84651946599999));
#342259=CARTESIAN_POINT('Ctrl Pts',(3.89522210699994,5.2,1.84651946599999));
#342260=CARTESIAN_POINT('Ctrl Pts',(3.89522210699994,2.2,1.84651946599999));
#342261=CARTESIAN_POINT('Ctrl Pts',(3.89339512899994,12.2,1.84641462899998));
#342262=CARTESIAN_POINT('Ctrl Pts',(3.89339512899994,5.2,1.84641462899998));
#342263=CARTESIAN_POINT('Ctrl Pts',(3.89339512899994,2.2,1.84641462899998));
#342264=CARTESIAN_POINT('Ctrl Pts',(3.89157254599994,12.2,1.84630797799999));
#342265=CARTESIAN_POINT('Ctrl Pts',(3.89157254599994,5.2,1.84630797799999));
#342266=CARTESIAN_POINT('Ctrl Pts',(3.89157254599994,2.2,1.84630797799999));
#342267=CARTESIAN_POINT('Ctrl Pts',(3.88975436499994,12.2,1.84619952299999));
#342268=CARTESIAN_POINT('Ctrl Pts',(3.88975436499994,5.2,1.84619952299999));
#342269=CARTESIAN_POINT('Ctrl Pts',(3.88975436499994,2.2,1.84619952299999));
#342270=CARTESIAN_POINT('Ctrl Pts',(3.88794059199994,12.2,1.84608927199998));
#342271=CARTESIAN_POINT('Ctrl Pts',(3.88794059199994,5.2,1.84608927199998));
#342272=CARTESIAN_POINT('Ctrl Pts',(3.88794059199994,2.2,1.84608927199998));
#342273=CARTESIAN_POINT('Ctrl Pts',(3.88613123699994,12.2,1.84597723499999));
#342274=CARTESIAN_POINT('Ctrl Pts',(3.88613123699994,5.2,1.84597723499999));
#342275=CARTESIAN_POINT('Ctrl Pts',(3.88613123699994,2.2,1.84597723499999));
#342276=CARTESIAN_POINT('Ctrl Pts',(3.88432630399994,12.2,1.84586342199998));
#342277=CARTESIAN_POINT('Ctrl Pts',(3.88432630399994,5.2,1.84586342199998));
#342278=CARTESIAN_POINT('Ctrl Pts',(3.88432630399994,2.2,1.84586342199998));
#342279=CARTESIAN_POINT('Ctrl Pts',(3.88252580199994,12.2,1.84574784099999));
#342280=CARTESIAN_POINT('Ctrl Pts',(3.88252580199994,5.2,1.84574784099999));
#342281=CARTESIAN_POINT('Ctrl Pts',(3.88252580199994,2.2,1.84574784099999));
#342282=CARTESIAN_POINT('Ctrl Pts',(3.88072973799995,12.2,1.84563050199999));
#342283=CARTESIAN_POINT('Ctrl Pts',(3.88072973799995,5.2,1.84563050199999));
#342284=CARTESIAN_POINT('Ctrl Pts',(3.88072973799995,2.2,1.84563050199999));
#342285=CARTESIAN_POINT('Ctrl Pts',(3.87893811799994,12.2,1.84551141499998));
#342286=CARTESIAN_POINT('Ctrl Pts',(3.87893811799994,5.2,1.84551141499998));
#342287=CARTESIAN_POINT('Ctrl Pts',(3.87893811799994,2.2,1.84551141499998));
#342288=CARTESIAN_POINT('Ctrl Pts',(3.87715095099994,12.2,1.84539058799999));
#342289=CARTESIAN_POINT('Ctrl Pts',(3.87715095099994,5.2,1.84539058799999));
#342290=CARTESIAN_POINT('Ctrl Pts',(3.87715095099994,2.2,1.84539058799999));
#342291=CARTESIAN_POINT('Ctrl Pts',(3.87536824199994,12.2,1.84526803199998));
#342292=CARTESIAN_POINT('Ctrl Pts',(3.87536824199994,5.2,1.84526803199998));
#342293=CARTESIAN_POINT('Ctrl Pts',(3.87536824199994,2.2,1.84526803199998));
#342294=CARTESIAN_POINT('Ctrl Pts',(3.87359000099994,12.2,1.84514375499999));
#342295=CARTESIAN_POINT('Ctrl Pts',(3.87359000099994,5.2,1.84514375499999));
#342296=CARTESIAN_POINT('Ctrl Pts',(3.87359000099994,2.2,1.84514375499999));
#342297=CARTESIAN_POINT('Ctrl Pts',(3.87181623199994,12.2,1.84501776699999));
#342298=CARTESIAN_POINT('Ctrl Pts',(3.87181623199994,5.2,1.84501776699999));
#342299=CARTESIAN_POINT('Ctrl Pts',(3.87181623199994,2.2,1.84501776699999));
#342300=CARTESIAN_POINT('Ctrl Pts',(3.87004694499994,12.2,1.84489007799999));
#342301=CARTESIAN_POINT('Ctrl Pts',(3.87004694499994,5.2,1.84489007799999));
#342302=CARTESIAN_POINT('Ctrl Pts',(3.87004694499994,2.2,1.84489007799999));
#342303=CARTESIAN_POINT('Ctrl Pts',(3.86828214499995,12.2,1.84476069599999));
#342304=CARTESIAN_POINT('Ctrl Pts',(3.86828214499995,5.2,1.84476069599999));
#342305=CARTESIAN_POINT('Ctrl Pts',(3.86828214499995,2.2,1.84476069599999));
#342306=CARTESIAN_POINT('Ctrl Pts',(3.86652183999994,12.2,1.84462963199998));
#342307=CARTESIAN_POINT('Ctrl Pts',(3.86652183999994,5.2,1.84462963199998));
#342308=CARTESIAN_POINT('Ctrl Pts',(3.86652183999994,2.2,1.84462963199998));
#342309=CARTESIAN_POINT('Ctrl Pts',(3.86476603699994,12.2,1.84449689599999));
#342310=CARTESIAN_POINT('Ctrl Pts',(3.86476603699994,5.2,1.84449689599999));
#342311=CARTESIAN_POINT('Ctrl Pts',(3.86476603699994,2.2,1.84449689599999));
#342312=CARTESIAN_POINT('Ctrl Pts',(3.86301474399994,12.2,1.84436249499999));
#342313=CARTESIAN_POINT('Ctrl Pts',(3.86301474399994,5.2,1.84436249499999));
#342314=CARTESIAN_POINT('Ctrl Pts',(3.86301474399994,2.2,1.84436249499999));
#342315=CARTESIAN_POINT('Ctrl Pts',(3.86126796699994,12.2,1.84422644199998));
#342316=CARTESIAN_POINT('Ctrl Pts',(3.86126796699994,5.2,1.84422644199998));
#342317=CARTESIAN_POINT('Ctrl Pts',(3.86126796699994,2.2,1.84422644199998));
#342318=CARTESIAN_POINT('Ctrl Pts',(3.85952571499994,12.2,1.84408874499999));
#342319=CARTESIAN_POINT('Ctrl Pts',(3.85952571499994,5.2,1.84408874499999));
#342320=CARTESIAN_POINT('Ctrl Pts',(3.85952571499994,2.2,1.84408874499999));
#342321=CARTESIAN_POINT('Ctrl Pts',(3.85778799299994,12.2,1.84394941199999));
#342322=CARTESIAN_POINT('Ctrl Pts',(3.85778799299994,5.2,1.84394941199999));
#342323=CARTESIAN_POINT('Ctrl Pts',(3.85778799299994,2.2,1.84394941199999));
#342324=CARTESIAN_POINT('Ctrl Pts',(3.85605480899994,12.2,1.84380845599998));
#342325=CARTESIAN_POINT('Ctrl Pts',(3.85605480899994,5.2,1.84380845599998));
#342326=CARTESIAN_POINT('Ctrl Pts',(3.85605480899994,2.2,1.84380845599998));
#342327=CARTESIAN_POINT('Ctrl Pts',(3.85432616999994,12.2,1.84366588399998));
#342328=CARTESIAN_POINT('Ctrl Pts',(3.85432616999994,5.2,1.84366588399998));
#342329=CARTESIAN_POINT('Ctrl Pts',(3.85432616999994,2.2,1.84366588399998));
#342330=CARTESIAN_POINT('Ctrl Pts',(3.85260208399994,12.2,1.84352170699999));
#342331=CARTESIAN_POINT('Ctrl Pts',(3.85260208399994,5.2,1.84352170699999));
#342332=CARTESIAN_POINT('Ctrl Pts',(3.85260208399994,2.2,1.84352170699999));
#342333=CARTESIAN_POINT('Ctrl Pts',(3.85088255699995,12.2,1.84337593499999));
#342334=CARTESIAN_POINT('Ctrl Pts',(3.85088255699995,5.2,1.84337593499999));
#342335=CARTESIAN_POINT('Ctrl Pts',(3.85088255699995,2.2,1.84337593499999));
#342336=CARTESIAN_POINT('Ctrl Pts',(3.84916759799994,12.2,1.84322857799998));
#342337=CARTESIAN_POINT('Ctrl Pts',(3.84916759799994,5.2,1.84322857799998));
#342338=CARTESIAN_POINT('Ctrl Pts',(3.84916759799994,2.2,1.84322857799998));
#342339=CARTESIAN_POINT('Ctrl Pts',(3.84745721099994,12.2,1.84307964399999));
#342340=CARTESIAN_POINT('Ctrl Pts',(3.84745721099994,5.2,1.84307964399999));
#342341=CARTESIAN_POINT('Ctrl Pts',(3.84745721099994,2.2,1.84307964399999));
#342342=CARTESIAN_POINT('Ctrl Pts',(3.84575140599994,12.2,1.84292914499999));
#342343=CARTESIAN_POINT('Ctrl Pts',(3.84575140599994,5.2,1.84292914499999));
#342344=CARTESIAN_POINT('Ctrl Pts',(3.84575140599994,2.2,1.84292914499999));
#342345=CARTESIAN_POINT('Ctrl Pts',(3.84405018899994,12.2,1.84277708999999));
#342346=CARTESIAN_POINT('Ctrl Pts',(3.84405018899994,5.2,1.84277708999999));
#342347=CARTESIAN_POINT('Ctrl Pts',(3.84405018899994,2.2,1.84277708999999));
#342348=CARTESIAN_POINT('Ctrl Pts',(3.84235356799994,12.2,1.84262348899999));
#342349=CARTESIAN_POINT('Ctrl Pts',(3.84235356799994,5.2,1.84262348899999));
#342350=CARTESIAN_POINT('Ctrl Pts',(3.84235356799994,2.2,1.84262348899999));
#342351=CARTESIAN_POINT('Ctrl Pts',(3.84066154899994,12.2,1.84246835099998));
#342352=CARTESIAN_POINT('Ctrl Pts',(3.84066154899994,5.2,1.84246835099998));
#342353=CARTESIAN_POINT('Ctrl Pts',(3.84066154899994,2.2,1.84246835099998));
#342354=CARTESIAN_POINT('Ctrl Pts',(3.83897413999994,12.2,1.84231168799998));
#342355=CARTESIAN_POINT('Ctrl Pts',(3.83897413999994,5.2,1.84231168799998));
#342356=CARTESIAN_POINT('Ctrl Pts',(3.83897413999994,2.2,1.84231168799998));
#342357=CARTESIAN_POINT('Ctrl Pts',(3.83729134699994,12.2,1.84215350799999));
#342358=CARTESIAN_POINT('Ctrl Pts',(3.83729134699994,5.2,1.84215350799999));
#342359=CARTESIAN_POINT('Ctrl Pts',(3.83729134699994,2.2,1.84215350799999));
#342360=CARTESIAN_POINT('Ctrl Pts',(3.83561317899995,12.2,1.84199382299999));
#342361=CARTESIAN_POINT('Ctrl Pts',(3.83561317899995,5.2,1.84199382299999));
#342362=CARTESIAN_POINT('Ctrl Pts',(3.83561317899995,2.2,1.84199382299999));
#342363=CARTESIAN_POINT('Ctrl Pts',(3.83393964199994,12.2,1.84183264099998));
#342364=CARTESIAN_POINT('Ctrl Pts',(3.83393964199994,5.2,1.84183264099998));
#342365=CARTESIAN_POINT('Ctrl Pts',(3.83393964199994,2.2,1.84183264099998));
#342366=CARTESIAN_POINT('Ctrl Pts',(3.83227074399994,12.2,1.84166997299998));
#342367=CARTESIAN_POINT('Ctrl Pts',(3.83227074399994,5.2,1.84166997299998));
#342368=CARTESIAN_POINT('Ctrl Pts',(3.83227074399994,2.2,1.84166997299998));
#342369=CARTESIAN_POINT('Ctrl Pts',(3.83060648999995,12.2,1.84150582999999));
#342370=CARTESIAN_POINT('Ctrl Pts',(3.83060648999995,5.2,1.84150582999999));
#342371=CARTESIAN_POINT('Ctrl Pts',(3.83060648999995,2.2,1.84150582999999));
#342372=CARTESIAN_POINT('Ctrl Pts',(3.82894688999994,12.2,1.84134021999999));
#342373=CARTESIAN_POINT('Ctrl Pts',(3.82894688999994,5.2,1.84134021999999));
#342374=CARTESIAN_POINT('Ctrl Pts',(3.82894688999994,2.2,1.84134021999999));
#342375=CARTESIAN_POINT('Ctrl Pts',(3.82729194999994,12.2,1.84117315599998));
#342376=CARTESIAN_POINT('Ctrl Pts',(3.82729194999994,5.2,1.84117315599998));
#342377=CARTESIAN_POINT('Ctrl Pts',(3.82729194999994,2.2,1.84117315599998));
#342378=CARTESIAN_POINT('Ctrl Pts',(3.82564167599994,12.2,1.84100464599998));
#342379=CARTESIAN_POINT('Ctrl Pts',(3.82564167599994,5.2,1.84100464599998));
#342380=CARTESIAN_POINT('Ctrl Pts',(3.82564167599994,2.2,1.84100464599998));
#342381=CARTESIAN_POINT('Ctrl Pts',(3.82399607699994,12.2,1.84083470099999));
#342382=CARTESIAN_POINT('Ctrl Pts',(3.82399607699994,5.2,1.84083470099999));
#342383=CARTESIAN_POINT('Ctrl Pts',(3.82399607699994,2.2,1.84083470099999));
#342384=CARTESIAN_POINT('Ctrl Pts',(3.82235515999994,12.2,1.84066333199999));
#342385=CARTESIAN_POINT('Ctrl Pts',(3.82235515999994,5.2,1.84066333199999));
#342386=CARTESIAN_POINT('Ctrl Pts',(3.82235515999994,2.2,1.84066333199999));
#342387=CARTESIAN_POINT('Ctrl Pts',(3.82071892999994,12.2,1.84049054699999));
#342388=CARTESIAN_POINT('Ctrl Pts',(3.82071892999994,5.2,1.84049054699999));
#342389=CARTESIAN_POINT('Ctrl Pts',(3.82071892999994,2.2,1.84049054699999));
#342390=CARTESIAN_POINT('Ctrl Pts',(3.81908739599994,12.2,1.84031635899998));
#342391=CARTESIAN_POINT('Ctrl Pts',(3.81908739599994,5.2,1.84031635899998));
#342392=CARTESIAN_POINT('Ctrl Pts',(3.81908739599994,2.2,1.84031635899998));
#342393=CARTESIAN_POINT('Ctrl Pts',(3.81746056499995,12.2,1.84014077599999));
#342394=CARTESIAN_POINT('Ctrl Pts',(3.81746056499995,5.2,1.84014077599999));
#342395=CARTESIAN_POINT('Ctrl Pts',(3.81746056499995,2.2,1.84014077599999));
#342396=CARTESIAN_POINT('Ctrl Pts',(3.81583844399994,12.2,1.83996380999998));
#342397=CARTESIAN_POINT('Ctrl Pts',(3.81583844399994,5.2,1.83996380999998));
#342398=CARTESIAN_POINT('Ctrl Pts',(3.81583844399994,2.2,1.83996380999998));
#342399=CARTESIAN_POINT('Ctrl Pts',(3.81422104099994,12.2,1.83978547199999));
#342400=CARTESIAN_POINT('Ctrl Pts',(3.81422104099994,5.2,1.83978547199999));
#342401=CARTESIAN_POINT('Ctrl Pts',(3.81422104099994,2.2,1.83978547199999));
#342402=CARTESIAN_POINT('Ctrl Pts',(3.81260836099994,12.2,1.83960576999999));
#342403=CARTESIAN_POINT('Ctrl Pts',(3.81260836099994,5.2,1.83960576999999));
#342404=CARTESIAN_POINT('Ctrl Pts',(3.81260836099994,2.2,1.83960576999999));
#342405=CARTESIAN_POINT('Ctrl Pts',(3.81100041299994,12.2,1.83942471699998));
#342406=CARTESIAN_POINT('Ctrl Pts',(3.81100041299994,5.2,1.83942471699998));
#342407=CARTESIAN_POINT('Ctrl Pts',(3.81100041299994,2.2,1.83942471699998));
#342408=CARTESIAN_POINT('Ctrl Pts',(3.80939720399994,12.2,1.83924232099999));
#342409=CARTESIAN_POINT('Ctrl Pts',(3.80939720399994,5.2,1.83924232099999));
#342410=CARTESIAN_POINT('Ctrl Pts',(3.80939720399994,2.2,1.83924232099999));
#342411=CARTESIAN_POINT('Ctrl Pts',(3.80779873999994,12.2,1.83905859499998));
#342412=CARTESIAN_POINT('Ctrl Pts',(3.80779873999994,5.2,1.83905859499998));
#342413=CARTESIAN_POINT('Ctrl Pts',(3.80779873999994,2.2,1.83905859499998));
#342414=CARTESIAN_POINT('Ctrl Pts',(3.80620502999994,12.2,1.83887354799999));
#342415=CARTESIAN_POINT('Ctrl Pts',(3.80620502999994,5.2,1.83887354799999));
#342416=CARTESIAN_POINT('Ctrl Pts',(3.80620502999994,2.2,1.83887354799999));
#342417=CARTESIAN_POINT('Ctrl Pts',(3.80461607899994,12.2,1.83868719099999));
#342418=CARTESIAN_POINT('Ctrl Pts',(3.80461607899994,5.2,1.83868719099999));
#342419=CARTESIAN_POINT('Ctrl Pts',(3.80461607899994,2.2,1.83868719099999));
#342420=CARTESIAN_POINT('Ctrl Pts',(3.80303189599994,12.2,1.83849953499998));
#342421=CARTESIAN_POINT('Ctrl Pts',(3.80303189599994,5.2,1.83849953499998));
#342422=CARTESIAN_POINT('Ctrl Pts',(3.80303189599994,2.2,1.83849953499998));
#342423=CARTESIAN_POINT('Ctrl Pts',(3.80145248699994,12.2,1.83831058999999));
#342424=CARTESIAN_POINT('Ctrl Pts',(3.80145248699994,5.2,1.83831058999999));
#342425=CARTESIAN_POINT('Ctrl Pts',(3.80145248699994,2.2,1.83831058999999));
#342426=CARTESIAN_POINT('Ctrl Pts',(3.79987785999994,12.2,1.83812036699999));
#342427=CARTESIAN_POINT('Ctrl Pts',(3.79987785999994,5.2,1.83812036699999));
#342428=CARTESIAN_POINT('Ctrl Pts',(3.79987785999994,2.2,1.83812036699999));
#342429=CARTESIAN_POINT('Ctrl Pts',(3.79830802199994,12.2,1.83792887599999));
#342430=CARTESIAN_POINT('Ctrl Pts',(3.79830802199994,5.2,1.83792887599999));
#342431=CARTESIAN_POINT('Ctrl Pts',(3.79830802199994,2.2,1.83792887599999));
#342432=CARTESIAN_POINT('Ctrl Pts',(3.79674297899994,12.2,1.83773612999999));
#342433=CARTESIAN_POINT('Ctrl Pts',(3.79674297899994,5.2,1.83773612999999));
#342434=CARTESIAN_POINT('Ctrl Pts',(3.79674297899994,2.2,1.83773612999999));
#342435=CARTESIAN_POINT('Ctrl Pts',(3.79518273999994,12.2,1.83754213599999));
#342436=CARTESIAN_POINT('Ctrl Pts',(3.79518273999994,5.2,1.83754213599999));
#342437=CARTESIAN_POINT('Ctrl Pts',(3.79518273999994,2.2,1.83754213599999));
#342438=CARTESIAN_POINT('Ctrl Pts',(3.79362730999994,12.2,1.83734690799998));
#342439=CARTESIAN_POINT('Ctrl Pts',(3.79362730999994,5.2,1.83734690799998));
#342440=CARTESIAN_POINT('Ctrl Pts',(3.79362730999994,2.2,1.83734690799998));
#342441=CARTESIAN_POINT('Ctrl Pts',(3.79207669799994,12.2,1.83715045699998));
#342442=CARTESIAN_POINT('Ctrl Pts',(3.79207669799994,5.2,1.83715045699998));
#342443=CARTESIAN_POINT('Ctrl Pts',(3.79207669799994,2.2,1.83715045699998));
#342444=CARTESIAN_POINT('Ctrl Pts',(3.79053090999994,12.2,1.83695279099998));
#342445=CARTESIAN_POINT('Ctrl Pts',(3.79053090999994,5.2,1.83695279099998));
#342446=CARTESIAN_POINT('Ctrl Pts',(3.79053090999994,2.2,1.83695279099998));
#342447=CARTESIAN_POINT('Ctrl Pts',(3.78898995399994,12.2,1.83675392399998));
#342448=CARTESIAN_POINT('Ctrl Pts',(3.78898995399994,5.2,1.83675392399998));
#342449=CARTESIAN_POINT('Ctrl Pts',(3.78898995399994,2.2,1.83675392399998));
#342450=CARTESIAN_POINT('Ctrl Pts',(3.78745383699994,12.2,1.83655386399999));
#342451=CARTESIAN_POINT('Ctrl Pts',(3.78745383699994,5.2,1.83655386399999));
#342452=CARTESIAN_POINT('Ctrl Pts',(3.78745383699994,2.2,1.83655386399999));
#342453=CARTESIAN_POINT('Ctrl Pts',(3.78592256599994,12.2,1.83635262399998));
#342454=CARTESIAN_POINT('Ctrl Pts',(3.78592256599994,5.2,1.83635262399998));
#342455=CARTESIAN_POINT('Ctrl Pts',(3.78592256599994,2.2,1.83635262399998));
#342456=CARTESIAN_POINT('Ctrl Pts',(3.78439614799994,12.2,1.83615021499998));
#342457=CARTESIAN_POINT('Ctrl Pts',(3.78439614799994,5.2,1.83615021499998));
#342458=CARTESIAN_POINT('Ctrl Pts',(3.78439614799994,2.2,1.83615021499998));
#342459=CARTESIAN_POINT('Ctrl Pts',(3.78287458899994,12.2,1.83594664599998));
#342460=CARTESIAN_POINT('Ctrl Pts',(3.78287458899994,5.2,1.83594664599998));
#342461=CARTESIAN_POINT('Ctrl Pts',(3.78287458899994,2.2,1.83594664599998));
#342462=CARTESIAN_POINT('Ctrl Pts',(3.78135789899994,12.2,1.83574193099998));
#342463=CARTESIAN_POINT('Ctrl Pts',(3.78135789899994,5.2,1.83574193099998));
#342464=CARTESIAN_POINT('Ctrl Pts',(3.78135789899994,2.2,1.83574193099998));
#342465=CARTESIAN_POINT('Ctrl Pts',(3.77984608399994,12.2,1.83553607799999));
#342466=CARTESIAN_POINT('Ctrl Pts',(3.77984608399994,5.2,1.83553607799999));
#342467=CARTESIAN_POINT('Ctrl Pts',(3.77984608399994,2.2,1.83553607799999));
#342468=CARTESIAN_POINT('Ctrl Pts',(3.77833914899994,12.2,1.83532910099999));
#342469=CARTESIAN_POINT('Ctrl Pts',(3.77833914899994,5.2,1.83532910099999));
#342470=CARTESIAN_POINT('Ctrl Pts',(3.77833914899994,2.2,1.83532910099999));
#342471=CARTESIAN_POINT('Ctrl Pts',(3.77683710299995,12.2,1.83512100899998));
#342472=CARTESIAN_POINT('Ctrl Pts',(3.77683710299995,5.2,1.83512100899998));
#342473=CARTESIAN_POINT('Ctrl Pts',(3.77683710299995,2.2,1.83512100899998));
#342474=CARTESIAN_POINT('Ctrl Pts',(3.77533995399994,12.2,1.83491181399999));
#342475=CARTESIAN_POINT('Ctrl Pts',(3.77533995399994,5.2,1.83491181399999));
#342476=CARTESIAN_POINT('Ctrl Pts',(3.77533995399994,2.2,1.83491181399999));
#342477=CARTESIAN_POINT('Ctrl Pts',(3.77384770799994,12.2,1.83470152699998));
#342478=CARTESIAN_POINT('Ctrl Pts',(3.77384770799994,5.2,1.83470152699998));
#342479=CARTESIAN_POINT('Ctrl Pts',(3.77384770799994,2.2,1.83470152699998));
#342480=CARTESIAN_POINT('Ctrl Pts',(3.77236037099994,12.2,1.83449015999999));
#342481=CARTESIAN_POINT('Ctrl Pts',(3.77236037099994,5.2,1.83449015999999));
#342482=CARTESIAN_POINT('Ctrl Pts',(3.77236037099994,2.2,1.83449015999999));
#342483=CARTESIAN_POINT('Ctrl Pts',(3.77087795299994,12.2,1.83427772399999));
#342484=CARTESIAN_POINT('Ctrl Pts',(3.77087795299994,5.2,1.83427772399999));
#342485=CARTESIAN_POINT('Ctrl Pts',(3.77087795299994,2.2,1.83427772399999));
#342486=CARTESIAN_POINT('Ctrl Pts',(3.76940045799994,12.2,1.83406422899999));
#342487=CARTESIAN_POINT('Ctrl Pts',(3.76940045799994,5.2,1.83406422899999));
#342488=CARTESIAN_POINT('Ctrl Pts',(3.76940045799994,2.2,1.83406422899999));
#342489=CARTESIAN_POINT('Ctrl Pts',(3.76792789499994,12.2,1.83384968799999));
#342490=CARTESIAN_POINT('Ctrl Pts',(3.76792789499994,5.2,1.83384968799999));
#342491=CARTESIAN_POINT('Ctrl Pts',(3.76792789499994,2.2,1.83384968799999));
#342492=CARTESIAN_POINT('Ctrl Pts',(3.76646027099994,12.2,1.83363411099998));
#342493=CARTESIAN_POINT('Ctrl Pts',(3.76646027099994,5.2,1.83363411099998));
#342494=CARTESIAN_POINT('Ctrl Pts',(3.76646027099994,2.2,1.83363411099998));
#342495=CARTESIAN_POINT('Ctrl Pts',(3.76499759399994,12.2,1.83341750999999));
#342496=CARTESIAN_POINT('Ctrl Pts',(3.76499759399994,5.2,1.83341750999999));
#342497=CARTESIAN_POINT('Ctrl Pts',(3.76499759399994,2.2,1.83341750999999));
#342498=CARTESIAN_POINT('Ctrl Pts',(3.76353986899994,12.2,1.83319989699998));
#342499=CARTESIAN_POINT('Ctrl Pts',(3.76353986899994,5.2,1.83319989699998));
#342500=CARTESIAN_POINT('Ctrl Pts',(3.76353986899994,2.2,1.83319989699998));
#342501=CARTESIAN_POINT('Ctrl Pts',(3.76208710599994,12.2,1.83298128299999));
#342502=CARTESIAN_POINT('Ctrl Pts',(3.76208710599994,5.2,1.83298128299999));
#342503=CARTESIAN_POINT('Ctrl Pts',(3.76208710599994,2.2,1.83298128299999));
#342504=CARTESIAN_POINT('Ctrl Pts',(3.76063930899994,12.2,1.83276167899999));
#342505=CARTESIAN_POINT('Ctrl Pts',(3.76063930899994,5.2,1.83276167899999));
#342506=CARTESIAN_POINT('Ctrl Pts',(3.76063930899994,2.2,1.83276167899999));
#342507=CARTESIAN_POINT('Ctrl Pts',(3.75919648599994,12.2,1.83254109699998));
#342508=CARTESIAN_POINT('Ctrl Pts',(3.75919648599994,5.2,1.83254109699998));
#342509=CARTESIAN_POINT('Ctrl Pts',(3.75919648599994,2.2,1.83254109699998));
#342510=CARTESIAN_POINT('Ctrl Pts',(3.75775864499994,12.2,1.83231954999998));
#342511=CARTESIAN_POINT('Ctrl Pts',(3.75775864499994,5.2,1.83231954999998));
#342512=CARTESIAN_POINT('Ctrl Pts',(3.75775864499994,2.2,1.83231954999998));
#342513=CARTESIAN_POINT('Ctrl Pts',(3.75632579299995,12.2,1.83209704599999));
#342514=CARTESIAN_POINT('Ctrl Pts',(3.75632579299995,5.2,1.83209704599999));
#342515=CARTESIAN_POINT('Ctrl Pts',(3.75632579299995,2.2,1.83209704599999));
#342516=CARTESIAN_POINT('Ctrl Pts',(3.75489793799994,12.2,1.83187359999998));
#342517=CARTESIAN_POINT('Ctrl Pts',(3.75489793799994,5.2,1.83187359999998));
#342518=CARTESIAN_POINT('Ctrl Pts',(3.75489793799994,2.2,1.83187359999998));
#342519=CARTESIAN_POINT('Ctrl Pts',(3.75347508399994,12.2,1.83164922199999));
#342520=CARTESIAN_POINT('Ctrl Pts',(3.75347508399994,5.2,1.83164922199999));
#342521=CARTESIAN_POINT('Ctrl Pts',(3.75347508399994,2.2,1.83164922199999));
#342522=CARTESIAN_POINT('Ctrl Pts',(3.75205724199994,12.2,1.83142392399999));
#342523=CARTESIAN_POINT('Ctrl Pts',(3.75205724199994,5.2,1.83142392399999));
#342524=CARTESIAN_POINT('Ctrl Pts',(3.75205724199994,2.2,1.83142392399999));
#342525=CARTESIAN_POINT('Ctrl Pts',(3.75064441599994,12.2,1.83119771799999));
#342526=CARTESIAN_POINT('Ctrl Pts',(3.75064441599994,5.2,1.83119771799999));
#342527=CARTESIAN_POINT('Ctrl Pts',(3.75064441599994,2.2,1.83119771799999));
#342528=CARTESIAN_POINT('Ctrl Pts',(3.74923661499994,12.2,1.83097061599999));
#342529=CARTESIAN_POINT('Ctrl Pts',(3.74923661499994,5.2,1.83097061599999));
#342530=CARTESIAN_POINT('Ctrl Pts',(3.74923661499994,2.2,1.83097061599999));
#342531=CARTESIAN_POINT('Ctrl Pts',(3.74783384499994,12.2,1.83074262899999));
#342532=CARTESIAN_POINT('Ctrl Pts',(3.74783384499994,5.2,1.83074262899999));
#342533=CARTESIAN_POINT('Ctrl Pts',(3.74783384499994,2.2,1.83074262899999));
#342534=CARTESIAN_POINT('Ctrl Pts',(3.74643611499994,12.2,1.83051377099999));
#342535=CARTESIAN_POINT('Ctrl Pts',(3.74643611499994,5.2,1.83051377099999));
#342536=CARTESIAN_POINT('Ctrl Pts',(3.74643611499994,2.2,1.83051377099999));
#342537=CARTESIAN_POINT('Ctrl Pts',(3.74504342999994,12.2,1.83028404999999));
#342538=CARTESIAN_POINT('Ctrl Pts',(3.74504342999994,5.2,1.83028404999999));
#342539=CARTESIAN_POINT('Ctrl Pts',(3.74504342999994,2.2,1.83028404999999));
#342540=CARTESIAN_POINT('Ctrl Pts',(3.74365579899994,12.2,1.83005348099998));
#342541=CARTESIAN_POINT('Ctrl Pts',(3.74365579899994,5.2,1.83005348099998));
#342542=CARTESIAN_POINT('Ctrl Pts',(3.74365579899994,2.2,1.83005348099998));
#342543=CARTESIAN_POINT('Ctrl Pts',(3.74227322699995,12.2,1.82982207499998));
#342544=CARTESIAN_POINT('Ctrl Pts',(3.74227322699995,5.2,1.82982207499998));
#342545=CARTESIAN_POINT('Ctrl Pts',(3.74227322699995,2.2,1.82982207499998));
#342546=CARTESIAN_POINT('Ctrl Pts',(3.74089572299994,12.2,1.82958984299999));
#342547=CARTESIAN_POINT('Ctrl Pts',(3.74089572299994,5.2,1.82958984299999));
#342548=CARTESIAN_POINT('Ctrl Pts',(3.74089572299994,2.2,1.82958984299999));
#342549=CARTESIAN_POINT('Ctrl Pts',(3.73952329299994,12.2,1.82935679899999));
#342550=CARTESIAN_POINT('Ctrl Pts',(3.73952329299994,5.2,1.82935679899999));
#342551=CARTESIAN_POINT('Ctrl Pts',(3.73952329299994,2.2,1.82935679899999));
#342552=CARTESIAN_POINT('Ctrl Pts',(3.73815594499994,12.2,1.82912295299999));
#342553=CARTESIAN_POINT('Ctrl Pts',(3.73815594499994,5.2,1.82912295299999));
#342554=CARTESIAN_POINT('Ctrl Pts',(3.73815594499994,2.2,1.82912295299999));
#342555=CARTESIAN_POINT('Ctrl Pts',(3.73679368499995,12.2,1.82888831899998));
#342556=CARTESIAN_POINT('Ctrl Pts',(3.73679368499995,5.2,1.82888831899998));
#342557=CARTESIAN_POINT('Ctrl Pts',(3.73679368499995,2.2,1.82888831899998));
#342558=CARTESIAN_POINT('Ctrl Pts',(3.73543651999994,12.2,1.82865290799999));
#342559=CARTESIAN_POINT('Ctrl Pts',(3.73543651999994,5.2,1.82865290799999));
#342560=CARTESIAN_POINT('Ctrl Pts',(3.73543651999994,2.2,1.82865290799999));
#342561=CARTESIAN_POINT('Ctrl Pts',(3.73408445899994,12.2,1.82841673099999));
#342562=CARTESIAN_POINT('Ctrl Pts',(3.73408445899994,5.2,1.82841673099999));
#342563=CARTESIAN_POINT('Ctrl Pts',(3.73408445899994,2.2,1.82841673099999));
#342564=CARTESIAN_POINT('Ctrl Pts',(3.73273750799994,12.2,1.82817980399999));
#342565=CARTESIAN_POINT('Ctrl Pts',(3.73273750799994,5.2,1.82817980399999));
#342566=CARTESIAN_POINT('Ctrl Pts',(3.73273750799994,2.2,1.82817980399999));
#342567=CARTESIAN_POINT('Ctrl Pts',(3.73139567399994,12.2,1.82794213499998));
#342568=CARTESIAN_POINT('Ctrl Pts',(3.73139567399994,5.2,1.82794213499998));
#342569=CARTESIAN_POINT('Ctrl Pts',(3.73139567399994,2.2,1.82794213499998));
#342570=CARTESIAN_POINT('Ctrl Pts',(3.73005896399994,12.2,1.82770373799999));
#342571=CARTESIAN_POINT('Ctrl Pts',(3.73005896399994,5.2,1.82770373799999));
#342572=CARTESIAN_POINT('Ctrl Pts',(3.73005896399994,2.2,1.82770373799999));
#342573=CARTESIAN_POINT('Ctrl Pts',(3.72872738599995,12.2,1.82746462599999));
#342574=CARTESIAN_POINT('Ctrl Pts',(3.72872738599995,5.2,1.82746462599999));
#342575=CARTESIAN_POINT('Ctrl Pts',(3.72872738599995,2.2,1.82746462599999));
#342576=CARTESIAN_POINT('Ctrl Pts',(3.72740094599994,12.2,1.82722480999999));
#342577=CARTESIAN_POINT('Ctrl Pts',(3.72740094599994,5.2,1.82722480999999));
#342578=CARTESIAN_POINT('Ctrl Pts',(3.72740094599994,2.2,1.82722480999999));
#342579=CARTESIAN_POINT('Ctrl Pts',(3.72607965099994,12.2,1.82698430299999));
#342580=CARTESIAN_POINT('Ctrl Pts',(3.72607965099994,5.2,1.82698430299999));
#342581=CARTESIAN_POINT('Ctrl Pts',(3.72607965099994,2.2,1.82698430299999));
#342582=CARTESIAN_POINT('Ctrl Pts',(3.72476350899994,12.2,1.82674311799999));
#342583=CARTESIAN_POINT('Ctrl Pts',(3.72476350899994,5.2,1.82674311799999));
#342584=CARTESIAN_POINT('Ctrl Pts',(3.72476350899994,2.2,1.82674311799999));
#342585=CARTESIAN_POINT('Ctrl Pts',(3.72345252799994,12.2,1.82650126599999));
#342586=CARTESIAN_POINT('Ctrl Pts',(3.72345252799994,5.2,1.82650126599999));
#342587=CARTESIAN_POINT('Ctrl Pts',(3.72345252799994,2.2,1.82650126599999));
#342588=CARTESIAN_POINT('Ctrl Pts',(3.72214671299994,12.2,1.82625875999999));
#342589=CARTESIAN_POINT('Ctrl Pts',(3.72214671299994,5.2,1.82625875999999));
#342590=CARTESIAN_POINT('Ctrl Pts',(3.72214671299994,2.2,1.82625875999999));
#342591=CARTESIAN_POINT('Ctrl Pts',(3.72084607199994,12.2,1.82601561299998));
#342592=CARTESIAN_POINT('Ctrl Pts',(3.72084607199994,5.2,1.82601561299998));
#342593=CARTESIAN_POINT('Ctrl Pts',(3.72084607199994,2.2,1.82601561299998));
#342594=CARTESIAN_POINT('Ctrl Pts',(3.71955061299994,12.2,1.82577183799999));
#342595=CARTESIAN_POINT('Ctrl Pts',(3.71955061299994,5.2,1.82577183799999));
#342596=CARTESIAN_POINT('Ctrl Pts',(3.71955061299994,2.2,1.82577183799999));
#342597=CARTESIAN_POINT('Ctrl Pts',(3.71826034199994,12.2,1.82552744599999));
#342598=CARTESIAN_POINT('Ctrl Pts',(3.71826034199994,5.2,1.82552744599999));
#342599=CARTESIAN_POINT('Ctrl Pts',(3.71826034199994,2.2,1.82552744599999));
#342600=CARTESIAN_POINT('Ctrl Pts',(3.71697526499994,12.2,1.82528245099999));
#342601=CARTESIAN_POINT('Ctrl Pts',(3.71697526499994,5.2,1.82528245099999));
#342602=CARTESIAN_POINT('Ctrl Pts',(3.71697526499994,2.2,1.82528245099999));
#342603=CARTESIAN_POINT('Ctrl Pts',(3.71569539199994,12.2,1.82503686499999));
#342604=CARTESIAN_POINT('Ctrl Pts',(3.71569539199994,5.2,1.82503686499999));
#342605=CARTESIAN_POINT('Ctrl Pts',(3.71569539199994,2.2,1.82503686499999));
#342606=CARTESIAN_POINT('Ctrl Pts',(3.71442072799994,12.2,1.82479070099999));
#342607=CARTESIAN_POINT('Ctrl Pts',(3.71442072799994,5.2,1.82479070099999));
#342608=CARTESIAN_POINT('Ctrl Pts',(3.71442072799994,2.2,1.82479070099999));
#342609=CARTESIAN_POINT('Ctrl Pts',(3.71315128099994,12.2,1.82454397199999));
#342610=CARTESIAN_POINT('Ctrl Pts',(3.71315128099994,5.2,1.82454397199999));
#342611=CARTESIAN_POINT('Ctrl Pts',(3.71315128099994,2.2,1.82454397199999));
#342612=CARTESIAN_POINT('Ctrl Pts',(3.71188705699994,12.2,1.82429668899998));
#342613=CARTESIAN_POINT('Ctrl Pts',(3.71188705699994,5.2,1.82429668899998));
#342614=CARTESIAN_POINT('Ctrl Pts',(3.71188705699994,2.2,1.82429668899998));
#342615=CARTESIAN_POINT('Ctrl Pts',(3.71062806599994,12.2,1.82404886699999));
#342616=CARTESIAN_POINT('Ctrl Pts',(3.71062806599994,5.2,1.82404886699999));
#342617=CARTESIAN_POINT('Ctrl Pts',(3.71062806599994,2.2,1.82404886699999));
#342618=CARTESIAN_POINT('Ctrl Pts',(3.70937431099994,12.2,1.82380051699999));
#342619=CARTESIAN_POINT('Ctrl Pts',(3.70937431099994,5.2,1.82380051699999));
#342620=CARTESIAN_POINT('Ctrl Pts',(3.70937431099994,2.2,1.82380051699999));
#342621=CARTESIAN_POINT('Ctrl Pts',(3.70812580199994,12.2,1.82355165499999));
#342622=CARTESIAN_POINT('Ctrl Pts',(3.70812580199994,5.2,1.82355165499999));
#342623=CARTESIAN_POINT('Ctrl Pts',(3.70812580199994,2.2,1.82355165499999));
#342624=CARTESIAN_POINT('Ctrl Pts',(3.70688254499994,12.2,1.82330228899998));
#342625=CARTESIAN_POINT('Ctrl Pts',(3.70688254499994,5.2,1.82330228899998));
#342626=CARTESIAN_POINT('Ctrl Pts',(3.70688254499994,2.2,1.82330228899998));
#342627=CARTESIAN_POINT('Ctrl Pts',(3.70564454699994,12.2,1.82305243699998));
#342628=CARTESIAN_POINT('Ctrl Pts',(3.70564454699994,5.2,1.82305243699998));
#342629=CARTESIAN_POINT('Ctrl Pts',(3.70564454699994,2.2,1.82305243699998));
#342630=CARTESIAN_POINT('Ctrl Pts',(3.70441181699994,12.2,1.82280210899998));
#342631=CARTESIAN_POINT('Ctrl Pts',(3.70441181699994,5.2,1.82280210899998));
#342632=CARTESIAN_POINT('Ctrl Pts',(3.70441181699994,2.2,1.82280210899998));
#342633=CARTESIAN_POINT('Ctrl Pts',(3.70318435899994,12.2,1.82255131799999));
#342634=CARTESIAN_POINT('Ctrl Pts',(3.70318435899994,5.2,1.82255131799999));
#342635=CARTESIAN_POINT('Ctrl Pts',(3.70318435899994,2.2,1.82255131799999));
#342636=CARTESIAN_POINT('Ctrl Pts',(3.70196218199994,12.2,1.82230007799999));
#342637=CARTESIAN_POINT('Ctrl Pts',(3.70196218199994,5.2,1.82230007799999));
#342638=CARTESIAN_POINT('Ctrl Pts',(3.70196218199994,2.2,1.82230007799999));
#342639=CARTESIAN_POINT('Ctrl Pts',(3.70074529299994,12.2,1.82204840299999));
#342640=CARTESIAN_POINT('Ctrl Pts',(3.70074529299994,5.2,1.82204840299999));
#342641=CARTESIAN_POINT('Ctrl Pts',(3.70074529299994,2.2,1.82204840299999));
#342642=CARTESIAN_POINT('Ctrl Pts',(3.69953369899994,12.2,1.82179630399999));
#342643=CARTESIAN_POINT('Ctrl Pts',(3.69953369899994,5.2,1.82179630399999));
#342644=CARTESIAN_POINT('Ctrl Pts',(3.69953369899994,2.2,1.82179630399999));
#342645=CARTESIAN_POINT('Ctrl Pts',(3.69832740599994,12.2,1.82154379499998));
#342646=CARTESIAN_POINT('Ctrl Pts',(3.69832740599994,5.2,1.82154379499998));
#342647=CARTESIAN_POINT('Ctrl Pts',(3.69832740599994,2.2,1.82154379499998));
#342648=CARTESIAN_POINT('Ctrl Pts',(3.69712642399994,12.2,1.82129088999998));
#342649=CARTESIAN_POINT('Ctrl Pts',(3.69712642399994,5.2,1.82129088999998));
#342650=CARTESIAN_POINT('Ctrl Pts',(3.69712642399994,2.2,1.82129088999998));
#342651=CARTESIAN_POINT('Ctrl Pts',(3.69593075599994,12.2,1.82103760199999));
#342652=CARTESIAN_POINT('Ctrl Pts',(3.69593075599994,5.2,1.82103760199999));
#342653=CARTESIAN_POINT('Ctrl Pts',(3.69593075599994,2.2,1.82103760199999));
#342654=CARTESIAN_POINT('Ctrl Pts',(3.69474041299994,12.2,1.82078394399999));
#342655=CARTESIAN_POINT('Ctrl Pts',(3.69474041299994,5.2,1.82078394399999));
#342656=CARTESIAN_POINT('Ctrl Pts',(3.69474041299994,2.2,1.82078394399999));
#342657=CARTESIAN_POINT('Ctrl Pts',(3.69355539899995,12.2,1.82052992899999));
#342658=CARTESIAN_POINT('Ctrl Pts',(3.69355539899995,5.2,1.82052992899999));
#342659=CARTESIAN_POINT('Ctrl Pts',(3.69355539899995,2.2,1.82052992899999));
#342660=CARTESIAN_POINT('Ctrl Pts',(3.69237572299994,12.2,1.82027557199998));
#342661=CARTESIAN_POINT('Ctrl Pts',(3.69237572299994,5.2,1.82027557199998));
#342662=CARTESIAN_POINT('Ctrl Pts',(3.69237572299994,2.2,1.82027557199998));
#342663=CARTESIAN_POINT('Ctrl Pts',(3.69120139099994,12.2,1.82002088299999));
#342664=CARTESIAN_POINT('Ctrl Pts',(3.69120139099994,5.2,1.82002088299999));
#342665=CARTESIAN_POINT('Ctrl Pts',(3.69120139099994,2.2,1.82002088299999));
#342666=CARTESIAN_POINT('Ctrl Pts',(3.69003241099994,12.2,1.81976587899999));
#342667=CARTESIAN_POINT('Ctrl Pts',(3.69003241099994,5.2,1.81976587899999));
#342668=CARTESIAN_POINT('Ctrl Pts',(3.69003241099994,2.2,1.81976587899999));
#342669=CARTESIAN_POINT('Ctrl Pts',(3.68886878899994,12.2,1.81951057199999));
#342670=CARTESIAN_POINT('Ctrl Pts',(3.68886878899994,5.2,1.81951057199999));
#342671=CARTESIAN_POINT('Ctrl Pts',(3.68886878899994,2.2,1.81951057199999));
#342672=CARTESIAN_POINT('Ctrl Pts',(3.68771053399994,12.2,1.81925497599998));
#342673=CARTESIAN_POINT('Ctrl Pts',(3.68771053399994,5.2,1.81925497599998));
#342674=CARTESIAN_POINT('Ctrl Pts',(3.68771053399994,2.2,1.81925497599998));
#342675=CARTESIAN_POINT('Ctrl Pts',(3.68655765099994,12.2,1.81899910299999));
#342676=CARTESIAN_POINT('Ctrl Pts',(3.68655765099994,5.2,1.81899910299999));
#342677=CARTESIAN_POINT('Ctrl Pts',(3.68655765099994,2.2,1.81899910299999));
#342678=CARTESIAN_POINT('Ctrl Pts',(3.68541014799994,12.2,1.81874296999998));
#342679=CARTESIAN_POINT('Ctrl Pts',(3.68541014799994,5.2,1.81874296999998));
#342680=CARTESIAN_POINT('Ctrl Pts',(3.68541014799994,2.2,1.81874296999998));
#342681=CARTESIAN_POINT('Ctrl Pts',(3.68426803199994,12.2,1.81848658699999));
#342682=CARTESIAN_POINT('Ctrl Pts',(3.68426803199994,5.2,1.81848658699999));
#342683=CARTESIAN_POINT('Ctrl Pts',(3.68426803199994,2.2,1.81848658699999));
#342684=CARTESIAN_POINT('Ctrl Pts',(3.68313131099994,12.2,1.81822996999998));
#342685=CARTESIAN_POINT('Ctrl Pts',(3.68313131099994,5.2,1.81822996999998));
#342686=CARTESIAN_POINT('Ctrl Pts',(3.68313131099994,2.2,1.81822996999998));
#342687=CARTESIAN_POINT('Ctrl Pts',(3.68199998999994,12.2,1.81797313199999));
#342688=CARTESIAN_POINT('Ctrl Pts',(3.68199998999994,5.2,1.81797313199999));
#342689=CARTESIAN_POINT('Ctrl Pts',(3.68199998999994,2.2,1.81797313199999));
#342690=CARTESIAN_POINT('Ctrl Pts',(3.68087407699994,12.2,1.81771608599998));
#342691=CARTESIAN_POINT('Ctrl Pts',(3.68087407699994,5.2,1.81771608599998));
#342692=CARTESIAN_POINT('Ctrl Pts',(3.68087407699994,2.2,1.81771608599998));
#342693=CARTESIAN_POINT('Ctrl Pts',(3.67975357999994,12.2,1.81745884699998));
#342694=CARTESIAN_POINT('Ctrl Pts',(3.67975357999994,5.2,1.81745884699998));
#342695=CARTESIAN_POINT('Ctrl Pts',(3.67975357999994,2.2,1.81745884699998));
#342696=CARTESIAN_POINT('Ctrl Pts',(3.67863850499994,12.2,1.81720142899998));
#342697=CARTESIAN_POINT('Ctrl Pts',(3.67863850499994,5.2,1.81720142899998));
#342698=CARTESIAN_POINT('Ctrl Pts',(3.67863850499994,2.2,1.81720142899998));
#342699=CARTESIAN_POINT('Ctrl Pts',(3.67752885999994,12.2,1.81694384599998));
#342700=CARTESIAN_POINT('Ctrl Pts',(3.67752885999994,5.2,1.81694384599998));
#342701=CARTESIAN_POINT('Ctrl Pts',(3.67752885999994,2.2,1.81694384599998));
#342702=CARTESIAN_POINT('Ctrl Pts',(3.67642465199994,12.2,1.81668610999999));
#342703=CARTESIAN_POINT('Ctrl Pts',(3.67642465199994,5.2,1.81668610999999));
#342704=CARTESIAN_POINT('Ctrl Pts',(3.67642465199994,2.2,1.81668610999999));
#342705=CARTESIAN_POINT('Ctrl Pts',(3.67532588699994,12.2,1.81642823799999));
#342706=CARTESIAN_POINT('Ctrl Pts',(3.67532588699994,5.2,1.81642823799999));
#342707=CARTESIAN_POINT('Ctrl Pts',(3.67532588699994,2.2,1.81642823799999));
#342708=CARTESIAN_POINT('Ctrl Pts',(3.67423257199994,12.2,1.81617024099999));
#342709=CARTESIAN_POINT('Ctrl Pts',(3.67423257199994,5.2,1.81617024099999));
#342710=CARTESIAN_POINT('Ctrl Pts',(3.67423257199994,2.2,1.81617024099999));
#342711=CARTESIAN_POINT('Ctrl Pts',(3.67314471499994,12.2,1.81591213499999));
#342712=CARTESIAN_POINT('Ctrl Pts',(3.67314471499994,5.2,1.81591213499999));
#342713=CARTESIAN_POINT('Ctrl Pts',(3.67314471499994,2.2,1.81591213499999));
#342714=CARTESIAN_POINT('Ctrl Pts',(3.67206232299994,12.2,1.81565393399998));
#342715=CARTESIAN_POINT('Ctrl Pts',(3.67206232299994,5.2,1.81565393399998));
#342716=CARTESIAN_POINT('Ctrl Pts',(3.67206232299994,2.2,1.81565393399998));
#342717=CARTESIAN_POINT('Ctrl Pts',(3.67098540399994,12.2,1.81539565199999));
#342718=CARTESIAN_POINT('Ctrl Pts',(3.67098540399994,5.2,1.81539565199999));
#342719=CARTESIAN_POINT('Ctrl Pts',(3.67098540399994,2.2,1.81539565199999));
#342720=CARTESIAN_POINT('Ctrl Pts',(3.66991396299994,12.2,1.81513730299999));
#342721=CARTESIAN_POINT('Ctrl Pts',(3.66991396299994,5.2,1.81513730299999));
#342722=CARTESIAN_POINT('Ctrl Pts',(3.66991396299994,2.2,1.81513730299999));
#342723=CARTESIAN_POINT('Ctrl Pts',(3.66884800699994,12.2,1.81487890099998));
#342724=CARTESIAN_POINT('Ctrl Pts',(3.66884800699994,5.2,1.81487890099998));
#342725=CARTESIAN_POINT('Ctrl Pts',(3.66884800699994,2.2,1.81487890099998));
#342726=CARTESIAN_POINT('Ctrl Pts',(3.66778754499994,12.2,1.81462046099998));
#342727=CARTESIAN_POINT('Ctrl Pts',(3.66778754499994,5.2,1.81462046099998));
#342728=CARTESIAN_POINT('Ctrl Pts',(3.66778754499994,2.2,1.81462046099998));
#342729=CARTESIAN_POINT('Ctrl Pts',(3.66673258299994,12.2,1.81436199699998));
#342730=CARTESIAN_POINT('Ctrl Pts',(3.66673258299994,5.2,1.81436199699998));
#342731=CARTESIAN_POINT('Ctrl Pts',(3.66673258299994,2.2,1.81436199699998));
#342732=CARTESIAN_POINT('Ctrl Pts',(3.66568312899994,12.2,1.81410352299999));
#342733=CARTESIAN_POINT('Ctrl Pts',(3.66568312899994,5.2,1.81410352299999));
#342734=CARTESIAN_POINT('Ctrl Pts',(3.66568312899994,2.2,1.81410352299999));
#342735=CARTESIAN_POINT('Ctrl Pts',(3.66463918899994,12.2,1.81384505499999));
#342736=CARTESIAN_POINT('Ctrl Pts',(3.66463918899994,5.2,1.81384505499999));
#342737=CARTESIAN_POINT('Ctrl Pts',(3.66463918899994,2.2,1.81384505499999));
#342738=CARTESIAN_POINT('Ctrl Pts',(3.66360076999994,12.2,1.81358660399999));
#342739=CARTESIAN_POINT('Ctrl Pts',(3.66360076999994,5.2,1.81358660399999));
#342740=CARTESIAN_POINT('Ctrl Pts',(3.66360076999994,2.2,1.81358660399999));
#342741=CARTESIAN_POINT('Ctrl Pts',(3.66256787899994,12.2,1.81332818799998));
#342742=CARTESIAN_POINT('Ctrl Pts',(3.66256787899994,5.2,1.81332818799998));
#342743=CARTESIAN_POINT('Ctrl Pts',(3.66256787899994,2.2,1.81332818799998));
#342744=CARTESIAN_POINT('Ctrl Pts',(3.66154052399994,12.2,1.81306981999999));
#342745=CARTESIAN_POINT('Ctrl Pts',(3.66154052399994,5.2,1.81306981999999));
#342746=CARTESIAN_POINT('Ctrl Pts',(3.66154052399994,2.2,1.81306981999999));
#342747=CARTESIAN_POINT('Ctrl Pts',(3.66051871099994,12.2,1.81281151599999));
#342748=CARTESIAN_POINT('Ctrl Pts',(3.66051871099994,5.2,1.81281151599999));
#342749=CARTESIAN_POINT('Ctrl Pts',(3.66051871099994,2.2,1.81281151599999));
#342750=CARTESIAN_POINT('Ctrl Pts',(3.65950244799994,12.2,1.81255328999999));
#342751=CARTESIAN_POINT('Ctrl Pts',(3.65950244799994,5.2,1.81255328999999));
#342752=CARTESIAN_POINT('Ctrl Pts',(3.65950244799994,2.2,1.81255328999999));
#342753=CARTESIAN_POINT('Ctrl Pts',(3.65849174099994,12.2,1.81229515499998));
#342754=CARTESIAN_POINT('Ctrl Pts',(3.65849174099994,5.2,1.81229515499998));
#342755=CARTESIAN_POINT('Ctrl Pts',(3.65849174099994,2.2,1.81229515499998));
#342756=CARTESIAN_POINT('Ctrl Pts',(3.65748659799995,12.2,1.81203712699999));
#342757=CARTESIAN_POINT('Ctrl Pts',(3.65748659799995,5.2,1.81203712699999));
#342758=CARTESIAN_POINT('Ctrl Pts',(3.65748659799995,2.2,1.81203712699999));
#342759=CARTESIAN_POINT('Ctrl Pts',(3.65648702599994,12.2,1.81177922199999));
#342760=CARTESIAN_POINT('Ctrl Pts',(3.65648702599994,5.2,1.81177922199999));
#342761=CARTESIAN_POINT('Ctrl Pts',(3.65648702599994,2.2,1.81177922199999));
#342762=CARTESIAN_POINT('Ctrl Pts',(3.65549302999994,12.2,1.81152145299999));
#342763=CARTESIAN_POINT('Ctrl Pts',(3.65549302999994,5.2,1.81152145299999));
#342764=CARTESIAN_POINT('Ctrl Pts',(3.65549302999994,2.2,1.81152145299999));
#342765=CARTESIAN_POINT('Ctrl Pts',(3.65450462099994,12.2,1.81126383599999));
#342766=CARTESIAN_POINT('Ctrl Pts',(3.65450462099994,5.2,1.81126383599999));
#342767=CARTESIAN_POINT('Ctrl Pts',(3.65450462099994,2.2,1.81126383599999));
#342768=CARTESIAN_POINT('Ctrl Pts',(3.65352180299995,12.2,1.81100638499998));
#342769=CARTESIAN_POINT('Ctrl Pts',(3.65352180299995,5.2,1.81100638499998));
#342770=CARTESIAN_POINT('Ctrl Pts',(3.65352180299995,2.2,1.81100638499998));
#342771=CARTESIAN_POINT('Ctrl Pts',(3.65254458399995,12.2,1.81074911599998));
#342772=CARTESIAN_POINT('Ctrl Pts',(3.65254458399995,5.2,1.81074911599998));
#342773=CARTESIAN_POINT('Ctrl Pts',(3.65254458399995,2.2,1.81074911599998));
#342774=CARTESIAN_POINT('Ctrl Pts',(3.65157297099994,12.2,1.81049204299998));
#342775=CARTESIAN_POINT('Ctrl Pts',(3.65157297099994,5.2,1.81049204299998));
#342776=CARTESIAN_POINT('Ctrl Pts',(3.65157297099994,2.2,1.81049204299998));
#342777=CARTESIAN_POINT('Ctrl Pts',(3.65060696999994,12.2,1.81023518199999));
#342778=CARTESIAN_POINT('Ctrl Pts',(3.65060696999994,5.2,1.81023518199999));
#342779=CARTESIAN_POINT('Ctrl Pts',(3.65060696999994,2.2,1.81023518199999));
#342780=CARTESIAN_POINT('Ctrl Pts',(3.64964658899994,12.2,1.80997854799998));
#342781=CARTESIAN_POINT('Ctrl Pts',(3.64964658899994,5.2,1.80997854799998));
#342782=CARTESIAN_POINT('Ctrl Pts',(3.64964658899994,2.2,1.80997854799998));
#342783=CARTESIAN_POINT('Ctrl Pts',(3.64869183599994,12.2,1.80972215599999));
#342784=CARTESIAN_POINT('Ctrl Pts',(3.64869183599994,5.2,1.80972215599999));
#342785=CARTESIAN_POINT('Ctrl Pts',(3.64869183599994,2.2,1.80972215599999));
#342786=CARTESIAN_POINT('Ctrl Pts',(3.64774271599994,12.2,1.80946602099999));
#342787=CARTESIAN_POINT('Ctrl Pts',(3.64774271599994,5.2,1.80946602099999));
#342788=CARTESIAN_POINT('Ctrl Pts',(3.64774271599994,2.2,1.80946602099999));
#342789=CARTESIAN_POINT('Ctrl Pts',(3.64679923799994,12.2,1.80921015799999));
#342790=CARTESIAN_POINT('Ctrl Pts',(3.64679923799994,5.2,1.80921015799999));
#342791=CARTESIAN_POINT('Ctrl Pts',(3.64679923799994,2.2,1.80921015799999));
#342792=CARTESIAN_POINT('Ctrl Pts',(3.64586140799994,12.2,1.80895458299998));
#342793=CARTESIAN_POINT('Ctrl Pts',(3.64586140799994,5.2,1.80895458299998));
#342794=CARTESIAN_POINT('Ctrl Pts',(3.64586140799994,2.2,1.80895458299998));
#342795=CARTESIAN_POINT('Ctrl Pts',(3.64492923299994,12.2,1.80869930999998));
#342796=CARTESIAN_POINT('Ctrl Pts',(3.64492923299994,5.2,1.80869930999998));
#342797=CARTESIAN_POINT('Ctrl Pts',(3.64492923299994,2.2,1.80869930999998));
#342798=CARTESIAN_POINT('Ctrl Pts',(3.64400271999994,12.2,1.80844435699999));
#342799=CARTESIAN_POINT('Ctrl Pts',(3.64400271999994,5.2,1.80844435699999));
#342800=CARTESIAN_POINT('Ctrl Pts',(3.64400271999994,2.2,1.80844435699999));
#342801=CARTESIAN_POINT('Ctrl Pts',(3.64308187599994,12.2,1.80818973699999));
#342802=CARTESIAN_POINT('Ctrl Pts',(3.64308187599994,5.2,1.80818973699999));
#342803=CARTESIAN_POINT('Ctrl Pts',(3.64308187599994,2.2,1.80818973699999));
#342804=CARTESIAN_POINT('Ctrl Pts',(3.64216670899994,12.2,1.80793546599999));
#342805=CARTESIAN_POINT('Ctrl Pts',(3.64216670899994,5.2,1.80793546599999));
#342806=CARTESIAN_POINT('Ctrl Pts',(3.64216670899994,2.2,1.80793546599999));
#342807=CARTESIAN_POINT('Ctrl Pts',(3.64125722499994,12.2,1.80768156099999));
#342808=CARTESIAN_POINT('Ctrl Pts',(3.64125722499994,5.2,1.80768156099999));
#342809=CARTESIAN_POINT('Ctrl Pts',(3.64125722499994,2.2,1.80768156099999));
#342810=CARTESIAN_POINT('Ctrl Pts',(3.64035343099994,12.2,1.80742803599999));
#342811=CARTESIAN_POINT('Ctrl Pts',(3.64035343099994,5.2,1.80742803599999));
#342812=CARTESIAN_POINT('Ctrl Pts',(3.64035343099994,2.2,1.80742803599999));
#342813=CARTESIAN_POINT('Ctrl Pts',(3.63945533399994,12.2,1.80717490699998));
#342814=CARTESIAN_POINT('Ctrl Pts',(3.63945533399994,5.2,1.80717490699998));
#342815=CARTESIAN_POINT('Ctrl Pts',(3.63945533399994,2.2,1.80717490699998));
#342816=CARTESIAN_POINT('Ctrl Pts',(3.63856294199994,12.2,1.80692218999999));
#342817=CARTESIAN_POINT('Ctrl Pts',(3.63856294199994,5.2,1.80692218999999));
#342818=CARTESIAN_POINT('Ctrl Pts',(3.63856294199994,2.2,1.80692218999999));
#342819=CARTESIAN_POINT('Ctrl Pts',(3.63767625999994,12.2,1.80666990099999));
#342820=CARTESIAN_POINT('Ctrl Pts',(3.63767625999994,5.2,1.80666990099999));
#342821=CARTESIAN_POINT('Ctrl Pts',(3.63767625999994,2.2,1.80666990099999));
#342822=CARTESIAN_POINT('Ctrl Pts',(3.63679529799994,12.2,1.80641805499999));
#342823=CARTESIAN_POINT('Ctrl Pts',(3.63679529799994,5.2,1.80641805499999));
#342824=CARTESIAN_POINT('Ctrl Pts',(3.63679529799994,2.2,1.80641805499999));
#342825=CARTESIAN_POINT('Ctrl Pts',(3.63592005999994,12.2,1.80616666899999));
#342826=CARTESIAN_POINT('Ctrl Pts',(3.63592005999994,5.2,1.80616666899999));
#342827=CARTESIAN_POINT('Ctrl Pts',(3.63592005999994,2.2,1.80616666899999));
#342828=CARTESIAN_POINT('Ctrl Pts',(3.63505055499994,12.2,1.80591575699999));
#342829=CARTESIAN_POINT('Ctrl Pts',(3.63505055499994,5.2,1.80591575699999));
#342830=CARTESIAN_POINT('Ctrl Pts',(3.63505055499994,2.2,1.80591575699999));
#342831=CARTESIAN_POINT('Ctrl Pts',(3.63418678899994,12.2,1.80566533699999));
#342832=CARTESIAN_POINT('Ctrl Pts',(3.63418678899994,5.2,1.80566533699999));
#342833=CARTESIAN_POINT('Ctrl Pts',(3.63418678899994,2.2,1.80566533699999));
#342834=CARTESIAN_POINT('Ctrl Pts',(3.63332876999995,12.2,1.80541542399999));
#342835=CARTESIAN_POINT('Ctrl Pts',(3.63332876999995,5.2,1.80541542399999));
#342836=CARTESIAN_POINT('Ctrl Pts',(3.63332876999995,2.2,1.80541542399999));
#342837=CARTESIAN_POINT('Ctrl Pts',(3.63247650399994,12.2,1.80516603399999));
#342838=CARTESIAN_POINT('Ctrl Pts',(3.63247650399994,5.2,1.80516603399999));
#342839=CARTESIAN_POINT('Ctrl Pts',(3.63247650399994,2.2,1.80516603399999));
#342840=CARTESIAN_POINT('Ctrl Pts',(3.63162999899994,12.2,1.80491718299999));
#342841=CARTESIAN_POINT('Ctrl Pts',(3.63162999899994,5.2,1.80491718299999));
#342842=CARTESIAN_POINT('Ctrl Pts',(3.63162999899994,2.2,1.80491718299999));
#342843=CARTESIAN_POINT('Ctrl Pts',(3.63078926099994,12.2,1.80466888799999));
#342844=CARTESIAN_POINT('Ctrl Pts',(3.63078926099994,5.2,1.80466888799999));
#342845=CARTESIAN_POINT('Ctrl Pts',(3.63078926099994,2.2,1.80466888799999));
#342846=CARTESIAN_POINT('Ctrl Pts',(3.62995429699994,12.2,1.80442116399998));
#342847=CARTESIAN_POINT('Ctrl Pts',(3.62995429699994,5.2,1.80442116399998));
#342848=CARTESIAN_POINT('Ctrl Pts',(3.62995429699994,2.2,1.80442116399998));
#342849=CARTESIAN_POINT('Ctrl Pts',(3.62912511499994,12.2,1.80417402799999));
#342850=CARTESIAN_POINT('Ctrl Pts',(3.62912511499994,5.2,1.80417402799999));
#342851=CARTESIAN_POINT('Ctrl Pts',(3.62912511499994,2.2,1.80417402799999));
#342852=CARTESIAN_POINT('Ctrl Pts',(3.62830172199994,12.2,1.80392749599998));
#342853=CARTESIAN_POINT('Ctrl Pts',(3.62830172199994,5.2,1.80392749599998));
#342854=CARTESIAN_POINT('Ctrl Pts',(3.62830172199994,2.2,1.80392749599998));
#342855=CARTESIAN_POINT('Ctrl Pts',(3.62748412299994,12.2,1.80368158599999));
#342856=CARTESIAN_POINT('Ctrl Pts',(3.62748412299994,5.2,1.80368158599999));
#342857=CARTESIAN_POINT('Ctrl Pts',(3.62748412299994,2.2,1.80368158599999));
#342858=CARTESIAN_POINT('Ctrl Pts',(3.62667232799994,12.2,1.80343631099999));
#342859=CARTESIAN_POINT('Ctrl Pts',(3.62667232799994,5.2,1.80343631099999));
#342860=CARTESIAN_POINT('Ctrl Pts',(3.62667232799994,2.2,1.80343631099999));
#342861=CARTESIAN_POINT('Ctrl Pts',(3.62586634099994,12.2,1.80319168999999));
#342862=CARTESIAN_POINT('Ctrl Pts',(3.62586634099994,5.2,1.80319168999999));
#342863=CARTESIAN_POINT('Ctrl Pts',(3.62586634099994,2.2,1.80319168999999));
#342864=CARTESIAN_POINT('Ctrl Pts',(3.62506617099994,12.2,1.80294773999998));
#342865=CARTESIAN_POINT('Ctrl Pts',(3.62506617099994,5.2,1.80294773999998));
#342866=CARTESIAN_POINT('Ctrl Pts',(3.62506617099994,2.2,1.80294773999998));
#342867=CARTESIAN_POINT('Ctrl Pts',(3.62427182399994,12.2,1.80270447599999));
#342868=CARTESIAN_POINT('Ctrl Pts',(3.62427182399994,5.2,1.80270447599999));
#342869=CARTESIAN_POINT('Ctrl Pts',(3.62427182399994,2.2,1.80270447599999));
#342870=CARTESIAN_POINT('Ctrl Pts',(3.62348330799994,12.2,1.80246191399998));
#342871=CARTESIAN_POINT('Ctrl Pts',(3.62348330799994,5.2,1.80246191399998));
#342872=CARTESIAN_POINT('Ctrl Pts',(3.62348330799994,2.2,1.80246191399998));
#342873=CARTESIAN_POINT('Ctrl Pts',(3.62270062899994,12.2,1.80222007199998));
#342874=CARTESIAN_POINT('Ctrl Pts',(3.62270062899994,5.2,1.80222007199998));
#342875=CARTESIAN_POINT('Ctrl Pts',(3.62270062899994,2.2,1.80222007199998));
#342876=CARTESIAN_POINT('Ctrl Pts',(3.62192379399994,12.2,1.80197896699998));
#342877=CARTESIAN_POINT('Ctrl Pts',(3.62192379399994,5.2,1.80197896699998));
#342878=CARTESIAN_POINT('Ctrl Pts',(3.62192379399994,2.2,1.80197896699998));
#342879=CARTESIAN_POINT('Ctrl Pts',(3.62115281099994,12.2,1.80173861599998));
#342880=CARTESIAN_POINT('Ctrl Pts',(3.62115281099994,5.2,1.80173861599998));
#342881=CARTESIAN_POINT('Ctrl Pts',(3.62115281099994,2.2,1.80173861599998));
#342882=CARTESIAN_POINT('Ctrl Pts',(3.62038768599994,12.2,1.80149903499998));
#342883=CARTESIAN_POINT('Ctrl Pts',(3.62038768599994,5.2,1.80149903499998));
#342884=CARTESIAN_POINT('Ctrl Pts',(3.62038768599994,2.2,1.80149903499998));
#342885=CARTESIAN_POINT('Ctrl Pts',(3.61962842599994,12.2,1.80126024099998));
#342886=CARTESIAN_POINT('Ctrl Pts',(3.61962842599994,5.2,1.80126024099998));
#342887=CARTESIAN_POINT('Ctrl Pts',(3.61962842599994,2.2,1.80126024099998));
#342888=CARTESIAN_POINT('Ctrl Pts',(3.61887503899994,12.2,1.80102225099999));
#342889=CARTESIAN_POINT('Ctrl Pts',(3.61887503899994,5.2,1.80102225099999));
#342890=CARTESIAN_POINT('Ctrl Pts',(3.61887503899994,2.2,1.80102225099999));
#342891=CARTESIAN_POINT('Ctrl Pts',(3.61812753099994,12.2,1.80078508099998));
#342892=CARTESIAN_POINT('Ctrl Pts',(3.61812753099994,5.2,1.80078508099998));
#342893=CARTESIAN_POINT('Ctrl Pts',(3.61812753099994,2.2,1.80078508099998));
#342894=CARTESIAN_POINT('Ctrl Pts',(3.61738590899995,12.2,1.80054874999998));
#342895=CARTESIAN_POINT('Ctrl Pts',(3.61738590899995,5.2,1.80054874999998));
#342896=CARTESIAN_POINT('Ctrl Pts',(3.61738590899995,2.2,1.80054874999998));
#342897=CARTESIAN_POINT('Ctrl Pts',(3.61665018099994,12.2,1.80031327399998));
#342898=CARTESIAN_POINT('Ctrl Pts',(3.61665018099994,5.2,1.80031327399998));
#342899=CARTESIAN_POINT('Ctrl Pts',(3.61665018099994,2.2,1.80031327399998));
#342900=CARTESIAN_POINT('Ctrl Pts',(3.61592035299994,12.2,1.80007867099999));
#342901=CARTESIAN_POINT('Ctrl Pts',(3.61592035299994,5.2,1.80007867099999));
#342902=CARTESIAN_POINT('Ctrl Pts',(3.61592035299994,2.2,1.80007867099999));
#342903=CARTESIAN_POINT('Ctrl Pts',(3.61519643199994,12.2,1.79984495799999));
#342904=CARTESIAN_POINT('Ctrl Pts',(3.61519643199994,5.2,1.79984495799999));
#342905=CARTESIAN_POINT('Ctrl Pts',(3.61519643199994,2.2,1.79984495799999));
#342906=CARTESIAN_POINT('Ctrl Pts',(3.61447842499994,12.2,1.79961215099999));
#342907=CARTESIAN_POINT('Ctrl Pts',(3.61447842499994,5.2,1.79961215099999));
#342908=CARTESIAN_POINT('Ctrl Pts',(3.61447842499994,2.2,1.79961215099999));
#342909=CARTESIAN_POINT('Ctrl Pts',(3.61376633899994,12.2,1.79938026799999));
#342910=CARTESIAN_POINT('Ctrl Pts',(3.61376633899994,5.2,1.79938026799999));
#342911=CARTESIAN_POINT('Ctrl Pts',(3.61376633899994,2.2,1.79938026799999));
#342912=CARTESIAN_POINT('Ctrl Pts',(3.61306018199994,12.2,1.79914932599999));
#342913=CARTESIAN_POINT('Ctrl Pts',(3.61306018199994,5.2,1.79914932599999));
#342914=CARTESIAN_POINT('Ctrl Pts',(3.61306018199994,2.2,1.79914932599999));
#342915=CARTESIAN_POINT('Ctrl Pts',(3.61235995899994,12.2,1.79891934399999));
#342916=CARTESIAN_POINT('Ctrl Pts',(3.61235995899994,5.2,1.79891934399999));
#342917=CARTESIAN_POINT('Ctrl Pts',(3.61235995899994,2.2,1.79891934399999));
#342918=CARTESIAN_POINT('Ctrl Pts',(3.61166567899994,12.2,1.79869033999998));
#342919=CARTESIAN_POINT('Ctrl Pts',(3.61166567899994,5.2,1.79869033999998));
#342920=CARTESIAN_POINT('Ctrl Pts',(3.61166567899994,2.2,1.79869033999998));
#342921=CARTESIAN_POINT('Ctrl Pts',(3.61097734699994,12.2,1.79846232899999));
#342922=CARTESIAN_POINT('Ctrl Pts',(3.61097734699994,5.2,1.79846232899999));
#342923=CARTESIAN_POINT('Ctrl Pts',(3.61097734699994,2.2,1.79846232899999));
#342924=CARTESIAN_POINT('Ctrl Pts',(3.61029497199994,12.2,1.79823532999999));
#342925=CARTESIAN_POINT('Ctrl Pts',(3.61029497199994,5.2,1.79823532999999));
#342926=CARTESIAN_POINT('Ctrl Pts',(3.61029497199994,2.2,1.79823532999999));
#342927=CARTESIAN_POINT('Ctrl Pts',(3.60961855799994,12.2,1.79800935999999));
#342928=CARTESIAN_POINT('Ctrl Pts',(3.60961855799994,5.2,1.79800935999999));
#342929=CARTESIAN_POINT('Ctrl Pts',(3.60961855799994,2.2,1.79800935999999));
#342930=CARTESIAN_POINT('Ctrl Pts',(3.60894811499994,12.2,1.79778443799998));
#342931=CARTESIAN_POINT('Ctrl Pts',(3.60894811499994,5.2,1.79778443799998));
#342932=CARTESIAN_POINT('Ctrl Pts',(3.60894811499994,2.2,1.79778443799998));
#342933=CARTESIAN_POINT('Ctrl Pts',(3.60828364999994,12.2,1.79756058099999));
#342934=CARTESIAN_POINT('Ctrl Pts',(3.60828364999994,5.2,1.79756058099999));
#342935=CARTESIAN_POINT('Ctrl Pts',(3.60828364999994,2.2,1.79756058099999));
#342936=CARTESIAN_POINT('Ctrl Pts',(3.60762516799995,12.2,1.79733780699999));
#342937=CARTESIAN_POINT('Ctrl Pts',(3.60762516799995,5.2,1.79733780699999));
#342938=CARTESIAN_POINT('Ctrl Pts',(3.60762516799995,2.2,1.79733780699999));
#342939=CARTESIAN_POINT('Ctrl Pts',(3.60697267599994,12.2,1.79711613399999));
#342940=CARTESIAN_POINT('Ctrl Pts',(3.60697267599994,5.2,1.79711613399999));
#342941=CARTESIAN_POINT('Ctrl Pts',(3.60697267599994,2.2,1.79711613399999));
#342942=CARTESIAN_POINT('Ctrl Pts',(3.60632618199995,12.2,1.79689557899998));
#342943=CARTESIAN_POINT('Ctrl Pts',(3.60632618199995,5.2,1.79689557899998));
#342944=CARTESIAN_POINT('Ctrl Pts',(3.60632618199995,2.2,1.79689557899998));
#342945=CARTESIAN_POINT('Ctrl Pts',(3.60568569299994,12.2,1.79667616299998));
#342946=CARTESIAN_POINT('Ctrl Pts',(3.60568569299994,5.2,1.79667616299998));
#342947=CARTESIAN_POINT('Ctrl Pts',(3.60568569299994,2.2,1.79667616299998));
#342948=CARTESIAN_POINT('Ctrl Pts',(3.60505121499994,12.2,1.79645790099999));
#342949=CARTESIAN_POINT('Ctrl Pts',(3.60505121499994,5.2,1.79645790099999));
#342950=CARTESIAN_POINT('Ctrl Pts',(3.60505121499994,2.2,1.79645790099999));
#342951=CARTESIAN_POINT('Ctrl Pts',(3.60442275599994,12.2,1.79624081099998));
#342952=CARTESIAN_POINT('Ctrl Pts',(3.60442275599994,5.2,1.79624081099998));
#342953=CARTESIAN_POINT('Ctrl Pts',(3.60442275599994,2.2,1.79624081099998));
#342954=CARTESIAN_POINT('Ctrl Pts',(3.60380032199994,12.2,1.79602491399999));
#342955=CARTESIAN_POINT('Ctrl Pts',(3.60380032199994,5.2,1.79602491399999));
#342956=CARTESIAN_POINT('Ctrl Pts',(3.60380032199994,2.2,1.79602491399999));
#342957=CARTESIAN_POINT('Ctrl Pts',(3.60318392099995,12.2,1.79581022599999));
#342958=CARTESIAN_POINT('Ctrl Pts',(3.60318392099995,5.2,1.79581022599999));
#342959=CARTESIAN_POINT('Ctrl Pts',(3.60318392099995,2.2,1.79581022599999));
#342960=CARTESIAN_POINT('Ctrl Pts',(3.60257355899994,12.2,1.79559676699999));
#342961=CARTESIAN_POINT('Ctrl Pts',(3.60257355899994,5.2,1.79559676699999));
#342962=CARTESIAN_POINT('Ctrl Pts',(3.60257355899994,2.2,1.79559676699999));
#342963=CARTESIAN_POINT('Ctrl Pts',(3.60196924399994,12.2,1.79538455399999));
#342964=CARTESIAN_POINT('Ctrl Pts',(3.60196924399994,5.2,1.79538455399999));
#342965=CARTESIAN_POINT('Ctrl Pts',(3.60196924399994,2.2,1.79538455399999));
#342966=CARTESIAN_POINT('Ctrl Pts',(3.60137098099994,12.2,1.79517360599998));
#342967=CARTESIAN_POINT('Ctrl Pts',(3.60137098099994,5.2,1.79517360599998));
#342968=CARTESIAN_POINT('Ctrl Pts',(3.60137098099994,2.2,1.79517360599998));
#342969=CARTESIAN_POINT('Ctrl Pts',(3.60077877899994,12.2,1.79496394199999));
#342970=CARTESIAN_POINT('Ctrl Pts',(3.60077877899994,5.2,1.79496394199999));
#342971=CARTESIAN_POINT('Ctrl Pts',(3.60077877899994,2.2,1.79496394199999));
#342972=CARTESIAN_POINT('Ctrl Pts',(3.60019264299994,12.2,1.79475557999998));
#342973=CARTESIAN_POINT('Ctrl Pts',(3.60019264299994,5.2,1.79475557999998));
#342974=CARTESIAN_POINT('Ctrl Pts',(3.60019264299994,2.2,1.79475557999998));
#342975=CARTESIAN_POINT('Ctrl Pts',(3.59961258299994,12.2,1.79454853799998));
#342976=CARTESIAN_POINT('Ctrl Pts',(3.59961258299994,5.2,1.79454853799998));
#342977=CARTESIAN_POINT('Ctrl Pts',(3.59961258299994,2.2,1.79454853799998));
#342978=CARTESIAN_POINT('Ctrl Pts',(3.59903860199994,12.2,1.79434283699999));
#342979=CARTESIAN_POINT('Ctrl Pts',(3.59903860199994,5.2,1.79434283699999));
#342980=CARTESIAN_POINT('Ctrl Pts',(3.59903860199994,2.2,1.79434283699999));
#342981=CARTESIAN_POINT('Ctrl Pts',(3.59847070999994,12.2,1.79413849399999));
#342982=CARTESIAN_POINT('Ctrl Pts',(3.59847070999994,5.2,1.79413849399999));
#342983=CARTESIAN_POINT('Ctrl Pts',(3.59847070999994,2.2,1.79413849399999));
#342984=CARTESIAN_POINT('Ctrl Pts',(3.59790891199994,12.2,1.79393552899999));
#342985=CARTESIAN_POINT('Ctrl Pts',(3.59790891199994,5.2,1.79393552899999));
#342986=CARTESIAN_POINT('Ctrl Pts',(3.59790891199994,2.2,1.79393552899999));
#342987=CARTESIAN_POINT('Ctrl Pts',(3.59735321699994,12.2,1.79373395799999));
#342988=CARTESIAN_POINT('Ctrl Pts',(3.59735321699994,5.2,1.79373395799999));
#342989=CARTESIAN_POINT('Ctrl Pts',(3.59735321699994,2.2,1.79373395799999));
#342990=CARTESIAN_POINT('Ctrl Pts',(3.59680362899994,12.2,1.79353380499998));
#342991=CARTESIAN_POINT('Ctrl Pts',(3.59680362899994,5.2,1.79353380499998));
#342992=CARTESIAN_POINT('Ctrl Pts',(3.59680362899994,2.2,1.79353380499998));
#342993=CARTESIAN_POINT('Ctrl Pts',(3.59626015799994,12.2,1.79333508399999));
#342994=CARTESIAN_POINT('Ctrl Pts',(3.59626015799994,5.2,1.79333508399999));
#342995=CARTESIAN_POINT('Ctrl Pts',(3.59626015799994,2.2,1.79333508399999));
#342996=CARTESIAN_POINT('Ctrl Pts',(3.59572280899994,12.2,1.79313781699999));
#342997=CARTESIAN_POINT('Ctrl Pts',(3.59572280899994,5.2,1.79313781699999));
#342998=CARTESIAN_POINT('Ctrl Pts',(3.59572280899994,2.2,1.79313781699999));
#342999=CARTESIAN_POINT('Ctrl Pts',(3.59519158999994,12.2,1.79294202399999));
#343000=CARTESIAN_POINT('Ctrl Pts',(3.59519158999994,5.2,1.79294202399999));
#343001=CARTESIAN_POINT('Ctrl Pts',(3.59519158999994,2.2,1.79294202399999));
#343002=CARTESIAN_POINT('Ctrl Pts',(3.59466650499995,12.2,1.79274772199999));
#343003=CARTESIAN_POINT('Ctrl Pts',(3.59466650499995,5.2,1.79274772199999));
#343004=CARTESIAN_POINT('Ctrl Pts',(3.59466650499995,2.2,1.79274772199999));
#343005=CARTESIAN_POINT('Ctrl Pts',(3.59414756599994,12.2,1.79255492999999));
#343006=CARTESIAN_POINT('Ctrl Pts',(3.59414756599994,5.2,1.79255492999999));
#343007=CARTESIAN_POINT('Ctrl Pts',(3.59414756599994,2.2,1.79255492999999));
#343008=CARTESIAN_POINT('Ctrl Pts',(3.59363477599994,12.2,1.79236366999998));
#343009=CARTESIAN_POINT('Ctrl Pts',(3.59363477599994,5.2,1.79236366999998));
#343010=CARTESIAN_POINT('Ctrl Pts',(3.59363477599994,2.2,1.79236366999998));
#343011=CARTESIAN_POINT('Ctrl Pts',(3.59312814299994,12.2,1.79217395899999));
#343012=CARTESIAN_POINT('Ctrl Pts',(3.59312814299994,5.2,1.79217395899999));
#343013=CARTESIAN_POINT('Ctrl Pts',(3.59312814299994,2.2,1.79217395899999));
#343014=CARTESIAN_POINT('Ctrl Pts',(3.59262767399994,12.2,1.79198581899998));
#343015=CARTESIAN_POINT('Ctrl Pts',(3.59262767399994,5.2,1.79198581899998));
#343016=CARTESIAN_POINT('Ctrl Pts',(3.59262767399994,2.2,1.79198581899998));
#343017=CARTESIAN_POINT('Ctrl Pts',(3.59213337499994,12.2,1.79179926699998));
#343018=CARTESIAN_POINT('Ctrl Pts',(3.59213337499994,5.2,1.79179926699998));
#343019=CARTESIAN_POINT('Ctrl Pts',(3.59213337499994,2.2,1.79179926699998));
#343020=CARTESIAN_POINT('Ctrl Pts',(3.59164525599994,12.2,1.79161432399999));
#343021=CARTESIAN_POINT('Ctrl Pts',(3.59164525599994,5.2,1.79161432399999));
#343022=CARTESIAN_POINT('Ctrl Pts',(3.59164525599994,2.2,1.79161432399999));
#343023=CARTESIAN_POINT('Ctrl Pts',(3.59116331899994,12.2,1.79143100999998));
#343024=CARTESIAN_POINT('Ctrl Pts',(3.59116331899994,5.2,1.79143100999998));
#343025=CARTESIAN_POINT('Ctrl Pts',(3.59116331899994,2.2,1.79143100999998));
#343026=CARTESIAN_POINT('Ctrl Pts',(3.59068757599994,12.2,1.79124934399999));
#343027=CARTESIAN_POINT('Ctrl Pts',(3.59068757599994,5.2,1.79124934399999));
#343028=CARTESIAN_POINT('Ctrl Pts',(3.59068757599994,2.2,1.79124934399999));
#343029=CARTESIAN_POINT('Ctrl Pts',(3.59021802899994,12.2,1.79106934699998));
#343030=CARTESIAN_POINT('Ctrl Pts',(3.59021802899994,5.2,1.79106934699998));
#343031=CARTESIAN_POINT('Ctrl Pts',(3.59021802899994,2.2,1.79106934699998));
#343032=CARTESIAN_POINT('Ctrl Pts',(3.58975468999994,12.2,1.79089103799999));
#343033=CARTESIAN_POINT('Ctrl Pts',(3.58975468999994,5.2,1.79089103799999));
#343034=CARTESIAN_POINT('Ctrl Pts',(3.58975468999994,2.2,1.79089103799999));
#343035=CARTESIAN_POINT('Ctrl Pts',(3.58929756199994,12.2,1.79071443699999));
#343036=CARTESIAN_POINT('Ctrl Pts',(3.58929756199994,5.2,1.79071443699999));
#343037=CARTESIAN_POINT('Ctrl Pts',(3.58929756199994,2.2,1.79071443699999));
#343038=CARTESIAN_POINT('Ctrl Pts',(3.58884665299994,12.2,1.79053956299999));
#343039=CARTESIAN_POINT('Ctrl Pts',(3.58884665299994,5.2,1.79053956299999));
#343040=CARTESIAN_POINT('Ctrl Pts',(3.58884665299994,2.2,1.79053956299999));
#343041=CARTESIAN_POINT('Ctrl Pts',(3.58840196999994,12.2,1.79036643899999));
#343042=CARTESIAN_POINT('Ctrl Pts',(3.58840196999994,5.2,1.79036643899999));
#343043=CARTESIAN_POINT('Ctrl Pts',(3.58840196999994,2.2,1.79036643899999));
#343044=CARTESIAN_POINT('Ctrl Pts',(3.58796351999994,12.2,1.79019508399998));
#343045=CARTESIAN_POINT('Ctrl Pts',(3.58796351999994,5.2,1.79019508399998));
#343046=CARTESIAN_POINT('Ctrl Pts',(3.58796351999994,2.2,1.79019508399998));
#343047=CARTESIAN_POINT('Ctrl Pts',(3.58753130999994,12.2,1.79002551699998));
#343048=CARTESIAN_POINT('Ctrl Pts',(3.58753130999994,5.2,1.79002551699998));
#343049=CARTESIAN_POINT('Ctrl Pts',(3.58753130999994,2.2,1.79002551699998));
#343050=CARTESIAN_POINT('Ctrl Pts',(3.58710534699994,12.2,1.78985775999998));
#343051=CARTESIAN_POINT('Ctrl Pts',(3.58710534699994,5.2,1.78985775999998));
#343052=CARTESIAN_POINT('Ctrl Pts',(3.58710534699994,2.2,1.78985775999998));
#343053=CARTESIAN_POINT('Ctrl Pts',(3.58668563699994,12.2,1.78969183199999));
#343054=CARTESIAN_POINT('Ctrl Pts',(3.58668563699994,5.2,1.78969183199999));
#343055=CARTESIAN_POINT('Ctrl Pts',(3.58668563699994,2.2,1.78969183199999));
#343056=CARTESIAN_POINT('Ctrl Pts',(3.58627218799994,12.2,1.78952775499999));
#343057=CARTESIAN_POINT('Ctrl Pts',(3.58627218799994,5.2,1.78952775499999));
#343058=CARTESIAN_POINT('Ctrl Pts',(3.58627218799994,2.2,1.78952775499999));
#343059=CARTESIAN_POINT('Ctrl Pts',(3.58586500599994,12.2,1.78936554899999));
#343060=CARTESIAN_POINT('Ctrl Pts',(3.58586500599994,5.2,1.78936554899999));
#343061=CARTESIAN_POINT('Ctrl Pts',(3.58586500599994,2.2,1.78936554899999));
#343062=CARTESIAN_POINT('Ctrl Pts',(3.58546409799994,12.2,1.78920523399999));
#343063=CARTESIAN_POINT('Ctrl Pts',(3.58546409799994,5.2,1.78920523399999));
#343064=CARTESIAN_POINT('Ctrl Pts',(3.58546409799994,2.2,1.78920523399999));
#343065=CARTESIAN_POINT('Ctrl Pts',(3.58506947199994,12.2,1.78904683199999));
#343066=CARTESIAN_POINT('Ctrl Pts',(3.58506947199994,5.2,1.78904683199999));
#343067=CARTESIAN_POINT('Ctrl Pts',(3.58506947199994,2.2,1.78904683199999));
#343068=CARTESIAN_POINT('Ctrl Pts',(3.58468113399994,12.2,1.78889036299998));
#343069=CARTESIAN_POINT('Ctrl Pts',(3.58468113399994,5.2,1.78889036299998));
#343070=CARTESIAN_POINT('Ctrl Pts',(3.58468113399994,2.2,1.78889036299998));
#343071=CARTESIAN_POINT('Ctrl Pts',(3.58429908999994,12.2,1.78873584799998));
#343072=CARTESIAN_POINT('Ctrl Pts',(3.58429908999994,5.2,1.78873584799998));
#343073=CARTESIAN_POINT('Ctrl Pts',(3.58429908999994,2.2,1.78873584799998));
#343074=CARTESIAN_POINT('Ctrl Pts',(3.58392334799994,12.2,1.78858330799998));
#343075=CARTESIAN_POINT('Ctrl Pts',(3.58392334799994,5.2,1.78858330799998));
#343076=CARTESIAN_POINT('Ctrl Pts',(3.58392334799994,2.2,1.78858330799998));
#343077=CARTESIAN_POINT('Ctrl Pts',(3.58355391499994,12.2,1.78843276399999));
#343078=CARTESIAN_POINT('Ctrl Pts',(3.58355391499994,5.2,1.78843276399999));
#343079=CARTESIAN_POINT('Ctrl Pts',(3.58355391499994,2.2,1.78843276399999));
#343080=CARTESIAN_POINT('Ctrl Pts',(3.58319079699994,12.2,1.78828423699999));
#343081=CARTESIAN_POINT('Ctrl Pts',(3.58319079699994,5.2,1.78828423699999));
#343082=CARTESIAN_POINT('Ctrl Pts',(3.58319079699994,2.2,1.78828423699999));
#343083=CARTESIAN_POINT('Ctrl Pts',(3.58283400099995,12.2,1.78813774899998));
#343084=CARTESIAN_POINT('Ctrl Pts',(3.58283400099995,5.2,1.78813774899998));
#343085=CARTESIAN_POINT('Ctrl Pts',(3.58283400099995,2.2,1.78813774899998));
#343086=CARTESIAN_POINT('Ctrl Pts',(3.58248353499994,12.2,1.78799332099999));
#343087=CARTESIAN_POINT('Ctrl Pts',(3.58248353499994,5.2,1.78799332099999));
#343088=CARTESIAN_POINT('Ctrl Pts',(3.58248353499994,2.2,1.78799332099999));
#343089=CARTESIAN_POINT('Ctrl Pts',(3.58213940499994,12.2,1.78785097299999));
#343090=CARTESIAN_POINT('Ctrl Pts',(3.58213940499994,5.2,1.78785097299999));
#343091=CARTESIAN_POINT('Ctrl Pts',(3.58213940499994,2.2,1.78785097299999));
#343092=CARTESIAN_POINT('Ctrl Pts',(3.58180161799994,12.2,1.78771072799998));
#343093=CARTESIAN_POINT('Ctrl Pts',(3.58180161799994,5.2,1.78771072799998));
#343094=CARTESIAN_POINT('Ctrl Pts',(3.58180161799994,2.2,1.78771072799998));
#343095=CARTESIAN_POINT('Ctrl Pts',(3.58147017999995,12.2,1.78757260699999));
#343096=CARTESIAN_POINT('Ctrl Pts',(3.58147017999995,5.2,1.78757260699999));
#343097=CARTESIAN_POINT('Ctrl Pts',(3.58147017999995,2.2,1.78757260699999));
#343098=CARTESIAN_POINT('Ctrl Pts',(3.58114509999994,12.2,1.78743663099999));
#343099=CARTESIAN_POINT('Ctrl Pts',(3.58114509999994,5.2,1.78743663099999));
#343100=CARTESIAN_POINT('Ctrl Pts',(3.58114509999994,2.2,1.78743663099999));
#343101=CARTESIAN_POINT('Ctrl Pts',(3.58082638199994,12.2,1.78730282199998));
#343102=CARTESIAN_POINT('Ctrl Pts',(3.58082638199994,5.2,1.78730282199998));
#343103=CARTESIAN_POINT('Ctrl Pts',(3.58082638199994,2.2,1.78730282199998));
#343104=CARTESIAN_POINT('Ctrl Pts',(3.58051403599994,12.2,1.78717120299998));
#343105=CARTESIAN_POINT('Ctrl Pts',(3.58051403599994,5.2,1.78717120299998));
#343106=CARTESIAN_POINT('Ctrl Pts',(3.58051403599994,2.2,1.78717120299998));
#343107=CARTESIAN_POINT('Ctrl Pts',(3.58020806599994,12.2,1.78704179399999));
#343108=CARTESIAN_POINT('Ctrl Pts',(3.58020806599994,5.2,1.78704179399999));
#343109=CARTESIAN_POINT('Ctrl Pts',(3.58020806599994,2.2,1.78704179399999));
#343110=CARTESIAN_POINT('Ctrl Pts',(3.57990847899994,12.2,1.78691461799998));
#343111=CARTESIAN_POINT('Ctrl Pts',(3.57990847899994,5.2,1.78691461799998));
#343112=CARTESIAN_POINT('Ctrl Pts',(3.57990847899994,2.2,1.78691461799998));
#343113=CARTESIAN_POINT('Ctrl Pts',(3.57961528499994,12.2,1.78678969699999));
#343114=CARTESIAN_POINT('Ctrl Pts',(3.57961528499994,5.2,1.78678969699999));
#343115=CARTESIAN_POINT('Ctrl Pts',(3.57961528499994,2.2,1.78678969699999));
#343116=CARTESIAN_POINT('Ctrl Pts',(3.57932848799994,12.2,1.78666705199999));
#343117=CARTESIAN_POINT('Ctrl Pts',(3.57932848799994,5.2,1.78666705199999));
#343118=CARTESIAN_POINT('Ctrl Pts',(3.57932848799994,2.2,1.78666705199999));
#343119=CARTESIAN_POINT('Ctrl Pts',(3.57904809599995,12.2,1.78654670699999));
#343120=CARTESIAN_POINT('Ctrl Pts',(3.57904809599995,5.2,1.78654670699999));
#343121=CARTESIAN_POINT('Ctrl Pts',(3.57904809599995,2.2,1.78654670699999));
#343122=CARTESIAN_POINT('Ctrl Pts',(3.57877411399994,12.2,1.78642868299999));
#343123=CARTESIAN_POINT('Ctrl Pts',(3.57877411399994,5.2,1.78642868299999));
#343124=CARTESIAN_POINT('Ctrl Pts',(3.57877411399994,2.2,1.78642868299999));
#343125=CARTESIAN_POINT('Ctrl Pts',(3.57850655199994,12.2,1.78631300199998));
#343126=CARTESIAN_POINT('Ctrl Pts',(3.57850655199994,5.2,1.78631300199998));
#343127=CARTESIAN_POINT('Ctrl Pts',(3.57850655199994,2.2,1.78631300199998));
#343128=CARTESIAN_POINT('Ctrl Pts',(3.57824541399994,12.2,1.78619968699998));
#343129=CARTESIAN_POINT('Ctrl Pts',(3.57824541399994,5.2,1.78619968699998));
#343130=CARTESIAN_POINT('Ctrl Pts',(3.57824541399994,2.2,1.78619968699998));
#343131=CARTESIAN_POINT('Ctrl Pts',(3.57799070899994,12.2,1.78608875999998));
#343132=CARTESIAN_POINT('Ctrl Pts',(3.57799070899994,5.2,1.78608875999998));
#343133=CARTESIAN_POINT('Ctrl Pts',(3.57799070899994,2.2,1.78608875999998));
#343134=CARTESIAN_POINT('Ctrl Pts',(3.57774244199994,12.2,1.78598024399999));
#343135=CARTESIAN_POINT('Ctrl Pts',(3.57774244199994,5.2,1.78598024399999));
#343136=CARTESIAN_POINT('Ctrl Pts',(3.57774244199994,2.2,1.78598024399999));
#343137=CARTESIAN_POINT('Ctrl Pts',(3.57750061999994,12.2,1.78587416299999));
#343138=CARTESIAN_POINT('Ctrl Pts',(3.57750061999994,5.2,1.78587416299999));
#343139=CARTESIAN_POINT('Ctrl Pts',(3.57750061999994,2.2,1.78587416299999));
#343140=CARTESIAN_POINT('Ctrl Pts',(3.57726525199995,12.2,1.78577053699998));
#343141=CARTESIAN_POINT('Ctrl Pts',(3.57726525199995,5.2,1.78577053699998));
#343142=CARTESIAN_POINT('Ctrl Pts',(3.57726525199995,2.2,1.78577053699998));
#343143=CARTESIAN_POINT('Ctrl Pts',(3.57703634199994,12.2,1.78566938999999));
#343144=CARTESIAN_POINT('Ctrl Pts',(3.57703634199994,5.2,1.78566938999999));
#343145=CARTESIAN_POINT('Ctrl Pts',(3.57703634199994,2.2,1.78566938999999));
#343146=CARTESIAN_POINT('Ctrl Pts',(3.57681389999994,12.2,1.78557074599999));
#343147=CARTESIAN_POINT('Ctrl Pts',(3.57681389999994,5.2,1.78557074599999));
#343148=CARTESIAN_POINT('Ctrl Pts',(3.57681389999994,2.2,1.78557074599999));
#343149=CARTESIAN_POINT('Ctrl Pts',(3.57659792899994,12.2,1.78547462699999));
#343150=CARTESIAN_POINT('Ctrl Pts',(3.57659792899994,5.2,1.78547462699999));
#343151=CARTESIAN_POINT('Ctrl Pts',(3.57659792899994,2.2,1.78547462699999));
#343152=CARTESIAN_POINT('Ctrl Pts',(3.57638843899994,12.2,1.78538105599999));
#343153=CARTESIAN_POINT('Ctrl Pts',(3.57638843899994,5.2,1.78538105599999));
#343154=CARTESIAN_POINT('Ctrl Pts',(3.57638843899994,2.2,1.78538105599999));
#343155=CARTESIAN_POINT('Ctrl Pts',(3.57618543499994,12.2,1.78529005699998));
#343156=CARTESIAN_POINT('Ctrl Pts',(3.57618543499994,5.2,1.78529005699998));
#343157=CARTESIAN_POINT('Ctrl Pts',(3.57618543499994,2.2,1.78529005699998));
#343158=CARTESIAN_POINT('Ctrl Pts',(3.57598892399994,12.2,1.78520165199998));
#343159=CARTESIAN_POINT('Ctrl Pts',(3.57598892399994,5.2,1.78520165199998));
#343160=CARTESIAN_POINT('Ctrl Pts',(3.57598892399994,2.2,1.78520165199998));
#343161=CARTESIAN_POINT('Ctrl Pts',(3.57579891299994,12.2,1.78511586499999));
#343162=CARTESIAN_POINT('Ctrl Pts',(3.57579891299994,5.2,1.78511586499999));
#343163=CARTESIAN_POINT('Ctrl Pts',(3.57579891299994,2.2,1.78511586499999));
#343164=CARTESIAN_POINT('Ctrl Pts',(3.57561540999995,12.2,1.78503271999999));
#343165=CARTESIAN_POINT('Ctrl Pts',(3.57561540999995,5.2,1.78503271999999));
#343166=CARTESIAN_POINT('Ctrl Pts',(3.57561540999995,2.2,1.78503271999999));
#343167=CARTESIAN_POINT('Ctrl Pts',(3.57543842099994,12.2,1.78495223999999));
#343168=CARTESIAN_POINT('Ctrl Pts',(3.57543842099994,5.2,1.78495223999999));
#343169=CARTESIAN_POINT('Ctrl Pts',(3.57543842099994,2.2,1.78495223999999));
#343170=CARTESIAN_POINT('Ctrl Pts',(3.57526795299994,12.2,1.78487444899998));
#343171=CARTESIAN_POINT('Ctrl Pts',(3.57526795299994,5.2,1.78487444899998));
#343172=CARTESIAN_POINT('Ctrl Pts',(3.57526795299994,2.2,1.78487444899998));
#343173=CARTESIAN_POINT('Ctrl Pts',(3.57510401099994,12.2,1.78479937099999));
#343174=CARTESIAN_POINT('Ctrl Pts',(3.57510401099994,5.2,1.78479937099999));
#343175=CARTESIAN_POINT('Ctrl Pts',(3.57510401099994,2.2,1.78479937099999));
#343176=CARTESIAN_POINT('Ctrl Pts',(3.57494660499994,12.2,1.78472702899999));
#343177=CARTESIAN_POINT('Ctrl Pts',(3.57494660499994,5.2,1.78472702899999));
#343178=CARTESIAN_POINT('Ctrl Pts',(3.57494660499994,2.2,1.78472702899999));
#343179=CARTESIAN_POINT('Ctrl Pts',(3.57479573999994,12.2,1.78465744599999));
#343180=CARTESIAN_POINT('Ctrl Pts',(3.57479573999994,5.2,1.78465744599999));
#343181=CARTESIAN_POINT('Ctrl Pts',(3.57479573999994,2.2,1.78465744599999));
#343182=CARTESIAN_POINT('Ctrl Pts',(3.57465142099994,12.2,1.78459064599998));
#343183=CARTESIAN_POINT('Ctrl Pts',(3.57465142099994,5.2,1.78459064599998));
#343184=CARTESIAN_POINT('Ctrl Pts',(3.57465142099994,2.2,1.78459064599998));
#343185=CARTESIAN_POINT('Ctrl Pts',(3.57451365799994,12.2,1.78452665399998));
#343186=CARTESIAN_POINT('Ctrl Pts',(3.57451365799994,5.2,1.78452665399998));
#343187=CARTESIAN_POINT('Ctrl Pts',(3.57451365799994,2.2,1.78452665399998));
#343188=CARTESIAN_POINT('Ctrl Pts',(3.57438245599994,12.2,1.78446549499998));
#343189=CARTESIAN_POINT('Ctrl Pts',(3.57438245599994,5.2,1.78446549499998));
#343190=CARTESIAN_POINT('Ctrl Pts',(3.57438245599994,2.2,1.78446549499998));
#343191=CARTESIAN_POINT('Ctrl Pts',(3.57425782399994,12.2,1.78440719399998));
#343192=CARTESIAN_POINT('Ctrl Pts',(3.57425782399994,5.2,1.78440719399998));
#343193=CARTESIAN_POINT('Ctrl Pts',(3.57425782399994,2.2,1.78440719399998));
#343194=CARTESIAN_POINT('Ctrl Pts',(3.57413976699994,12.2,1.78435177699999));
#343195=CARTESIAN_POINT('Ctrl Pts',(3.57413976699994,5.2,1.78435177699999));
#343196=CARTESIAN_POINT('Ctrl Pts',(3.57413976699994,2.2,1.78435177699999));
#343197=CARTESIAN_POINT('Ctrl Pts',(3.57402829299994,12.2,1.78429926699998));
#343198=CARTESIAN_POINT('Ctrl Pts',(3.57402829299994,5.2,1.78429926699998));
#343199=CARTESIAN_POINT('Ctrl Pts',(3.57402829299994,2.2,1.78429926699998));
#343200=CARTESIAN_POINT('Ctrl Pts',(3.57392340599994,12.2,1.78424968799999));
#343201=CARTESIAN_POINT('Ctrl Pts',(3.57392340599994,5.2,1.78424968799999));
#343202=CARTESIAN_POINT('Ctrl Pts',(3.57392340599994,2.2,1.78424968799999));
#343203=CARTESIAN_POINT('Ctrl Pts',(3.57382511499994,12.2,1.78420305899999));
#343204=CARTESIAN_POINT('Ctrl Pts',(3.57382511499994,5.2,1.78420305899999));
#343205=CARTESIAN_POINT('Ctrl Pts',(3.57382511499994,2.2,1.78420305899999));
#343206=CARTESIAN_POINT('Ctrl Pts',(3.57373342599994,12.2,1.78415940499999));
#343207=CARTESIAN_POINT('Ctrl Pts',(3.57373342599994,5.2,1.78415940499999));
#343208=CARTESIAN_POINT('Ctrl Pts',(3.57373342599994,2.2,1.78415940499999));
#343209=CARTESIAN_POINT('Ctrl Pts',(3.57364834299994,12.2,1.78411874999998));
#343210=CARTESIAN_POINT('Ctrl Pts',(3.57364834299994,5.2,1.78411874999998));
#343211=CARTESIAN_POINT('Ctrl Pts',(3.57364834299994,2.2,1.78411874999998));
#343212=CARTESIAN_POINT('Ctrl Pts',(3.57356987599994,12.2,1.78408112399998));
#343213=CARTESIAN_POINT('Ctrl Pts',(3.57356987599994,5.2,1.78408112399998));
#343214=CARTESIAN_POINT('Ctrl Pts',(3.57356987599994,2.2,1.78408112399998));
#343215=CARTESIAN_POINT('Ctrl Pts',(3.57349803399994,12.2,1.78404655699998));
#343216=CARTESIAN_POINT('Ctrl Pts',(3.57349803399994,5.2,1.78404655699998));
#343217=CARTESIAN_POINT('Ctrl Pts',(3.57349803399994,2.2,1.78404655699998));
#343218=CARTESIAN_POINT('Ctrl Pts',(3.57343282299994,12.2,1.78401508199999));
#343219=CARTESIAN_POINT('Ctrl Pts',(3.57343282299994,5.2,1.78401508199999));
#343220=CARTESIAN_POINT('Ctrl Pts',(3.57343282299994,2.2,1.78401508199999));
#343221=CARTESIAN_POINT('Ctrl Pts',(3.57337425399994,12.2,1.78398672599998));
#343222=CARTESIAN_POINT('Ctrl Pts',(3.57337425399994,5.2,1.78398672599998));
#343223=CARTESIAN_POINT('Ctrl Pts',(3.57337425399994,2.2,1.78398672599998));
#343224=CARTESIAN_POINT('Ctrl Pts',(3.57332232999994,12.2,1.78396150999999));
#343225=CARTESIAN_POINT('Ctrl Pts',(3.57332232999994,5.2,1.78396150999999));
#343226=CARTESIAN_POINT('Ctrl Pts',(3.57332232999994,2.2,1.78396150999999));
#343227=CARTESIAN_POINT('Ctrl Pts',(3.57327705499995,12.2,1.78393944699998));
#343228=CARTESIAN_POINT('Ctrl Pts',(3.57327705499995,5.2,1.78393944699998));
#343229=CARTESIAN_POINT('Ctrl Pts',(3.57327705499995,2.2,1.78393944699998));
#343230=CARTESIAN_POINT('Ctrl Pts',(3.57324615599994,12.2,1.78392432099999));
#343231=CARTESIAN_POINT('Ctrl Pts',(3.57324615599994,5.2,1.78392432099999));
#343232=CARTESIAN_POINT('Ctrl Pts',(3.57324615599994,2.2,1.78392432099999));
#343233=CARTESIAN_POINT('Ctrl Pts',(3.57322597299994,12.2,1.78391439999999));
#343234=CARTESIAN_POINT('Ctrl Pts',(3.57322597299994,5.2,1.78391439999999));
#343235=CARTESIAN_POINT('Ctrl Pts',(3.57322597299994,2.2,1.78391439999999));
#343236=CARTESIAN_POINT('Ctrl Pts',(3.57321384899994,12.2,1.78390841799999));
#343237=CARTESIAN_POINT('Ctrl Pts',(3.57321384899994,5.2,1.78390841799999));
#343238=CARTESIAN_POINT('Ctrl Pts',(3.57321384899994,2.2,1.78390841799999));
#343239=CARTESIAN_POINT('Ctrl Pts',(3.57320811899994,12.2,1.78390558399999));
#343240=CARTESIAN_POINT('Ctrl Pts',(3.57320811899994,5.2,1.78390558399999));
#343241=CARTESIAN_POINT('Ctrl Pts',(3.57320811899994,2.2,1.78390558399999));
#343242=CARTESIAN_POINT('',(4.39111701799995,12.2,1.81124027399999));
#343243=CARTESIAN_POINT('Origin',(-5.66300478732629E-14,15.2,-1.77635683940025E-14));
#343244=CARTESIAN_POINT('',(4.50847758599994,12.2,1.49536946999998));
#343245=CARTESIAN_POINT('Ctrl Pts',(3.87111406899994,12.2,0.982007125999989));
#343246=CARTESIAN_POINT('Ctrl Pts',(3.87111406899994,5.2,0.982007125999989));
#343247=CARTESIAN_POINT('Ctrl Pts',(3.87111406899994,2.2,0.982007125999989));
#343248=CARTESIAN_POINT('Ctrl Pts',(3.87112069459513,12.2,0.98200883489564));
#343249=CARTESIAN_POINT('Ctrl Pts',(3.87112069459513,5.2,0.98200883489564));
#343250=CARTESIAN_POINT('Ctrl Pts',(3.87112069459513,2.2,0.98200883489564));
#343251=CARTESIAN_POINT('Ctrl Pts',(3.87113351057882,12.2,0.982012138502726));
#343252=CARTESIAN_POINT('Ctrl Pts',(3.87113351057882,5.2,0.982012138502726));
#343253=CARTESIAN_POINT('Ctrl Pts',(3.87113351057882,2.2,0.982012138502726));
#343254=CARTESIAN_POINT('Ctrl Pts',(3.8711525108998,12.2,0.982017032143299));
#343255=CARTESIAN_POINT('Ctrl Pts',(3.8711525108998,5.2,0.982017032143299));
#343256=CARTESIAN_POINT('Ctrl Pts',(3.8711525108998,2.2,0.982017032143299));
#343257=CARTESIAN_POINT('Ctrl Pts',(3.87117775167996,12.2,0.982023550844282));
#343258=CARTESIAN_POINT('Ctrl Pts',(3.87117775167996,5.2,0.982023550844282));
#343259=CARTESIAN_POINT('Ctrl Pts',(3.87117775167996,2.2,0.982023550844282));
#343260=CARTESIAN_POINT('Ctrl Pts',(3.87122151999994,12.2,0.982035030999988));
#343261=CARTESIAN_POINT('Ctrl Pts',(3.87122151999994,5.2,0.982035030999988));
#343262=CARTESIAN_POINT('Ctrl Pts',(3.87122151999994,2.2,0.982035030999988));
#343263=CARTESIAN_POINT('Ctrl Pts',(3.87127021899994,12.2,0.982047882999986));
#343264=CARTESIAN_POINT('Ctrl Pts',(3.87127021899994,5.2,0.982047882999986));
#343265=CARTESIAN_POINT('Ctrl Pts',(3.87127021899994,2.2,0.982047882999986));
#343266=CARTESIAN_POINT('Ctrl Pts',(3.87132600999994,12.2,0.982062687999985));
#343267=CARTESIAN_POINT('Ctrl Pts',(3.87132600999994,5.2,0.982062687999985));
#343268=CARTESIAN_POINT('Ctrl Pts',(3.87132600999994,2.2,0.982062687999985));
#343269=CARTESIAN_POINT('Ctrl Pts',(3.87138888599994,12.2,0.982079453999987));
#343270=CARTESIAN_POINT('Ctrl Pts',(3.87138888599994,5.2,0.982079453999987));
#343271=CARTESIAN_POINT('Ctrl Pts',(3.87138888599994,2.2,0.982079453999987));
#343272=CARTESIAN_POINT('Ctrl Pts',(3.87145882699994,12.2,0.982098194999987));
#343273=CARTESIAN_POINT('Ctrl Pts',(3.87145882699994,5.2,0.982098194999987));
#343274=CARTESIAN_POINT('Ctrl Pts',(3.87145882699994,2.2,0.982098194999987));
#343275=CARTESIAN_POINT('Ctrl Pts',(3.87153580999994,12.2,0.982118923999984));
#343276=CARTESIAN_POINT('Ctrl Pts',(3.87153580999994,5.2,0.982118923999984));
#343277=CARTESIAN_POINT('Ctrl Pts',(3.87153580999994,2.2,0.982118923999984));
#343278=CARTESIAN_POINT('Ctrl Pts',(3.87161980999994,12.2,0.982141659999982));
#343279=CARTESIAN_POINT('Ctrl Pts',(3.87161980999994,5.2,0.982141659999982));
#343280=CARTESIAN_POINT('Ctrl Pts',(3.87161980999994,2.2,0.982141659999982));
#343281=CARTESIAN_POINT('Ctrl Pts',(3.87171079599994,12.2,0.982166423999988));
#343282=CARTESIAN_POINT('Ctrl Pts',(3.87171079599994,5.2,0.982166423999988));
#343283=CARTESIAN_POINT('Ctrl Pts',(3.87171079599994,2.2,0.982166423999988));
#343284=CARTESIAN_POINT('Ctrl Pts',(3.87180874699994,12.2,0.982193229999986));
#343285=CARTESIAN_POINT('Ctrl Pts',(3.87180874699994,5.2,0.982193229999986));
#343286=CARTESIAN_POINT('Ctrl Pts',(3.87180874699994,2.2,0.982193229999986));
#343287=CARTESIAN_POINT('Ctrl Pts',(3.87191363799994,12.2,0.982222092999985));
#343288=CARTESIAN_POINT('Ctrl Pts',(3.87191363799994,5.2,0.982222092999985));
#343289=CARTESIAN_POINT('Ctrl Pts',(3.87191363799994,2.2,0.982222092999985));
#343290=CARTESIAN_POINT('Ctrl Pts',(3.87202545199994,12.2,0.982253026999986));
#343291=CARTESIAN_POINT('Ctrl Pts',(3.87202545199994,5.2,0.982253026999986));
#343292=CARTESIAN_POINT('Ctrl Pts',(3.87202545199994,2.2,0.982253026999986));
#343293=CARTESIAN_POINT('Ctrl Pts',(3.87214416899994,12.2,0.982286043999987));
#343294=CARTESIAN_POINT('Ctrl Pts',(3.87214416899994,5.2,0.982286043999987));
#343295=CARTESIAN_POINT('Ctrl Pts',(3.87214416899994,2.2,0.982286043999987));
#343296=CARTESIAN_POINT('Ctrl Pts',(3.87226976899994,12.2,0.982321156999983));
#343297=CARTESIAN_POINT('Ctrl Pts',(3.87226976899994,5.2,0.982321156999983));
#343298=CARTESIAN_POINT('Ctrl Pts',(3.87226976899994,2.2,0.982321156999983));
#343299=CARTESIAN_POINT('Ctrl Pts',(3.87240223399994,12.2,0.982358379999986));
#343300=CARTESIAN_POINT('Ctrl Pts',(3.87240223399994,5.2,0.982358379999986));
#343301=CARTESIAN_POINT('Ctrl Pts',(3.87240223399994,2.2,0.982358379999986));
#343302=CARTESIAN_POINT('Ctrl Pts',(3.87254153999994,12.2,0.982397726999986));
#343303=CARTESIAN_POINT('Ctrl Pts',(3.87254153999994,5.2,0.982397726999986));
#343304=CARTESIAN_POINT('Ctrl Pts',(3.87254153999994,2.2,0.982397726999986));
#343305=CARTESIAN_POINT('Ctrl Pts',(3.87268766499994,12.2,0.982439212999986));
#343306=CARTESIAN_POINT('Ctrl Pts',(3.87268766499994,5.2,0.982439212999986));
#343307=CARTESIAN_POINT('Ctrl Pts',(3.87268766499994,2.2,0.982439212999986));
#343308=CARTESIAN_POINT('Ctrl Pts',(3.87284058799994,12.2,0.982482850999986));
#343309=CARTESIAN_POINT('Ctrl Pts',(3.87284058799994,5.2,0.982482850999986));
#343310=CARTESIAN_POINT('Ctrl Pts',(3.87284058799994,2.2,0.982482850999986));
#343311=CARTESIAN_POINT('Ctrl Pts',(3.87300028899995,12.2,0.982528657999988));
#343312=CARTESIAN_POINT('Ctrl Pts',(3.87300028899995,5.2,0.982528657999988));
#343313=CARTESIAN_POINT('Ctrl Pts',(3.87300028899995,2.2,0.982528657999988));
#343314=CARTESIAN_POINT('Ctrl Pts',(3.87316674399994,12.2,0.982576645999984));
#343315=CARTESIAN_POINT('Ctrl Pts',(3.87316674399994,5.2,0.982576645999984));
#343316=CARTESIAN_POINT('Ctrl Pts',(3.87316674399994,2.2,0.982576645999984));
#343317=CARTESIAN_POINT('Ctrl Pts',(3.87333993499994,12.2,0.982626826999984));
#343318=CARTESIAN_POINT('Ctrl Pts',(3.87333993499994,5.2,0.982626826999984));
#343319=CARTESIAN_POINT('Ctrl Pts',(3.87333993499994,2.2,0.982626826999984));
#343320=CARTESIAN_POINT('Ctrl Pts',(3.87351984099995,12.2,0.982679216999984));
#343321=CARTESIAN_POINT('Ctrl Pts',(3.87351984099995,5.2,0.982679216999984));
#343322=CARTESIAN_POINT('Ctrl Pts',(3.87351984099995,2.2,0.982679216999984));
#343323=CARTESIAN_POINT('Ctrl Pts',(3.87370644199994,12.2,0.982733826999986));
#343324=CARTESIAN_POINT('Ctrl Pts',(3.87370644199994,5.2,0.982733826999986));
#343325=CARTESIAN_POINT('Ctrl Pts',(3.87370644199994,2.2,0.982733826999986));
#343326=CARTESIAN_POINT('Ctrl Pts',(3.87389971699994,12.2,0.982790672999982));
#343327=CARTESIAN_POINT('Ctrl Pts',(3.87389971699994,5.2,0.982790672999982));
#343328=CARTESIAN_POINT('Ctrl Pts',(3.87389971699994,2.2,0.982790672999982));
#343329=CARTESIAN_POINT('Ctrl Pts',(3.87409964499994,12.2,0.982849765999987));
#343330=CARTESIAN_POINT('Ctrl Pts',(3.87409964499994,5.2,0.982849765999987));
#343331=CARTESIAN_POINT('Ctrl Pts',(3.87409964499994,2.2,0.982849765999987));
#343332=CARTESIAN_POINT('Ctrl Pts',(3.87430620599994,12.2,0.982911120999983));
#343333=CARTESIAN_POINT('Ctrl Pts',(3.87430620599994,5.2,0.982911120999983));
#343334=CARTESIAN_POINT('Ctrl Pts',(3.87430620599994,2.2,0.982911120999983));
#343335=CARTESIAN_POINT('Ctrl Pts',(3.87451937999994,12.2,0.982974749999985));
#343336=CARTESIAN_POINT('Ctrl Pts',(3.87451937999994,5.2,0.982974749999985));
#343337=CARTESIAN_POINT('Ctrl Pts',(3.87451937999994,2.2,0.982974749999985));
#343338=CARTESIAN_POINT('Ctrl Pts',(3.87473914399994,12.2,0.983040666999986));
#343339=CARTESIAN_POINT('Ctrl Pts',(3.87473914399994,5.2,0.983040666999986));
#343340=CARTESIAN_POINT('Ctrl Pts',(3.87473914399994,2.2,0.983040666999986));
#343341=CARTESIAN_POINT('Ctrl Pts',(3.87496548099994,12.2,0.983108885999986));
#343342=CARTESIAN_POINT('Ctrl Pts',(3.87496548099994,5.2,0.983108885999986));
#343343=CARTESIAN_POINT('Ctrl Pts',(3.87496548099994,2.2,0.983108885999986));
#343344=CARTESIAN_POINT('Ctrl Pts',(3.87519836899994,12.2,0.983179417999986));
#343345=CARTESIAN_POINT('Ctrl Pts',(3.87519836899994,5.2,0.983179417999986));
#343346=CARTESIAN_POINT('Ctrl Pts',(3.87519836899994,2.2,0.983179417999986));
#343347=CARTESIAN_POINT('Ctrl Pts',(3.87543778799994,12.2,0.983252276999984));
#343348=CARTESIAN_POINT('Ctrl Pts',(3.87543778799994,5.2,0.983252276999984));
#343349=CARTESIAN_POINT('Ctrl Pts',(3.87543778799994,2.2,0.983252276999984));
#343350=CARTESIAN_POINT('Ctrl Pts',(3.87568371899994,12.2,0.983327476999989));
#343351=CARTESIAN_POINT('Ctrl Pts',(3.87568371899994,5.2,0.983327476999989));
#343352=CARTESIAN_POINT('Ctrl Pts',(3.87568371899994,2.2,0.983327476999989));
#343353=CARTESIAN_POINT('Ctrl Pts',(3.87593613999994,12.2,0.983405027999984));
#343354=CARTESIAN_POINT('Ctrl Pts',(3.87593613999994,5.2,0.983405027999984));
#343355=CARTESIAN_POINT('Ctrl Pts',(3.87593613999994,2.2,0.983405027999984));
#343356=CARTESIAN_POINT('Ctrl Pts',(3.87619503199994,12.2,0.983484946999984));
#343357=CARTESIAN_POINT('Ctrl Pts',(3.87619503199994,5.2,0.983484946999984));
#343358=CARTESIAN_POINT('Ctrl Pts',(3.87619503199994,2.2,0.983484946999984));
#343359=CARTESIAN_POINT('Ctrl Pts',(3.87646037599994,12.2,0.983567240999985));
#343360=CARTESIAN_POINT('Ctrl Pts',(3.87646037599994,5.2,0.983567240999985));
#343361=CARTESIAN_POINT('Ctrl Pts',(3.87646037599994,2.2,0.983567240999985));
#343362=CARTESIAN_POINT('Ctrl Pts',(3.87673214999994,12.2,0.983651927999984));
#343363=CARTESIAN_POINT('Ctrl Pts',(3.87673214999994,5.2,0.983651927999984));
#343364=CARTESIAN_POINT('Ctrl Pts',(3.87673214999994,2.2,0.983651927999984));
#343365=CARTESIAN_POINT('Ctrl Pts',(3.87701033499994,12.2,0.983739017999987));
#343366=CARTESIAN_POINT('Ctrl Pts',(3.87701033499994,5.2,0.983739017999987));
#343367=CARTESIAN_POINT('Ctrl Pts',(3.87701033499994,2.2,0.983739017999987));
#343368=CARTESIAN_POINT('Ctrl Pts',(3.87729491299994,12.2,0.983828522999985));
#343369=CARTESIAN_POINT('Ctrl Pts',(3.87729491299994,5.2,0.983828522999985));
#343370=CARTESIAN_POINT('Ctrl Pts',(3.87729491299994,2.2,0.983828522999985));
#343371=CARTESIAN_POINT('Ctrl Pts',(3.87758586199995,12.2,0.983920457999985));
#343372=CARTESIAN_POINT('Ctrl Pts',(3.87758586199995,5.2,0.983920457999985));
#343373=CARTESIAN_POINT('Ctrl Pts',(3.87758586199995,2.2,0.983920457999985));
#343374=CARTESIAN_POINT('Ctrl Pts',(3.87788316199994,12.2,0.984014831999982));
#343375=CARTESIAN_POINT('Ctrl Pts',(3.87788316199994,5.2,0.984014831999982));
#343376=CARTESIAN_POINT('Ctrl Pts',(3.87788316199994,2.2,0.984014831999982));
#343377=CARTESIAN_POINT('Ctrl Pts',(3.87818679499994,12.2,0.984111659999982));
#343378=CARTESIAN_POINT('Ctrl Pts',(3.87818679499994,5.2,0.984111659999982));
#343379=CARTESIAN_POINT('Ctrl Pts',(3.87818679499994,2.2,0.984111659999982));
#343380=CARTESIAN_POINT('Ctrl Pts',(3.87849674099995,12.2,0.984210952999987));
#343381=CARTESIAN_POINT('Ctrl Pts',(3.87849674099995,5.2,0.984210952999987));
#343382=CARTESIAN_POINT('Ctrl Pts',(3.87849674099995,2.2,0.984210952999987));
#343383=CARTESIAN_POINT('Ctrl Pts',(3.87881297899995,12.2,0.984312722999987));
#343384=CARTESIAN_POINT('Ctrl Pts',(3.87881297899995,5.2,0.984312722999987));
#343385=CARTESIAN_POINT('Ctrl Pts',(3.87881297899995,2.2,0.984312722999987));
#343386=CARTESIAN_POINT('Ctrl Pts',(3.87913549099994,12.2,0.984416982999985));
#343387=CARTESIAN_POINT('Ctrl Pts',(3.87913549099994,5.2,0.984416982999985));
#343388=CARTESIAN_POINT('Ctrl Pts',(3.87913549099994,2.2,0.984416982999985));
#343389=CARTESIAN_POINT('Ctrl Pts',(3.87946425799994,12.2,0.984523744999986));
#343390=CARTESIAN_POINT('Ctrl Pts',(3.87946425799994,5.2,0.984523744999986));
#343391=CARTESIAN_POINT('Ctrl Pts',(3.87946425799994,2.2,0.984523744999986));
#343392=CARTESIAN_POINT('Ctrl Pts',(3.87979925899994,12.2,0.984633019999985));
#343393=CARTESIAN_POINT('Ctrl Pts',(3.87979925899994,5.2,0.984633019999985));
#343394=CARTESIAN_POINT('Ctrl Pts',(3.87979925899994,2.2,0.984633019999985));
#343395=CARTESIAN_POINT('Ctrl Pts',(3.88014047599994,12.2,0.984744821999985));
#343396=CARTESIAN_POINT('Ctrl Pts',(3.88014047599994,5.2,0.984744821999985));
#343397=CARTESIAN_POINT('Ctrl Pts',(3.88014047599994,2.2,0.984744821999985));
#343398=CARTESIAN_POINT('Ctrl Pts',(3.88048788899995,12.2,0.984859158999987));
#343399=CARTESIAN_POINT('Ctrl Pts',(3.88048788899995,5.2,0.984859158999987));
#343400=CARTESIAN_POINT('Ctrl Pts',(3.88048788899995,2.2,0.984859158999987));
#343401=CARTESIAN_POINT('Ctrl Pts',(3.88084147899994,12.2,0.984976046999986));
#343402=CARTESIAN_POINT('Ctrl Pts',(3.88084147899994,5.2,0.984976046999986));
#343403=CARTESIAN_POINT('Ctrl Pts',(3.88084147899994,2.2,0.984976046999986));
#343404=CARTESIAN_POINT('Ctrl Pts',(3.88120122599994,12.2,0.985095495999988));
#343405=CARTESIAN_POINT('Ctrl Pts',(3.88120122599994,5.2,0.985095495999988));
#343406=CARTESIAN_POINT('Ctrl Pts',(3.88120122599994,2.2,0.985095495999988));
#343407=CARTESIAN_POINT('Ctrl Pts',(3.88156711199994,12.2,0.985217516999985));
#343408=CARTESIAN_POINT('Ctrl Pts',(3.88156711199994,5.2,0.985217516999985));
#343409=CARTESIAN_POINT('Ctrl Pts',(3.88156711199994,2.2,0.985217516999985));
#343410=CARTESIAN_POINT('Ctrl Pts',(3.88193911799994,12.2,0.985342121999988));
#343411=CARTESIAN_POINT('Ctrl Pts',(3.88193911799994,5.2,0.985342121999988));
#343412=CARTESIAN_POINT('Ctrl Pts',(3.88193911799994,2.2,0.985342121999988));
#343413=CARTESIAN_POINT('Ctrl Pts',(3.88231722399994,12.2,0.985469323999983));
#343414=CARTESIAN_POINT('Ctrl Pts',(3.88231722399994,5.2,0.985469323999983));
#343415=CARTESIAN_POINT('Ctrl Pts',(3.88231722399994,2.2,0.985469323999983));
#343416=CARTESIAN_POINT('Ctrl Pts',(3.88270141199994,12.2,0.985599131999986));
#343417=CARTESIAN_POINT('Ctrl Pts',(3.88270141199994,5.2,0.985599131999986));
#343418=CARTESIAN_POINT('Ctrl Pts',(3.88270141199994,2.2,0.985599131999986));
#343419=CARTESIAN_POINT('Ctrl Pts',(3.88309166199994,12.2,0.985731559999987));
#343420=CARTESIAN_POINT('Ctrl Pts',(3.88309166199994,5.2,0.985731559999987));
#343421=CARTESIAN_POINT('Ctrl Pts',(3.88309166199994,2.2,0.985731559999987));
#343422=CARTESIAN_POINT('Ctrl Pts',(3.88348795599994,12.2,0.985866618999989));
#343423=CARTESIAN_POINT('Ctrl Pts',(3.88348795599994,5.2,0.985866618999989));
#343424=CARTESIAN_POINT('Ctrl Pts',(3.88348795599994,2.2,0.985866618999989));
#343425=CARTESIAN_POINT('Ctrl Pts',(3.88389027299994,12.2,0.986004317999987));
#343426=CARTESIAN_POINT('Ctrl Pts',(3.88389027299994,5.2,0.986004317999987));
#343427=CARTESIAN_POINT('Ctrl Pts',(3.88389027299994,2.2,0.986004317999987));
#343428=CARTESIAN_POINT('Ctrl Pts',(3.88429859799994,12.2,0.986144669999987));
#343429=CARTESIAN_POINT('Ctrl Pts',(3.88429859799994,5.2,0.986144669999987));
#343430=CARTESIAN_POINT('Ctrl Pts',(3.88429859799994,2.2,0.986144669999987));
#343431=CARTESIAN_POINT('Ctrl Pts',(3.88471290899994,12.2,0.986287686999985));
#343432=CARTESIAN_POINT('Ctrl Pts',(3.88471290899994,5.2,0.986287686999985));
#343433=CARTESIAN_POINT('Ctrl Pts',(3.88471290899994,2.2,0.986287686999985));
#343434=CARTESIAN_POINT('Ctrl Pts',(3.88513318999994,12.2,0.986433378999987));
#343435=CARTESIAN_POINT('Ctrl Pts',(3.88513318999994,5.2,0.986433378999987));
#343436=CARTESIAN_POINT('Ctrl Pts',(3.88513318999994,2.2,0.986433378999987));
#343437=CARTESIAN_POINT('Ctrl Pts',(3.88555942099994,12.2,0.986581756999985));
#343438=CARTESIAN_POINT('Ctrl Pts',(3.88555942099994,5.2,0.986581756999985));
#343439=CARTESIAN_POINT('Ctrl Pts',(3.88555942099994,2.2,0.986581756999985));
#343440=CARTESIAN_POINT('Ctrl Pts',(3.88599158099994,12.2,0.986732831999984));
#343441=CARTESIAN_POINT('Ctrl Pts',(3.88599158099994,5.2,0.986732831999984));
#343442=CARTESIAN_POINT('Ctrl Pts',(3.88599158099994,2.2,0.986732831999984));
#343443=CARTESIAN_POINT('Ctrl Pts',(3.88642965499994,12.2,0.986886615999989));
#343444=CARTESIAN_POINT('Ctrl Pts',(3.88642965499994,5.2,0.986886615999989));
#343445=CARTESIAN_POINT('Ctrl Pts',(3.88642965499994,2.2,0.986886615999989));
#343446=CARTESIAN_POINT('Ctrl Pts',(3.88687362299994,12.2,0.987043119999989));
#343447=CARTESIAN_POINT('Ctrl Pts',(3.88687362299994,5.2,0.987043119999989));
#343448=CARTESIAN_POINT('Ctrl Pts',(3.88687362299994,2.2,0.987043119999989));
#343449=CARTESIAN_POINT('Ctrl Pts',(3.88732346699994,12.2,0.987202352999983));
#343450=CARTESIAN_POINT('Ctrl Pts',(3.88732346699994,5.2,0.987202352999983));
#343451=CARTESIAN_POINT('Ctrl Pts',(3.88732346699994,2.2,0.987202352999983));
#343452=CARTESIAN_POINT('Ctrl Pts',(3.88777916899994,12.2,0.987364327999987));
#343453=CARTESIAN_POINT('Ctrl Pts',(3.88777916899994,5.2,0.987364327999987));
#343454=CARTESIAN_POINT('Ctrl Pts',(3.88777916899994,2.2,0.987364327999987));
#343455=CARTESIAN_POINT('Ctrl Pts',(3.88824070799994,12.2,0.987529053999987));
#343456=CARTESIAN_POINT('Ctrl Pts',(3.88824070799994,5.2,0.987529053999987));
#343457=CARTESIAN_POINT('Ctrl Pts',(3.88824070799994,2.2,0.987529053999987));
#343458=CARTESIAN_POINT('Ctrl Pts',(3.88870806899994,12.2,0.987696542999985));
#343459=CARTESIAN_POINT('Ctrl Pts',(3.88870806899994,5.2,0.987696542999985));
#343460=CARTESIAN_POINT('Ctrl Pts',(3.88870806899994,2.2,0.987696542999985));
#343461=CARTESIAN_POINT('Ctrl Pts',(3.88918123199994,12.2,0.987866804999986));
#343462=CARTESIAN_POINT('Ctrl Pts',(3.88918123199994,5.2,0.987866804999986));
#343463=CARTESIAN_POINT('Ctrl Pts',(3.88918123199994,2.2,0.987866804999986));
#343464=CARTESIAN_POINT('Ctrl Pts',(3.88966017899994,12.2,0.988039850999982));
#343465=CARTESIAN_POINT('Ctrl Pts',(3.88966017899994,5.2,0.988039850999982));
#343466=CARTESIAN_POINT('Ctrl Pts',(3.88966017899994,2.2,0.988039850999982));
#343467=CARTESIAN_POINT('Ctrl Pts',(3.89014489099994,12.2,0.988215690999983));
#343468=CARTESIAN_POINT('Ctrl Pts',(3.89014489099994,5.2,0.988215690999983));
#343469=CARTESIAN_POINT('Ctrl Pts',(3.89014489099994,2.2,0.988215690999983));
#343470=CARTESIAN_POINT('Ctrl Pts',(3.89063535099994,12.2,0.988394335999985));
#343471=CARTESIAN_POINT('Ctrl Pts',(3.89063535099994,5.2,0.988394335999985));
#343472=CARTESIAN_POINT('Ctrl Pts',(3.89063535099994,2.2,0.988394335999985));
#343473=CARTESIAN_POINT('Ctrl Pts',(3.89113154099994,12.2,0.988575795999989));
#343474=CARTESIAN_POINT('Ctrl Pts',(3.89113154099994,5.2,0.988575795999989));
#343475=CARTESIAN_POINT('Ctrl Pts',(3.89113154099994,2.2,0.988575795999989));
#343476=CARTESIAN_POINT('Ctrl Pts',(3.89163344299994,12.2,0.988760082999987));
#343477=CARTESIAN_POINT('Ctrl Pts',(3.89163344299994,5.2,0.988760082999987));
#343478=CARTESIAN_POINT('Ctrl Pts',(3.89163344299994,2.2,0.988760082999987));
#343479=CARTESIAN_POINT('Ctrl Pts',(3.89214103699994,12.2,0.988947204999988));
#343480=CARTESIAN_POINT('Ctrl Pts',(3.89214103699994,5.2,0.988947204999988));
#343481=CARTESIAN_POINT('Ctrl Pts',(3.89214103699994,2.2,0.988947204999988));
#343482=CARTESIAN_POINT('Ctrl Pts',(3.89265430699994,12.2,0.989137172999985));
#343483=CARTESIAN_POINT('Ctrl Pts',(3.89265430699994,5.2,0.989137172999985));
#343484=CARTESIAN_POINT('Ctrl Pts',(3.89265430699994,2.2,0.989137172999985));
#343485=CARTESIAN_POINT('Ctrl Pts',(3.89317323499994,12.2,0.989329997999988));
#343486=CARTESIAN_POINT('Ctrl Pts',(3.89317323499994,5.2,0.989329997999988));
#343487=CARTESIAN_POINT('Ctrl Pts',(3.89317323499994,2.2,0.989329997999988));
#343488=CARTESIAN_POINT('Ctrl Pts',(3.89369780199994,12.2,0.989525688999984));
#343489=CARTESIAN_POINT('Ctrl Pts',(3.89369780199994,5.2,0.989525688999984));
#343490=CARTESIAN_POINT('Ctrl Pts',(3.89369780199994,2.2,0.989525688999984));
#343491=CARTESIAN_POINT('Ctrl Pts',(3.89422799099994,12.2,0.989724256999986));
#343492=CARTESIAN_POINT('Ctrl Pts',(3.89422799099994,5.2,0.989724256999986));
#343493=CARTESIAN_POINT('Ctrl Pts',(3.89422799099994,2.2,0.989724256999986));
#343494=CARTESIAN_POINT('Ctrl Pts',(3.89476378299995,12.2,0.989925711999984));
#343495=CARTESIAN_POINT('Ctrl Pts',(3.89476378299995,5.2,0.989925711999984));
#343496=CARTESIAN_POINT('Ctrl Pts',(3.89476378299995,2.2,0.989925711999984));
#343497=CARTESIAN_POINT('Ctrl Pts',(3.89530516299994,12.2,0.990130063999985));
#343498=CARTESIAN_POINT('Ctrl Pts',(3.89530516299994,5.2,0.990130063999985));
#343499=CARTESIAN_POINT('Ctrl Pts',(3.89530516299994,2.2,0.990130063999985));
#343500=CARTESIAN_POINT('Ctrl Pts',(3.89585210999994,12.2,0.990337322999988));
#343501=CARTESIAN_POINT('Ctrl Pts',(3.89585210999994,5.2,0.990337322999988));
#343502=CARTESIAN_POINT('Ctrl Pts',(3.89585210999994,2.2,0.990337322999988));
#343503=CARTESIAN_POINT('Ctrl Pts',(3.89640460899995,12.2,0.990547498999987));
#343504=CARTESIAN_POINT('Ctrl Pts',(3.89640460899995,5.2,0.990547498999987));
#343505=CARTESIAN_POINT('Ctrl Pts',(3.89640460899995,2.2,0.990547498999987));
#343506=CARTESIAN_POINT('Ctrl Pts',(3.89696263999994,12.2,0.990760599999985));
#343507=CARTESIAN_POINT('Ctrl Pts',(3.89696263999994,5.2,0.990760599999985));
#343508=CARTESIAN_POINT('Ctrl Pts',(3.89696263999994,2.2,0.990760599999985));
#343509=CARTESIAN_POINT('Ctrl Pts',(3.89752618599994,12.2,0.990976638999985));
#343510=CARTESIAN_POINT('Ctrl Pts',(3.89752618599994,5.2,0.990976638999985));
#343511=CARTESIAN_POINT('Ctrl Pts',(3.89752618599994,2.2,0.990976638999985));
#343512=CARTESIAN_POINT('Ctrl Pts',(3.89809523199994,12.2,0.991195624999985));
#343513=CARTESIAN_POINT('Ctrl Pts',(3.89809523199994,5.2,0.991195624999985));
#343514=CARTESIAN_POINT('Ctrl Pts',(3.89809523199994,2.2,0.991195624999985));
#343515=CARTESIAN_POINT('Ctrl Pts',(3.89866975699994,12.2,0.991417564999986));
#343516=CARTESIAN_POINT('Ctrl Pts',(3.89866975699994,5.2,0.991417564999986));
#343517=CARTESIAN_POINT('Ctrl Pts',(3.89866975699994,2.2,0.991417564999986));
#343518=CARTESIAN_POINT('Ctrl Pts',(3.89924974499994,12.2,0.991642471999987));
#343519=CARTESIAN_POINT('Ctrl Pts',(3.89924974499994,5.2,0.991642471999987));
#343520=CARTESIAN_POINT('Ctrl Pts',(3.89924974499994,2.2,0.991642471999987));
#343521=CARTESIAN_POINT('Ctrl Pts',(3.89983517799994,12.2,0.991870353999986));
#343522=CARTESIAN_POINT('Ctrl Pts',(3.89983517799994,5.2,0.991870353999986));
#343523=CARTESIAN_POINT('Ctrl Pts',(3.89983517799994,2.2,0.991870353999986));
#343524=CARTESIAN_POINT('Ctrl Pts',(3.90042604099994,12.2,0.992101219999988));
#343525=CARTESIAN_POINT('Ctrl Pts',(3.90042604099994,5.2,0.992101219999988));
#343526=CARTESIAN_POINT('Ctrl Pts',(3.90042604099994,2.2,0.992101219999988));
#343527=CARTESIAN_POINT('Ctrl Pts',(3.90102231199994,12.2,0.992335080999984));
#343528=CARTESIAN_POINT('Ctrl Pts',(3.90102231199994,5.2,0.992335080999984));
#343529=CARTESIAN_POINT('Ctrl Pts',(3.90102231199994,2.2,0.992335080999984));
#343530=CARTESIAN_POINT('Ctrl Pts',(3.90162397899994,12.2,0.992571945999985));
#343531=CARTESIAN_POINT('Ctrl Pts',(3.90162397899994,5.2,0.992571945999985));
#343532=CARTESIAN_POINT('Ctrl Pts',(3.90162397899994,2.2,0.992571945999985));
#343533=CARTESIAN_POINT('Ctrl Pts',(3.90223102099994,12.2,0.992811823999986));
#343534=CARTESIAN_POINT('Ctrl Pts',(3.90223102099994,5.2,0.992811823999986));
#343535=CARTESIAN_POINT('Ctrl Pts',(3.90223102099994,2.2,0.992811823999986));
#343536=CARTESIAN_POINT('Ctrl Pts',(3.90284342099994,12.2,0.993054724999984));
#343537=CARTESIAN_POINT('Ctrl Pts',(3.90284342099994,5.2,0.993054724999984));
#343538=CARTESIAN_POINT('Ctrl Pts',(3.90284342099994,2.2,0.993054724999984));
#343539=CARTESIAN_POINT('Ctrl Pts',(3.90346116399995,12.2,0.993300655999985));
#343540=CARTESIAN_POINT('Ctrl Pts',(3.90346116399995,5.2,0.993300655999985));
#343541=CARTESIAN_POINT('Ctrl Pts',(3.90346116399995,2.2,0.993300655999985));
#343542=CARTESIAN_POINT('Ctrl Pts',(3.90408422999994,12.2,0.993549630999984));
#343543=CARTESIAN_POINT('Ctrl Pts',(3.90408422999994,5.2,0.993549630999984));
#343544=CARTESIAN_POINT('Ctrl Pts',(3.90408422999994,2.2,0.993549630999984));
#343545=CARTESIAN_POINT('Ctrl Pts',(3.90471260399994,12.2,0.993801653999986));
#343546=CARTESIAN_POINT('Ctrl Pts',(3.90471260399994,5.2,0.993801653999986));
#343547=CARTESIAN_POINT('Ctrl Pts',(3.90471260399994,2.2,0.993801653999986));
#343548=CARTESIAN_POINT('Ctrl Pts',(3.90534626899994,12.2,0.994056737999984));
#343549=CARTESIAN_POINT('Ctrl Pts',(3.90534626899994,5.2,0.994056737999984));
#343550=CARTESIAN_POINT('Ctrl Pts',(3.90534626899994,2.2,0.994056737999984));
#343551=CARTESIAN_POINT('Ctrl Pts',(3.90598520699994,12.2,0.994314889999988));
#343552=CARTESIAN_POINT('Ctrl Pts',(3.90598520699994,5.2,0.994314889999988));
#343553=CARTESIAN_POINT('Ctrl Pts',(3.90598520699994,2.2,0.994314889999988));
#343554=CARTESIAN_POINT('Ctrl Pts',(3.90662940099994,12.2,0.994576120999984));
#343555=CARTESIAN_POINT('Ctrl Pts',(3.90662940099994,5.2,0.994576120999984));
#343556=CARTESIAN_POINT('Ctrl Pts',(3.90662940099994,2.2,0.994576120999984));
#343557=CARTESIAN_POINT('Ctrl Pts',(3.90727883399994,12.2,0.994840437999986));
#343558=CARTESIAN_POINT('Ctrl Pts',(3.90727883399994,5.2,0.994840437999986));
#343559=CARTESIAN_POINT('Ctrl Pts',(3.90727883399994,2.2,0.994840437999986));
#343560=CARTESIAN_POINT('Ctrl Pts',(3.90793348999994,12.2,0.995107849999983));
#343561=CARTESIAN_POINT('Ctrl Pts',(3.90793348999994,5.2,0.995107849999983));
#343562=CARTESIAN_POINT('Ctrl Pts',(3.90793348999994,2.2,0.995107849999983));
#343563=CARTESIAN_POINT('Ctrl Pts',(3.90859335099994,12.2,0.995378367999984));
#343564=CARTESIAN_POINT('Ctrl Pts',(3.90859335099994,5.2,0.995378367999984));
#343565=CARTESIAN_POINT('Ctrl Pts',(3.90859335099994,2.2,0.995378367999984));
#343566=CARTESIAN_POINT('Ctrl Pts',(3.90925840099994,12.2,0.995651999999985));
#343567=CARTESIAN_POINT('Ctrl Pts',(3.90925840099994,5.2,0.995651999999985));
#343568=CARTESIAN_POINT('Ctrl Pts',(3.90925840099994,2.2,0.995651999999985));
#343569=CARTESIAN_POINT('Ctrl Pts',(3.90992862199994,12.2,0.995928753999986));
#343570=CARTESIAN_POINT('Ctrl Pts',(3.90992862199994,5.2,0.995928753999986));
#343571=CARTESIAN_POINT('Ctrl Pts',(3.90992862199994,2.2,0.995928753999986));
#343572=CARTESIAN_POINT('Ctrl Pts',(3.91060399799994,12.2,0.996208638999985));
#343573=CARTESIAN_POINT('Ctrl Pts',(3.91060399799994,5.2,0.996208638999985));
#343574=CARTESIAN_POINT('Ctrl Pts',(3.91060399799994,2.2,0.996208638999985));
#343575=CARTESIAN_POINT('Ctrl Pts',(3.91128451199994,12.2,0.996491665999986));
#343576=CARTESIAN_POINT('Ctrl Pts',(3.91128451199994,5.2,0.996491665999986));
#343577=CARTESIAN_POINT('Ctrl Pts',(3.91128451199994,2.2,0.996491665999986));
#343578=CARTESIAN_POINT('Ctrl Pts',(3.91197014899994,12.2,0.996777839999985));
#343579=CARTESIAN_POINT('Ctrl Pts',(3.91197014899994,5.2,0.996777839999985));
#343580=CARTESIAN_POINT('Ctrl Pts',(3.91197014899994,2.2,0.996777839999985));
#343581=CARTESIAN_POINT('Ctrl Pts',(3.91266088899994,12.2,0.997067171999984));
#343582=CARTESIAN_POINT('Ctrl Pts',(3.91266088899994,5.2,0.997067171999984));
#343583=CARTESIAN_POINT('Ctrl Pts',(3.91266088899994,2.2,0.997067171999984));
#343584=CARTESIAN_POINT('Ctrl Pts',(3.91335671699994,12.2,0.997359669999986));
#343585=CARTESIAN_POINT('Ctrl Pts',(3.91335671699994,5.2,0.997359669999986));
#343586=CARTESIAN_POINT('Ctrl Pts',(3.91335671699994,2.2,0.997359669999986));
#343587=CARTESIAN_POINT('Ctrl Pts',(3.91405761799994,12.2,0.997655342999986));
#343588=CARTESIAN_POINT('Ctrl Pts',(3.91405761799994,5.2,0.997655342999986));
#343589=CARTESIAN_POINT('Ctrl Pts',(3.91405761799994,2.2,0.997655342999986));
#343590=CARTESIAN_POINT('Ctrl Pts',(3.91476357299994,12.2,0.997954198999986));
#343591=CARTESIAN_POINT('Ctrl Pts',(3.91476357299994,5.2,0.997954198999986));
#343592=CARTESIAN_POINT('Ctrl Pts',(3.91476357299994,2.2,0.997954198999986));
#343593=CARTESIAN_POINT('Ctrl Pts',(3.91547456599994,12.2,0.998256247999985));
#343594=CARTESIAN_POINT('Ctrl Pts',(3.91547456599994,5.2,0.998256247999985));
#343595=CARTESIAN_POINT('Ctrl Pts',(3.91547456599994,2.2,0.998256247999985));
#343596=CARTESIAN_POINT('Ctrl Pts',(3.91619058299994,12.2,0.998561495999986));
#343597=CARTESIAN_POINT('Ctrl Pts',(3.91619058299994,5.2,0.998561495999986));
#343598=CARTESIAN_POINT('Ctrl Pts',(3.91619058299994,2.2,0.998561495999986));
#343599=CARTESIAN_POINT('Ctrl Pts',(3.91691160399994,12.2,0.998869953999986));
#343600=CARTESIAN_POINT('Ctrl Pts',(3.91691160399994,5.2,0.998869953999986));
#343601=CARTESIAN_POINT('Ctrl Pts',(3.91691160399994,2.2,0.998869953999986));
#343602=CARTESIAN_POINT('Ctrl Pts',(3.91763761399994,12.2,0.999181626999985));
#343603=CARTESIAN_POINT('Ctrl Pts',(3.91763761399994,5.2,0.999181626999985));
#343604=CARTESIAN_POINT('Ctrl Pts',(3.91763761399994,2.2,0.999181626999985));
#343605=CARTESIAN_POINT('Ctrl Pts',(3.91836859699994,12.2,0.999496526999986));
#343606=CARTESIAN_POINT('Ctrl Pts',(3.91836859699994,5.2,0.999496526999986));
#343607=CARTESIAN_POINT('Ctrl Pts',(3.91836859699994,2.2,0.999496526999986));
#343608=CARTESIAN_POINT('Ctrl Pts',(3.91910453599994,12.2,0.999814659999987));
#343609=CARTESIAN_POINT('Ctrl Pts',(3.91910453599994,5.2,0.999814659999987));
#343610=CARTESIAN_POINT('Ctrl Pts',(3.91910453599994,2.2,0.999814659999987));
#343611=CARTESIAN_POINT('Ctrl Pts',(3.91984541599994,12.2,1.00013603499999));
#343612=CARTESIAN_POINT('Ctrl Pts',(3.91984541599994,5.2,1.00013603499999));
#343613=CARTESIAN_POINT('Ctrl Pts',(3.91984541599994,2.2,1.00013603499999));
#343614=CARTESIAN_POINT('Ctrl Pts',(3.92059121899994,12.2,1.00046065999999));
#343615=CARTESIAN_POINT('Ctrl Pts',(3.92059121899994,5.2,1.00046065999999));
#343616=CARTESIAN_POINT('Ctrl Pts',(3.92059121899994,2.2,1.00046065999999));
#343617=CARTESIAN_POINT('Ctrl Pts',(3.92134192799994,12.2,1.00078854399999));
#343618=CARTESIAN_POINT('Ctrl Pts',(3.92134192799994,5.2,1.00078854399999));
#343619=CARTESIAN_POINT('Ctrl Pts',(3.92134192799994,2.2,1.00078854399999));
#343620=CARTESIAN_POINT('Ctrl Pts',(3.92209752999995,12.2,1.00111969399999));
#343621=CARTESIAN_POINT('Ctrl Pts',(3.92209752999995,5.2,1.00111969399999));
#343622=CARTESIAN_POINT('Ctrl Pts',(3.92209752999995,2.2,1.00111969399999));
#343623=CARTESIAN_POINT('Ctrl Pts',(3.92285800599994,12.2,1.00145411799998));
#343624=CARTESIAN_POINT('Ctrl Pts',(3.92285800599994,5.2,1.00145411799998));
#343625=CARTESIAN_POINT('Ctrl Pts',(3.92285800599994,2.2,1.00145411799998));
#343626=CARTESIAN_POINT('Ctrl Pts',(3.92362334199994,12.2,1.00179182499998));
#343627=CARTESIAN_POINT('Ctrl Pts',(3.92362334199994,5.2,1.00179182499998));
#343628=CARTESIAN_POINT('Ctrl Pts',(3.92362334199994,2.2,1.00179182499998));
#343629=CARTESIAN_POINT('Ctrl Pts',(3.92439352099994,12.2,1.00213282199999));
#343630=CARTESIAN_POINT('Ctrl Pts',(3.92439352099994,5.2,1.00213282199999));
#343631=CARTESIAN_POINT('Ctrl Pts',(3.92439352099994,2.2,1.00213282199999));
#343632=CARTESIAN_POINT('Ctrl Pts',(3.92516852499994,12.2,1.00247711799998));
#343633=CARTESIAN_POINT('Ctrl Pts',(3.92516852499994,5.2,1.00247711799998));
#343634=CARTESIAN_POINT('Ctrl Pts',(3.92516852499994,2.2,1.00247711799998));
#343635=CARTESIAN_POINT('Ctrl Pts',(3.92594834099994,12.2,1.00282471899999));
#343636=CARTESIAN_POINT('Ctrl Pts',(3.92594834099994,5.2,1.00282471899999));
#343637=CARTESIAN_POINT('Ctrl Pts',(3.92594834099994,2.2,1.00282471899999));
#343638=CARTESIAN_POINT('Ctrl Pts',(3.92673295199994,12.2,1.00317563499999));
#343639=CARTESIAN_POINT('Ctrl Pts',(3.92673295199994,5.2,1.00317563499999));
#343640=CARTESIAN_POINT('Ctrl Pts',(3.92673295199994,2.2,1.00317563499999));
#343641=CARTESIAN_POINT('Ctrl Pts',(3.92752233999994,12.2,1.00352987299999));
#343642=CARTESIAN_POINT('Ctrl Pts',(3.92752233999994,5.2,1.00352987299999));
#343643=CARTESIAN_POINT('Ctrl Pts',(3.92752233999994,2.2,1.00352987299999));
#343644=CARTESIAN_POINT('Ctrl Pts',(3.92831649199994,12.2,1.00388744099998));
#343645=CARTESIAN_POINT('Ctrl Pts',(3.92831649199994,5.2,1.00388744099998));
#343646=CARTESIAN_POINT('Ctrl Pts',(3.92831649199994,2.2,1.00388744099998));
#343647=CARTESIAN_POINT('Ctrl Pts',(3.92911538899994,12.2,1.00424834599998));
#343648=CARTESIAN_POINT('Ctrl Pts',(3.92911538899994,5.2,1.00424834599998));
#343649=CARTESIAN_POINT('Ctrl Pts',(3.92911538899994,2.2,1.00424834599998));
#343650=CARTESIAN_POINT('Ctrl Pts',(3.92991901899994,12.2,1.00461259699999));
#343651=CARTESIAN_POINT('Ctrl Pts',(3.92991901899994,5.2,1.00461259699999));
#343652=CARTESIAN_POINT('Ctrl Pts',(3.92991901899994,2.2,1.00461259699999));
#343653=CARTESIAN_POINT('Ctrl Pts',(3.93072736299994,12.2,1.00498019899999));
#343654=CARTESIAN_POINT('Ctrl Pts',(3.93072736299994,5.2,1.00498019899999));
#343655=CARTESIAN_POINT('Ctrl Pts',(3.93072736299994,2.2,1.00498019899999));
#343656=CARTESIAN_POINT('Ctrl Pts',(3.93154040599994,12.2,1.00535116299998));
#343657=CARTESIAN_POINT('Ctrl Pts',(3.93154040599994,5.2,1.00535116299998));
#343658=CARTESIAN_POINT('Ctrl Pts',(3.93154040599994,2.2,1.00535116299998));
#343659=CARTESIAN_POINT('Ctrl Pts',(3.93235813299994,12.2,1.00572549499998));
#343660=CARTESIAN_POINT('Ctrl Pts',(3.93235813299994,5.2,1.00572549499998));
#343661=CARTESIAN_POINT('Ctrl Pts',(3.93235813299994,2.2,1.00572549499998));
#343662=CARTESIAN_POINT('Ctrl Pts',(3.93318052799994,12.2,1.00610320199999));
#343663=CARTESIAN_POINT('Ctrl Pts',(3.93318052799994,5.2,1.00610320199999));
#343664=CARTESIAN_POINT('Ctrl Pts',(3.93318052799994,2.2,1.00610320199999));
#343665=CARTESIAN_POINT('Ctrl Pts',(3.93400757499994,12.2,1.00648429199999));
#343666=CARTESIAN_POINT('Ctrl Pts',(3.93400757499994,5.2,1.00648429199999));
#343667=CARTESIAN_POINT('Ctrl Pts',(3.93400757499994,2.2,1.00648429199999));
#343668=CARTESIAN_POINT('Ctrl Pts',(3.93483925699994,12.2,1.00686877299998));
#343669=CARTESIAN_POINT('Ctrl Pts',(3.93483925699994,5.2,1.00686877299998));
#343670=CARTESIAN_POINT('Ctrl Pts',(3.93483925699994,2.2,1.00686877299998));
#343671=CARTESIAN_POINT('Ctrl Pts',(3.93567556099994,12.2,1.00725665199999));
#343672=CARTESIAN_POINT('Ctrl Pts',(3.93567556099994,5.2,1.00725665199999));
#343673=CARTESIAN_POINT('Ctrl Pts',(3.93567556099994,2.2,1.00725665199999));
#343674=CARTESIAN_POINT('Ctrl Pts',(3.93651646899994,12.2,1.00764793699998));
#343675=CARTESIAN_POINT('Ctrl Pts',(3.93651646899994,5.2,1.00764793699998));
#343676=CARTESIAN_POINT('Ctrl Pts',(3.93651646899994,2.2,1.00764793699998));
#343677=CARTESIAN_POINT('Ctrl Pts',(3.93736196599995,12.2,1.00804263299999));
#343678=CARTESIAN_POINT('Ctrl Pts',(3.93736196599995,5.2,1.00804263299999));
#343679=CARTESIAN_POINT('Ctrl Pts',(3.93736196599995,2.2,1.00804263299999));
#343680=CARTESIAN_POINT('Ctrl Pts',(3.93821203799994,12.2,1.00844074999999));
#343681=CARTESIAN_POINT('Ctrl Pts',(3.93821203799994,5.2,1.00844074999999));
#343682=CARTESIAN_POINT('Ctrl Pts',(3.93821203799994,2.2,1.00844074999999));
#343683=CARTESIAN_POINT('Ctrl Pts',(3.93906666699994,12.2,1.00884229399998));
#343684=CARTESIAN_POINT('Ctrl Pts',(3.93906666699994,5.2,1.00884229399998));
#343685=CARTESIAN_POINT('Ctrl Pts',(3.93906666699994,2.2,1.00884229399998));
#343686=CARTESIAN_POINT('Ctrl Pts',(3.93992583999994,12.2,1.00924727299998));
#343687=CARTESIAN_POINT('Ctrl Pts',(3.93992583999994,5.2,1.00924727299998));
#343688=CARTESIAN_POINT('Ctrl Pts',(3.93992583999994,2.2,1.00924727299998));
#343689=CARTESIAN_POINT('Ctrl Pts',(3.94078953999994,12.2,1.00965569399999));
#343690=CARTESIAN_POINT('Ctrl Pts',(3.94078953999994,5.2,1.00965569399999));
#343691=CARTESIAN_POINT('Ctrl Pts',(3.94078953999994,2.2,1.00965569399999));
#343692=CARTESIAN_POINT('Ctrl Pts',(3.94165775099994,12.2,1.01006756199999));
#343693=CARTESIAN_POINT('Ctrl Pts',(3.94165775099994,5.2,1.01006756199999));
#343694=CARTESIAN_POINT('Ctrl Pts',(3.94165775099994,2.2,1.01006756199999));
#343695=CARTESIAN_POINT('Ctrl Pts',(3.94253045899994,12.2,1.01048288799999));
#343696=CARTESIAN_POINT('Ctrl Pts',(3.94253045899994,5.2,1.01048288799999));
#343697=CARTESIAN_POINT('Ctrl Pts',(3.94253045899994,2.2,1.01048288799999));
#343698=CARTESIAN_POINT('Ctrl Pts',(3.94340764899995,12.2,1.01090167499999));
#343699=CARTESIAN_POINT('Ctrl Pts',(3.94340764899995,5.2,1.01090167499999));
#343700=CARTESIAN_POINT('Ctrl Pts',(3.94340764899995,2.2,1.01090167499999));
#343701=CARTESIAN_POINT('Ctrl Pts',(3.94428930299994,12.2,1.01132393399999));
#343702=CARTESIAN_POINT('Ctrl Pts',(3.94428930299994,5.2,1.01132393399999));
#343703=CARTESIAN_POINT('Ctrl Pts',(3.94428930299994,2.2,1.01132393399999));
#343704=CARTESIAN_POINT('Ctrl Pts',(3.94517540899994,12.2,1.01174966899999));
#343705=CARTESIAN_POINT('Ctrl Pts',(3.94517540899994,5.2,1.01174966899999));
#343706=CARTESIAN_POINT('Ctrl Pts',(3.94517540899994,2.2,1.01174966899999));
#343707=CARTESIAN_POINT('Ctrl Pts',(3.94606594899995,12.2,1.01217888899999));
#343708=CARTESIAN_POINT('Ctrl Pts',(3.94606594899995,5.2,1.01217888899999));
#343709=CARTESIAN_POINT('Ctrl Pts',(3.94606594899995,2.2,1.01217888899999));
#343710=CARTESIAN_POINT('Ctrl Pts',(3.94696090899994,12.2,1.01261159899999));
#343711=CARTESIAN_POINT('Ctrl Pts',(3.94696090899994,5.2,1.01261159899999));
#343712=CARTESIAN_POINT('Ctrl Pts',(3.94696090899994,2.2,1.01261159899999));
#343713=CARTESIAN_POINT('Ctrl Pts',(3.94786027299994,12.2,1.01304780699999));
#343714=CARTESIAN_POINT('Ctrl Pts',(3.94786027299994,5.2,1.01304780699999));
#343715=CARTESIAN_POINT('Ctrl Pts',(3.94786027299994,2.2,1.01304780699999));
#343716=CARTESIAN_POINT('Ctrl Pts',(3.94876402799994,12.2,1.01348751999998));
#343717=CARTESIAN_POINT('Ctrl Pts',(3.94876402799994,5.2,1.01348751999998));
#343718=CARTESIAN_POINT('Ctrl Pts',(3.94876402799994,2.2,1.01348751999998));
#343719=CARTESIAN_POINT('Ctrl Pts',(3.94967215599995,12.2,1.01393074399999));
#343720=CARTESIAN_POINT('Ctrl Pts',(3.94967215599995,5.2,1.01393074399999));
#343721=CARTESIAN_POINT('Ctrl Pts',(3.94967215599995,2.2,1.01393074399999));
#343722=CARTESIAN_POINT('Ctrl Pts',(3.95058464299994,12.2,1.01437748699999));
#343723=CARTESIAN_POINT('Ctrl Pts',(3.95058464299994,5.2,1.01437748699999));
#343724=CARTESIAN_POINT('Ctrl Pts',(3.95058464299994,2.2,1.01437748699999));
#343725=CARTESIAN_POINT('Ctrl Pts',(3.95150147499994,12.2,1.01482775399999));
#343726=CARTESIAN_POINT('Ctrl Pts',(3.95150147499994,5.2,1.01482775399999));
#343727=CARTESIAN_POINT('Ctrl Pts',(3.95150147499994,2.2,1.01482775399999));
#343728=CARTESIAN_POINT('Ctrl Pts',(3.95242263499994,12.2,1.01528155399999));
#343729=CARTESIAN_POINT('Ctrl Pts',(3.95242263499994,5.2,1.01528155399999));
#343730=CARTESIAN_POINT('Ctrl Pts',(3.95242263499994,2.2,1.01528155399999));
#343731=CARTESIAN_POINT('Ctrl Pts',(3.95334810899994,12.2,1.01573889199999));
#343732=CARTESIAN_POINT('Ctrl Pts',(3.95334810899994,5.2,1.01573889199999));
#343733=CARTESIAN_POINT('Ctrl Pts',(3.95334810899994,2.2,1.01573889199999));
#343734=CARTESIAN_POINT('Ctrl Pts',(3.95427788199994,12.2,1.01619977599999));
#343735=CARTESIAN_POINT('Ctrl Pts',(3.95427788199994,5.2,1.01619977599999));
#343736=CARTESIAN_POINT('Ctrl Pts',(3.95427788199994,2.2,1.01619977599999));
#343737=CARTESIAN_POINT('Ctrl Pts',(3.95521193899994,12.2,1.01666420999999));
#343738=CARTESIAN_POINT('Ctrl Pts',(3.95521193899994,5.2,1.01666420999999));
#343739=CARTESIAN_POINT('Ctrl Pts',(3.95521193899994,2.2,1.01666420999999));
#343740=CARTESIAN_POINT('Ctrl Pts',(3.95615026299994,12.2,1.01713220299999));
#343741=CARTESIAN_POINT('Ctrl Pts',(3.95615026299994,5.2,1.01713220299999));
#343742=CARTESIAN_POINT('Ctrl Pts',(3.95615026299994,2.2,1.01713220299999));
#343743=CARTESIAN_POINT('Ctrl Pts',(3.95709284299994,12.2,1.01760375999998));
#343744=CARTESIAN_POINT('Ctrl Pts',(3.95709284299994,5.2,1.01760375999998));
#343745=CARTESIAN_POINT('Ctrl Pts',(3.95709284299994,2.2,1.01760375999998));
#343746=CARTESIAN_POINT('Ctrl Pts',(3.95803966099994,12.2,1.01807888899998));
#343747=CARTESIAN_POINT('Ctrl Pts',(3.95803966099994,5.2,1.01807888899998));
#343748=CARTESIAN_POINT('Ctrl Pts',(3.95803966099994,2.2,1.01807888899998));
#343749=CARTESIAN_POINT('Ctrl Pts',(3.95899070299994,12.2,1.01855759699998));
#343750=CARTESIAN_POINT('Ctrl Pts',(3.95899070299994,5.2,1.01855759699998));
#343751=CARTESIAN_POINT('Ctrl Pts',(3.95899070299994,2.2,1.01855759699998));
#343752=CARTESIAN_POINT('Ctrl Pts',(3.95994595499995,12.2,1.01903988699998));
#343753=CARTESIAN_POINT('Ctrl Pts',(3.95994595499995,5.2,1.01903988699998));
#343754=CARTESIAN_POINT('Ctrl Pts',(3.95994595499995,2.2,1.01903988699998));
#343755=CARTESIAN_POINT('Ctrl Pts',(3.96090540099994,12.2,1.01952576899999));
#343756=CARTESIAN_POINT('Ctrl Pts',(3.96090540099994,5.2,1.01952576899999));
#343757=CARTESIAN_POINT('Ctrl Pts',(3.96090540099994,2.2,1.01952576899999));
#343758=CARTESIAN_POINT('Ctrl Pts',(3.96186902799994,12.2,1.02001524699999));
#343759=CARTESIAN_POINT('Ctrl Pts',(3.96186902799994,5.2,1.02001524699999));
#343760=CARTESIAN_POINT('Ctrl Pts',(3.96186902799994,2.2,1.02001524699999));
#343761=CARTESIAN_POINT('Ctrl Pts',(3.96283681799994,12.2,1.02050832899999));
#343762=CARTESIAN_POINT('Ctrl Pts',(3.96283681799994,5.2,1.02050832899999));
#343763=CARTESIAN_POINT('Ctrl Pts',(3.96283681799994,2.2,1.02050832899999));
#343764=CARTESIAN_POINT('Ctrl Pts',(3.96380875899994,12.2,1.02100501999999));
#343765=CARTESIAN_POINT('Ctrl Pts',(3.96380875899994,5.2,1.02100501999999));
#343766=CARTESIAN_POINT('Ctrl Pts',(3.96380875899994,2.2,1.02100501999999));
#343767=CARTESIAN_POINT('Ctrl Pts',(3.96478483499994,12.2,1.02150532699998));
#343768=CARTESIAN_POINT('Ctrl Pts',(3.96478483499994,5.2,1.02150532699998));
#343769=CARTESIAN_POINT('Ctrl Pts',(3.96478483499994,2.2,1.02150532699998));
#343770=CARTESIAN_POINT('Ctrl Pts',(3.96576503099995,12.2,1.02200925599998));
#343771=CARTESIAN_POINT('Ctrl Pts',(3.96576503099995,5.2,1.02200925599998));
#343772=CARTESIAN_POINT('Ctrl Pts',(3.96576503099995,2.2,1.02200925599998));
#343773=CARTESIAN_POINT('Ctrl Pts',(3.96674933499995,12.2,1.02251681299999));
#343774=CARTESIAN_POINT('Ctrl Pts',(3.96674933499995,5.2,1.02251681299999));
#343775=CARTESIAN_POINT('Ctrl Pts',(3.96674933499995,2.2,1.02251681299999));
#343776=CARTESIAN_POINT('Ctrl Pts',(3.96773772899994,12.2,1.02302800399999));
#343777=CARTESIAN_POINT('Ctrl Pts',(3.96773772899994,5.2,1.02302800399999));
#343778=CARTESIAN_POINT('Ctrl Pts',(3.96773772899994,2.2,1.02302800399999));
#343779=CARTESIAN_POINT('Ctrl Pts',(3.96873019999994,12.2,1.02354283599999));
#343780=CARTESIAN_POINT('Ctrl Pts',(3.96873019999994,5.2,1.02354283599999));
#343781=CARTESIAN_POINT('Ctrl Pts',(3.96873019999994,2.2,1.02354283599999));
#343782=CARTESIAN_POINT('Ctrl Pts',(3.96972673299994,12.2,1.02406131499999));
#343783=CARTESIAN_POINT('Ctrl Pts',(3.96972673299994,5.2,1.02406131499999));
#343784=CARTESIAN_POINT('Ctrl Pts',(3.96972673299994,2.2,1.02406131499999));
#343785=CARTESIAN_POINT('Ctrl Pts',(3.97072731399994,12.2,1.02458344599999));
#343786=CARTESIAN_POINT('Ctrl Pts',(3.97072731399994,5.2,1.02458344599999));
#343787=CARTESIAN_POINT('Ctrl Pts',(3.97072731399994,2.2,1.02458344599999));
#343788=CARTESIAN_POINT('Ctrl Pts',(3.97173192799994,12.2,1.02510923499999));
#343789=CARTESIAN_POINT('Ctrl Pts',(3.97173192799994,5.2,1.02510923499999));
#343790=CARTESIAN_POINT('Ctrl Pts',(3.97173192799994,2.2,1.02510923499999));
#343791=CARTESIAN_POINT('Ctrl Pts',(3.97274056099994,12.2,1.02563868999999));
#343792=CARTESIAN_POINT('Ctrl Pts',(3.97274056099994,5.2,1.02563868999999));
#343793=CARTESIAN_POINT('Ctrl Pts',(3.97274056099994,2.2,1.02563868999999));
#343794=CARTESIAN_POINT('Ctrl Pts',(3.97375319799994,12.2,1.02617181399999));
#343795=CARTESIAN_POINT('Ctrl Pts',(3.97375319799994,5.2,1.02617181399999));
#343796=CARTESIAN_POINT('Ctrl Pts',(3.97375319799994,2.2,1.02617181399999));
#343797=CARTESIAN_POINT('Ctrl Pts',(3.97476982499994,12.2,1.02670861599998));
#343798=CARTESIAN_POINT('Ctrl Pts',(3.97476982499994,5.2,1.02670861599998));
#343799=CARTESIAN_POINT('Ctrl Pts',(3.97476982499994,2.2,1.02670861599998));
#343800=CARTESIAN_POINT('Ctrl Pts',(3.97579042599994,12.2,1.02724909999999));
#343801=CARTESIAN_POINT('Ctrl Pts',(3.97579042599994,5.2,1.02724909999999));
#343802=CARTESIAN_POINT('Ctrl Pts',(3.97579042599994,2.2,1.02724909999999));
#343803=CARTESIAN_POINT('Ctrl Pts',(3.97681498899995,12.2,1.02779327199999));
#343804=CARTESIAN_POINT('Ctrl Pts',(3.97681498899995,5.2,1.02779327199999));
#343805=CARTESIAN_POINT('Ctrl Pts',(3.97681498899995,2.2,1.02779327199999));
#343806=CARTESIAN_POINT('Ctrl Pts',(3.97784349899994,12.2,1.02834113799998));
#343807=CARTESIAN_POINT('Ctrl Pts',(3.97784349899994,5.2,1.02834113799998));
#343808=CARTESIAN_POINT('Ctrl Pts',(3.97784349899994,2.2,1.02834113799998));
#343809=CARTESIAN_POINT('Ctrl Pts',(3.97887594099994,12.2,1.02889270399999));
#343810=CARTESIAN_POINT('Ctrl Pts',(3.97887594099994,5.2,1.02889270399999));
#343811=CARTESIAN_POINT('Ctrl Pts',(3.97887594099994,2.2,1.02889270399999));
#343812=CARTESIAN_POINT('Ctrl Pts',(3.97991229999994,12.2,1.02944797499998));
#343813=CARTESIAN_POINT('Ctrl Pts',(3.97991229999994,5.2,1.02944797499998));
#343814=CARTESIAN_POINT('Ctrl Pts',(3.97991229999994,2.2,1.02944797499998));
#343815=CARTESIAN_POINT('Ctrl Pts',(3.98095256299994,12.2,1.03000695799999));
#343816=CARTESIAN_POINT('Ctrl Pts',(3.98095256299994,5.2,1.03000695799999));
#343817=CARTESIAN_POINT('Ctrl Pts',(3.98095256299994,2.2,1.03000695799999));
#343818=CARTESIAN_POINT('Ctrl Pts',(3.98199671599994,12.2,1.03056965699999));
#343819=CARTESIAN_POINT('Ctrl Pts',(3.98199671599994,5.2,1.03056965699999));
#343820=CARTESIAN_POINT('Ctrl Pts',(3.98199671599994,2.2,1.03056965699999));
#343821=CARTESIAN_POINT('Ctrl Pts',(3.98304474399994,12.2,1.03113607999999));
#343822=CARTESIAN_POINT('Ctrl Pts',(3.98304474399994,5.2,1.03113607999999));
#343823=CARTESIAN_POINT('Ctrl Pts',(3.98304474399994,2.2,1.03113607999999));
#343824=CARTESIAN_POINT('Ctrl Pts',(3.98409663299994,12.2,1.03170623099999));
#343825=CARTESIAN_POINT('Ctrl Pts',(3.98409663299994,5.2,1.03170623099999));
#343826=CARTESIAN_POINT('Ctrl Pts',(3.98409663299994,2.2,1.03170623099999));
#343827=CARTESIAN_POINT('Ctrl Pts',(3.98515236799994,12.2,1.03228011599999));
#343828=CARTESIAN_POINT('Ctrl Pts',(3.98515236799994,5.2,1.03228011599999));
#343829=CARTESIAN_POINT('Ctrl Pts',(3.98515236799994,2.2,1.03228011599999));
#343830=CARTESIAN_POINT('Ctrl Pts',(3.98621193499994,12.2,1.03285773999998));
#343831=CARTESIAN_POINT('Ctrl Pts',(3.98621193499994,5.2,1.03285773999998));
#343832=CARTESIAN_POINT('Ctrl Pts',(3.98621193499994,2.2,1.03285773999998));
#343833=CARTESIAN_POINT('Ctrl Pts',(3.98727532099994,12.2,1.03343910999998));
#343834=CARTESIAN_POINT('Ctrl Pts',(3.98727532099994,5.2,1.03343910999998));
#343835=CARTESIAN_POINT('Ctrl Pts',(3.98727532099994,2.2,1.03343910999998));
#343836=CARTESIAN_POINT('Ctrl Pts',(3.98834251199994,12.2,1.03402422899999));
#343837=CARTESIAN_POINT('Ctrl Pts',(3.98834251199994,5.2,1.03402422899999));
#343838=CARTESIAN_POINT('Ctrl Pts',(3.98834251199994,2.2,1.03402422899999));
#343839=CARTESIAN_POINT('Ctrl Pts',(3.98941349399994,12.2,1.03461310499998));
#343840=CARTESIAN_POINT('Ctrl Pts',(3.98941349399994,5.2,1.03461310499998));
#343841=CARTESIAN_POINT('Ctrl Pts',(3.98941349399994,2.2,1.03461310499998));
#343842=CARTESIAN_POINT('Ctrl Pts',(3.99048824999995,12.2,1.03520574299999));
#343843=CARTESIAN_POINT('Ctrl Pts',(3.99048824999995,5.2,1.03520574299999));
#343844=CARTESIAN_POINT('Ctrl Pts',(3.99048824999995,2.2,1.03520574299999));
#343845=CARTESIAN_POINT('Ctrl Pts',(3.99156676899994,12.2,1.03580214699999));
#343846=CARTESIAN_POINT('Ctrl Pts',(3.99156676899994,5.2,1.03580214699999));
#343847=CARTESIAN_POINT('Ctrl Pts',(3.99156676899994,2.2,1.03580214699999));
#343848=CARTESIAN_POINT('Ctrl Pts',(3.99264903699994,12.2,1.03640232399998));
#343849=CARTESIAN_POINT('Ctrl Pts',(3.99264903699994,5.2,1.03640232399998));
#343850=CARTESIAN_POINT('Ctrl Pts',(3.99264903699994,2.2,1.03640232399998));
#343851=CARTESIAN_POINT('Ctrl Pts',(3.99373503799994,12.2,1.03700627899999));
#343852=CARTESIAN_POINT('Ctrl Pts',(3.99373503799994,5.2,1.03700627899999));
#343853=CARTESIAN_POINT('Ctrl Pts',(3.99373503799994,2.2,1.03700627899999));
#343854=CARTESIAN_POINT('Ctrl Pts',(3.99482475899994,12.2,1.03761401499999));
#343855=CARTESIAN_POINT('Ctrl Pts',(3.99482475899994,5.2,1.03761401499999));
#343856=CARTESIAN_POINT('Ctrl Pts',(3.99482475899994,2.2,1.03761401499999));
#343857=CARTESIAN_POINT('Ctrl Pts',(3.99591818699994,12.2,1.03822554099999));
#343858=CARTESIAN_POINT('Ctrl Pts',(3.99591818699994,5.2,1.03822554099999));
#343859=CARTESIAN_POINT('Ctrl Pts',(3.99591818699994,2.2,1.03822554099999));
#343860=CARTESIAN_POINT('Ctrl Pts',(3.99701530699994,12.2,1.03884085899999));
#343861=CARTESIAN_POINT('Ctrl Pts',(3.99701530699994,5.2,1.03884085899999));
#343862=CARTESIAN_POINT('Ctrl Pts',(3.99701530699994,2.2,1.03884085899999));
#343863=CARTESIAN_POINT('Ctrl Pts',(3.99811610699994,12.2,1.03945997699999));
#343864=CARTESIAN_POINT('Ctrl Pts',(3.99811610699994,5.2,1.03945997699999));
#343865=CARTESIAN_POINT('Ctrl Pts',(3.99811610699994,2.2,1.03945997699999));
#343866=CARTESIAN_POINT('Ctrl Pts',(3.99922056899995,12.2,1.04008289899999));
#343867=CARTESIAN_POINT('Ctrl Pts',(3.99922056899995,5.2,1.04008289899999));
#343868=CARTESIAN_POINT('Ctrl Pts',(3.99922056899995,2.2,1.04008289899999));
#343869=CARTESIAN_POINT('Ctrl Pts',(4.00032868299994,12.2,1.04070962899999));
#343870=CARTESIAN_POINT('Ctrl Pts',(4.00032868299994,5.2,1.04070962899999));
#343871=CARTESIAN_POINT('Ctrl Pts',(4.00032868299994,2.2,1.04070962899999));
#343872=CARTESIAN_POINT('Ctrl Pts',(4.00144043399994,12.2,1.04134017399999));
#343873=CARTESIAN_POINT('Ctrl Pts',(4.00144043399994,5.2,1.04134017399999));
#343874=CARTESIAN_POINT('Ctrl Pts',(4.00144043399994,2.2,1.04134017399999));
#343875=CARTESIAN_POINT('Ctrl Pts',(4.00255580899994,12.2,1.04197453899999));
#343876=CARTESIAN_POINT('Ctrl Pts',(4.00255580899994,5.2,1.04197453899999));
#343877=CARTESIAN_POINT('Ctrl Pts',(4.00255580899994,2.2,1.04197453899999));
#343878=CARTESIAN_POINT('Ctrl Pts',(4.00367479199994,12.2,1.04261272799999));
#343879=CARTESIAN_POINT('Ctrl Pts',(4.00367479199994,5.2,1.04261272799999));
#343880=CARTESIAN_POINT('Ctrl Pts',(4.00367479199994,2.2,1.04261272799999));
#343881=CARTESIAN_POINT('Ctrl Pts',(4.00479737099994,12.2,1.04325474599999));
#343882=CARTESIAN_POINT('Ctrl Pts',(4.00479737099994,5.2,1.04325474599999));
#343883=CARTESIAN_POINT('Ctrl Pts',(4.00479737099994,2.2,1.04325474599999));
#343884=CARTESIAN_POINT('Ctrl Pts',(4.00592353199994,12.2,1.04390059899998));
#343885=CARTESIAN_POINT('Ctrl Pts',(4.00592353199994,5.2,1.04390059899998));
#343886=CARTESIAN_POINT('Ctrl Pts',(4.00592353199994,2.2,1.04390059899998));
#343887=CARTESIAN_POINT('Ctrl Pts',(4.00705326099995,12.2,1.04455029199999));
#343888=CARTESIAN_POINT('Ctrl Pts',(4.00705326099995,5.2,1.04455029199999));
#343889=CARTESIAN_POINT('Ctrl Pts',(4.00705326099995,2.2,1.04455029199999));
#343890=CARTESIAN_POINT('Ctrl Pts',(4.00818654499994,12.2,1.04520382899999));
#343891=CARTESIAN_POINT('Ctrl Pts',(4.00818654499994,5.2,1.04520382899999));
#343892=CARTESIAN_POINT('Ctrl Pts',(4.00818654499994,2.2,1.04520382899999));
#343893=CARTESIAN_POINT('Ctrl Pts',(4.00932336999994,12.2,1.04586121499999));
#343894=CARTESIAN_POINT('Ctrl Pts',(4.00932336999994,5.2,1.04586121499999));
#343895=CARTESIAN_POINT('Ctrl Pts',(4.00932336999994,2.2,1.04586121499999));
#343896=CARTESIAN_POINT('Ctrl Pts',(4.01046372199994,12.2,1.04652245599999));
#343897=CARTESIAN_POINT('Ctrl Pts',(4.01046372199994,5.2,1.04652245599999));
#343898=CARTESIAN_POINT('Ctrl Pts',(4.01046372199994,2.2,1.04652245599999));
#343899=CARTESIAN_POINT('Ctrl Pts',(4.01160758699994,12.2,1.04718755599999));
#343900=CARTESIAN_POINT('Ctrl Pts',(4.01160758699994,5.2,1.04718755599999));
#343901=CARTESIAN_POINT('Ctrl Pts',(4.01160758699994,2.2,1.04718755599999));
#343902=CARTESIAN_POINT('Ctrl Pts',(4.01275495299994,12.2,1.04785651999999));
#343903=CARTESIAN_POINT('Ctrl Pts',(4.01275495299994,5.2,1.04785651999999));
#343904=CARTESIAN_POINT('Ctrl Pts',(4.01275495299994,2.2,1.04785651999999));
#343905=CARTESIAN_POINT('Ctrl Pts',(4.01390580599994,12.2,1.04852935399999));
#343906=CARTESIAN_POINT('Ctrl Pts',(4.01390580599994,5.2,1.04852935399999));
#343907=CARTESIAN_POINT('Ctrl Pts',(4.01390580599994,2.2,1.04852935399999));
#343908=CARTESIAN_POINT('Ctrl Pts',(4.01506013099994,12.2,1.04920606099999));
#343909=CARTESIAN_POINT('Ctrl Pts',(4.01506013099994,5.2,1.04920606099999));
#343910=CARTESIAN_POINT('Ctrl Pts',(4.01506013099994,2.2,1.04920606099999));
#343911=CARTESIAN_POINT('Ctrl Pts',(4.01621791599994,12.2,1.04988664599999));
#343912=CARTESIAN_POINT('Ctrl Pts',(4.01621791599994,5.2,1.04988664599999));
#343913=CARTESIAN_POINT('Ctrl Pts',(4.01621791599994,2.2,1.04988664599999));
#343914=CARTESIAN_POINT('Ctrl Pts',(4.01737914599994,12.2,1.05057111399999));
#343915=CARTESIAN_POINT('Ctrl Pts',(4.01737914599994,5.2,1.05057111399999));
#343916=CARTESIAN_POINT('Ctrl Pts',(4.01737914599994,2.2,1.05057111399999));
#343917=CARTESIAN_POINT('Ctrl Pts',(4.01854380999994,12.2,1.05125947099999));
#343918=CARTESIAN_POINT('Ctrl Pts',(4.01854380999994,5.2,1.05125947099999));
#343919=CARTESIAN_POINT('Ctrl Pts',(4.01854380999994,2.2,1.05125947099999));
#343920=CARTESIAN_POINT('Ctrl Pts',(4.01971189299995,12.2,1.05195172099998));
#343921=CARTESIAN_POINT('Ctrl Pts',(4.01971189299995,5.2,1.05195172099998));
#343922=CARTESIAN_POINT('Ctrl Pts',(4.01971189299995,2.2,1.05195172099998));
#343923=CARTESIAN_POINT('Ctrl Pts',(4.02088338099994,12.2,1.05264786699999));
#343924=CARTESIAN_POINT('Ctrl Pts',(4.02088338099994,5.2,1.05264786699999));
#343925=CARTESIAN_POINT('Ctrl Pts',(4.02088338099994,2.2,1.05264786699999));
#343926=CARTESIAN_POINT('Ctrl Pts',(4.02205826199994,12.2,1.05334791499998));
#343927=CARTESIAN_POINT('Ctrl Pts',(4.02205826199994,5.2,1.05334791499998));
#343928=CARTESIAN_POINT('Ctrl Pts',(4.02205826199994,2.2,1.05334791499998));
#343929=CARTESIAN_POINT('Ctrl Pts',(4.02323652199994,12.2,1.05405186999999));
#343930=CARTESIAN_POINT('Ctrl Pts',(4.02323652199994,5.2,1.05405186999999));
#343931=CARTESIAN_POINT('Ctrl Pts',(4.02323652199994,2.2,1.05405186999999));
#343932=CARTESIAN_POINT('Ctrl Pts',(4.02441814699994,12.2,1.05475973599999));
#343933=CARTESIAN_POINT('Ctrl Pts',(4.02441814699994,5.2,1.05475973599999));
#343934=CARTESIAN_POINT('Ctrl Pts',(4.02441814699994,2.2,1.05475973599999));
#343935=CARTESIAN_POINT('Ctrl Pts',(4.02560312399994,12.2,1.05547151799998));
#343936=CARTESIAN_POINT('Ctrl Pts',(4.02560312399994,5.2,1.05547151799998));
#343937=CARTESIAN_POINT('Ctrl Pts',(4.02560312399994,2.2,1.05547151799998));
#343938=CARTESIAN_POINT('Ctrl Pts',(4.02679144099995,12.2,1.05618721999999));
#343939=CARTESIAN_POINT('Ctrl Pts',(4.02679144099995,5.2,1.05618721999999));
#343940=CARTESIAN_POINT('Ctrl Pts',(4.02679144099995,2.2,1.05618721999999));
#343941=CARTESIAN_POINT('Ctrl Pts',(4.02798308299994,12.2,1.05690684699999));
#343942=CARTESIAN_POINT('Ctrl Pts',(4.02798308299994,5.2,1.05690684699999));
#343943=CARTESIAN_POINT('Ctrl Pts',(4.02798308299994,2.2,1.05690684699999));
#343944=CARTESIAN_POINT('Ctrl Pts',(4.02917803799994,12.2,1.05763040199998));
#343945=CARTESIAN_POINT('Ctrl Pts',(4.02917803799994,5.2,1.05763040199998));
#343946=CARTESIAN_POINT('Ctrl Pts',(4.02917803799994,2.2,1.05763040199998));
#343947=CARTESIAN_POINT('Ctrl Pts',(4.03037629099994,12.2,1.05835789199999));
#343948=CARTESIAN_POINT('Ctrl Pts',(4.03037629099994,5.2,1.05835789199999));
#343949=CARTESIAN_POINT('Ctrl Pts',(4.03037629099994,2.2,1.05835789199999));
#343950=CARTESIAN_POINT('Ctrl Pts',(4.03157783099994,12.2,1.05908931899998));
#343951=CARTESIAN_POINT('Ctrl Pts',(4.03157783099994,5.2,1.05908931899998));
#343952=CARTESIAN_POINT('Ctrl Pts',(4.03157783099994,2.2,1.05908931899998));
#343953=CARTESIAN_POINT('Ctrl Pts',(4.03278264399995,12.2,1.05982468899999));
#343954=CARTESIAN_POINT('Ctrl Pts',(4.03278264399995,5.2,1.05982468899999));
#343955=CARTESIAN_POINT('Ctrl Pts',(4.03278264399995,2.2,1.05982468899999));
#343956=CARTESIAN_POINT('Ctrl Pts',(4.03399071699994,12.2,1.06056400499998));
#343957=CARTESIAN_POINT('Ctrl Pts',(4.03399071699994,5.2,1.06056400499998));
#343958=CARTESIAN_POINT('Ctrl Pts',(4.03399071699994,2.2,1.06056400499998));
#343959=CARTESIAN_POINT('Ctrl Pts',(4.03520203599994,12.2,1.06130727299998));
#343960=CARTESIAN_POINT('Ctrl Pts',(4.03520203599994,5.2,1.06130727299998));
#343961=CARTESIAN_POINT('Ctrl Pts',(4.03520203599994,2.2,1.06130727299998));
#343962=CARTESIAN_POINT('Ctrl Pts',(4.03641658799994,12.2,1.06205449599999));
#343963=CARTESIAN_POINT('Ctrl Pts',(4.03641658799994,5.2,1.06205449599999));
#343964=CARTESIAN_POINT('Ctrl Pts',(4.03641658799994,2.2,1.06205449599999));
#343965=CARTESIAN_POINT('Ctrl Pts',(4.03763435999995,12.2,1.06280567799999));
#343966=CARTESIAN_POINT('Ctrl Pts',(4.03763435999995,5.2,1.06280567799999));
#343967=CARTESIAN_POINT('Ctrl Pts',(4.03763435999995,2.2,1.06280567799999));
#343968=CARTESIAN_POINT('Ctrl Pts',(4.03885533999994,12.2,1.06356082499998));
#343969=CARTESIAN_POINT('Ctrl Pts',(4.03885533999994,5.2,1.06356082499998));
#343970=CARTESIAN_POINT('Ctrl Pts',(4.03885533999994,2.2,1.06356082499998));
#343971=CARTESIAN_POINT('Ctrl Pts',(4.04007951299994,12.2,1.06431993999998));
#343972=CARTESIAN_POINT('Ctrl Pts',(4.04007951299994,5.2,1.06431993999998));
#343973=CARTESIAN_POINT('Ctrl Pts',(4.04007951299994,2.2,1.06431993999998));
#343974=CARTESIAN_POINT('Ctrl Pts',(4.04130686699994,12.2,1.06508302599998));
#343975=CARTESIAN_POINT('Ctrl Pts',(4.04130686699994,5.2,1.06508302599998));
#343976=CARTESIAN_POINT('Ctrl Pts',(4.04130686699994,2.2,1.06508302599998));
#343977=CARTESIAN_POINT('Ctrl Pts',(4.04253738999994,12.2,1.06585008899998));
#343978=CARTESIAN_POINT('Ctrl Pts',(4.04253738999994,5.2,1.06585008899998));
#343979=CARTESIAN_POINT('Ctrl Pts',(4.04253738999994,2.2,1.06585008899998));
#343980=CARTESIAN_POINT('Ctrl Pts',(4.04377106799994,12.2,1.06662113399999));
#343981=CARTESIAN_POINT('Ctrl Pts',(4.04377106799994,5.2,1.06662113399999));
#343982=CARTESIAN_POINT('Ctrl Pts',(4.04377106799994,2.2,1.06662113399999));
#343983=CARTESIAN_POINT('Ctrl Pts',(4.04500788799994,12.2,1.06739616299999));
#343984=CARTESIAN_POINT('Ctrl Pts',(4.04500788799994,5.2,1.06739616299999));
#343985=CARTESIAN_POINT('Ctrl Pts',(4.04500788799994,2.2,1.06739616299999));
#343986=CARTESIAN_POINT('Ctrl Pts',(4.04624783599994,12.2,1.06817518099998));
#343987=CARTESIAN_POINT('Ctrl Pts',(4.04624783599994,5.2,1.06817518099998));
#343988=CARTESIAN_POINT('Ctrl Pts',(4.04624783599994,2.2,1.06817518099998));
#343989=CARTESIAN_POINT('Ctrl Pts',(4.04749090199994,12.2,1.06895819199998));
#343990=CARTESIAN_POINT('Ctrl Pts',(4.04749090199994,5.2,1.06895819199998));
#343991=CARTESIAN_POINT('Ctrl Pts',(4.04749090199994,2.2,1.06895819199998));
#343992=CARTESIAN_POINT('Ctrl Pts',(4.04873706999994,12.2,1.06974519899998));
#343993=CARTESIAN_POINT('Ctrl Pts',(4.04873706999994,5.2,1.06974519899998));
#343994=CARTESIAN_POINT('Ctrl Pts',(4.04873706999994,2.2,1.06974519899998));
#343995=CARTESIAN_POINT('Ctrl Pts',(4.04998632799995,12.2,1.07053620799999));
#343996=CARTESIAN_POINT('Ctrl Pts',(4.04998632799995,5.2,1.07053620799999));
#343997=CARTESIAN_POINT('Ctrl Pts',(4.04998632799995,2.2,1.07053620799999));
#343998=CARTESIAN_POINT('Ctrl Pts',(4.05123866399994,12.2,1.07133122099999));
#343999=CARTESIAN_POINT('Ctrl Pts',(4.05123866399994,5.2,1.07133122099999));
#344000=CARTESIAN_POINT('Ctrl Pts',(4.05123866399994,2.2,1.07133122099999));
#344001=CARTESIAN_POINT('Ctrl Pts',(4.05249406499994,12.2,1.07213024499998));
#344002=CARTESIAN_POINT('Ctrl Pts',(4.05249406499994,5.2,1.07213024499998));
#344003=CARTESIAN_POINT('Ctrl Pts',(4.05249406499994,2.2,1.07213024499998));
#344004=CARTESIAN_POINT('Ctrl Pts',(4.05375251799994,12.2,1.07293327999999));
#344005=CARTESIAN_POINT('Ctrl Pts',(4.05375251799994,5.2,1.07293327999999));
#344006=CARTESIAN_POINT('Ctrl Pts',(4.05375251799994,2.2,1.07293327999999));
#344007=CARTESIAN_POINT('Ctrl Pts',(4.05501400899994,12.2,1.07374033199998));
#344008=CARTESIAN_POINT('Ctrl Pts',(4.05501400899994,5.2,1.07374033199998));
#344009=CARTESIAN_POINT('Ctrl Pts',(4.05501400899994,2.2,1.07374033199998));
#344010=CARTESIAN_POINT('Ctrl Pts',(4.05627852699994,12.2,1.07455140599999));
#344011=CARTESIAN_POINT('Ctrl Pts',(4.05627852699994,5.2,1.07455140599999));
#344012=CARTESIAN_POINT('Ctrl Pts',(4.05627852699994,2.2,1.07455140599999));
#344013=CARTESIAN_POINT('Ctrl Pts',(4.05754605799994,12.2,1.07536650399998));
#344014=CARTESIAN_POINT('Ctrl Pts',(4.05754605799994,5.2,1.07536650399998));
#344015=CARTESIAN_POINT('Ctrl Pts',(4.05754605799994,2.2,1.07536650399998));
#344016=CARTESIAN_POINT('Ctrl Pts',(4.05881658999994,12.2,1.07618562999999));
#344017=CARTESIAN_POINT('Ctrl Pts',(4.05881658999994,5.2,1.07618562999999));
#344018=CARTESIAN_POINT('Ctrl Pts',(4.05881658999994,2.2,1.07618562999999));
#344019=CARTESIAN_POINT('Ctrl Pts',(4.06009010899994,12.2,1.07700878899998));
#344020=CARTESIAN_POINT('Ctrl Pts',(4.06009010899994,5.2,1.07700878899998));
#344021=CARTESIAN_POINT('Ctrl Pts',(4.06009010899994,2.2,1.07700878899998));
#344022=CARTESIAN_POINT('Ctrl Pts',(4.06136660399994,12.2,1.07783598399998));
#344023=CARTESIAN_POINT('Ctrl Pts',(4.06136660399994,5.2,1.07783598399998));
#344024=CARTESIAN_POINT('Ctrl Pts',(4.06136660399994,2.2,1.07783598399998));
#344025=CARTESIAN_POINT('Ctrl Pts',(4.06264606199994,12.2,1.07866721799999));
#344026=CARTESIAN_POINT('Ctrl Pts',(4.06264606199994,5.2,1.07866721799999));
#344027=CARTESIAN_POINT('Ctrl Pts',(4.06264606199994,2.2,1.07866721799999));
#344028=CARTESIAN_POINT('Ctrl Pts',(4.06392846999994,12.2,1.07950249699998));
#344029=CARTESIAN_POINT('Ctrl Pts',(4.06392846999994,5.2,1.07950249699998));
#344030=CARTESIAN_POINT('Ctrl Pts',(4.06392846999994,2.2,1.07950249699998));
#344031=CARTESIAN_POINT('Ctrl Pts',(4.06521381399994,12.2,1.08034182199999));
#344032=CARTESIAN_POINT('Ctrl Pts',(4.06521381399994,5.2,1.08034182199999));
#344033=CARTESIAN_POINT('Ctrl Pts',(4.06521381399994,2.2,1.08034182199999));
#344034=CARTESIAN_POINT('Ctrl Pts',(4.06650208399994,12.2,1.08118519899998));
#344035=CARTESIAN_POINT('Ctrl Pts',(4.06650208399994,5.2,1.08118519899998));
#344036=CARTESIAN_POINT('Ctrl Pts',(4.06650208399994,2.2,1.08118519899998));
#344037=CARTESIAN_POINT('Ctrl Pts',(4.06779326599994,12.2,1.08203262999998));
#344038=CARTESIAN_POINT('Ctrl Pts',(4.06779326599994,5.2,1.08203262999998));
#344039=CARTESIAN_POINT('Ctrl Pts',(4.06779326599994,2.2,1.08203262999998));
#344040=CARTESIAN_POINT('Ctrl Pts',(4.06908734599994,12.2,1.08288411999999));
#344041=CARTESIAN_POINT('Ctrl Pts',(4.06908734599994,5.2,1.08288411999999));
#344042=CARTESIAN_POINT('Ctrl Pts',(4.06908734599994,2.2,1.08288411999999));
#344043=CARTESIAN_POINT('Ctrl Pts',(4.07038431399994,12.2,1.08373967099999));
#344044=CARTESIAN_POINT('Ctrl Pts',(4.07038431399994,5.2,1.08373967099999));
#344045=CARTESIAN_POINT('Ctrl Pts',(4.07038431399994,2.2,1.08373967099999));
#344046=CARTESIAN_POINT('Ctrl Pts',(4.07168415599994,12.2,1.08459928899999));
#344047=CARTESIAN_POINT('Ctrl Pts',(4.07168415599994,5.2,1.08459928899999));
#344048=CARTESIAN_POINT('Ctrl Pts',(4.07168415599994,2.2,1.08459928899999));
#344049=CARTESIAN_POINT('Ctrl Pts',(4.07298685999994,12.2,1.08546297499998));
#344050=CARTESIAN_POINT('Ctrl Pts',(4.07298685999994,5.2,1.08546297499998));
#344051=CARTESIAN_POINT('Ctrl Pts',(4.07298685999994,2.2,1.08546297499998));
#344052=CARTESIAN_POINT('Ctrl Pts',(4.07429241299995,12.2,1.08633073399998));
#344053=CARTESIAN_POINT('Ctrl Pts',(4.07429241299995,5.2,1.08633073399998));
#344054=CARTESIAN_POINT('Ctrl Pts',(4.07429241299995,2.2,1.08633073399998));
#344055=CARTESIAN_POINT('Ctrl Pts',(4.07560080199994,12.2,1.08720256999999));
#344056=CARTESIAN_POINT('Ctrl Pts',(4.07560080199994,5.2,1.08720256999999));
#344057=CARTESIAN_POINT('Ctrl Pts',(4.07560080199994,2.2,1.08720256999999));
#344058=CARTESIAN_POINT('Ctrl Pts',(4.07691201699994,12.2,1.08807848499998));
#344059=CARTESIAN_POINT('Ctrl Pts',(4.07691201699994,5.2,1.08807848499998));
#344060=CARTESIAN_POINT('Ctrl Pts',(4.07691201699994,2.2,1.08807848499998));
#344061=CARTESIAN_POINT('Ctrl Pts',(4.07822604299994,12.2,1.08895848199999));
#344062=CARTESIAN_POINT('Ctrl Pts',(4.07822604299994,5.2,1.08895848199999));
#344063=CARTESIAN_POINT('Ctrl Pts',(4.07822604299994,2.2,1.08895848199999));
#344064=CARTESIAN_POINT('Ctrl Pts',(4.07954286799994,12.2,1.08984256799999));
#344065=CARTESIAN_POINT('Ctrl Pts',(4.07954286799994,5.2,1.08984256799999));
#344066=CARTESIAN_POINT('Ctrl Pts',(4.07954286799994,2.2,1.08984256799999));
#344067=CARTESIAN_POINT('Ctrl Pts',(4.08086248099994,12.2,1.09073074299999));
#344068=CARTESIAN_POINT('Ctrl Pts',(4.08086248099994,5.2,1.09073074299999));
#344069=CARTESIAN_POINT('Ctrl Pts',(4.08086248099994,2.2,1.09073074299999));
#344070=CARTESIAN_POINT('Ctrl Pts',(4.08218486799994,12.2,1.09162301099999));
#344071=CARTESIAN_POINT('Ctrl Pts',(4.08218486799994,5.2,1.09162301099999));
#344072=CARTESIAN_POINT('Ctrl Pts',(4.08218486799994,2.2,1.09162301099999));
#344073=CARTESIAN_POINT('Ctrl Pts',(4.08351001799994,12.2,1.09251937699999));
#344074=CARTESIAN_POINT('Ctrl Pts',(4.08351001799994,5.2,1.09251937699999));
#344075=CARTESIAN_POINT('Ctrl Pts',(4.08351001799994,2.2,1.09251937699999));
#344076=CARTESIAN_POINT('Ctrl Pts',(4.08483791699994,12.2,1.09341984299999));
#344077=CARTESIAN_POINT('Ctrl Pts',(4.08483791699994,5.2,1.09341984299999));
#344078=CARTESIAN_POINT('Ctrl Pts',(4.08483791699994,2.2,1.09341984299999));
#344079=CARTESIAN_POINT('Ctrl Pts',(4.08616855399995,12.2,1.09432441199999));
#344080=CARTESIAN_POINT('Ctrl Pts',(4.08616855399995,5.2,1.09432441199999));
#344081=CARTESIAN_POINT('Ctrl Pts',(4.08616855399995,2.2,1.09432441199999));
#344082=CARTESIAN_POINT('Ctrl Pts',(4.08750191699994,12.2,1.09523308899998));
#344083=CARTESIAN_POINT('Ctrl Pts',(4.08750191699994,5.2,1.09523308899998));
#344084=CARTESIAN_POINT('Ctrl Pts',(4.08750191699994,2.2,1.09523308899998));
#344085=CARTESIAN_POINT('Ctrl Pts',(4.08883799199994,12.2,1.09614587499999));
#344086=CARTESIAN_POINT('Ctrl Pts',(4.08883799199994,5.2,1.09614587499999));
#344087=CARTESIAN_POINT('Ctrl Pts',(4.08883799199994,2.2,1.09614587499999));
#344088=CARTESIAN_POINT('Ctrl Pts',(4.09017676799994,12.2,1.09706277699999));
#344089=CARTESIAN_POINT('Ctrl Pts',(4.09017676799994,5.2,1.09706277699999));
#344090=CARTESIAN_POINT('Ctrl Pts',(4.09017676799994,2.2,1.09706277699999));
#344091=CARTESIAN_POINT('Ctrl Pts',(4.09151823199995,12.2,1.09798379399999));
#344092=CARTESIAN_POINT('Ctrl Pts',(4.09151823199995,5.2,1.09798379399999));
#344093=CARTESIAN_POINT('Ctrl Pts',(4.09151823199995,2.2,1.09798379399999));
#344094=CARTESIAN_POINT('Ctrl Pts',(4.09286237299994,12.2,1.09890893099998));
#344095=CARTESIAN_POINT('Ctrl Pts',(4.09286237299994,5.2,1.09890893099998));
#344096=CARTESIAN_POINT('Ctrl Pts',(4.09286237299994,2.2,1.09890893099998));
#344097=CARTESIAN_POINT('Ctrl Pts',(4.09420917799994,12.2,1.09983819099998));
#344098=CARTESIAN_POINT('Ctrl Pts',(4.09420917799994,5.2,1.09983819099998));
#344099=CARTESIAN_POINT('Ctrl Pts',(4.09420917799994,2.2,1.09983819099998));
#344100=CARTESIAN_POINT('Ctrl Pts',(4.09555863499994,12.2,1.10077157799998));
#344101=CARTESIAN_POINT('Ctrl Pts',(4.09555863499994,5.2,1.10077157799998));
#344102=CARTESIAN_POINT('Ctrl Pts',(4.09555863499994,2.2,1.10077157799998));
#344103=CARTESIAN_POINT('Ctrl Pts',(4.09691072999994,12.2,1.10170909499999));
#344104=CARTESIAN_POINT('Ctrl Pts',(4.09691072999994,5.2,1.10170909499999));
#344105=CARTESIAN_POINT('Ctrl Pts',(4.09691072999994,2.2,1.10170909499999));
#344106=CARTESIAN_POINT('Ctrl Pts',(4.09826545399994,12.2,1.10265074399999));
#344107=CARTESIAN_POINT('Ctrl Pts',(4.09826545399994,5.2,1.10265074399999));
#344108=CARTESIAN_POINT('Ctrl Pts',(4.09826545399994,2.2,1.10265074399999));
#344109=CARTESIAN_POINT('Ctrl Pts',(4.09962279199994,12.2,1.10359652899998));
#344110=CARTESIAN_POINT('Ctrl Pts',(4.09962279199994,5.2,1.10359652899998));
#344111=CARTESIAN_POINT('Ctrl Pts',(4.09962279199994,2.2,1.10359652899998));
#344112=CARTESIAN_POINT('Ctrl Pts',(4.10098273499994,12.2,1.10454645299999));
#344113=CARTESIAN_POINT('Ctrl Pts',(4.10098273499994,5.2,1.10454645299999));
#344114=CARTESIAN_POINT('Ctrl Pts',(4.10098273499994,2.2,1.10454645299999));
#344115=CARTESIAN_POINT('Ctrl Pts',(4.10234526799994,12.2,1.10550051799999));
#344116=CARTESIAN_POINT('Ctrl Pts',(4.10234526799994,5.2,1.10550051799999));
#344117=CARTESIAN_POINT('Ctrl Pts',(4.10234526799994,2.2,1.10550051799999));
#344118=CARTESIAN_POINT('Ctrl Pts',(4.10371038099994,12.2,1.10645872899998));
#344119=CARTESIAN_POINT('Ctrl Pts',(4.10371038099994,5.2,1.10645872899998));
#344120=CARTESIAN_POINT('Ctrl Pts',(4.10371038099994,2.2,1.10645872899998));
#344121=CARTESIAN_POINT('Ctrl Pts',(4.10507805999995,12.2,1.10742108799998));
#344122=CARTESIAN_POINT('Ctrl Pts',(4.10507805999995,5.2,1.10742108799998));
#344123=CARTESIAN_POINT('Ctrl Pts',(4.10507805999995,2.2,1.10742108799998));
#344124=CARTESIAN_POINT('Ctrl Pts',(4.10644829399994,12.2,1.10838759899998));
#344125=CARTESIAN_POINT('Ctrl Pts',(4.10644829399994,5.2,1.10838759899998));
#344126=CARTESIAN_POINT('Ctrl Pts',(4.10644829399994,2.2,1.10838759899998));
#344127=CARTESIAN_POINT('Ctrl Pts',(4.10782107099994,12.2,1.10935826299999));
#344128=CARTESIAN_POINT('Ctrl Pts',(4.10782107099994,5.2,1.10935826299999));
#344129=CARTESIAN_POINT('Ctrl Pts',(4.10782107099994,2.2,1.10935826299999));
#344130=CARTESIAN_POINT('Ctrl Pts',(4.10919637799994,12.2,1.11033308499998));
#344131=CARTESIAN_POINT('Ctrl Pts',(4.10919637799994,5.2,1.11033308499998));
#344132=CARTESIAN_POINT('Ctrl Pts',(4.10919637799994,2.2,1.11033308499998));
#344133=CARTESIAN_POINT('Ctrl Pts',(4.11057420499994,12.2,1.11131206599998));
#344134=CARTESIAN_POINT('Ctrl Pts',(4.11057420499994,5.2,1.11131206599998));
#344135=CARTESIAN_POINT('Ctrl Pts',(4.11057420499994,2.2,1.11131206599998));
#344136=CARTESIAN_POINT('Ctrl Pts',(4.11195453799994,12.2,1.11229520999998));
#344137=CARTESIAN_POINT('Ctrl Pts',(4.11195453799994,5.2,1.11229520999998));
#344138=CARTESIAN_POINT('Ctrl Pts',(4.11195453799994,2.2,1.11229520999998));
#344139=CARTESIAN_POINT('Ctrl Pts',(4.11333736599994,12.2,1.11328251999999));
#344140=CARTESIAN_POINT('Ctrl Pts',(4.11333736599994,5.2,1.11328251999999));
#344141=CARTESIAN_POINT('Ctrl Pts',(4.11333736599994,2.2,1.11328251999999));
#344142=CARTESIAN_POINT('Ctrl Pts',(4.11472267799994,12.2,1.11427399899998));
#344143=CARTESIAN_POINT('Ctrl Pts',(4.11472267799994,5.2,1.11427399899998));
#344144=CARTESIAN_POINT('Ctrl Pts',(4.11472267799994,2.2,1.11427399899998));
#344145=CARTESIAN_POINT('Ctrl Pts',(4.11611045999994,12.2,1.11526964999999));
#344146=CARTESIAN_POINT('Ctrl Pts',(4.11611045999994,5.2,1.11526964999999));
#344147=CARTESIAN_POINT('Ctrl Pts',(4.11611045999994,2.2,1.11526964999999));
#344148=CARTESIAN_POINT('Ctrl Pts',(4.11750070199994,12.2,1.11626947399999));
#344149=CARTESIAN_POINT('Ctrl Pts',(4.11750070199994,5.2,1.11626947399999));
#344150=CARTESIAN_POINT('Ctrl Pts',(4.11750070199994,2.2,1.11626947399999));
#344151=CARTESIAN_POINT('Ctrl Pts',(4.11889338999995,12.2,1.11727347599999));
#344152=CARTESIAN_POINT('Ctrl Pts',(4.11889338999995,5.2,1.11727347599999));
#344153=CARTESIAN_POINT('Ctrl Pts',(4.11889338999995,2.2,1.11727347599999));
#344154=CARTESIAN_POINT('Ctrl Pts',(4.12028851399994,12.2,1.11828165799999));
#344155=CARTESIAN_POINT('Ctrl Pts',(4.12028851399994,5.2,1.11828165799999));
#344156=CARTESIAN_POINT('Ctrl Pts',(4.12028851399994,2.2,1.11828165799999));
#344157=CARTESIAN_POINT('Ctrl Pts',(4.12168606199994,12.2,1.11929402299999));
#344158=CARTESIAN_POINT('Ctrl Pts',(4.12168606199994,5.2,1.11929402299999));
#344159=CARTESIAN_POINT('Ctrl Pts',(4.12168606199994,2.2,1.11929402299999));
#344160=CARTESIAN_POINT('Ctrl Pts',(4.12308602099994,12.2,1.12031057299999));
#344161=CARTESIAN_POINT('Ctrl Pts',(4.12308602099994,5.2,1.12031057299999));
#344162=CARTESIAN_POINT('Ctrl Pts',(4.12308602099994,2.2,1.12031057299999));
#344163=CARTESIAN_POINT('Ctrl Pts',(4.12448838099994,12.2,1.12133131199998));
#344164=CARTESIAN_POINT('Ctrl Pts',(4.12448838099994,5.2,1.12133131199998));
#344165=CARTESIAN_POINT('Ctrl Pts',(4.12448838099994,2.2,1.12133131199998));
#344166=CARTESIAN_POINT('Ctrl Pts',(4.12589312799994,12.2,1.12235624199998));
#344167=CARTESIAN_POINT('Ctrl Pts',(4.12589312799994,5.2,1.12235624199998));
#344168=CARTESIAN_POINT('Ctrl Pts',(4.12589312799994,2.2,1.12235624199998));
#344169=CARTESIAN_POINT('Ctrl Pts',(4.12730025099994,12.2,1.12338536399998));
#344170=CARTESIAN_POINT('Ctrl Pts',(4.12730025099994,5.2,1.12338536399998));
#344171=CARTESIAN_POINT('Ctrl Pts',(4.12730025099994,2.2,1.12338536399998));
#344172=CARTESIAN_POINT('Ctrl Pts',(4.12870973899994,12.2,1.12441868399999));
#344173=CARTESIAN_POINT('Ctrl Pts',(4.12870973899994,5.2,1.12441868399999));
#344174=CARTESIAN_POINT('Ctrl Pts',(4.12870973899994,2.2,1.12441868399999));
#344175=CARTESIAN_POINT('Ctrl Pts',(4.13012157999994,12.2,1.12545620199999));
#344176=CARTESIAN_POINT('Ctrl Pts',(4.13012157999994,5.2,1.12545620199999));
#344177=CARTESIAN_POINT('Ctrl Pts',(4.13012157999994,2.2,1.12545620199999));
#344178=CARTESIAN_POINT('Ctrl Pts',(4.13153576199994,12.2,1.12649792199999));
#344179=CARTESIAN_POINT('Ctrl Pts',(4.13153576199994,5.2,1.12649792199999));
#344180=CARTESIAN_POINT('Ctrl Pts',(4.13153576199994,2.2,1.12649792199999));
#344181=CARTESIAN_POINT('Ctrl Pts',(4.13295227299994,12.2,1.12754384699999));
#344182=CARTESIAN_POINT('Ctrl Pts',(4.13295227299994,5.2,1.12754384699999));
#344183=CARTESIAN_POINT('Ctrl Pts',(4.13295227299994,2.2,1.12754384699999));
#344184=CARTESIAN_POINT('Ctrl Pts',(4.13437110199994,12.2,1.12859397699999));
#344185=CARTESIAN_POINT('Ctrl Pts',(4.13437110199994,5.2,1.12859397699999));
#344186=CARTESIAN_POINT('Ctrl Pts',(4.13437110199994,2.2,1.12859397699999));
#344187=CARTESIAN_POINT('Ctrl Pts',(4.13579223699994,12.2,1.12964831799998));
#344188=CARTESIAN_POINT('Ctrl Pts',(4.13579223699994,5.2,1.12964831799998));
#344189=CARTESIAN_POINT('Ctrl Pts',(4.13579223699994,2.2,1.12964831799998));
#344190=CARTESIAN_POINT('Ctrl Pts',(4.13721566599994,12.2,1.13070686999999));
#344191=CARTESIAN_POINT('Ctrl Pts',(4.13721566599994,5.2,1.13070686999999));
#344192=CARTESIAN_POINT('Ctrl Pts',(4.13721566599994,2.2,1.13070686999999));
#344193=CARTESIAN_POINT('Ctrl Pts',(4.13864137799994,12.2,1.13176963599999));
#344194=CARTESIAN_POINT('Ctrl Pts',(4.13864137799994,5.2,1.13176963599999));
#344195=CARTESIAN_POINT('Ctrl Pts',(4.13864137799994,2.2,1.13176963599999));
#344196=CARTESIAN_POINT('Ctrl Pts',(4.14006936099994,12.2,1.13283661899999));
#344197=CARTESIAN_POINT('Ctrl Pts',(4.14006936099994,5.2,1.13283661899999));
#344198=CARTESIAN_POINT('Ctrl Pts',(4.14006936099994,2.2,1.13283661899999));
#344199=CARTESIAN_POINT('Ctrl Pts',(4.14149960399994,12.2,1.13390782299998));
#344200=CARTESIAN_POINT('Ctrl Pts',(4.14149960399994,5.2,1.13390782299998));
#344201=CARTESIAN_POINT('Ctrl Pts',(4.14149960399994,2.2,1.13390782299998));
#344202=CARTESIAN_POINT('Ctrl Pts',(4.14293209399994,12.2,1.13498324699998));
#344203=CARTESIAN_POINT('Ctrl Pts',(4.14293209399994,5.2,1.13498324699998));
#344204=CARTESIAN_POINT('Ctrl Pts',(4.14293209399994,2.2,1.13498324699998));
#344205=CARTESIAN_POINT('Ctrl Pts',(4.14436682099994,12.2,1.13606289599999));
#344206=CARTESIAN_POINT('Ctrl Pts',(4.14436682099994,5.2,1.13606289599999));
#344207=CARTESIAN_POINT('Ctrl Pts',(4.14436682099994,2.2,1.13606289599999));
#344208=CARTESIAN_POINT('Ctrl Pts',(4.14580377199994,12.2,1.13714677199999));
#344209=CARTESIAN_POINT('Ctrl Pts',(4.14580377199994,5.2,1.13714677199999));
#344210=CARTESIAN_POINT('Ctrl Pts',(4.14580377199994,2.2,1.13714677199999));
#344211=CARTESIAN_POINT('Ctrl Pts',(4.14724293699994,12.2,1.13823487699999));
#344212=CARTESIAN_POINT('Ctrl Pts',(4.14724293699994,5.2,1.13823487699999));
#344213=CARTESIAN_POINT('Ctrl Pts',(4.14724293699994,2.2,1.13823487699999));
#344214=CARTESIAN_POINT('Ctrl Pts',(4.14868430299994,12.2,1.13932721399999));
#344215=CARTESIAN_POINT('Ctrl Pts',(4.14868430299994,5.2,1.13932721399999));
#344216=CARTESIAN_POINT('Ctrl Pts',(4.14868430299994,2.2,1.13932721399999));
#344217=CARTESIAN_POINT('Ctrl Pts',(4.15012785899994,12.2,1.14042378299999));
#344218=CARTESIAN_POINT('Ctrl Pts',(4.15012785899994,5.2,1.14042378299999));
#344219=CARTESIAN_POINT('Ctrl Pts',(4.15012785899994,2.2,1.14042378299999));
#344220=CARTESIAN_POINT('Ctrl Pts',(4.15157359399995,12.2,1.14152458999999));
#344221=CARTESIAN_POINT('Ctrl Pts',(4.15157359399995,5.2,1.14152458999999));
#344222=CARTESIAN_POINT('Ctrl Pts',(4.15157359399995,2.2,1.14152458999999));
#344223=CARTESIAN_POINT('Ctrl Pts',(4.15302149599994,12.2,1.14262963499999));
#344224=CARTESIAN_POINT('Ctrl Pts',(4.15302149599994,5.2,1.14262963499999));
#344225=CARTESIAN_POINT('Ctrl Pts',(4.15302149599994,2.2,1.14262963499999));
#344226=CARTESIAN_POINT('Ctrl Pts',(4.15447155399994,12.2,1.14373892099998));
#344227=CARTESIAN_POINT('Ctrl Pts',(4.15447155399994,5.2,1.14373892099998));
#344228=CARTESIAN_POINT('Ctrl Pts',(4.15447155399994,2.2,1.14373892099998));
#344229=CARTESIAN_POINT('Ctrl Pts',(4.15592375599994,12.2,1.14485244999999));
#344230=CARTESIAN_POINT('Ctrl Pts',(4.15592375599994,5.2,1.14485244999999));
#344231=CARTESIAN_POINT('Ctrl Pts',(4.15592375599994,2.2,1.14485244999999));
#344232=CARTESIAN_POINT('Ctrl Pts',(4.15737809199995,12.2,1.14597022399999));
#344233=CARTESIAN_POINT('Ctrl Pts',(4.15737809199995,5.2,1.14597022399999));
#344234=CARTESIAN_POINT('Ctrl Pts',(4.15737809199995,2.2,1.14597022399999));
#344235=CARTESIAN_POINT('Ctrl Pts',(4.15883454899994,12.2,1.14709224599999));
#344236=CARTESIAN_POINT('Ctrl Pts',(4.15883454899994,5.2,1.14709224599999));
#344237=CARTESIAN_POINT('Ctrl Pts',(4.15883454899994,2.2,1.14709224599999));
#344238=CARTESIAN_POINT('Ctrl Pts',(4.16029311599995,12.2,1.14821851799999));
#344239=CARTESIAN_POINT('Ctrl Pts',(4.16029311599995,5.2,1.14821851799999));
#344240=CARTESIAN_POINT('Ctrl Pts',(4.16029311599995,2.2,1.14821851799999));
#344241=CARTESIAN_POINT('Ctrl Pts',(4.16175377999994,12.2,1.14934904099998));
#344242=CARTESIAN_POINT('Ctrl Pts',(4.16175377999994,5.2,1.14934904099998));
#344243=CARTESIAN_POINT('Ctrl Pts',(4.16175377999994,2.2,1.14934904099998));
#344244=CARTESIAN_POINT('Ctrl Pts',(4.16321653299994,12.2,1.15048381999999));
#344245=CARTESIAN_POINT('Ctrl Pts',(4.16321653299994,5.2,1.15048381999999));
#344246=CARTESIAN_POINT('Ctrl Pts',(4.16321653299994,2.2,1.15048381999999));
#344247=CARTESIAN_POINT('Ctrl Pts',(4.16468136199994,12.2,1.15162285499999));
#344248=CARTESIAN_POINT('Ctrl Pts',(4.16468136199994,5.2,1.15162285499999));
#344249=CARTESIAN_POINT('Ctrl Pts',(4.16468136199994,2.2,1.15162285499999));
#344250=CARTESIAN_POINT('Ctrl Pts',(4.16614825599994,12.2,1.15276614799999));
#344251=CARTESIAN_POINT('Ctrl Pts',(4.16614825599994,5.2,1.15276614799999));
#344252=CARTESIAN_POINT('Ctrl Pts',(4.16614825599994,2.2,1.15276614799999));
#344253=CARTESIAN_POINT('Ctrl Pts',(4.16761720299994,12.2,1.15391370199998));
#344254=CARTESIAN_POINT('Ctrl Pts',(4.16761720299994,5.2,1.15391370199998));
#344255=CARTESIAN_POINT('Ctrl Pts',(4.16761720299994,2.2,1.15391370199998));
#344256=CARTESIAN_POINT('Ctrl Pts',(4.16908819199994,12.2,1.15506551899998));
#344257=CARTESIAN_POINT('Ctrl Pts',(4.16908819199994,5.2,1.15506551899998));
#344258=CARTESIAN_POINT('Ctrl Pts',(4.16908819199994,2.2,1.15506551899998));
#344259=CARTESIAN_POINT('Ctrl Pts',(4.17056121199994,12.2,1.15622159999999));
#344260=CARTESIAN_POINT('Ctrl Pts',(4.17056121199994,5.2,1.15622159999999));
#344261=CARTESIAN_POINT('Ctrl Pts',(4.17056121199994,2.2,1.15622159999999));
#344262=CARTESIAN_POINT('Ctrl Pts',(4.17203625199994,12.2,1.15738194899999));
#344263=CARTESIAN_POINT('Ctrl Pts',(4.17203625199994,5.2,1.15738194899999));
#344264=CARTESIAN_POINT('Ctrl Pts',(4.17203625199994,2.2,1.15738194899999));
#344265=CARTESIAN_POINT('Ctrl Pts',(4.17351329999994,12.2,1.15854656699999));
#344266=CARTESIAN_POINT('Ctrl Pts',(4.17351329999994,5.2,1.15854656699999));
#344267=CARTESIAN_POINT('Ctrl Pts',(4.17351329999994,2.2,1.15854656699999));
#344268=CARTESIAN_POINT('Ctrl Pts',(4.17499234499994,12.2,1.15971545599999));
#344269=CARTESIAN_POINT('Ctrl Pts',(4.17499234499994,5.2,1.15971545599999));
#344270=CARTESIAN_POINT('Ctrl Pts',(4.17499234499994,2.2,1.15971545599999));
#344271=CARTESIAN_POINT('Ctrl Pts',(4.17647337599994,12.2,1.16088861699998));
#344272=CARTESIAN_POINT('Ctrl Pts',(4.17647337599994,5.2,1.16088861699998));
#344273=CARTESIAN_POINT('Ctrl Pts',(4.17647337599994,2.2,1.16088861699998));
#344274=CARTESIAN_POINT('Ctrl Pts',(4.17795638199994,12.2,1.16206605399999));
#344275=CARTESIAN_POINT('Ctrl Pts',(4.17795638199994,5.2,1.16206605399999));
#344276=CARTESIAN_POINT('Ctrl Pts',(4.17795638199994,2.2,1.16206605399999));
#344277=CARTESIAN_POINT('Ctrl Pts',(4.17944135099994,12.2,1.16324776899999));
#344278=CARTESIAN_POINT('Ctrl Pts',(4.17944135099994,5.2,1.16324776899999));
#344279=CARTESIAN_POINT('Ctrl Pts',(4.17944135099994,2.2,1.16324776899999));
#344280=CARTESIAN_POINT('Ctrl Pts',(4.18092827299995,12.2,1.16443376099999));
#344281=CARTESIAN_POINT('Ctrl Pts',(4.18092827299995,5.2,1.16443376099999));
#344282=CARTESIAN_POINT('Ctrl Pts',(4.18092827299995,2.2,1.16443376099999));
#344283=CARTESIAN_POINT('Ctrl Pts',(4.18241713599994,12.2,1.16562403599998));
#344284=CARTESIAN_POINT('Ctrl Pts',(4.18241713599994,5.2,1.16562403599998));
#344285=CARTESIAN_POINT('Ctrl Pts',(4.18241713599994,2.2,1.16562403599998));
#344286=CARTESIAN_POINT('Ctrl Pts',(4.18390792899995,12.2,1.16681859199999));
#344287=CARTESIAN_POINT('Ctrl Pts',(4.18390792899995,5.2,1.16681859199999));
#344288=CARTESIAN_POINT('Ctrl Pts',(4.18390792899995,2.2,1.16681859199999));
#344289=CARTESIAN_POINT('Ctrl Pts',(4.18540064099994,12.2,1.16801743399999));
#344290=CARTESIAN_POINT('Ctrl Pts',(4.18540064099994,5.2,1.16801743399999));
#344291=CARTESIAN_POINT('Ctrl Pts',(4.18540064099994,2.2,1.16801743399999));
#344292=CARTESIAN_POINT('Ctrl Pts',(4.18689526199994,12.2,1.16922056299999));
#344293=CARTESIAN_POINT('Ctrl Pts',(4.18689526199994,5.2,1.16922056299999));
#344294=CARTESIAN_POINT('Ctrl Pts',(4.18689526199994,2.2,1.16922056299999));
#344295=CARTESIAN_POINT('Ctrl Pts',(4.18839177799994,12.2,1.17042797999999));
#344296=CARTESIAN_POINT('Ctrl Pts',(4.18839177799994,5.2,1.17042797999999));
#344297=CARTESIAN_POINT('Ctrl Pts',(4.18839177799994,2.2,1.17042797999999));
#344298=CARTESIAN_POINT('Ctrl Pts',(4.18989018099994,12.2,1.17163968799999));
#344299=CARTESIAN_POINT('Ctrl Pts',(4.18989018099994,5.2,1.17163968799999));
#344300=CARTESIAN_POINT('Ctrl Pts',(4.18989018099994,2.2,1.17163968799999));
#344301=CARTESIAN_POINT('Ctrl Pts',(4.19139045799994,12.2,1.17285568699999));
#344302=CARTESIAN_POINT('Ctrl Pts',(4.19139045799994,5.2,1.17285568699999));
#344303=CARTESIAN_POINT('Ctrl Pts',(4.19139045799994,2.2,1.17285568699999));
#344304=CARTESIAN_POINT('Ctrl Pts',(4.19289259999994,12.2,1.17407598099998));
#344305=CARTESIAN_POINT('Ctrl Pts',(4.19289259999994,5.2,1.17407598099998));
#344306=CARTESIAN_POINT('Ctrl Pts',(4.19289259999994,2.2,1.17407598099998));
#344307=CARTESIAN_POINT('Ctrl Pts',(4.19439659299994,12.2,1.17530057099998));
#344308=CARTESIAN_POINT('Ctrl Pts',(4.19439659299994,5.2,1.17530057099998));
#344309=CARTESIAN_POINT('Ctrl Pts',(4.19439659299994,2.2,1.17530057099998));
#344310=CARTESIAN_POINT('Ctrl Pts',(4.19590242799995,12.2,1.17652945699998));
#344311=CARTESIAN_POINT('Ctrl Pts',(4.19590242799995,5.2,1.17652945699998));
#344312=CARTESIAN_POINT('Ctrl Pts',(4.19590242799995,2.2,1.17652945699998));
#344313=CARTESIAN_POINT('Ctrl Pts',(4.19741009499994,12.2,1.17776264499998));
#344314=CARTESIAN_POINT('Ctrl Pts',(4.19741009499994,5.2,1.17776264499998));
#344315=CARTESIAN_POINT('Ctrl Pts',(4.19741009499994,2.2,1.17776264499998));
#344316=CARTESIAN_POINT('Ctrl Pts',(4.19891957999995,12.2,1.17900013199999));
#344317=CARTESIAN_POINT('Ctrl Pts',(4.19891957999995,5.2,1.17900013199999));
#344318=CARTESIAN_POINT('Ctrl Pts',(4.19891957999995,2.2,1.17900013199999));
#344319=CARTESIAN_POINT('Ctrl Pts',(4.20043087499994,12.2,1.18024192399998));
#344320=CARTESIAN_POINT('Ctrl Pts',(4.20043087499994,5.2,1.18024192399998));
#344321=CARTESIAN_POINT('Ctrl Pts',(4.20043087499994,2.2,1.18024192399998));
#344322=CARTESIAN_POINT('Ctrl Pts',(4.20194396799995,12.2,1.18148801899999));
#344323=CARTESIAN_POINT('Ctrl Pts',(4.20194396799995,5.2,1.18148801899999));
#344324=CARTESIAN_POINT('Ctrl Pts',(4.20194396799995,2.2,1.18148801899999));
#344325=CARTESIAN_POINT('Ctrl Pts',(4.20345884699994,12.2,1.18273841999998));
#344326=CARTESIAN_POINT('Ctrl Pts',(4.20345884699994,5.2,1.18273841999998));
#344327=CARTESIAN_POINT('Ctrl Pts',(4.20345884699994,2.2,1.18273841999998));
#344328=CARTESIAN_POINT('Ctrl Pts',(4.20497550199994,12.2,1.18399312999999));
#344329=CARTESIAN_POINT('Ctrl Pts',(4.20497550199994,5.2,1.18399312999999));
#344330=CARTESIAN_POINT('Ctrl Pts',(4.20497550199994,2.2,1.18399312999999));
#344331=CARTESIAN_POINT('Ctrl Pts',(4.20649392199994,12.2,1.18525214899998));
#344332=CARTESIAN_POINT('Ctrl Pts',(4.20649392199994,5.2,1.18525214899998));
#344333=CARTESIAN_POINT('Ctrl Pts',(4.20649392199994,2.2,1.18525214899998));
#344334=CARTESIAN_POINT('Ctrl Pts',(4.20801409699994,12.2,1.18651547999999));
#344335=CARTESIAN_POINT('Ctrl Pts',(4.20801409699994,5.2,1.18651547999999));
#344336=CARTESIAN_POINT('Ctrl Pts',(4.20801409699994,2.2,1.18651547999999));
#344337=CARTESIAN_POINT('Ctrl Pts',(4.20953601499995,12.2,1.18778312299999));
#344338=CARTESIAN_POINT('Ctrl Pts',(4.20953601499995,5.2,1.18778312299999));
#344339=CARTESIAN_POINT('Ctrl Pts',(4.20953601499995,2.2,1.18778312299999));
#344340=CARTESIAN_POINT('Ctrl Pts',(4.21105966599994,12.2,1.18905508099999));
#344341=CARTESIAN_POINT('Ctrl Pts',(4.21105966599994,5.2,1.18905508099999));
#344342=CARTESIAN_POINT('Ctrl Pts',(4.21105966599994,2.2,1.18905508099999));
#344343=CARTESIAN_POINT('Ctrl Pts',(4.21258503799994,12.2,1.19033135499999));
#344344=CARTESIAN_POINT('Ctrl Pts',(4.21258503799994,5.2,1.19033135499999));
#344345=CARTESIAN_POINT('Ctrl Pts',(4.21258503799994,2.2,1.19033135499999));
#344346=CARTESIAN_POINT('Ctrl Pts',(4.21411212099995,12.2,1.19161194699998));
#344347=CARTESIAN_POINT('Ctrl Pts',(4.21411212099995,5.2,1.19161194699998));
#344348=CARTESIAN_POINT('Ctrl Pts',(4.21411212099995,2.2,1.19161194699998));
#344349=CARTESIAN_POINT('Ctrl Pts',(4.21564090399994,12.2,1.19289685699998));
#344350=CARTESIAN_POINT('Ctrl Pts',(4.21564090399994,5.2,1.19289685699998));
#344351=CARTESIAN_POINT('Ctrl Pts',(4.21564090399994,2.2,1.19289685699998));
#344352=CARTESIAN_POINT('Ctrl Pts',(4.21717137599994,12.2,1.19418608799998));
#344353=CARTESIAN_POINT('Ctrl Pts',(4.21717137599994,5.2,1.19418608799998));
#344354=CARTESIAN_POINT('Ctrl Pts',(4.21717137599994,2.2,1.19418608799998));
#344355=CARTESIAN_POINT('Ctrl Pts',(4.21870352699994,12.2,1.19547964099999));
#344356=CARTESIAN_POINT('Ctrl Pts',(4.21870352699994,5.2,1.19547964099999));
#344357=CARTESIAN_POINT('Ctrl Pts',(4.21870352699994,2.2,1.19547964099999));
#344358=CARTESIAN_POINT('Ctrl Pts',(4.22023734499995,12.2,1.19677751899999));
#344359=CARTESIAN_POINT('Ctrl Pts',(4.22023734499995,5.2,1.19677751899999));
#344360=CARTESIAN_POINT('Ctrl Pts',(4.22023734499995,2.2,1.19677751899999));
#344361=CARTESIAN_POINT('Ctrl Pts',(4.22177282099994,12.2,1.19807972199999));
#344362=CARTESIAN_POINT('Ctrl Pts',(4.22177282099994,5.2,1.19807972199999));
#344363=CARTESIAN_POINT('Ctrl Pts',(4.22177282099994,2.2,1.19807972199999));
#344364=CARTESIAN_POINT('Ctrl Pts',(4.22330994299995,12.2,1.19938625099998));
#344365=CARTESIAN_POINT('Ctrl Pts',(4.22330994299995,5.2,1.19938625099998));
#344366=CARTESIAN_POINT('Ctrl Pts',(4.22330994299995,2.2,1.19938625099998));
#344367=CARTESIAN_POINT('Ctrl Pts',(4.22484870099994,12.2,1.20069710799998));
#344368=CARTESIAN_POINT('Ctrl Pts',(4.22484870099994,5.2,1.20069710799998));
#344369=CARTESIAN_POINT('Ctrl Pts',(4.22484870099994,2.2,1.20069710799998));
#344370=CARTESIAN_POINT('Ctrl Pts',(4.22638908299994,12.2,1.20201229499999));
#344371=CARTESIAN_POINT('Ctrl Pts',(4.22638908299994,5.2,1.20201229499999));
#344372=CARTESIAN_POINT('Ctrl Pts',(4.22638908299994,2.2,1.20201229499999));
#344373=CARTESIAN_POINT('Ctrl Pts',(4.22793107999994,12.2,1.20333181299999));
#344374=CARTESIAN_POINT('Ctrl Pts',(4.22793107999994,5.2,1.20333181299999));
#344375=CARTESIAN_POINT('Ctrl Pts',(4.22793107999994,2.2,1.20333181299999));
#344376=CARTESIAN_POINT('Ctrl Pts',(4.22947467999994,12.2,1.20465566299998));
#344377=CARTESIAN_POINT('Ctrl Pts',(4.22947467999994,5.2,1.20465566299998));
#344378=CARTESIAN_POINT('Ctrl Pts',(4.22947467999994,2.2,1.20465566299998));
#344379=CARTESIAN_POINT('Ctrl Pts',(4.23101987299995,12.2,1.20598384699999));
#344380=CARTESIAN_POINT('Ctrl Pts',(4.23101987299995,5.2,1.20598384699999));
#344381=CARTESIAN_POINT('Ctrl Pts',(4.23101987299995,2.2,1.20598384699999));
#344382=CARTESIAN_POINT('Ctrl Pts',(4.23256664799994,12.2,1.20731636599999));
#344383=CARTESIAN_POINT('Ctrl Pts',(4.23256664799994,5.2,1.20731636599999));
#344384=CARTESIAN_POINT('Ctrl Pts',(4.23256664799994,2.2,1.20731636599999));
#344385=CARTESIAN_POINT('Ctrl Pts',(4.23411499399994,12.2,1.20865322199998));
#344386=CARTESIAN_POINT('Ctrl Pts',(4.23411499399994,5.2,1.20865322199998));
#344387=CARTESIAN_POINT('Ctrl Pts',(4.23411499399994,2.2,1.20865322199998));
#344388=CARTESIAN_POINT('Ctrl Pts',(4.23566490199994,12.2,1.20999441399999));
#344389=CARTESIAN_POINT('Ctrl Pts',(4.23566490199994,5.2,1.20999441399999));
#344390=CARTESIAN_POINT('Ctrl Pts',(4.23566490199994,2.2,1.20999441399999));
#344391=CARTESIAN_POINT('Ctrl Pts',(4.23721636099994,12.2,1.21133994699999));
#344392=CARTESIAN_POINT('Ctrl Pts',(4.23721636099994,5.2,1.21133994699999));
#344393=CARTESIAN_POINT('Ctrl Pts',(4.23721636099994,2.2,1.21133994699999));
#344394=CARTESIAN_POINT('Ctrl Pts',(4.23876935899994,12.2,1.21268981999998));
#344395=CARTESIAN_POINT('Ctrl Pts',(4.23876935899994,5.2,1.21268981999998));
#344396=CARTESIAN_POINT('Ctrl Pts',(4.23876935899994,2.2,1.21268981999998));
#344397=CARTESIAN_POINT('Ctrl Pts',(4.24032388699994,12.2,1.21404403499998));
#344398=CARTESIAN_POINT('Ctrl Pts',(4.24032388699994,5.2,1.21404403499998));
#344399=CARTESIAN_POINT('Ctrl Pts',(4.24032388699994,2.2,1.21404403499998));
#344400=CARTESIAN_POINT('Ctrl Pts',(4.24187993299994,12.2,1.21540259199998));
#344401=CARTESIAN_POINT('Ctrl Pts',(4.24187993299994,5.2,1.21540259199998));
#344402=CARTESIAN_POINT('Ctrl Pts',(4.24187993299994,2.2,1.21540259199998));
#344403=CARTESIAN_POINT('Ctrl Pts',(4.24343748699994,12.2,1.21676549299998));
#344404=CARTESIAN_POINT('Ctrl Pts',(4.24343748699994,5.2,1.21676549299998));
#344405=CARTESIAN_POINT('Ctrl Pts',(4.24343748699994,2.2,1.21676549299998));
#344406=CARTESIAN_POINT('Ctrl Pts',(4.24499653899994,12.2,1.21813273999999));
#344407=CARTESIAN_POINT('Ctrl Pts',(4.24499653899994,5.2,1.21813273999999));
#344408=CARTESIAN_POINT('Ctrl Pts',(4.24499653899994,2.2,1.21813273999999));
#344409=CARTESIAN_POINT('Ctrl Pts',(4.24655707799994,12.2,1.21950433399999));
#344410=CARTESIAN_POINT('Ctrl Pts',(4.24655707799994,5.2,1.21950433399999));
#344411=CARTESIAN_POINT('Ctrl Pts',(4.24655707799994,2.2,1.21950433399999));
#344412=CARTESIAN_POINT('Ctrl Pts',(4.24811909399994,12.2,1.22088027599998));
#344413=CARTESIAN_POINT('Ctrl Pts',(4.24811909399994,5.2,1.22088027599998));
#344414=CARTESIAN_POINT('Ctrl Pts',(4.24811909399994,2.2,1.22088027599998));
#344415=CARTESIAN_POINT('Ctrl Pts',(4.24968257599994,12.2,1.22226056599999));
#344416=CARTESIAN_POINT('Ctrl Pts',(4.24968257599994,5.2,1.22226056599999));
#344417=CARTESIAN_POINT('Ctrl Pts',(4.24968257599994,2.2,1.22226056599999));
#344418=CARTESIAN_POINT('Ctrl Pts',(4.25124751399994,12.2,1.22364520699998));
#344419=CARTESIAN_POINT('Ctrl Pts',(4.25124751399994,5.2,1.22364520699998));
#344420=CARTESIAN_POINT('Ctrl Pts',(4.25124751399994,2.2,1.22364520699998));
#344421=CARTESIAN_POINT('Ctrl Pts',(4.25281389699994,12.2,1.22503419899999));
#344422=CARTESIAN_POINT('Ctrl Pts',(4.25281389699994,5.2,1.22503419899999));
#344423=CARTESIAN_POINT('Ctrl Pts',(4.25281389699994,2.2,1.22503419899999));
#344424=CARTESIAN_POINT('Ctrl Pts',(4.25438171499994,12.2,1.22642754299998));
#344425=CARTESIAN_POINT('Ctrl Pts',(4.25438171499994,5.2,1.22642754299998));
#344426=CARTESIAN_POINT('Ctrl Pts',(4.25438171499994,2.2,1.22642754299998));
#344427=CARTESIAN_POINT('Ctrl Pts',(4.25595095699994,12.2,1.22782524099998));
#344428=CARTESIAN_POINT('Ctrl Pts',(4.25595095699994,5.2,1.22782524099998));
#344429=CARTESIAN_POINT('Ctrl Pts',(4.25595095699994,2.2,1.22782524099998));
#344430=CARTESIAN_POINT('Ctrl Pts',(4.25752161399994,12.2,1.22922729499999));
#344431=CARTESIAN_POINT('Ctrl Pts',(4.25752161399994,5.2,1.22922729499999));
#344432=CARTESIAN_POINT('Ctrl Pts',(4.25752161399994,2.2,1.22922729499999));
#344433=CARTESIAN_POINT('Ctrl Pts',(4.25909367399994,12.2,1.23063370299999));
#344434=CARTESIAN_POINT('Ctrl Pts',(4.25909367399994,5.2,1.23063370299999));
#344435=CARTESIAN_POINT('Ctrl Pts',(4.25909367399994,2.2,1.23063370299999));
#344436=CARTESIAN_POINT('Ctrl Pts',(4.26066712699994,12.2,1.23204446899999));
#344437=CARTESIAN_POINT('Ctrl Pts',(4.26066712699994,5.2,1.23204446899999));
#344438=CARTESIAN_POINT('Ctrl Pts',(4.26066712699994,2.2,1.23204446899999));
#344439=CARTESIAN_POINT('Ctrl Pts',(4.26224196399995,12.2,1.23345959199999));
#344440=CARTESIAN_POINT('Ctrl Pts',(4.26224196399995,5.2,1.23345959199999));
#344441=CARTESIAN_POINT('Ctrl Pts',(4.26224196399995,2.2,1.23345959199999));
#344442=CARTESIAN_POINT('Ctrl Pts',(4.26381817199994,12.2,1.23487907399999));
#344443=CARTESIAN_POINT('Ctrl Pts',(4.26381817199994,5.2,1.23487907399999));
#344444=CARTESIAN_POINT('Ctrl Pts',(4.26381817199994,2.2,1.23487907399999));
#344445=CARTESIAN_POINT('Ctrl Pts',(4.26539574399994,12.2,1.23630291699998));
#344446=CARTESIAN_POINT('Ctrl Pts',(4.26539574399994,5.2,1.23630291699998));
#344447=CARTESIAN_POINT('Ctrl Pts',(4.26539574399994,2.2,1.23630291699998));
#344448=CARTESIAN_POINT('Ctrl Pts',(4.26697466699994,12.2,1.23773111999999));
#344449=CARTESIAN_POINT('Ctrl Pts',(4.26697466699994,5.2,1.23773111999999));
#344450=CARTESIAN_POINT('Ctrl Pts',(4.26697466699994,2.2,1.23773111999999));
#344451=CARTESIAN_POINT('Ctrl Pts',(4.26855493199994,12.2,1.23916368499998));
#344452=CARTESIAN_POINT('Ctrl Pts',(4.26855493199994,5.2,1.23916368499998));
#344453=CARTESIAN_POINT('Ctrl Pts',(4.26855493199994,2.2,1.23916368499998));
#344454=CARTESIAN_POINT('Ctrl Pts',(4.27013652799995,12.2,1.24060061399998));
#344455=CARTESIAN_POINT('Ctrl Pts',(4.27013652799995,5.2,1.24060061399998));
#344456=CARTESIAN_POINT('Ctrl Pts',(4.27013652799995,2.2,1.24060061399998));
#344457=CARTESIAN_POINT('Ctrl Pts',(4.27171944499994,12.2,1.24204190499999));
#344458=CARTESIAN_POINT('Ctrl Pts',(4.27171944499994,5.2,1.24204190499999));
#344459=CARTESIAN_POINT('Ctrl Pts',(4.27171944499994,2.2,1.24204190499999));
#344460=CARTESIAN_POINT('Ctrl Pts',(4.27330367199994,12.2,1.24348756299999));
#344461=CARTESIAN_POINT('Ctrl Pts',(4.27330367199994,5.2,1.24348756299999));
#344462=CARTESIAN_POINT('Ctrl Pts',(4.27330367199994,2.2,1.24348756299999));
#344463=CARTESIAN_POINT('Ctrl Pts',(4.27488920099994,12.2,1.24493758599999));
#344464=CARTESIAN_POINT('Ctrl Pts',(4.27488920099994,5.2,1.24493758599999));
#344465=CARTESIAN_POINT('Ctrl Pts',(4.27488920099994,2.2,1.24493758599999));
#344466=CARTESIAN_POINT('Ctrl Pts',(4.27647601999994,12.2,1.24639197499999));
#344467=CARTESIAN_POINT('Ctrl Pts',(4.27647601999994,5.2,1.24639197499999));
#344468=CARTESIAN_POINT('Ctrl Pts',(4.27647601999994,2.2,1.24639197499999));
#344469=CARTESIAN_POINT('Ctrl Pts',(4.27806411899994,12.2,1.24785073299998));
#344470=CARTESIAN_POINT('Ctrl Pts',(4.27806411899994,5.2,1.24785073299998));
#344471=CARTESIAN_POINT('Ctrl Pts',(4.27806411899994,2.2,1.24785073299998));
#344472=CARTESIAN_POINT('Ctrl Pts',(4.27965348699994,12.2,1.24931385799998));
#344473=CARTESIAN_POINT('Ctrl Pts',(4.27965348699994,5.2,1.24931385799998));
#344474=CARTESIAN_POINT('Ctrl Pts',(4.27965348699994,2.2,1.24931385799998));
#344475=CARTESIAN_POINT('Ctrl Pts',(4.28124411599994,12.2,1.25078135299999));
#344476=CARTESIAN_POINT('Ctrl Pts',(4.28124411599994,5.2,1.25078135299999));
#344477=CARTESIAN_POINT('Ctrl Pts',(4.28124411599994,2.2,1.25078135299999));
#344478=CARTESIAN_POINT('Ctrl Pts',(4.28283599299994,12.2,1.25225321799999));
#344479=CARTESIAN_POINT('Ctrl Pts',(4.28283599299994,5.2,1.25225321799999));
#344480=CARTESIAN_POINT('Ctrl Pts',(4.28283599299994,2.2,1.25225321799999));
#344481=CARTESIAN_POINT('Ctrl Pts',(4.28442910999994,12.2,1.25372945399999));
#344482=CARTESIAN_POINT('Ctrl Pts',(4.28442910999994,5.2,1.25372945399999));
#344483=CARTESIAN_POINT('Ctrl Pts',(4.28442910999994,2.2,1.25372945399999));
#344484=CARTESIAN_POINT('Ctrl Pts',(4.28602345699994,12.2,1.25521006299998));
#344485=CARTESIAN_POINT('Ctrl Pts',(4.28602345699994,5.2,1.25521006299998));
#344486=CARTESIAN_POINT('Ctrl Pts',(4.28602345699994,2.2,1.25521006299998));
#344487=CARTESIAN_POINT('Ctrl Pts',(4.28761902199995,12.2,1.25669504399998));
#344488=CARTESIAN_POINT('Ctrl Pts',(4.28761902199995,5.2,1.25669504399998));
#344489=CARTESIAN_POINT('Ctrl Pts',(4.28761902199995,2.2,1.25669504399998));
#344490=CARTESIAN_POINT('Ctrl Pts',(4.28921579599994,12.2,1.25818439799998));
#344491=CARTESIAN_POINT('Ctrl Pts',(4.28921579599994,5.2,1.25818439799998));
#344492=CARTESIAN_POINT('Ctrl Pts',(4.28921579599994,2.2,1.25818439799998));
#344493=CARTESIAN_POINT('Ctrl Pts',(4.29081376899994,12.2,1.25967812699999));
#344494=CARTESIAN_POINT('Ctrl Pts',(4.29081376899994,5.2,1.25967812699999));
#344495=CARTESIAN_POINT('Ctrl Pts',(4.29081376899994,2.2,1.25967812699999));
#344496=CARTESIAN_POINT('Ctrl Pts',(4.29241293099994,12.2,1.26117623099999));
#344497=CARTESIAN_POINT('Ctrl Pts',(4.29241293099994,5.2,1.26117623099999));
#344498=CARTESIAN_POINT('Ctrl Pts',(4.29241293099994,2.2,1.26117623099999));
#344499=CARTESIAN_POINT('Ctrl Pts',(4.29401327199994,12.2,1.26267870999999));
#344500=CARTESIAN_POINT('Ctrl Pts',(4.29401327199994,5.2,1.26267870999999));
#344501=CARTESIAN_POINT('Ctrl Pts',(4.29401327199994,2.2,1.26267870999999));
#344502=CARTESIAN_POINT('Ctrl Pts',(4.29561478099994,12.2,1.26418556599999));
#344503=CARTESIAN_POINT('Ctrl Pts',(4.29561478099994,5.2,1.26418556599999));
#344504=CARTESIAN_POINT('Ctrl Pts',(4.29561478099994,2.2,1.26418556599999));
#344505=CARTESIAN_POINT('Ctrl Pts',(4.29721744799994,12.2,1.26569679999998));
#344506=CARTESIAN_POINT('Ctrl Pts',(4.29721744799994,5.2,1.26569679999998));
#344507=CARTESIAN_POINT('Ctrl Pts',(4.29721744799994,2.2,1.26569679999998));
#344508=CARTESIAN_POINT('Ctrl Pts',(4.29882126499994,12.2,1.26721241099998));
#344509=CARTESIAN_POINT('Ctrl Pts',(4.29882126499994,5.2,1.26721241099998));
#344510=CARTESIAN_POINT('Ctrl Pts',(4.29882126499994,2.2,1.26721241099998));
#344511=CARTESIAN_POINT('Ctrl Pts',(4.30042621899995,12.2,1.26873239999998));
#344512=CARTESIAN_POINT('Ctrl Pts',(4.30042621899995,5.2,1.26873239999998));
#344513=CARTESIAN_POINT('Ctrl Pts',(4.30042621899995,2.2,1.26873239999998));
#344514=CARTESIAN_POINT('Ctrl Pts',(4.30203230199994,12.2,1.27025676999999));
#344515=CARTESIAN_POINT('Ctrl Pts',(4.30203230199994,5.2,1.27025676999999));
#344516=CARTESIAN_POINT('Ctrl Pts',(4.30203230199994,2.2,1.27025676999999));
#344517=CARTESIAN_POINT('Ctrl Pts',(4.30363950299994,12.2,1.27178551899998));
#344518=CARTESIAN_POINT('Ctrl Pts',(4.30363950299994,5.2,1.27178551899998));
#344519=CARTESIAN_POINT('Ctrl Pts',(4.30363950299994,2.2,1.27178551899998));
#344520=CARTESIAN_POINT('Ctrl Pts',(4.30524781299995,12.2,1.27331864799999));
#344521=CARTESIAN_POINT('Ctrl Pts',(4.30524781299995,5.2,1.27331864799999));
#344522=CARTESIAN_POINT('Ctrl Pts',(4.30524781299995,2.2,1.27331864799999));
#344523=CARTESIAN_POINT('Ctrl Pts',(4.30685722099994,12.2,1.27485615899999));
#344524=CARTESIAN_POINT('Ctrl Pts',(4.30685722099994,5.2,1.27485615899999));
#344525=CARTESIAN_POINT('Ctrl Pts',(4.30685722099994,2.2,1.27485615899999));
#344526=CARTESIAN_POINT('Ctrl Pts',(4.30846771799995,12.2,1.27639805199999));
#344527=CARTESIAN_POINT('Ctrl Pts',(4.30846771799995,5.2,1.27639805199999));
#344528=CARTESIAN_POINT('Ctrl Pts',(4.30846771799995,2.2,1.27639805199999));
#344529=CARTESIAN_POINT('Ctrl Pts',(4.31007929299995,12.2,1.27794432699998));
#344530=CARTESIAN_POINT('Ctrl Pts',(4.31007929299995,5.2,1.27794432699998));
#344531=CARTESIAN_POINT('Ctrl Pts',(4.31007929299995,2.2,1.27794432699998));
#344532=CARTESIAN_POINT('Ctrl Pts',(4.31169193699994,12.2,1.27949498499999));
#344533=CARTESIAN_POINT('Ctrl Pts',(4.31169193699994,5.2,1.27949498499999));
#344534=CARTESIAN_POINT('Ctrl Pts',(4.31169193699994,2.2,1.27949498499999));
#344535=CARTESIAN_POINT('Ctrl Pts',(4.31330563999994,12.2,1.28105002699999));
#344536=CARTESIAN_POINT('Ctrl Pts',(4.31330563999994,5.2,1.28105002699999));
#344537=CARTESIAN_POINT('Ctrl Pts',(4.31330563999994,2.2,1.28105002699999));
#344538=CARTESIAN_POINT('Ctrl Pts',(4.31492039099994,12.2,1.28260945399999));
#344539=CARTESIAN_POINT('Ctrl Pts',(4.31492039099994,5.2,1.28260945399999));
#344540=CARTESIAN_POINT('Ctrl Pts',(4.31492039099994,2.2,1.28260945399999));
#344541=CARTESIAN_POINT('Ctrl Pts',(4.31653618199995,12.2,1.28417326399999));
#344542=CARTESIAN_POINT('Ctrl Pts',(4.31653618199995,5.2,1.28417326399999));
#344543=CARTESIAN_POINT('Ctrl Pts',(4.31653618199995,2.2,1.28417326399999));
#344544=CARTESIAN_POINT('Ctrl Pts',(4.31815299999994,12.2,1.28574145999998));
#344545=CARTESIAN_POINT('Ctrl Pts',(4.31815299999994,5.2,1.28574145999998));
#344546=CARTESIAN_POINT('Ctrl Pts',(4.31815299999994,2.2,1.28574145999998));
#344547=CARTESIAN_POINT('Ctrl Pts',(4.31977083899994,12.2,1.28731404199999));
#344548=CARTESIAN_POINT('Ctrl Pts',(4.31977083899994,5.2,1.28731404199999));
#344549=CARTESIAN_POINT('Ctrl Pts',(4.31977083899994,2.2,1.28731404199999));
#344550=CARTESIAN_POINT('Ctrl Pts',(4.32138968599994,12.2,1.28889100999999));
#344551=CARTESIAN_POINT('Ctrl Pts',(4.32138968599994,5.2,1.28889100999999));
#344552=CARTESIAN_POINT('Ctrl Pts',(4.32138968599994,2.2,1.28889100999999));
#344553=CARTESIAN_POINT('Ctrl Pts',(4.32300953299994,12.2,1.29047236499999));
#344554=CARTESIAN_POINT('Ctrl Pts',(4.32300953299994,5.2,1.29047236499999));
#344555=CARTESIAN_POINT('Ctrl Pts',(4.32300953299994,2.2,1.29047236499999));
#344556=CARTESIAN_POINT('Ctrl Pts',(4.32463036999994,12.2,1.29205810699998));
#344557=CARTESIAN_POINT('Ctrl Pts',(4.32463036999994,5.2,1.29205810699998));
#344558=CARTESIAN_POINT('Ctrl Pts',(4.32463036999994,2.2,1.29205810699998));
#344559=CARTESIAN_POINT('Ctrl Pts',(4.32625218699994,12.2,1.29364823599999));
#344560=CARTESIAN_POINT('Ctrl Pts',(4.32625218699994,5.2,1.29364823599999));
#344561=CARTESIAN_POINT('Ctrl Pts',(4.32625218699994,2.2,1.29364823599999));
#344562=CARTESIAN_POINT('Ctrl Pts',(4.32787497299994,12.2,1.29524275399998));
#344563=CARTESIAN_POINT('Ctrl Pts',(4.32787497299994,5.2,1.29524275399998));
#344564=CARTESIAN_POINT('Ctrl Pts',(4.32787497299994,2.2,1.29524275399998));
#344565=CARTESIAN_POINT('Ctrl Pts',(4.32949871899994,12.2,1.29684166099999));
#344566=CARTESIAN_POINT('Ctrl Pts',(4.32949871899994,5.2,1.29684166099999));
#344567=CARTESIAN_POINT('Ctrl Pts',(4.32949871899994,2.2,1.29684166099999));
#344568=CARTESIAN_POINT('Ctrl Pts',(4.33112341699994,12.2,1.29844495599999));
#344569=CARTESIAN_POINT('Ctrl Pts',(4.33112341699994,5.2,1.29844495599999));
#344570=CARTESIAN_POINT('Ctrl Pts',(4.33112341699994,2.2,1.29844495599999));
#344571=CARTESIAN_POINT('Ctrl Pts',(4.33274905499994,12.2,1.30005264099998));
#344572=CARTESIAN_POINT('Ctrl Pts',(4.33274905499994,5.2,1.30005264099998));
#344573=CARTESIAN_POINT('Ctrl Pts',(4.33274905499994,2.2,1.30005264099998));
#344574=CARTESIAN_POINT('Ctrl Pts',(4.33437562399994,12.2,1.30166471499999));
#344575=CARTESIAN_POINT('Ctrl Pts',(4.33437562399994,5.2,1.30166471499999));
#344576=CARTESIAN_POINT('Ctrl Pts',(4.33437562399994,2.2,1.30166471499999));
#344577=CARTESIAN_POINT('Ctrl Pts',(4.33600311299995,12.2,1.30328117999999));
#344578=CARTESIAN_POINT('Ctrl Pts',(4.33600311299995,5.2,1.30328117999999));
#344579=CARTESIAN_POINT('Ctrl Pts',(4.33600311299995,2.2,1.30328117999999));
#344580=CARTESIAN_POINT('Ctrl Pts',(4.33763151499994,12.2,1.30490203499999));
#344581=CARTESIAN_POINT('Ctrl Pts',(4.33763151499994,5.2,1.30490203499999));
#344582=CARTESIAN_POINT('Ctrl Pts',(4.33763151499994,2.2,1.30490203499999));
#344583=CARTESIAN_POINT('Ctrl Pts',(4.33926081799994,12.2,1.30652727999998));
#344584=CARTESIAN_POINT('Ctrl Pts',(4.33926081799994,5.2,1.30652727999998));
#344585=CARTESIAN_POINT('Ctrl Pts',(4.33926081799994,2.2,1.30652727999998));
#344586=CARTESIAN_POINT('Ctrl Pts',(4.34089101299994,12.2,1.30815691799999));
#344587=CARTESIAN_POINT('Ctrl Pts',(4.34089101299994,5.2,1.30815691799999));
#344588=CARTESIAN_POINT('Ctrl Pts',(4.34089101299994,2.2,1.30815691799999));
#344589=CARTESIAN_POINT('Ctrl Pts',(4.34252208999994,12.2,1.30979094599999));
#344590=CARTESIAN_POINT('Ctrl Pts',(4.34252208999994,5.2,1.30979094599999));
#344591=CARTESIAN_POINT('Ctrl Pts',(4.34252208999994,2.2,1.30979094599999));
#344592=CARTESIAN_POINT('Ctrl Pts',(4.34415404099994,12.2,1.31142936699999));
#344593=CARTESIAN_POINT('Ctrl Pts',(4.34415404099994,5.2,1.31142936699999));
#344594=CARTESIAN_POINT('Ctrl Pts',(4.34415404099994,2.2,1.31142936699999));
#344595=CARTESIAN_POINT('Ctrl Pts',(4.34578685399994,12.2,1.31307217999999));
#344596=CARTESIAN_POINT('Ctrl Pts',(4.34578685399994,5.2,1.31307217999999));
#344597=CARTESIAN_POINT('Ctrl Pts',(4.34578685399994,2.2,1.31307217999999));
#344598=CARTESIAN_POINT('Ctrl Pts',(4.34742051999994,12.2,1.31471938499998));
#344599=CARTESIAN_POINT('Ctrl Pts',(4.34742051999994,5.2,1.31471938499998));
#344600=CARTESIAN_POINT('Ctrl Pts',(4.34742051999994,2.2,1.31471938499998));
#344601=CARTESIAN_POINT('Ctrl Pts',(4.34905503099994,12.2,1.31637098199999));
#344602=CARTESIAN_POINT('Ctrl Pts',(4.34905503099994,5.2,1.31637098199999));
#344603=CARTESIAN_POINT('Ctrl Pts',(4.34905503099994,2.2,1.31637098199999));
#344604=CARTESIAN_POINT('Ctrl Pts',(4.35069037499995,12.2,1.31802697399999));
#344605=CARTESIAN_POINT('Ctrl Pts',(4.35069037499995,5.2,1.31802697399999));
#344606=CARTESIAN_POINT('Ctrl Pts',(4.35069037499995,2.2,1.31802697399999));
#344607=CARTESIAN_POINT('Ctrl Pts',(4.35232654399995,12.2,1.31968735699999));
#344608=CARTESIAN_POINT('Ctrl Pts',(4.35232654399995,5.2,1.31968735699999));
#344609=CARTESIAN_POINT('Ctrl Pts',(4.35232654399995,2.2,1.31968735699999));
#344610=CARTESIAN_POINT('Ctrl Pts',(4.35396352699995,12.2,1.32135213299998));
#344611=CARTESIAN_POINT('Ctrl Pts',(4.35396352699995,5.2,1.32135213299998));
#344612=CARTESIAN_POINT('Ctrl Pts',(4.35396352699995,2.2,1.32135213299998));
#344613=CARTESIAN_POINT('Ctrl Pts',(4.35560131699994,12.2,1.32302130499999));
#344614=CARTESIAN_POINT('Ctrl Pts',(4.35560131699994,5.2,1.32302130499999));
#344615=CARTESIAN_POINT('Ctrl Pts',(4.35560131699994,2.2,1.32302130499999));
#344616=CARTESIAN_POINT('Ctrl Pts',(4.35723990199994,12.2,1.32469486899998));
#344617=CARTESIAN_POINT('Ctrl Pts',(4.35723990199994,5.2,1.32469486899998));
#344618=CARTESIAN_POINT('Ctrl Pts',(4.35723990199994,2.2,1.32469486899998));
#344619=CARTESIAN_POINT('Ctrl Pts',(4.35887927299994,12.2,1.32637282699998));
#344620=CARTESIAN_POINT('Ctrl Pts',(4.35887927299994,5.2,1.32637282699998));
#344621=CARTESIAN_POINT('Ctrl Pts',(4.35887927299994,2.2,1.32637282699998));
#344622=CARTESIAN_POINT('Ctrl Pts',(4.36051941999995,12.2,1.32805517999998));
#344623=CARTESIAN_POINT('Ctrl Pts',(4.36051941999995,5.2,1.32805517999998));
#344624=CARTESIAN_POINT('Ctrl Pts',(4.36051941999995,2.2,1.32805517999998));
#344625=CARTESIAN_POINT('Ctrl Pts',(4.36216033499994,12.2,1.32974192599999));
#344626=CARTESIAN_POINT('Ctrl Pts',(4.36216033499994,5.2,1.32974192599999));
#344627=CARTESIAN_POINT('Ctrl Pts',(4.36216033499994,2.2,1.32974192599999));
#344628=CARTESIAN_POINT('Ctrl Pts',(4.36380200799994,12.2,1.33143306799999));
#344629=CARTESIAN_POINT('Ctrl Pts',(4.36380200799994,5.2,1.33143306799999));
#344630=CARTESIAN_POINT('Ctrl Pts',(4.36380200799994,2.2,1.33143306799999));
#344631=CARTESIAN_POINT('Ctrl Pts',(4.36544442799994,12.2,1.33312860399998));
#344632=CARTESIAN_POINT('Ctrl Pts',(4.36544442799994,5.2,1.33312860399998));
#344633=CARTESIAN_POINT('Ctrl Pts',(4.36544442799994,2.2,1.33312860399998));
#344634=CARTESIAN_POINT('Ctrl Pts',(4.36708758799994,12.2,1.33482853399999));
#344635=CARTESIAN_POINT('Ctrl Pts',(4.36708758799994,5.2,1.33482853399999));
#344636=CARTESIAN_POINT('Ctrl Pts',(4.36708758799994,2.2,1.33482853399999));
#344637=CARTESIAN_POINT('Ctrl Pts',(4.36873147599994,12.2,1.33653285899999));
#344638=CARTESIAN_POINT('Ctrl Pts',(4.36873147599994,5.2,1.33653285899999));
#344639=CARTESIAN_POINT('Ctrl Pts',(4.36873147599994,2.2,1.33653285899999));
#344640=CARTESIAN_POINT('Ctrl Pts',(4.37037608399994,12.2,1.33824157899999));
#344641=CARTESIAN_POINT('Ctrl Pts',(4.37037608399994,5.2,1.33824157899999));
#344642=CARTESIAN_POINT('Ctrl Pts',(4.37037608399994,2.2,1.33824157899999));
#344643=CARTESIAN_POINT('Ctrl Pts',(4.37202140199994,12.2,1.33995469399999));
#344644=CARTESIAN_POINT('Ctrl Pts',(4.37202140199994,5.2,1.33995469399999));
#344645=CARTESIAN_POINT('Ctrl Pts',(4.37202140199994,2.2,1.33995469399999));
#344646=CARTESIAN_POINT('Ctrl Pts',(4.37366742099994,12.2,1.34167220399998));
#344647=CARTESIAN_POINT('Ctrl Pts',(4.37366742099994,5.2,1.34167220399998));
#344648=CARTESIAN_POINT('Ctrl Pts',(4.37366742099994,2.2,1.34167220399998));
#344649=CARTESIAN_POINT('Ctrl Pts',(4.37531413099994,12.2,1.34339410999999));
#344650=CARTESIAN_POINT('Ctrl Pts',(4.37531413099994,5.2,1.34339410999999));
#344651=CARTESIAN_POINT('Ctrl Pts',(4.37531413099994,2.2,1.34339410999999));
#344652=CARTESIAN_POINT('Ctrl Pts',(4.37696152299995,12.2,1.34512040999998));
#344653=CARTESIAN_POINT('Ctrl Pts',(4.37696152299995,5.2,1.34512040999998));
#344654=CARTESIAN_POINT('Ctrl Pts',(4.37696152299995,2.2,1.34512040999998));
#344655=CARTESIAN_POINT('Ctrl Pts',(4.37860958799994,12.2,1.34685110599999));
#344656=CARTESIAN_POINT('Ctrl Pts',(4.37860958799994,5.2,1.34685110599999));
#344657=CARTESIAN_POINT('Ctrl Pts',(4.37860958799994,2.2,1.34685110599999));
#344658=CARTESIAN_POINT('Ctrl Pts',(4.38025831499994,12.2,1.34858619499999));
#344659=CARTESIAN_POINT('Ctrl Pts',(4.38025831499994,5.2,1.34858619499999));
#344660=CARTESIAN_POINT('Ctrl Pts',(4.38025831499994,2.2,1.34858619499999));
#344661=CARTESIAN_POINT('Ctrl Pts',(4.38190769699994,12.2,1.35032568199998));
#344662=CARTESIAN_POINT('Ctrl Pts',(4.38190769699994,5.2,1.35032568199998));
#344663=CARTESIAN_POINT('Ctrl Pts',(4.38190769699994,2.2,1.35032568199998));
#344664=CARTESIAN_POINT('Ctrl Pts',(4.38355772299994,12.2,1.35206956199998));
#344665=CARTESIAN_POINT('Ctrl Pts',(4.38355772299994,5.2,1.35206956199998));
#344666=CARTESIAN_POINT('Ctrl Pts',(4.38355772299994,2.2,1.35206956199998));
#344667=CARTESIAN_POINT('Ctrl Pts',(4.38520838299994,12.2,1.35381783799998));
#344668=CARTESIAN_POINT('Ctrl Pts',(4.38520838299994,5.2,1.35381783799998));
#344669=CARTESIAN_POINT('Ctrl Pts',(4.38520838299994,2.2,1.35381783799998));
#344670=CARTESIAN_POINT('Ctrl Pts',(4.38685966999994,12.2,1.35557050899999));
#344671=CARTESIAN_POINT('Ctrl Pts',(4.38685966999994,5.2,1.35557050899999));
#344672=CARTESIAN_POINT('Ctrl Pts',(4.38685966999994,2.2,1.35557050899999));
#344673=CARTESIAN_POINT('Ctrl Pts',(4.38851157199994,12.2,1.35732757499999));
#344674=CARTESIAN_POINT('Ctrl Pts',(4.38851157199994,5.2,1.35732757499999));
#344675=CARTESIAN_POINT('Ctrl Pts',(4.38851157199994,2.2,1.35732757499999));
#344676=CARTESIAN_POINT('Ctrl Pts',(4.39016408099994,12.2,1.35908903699999));
#344677=CARTESIAN_POINT('Ctrl Pts',(4.39016408099994,5.2,1.35908903699999));
#344678=CARTESIAN_POINT('Ctrl Pts',(4.39016408099994,2.2,1.35908903699999));
#344679=CARTESIAN_POINT('Ctrl Pts',(4.39181718799994,12.2,1.36085489299999));
#344680=CARTESIAN_POINT('Ctrl Pts',(4.39181718799994,5.2,1.36085489299999));
#344681=CARTESIAN_POINT('Ctrl Pts',(4.39181718799994,2.2,1.36085489299999));
#344682=CARTESIAN_POINT('Ctrl Pts',(4.39347088399995,12.2,1.36262514299998));
#344683=CARTESIAN_POINT('Ctrl Pts',(4.39347088399995,5.2,1.36262514299998));
#344684=CARTESIAN_POINT('Ctrl Pts',(4.39347088399995,2.2,1.36262514299998));
#344685=CARTESIAN_POINT('Ctrl Pts',(4.39512515799994,12.2,1.36439978799999));
#344686=CARTESIAN_POINT('Ctrl Pts',(4.39512515799994,5.2,1.36439978799999));
#344687=CARTESIAN_POINT('Ctrl Pts',(4.39512515799994,2.2,1.36439978799999));
#344688=CARTESIAN_POINT('Ctrl Pts',(4.39678000299994,12.2,1.36617882899999));
#344689=CARTESIAN_POINT('Ctrl Pts',(4.39678000299994,5.2,1.36617882899999));
#344690=CARTESIAN_POINT('Ctrl Pts',(4.39678000299994,2.2,1.36617882899999));
#344691=CARTESIAN_POINT('Ctrl Pts',(4.39843540799994,12.2,1.36796226299999));
#344692=CARTESIAN_POINT('Ctrl Pts',(4.39843540799994,5.2,1.36796226299999));
#344693=CARTESIAN_POINT('Ctrl Pts',(4.39843540799994,2.2,1.36796226299999));
#344694=CARTESIAN_POINT('Ctrl Pts',(4.40009136299994,12.2,1.36975009199999));
#344695=CARTESIAN_POINT('Ctrl Pts',(4.40009136299994,5.2,1.36975009199999));
#344696=CARTESIAN_POINT('Ctrl Pts',(4.40009136299994,2.2,1.36975009199999));
#344697=CARTESIAN_POINT('Ctrl Pts',(4.40174786199994,12.2,1.37154231599999));
#344698=CARTESIAN_POINT('Ctrl Pts',(4.40174786199994,5.2,1.37154231599999));
#344699=CARTESIAN_POINT('Ctrl Pts',(4.40174786199994,2.2,1.37154231599999));
#344700=CARTESIAN_POINT('Ctrl Pts',(4.40340489299994,12.2,1.37333893199999));
#344701=CARTESIAN_POINT('Ctrl Pts',(4.40340489299994,5.2,1.37333893199999));
#344702=CARTESIAN_POINT('Ctrl Pts',(4.40340489299994,2.2,1.37333893199999));
#344703=CARTESIAN_POINT('Ctrl Pts',(4.40506244799994,12.2,1.37513994299999));
#344704=CARTESIAN_POINT('Ctrl Pts',(4.40506244799994,5.2,1.37513994299999));
#344705=CARTESIAN_POINT('Ctrl Pts',(4.40506244799994,2.2,1.37513994299999));
#344706=CARTESIAN_POINT('Ctrl Pts',(4.40672051699995,12.2,1.37694534799999));
#344707=CARTESIAN_POINT('Ctrl Pts',(4.40672051699995,5.2,1.37694534799999));
#344708=CARTESIAN_POINT('Ctrl Pts',(4.40672051699995,2.2,1.37694534799999));
#344709=CARTESIAN_POINT('Ctrl Pts',(4.40837909099994,12.2,1.37875514499999));
#344710=CARTESIAN_POINT('Ctrl Pts',(4.40837909099994,5.2,1.37875514499999));
#344711=CARTESIAN_POINT('Ctrl Pts',(4.40837909099994,2.2,1.37875514499999));
#344712=CARTESIAN_POINT('Ctrl Pts',(4.41003816199994,12.2,1.38056933699998));
#344713=CARTESIAN_POINT('Ctrl Pts',(4.41003816199994,5.2,1.38056933699998));
#344714=CARTESIAN_POINT('Ctrl Pts',(4.41003816199994,2.2,1.38056933699998));
#344715=CARTESIAN_POINT('Ctrl Pts',(4.41169771899994,12.2,1.38238792099999));
#344716=CARTESIAN_POINT('Ctrl Pts',(4.41169771899994,5.2,1.38238792099999));
#344717=CARTESIAN_POINT('Ctrl Pts',(4.41169771899994,2.2,1.38238792099999));
#344718=CARTESIAN_POINT('Ctrl Pts',(4.41335775399994,12.2,1.38421089799999));
#344719=CARTESIAN_POINT('Ctrl Pts',(4.41335775399994,5.2,1.38421089799999));
#344720=CARTESIAN_POINT('Ctrl Pts',(4.41335775399994,2.2,1.38421089799999));
#344721=CARTESIAN_POINT('Ctrl Pts',(4.41501825699994,12.2,1.38603826799998));
#344722=CARTESIAN_POINT('Ctrl Pts',(4.41501825699994,5.2,1.38603826799998));
#344723=CARTESIAN_POINT('Ctrl Pts',(4.41501825699994,2.2,1.38603826799998));
#344724=CARTESIAN_POINT('Ctrl Pts',(4.41667922099994,12.2,1.38787002999999));
#344725=CARTESIAN_POINT('Ctrl Pts',(4.41667922099994,5.2,1.38787002999999));
#344726=CARTESIAN_POINT('Ctrl Pts',(4.41667922099994,2.2,1.38787002999999));
#344727=CARTESIAN_POINT('Ctrl Pts',(4.41834063399994,12.2,1.38970618399998));
#344728=CARTESIAN_POINT('Ctrl Pts',(4.41834063399994,5.2,1.38970618399998));
#344729=CARTESIAN_POINT('Ctrl Pts',(4.41834063399994,2.2,1.38970618399998));
#344730=CARTESIAN_POINT('Ctrl Pts',(4.42000248799994,12.2,1.39154672899998));
#344731=CARTESIAN_POINT('Ctrl Pts',(4.42000248799994,5.2,1.39154672899998));
#344732=CARTESIAN_POINT('Ctrl Pts',(4.42000248799994,2.2,1.39154672899998));
#344733=CARTESIAN_POINT('Ctrl Pts',(4.42166477499994,12.2,1.39339166599999));
#344734=CARTESIAN_POINT('Ctrl Pts',(4.42166477499994,5.2,1.39339166599999));
#344735=CARTESIAN_POINT('Ctrl Pts',(4.42166477499994,2.2,1.39339166599999));
#344736=CARTESIAN_POINT('Ctrl Pts',(4.42332748499994,12.2,1.39524099499999));
#344737=CARTESIAN_POINT('Ctrl Pts',(4.42332748499994,5.2,1.39524099499999));
#344738=CARTESIAN_POINT('Ctrl Pts',(4.42332748499994,2.2,1.39524099499999));
#344739=CARTESIAN_POINT('Ctrl Pts',(4.42499060899994,12.2,1.39709471299998));
#344740=CARTESIAN_POINT('Ctrl Pts',(4.42499060899994,5.2,1.39709471299998));
#344741=CARTESIAN_POINT('Ctrl Pts',(4.42499060899994,2.2,1.39709471299998));
#344742=CARTESIAN_POINT('Ctrl Pts',(4.42665413799994,12.2,1.39895282199999));
#344743=CARTESIAN_POINT('Ctrl Pts',(4.42665413799994,5.2,1.39895282199999));
#344744=CARTESIAN_POINT('Ctrl Pts',(4.42665413799994,2.2,1.39895282199999));
#344745=CARTESIAN_POINT('Ctrl Pts',(4.42831806199994,12.2,1.40081532299998));
#344746=CARTESIAN_POINT('Ctrl Pts',(4.42831806199994,5.2,1.40081532299998));
#344747=CARTESIAN_POINT('Ctrl Pts',(4.42831806199994,2.2,1.40081532299998));
#344748=CARTESIAN_POINT('Ctrl Pts',(4.42998237399994,12.2,1.40268221199999));
#344749=CARTESIAN_POINT('Ctrl Pts',(4.42998237399994,5.2,1.40268221199999));
#344750=CARTESIAN_POINT('Ctrl Pts',(4.42998237399994,2.2,1.40268221199999));
#344751=CARTESIAN_POINT('Ctrl Pts',(4.43164706299994,12.2,1.40455348999998));
#344752=CARTESIAN_POINT('Ctrl Pts',(4.43164706299994,5.2,1.40455348999998));
#344753=CARTESIAN_POINT('Ctrl Pts',(4.43164706299994,2.2,1.40455348999998));
#344754=CARTESIAN_POINT('Ctrl Pts',(4.43331212099995,12.2,1.40642915799999));
#344755=CARTESIAN_POINT('Ctrl Pts',(4.43331212099995,5.2,1.40642915799999));
#344756=CARTESIAN_POINT('Ctrl Pts',(4.43331212099995,2.2,1.40642915799999));
#344757=CARTESIAN_POINT('Ctrl Pts',(4.43497753899995,12.2,1.40830921399999));
#344758=CARTESIAN_POINT('Ctrl Pts',(4.43497753899995,5.2,1.40830921399999));
#344759=CARTESIAN_POINT('Ctrl Pts',(4.43497753899995,2.2,1.40830921399999));
#344760=CARTESIAN_POINT('Ctrl Pts',(4.43664330699994,12.2,1.41019365799998));
#344761=CARTESIAN_POINT('Ctrl Pts',(4.43664330699994,5.2,1.41019365799998));
#344762=CARTESIAN_POINT('Ctrl Pts',(4.43664330699994,2.2,1.41019365799998));
#344763=CARTESIAN_POINT('Ctrl Pts',(4.43830941799995,12.2,1.41208248999999));
#344764=CARTESIAN_POINT('Ctrl Pts',(4.43830941799995,5.2,1.41208248999999));
#344765=CARTESIAN_POINT('Ctrl Pts',(4.43830941799995,2.2,1.41208248999999));
#344766=CARTESIAN_POINT('Ctrl Pts',(4.43997586199994,12.2,1.41397570899999));
#344767=CARTESIAN_POINT('Ctrl Pts',(4.43997586199994,5.2,1.41397570899999));
#344768=CARTESIAN_POINT('Ctrl Pts',(4.43997586199994,2.2,1.41397570899999));
#344769=CARTESIAN_POINT('Ctrl Pts',(4.44164262899994,12.2,1.41587331599998));
#344770=CARTESIAN_POINT('Ctrl Pts',(4.44164262899994,5.2,1.41587331599998));
#344771=CARTESIAN_POINT('Ctrl Pts',(4.44164262899994,2.2,1.41587331599998));
#344772=CARTESIAN_POINT('Ctrl Pts',(4.44330971099994,12.2,1.41777530899999));
#344773=CARTESIAN_POINT('Ctrl Pts',(4.44330971099994,5.2,1.41777530899999));
#344774=CARTESIAN_POINT('Ctrl Pts',(4.44330971099994,2.2,1.41777530899999));
#344775=CARTESIAN_POINT('Ctrl Pts',(4.44497709999994,12.2,1.41968168799998));
#344776=CARTESIAN_POINT('Ctrl Pts',(4.44497709999994,5.2,1.41968168799998));
#344777=CARTESIAN_POINT('Ctrl Pts',(4.44497709999994,2.2,1.41968168799998));
#344778=CARTESIAN_POINT('Ctrl Pts',(4.44664478499995,12.2,1.42159245199998));
#344779=CARTESIAN_POINT('Ctrl Pts',(4.44664478499995,5.2,1.42159245199998));
#344780=CARTESIAN_POINT('Ctrl Pts',(4.44664478499995,2.2,1.42159245199998));
#344781=CARTESIAN_POINT('Ctrl Pts',(4.44831275899995,12.2,1.42350760199998));
#344782=CARTESIAN_POINT('Ctrl Pts',(4.44831275899995,5.2,1.42350760199998));
#344783=CARTESIAN_POINT('Ctrl Pts',(4.44831275899995,2.2,1.42350760199998));
#344784=CARTESIAN_POINT('Ctrl Pts',(4.44998101199995,12.2,1.42542713599998));
#344785=CARTESIAN_POINT('Ctrl Pts',(4.44998101199995,5.2,1.42542713599998));
#344786=CARTESIAN_POINT('Ctrl Pts',(4.44998101199995,2.2,1.42542713599998));
#344787=CARTESIAN_POINT('Ctrl Pts',(4.45164953699994,12.2,1.42735105399999));
#344788=CARTESIAN_POINT('Ctrl Pts',(4.45164953699994,5.2,1.42735105399999));
#344789=CARTESIAN_POINT('Ctrl Pts',(4.45164953699994,2.2,1.42735105399999));
#344790=CARTESIAN_POINT('Ctrl Pts',(4.45331832199995,12.2,1.42927935499999));
#344791=CARTESIAN_POINT('Ctrl Pts',(4.45331832199995,5.2,1.42927935499999));
#344792=CARTESIAN_POINT('Ctrl Pts',(4.45331832199995,2.2,1.42927935499999));
#344793=CARTESIAN_POINT('Ctrl Pts',(4.45498735999994,12.2,1.43121203999999));
#344794=CARTESIAN_POINT('Ctrl Pts',(4.45498735999994,5.2,1.43121203999999));
#344795=CARTESIAN_POINT('Ctrl Pts',(4.45498735999994,2.2,1.43121203999999));
#344796=CARTESIAN_POINT('Ctrl Pts',(4.45665664199994,12.2,1.43314910699999));
#344797=CARTESIAN_POINT('Ctrl Pts',(4.45665664199994,5.2,1.43314910699999));
#344798=CARTESIAN_POINT('Ctrl Pts',(4.45665664199994,2.2,1.43314910699999));
#344799=CARTESIAN_POINT('Ctrl Pts',(4.45832615899994,12.2,1.43509055599999));
#344800=CARTESIAN_POINT('Ctrl Pts',(4.45832615899994,5.2,1.43509055599999));
#344801=CARTESIAN_POINT('Ctrl Pts',(4.45832615899994,2.2,1.43509055599999));
#344802=CARTESIAN_POINT('Ctrl Pts',(4.45999590199994,12.2,1.43703638499999));
#344803=CARTESIAN_POINT('Ctrl Pts',(4.45999590199994,5.2,1.43703638499999));
#344804=CARTESIAN_POINT('Ctrl Pts',(4.45999590199994,2.2,1.43703638499999));
#344805=CARTESIAN_POINT('Ctrl Pts',(4.46166586199995,12.2,1.43898659599999));
#344806=CARTESIAN_POINT('Ctrl Pts',(4.46166586199995,5.2,1.43898659599999));
#344807=CARTESIAN_POINT('Ctrl Pts',(4.46166586199995,2.2,1.43898659599999));
#344808=CARTESIAN_POINT('Ctrl Pts',(4.46333603099994,12.2,1.44094118699998));
#344809=CARTESIAN_POINT('Ctrl Pts',(4.46333603099994,5.2,1.44094118699998));
#344810=CARTESIAN_POINT('Ctrl Pts',(4.46333603099994,2.2,1.44094118699998));
#344811=CARTESIAN_POINT('Ctrl Pts',(4.46500639899994,12.2,1.44290015799998));
#344812=CARTESIAN_POINT('Ctrl Pts',(4.46500639899994,5.2,1.44290015799998));
#344813=CARTESIAN_POINT('Ctrl Pts',(4.46500639899994,2.2,1.44290015799998));
#344814=CARTESIAN_POINT('Ctrl Pts',(4.46667695899994,12.2,1.44486350799998));
#344815=CARTESIAN_POINT('Ctrl Pts',(4.46667695899994,5.2,1.44486350799998));
#344816=CARTESIAN_POINT('Ctrl Pts',(4.46667695899994,2.2,1.44486350799998));
#344817=CARTESIAN_POINT('Ctrl Pts',(4.46834770199994,12.2,1.44683123499998));
#344818=CARTESIAN_POINT('Ctrl Pts',(4.46834770199994,5.2,1.44683123499998));
#344819=CARTESIAN_POINT('Ctrl Pts',(4.46834770199994,2.2,1.44683123499998));
#344820=CARTESIAN_POINT('Ctrl Pts',(4.47001861799994,12.2,1.44880333999998));
#344821=CARTESIAN_POINT('Ctrl Pts',(4.47001861799994,5.2,1.44880333999998));
#344822=CARTESIAN_POINT('Ctrl Pts',(4.47001861799994,2.2,1.44880333999998));
#344823=CARTESIAN_POINT('Ctrl Pts',(4.47168969899994,12.2,1.45077982299998));
#344824=CARTESIAN_POINT('Ctrl Pts',(4.47168969899994,5.2,1.45077982299998));
#344825=CARTESIAN_POINT('Ctrl Pts',(4.47168969899994,2.2,1.45077982299998));
#344826=CARTESIAN_POINT('Ctrl Pts',(4.47336093799994,12.2,1.45276068199998));
#344827=CARTESIAN_POINT('Ctrl Pts',(4.47336093799994,5.2,1.45276068199998));
#344828=CARTESIAN_POINT('Ctrl Pts',(4.47336093799994,2.2,1.45276068199998));
#344829=CARTESIAN_POINT('Ctrl Pts',(4.47503232199994,12.2,1.45474591699998));
#344830=CARTESIAN_POINT('Ctrl Pts',(4.47503232199994,5.2,1.45474591699998));
#344831=CARTESIAN_POINT('Ctrl Pts',(4.47503232199994,2.2,1.45474591699998));
#344832=CARTESIAN_POINT('Ctrl Pts',(4.47670384499994,12.2,1.45673552699999));
#344833=CARTESIAN_POINT('Ctrl Pts',(4.47670384499994,5.2,1.45673552699999));
#344834=CARTESIAN_POINT('Ctrl Pts',(4.47670384499994,2.2,1.45673552699999));
#344835=CARTESIAN_POINT('Ctrl Pts',(4.47837549599994,12.2,1.45872950999999));
#344836=CARTESIAN_POINT('Ctrl Pts',(4.47837549599994,5.2,1.45872950999999));
#344837=CARTESIAN_POINT('Ctrl Pts',(4.47837549599994,2.2,1.45872950999999));
#344838=CARTESIAN_POINT('Ctrl Pts',(4.48004726799994,12.2,1.46072786799999));
#344839=CARTESIAN_POINT('Ctrl Pts',(4.48004726799994,5.2,1.46072786799999));
#344840=CARTESIAN_POINT('Ctrl Pts',(4.48004726799994,2.2,1.46072786799999));
#344841=CARTESIAN_POINT('Ctrl Pts',(4.48171915199994,12.2,1.46273059799999));
#344842=CARTESIAN_POINT('Ctrl Pts',(4.48171915199994,5.2,1.46273059799999));
#344843=CARTESIAN_POINT('Ctrl Pts',(4.48171915199994,2.2,1.46273059799999));
#344844=CARTESIAN_POINT('Ctrl Pts',(4.48339113899995,12.2,1.46473769999998));
#344845=CARTESIAN_POINT('Ctrl Pts',(4.48339113899995,5.2,1.46473769999998));
#344846=CARTESIAN_POINT('Ctrl Pts',(4.48339113899995,2.2,1.46473769999998));
#344847=CARTESIAN_POINT('Ctrl Pts',(4.48506322299994,12.2,1.46674917399999));
#344848=CARTESIAN_POINT('Ctrl Pts',(4.48506322299994,5.2,1.46674917399999));
#344849=CARTESIAN_POINT('Ctrl Pts',(4.48506322299994,2.2,1.46674917399999));
#344850=CARTESIAN_POINT('Ctrl Pts',(4.48673539399994,12.2,1.46876501899999));
#344851=CARTESIAN_POINT('Ctrl Pts',(4.48673539399994,5.2,1.46876501899999));
#344852=CARTESIAN_POINT('Ctrl Pts',(4.48673539399994,2.2,1.46876501899999));
#344853=CARTESIAN_POINT('Ctrl Pts',(4.48840764599994,12.2,1.47078523499999));
#344854=CARTESIAN_POINT('Ctrl Pts',(4.48840764599994,5.2,1.47078523499999));
#344855=CARTESIAN_POINT('Ctrl Pts',(4.48840764599994,2.2,1.47078523499999));
#344856=CARTESIAN_POINT('Ctrl Pts',(4.49007996999994,12.2,1.47280981899998));
#344857=CARTESIAN_POINT('Ctrl Pts',(4.49007996999994,5.2,1.47280981899998));
#344858=CARTESIAN_POINT('Ctrl Pts',(4.49007996999994,2.2,1.47280981899998));
#344859=CARTESIAN_POINT('Ctrl Pts',(4.49175235499994,12.2,1.47483877199999));
#344860=CARTESIAN_POINT('Ctrl Pts',(4.49175235499994,5.2,1.47483877199999));
#344861=CARTESIAN_POINT('Ctrl Pts',(4.49175235499994,2.2,1.47483877199999));
#344862=CARTESIAN_POINT('Ctrl Pts',(4.49342479299994,12.2,1.47687209299999));
#344863=CARTESIAN_POINT('Ctrl Pts',(4.49342479299994,5.2,1.47687209299999));
#344864=CARTESIAN_POINT('Ctrl Pts',(4.49342479299994,2.2,1.47687209299999));
#344865=CARTESIAN_POINT('Ctrl Pts',(4.49509727099994,12.2,1.47890977999999));
#344866=CARTESIAN_POINT('Ctrl Pts',(4.49509727099994,5.2,1.47890977999999));
#344867=CARTESIAN_POINT('Ctrl Pts',(4.49509727099994,2.2,1.47890977999999));
#344868=CARTESIAN_POINT('Ctrl Pts',(4.49676977799994,12.2,1.48095183199999));
#344869=CARTESIAN_POINT('Ctrl Pts',(4.49676977799994,5.2,1.48095183199999));
#344870=CARTESIAN_POINT('Ctrl Pts',(4.49676977799994,2.2,1.48095183199999));
#344871=CARTESIAN_POINT('Ctrl Pts',(4.49844230699994,12.2,1.48299824999999));
#344872=CARTESIAN_POINT('Ctrl Pts',(4.49844230699994,5.2,1.48299824999999));
#344873=CARTESIAN_POINT('Ctrl Pts',(4.49844230699994,2.2,1.48299824999999));
#344874=CARTESIAN_POINT('Ctrl Pts',(4.50011484799994,12.2,1.48504903199999));
#344875=CARTESIAN_POINT('Ctrl Pts',(4.50011484799994,5.2,1.48504903199999));
#344876=CARTESIAN_POINT('Ctrl Pts',(4.50011484799994,2.2,1.48504903199999));
#344877=CARTESIAN_POINT('Ctrl Pts',(4.50178739499994,12.2,1.48710417599998));
#344878=CARTESIAN_POINT('Ctrl Pts',(4.50178739499994,5.2,1.48710417599998));
#344879=CARTESIAN_POINT('Ctrl Pts',(4.50178739499994,2.2,1.48710417599998));
#344880=CARTESIAN_POINT('Ctrl Pts',(4.50345994399994,12.2,1.48916368399998));
#344881=CARTESIAN_POINT('Ctrl Pts',(4.50345994399994,5.2,1.48916368399998));
#344882=CARTESIAN_POINT('Ctrl Pts',(4.50345994399994,2.2,1.48916368399998));
#344883=CARTESIAN_POINT('Ctrl Pts',(4.5051324930519,12.2,1.4912275540641));
#344884=CARTESIAN_POINT('Ctrl Pts',(4.5051324930519,5.2,1.4912275540641));
#344885=CARTESIAN_POINT('Ctrl Pts',(4.5051324930519,2.2,1.4912275540641));
#344886=CARTESIAN_POINT('Ctrl Pts',(4.50647053110386,12.2,1.49288214012849));
#344887=CARTESIAN_POINT('Ctrl Pts',(4.50647053110386,5.2,1.49288214012849));
#344888=CARTESIAN_POINT('Ctrl Pts',(4.50647053110386,2.2,1.49288214012849));
#344889=CARTESIAN_POINT('Ctrl Pts',(4.50747405915582,12.2,1.49412504219303));
#344890=CARTESIAN_POINT('Ctrl Pts',(4.50747405915582,5.2,1.49412504219303));
#344891=CARTESIAN_POINT('Ctrl Pts',(4.50747405915582,2.2,1.49412504219303));
#344892=CARTESIAN_POINT('Ctrl Pts',(4.50814307720777,12.2,1.49495451625766));
#344893=CARTESIAN_POINT('Ctrl Pts',(4.50814307720777,5.2,1.49495451625766));
#344894=CARTESIAN_POINT('Ctrl Pts',(4.50814307720777,2.2,1.49495451625766));
#344895=CARTESIAN_POINT('Ctrl Pts',(4.50847758599994,12.2,1.49536947099998));
#344896=CARTESIAN_POINT('Ctrl Pts',(4.50847758599994,5.2,1.49536947099998));
#344897=CARTESIAN_POINT('Ctrl Pts',(4.50847758599994,2.2,1.49536947099998));
#344898=CARTESIAN_POINT('',(3.87111410199994,12.2,0.982006995999987));
#344899=CARTESIAN_POINT('Origin',(-5.66300478732629E-14,15.2,-1.77635683940025E-14));
#344900=CARTESIAN_POINT('',(3.51370677999994,12.2,0.891341496999987));
#344901=CARTESIAN_POINT('Origin',(-5.66300478732629E-14,15.2,-1.77635683940025E-14));
#344902=CARTESIAN_POINT('Origin',(-5.66300478732629E-14,15.2,-1.77635683940025E-14));
#344903=CARTESIAN_POINT('',(3.60918509199994,2.2,0.338242477999984));
#344904=CARTESIAN_POINT('Origin',(-5.66300478732629E-14,15.2,-1.77635683940025E-14));
#344905=CARTESIAN_POINT('',(3.96444824099994,12.2,-0.482713455000017));
#344906=CARTESIAN_POINT('',(3.59842368199994,12.2,-0.438146099000014));
#344907=CARTESIAN_POINT('Origin',(3.97627021699994,15.2,0.372644643999984));
#344908=CARTESIAN_POINT('',(3.97632130999995,12.2,0.372649431999985));
#344909=CARTESIAN_POINT('Ctrl Pts',(4.74889012999994,12.2,0.102676827999986));
#344910=CARTESIAN_POINT('Ctrl Pts',(4.74889012999994,5.2,0.102676827999986));
#344911=CARTESIAN_POINT('Ctrl Pts',(4.74889012999994,2.2,0.102676827999986));
#344912=CARTESIAN_POINT('Ctrl Pts',(4.74843586199994,12.2,0.102955621999987));
#344913=CARTESIAN_POINT('Ctrl Pts',(4.74843586199994,5.2,0.102955621999987));
#344914=CARTESIAN_POINT('Ctrl Pts',(4.74843586199994,2.2,0.102955621999987));
#344915=CARTESIAN_POINT('Ctrl Pts',(4.74752747599994,12.2,0.103512796999983));
#344916=CARTESIAN_POINT('Ctrl Pts',(4.74752747599994,5.2,0.103512796999983));
#344917=CARTESIAN_POINT('Ctrl Pts',(4.74752747599994,2.2,0.103512796999983));
#344918=CARTESIAN_POINT('Ctrl Pts',(4.74616533299994,12.2,0.104347326999985));
#344919=CARTESIAN_POINT('Ctrl Pts',(4.74616533299994,5.2,0.104347326999985));
#344920=CARTESIAN_POINT('Ctrl Pts',(4.74616533299994,2.2,0.104347326999985));
#344921=CARTESIAN_POINT('Ctrl Pts',(4.74435001799994,12.2,0.105457566999987));
#344922=CARTESIAN_POINT('Ctrl Pts',(4.74435001799994,5.2,0.105457566999987));
#344923=CARTESIAN_POINT('Ctrl Pts',(4.74435001799994,2.2,0.105457566999987));
#344924=CARTESIAN_POINT('Ctrl Pts',(4.74208233599994,12.2,0.106841257999988));
#344925=CARTESIAN_POINT('Ctrl Pts',(4.74208233599994,5.2,0.106841257999988));
#344926=CARTESIAN_POINT('Ctrl Pts',(4.74208233599994,2.2,0.106841257999988));
#344927=CARTESIAN_POINT('Ctrl Pts',(4.73981611699994,12.2,0.108220837999986));
#344928=CARTESIAN_POINT('Ctrl Pts',(4.73981611699994,5.2,0.108220837999986));
#344929=CARTESIAN_POINT('Ctrl Pts',(4.73981611699994,2.2,0.108220837999986));
#344930=CARTESIAN_POINT('Ctrl Pts',(4.73755136299994,12.2,0.109596309999986));
#344931=CARTESIAN_POINT('Ctrl Pts',(4.73755136299994,5.2,0.109596309999986));
#344932=CARTESIAN_POINT('Ctrl Pts',(4.73755136299994,2.2,0.109596309999986));
#344933=CARTESIAN_POINT('Ctrl Pts',(4.73528807699994,12.2,0.110967671999984));
#344934=CARTESIAN_POINT('Ctrl Pts',(4.73528807699994,5.2,0.110967671999984));
#344935=CARTESIAN_POINT('Ctrl Pts',(4.73528807699994,2.2,0.110967671999984));
#344936=CARTESIAN_POINT('Ctrl Pts',(4.73302626599994,12.2,0.112334925999988));
#344937=CARTESIAN_POINT('Ctrl Pts',(4.73302626599994,5.2,0.112334925999988));
#344938=CARTESIAN_POINT('Ctrl Pts',(4.73302626599994,2.2,0.112334925999988));
#344939=CARTESIAN_POINT('Ctrl Pts',(4.73076593799994,12.2,0.113698076999986));
#344940=CARTESIAN_POINT('Ctrl Pts',(4.73076593799994,5.2,0.113698076999986));
#344941=CARTESIAN_POINT('Ctrl Pts',(4.73076593799994,2.2,0.113698076999986));
#344942=CARTESIAN_POINT('Ctrl Pts',(4.72850710099994,12.2,0.115057122999982));
#344943=CARTESIAN_POINT('Ctrl Pts',(4.72850710099994,5.2,0.115057122999982));
#344944=CARTESIAN_POINT('Ctrl Pts',(4.72850710099994,2.2,0.115057122999982));
#344945=CARTESIAN_POINT('Ctrl Pts',(4.72624976699994,12.2,0.116412069999985));
#344946=CARTESIAN_POINT('Ctrl Pts',(4.72624976699994,5.2,0.116412069999985));
#344947=CARTESIAN_POINT('Ctrl Pts',(4.72624976699994,2.2,0.116412069999985));
#344948=CARTESIAN_POINT('Ctrl Pts',(4.72399394499994,12.2,0.117762919999986));
#344949=CARTESIAN_POINT('Ctrl Pts',(4.72399394499994,5.2,0.117762919999986));
#344950=CARTESIAN_POINT('Ctrl Pts',(4.72399394499994,2.2,0.117762919999986));
#344951=CARTESIAN_POINT('Ctrl Pts',(4.72173964699994,12.2,0.119109672999986));
#344952=CARTESIAN_POINT('Ctrl Pts',(4.72173964699994,5.2,0.119109672999986));
#344953=CARTESIAN_POINT('Ctrl Pts',(4.72173964699994,2.2,0.119109672999986));
#344954=CARTESIAN_POINT('Ctrl Pts',(4.71948688099994,12.2,0.120452335999985));
#344955=CARTESIAN_POINT('Ctrl Pts',(4.71948688099994,5.2,0.120452335999985));
#344956=CARTESIAN_POINT('Ctrl Pts',(4.71948688099994,2.2,0.120452335999985));
#344957=CARTESIAN_POINT('Ctrl Pts',(4.71723565499994,12.2,0.121790906999983));
#344958=CARTESIAN_POINT('Ctrl Pts',(4.71723565499994,5.2,0.121790906999983));
#344959=CARTESIAN_POINT('Ctrl Pts',(4.71723565499994,2.2,0.121790906999983));
#344960=CARTESIAN_POINT('Ctrl Pts',(4.71498597799994,12.2,0.123125388999985));
#344961=CARTESIAN_POINT('Ctrl Pts',(4.71498597799994,5.2,0.123125388999985));
#344962=CARTESIAN_POINT('Ctrl Pts',(4.71498597799994,2.2,0.123125388999985));
#344963=CARTESIAN_POINT('Ctrl Pts',(4.71273785699994,12.2,0.124455785999986));
#344964=CARTESIAN_POINT('Ctrl Pts',(4.71273785699994,5.2,0.124455785999986));
#344965=CARTESIAN_POINT('Ctrl Pts',(4.71273785699994,2.2,0.124455785999986));
#344966=CARTESIAN_POINT('Ctrl Pts',(4.71049130099994,12.2,0.125782098999987));
#344967=CARTESIAN_POINT('Ctrl Pts',(4.71049130099994,5.2,0.125782098999987));
#344968=CARTESIAN_POINT('Ctrl Pts',(4.71049130099994,2.2,0.125782098999987));
#344969=CARTESIAN_POINT('Ctrl Pts',(4.70824631499994,12.2,0.127104328999987));
#344970=CARTESIAN_POINT('Ctrl Pts',(4.70824631499994,5.2,0.127104328999987));
#344971=CARTESIAN_POINT('Ctrl Pts',(4.70824631499994,2.2,0.127104328999987));
#344972=CARTESIAN_POINT('Ctrl Pts',(4.70600290799994,12.2,0.128422478999983));
#344973=CARTESIAN_POINT('Ctrl Pts',(4.70600290799994,5.2,0.128422478999983));
#344974=CARTESIAN_POINT('Ctrl Pts',(4.70600290799994,2.2,0.128422478999983));
#344975=CARTESIAN_POINT('Ctrl Pts',(4.70376108999994,12.2,0.129736550999984));
#344976=CARTESIAN_POINT('Ctrl Pts',(4.70376108999994,5.2,0.129736550999984));
#344977=CARTESIAN_POINT('Ctrl Pts',(4.70376108999994,2.2,0.129736550999984));
#344978=CARTESIAN_POINT('Ctrl Pts',(4.70152086799994,12.2,0.131046545999984));
#344979=CARTESIAN_POINT('Ctrl Pts',(4.70152086799994,5.2,0.131046545999984));
#344980=CARTESIAN_POINT('Ctrl Pts',(4.70152086799994,2.2,0.131046545999984));
#344981=CARTESIAN_POINT('Ctrl Pts',(4.69928225199994,12.2,0.132352469999986));
#344982=CARTESIAN_POINT('Ctrl Pts',(4.69928225199994,5.2,0.132352469999986));
#344983=CARTESIAN_POINT('Ctrl Pts',(4.69928225199994,2.2,0.132352469999986));
#344984=CARTESIAN_POINT('Ctrl Pts',(4.69704524999994,12.2,0.133654322999988));
#344985=CARTESIAN_POINT('Ctrl Pts',(4.69704524999994,5.2,0.133654322999988));
#344986=CARTESIAN_POINT('Ctrl Pts',(4.69704524999994,2.2,0.133654322999988));
#344987=CARTESIAN_POINT('Ctrl Pts',(4.69480987199994,12.2,0.134952106999986));
#344988=CARTESIAN_POINT('Ctrl Pts',(4.69480987199994,5.2,0.134952106999986));
#344989=CARTESIAN_POINT('Ctrl Pts',(4.69480987199994,2.2,0.134952106999986));
#344990=CARTESIAN_POINT('Ctrl Pts',(4.69257612499994,12.2,0.136245824999985));
#344991=CARTESIAN_POINT('Ctrl Pts',(4.69257612499994,5.2,0.136245824999985));
#344992=CARTESIAN_POINT('Ctrl Pts',(4.69257612499994,2.2,0.136245824999985));
#344993=CARTESIAN_POINT('Ctrl Pts',(4.69034401799994,12.2,0.137535479999986));
#344994=CARTESIAN_POINT('Ctrl Pts',(4.69034401799994,5.2,0.137535479999986));
#344995=CARTESIAN_POINT('Ctrl Pts',(4.69034401799994,2.2,0.137535479999986));
#344996=CARTESIAN_POINT('Ctrl Pts',(4.68811355899994,12.2,0.138821072999988));
#344997=CARTESIAN_POINT('Ctrl Pts',(4.68811355899994,5.2,0.138821072999988));
#344998=CARTESIAN_POINT('Ctrl Pts',(4.68811355899994,2.2,0.138821072999988));
#344999=CARTESIAN_POINT('Ctrl Pts',(4.68588475599994,12.2,0.140102605999988));
#345000=CARTESIAN_POINT('Ctrl Pts',(4.68588475599994,5.2,0.140102605999988));
#345001=CARTESIAN_POINT('Ctrl Pts',(4.68588475599994,2.2,0.140102605999988));
#345002=CARTESIAN_POINT('Ctrl Pts',(4.68365761899994,12.2,0.141380083999985));
#345003=CARTESIAN_POINT('Ctrl Pts',(4.68365761899994,5.2,0.141380083999985));
#345004=CARTESIAN_POINT('Ctrl Pts',(4.68365761899994,2.2,0.141380083999985));
#345005=CARTESIAN_POINT('Ctrl Pts',(4.68143215399994,12.2,0.142653506999988));
#345006=CARTESIAN_POINT('Ctrl Pts',(4.68143215399994,5.2,0.142653506999988));
#345007=CARTESIAN_POINT('Ctrl Pts',(4.68143215399994,2.2,0.142653506999988));
#345008=CARTESIAN_POINT('Ctrl Pts',(4.67920837299994,12.2,0.143922876999985));
#345009=CARTESIAN_POINT('Ctrl Pts',(4.67920837299994,5.2,0.143922876999985));
#345010=CARTESIAN_POINT('Ctrl Pts',(4.67920837299994,2.2,0.143922876999985));
#345011=CARTESIAN_POINT('Ctrl Pts',(4.67698627999994,12.2,0.145188198999988));
#345012=CARTESIAN_POINT('Ctrl Pts',(4.67698627999994,5.2,0.145188198999988));
#345013=CARTESIAN_POINT('Ctrl Pts',(4.67698627999994,2.2,0.145188198999988));
#345014=CARTESIAN_POINT('Ctrl Pts',(4.67476588699994,12.2,0.146449472999985));
#345015=CARTESIAN_POINT('Ctrl Pts',(4.67476588699994,5.2,0.146449472999985));
#345016=CARTESIAN_POINT('Ctrl Pts',(4.67476588699994,2.2,0.146449472999985));
#345017=CARTESIAN_POINT('Ctrl Pts',(4.67254720199994,12.2,0.147706702999986));
#345018=CARTESIAN_POINT('Ctrl Pts',(4.67254720199994,5.2,0.147706702999986));
#345019=CARTESIAN_POINT('Ctrl Pts',(4.67254720199994,2.2,0.147706702999986));
#345020=CARTESIAN_POINT('Ctrl Pts',(4.67033023199994,12.2,0.148959889999984));
#345021=CARTESIAN_POINT('Ctrl Pts',(4.67033023199994,5.2,0.148959889999984));
#345022=CARTESIAN_POINT('Ctrl Pts',(4.67033023199994,2.2,0.148959889999984));
#345023=CARTESIAN_POINT('Ctrl Pts',(4.66811498799994,12.2,0.150209038999982));
#345024=CARTESIAN_POINT('Ctrl Pts',(4.66811498799994,5.2,0.150209038999982));
#345025=CARTESIAN_POINT('Ctrl Pts',(4.66811498799994,2.2,0.150209038999982));
#345026=CARTESIAN_POINT('Ctrl Pts',(4.66590147699994,12.2,0.151454149999988));
#345027=CARTESIAN_POINT('Ctrl Pts',(4.66590147699994,5.2,0.151454149999988));
#345028=CARTESIAN_POINT('Ctrl Pts',(4.66590147699994,2.2,0.151454149999988));
#345029=CARTESIAN_POINT('Ctrl Pts',(4.66368970599994,12.2,0.152695225999988));
#345030=CARTESIAN_POINT('Ctrl Pts',(4.66368970599994,5.2,0.152695225999988));
#345031=CARTESIAN_POINT('Ctrl Pts',(4.66368970599994,2.2,0.152695225999988));
#345032=CARTESIAN_POINT('Ctrl Pts',(4.66147968699994,12.2,0.153932269999988));
#345033=CARTESIAN_POINT('Ctrl Pts',(4.66147968699994,5.2,0.153932269999988));
#345034=CARTESIAN_POINT('Ctrl Pts',(4.66147968699994,2.2,0.153932269999988));
#345035=CARTESIAN_POINT('Ctrl Pts',(4.65927142699994,12.2,0.155165283999987));
#345036=CARTESIAN_POINT('Ctrl Pts',(4.65927142699994,5.2,0.155165283999987));
#345037=CARTESIAN_POINT('Ctrl Pts',(4.65927142699994,2.2,0.155165283999987));
#345038=CARTESIAN_POINT('Ctrl Pts',(4.65706493399995,12.2,0.156394271999982));
#345039=CARTESIAN_POINT('Ctrl Pts',(4.65706493399995,5.2,0.156394271999982));
#345040=CARTESIAN_POINT('Ctrl Pts',(4.65706493399995,2.2,0.156394271999982));
#345041=CARTESIAN_POINT('Ctrl Pts',(4.65486021599994,12.2,0.157619235999986));
#345042=CARTESIAN_POINT('Ctrl Pts',(4.65486021599994,5.2,0.157619235999986));
#345043=CARTESIAN_POINT('Ctrl Pts',(4.65486021599994,2.2,0.157619235999986));
#345044=CARTESIAN_POINT('Ctrl Pts',(4.65265728299994,12.2,0.158840176999986));
#345045=CARTESIAN_POINT('Ctrl Pts',(4.65265728299994,5.2,0.158840176999986));
#345046=CARTESIAN_POINT('Ctrl Pts',(4.65265728299994,2.2,0.158840176999986));
#345047=CARTESIAN_POINT('Ctrl Pts',(4.65045614299994,12.2,0.160057098999986));
#345048=CARTESIAN_POINT('Ctrl Pts',(4.65045614299994,5.2,0.160057098999986));
#345049=CARTESIAN_POINT('Ctrl Pts',(4.65045614299994,2.2,0.160057098999986));
#345050=CARTESIAN_POINT('Ctrl Pts',(4.64825680499994,12.2,0.161270003999987));
#345051=CARTESIAN_POINT('Ctrl Pts',(4.64825680499994,5.2,0.161270003999987));
#345052=CARTESIAN_POINT('Ctrl Pts',(4.64825680499994,2.2,0.161270003999987));
#345053=CARTESIAN_POINT('Ctrl Pts',(4.64605927599994,12.2,0.162478894999989));
#345054=CARTESIAN_POINT('Ctrl Pts',(4.64605927599994,5.2,0.162478894999989));
#345055=CARTESIAN_POINT('Ctrl Pts',(4.64605927599994,2.2,0.162478894999989));
#345056=CARTESIAN_POINT('Ctrl Pts',(4.64386356799994,12.2,0.163683775999988));
#345057=CARTESIAN_POINT('Ctrl Pts',(4.64386356799994,5.2,0.163683775999988));
#345058=CARTESIAN_POINT('Ctrl Pts',(4.64386356799994,2.2,0.163683775999988));
#345059=CARTESIAN_POINT('Ctrl Pts',(4.64166968599994,12.2,0.164884647999983));
#345060=CARTESIAN_POINT('Ctrl Pts',(4.64166968599994,5.2,0.164884647999983));
#345061=CARTESIAN_POINT('Ctrl Pts',(4.64166968599994,2.2,0.164884647999983));
#345062=CARTESIAN_POINT('Ctrl Pts',(4.63947764099994,12.2,0.166081512999985));
#345063=CARTESIAN_POINT('Ctrl Pts',(4.63947764099994,5.2,0.166081512999985));
#345064=CARTESIAN_POINT('Ctrl Pts',(4.63947764099994,2.2,0.166081512999985));
#345065=CARTESIAN_POINT('Ctrl Pts',(4.63728744099994,12.2,0.167274374999984));
#345066=CARTESIAN_POINT('Ctrl Pts',(4.63728744099994,5.2,0.167274374999984));
#345067=CARTESIAN_POINT('Ctrl Pts',(4.63728744099994,2.2,0.167274374999984));
#345068=CARTESIAN_POINT('Ctrl Pts',(4.63509909399995,12.2,0.168463236999985));
#345069=CARTESIAN_POINT('Ctrl Pts',(4.63509909399995,5.2,0.168463236999985));
#345070=CARTESIAN_POINT('Ctrl Pts',(4.63509909399995,2.2,0.168463236999985));
#345071=CARTESIAN_POINT('Ctrl Pts',(4.63291260899994,12.2,0.169648099999984));
#345072=CARTESIAN_POINT('Ctrl Pts',(4.63291260899994,5.2,0.169648099999984));
#345073=CARTESIAN_POINT('Ctrl Pts',(4.63291260899994,2.2,0.169648099999984));
#345074=CARTESIAN_POINT('Ctrl Pts',(4.63072799499994,12.2,0.170828968999985));
#345075=CARTESIAN_POINT('Ctrl Pts',(4.63072799499994,5.2,0.170828968999985));
#345076=CARTESIAN_POINT('Ctrl Pts',(4.63072799499994,2.2,0.170828968999985));
#345077=CARTESIAN_POINT('Ctrl Pts',(4.62854525999994,12.2,0.172005844999985));
#345078=CARTESIAN_POINT('Ctrl Pts',(4.62854525999994,5.2,0.172005844999985));
#345079=CARTESIAN_POINT('Ctrl Pts',(4.62854525999994,2.2,0.172005844999985));
#345080=CARTESIAN_POINT('Ctrl Pts',(4.62636441299995,12.2,0.173178731999983));
#345081=CARTESIAN_POINT('Ctrl Pts',(4.62636441299995,5.2,0.173178731999983));
#345082=CARTESIAN_POINT('Ctrl Pts',(4.62636441299995,2.2,0.173178731999983));
#345083=CARTESIAN_POINT('Ctrl Pts',(4.62418546299994,12.2,0.174347630999985));
#345084=CARTESIAN_POINT('Ctrl Pts',(4.62418546299994,5.2,0.174347630999985));
#345085=CARTESIAN_POINT('Ctrl Pts',(4.62418546299994,2.2,0.174347630999985));
#345086=CARTESIAN_POINT('Ctrl Pts',(4.62200841899994,12.2,0.175512546999985));
#345087=CARTESIAN_POINT('Ctrl Pts',(4.62200841899994,5.2,0.175512546999985));
#345088=CARTESIAN_POINT('Ctrl Pts',(4.62200841899994,2.2,0.175512546999985));
#345089=CARTESIAN_POINT('Ctrl Pts',(4.61983328799994,12.2,0.176673481999985));
#345090=CARTESIAN_POINT('Ctrl Pts',(4.61983328799994,5.2,0.176673481999985));
#345091=CARTESIAN_POINT('Ctrl Pts',(4.61983328799994,2.2,0.176673481999985));
#345092=CARTESIAN_POINT('Ctrl Pts',(4.61766008099994,12.2,0.177830437999984));
#345093=CARTESIAN_POINT('Ctrl Pts',(4.61766008099994,5.2,0.177830437999984));
#345094=CARTESIAN_POINT('Ctrl Pts',(4.61766008099994,2.2,0.177830437999984));
#345095=CARTESIAN_POINT('Ctrl Pts',(4.61548880399994,12.2,0.178983417999987));
#345096=CARTESIAN_POINT('Ctrl Pts',(4.61548880399994,5.2,0.178983417999987));
#345097=CARTESIAN_POINT('Ctrl Pts',(4.61548880399994,2.2,0.178983417999987));
#345098=CARTESIAN_POINT('Ctrl Pts',(4.61331946799994,12.2,0.180132425999986));
#345099=CARTESIAN_POINT('Ctrl Pts',(4.61331946799994,5.2,0.180132425999986));
#345100=CARTESIAN_POINT('Ctrl Pts',(4.61331946799994,2.2,0.180132425999986));
#345101=CARTESIAN_POINT('Ctrl Pts',(4.61115208099994,12.2,0.181277463999985));
#345102=CARTESIAN_POINT('Ctrl Pts',(4.61115208099994,5.2,0.181277463999985));
#345103=CARTESIAN_POINT('Ctrl Pts',(4.61115208099994,2.2,0.181277463999985));
#345104=CARTESIAN_POINT('Ctrl Pts',(4.60898665099994,12.2,0.182418534999984));
#345105=CARTESIAN_POINT('Ctrl Pts',(4.60898665099994,5.2,0.182418534999984));
#345106=CARTESIAN_POINT('Ctrl Pts',(4.60898665099994,2.2,0.182418534999984));
#345107=CARTESIAN_POINT('Ctrl Pts',(4.60682318899994,12.2,0.183555642999984));
#345108=CARTESIAN_POINT('Ctrl Pts',(4.60682318899994,5.2,0.183555642999984));
#345109=CARTESIAN_POINT('Ctrl Pts',(4.60682318899994,2.2,0.183555642999984));
#345110=CARTESIAN_POINT('Ctrl Pts',(4.60466170099994,12.2,0.184688787999985));
#345111=CARTESIAN_POINT('Ctrl Pts',(4.60466170099994,5.2,0.184688787999985));
#345112=CARTESIAN_POINT('Ctrl Pts',(4.60466170099994,2.2,0.184688787999985));
#345113=CARTESIAN_POINT('Ctrl Pts',(4.60250219699994,12.2,0.185817975999987));
#345114=CARTESIAN_POINT('Ctrl Pts',(4.60250219699994,5.2,0.185817975999987));
#345115=CARTESIAN_POINT('Ctrl Pts',(4.60250219699994,2.2,0.185817975999987));
#345116=CARTESIAN_POINT('Ctrl Pts',(4.60034468499994,12.2,0.186943208999986));
#345117=CARTESIAN_POINT('Ctrl Pts',(4.60034468499994,5.2,0.186943208999986));
#345118=CARTESIAN_POINT('Ctrl Pts',(4.60034468499994,2.2,0.186943208999986));
#345119=CARTESIAN_POINT('Ctrl Pts',(4.59818917499994,12.2,0.188064488999986));
#345120=CARTESIAN_POINT('Ctrl Pts',(4.59818917499994,5.2,0.188064488999986));
#345121=CARTESIAN_POINT('Ctrl Pts',(4.59818917499994,2.2,0.188064488999986));
#345122=CARTESIAN_POINT('Ctrl Pts',(4.59603567499994,12.2,0.189181820999984));
#345123=CARTESIAN_POINT('Ctrl Pts',(4.59603567499994,5.2,0.189181820999984));
#345124=CARTESIAN_POINT('Ctrl Pts',(4.59603567499994,2.2,0.189181820999984));
#345125=CARTESIAN_POINT('Ctrl Pts',(4.59388419399994,12.2,0.190295204999984));
#345126=CARTESIAN_POINT('Ctrl Pts',(4.59388419399994,5.2,0.190295204999984));
#345127=CARTESIAN_POINT('Ctrl Pts',(4.59388419399994,2.2,0.190295204999984));
#345128=CARTESIAN_POINT('Ctrl Pts',(4.59173473999994,12.2,0.191404646999986));
#345129=CARTESIAN_POINT('Ctrl Pts',(4.59173473999994,5.2,0.191404646999986));
#345130=CARTESIAN_POINT('Ctrl Pts',(4.59173473999994,2.2,0.191404646999986));
#345131=CARTESIAN_POINT('Ctrl Pts',(4.58958732499995,12.2,0.192510148999983));
#345132=CARTESIAN_POINT('Ctrl Pts',(4.58958732499995,5.2,0.192510148999983));
#345133=CARTESIAN_POINT('Ctrl Pts',(4.58958732499995,2.2,0.192510148999983));
#345134=CARTESIAN_POINT('Ctrl Pts',(4.58744195199994,12.2,0.193611713999986));
#345135=CARTESIAN_POINT('Ctrl Pts',(4.58744195199994,5.2,0.193611713999986));
#345136=CARTESIAN_POINT('Ctrl Pts',(4.58744195199994,2.2,0.193611713999986));
#345137=CARTESIAN_POINT('Ctrl Pts',(4.58529863499994,12.2,0.194709342999988));
#345138=CARTESIAN_POINT('Ctrl Pts',(4.58529863499994,5.2,0.194709342999988));
#345139=CARTESIAN_POINT('Ctrl Pts',(4.58529863499994,2.2,0.194709342999988));
#345140=CARTESIAN_POINT('Ctrl Pts',(4.58315737999994,12.2,0.195803042999985));
#345141=CARTESIAN_POINT('Ctrl Pts',(4.58315737999994,5.2,0.195803042999985));
#345142=CARTESIAN_POINT('Ctrl Pts',(4.58315737999994,2.2,0.195803042999985));
#345143=CARTESIAN_POINT('Ctrl Pts',(4.58101819799994,12.2,0.196892814999985));
#345144=CARTESIAN_POINT('Ctrl Pts',(4.58101819799994,5.2,0.196892814999985));
#345145=CARTESIAN_POINT('Ctrl Pts',(4.58101819799994,2.2,0.196892814999985));
#345146=CARTESIAN_POINT('Ctrl Pts',(4.57888109499994,12.2,0.197978660999985));
#345147=CARTESIAN_POINT('Ctrl Pts',(4.57888109499994,5.2,0.197978660999985));
#345148=CARTESIAN_POINT('Ctrl Pts',(4.57888109499994,2.2,0.197978660999985));
#345149=CARTESIAN_POINT('Ctrl Pts',(4.57674608199994,12.2,0.199060585999984));
#345150=CARTESIAN_POINT('Ctrl Pts',(4.57674608199994,5.2,0.199060585999984));
#345151=CARTESIAN_POINT('Ctrl Pts',(4.57674608199994,2.2,0.199060585999984));
#345152=CARTESIAN_POINT('Ctrl Pts',(4.57461316799994,12.2,0.200138592999988));
#345153=CARTESIAN_POINT('Ctrl Pts',(4.57461316799994,5.2,0.200138592999988));
#345154=CARTESIAN_POINT('Ctrl Pts',(4.57461316799994,2.2,0.200138592999988));
#345155=CARTESIAN_POINT('Ctrl Pts',(4.57248235999994,12.2,0.201212683999987));
#345156=CARTESIAN_POINT('Ctrl Pts',(4.57248235999994,5.2,0.201212683999987));
#345157=CARTESIAN_POINT('Ctrl Pts',(4.57248235999994,2.2,0.201212683999987));
#345158=CARTESIAN_POINT('Ctrl Pts',(4.57035366899994,12.2,0.202282863999983));
#345159=CARTESIAN_POINT('Ctrl Pts',(4.57035366899994,5.2,0.202282863999983));
#345160=CARTESIAN_POINT('Ctrl Pts',(4.57035366899994,2.2,0.202282863999983));
#345161=CARTESIAN_POINT('Ctrl Pts',(4.56822710199994,12.2,0.203349133999984));
#345162=CARTESIAN_POINT('Ctrl Pts',(4.56822710199994,5.2,0.203349133999984));
#345163=CARTESIAN_POINT('Ctrl Pts',(4.56822710199994,2.2,0.203349133999984));
#345164=CARTESIAN_POINT('Ctrl Pts',(4.56610266799994,12.2,0.204411497999986));
#345165=CARTESIAN_POINT('Ctrl Pts',(4.56610266799994,5.2,0.204411497999986));
#345166=CARTESIAN_POINT('Ctrl Pts',(4.56610266799994,2.2,0.204411497999986));
#345167=CARTESIAN_POINT('Ctrl Pts',(4.56398037799994,12.2,0.205469959999984));
#345168=CARTESIAN_POINT('Ctrl Pts',(4.56398037799994,5.2,0.205469959999984));
#345169=CARTESIAN_POINT('Ctrl Pts',(4.56398037799994,2.2,0.205469959999984));
#345170=CARTESIAN_POINT('Ctrl Pts',(4.56186023799994,12.2,0.206524522999985));
#345171=CARTESIAN_POINT('Ctrl Pts',(4.56186023799994,5.2,0.206524522999985));
#345172=CARTESIAN_POINT('Ctrl Pts',(4.56186023799994,2.2,0.206524522999985));
#345173=CARTESIAN_POINT('Ctrl Pts',(4.55974225999994,12.2,0.207575188999982));
#345174=CARTESIAN_POINT('Ctrl Pts',(4.55974225999994,5.2,0.207575188999982));
#345175=CARTESIAN_POINT('Ctrl Pts',(4.55974225999994,2.2,0.207575188999982));
#345176=CARTESIAN_POINT('Ctrl Pts',(4.55762644999994,12.2,0.208621963999986));
#345177=CARTESIAN_POINT('Ctrl Pts',(4.55762644999994,5.2,0.208621963999986));
#345178=CARTESIAN_POINT('Ctrl Pts',(4.55762644999994,2.2,0.208621963999986));
#345179=CARTESIAN_POINT('Ctrl Pts',(4.55551281799994,12.2,0.209664847999989));
#345180=CARTESIAN_POINT('Ctrl Pts',(4.55551281799994,5.2,0.209664847999989));
#345181=CARTESIAN_POINT('Ctrl Pts',(4.55551281799994,2.2,0.209664847999989));
#345182=CARTESIAN_POINT('Ctrl Pts',(4.55340137299994,12.2,0.210703846999984));
#345183=CARTESIAN_POINT('Ctrl Pts',(4.55340137299994,5.2,0.210703846999984));
#345184=CARTESIAN_POINT('Ctrl Pts',(4.55340137299994,2.2,0.210703846999984));
#345185=CARTESIAN_POINT('Ctrl Pts',(4.55129212499994,12.2,0.211738961999988));
#345186=CARTESIAN_POINT('Ctrl Pts',(4.55129212499994,5.2,0.211738961999988));
#345187=CARTESIAN_POINT('Ctrl Pts',(4.55129212499994,2.2,0.211738961999988));
#345188=CARTESIAN_POINT('Ctrl Pts',(4.54918508099994,12.2,0.212770198999985));
#345189=CARTESIAN_POINT('Ctrl Pts',(4.54918508099994,5.2,0.212770198999985));
#345190=CARTESIAN_POINT('Ctrl Pts',(4.54918508099994,2.2,0.212770198999985));
#345191=CARTESIAN_POINT('Ctrl Pts',(4.54708025099994,12.2,0.213797558999986));
#345192=CARTESIAN_POINT('Ctrl Pts',(4.54708025099994,5.2,0.213797558999986));
#345193=CARTESIAN_POINT('Ctrl Pts',(4.54708025099994,2.2,0.213797558999986));
#345194=CARTESIAN_POINT('Ctrl Pts',(4.54497764299994,12.2,0.214821045999987));
#345195=CARTESIAN_POINT('Ctrl Pts',(4.54497764299994,5.2,0.214821045999987));
#345196=CARTESIAN_POINT('Ctrl Pts',(4.54497764299994,2.2,0.214821045999987));
#345197=CARTESIAN_POINT('Ctrl Pts',(4.54287726799994,12.2,0.215840664999987));
#345198=CARTESIAN_POINT('Ctrl Pts',(4.54287726799994,5.2,0.215840664999987));
#345199=CARTESIAN_POINT('Ctrl Pts',(4.54287726799994,2.2,0.215840664999987));
#345200=CARTESIAN_POINT('Ctrl Pts',(4.54077913299994,12.2,0.216856416999986));
#345201=CARTESIAN_POINT('Ctrl Pts',(4.54077913299994,5.2,0.216856416999986));
#345202=CARTESIAN_POINT('Ctrl Pts',(4.54077913299994,2.2,0.216856416999986));
#345203=CARTESIAN_POINT('Ctrl Pts',(4.53868324699994,12.2,0.217868305999982));
#345204=CARTESIAN_POINT('Ctrl Pts',(4.53868324699994,5.2,0.217868305999982));
#345205=CARTESIAN_POINT('Ctrl Pts',(4.53868324699994,2.2,0.217868305999982));
#345206=CARTESIAN_POINT('Ctrl Pts',(4.53658962099994,12.2,0.218876336999987));
#345207=CARTESIAN_POINT('Ctrl Pts',(4.53658962099994,5.2,0.218876336999987));
#345208=CARTESIAN_POINT('Ctrl Pts',(4.53658962099994,2.2,0.218876336999987));
#345209=CARTESIAN_POINT('Ctrl Pts',(4.53449826199994,12.2,0.219880511999988));
#345210=CARTESIAN_POINT('Ctrl Pts',(4.53449826199994,5.2,0.219880511999988));
#345211=CARTESIAN_POINT('Ctrl Pts',(4.53449826199994,2.2,0.219880511999988));
#345212=CARTESIAN_POINT('Ctrl Pts',(4.53240917899994,12.2,0.220880834999986));
#345213=CARTESIAN_POINT('Ctrl Pts',(4.53240917899994,5.2,0.220880834999986));
#345214=CARTESIAN_POINT('Ctrl Pts',(4.53240917899994,2.2,0.220880834999986));
#345215=CARTESIAN_POINT('Ctrl Pts',(4.53032238199994,12.2,0.221877309999985));
#345216=CARTESIAN_POINT('Ctrl Pts',(4.53032238199994,5.2,0.221877309999985));
#345217=CARTESIAN_POINT('Ctrl Pts',(4.53032238199994,2.2,0.221877309999985));
#345218=CARTESIAN_POINT('Ctrl Pts',(4.52823787999994,12.2,0.222869938999986));
#345219=CARTESIAN_POINT('Ctrl Pts',(4.52823787999994,5.2,0.222869938999986));
#345220=CARTESIAN_POINT('Ctrl Pts',(4.52823787999994,2.2,0.222869938999986));
#345221=CARTESIAN_POINT('Ctrl Pts',(4.52615568099994,12.2,0.223858726999988));
#345222=CARTESIAN_POINT('Ctrl Pts',(4.52615568099994,5.2,0.223858726999988));
#345223=CARTESIAN_POINT('Ctrl Pts',(4.52615568099994,2.2,0.223858726999988));
#345224=CARTESIAN_POINT('Ctrl Pts',(4.52407579499994,12.2,0.224843676999988));
#345225=CARTESIAN_POINT('Ctrl Pts',(4.52407579499994,5.2,0.224843676999988));
#345226=CARTESIAN_POINT('Ctrl Pts',(4.52407579499994,2.2,0.224843676999988));
#345227=CARTESIAN_POINT('Ctrl Pts',(4.52199822999994,12.2,0.225824792999987));
#345228=CARTESIAN_POINT('Ctrl Pts',(4.52199822999994,5.2,0.225824792999987));
#345229=CARTESIAN_POINT('Ctrl Pts',(4.52199822999994,2.2,0.225824792999987));
#345230=CARTESIAN_POINT('Ctrl Pts',(4.51992299599994,12.2,0.226802076999988));
#345231=CARTESIAN_POINT('Ctrl Pts',(4.51992299599994,5.2,0.226802076999988));
#345232=CARTESIAN_POINT('Ctrl Pts',(4.51992299599994,2.2,0.226802076999988));
#345233=CARTESIAN_POINT('Ctrl Pts',(4.51785010199994,12.2,0.227775534999988));
#345234=CARTESIAN_POINT('Ctrl Pts',(4.51785010199994,5.2,0.227775534999988));
#345235=CARTESIAN_POINT('Ctrl Pts',(4.51785010199994,2.2,0.227775534999988));
#345236=CARTESIAN_POINT('Ctrl Pts',(4.51577955699995,12.2,0.228745167999986));
#345237=CARTESIAN_POINT('Ctrl Pts',(4.51577955699995,5.2,0.228745167999986));
#345238=CARTESIAN_POINT('Ctrl Pts',(4.51577955699995,2.2,0.228745167999986));
#345239=CARTESIAN_POINT('Ctrl Pts',(4.51371136899994,12.2,0.229710981999984));
#345240=CARTESIAN_POINT('Ctrl Pts',(4.51371136899994,5.2,0.229710981999984));
#345241=CARTESIAN_POINT('Ctrl Pts',(4.51371136899994,2.2,0.229710981999984));
#345242=CARTESIAN_POINT('Ctrl Pts',(4.51164554799994,12.2,0.230672978999986));
#345243=CARTESIAN_POINT('Ctrl Pts',(4.51164554799994,5.2,0.230672978999986));
#345244=CARTESIAN_POINT('Ctrl Pts',(4.51164554799994,2.2,0.230672978999986));
#345245=CARTESIAN_POINT('Ctrl Pts',(4.50958210299994,12.2,0.231631163999988));
#345246=CARTESIAN_POINT('Ctrl Pts',(4.50958210299994,5.2,0.231631163999988));
#345247=CARTESIAN_POINT('Ctrl Pts',(4.50958210299994,2.2,0.231631163999988));
#345248=CARTESIAN_POINT('Ctrl Pts',(4.50752104299994,12.2,0.232585539999985));
#345249=CARTESIAN_POINT('Ctrl Pts',(4.50752104299994,5.2,0.232585539999985));
#345250=CARTESIAN_POINT('Ctrl Pts',(4.50752104299994,2.2,0.232585539999985));
#345251=CARTESIAN_POINT('Ctrl Pts',(4.50546237799994,12.2,0.233536110999988));
#345252=CARTESIAN_POINT('Ctrl Pts',(4.50546237799994,5.2,0.233536110999988));
#345253=CARTESIAN_POINT('Ctrl Pts',(4.50546237799994,2.2,0.233536110999988));
#345254=CARTESIAN_POINT('Ctrl Pts',(4.50340611499994,12.2,0.234482879999987));
#345255=CARTESIAN_POINT('Ctrl Pts',(4.50340611499994,5.2,0.234482879999987));
#345256=CARTESIAN_POINT('Ctrl Pts',(4.50340611499994,2.2,0.234482879999987));
#345257=CARTESIAN_POINT('Ctrl Pts',(4.50135226499994,12.2,0.235425850999986));
#345258=CARTESIAN_POINT('Ctrl Pts',(4.50135226499994,5.2,0.235425850999986));
#345259=CARTESIAN_POINT('Ctrl Pts',(4.50135226499994,2.2,0.235425850999986));
#345260=CARTESIAN_POINT('Ctrl Pts',(4.49930083599994,12.2,0.236365028999987));
#345261=CARTESIAN_POINT('Ctrl Pts',(4.49930083599994,5.2,0.236365028999987));
#345262=CARTESIAN_POINT('Ctrl Pts',(4.49930083599994,2.2,0.236365028999987));
#345263=CARTESIAN_POINT('Ctrl Pts',(4.49725183699995,12.2,0.237300414999986));
#345264=CARTESIAN_POINT('Ctrl Pts',(4.49725183699995,5.2,0.237300414999986));
#345265=CARTESIAN_POINT('Ctrl Pts',(4.49725183699995,2.2,0.237300414999986));
#345266=CARTESIAN_POINT('Ctrl Pts',(4.49520527799994,12.2,0.238232014999986));
#345267=CARTESIAN_POINT('Ctrl Pts',(4.49520527799994,5.2,0.238232014999986));
#345268=CARTESIAN_POINT('Ctrl Pts',(4.49520527799994,2.2,0.238232014999986));
#345269=CARTESIAN_POINT('Ctrl Pts',(4.49316116899994,12.2,0.239159833999985));
#345270=CARTESIAN_POINT('Ctrl Pts',(4.49316116899994,5.2,0.239159833999985));
#345271=CARTESIAN_POINT('Ctrl Pts',(4.49316116899994,2.2,0.239159833999985));
#345272=CARTESIAN_POINT('Ctrl Pts',(4.49111951599994,12.2,0.240083871999985));
#345273=CARTESIAN_POINT('Ctrl Pts',(4.49111951599994,5.2,0.240083871999985));
#345274=CARTESIAN_POINT('Ctrl Pts',(4.49111951599994,2.2,0.240083871999985));
#345275=CARTESIAN_POINT('Ctrl Pts',(4.48908033099995,12.2,0.241004136999985));
#345276=CARTESIAN_POINT('Ctrl Pts',(4.48908033099995,5.2,0.241004136999985));
#345277=CARTESIAN_POINT('Ctrl Pts',(4.48908033099995,2.2,0.241004136999985));
#345278=CARTESIAN_POINT('Ctrl Pts',(4.48704362299994,12.2,0.241920629999988));
#345279=CARTESIAN_POINT('Ctrl Pts',(4.48704362299994,5.2,0.241920629999988));
#345280=CARTESIAN_POINT('Ctrl Pts',(4.48704362299994,2.2,0.241920629999988));
#345281=CARTESIAN_POINT('Ctrl Pts',(4.48500939999994,12.2,0.242833354999985));
#345282=CARTESIAN_POINT('Ctrl Pts',(4.48500939999994,5.2,0.242833354999985));
#345283=CARTESIAN_POINT('Ctrl Pts',(4.48500939999994,2.2,0.242833354999985));
#345284=CARTESIAN_POINT('Ctrl Pts',(4.48297766999994,12.2,0.243742316999986));
#345285=CARTESIAN_POINT('Ctrl Pts',(4.48297766999994,5.2,0.243742316999986));
#345286=CARTESIAN_POINT('Ctrl Pts',(4.48297766999994,2.2,0.243742316999986));
#345287=CARTESIAN_POINT('Ctrl Pts',(4.48094844499995,12.2,0.244647520999983));
#345288=CARTESIAN_POINT('Ctrl Pts',(4.48094844499995,5.2,0.244647520999983));
#345289=CARTESIAN_POINT('Ctrl Pts',(4.48094844499995,2.2,0.244647520999983));
#345290=CARTESIAN_POINT('Ctrl Pts',(4.47892173299994,12.2,0.245548966999984));
#345291=CARTESIAN_POINT('Ctrl Pts',(4.47892173299994,5.2,0.245548966999984));
#345292=CARTESIAN_POINT('Ctrl Pts',(4.47892173299994,2.2,0.245548966999984));
#345293=CARTESIAN_POINT('Ctrl Pts',(4.47689754399994,12.2,0.246446662999986));
#345294=CARTESIAN_POINT('Ctrl Pts',(4.47689754399994,5.2,0.246446662999986));
#345295=CARTESIAN_POINT('Ctrl Pts',(4.47689754399994,2.2,0.246446662999986));
#345296=CARTESIAN_POINT('Ctrl Pts',(4.47487588399994,12.2,0.247340611999984));
#345297=CARTESIAN_POINT('Ctrl Pts',(4.47487588399994,5.2,0.247340611999984));
#345298=CARTESIAN_POINT('Ctrl Pts',(4.47487588399994,2.2,0.247340611999984));
#345299=CARTESIAN_POINT('Ctrl Pts',(4.47285676699994,12.2,0.248230816999988));
#345300=CARTESIAN_POINT('Ctrl Pts',(4.47285676699994,5.2,0.248230816999988));
#345301=CARTESIAN_POINT('Ctrl Pts',(4.47285676699994,2.2,0.248230816999988));
#345302=CARTESIAN_POINT('Ctrl Pts',(4.47084019799994,12.2,0.249117281999984));
#345303=CARTESIAN_POINT('Ctrl Pts',(4.47084019799994,5.2,0.249117281999984));
#345304=CARTESIAN_POINT('Ctrl Pts',(4.47084019799994,2.2,0.249117281999984));
#345305=CARTESIAN_POINT('Ctrl Pts',(4.46882618799994,12.2,0.250000010999987));
#345306=CARTESIAN_POINT('Ctrl Pts',(4.46882618799994,5.2,0.250000010999987));
#345307=CARTESIAN_POINT('Ctrl Pts',(4.46882618799994,2.2,0.250000010999987));
#345308=CARTESIAN_POINT('Ctrl Pts',(4.46681474699994,12.2,0.250879009999987));
#345309=CARTESIAN_POINT('Ctrl Pts',(4.46681474699994,5.2,0.250879009999987));
#345310=CARTESIAN_POINT('Ctrl Pts',(4.46681474699994,2.2,0.250879009999987));
#345311=CARTESIAN_POINT('Ctrl Pts',(4.46480588299994,12.2,0.251754280999985));
#345312=CARTESIAN_POINT('Ctrl Pts',(4.46480588299994,5.2,0.251754280999985));
#345313=CARTESIAN_POINT('Ctrl Pts',(4.46480588299994,2.2,0.251754280999985));
#345314=CARTESIAN_POINT('Ctrl Pts',(4.46279960599994,12.2,0.252625828999986));
#345315=CARTESIAN_POINT('Ctrl Pts',(4.46279960599994,5.2,0.252625828999986));
#345316=CARTESIAN_POINT('Ctrl Pts',(4.46279960599994,2.2,0.252625828999986));
#345317=CARTESIAN_POINT('Ctrl Pts',(4.46079592399994,12.2,0.253493656999986));
#345318=CARTESIAN_POINT('Ctrl Pts',(4.46079592399994,5.2,0.253493656999986));
#345319=CARTESIAN_POINT('Ctrl Pts',(4.46079592399994,2.2,0.253493656999986));
#345320=CARTESIAN_POINT('Ctrl Pts',(4.45879484899994,12.2,0.254357769999984));
#345321=CARTESIAN_POINT('Ctrl Pts',(4.45879484899994,5.2,0.254357769999984));
#345322=CARTESIAN_POINT('Ctrl Pts',(4.45879484899994,2.2,0.254357769999984));
#345323=CARTESIAN_POINT('Ctrl Pts',(4.45679638699994,12.2,0.255218172999987));
#345324=CARTESIAN_POINT('Ctrl Pts',(4.45679638699994,5.2,0.255218172999987));
#345325=CARTESIAN_POINT('Ctrl Pts',(4.45679638699994,2.2,0.255218172999987));
#345326=CARTESIAN_POINT('Ctrl Pts',(4.45480054899994,12.2,0.256074867999985));
#345327=CARTESIAN_POINT('Ctrl Pts',(4.45480054899994,5.2,0.256074867999985));
#345328=CARTESIAN_POINT('Ctrl Pts',(4.45480054899994,2.2,0.256074867999985));
#345329=CARTESIAN_POINT('Ctrl Pts',(4.45280734399994,12.2,0.256927860999987));
#345330=CARTESIAN_POINT('Ctrl Pts',(4.45280734399994,5.2,0.256927860999987));
#345331=CARTESIAN_POINT('Ctrl Pts',(4.45280734399994,2.2,0.256927860999987));
#345332=CARTESIAN_POINT('Ctrl Pts',(4.45081678199994,12.2,0.257777155999985));
#345333=CARTESIAN_POINT('Ctrl Pts',(4.45081678199994,5.2,0.257777155999985));
#345334=CARTESIAN_POINT('Ctrl Pts',(4.45081678199994,2.2,0.257777155999985));
#345335=CARTESIAN_POINT('Ctrl Pts',(4.44882887099994,12.2,0.258622755999984));
#345336=CARTESIAN_POINT('Ctrl Pts',(4.44882887099994,5.2,0.258622755999984));
#345337=CARTESIAN_POINT('Ctrl Pts',(4.44882887099994,2.2,0.258622755999984));
#345338=CARTESIAN_POINT('Ctrl Pts',(4.44684362099994,12.2,0.259464666999989));
#345339=CARTESIAN_POINT('Ctrl Pts',(4.44684362099994,5.2,0.259464666999989));
#345340=CARTESIAN_POINT('Ctrl Pts',(4.44684362099994,2.2,0.259464666999989));
#345341=CARTESIAN_POINT('Ctrl Pts',(4.44486104099994,12.2,0.260302891999986));
#345342=CARTESIAN_POINT('Ctrl Pts',(4.44486104099994,5.2,0.260302891999986));
#345343=CARTESIAN_POINT('Ctrl Pts',(4.44486104099994,2.2,0.260302891999986));
#345344=CARTESIAN_POINT('Ctrl Pts',(4.44288114199994,12.2,0.261137435999985));
#345345=CARTESIAN_POINT('Ctrl Pts',(4.44288114199994,5.2,0.261137435999985));
#345346=CARTESIAN_POINT('Ctrl Pts',(4.44288114199994,2.2,0.261137435999985));
#345347=CARTESIAN_POINT('Ctrl Pts',(4.44090392999995,12.2,0.261968301999986));
#345348=CARTESIAN_POINT('Ctrl Pts',(4.44090392999995,5.2,0.261968301999986));
#345349=CARTESIAN_POINT('Ctrl Pts',(4.44090392999995,2.2,0.261968301999986));
#345350=CARTESIAN_POINT('Ctrl Pts',(4.43892941799994,12.2,0.262795494999986));
#345351=CARTESIAN_POINT('Ctrl Pts',(4.43892941799994,5.2,0.262795494999986));
#345352=CARTESIAN_POINT('Ctrl Pts',(4.43892941799994,2.2,0.262795494999986));
#345353=CARTESIAN_POINT('Ctrl Pts',(4.43695761199994,12.2,0.263619019999983));
#345354=CARTESIAN_POINT('Ctrl Pts',(4.43695761199994,5.2,0.263619019999983));
#345355=CARTESIAN_POINT('Ctrl Pts',(4.43695761199994,2.2,0.263619019999983));
#345356=CARTESIAN_POINT('Ctrl Pts',(4.43498852499994,12.2,0.264438880999984));
#345357=CARTESIAN_POINT('Ctrl Pts',(4.43498852499994,5.2,0.264438880999984));
#345358=CARTESIAN_POINT('Ctrl Pts',(4.43498852499994,2.2,0.264438880999984));
#345359=CARTESIAN_POINT('Ctrl Pts',(4.43302216299994,12.2,0.265255081999989));
#345360=CARTESIAN_POINT('Ctrl Pts',(4.43302216299994,5.2,0.265255081999989));
#345361=CARTESIAN_POINT('Ctrl Pts',(4.43302216299994,2.2,0.265255081999989));
#345362=CARTESIAN_POINT('Ctrl Pts',(4.43105853599994,12.2,0.266067626999984));
#345363=CARTESIAN_POINT('Ctrl Pts',(4.43105853599994,5.2,0.266067626999984));
#345364=CARTESIAN_POINT('Ctrl Pts',(4.43105853599994,2.2,0.266067626999984));
#345365=CARTESIAN_POINT('Ctrl Pts',(4.42909765599994,12.2,0.266876522999984));
#345366=CARTESIAN_POINT('Ctrl Pts',(4.42909765599994,5.2,0.266876522999984));
#345367=CARTESIAN_POINT('Ctrl Pts',(4.42909765599994,2.2,0.266876522999984));
#345368=CARTESIAN_POINT('Ctrl Pts',(4.42713952999994,12.2,0.267681770999988));
#345369=CARTESIAN_POINT('Ctrl Pts',(4.42713952999994,5.2,0.267681770999988));
#345370=CARTESIAN_POINT('Ctrl Pts',(4.42713952999994,2.2,0.267681770999988));
#345371=CARTESIAN_POINT('Ctrl Pts',(4.42518416699994,12.2,0.268483376999988));
#345372=CARTESIAN_POINT('Ctrl Pts',(4.42518416699994,5.2,0.268483376999988));
#345373=CARTESIAN_POINT('Ctrl Pts',(4.42518416699994,2.2,0.268483376999988));
#345374=CARTESIAN_POINT('Ctrl Pts',(4.42323157799995,12.2,0.269281345999985));
#345375=CARTESIAN_POINT('Ctrl Pts',(4.42323157799995,5.2,0.269281345999985));
#345376=CARTESIAN_POINT('Ctrl Pts',(4.42323157799995,2.2,0.269281345999985));
#345377=CARTESIAN_POINT('Ctrl Pts',(4.42128177099994,12.2,0.270075680999984));
#345378=CARTESIAN_POINT('Ctrl Pts',(4.42128177099994,5.2,0.270075680999984));
#345379=CARTESIAN_POINT('Ctrl Pts',(4.42128177099994,2.2,0.270075680999984));
#345380=CARTESIAN_POINT('Ctrl Pts',(4.41933475699994,12.2,0.270866387999984));
#345381=CARTESIAN_POINT('Ctrl Pts',(4.41933475699994,5.2,0.270866387999984));
#345382=CARTESIAN_POINT('Ctrl Pts',(4.41933475699994,2.2,0.270866387999984));
#345383=CARTESIAN_POINT('Ctrl Pts',(4.41739054399994,12.2,0.271653470999986));
#345384=CARTESIAN_POINT('Ctrl Pts',(4.41739054399994,5.2,0.271653470999986));
#345385=CARTESIAN_POINT('Ctrl Pts',(4.41739054399994,2.2,0.271653470999986));
#345386=CARTESIAN_POINT('Ctrl Pts',(4.41544914199994,12.2,0.272436934999987));
#345387=CARTESIAN_POINT('Ctrl Pts',(4.41544914199994,5.2,0.272436934999987));
#345388=CARTESIAN_POINT('Ctrl Pts',(4.41544914199994,2.2,0.272436934999987));
#345389=CARTESIAN_POINT('Ctrl Pts',(4.41351056199994,12.2,0.273216782999985));
#345390=CARTESIAN_POINT('Ctrl Pts',(4.41351056199994,5.2,0.273216782999985));
#345391=CARTESIAN_POINT('Ctrl Pts',(4.41351056199994,2.2,0.273216782999985));
#345392=CARTESIAN_POINT('Ctrl Pts',(4.41157481099994,12.2,0.273993020999987));
#345393=CARTESIAN_POINT('Ctrl Pts',(4.41157481099994,5.2,0.273993020999987));
#345394=CARTESIAN_POINT('Ctrl Pts',(4.41157481099994,2.2,0.273993020999987));
#345395=CARTESIAN_POINT('Ctrl Pts',(4.40964189899994,12.2,0.274765652999989));
#345396=CARTESIAN_POINT('Ctrl Pts',(4.40964189899994,5.2,0.274765652999989));
#345397=CARTESIAN_POINT('Ctrl Pts',(4.40964189899994,2.2,0.274765652999989));
#345398=CARTESIAN_POINT('Ctrl Pts',(4.40771183599994,12.2,0.275534683999985));
#345399=CARTESIAN_POINT('Ctrl Pts',(4.40771183599994,5.2,0.275534683999985));
#345400=CARTESIAN_POINT('Ctrl Pts',(4.40771183599994,2.2,0.275534683999985));
#345401=CARTESIAN_POINT('Ctrl Pts',(4.40578463099994,12.2,0.276300118999986));
#345402=CARTESIAN_POINT('Ctrl Pts',(4.40578463099994,5.2,0.276300118999986));
#345403=CARTESIAN_POINT('Ctrl Pts',(4.40578463099994,2.2,0.276300118999986));
#345404=CARTESIAN_POINT('Ctrl Pts',(4.40386029399995,12.2,0.277061960999987));
#345405=CARTESIAN_POINT('Ctrl Pts',(4.40386029399995,5.2,0.277061960999987));
#345406=CARTESIAN_POINT('Ctrl Pts',(4.40386029399995,2.2,0.277061960999987));
#345407=CARTESIAN_POINT('Ctrl Pts',(4.40193883499994,12.2,0.277820216999984));
#345408=CARTESIAN_POINT('Ctrl Pts',(4.40193883499994,5.2,0.277820216999984));
#345409=CARTESIAN_POINT('Ctrl Pts',(4.40193883499994,2.2,0.277820216999984));
#345410=CARTESIAN_POINT('Ctrl Pts',(4.40002026299994,12.2,0.278574889999987));
#345411=CARTESIAN_POINT('Ctrl Pts',(4.40002026299994,5.2,0.278574889999987));
#345412=CARTESIAN_POINT('Ctrl Pts',(4.40002026299994,2.2,0.278574889999987));
#345413=CARTESIAN_POINT('Ctrl Pts',(4.39810458599994,12.2,0.279325985999983));
#345414=CARTESIAN_POINT('Ctrl Pts',(4.39810458599994,5.2,0.279325985999983));
#345415=CARTESIAN_POINT('Ctrl Pts',(4.39810458599994,2.2,0.279325985999983));
#345416=CARTESIAN_POINT('Ctrl Pts',(4.39619181599994,12.2,0.280073507999985));
#345417=CARTESIAN_POINT('Ctrl Pts',(4.39619181599994,5.2,0.280073507999985));
#345418=CARTESIAN_POINT('Ctrl Pts',(4.39619181599994,2.2,0.280073507999985));
#345419=CARTESIAN_POINT('Ctrl Pts',(4.39428196099994,12.2,0.280817461999985));
#345420=CARTESIAN_POINT('Ctrl Pts',(4.39428196099994,5.2,0.280817461999985));
#345421=CARTESIAN_POINT('Ctrl Pts',(4.39428196099994,2.2,0.280817461999985));
#345422=CARTESIAN_POINT('Ctrl Pts',(4.39237503099995,12.2,0.281557852999987));
#345423=CARTESIAN_POINT('Ctrl Pts',(4.39237503099995,5.2,0.281557852999987));
#345424=CARTESIAN_POINT('Ctrl Pts',(4.39237503099995,2.2,0.281557852999987));
#345425=CARTESIAN_POINT('Ctrl Pts',(4.39047103599994,12.2,0.282294684999984));
#345426=CARTESIAN_POINT('Ctrl Pts',(4.39047103599994,5.2,0.282294684999984));
#345427=CARTESIAN_POINT('Ctrl Pts',(4.39047103599994,2.2,0.282294684999984));
#345428=CARTESIAN_POINT('Ctrl Pts',(4.38856998399995,12.2,0.283027963999984));
#345429=CARTESIAN_POINT('Ctrl Pts',(4.38856998399995,5.2,0.283027963999984));
#345430=CARTESIAN_POINT('Ctrl Pts',(4.38856998399995,2.2,0.283027963999984));
#345431=CARTESIAN_POINT('Ctrl Pts',(4.38667188599995,12.2,0.283757692999984));
#345432=CARTESIAN_POINT('Ctrl Pts',(4.38667188599995,5.2,0.283757692999984));
#345433=CARTESIAN_POINT('Ctrl Pts',(4.38667188599995,2.2,0.283757692999984));
#345434=CARTESIAN_POINT('Ctrl Pts',(4.38477675099994,12.2,0.284483878999984));
#345435=CARTESIAN_POINT('Ctrl Pts',(4.38477675099994,5.2,0.284483878999984));
#345436=CARTESIAN_POINT('Ctrl Pts',(4.38477675099994,2.2,0.284483878999984));
#345437=CARTESIAN_POINT('Ctrl Pts',(4.38288458899994,12.2,0.285206524999988));
#345438=CARTESIAN_POINT('Ctrl Pts',(4.38288458899994,5.2,0.285206524999988));
#345439=CARTESIAN_POINT('Ctrl Pts',(4.38288458899994,2.2,0.285206524999988));
#345440=CARTESIAN_POINT('Ctrl Pts',(4.38099540999994,12.2,0.285925636999984));
#345441=CARTESIAN_POINT('Ctrl Pts',(4.38099540999994,5.2,0.285925636999984));
#345442=CARTESIAN_POINT('Ctrl Pts',(4.38099540999994,2.2,0.285925636999984));
#345443=CARTESIAN_POINT('Ctrl Pts',(4.37910922299994,12.2,0.286641219999986));
#345444=CARTESIAN_POINT('Ctrl Pts',(4.37910922299994,5.2,0.286641219999986));
#345445=CARTESIAN_POINT('Ctrl Pts',(4.37910922299994,2.2,0.286641219999986));
#345446=CARTESIAN_POINT('Ctrl Pts',(4.37722603699994,12.2,0.287353278999984));
#345447=CARTESIAN_POINT('Ctrl Pts',(4.37722603699994,5.2,0.287353278999984));
#345448=CARTESIAN_POINT('Ctrl Pts',(4.37722603699994,2.2,0.287353278999984));
#345449=CARTESIAN_POINT('Ctrl Pts',(4.37534586199994,12.2,0.288061817999985));
#345450=CARTESIAN_POINT('Ctrl Pts',(4.37534586199994,5.2,0.288061817999985));
#345451=CARTESIAN_POINT('Ctrl Pts',(4.37534586199994,2.2,0.288061817999985));
#345452=CARTESIAN_POINT('Ctrl Pts',(4.37346870799994,12.2,0.288766842999983));
#345453=CARTESIAN_POINT('Ctrl Pts',(4.37346870799994,5.2,0.288766842999983));
#345454=CARTESIAN_POINT('Ctrl Pts',(4.37346870799994,2.2,0.288766842999983));
#345455=CARTESIAN_POINT('Ctrl Pts',(4.37159458399995,12.2,0.289468358999985));
#345456=CARTESIAN_POINT('Ctrl Pts',(4.37159458399995,5.2,0.289468358999985));
#345457=CARTESIAN_POINT('Ctrl Pts',(4.37159458399995,2.2,0.289468358999985));
#345458=CARTESIAN_POINT('Ctrl Pts',(4.36972350099994,12.2,0.290166369999985));
#345459=CARTESIAN_POINT('Ctrl Pts',(4.36972350099994,5.2,0.290166369999985));
#345460=CARTESIAN_POINT('Ctrl Pts',(4.36972350099994,2.2,0.290166369999985));
#345461=CARTESIAN_POINT('Ctrl Pts',(4.36785546599994,12.2,0.290860881999984));
#345462=CARTESIAN_POINT('Ctrl Pts',(4.36785546599994,5.2,0.290860881999984));
#345463=CARTESIAN_POINT('Ctrl Pts',(4.36785546599994,2.2,0.290860881999984));
#345464=CARTESIAN_POINT('Ctrl Pts',(4.36599049299994,12.2,0.291551899999987));
#345465=CARTESIAN_POINT('Ctrl Pts',(4.36599049299994,5.2,0.291551899999987));
#345466=CARTESIAN_POINT('Ctrl Pts',(4.36599049299994,2.2,0.291551899999987));
#345467=CARTESIAN_POINT('Ctrl Pts',(4.36412858699994,12.2,0.292239427999985));
#345468=CARTESIAN_POINT('Ctrl Pts',(4.36412858699994,5.2,0.292239427999985));
#345469=CARTESIAN_POINT('Ctrl Pts',(4.36412858699994,2.2,0.292239427999985));
#345470=CARTESIAN_POINT('Ctrl Pts',(4.36226975999995,12.2,0.292923472999984));
#345471=CARTESIAN_POINT('Ctrl Pts',(4.36226975999995,5.2,0.292923472999984));
#345472=CARTESIAN_POINT('Ctrl Pts',(4.36226975999995,2.2,0.292923472999984));
#345473=CARTESIAN_POINT('Ctrl Pts',(4.36041402199994,12.2,0.293604038999984));
#345474=CARTESIAN_POINT('Ctrl Pts',(4.36041402199994,5.2,0.293604038999984));
#345475=CARTESIAN_POINT('Ctrl Pts',(4.36041402199994,2.2,0.293604038999984));
#345476=CARTESIAN_POINT('Ctrl Pts',(4.35856138199994,12.2,0.294281131999985));
#345477=CARTESIAN_POINT('Ctrl Pts',(4.35856138199994,5.2,0.294281131999985));
#345478=CARTESIAN_POINT('Ctrl Pts',(4.35856138199994,2.2,0.294281131999985));
#345479=CARTESIAN_POINT('Ctrl Pts',(4.35671184899994,12.2,0.294954754999988));
#345480=CARTESIAN_POINT('Ctrl Pts',(4.35671184899994,5.2,0.294954754999988));
#345481=CARTESIAN_POINT('Ctrl Pts',(4.35671184899994,2.2,0.294954754999988));
#345482=CARTESIAN_POINT('Ctrl Pts',(4.35486543399994,12.2,0.295624915999984));
#345483=CARTESIAN_POINT('Ctrl Pts',(4.35486543399994,5.2,0.295624915999984));
#345484=CARTESIAN_POINT('Ctrl Pts',(4.35486543399994,2.2,0.295624915999984));
#345485=CARTESIAN_POINT('Ctrl Pts',(4.35302214599994,12.2,0.296291618999986));
#345486=CARTESIAN_POINT('Ctrl Pts',(4.35302214599994,5.2,0.296291618999986));
#345487=CARTESIAN_POINT('Ctrl Pts',(4.35302214599994,2.2,0.296291618999986));
#345488=CARTESIAN_POINT('Ctrl Pts',(4.35118199599995,12.2,0.296954867999983));
#345489=CARTESIAN_POINT('Ctrl Pts',(4.35118199599995,5.2,0.296954867999983));
#345490=CARTESIAN_POINT('Ctrl Pts',(4.35118199599995,2.2,0.296954867999983));
#345491=CARTESIAN_POINT('Ctrl Pts',(4.34934499099994,12.2,0.297614670999984));
#345492=CARTESIAN_POINT('Ctrl Pts',(4.34934499099994,5.2,0.297614670999984));
#345493=CARTESIAN_POINT('Ctrl Pts',(4.34934499099994,2.2,0.297614670999984));
#345494=CARTESIAN_POINT('Ctrl Pts',(4.34751114399995,12.2,0.298271030999988));
#345495=CARTESIAN_POINT('Ctrl Pts',(4.34751114399995,5.2,0.298271030999988));
#345496=CARTESIAN_POINT('Ctrl Pts',(4.34751114399995,2.2,0.298271030999988));
#345497=CARTESIAN_POINT('Ctrl Pts',(4.34568046199994,12.2,0.298923954999988));
#345498=CARTESIAN_POINT('Ctrl Pts',(4.34568046199994,5.2,0.298923954999988));
#345499=CARTESIAN_POINT('Ctrl Pts',(4.34568046199994,2.2,0.298923954999988));
#345500=CARTESIAN_POINT('Ctrl Pts',(4.34385295599994,12.2,0.299573446999983));
#345501=CARTESIAN_POINT('Ctrl Pts',(4.34385295599994,5.2,0.299573446999983));
#345502=CARTESIAN_POINT('Ctrl Pts',(4.34385295599994,2.2,0.299573446999983));
#345503=CARTESIAN_POINT('Ctrl Pts',(4.34202863699995,12.2,0.300219512999984));
#345504=CARTESIAN_POINT('Ctrl Pts',(4.34202863699995,5.2,0.300219512999984));
#345505=CARTESIAN_POINT('Ctrl Pts',(4.34202863699995,2.2,0.300219512999984));
#345506=CARTESIAN_POINT('Ctrl Pts',(4.34020751199994,12.2,0.300862157999986));
#345507=CARTESIAN_POINT('Ctrl Pts',(4.34020751199994,5.2,0.300862157999986));
#345508=CARTESIAN_POINT('Ctrl Pts',(4.34020751199994,2.2,0.300862157999986));
#345509=CARTESIAN_POINT('Ctrl Pts',(4.33838959199994,12.2,0.301501387999985));
#345510=CARTESIAN_POINT('Ctrl Pts',(4.33838959199994,5.2,0.301501387999985));
#345511=CARTESIAN_POINT('Ctrl Pts',(4.33838959199994,2.2,0.301501387999985));
#345512=CARTESIAN_POINT('Ctrl Pts',(4.33657488799994,12.2,0.302137207999986));
#345513=CARTESIAN_POINT('Ctrl Pts',(4.33657488799994,5.2,0.302137207999986));
#345514=CARTESIAN_POINT('Ctrl Pts',(4.33657488799994,2.2,0.302137207999986));
#345515=CARTESIAN_POINT('Ctrl Pts',(4.33476340899994,12.2,0.302769622999985));
#345516=CARTESIAN_POINT('Ctrl Pts',(4.33476340899994,5.2,0.302769622999985));
#345517=CARTESIAN_POINT('Ctrl Pts',(4.33476340899994,2.2,0.302769622999985));
#345518=CARTESIAN_POINT('Ctrl Pts',(4.33295516399994,12.2,0.303398639999983));
#345519=CARTESIAN_POINT('Ctrl Pts',(4.33295516399994,5.2,0.303398639999983));
#345520=CARTESIAN_POINT('Ctrl Pts',(4.33295516399994,2.2,0.303398639999983));
#345521=CARTESIAN_POINT('Ctrl Pts',(4.33115016299995,12.2,0.304024262999985));
#345522=CARTESIAN_POINT('Ctrl Pts',(4.33115016299995,5.2,0.304024262999985));
#345523=CARTESIAN_POINT('Ctrl Pts',(4.33115016299995,2.2,0.304024262999985));
#345524=CARTESIAN_POINT('Ctrl Pts',(4.32934841799994,12.2,0.304646498999985));
#345525=CARTESIAN_POINT('Ctrl Pts',(4.32934841799994,5.2,0.304646498999985));
#345526=CARTESIAN_POINT('Ctrl Pts',(4.32934841799994,2.2,0.304646498999985));
#345527=CARTESIAN_POINT('Ctrl Pts',(4.32754993599994,12.2,0.305265350999986));
#345528=CARTESIAN_POINT('Ctrl Pts',(4.32754993599994,5.2,0.305265350999986));
#345529=CARTESIAN_POINT('Ctrl Pts',(4.32754993599994,2.2,0.305265350999986));
#345530=CARTESIAN_POINT('Ctrl Pts',(4.32575472799994,12.2,0.305880825999987));
#345531=CARTESIAN_POINT('Ctrl Pts',(4.32575472799994,5.2,0.305880825999987));
#345532=CARTESIAN_POINT('Ctrl Pts',(4.32575472799994,2.2,0.305880825999987));
#345533=CARTESIAN_POINT('Ctrl Pts',(4.32396280299994,12.2,0.306492931999984));
#345534=CARTESIAN_POINT('Ctrl Pts',(4.32396280299994,5.2,0.306492931999984));
#345535=CARTESIAN_POINT('Ctrl Pts',(4.32396280299994,2.2,0.306492931999984));
#345536=CARTESIAN_POINT('Ctrl Pts',(4.32217417299994,12.2,0.307101670999987));
#345537=CARTESIAN_POINT('Ctrl Pts',(4.32217417299994,5.2,0.307101670999987));
#345538=CARTESIAN_POINT('Ctrl Pts',(4.32217417299994,2.2,0.307101670999987));
#345539=CARTESIAN_POINT('Ctrl Pts',(4.32038884599994,12.2,0.307707049999983));
#345540=CARTESIAN_POINT('Ctrl Pts',(4.32038884599994,5.2,0.307707049999983));
#345541=CARTESIAN_POINT('Ctrl Pts',(4.32038884599994,2.2,0.307707049999983));
#345542=CARTESIAN_POINT('Ctrl Pts',(4.31860683299994,12.2,0.308309073999986));
#345543=CARTESIAN_POINT('Ctrl Pts',(4.31860683299994,5.2,0.308309073999986));
#345544=CARTESIAN_POINT('Ctrl Pts',(4.31860683299994,2.2,0.308309073999986));
#345545=CARTESIAN_POINT('Ctrl Pts',(4.31682814299994,12.2,0.308907748999987));
#345546=CARTESIAN_POINT('Ctrl Pts',(4.31682814299994,5.2,0.308907748999987));
#345547=CARTESIAN_POINT('Ctrl Pts',(4.31682814299994,2.2,0.308907748999987));
#345548=CARTESIAN_POINT('Ctrl Pts',(4.31505278699994,12.2,0.309503082999987));
#345549=CARTESIAN_POINT('Ctrl Pts',(4.31505278699994,5.2,0.309503082999987));
#345550=CARTESIAN_POINT('Ctrl Pts',(4.31505278699994,2.2,0.309503082999987));
#345551=CARTESIAN_POINT('Ctrl Pts',(4.31328077299994,12.2,0.310095078999986));
#345552=CARTESIAN_POINT('Ctrl Pts',(4.31328077299994,5.2,0.310095078999986));
#345553=CARTESIAN_POINT('Ctrl Pts',(4.31328077299994,2.2,0.310095078999986));
#345554=CARTESIAN_POINT('Ctrl Pts',(4.31151211199994,12.2,0.310683742999984));
#345555=CARTESIAN_POINT('Ctrl Pts',(4.31151211199994,5.2,0.310683742999984));
#345556=CARTESIAN_POINT('Ctrl Pts',(4.31151211199994,2.2,0.310683742999984));
#345557=CARTESIAN_POINT('Ctrl Pts',(4.30974681499994,12.2,0.311269080999987));
#345558=CARTESIAN_POINT('Ctrl Pts',(4.30974681499994,5.2,0.311269080999987));
#345559=CARTESIAN_POINT('Ctrl Pts',(4.30974681499994,2.2,0.311269080999987));
#345560=CARTESIAN_POINT('Ctrl Pts',(4.30798488999994,12.2,0.311851100999987));
#345561=CARTESIAN_POINT('Ctrl Pts',(4.30798488999994,5.2,0.311851100999987));
#345562=CARTESIAN_POINT('Ctrl Pts',(4.30798488999994,2.2,0.311851100999987));
#345563=CARTESIAN_POINT('Ctrl Pts',(4.30622634899995,12.2,0.312429804999983));
#345564=CARTESIAN_POINT('Ctrl Pts',(4.30622634899995,5.2,0.312429804999983));
#345565=CARTESIAN_POINT('Ctrl Pts',(4.30622634899995,2.2,0.312429804999983));
#345566=CARTESIAN_POINT('Ctrl Pts',(4.30447119999994,12.2,0.313005201999985));
#345567=CARTESIAN_POINT('Ctrl Pts',(4.30447119999994,5.2,0.313005201999985));
#345568=CARTESIAN_POINT('Ctrl Pts',(4.30447119999994,2.2,0.313005201999985));
#345569=CARTESIAN_POINT('Ctrl Pts',(4.30271945399994,12.2,0.313577295999985));
#345570=CARTESIAN_POINT('Ctrl Pts',(4.30271945399994,5.2,0.313577295999985));
#345571=CARTESIAN_POINT('Ctrl Pts',(4.30271945399994,2.2,0.313577295999985));
#345572=CARTESIAN_POINT('Ctrl Pts',(4.30097112099994,12.2,0.314146092999987));
#345573=CARTESIAN_POINT('Ctrl Pts',(4.30097112099994,5.2,0.314146092999987));
#345574=CARTESIAN_POINT('Ctrl Pts',(4.30097112099994,2.2,0.314146092999987));
#345575=CARTESIAN_POINT('Ctrl Pts',(4.29922621099994,12.2,0.314711599999988));
#345576=CARTESIAN_POINT('Ctrl Pts',(4.29922621099994,5.2,0.314711599999988));
#345577=CARTESIAN_POINT('Ctrl Pts',(4.29922621099994,2.2,0.314711599999988));
#345578=CARTESIAN_POINT('Ctrl Pts',(4.29748473299994,12.2,0.315273821999984));
#345579=CARTESIAN_POINT('Ctrl Pts',(4.29748473299994,5.2,0.315273821999984));
#345580=CARTESIAN_POINT('Ctrl Pts',(4.29748473299994,2.2,0.315273821999984));
#345581=CARTESIAN_POINT('Ctrl Pts',(4.29574669799995,12.2,0.315832764999988));
#345582=CARTESIAN_POINT('Ctrl Pts',(4.29574669799995,5.2,0.315832764999988));
#345583=CARTESIAN_POINT('Ctrl Pts',(4.29574669799995,2.2,0.315832764999988));
#345584=CARTESIAN_POINT('Ctrl Pts',(4.29401211599994,12.2,0.316388435999984));
#345585=CARTESIAN_POINT('Ctrl Pts',(4.29401211599994,5.2,0.316388435999984));
#345586=CARTESIAN_POINT('Ctrl Pts',(4.29401211599994,2.2,0.316388435999984));
#345587=CARTESIAN_POINT('Ctrl Pts',(4.29228099699994,12.2,0.316940840999984));
#345588=CARTESIAN_POINT('Ctrl Pts',(4.29228099699994,5.2,0.316940840999984));
#345589=CARTESIAN_POINT('Ctrl Pts',(4.29228099699994,2.2,0.316940840999984));
#345590=CARTESIAN_POINT('Ctrl Pts',(4.29055334999994,12.2,0.317489983999986));
#345591=CARTESIAN_POINT('Ctrl Pts',(4.29055334999994,5.2,0.317489983999986));
#345592=CARTESIAN_POINT('Ctrl Pts',(4.29055334999994,2.2,0.317489983999986));
#345593=CARTESIAN_POINT('Ctrl Pts',(4.28882918699994,12.2,0.318035873999989));
#345594=CARTESIAN_POINT('Ctrl Pts',(4.28882918699994,5.2,0.318035873999989));
#345595=CARTESIAN_POINT('Ctrl Pts',(4.28882918699994,2.2,0.318035873999989));
#345596=CARTESIAN_POINT('Ctrl Pts',(4.28710851599994,12.2,0.318578514999985));
#345597=CARTESIAN_POINT('Ctrl Pts',(4.28710851599994,5.2,0.318578514999985));
#345598=CARTESIAN_POINT('Ctrl Pts',(4.28710851599994,2.2,0.318578514999985));
#345599=CARTESIAN_POINT('Ctrl Pts',(4.28539134799994,12.2,0.319117911999989));
#345600=CARTESIAN_POINT('Ctrl Pts',(4.28539134799994,5.2,0.319117911999989));
#345601=CARTESIAN_POINT('Ctrl Pts',(4.28539134799994,2.2,0.319117911999989));
#345602=CARTESIAN_POINT('Ctrl Pts',(4.28367769399994,12.2,0.319654074999987));
#345603=CARTESIAN_POINT('Ctrl Pts',(4.28367769399994,5.2,0.319654074999987));
#345604=CARTESIAN_POINT('Ctrl Pts',(4.28367769399994,2.2,0.319654074999987));
#345605=CARTESIAN_POINT('Ctrl Pts',(4.28196756099995,12.2,0.320187006999983));
#345606=CARTESIAN_POINT('Ctrl Pts',(4.28196756099995,5.2,0.320187006999983));
#345607=CARTESIAN_POINT('Ctrl Pts',(4.28196756099995,2.2,0.320187006999983));
#345608=CARTESIAN_POINT('Ctrl Pts',(4.28026096299994,12.2,0.320716713999989));
#345609=CARTESIAN_POINT('Ctrl Pts',(4.28026096299994,5.2,0.320716713999989));
#345610=CARTESIAN_POINT('Ctrl Pts',(4.28026096299994,2.2,0.320716713999989));
#345611=CARTESIAN_POINT('Ctrl Pts',(4.27855790799994,12.2,0.321243204999986));
#345612=CARTESIAN_POINT('Ctrl Pts',(4.27855790799994,5.2,0.321243204999986));
#345613=CARTESIAN_POINT('Ctrl Pts',(4.27855790799994,2.2,0.321243204999986));
#345614=CARTESIAN_POINT('Ctrl Pts',(4.27685840599994,12.2,0.321766483999983));
#345615=CARTESIAN_POINT('Ctrl Pts',(4.27685840599994,5.2,0.321766483999983));
#345616=CARTESIAN_POINT('Ctrl Pts',(4.27685840599994,2.2,0.321766483999983));
#345617=CARTESIAN_POINT('Ctrl Pts',(4.27516246799994,12.2,0.322286556999987));
#345618=CARTESIAN_POINT('Ctrl Pts',(4.27516246799994,5.2,0.322286556999987));
#345619=CARTESIAN_POINT('Ctrl Pts',(4.27516246799994,2.2,0.322286556999987));
#345620=CARTESIAN_POINT('Ctrl Pts',(4.27347010299994,12.2,0.322803431999983));
#345621=CARTESIAN_POINT('Ctrl Pts',(4.27347010299994,5.2,0.322803431999983));
#345622=CARTESIAN_POINT('Ctrl Pts',(4.27347010299994,2.2,0.322803431999983));
#345623=CARTESIAN_POINT('Ctrl Pts',(4.27178132099994,12.2,0.323317113999986));
#345624=CARTESIAN_POINT('Ctrl Pts',(4.27178132099994,5.2,0.323317113999986));
#345625=CARTESIAN_POINT('Ctrl Pts',(4.27178132099994,2.2,0.323317113999986));
#345626=CARTESIAN_POINT('Ctrl Pts',(4.27009613399994,12.2,0.323827609999987));
#345627=CARTESIAN_POINT('Ctrl Pts',(4.27009613399994,5.2,0.323827609999987));
#345628=CARTESIAN_POINT('Ctrl Pts',(4.27009613399994,2.2,0.323827609999987));
#345629=CARTESIAN_POINT('Ctrl Pts',(4.26841455099995,12.2,0.324334924999987));
#345630=CARTESIAN_POINT('Ctrl Pts',(4.26841455099995,5.2,0.324334924999987));
#345631=CARTESIAN_POINT('Ctrl Pts',(4.26841455099995,2.2,0.324334924999987));
#345632=CARTESIAN_POINT('Ctrl Pts',(4.26673658299995,12.2,0.324839067999987));
#345633=CARTESIAN_POINT('Ctrl Pts',(4.26673658299995,5.2,0.324839067999987));
#345634=CARTESIAN_POINT('Ctrl Pts',(4.26673658299995,2.2,0.324839067999987));
#345635=CARTESIAN_POINT('Ctrl Pts',(4.26506223899994,12.2,0.325340042999986));
#345636=CARTESIAN_POINT('Ctrl Pts',(4.26506223899994,5.2,0.325340042999986));
#345637=CARTESIAN_POINT('Ctrl Pts',(4.26506223899994,2.2,0.325340042999986));
#345638=CARTESIAN_POINT('Ctrl Pts',(4.26339152799994,12.2,0.325837856999982));
#345639=CARTESIAN_POINT('Ctrl Pts',(4.26339152799994,5.2,0.325837856999982));
#345640=CARTESIAN_POINT('Ctrl Pts',(4.26339152799994,2.2,0.325837856999982));
#345641=CARTESIAN_POINT('Ctrl Pts',(4.26172446299994,12.2,0.326332516999983));
#345642=CARTESIAN_POINT('Ctrl Pts',(4.26172446299994,5.2,0.326332516999983));
#345643=CARTESIAN_POINT('Ctrl Pts',(4.26172446299994,2.2,0.326332516999983));
#345644=CARTESIAN_POINT('Ctrl Pts',(4.26006105299995,12.2,0.326824029999986));
#345645=CARTESIAN_POINT('Ctrl Pts',(4.26006105299995,5.2,0.326824029999986));
#345646=CARTESIAN_POINT('Ctrl Pts',(4.26006105299995,2.2,0.326824029999986));
#345647=CARTESIAN_POINT('Ctrl Pts',(4.25840130699994,12.2,0.327312400999986));
#345648=CARTESIAN_POINT('Ctrl Pts',(4.25840130699994,5.2,0.327312400999986));
#345649=CARTESIAN_POINT('Ctrl Pts',(4.25840130699994,2.2,0.327312400999986));
#345650=CARTESIAN_POINT('Ctrl Pts',(4.25674523699994,12.2,0.327797636999985));
#345651=CARTESIAN_POINT('Ctrl Pts',(4.25674523699994,5.2,0.327797636999985));
#345652=CARTESIAN_POINT('Ctrl Pts',(4.25674523699994,2.2,0.327797636999985));
#345653=CARTESIAN_POINT('Ctrl Pts',(4.25509285299994,12.2,0.328279744999986));
#345654=CARTESIAN_POINT('Ctrl Pts',(4.25509285299994,5.2,0.328279744999986));
#345655=CARTESIAN_POINT('Ctrl Pts',(4.25509285299994,2.2,0.328279744999986));
#345656=CARTESIAN_POINT('Ctrl Pts',(4.25344416499995,12.2,0.328758731999983));
#345657=CARTESIAN_POINT('Ctrl Pts',(4.25344416499995,5.2,0.328758731999983));
#345658=CARTESIAN_POINT('Ctrl Pts',(4.25344416499995,2.2,0.328758731999983));
#345659=CARTESIAN_POINT('Ctrl Pts',(4.25179918199994,12.2,0.329234602999984));
#345660=CARTESIAN_POINT('Ctrl Pts',(4.25179918199994,5.2,0.329234602999984));
#345661=CARTESIAN_POINT('Ctrl Pts',(4.25179918199994,2.2,0.329234602999984));
#345662=CARTESIAN_POINT('Ctrl Pts',(4.25015791599994,12.2,0.329707365999985));
#345663=CARTESIAN_POINT('Ctrl Pts',(4.25015791599994,5.2,0.329707365999985));
#345664=CARTESIAN_POINT('Ctrl Pts',(4.25015791599994,2.2,0.329707365999985));
#345665=CARTESIAN_POINT('Ctrl Pts',(4.24852037599995,12.2,0.330177027999987));
#345666=CARTESIAN_POINT('Ctrl Pts',(4.24852037599995,5.2,0.330177027999987));
#345667=CARTESIAN_POINT('Ctrl Pts',(4.24852037599995,2.2,0.330177027999987));
#345668=CARTESIAN_POINT('Ctrl Pts',(4.24688657399994,12.2,0.330643593999986));
#345669=CARTESIAN_POINT('Ctrl Pts',(4.24688657399994,5.2,0.330643593999986));
#345670=CARTESIAN_POINT('Ctrl Pts',(4.24688657399994,2.2,0.330643593999986));
#345671=CARTESIAN_POINT('Ctrl Pts',(4.24525651799994,12.2,0.331107071999988));
#345672=CARTESIAN_POINT('Ctrl Pts',(4.24525651799994,5.2,0.331107071999988));
#345673=CARTESIAN_POINT('Ctrl Pts',(4.24525651799994,2.2,0.331107071999988));
#345674=CARTESIAN_POINT('Ctrl Pts',(4.24363022099994,12.2,0.331567468999987));
#345675=CARTESIAN_POINT('Ctrl Pts',(4.24363022099994,5.2,0.331567468999987));
#345676=CARTESIAN_POINT('Ctrl Pts',(4.24363022099994,2.2,0.331567468999987));
#345677=CARTESIAN_POINT('Ctrl Pts',(4.24200768999994,12.2,0.332024789999985));
#345678=CARTESIAN_POINT('Ctrl Pts',(4.24200768999994,5.2,0.332024789999985));
#345679=CARTESIAN_POINT('Ctrl Pts',(4.24200768999994,2.2,0.332024789999985));
#345680=CARTESIAN_POINT('Ctrl Pts',(4.24038893699994,12.2,0.332479043999987));
#345681=CARTESIAN_POINT('Ctrl Pts',(4.24038893699994,5.2,0.332479043999987));
#345682=CARTESIAN_POINT('Ctrl Pts',(4.24038893699994,2.2,0.332479043999987));
#345683=CARTESIAN_POINT('Ctrl Pts',(4.23877397399994,12.2,0.332930236999989));
#345684=CARTESIAN_POINT('Ctrl Pts',(4.23877397399994,5.2,0.332930236999989));
#345685=CARTESIAN_POINT('Ctrl Pts',(4.23877397399994,2.2,0.332930236999989));
#345686=CARTESIAN_POINT('Ctrl Pts',(4.23716280899994,12.2,0.333378374999986));
#345687=CARTESIAN_POINT('Ctrl Pts',(4.23716280899994,5.2,0.333378374999986));
#345688=CARTESIAN_POINT('Ctrl Pts',(4.23716280899994,2.2,0.333378374999986));
#345689=CARTESIAN_POINT('Ctrl Pts',(4.23555545199994,12.2,0.333823465999985));
#345690=CARTESIAN_POINT('Ctrl Pts',(4.23555545199994,5.2,0.333823465999985));
#345691=CARTESIAN_POINT('Ctrl Pts',(4.23555545199994,2.2,0.333823465999985));
#345692=CARTESIAN_POINT('Ctrl Pts',(4.23395191599994,12.2,0.334265516999985));
#345693=CARTESIAN_POINT('Ctrl Pts',(4.23395191599994,5.2,0.334265516999985));
#345694=CARTESIAN_POINT('Ctrl Pts',(4.23395191599994,2.2,0.334265516999985));
#345695=CARTESIAN_POINT('Ctrl Pts',(4.23235220799994,12.2,0.334704532999983));
#345696=CARTESIAN_POINT('Ctrl Pts',(4.23235220799994,5.2,0.334704532999983));
#345697=CARTESIAN_POINT('Ctrl Pts',(4.23235220799994,2.2,0.334704532999983));
#345698=CARTESIAN_POINT('Ctrl Pts',(4.23075634099995,12.2,0.335140522999984));
#345699=CARTESIAN_POINT('Ctrl Pts',(4.23075634099995,5.2,0.335140522999984));
#345700=CARTESIAN_POINT('Ctrl Pts',(4.23075634099995,2.2,0.335140522999984));
#345701=CARTESIAN_POINT('Ctrl Pts',(4.22916432499994,12.2,0.335573492999988));
#345702=CARTESIAN_POINT('Ctrl Pts',(4.22916432499994,5.2,0.335573492999988));
#345703=CARTESIAN_POINT('Ctrl Pts',(4.22916432499994,2.2,0.335573492999988));
#345704=CARTESIAN_POINT('Ctrl Pts',(4.22757616999994,12.2,0.336003450999982));
#345705=CARTESIAN_POINT('Ctrl Pts',(4.22757616999994,5.2,0.336003450999982));
#345706=CARTESIAN_POINT('Ctrl Pts',(4.22757616999994,2.2,0.336003450999982));
#345707=CARTESIAN_POINT('Ctrl Pts',(4.22599188699994,12.2,0.336430402999985));
#345708=CARTESIAN_POINT('Ctrl Pts',(4.22599188699994,5.2,0.336430402999985));
#345709=CARTESIAN_POINT('Ctrl Pts',(4.22599188699994,2.2,0.336430402999985));
#345710=CARTESIAN_POINT('Ctrl Pts',(4.22441148399994,12.2,0.336854356999985));
#345711=CARTESIAN_POINT('Ctrl Pts',(4.22441148399994,5.2,0.336854356999985));
#345712=CARTESIAN_POINT('Ctrl Pts',(4.22441148399994,2.2,0.336854356999985));
#345713=CARTESIAN_POINT('Ctrl Pts',(4.22283497399994,12.2,0.337275318999986));
#345714=CARTESIAN_POINT('Ctrl Pts',(4.22283497399994,5.2,0.337275318999986));
#345715=CARTESIAN_POINT('Ctrl Pts',(4.22283497399994,2.2,0.337275318999986));
#345716=CARTESIAN_POINT('Ctrl Pts',(4.22126236599994,12.2,0.337693296999984));
#345717=CARTESIAN_POINT('Ctrl Pts',(4.22126236599994,5.2,0.337693296999984));
#345718=CARTESIAN_POINT('Ctrl Pts',(4.22126236599994,2.2,0.337693296999984));
#345719=CARTESIAN_POINT('Ctrl Pts',(4.21969367199994,12.2,0.338108296999984));
#345720=CARTESIAN_POINT('Ctrl Pts',(4.21969367199994,5.2,0.338108296999984));
#345721=CARTESIAN_POINT('Ctrl Pts',(4.21969367199994,2.2,0.338108296999984));
#345722=CARTESIAN_POINT('Ctrl Pts',(4.21812890099994,12.2,0.338520327999987));
#345723=CARTESIAN_POINT('Ctrl Pts',(4.21812890099994,5.2,0.338520327999987));
#345724=CARTESIAN_POINT('Ctrl Pts',(4.21812890099994,2.2,0.338520327999987));
#345725=CARTESIAN_POINT('Ctrl Pts',(4.21656806399994,12.2,0.338929394999985));
#345726=CARTESIAN_POINT('Ctrl Pts',(4.21656806399994,5.2,0.338929394999985));
#345727=CARTESIAN_POINT('Ctrl Pts',(4.21656806399994,2.2,0.338929394999985));
#345728=CARTESIAN_POINT('Ctrl Pts',(4.21501117099994,12.2,0.339335506999987));
#345729=CARTESIAN_POINT('Ctrl Pts',(4.21501117099994,5.2,0.339335506999987));
#345730=CARTESIAN_POINT('Ctrl Pts',(4.21501117099994,2.2,0.339335506999987));
#345731=CARTESIAN_POINT('Ctrl Pts',(4.21345823399994,12.2,0.339738669999985));
#345732=CARTESIAN_POINT('Ctrl Pts',(4.21345823399994,5.2,0.339738669999985));
#345733=CARTESIAN_POINT('Ctrl Pts',(4.21345823399994,2.2,0.339738669999985));
#345734=CARTESIAN_POINT('Ctrl Pts',(4.21190926199994,12.2,0.340138891999988));
#345735=CARTESIAN_POINT('Ctrl Pts',(4.21190926199994,5.2,0.340138891999988));
#345736=CARTESIAN_POINT('Ctrl Pts',(4.21190926199994,2.2,0.340138891999988));
#345737=CARTESIAN_POINT('Ctrl Pts',(4.21036426599994,12.2,0.340536181999984));
#345738=CARTESIAN_POINT('Ctrl Pts',(4.21036426599994,5.2,0.340536181999984));
#345739=CARTESIAN_POINT('Ctrl Pts',(4.21036426599994,2.2,0.340536181999984));
#345740=CARTESIAN_POINT('Ctrl Pts',(4.20882325699994,12.2,0.340930543999987));
#345741=CARTESIAN_POINT('Ctrl Pts',(4.20882325699994,5.2,0.340930543999987));
#345742=CARTESIAN_POINT('Ctrl Pts',(4.20882325699994,2.2,0.340930543999987));
#345743=CARTESIAN_POINT('Ctrl Pts',(4.20728624399994,12.2,0.341321986999983));
#345744=CARTESIAN_POINT('Ctrl Pts',(4.20728624399994,5.2,0.341321986999983));
#345745=CARTESIAN_POINT('Ctrl Pts',(4.20728624399994,2.2,0.341321986999983));
#345746=CARTESIAN_POINT('Ctrl Pts',(4.20575323899994,12.2,0.341710518999987));
#345747=CARTESIAN_POINT('Ctrl Pts',(4.20575323899994,5.2,0.341710518999987));
#345748=CARTESIAN_POINT('Ctrl Pts',(4.20575323899994,2.2,0.341710518999987));
#345749=CARTESIAN_POINT('Ctrl Pts',(4.20422425099995,12.2,0.342096144999986));
#345750=CARTESIAN_POINT('Ctrl Pts',(4.20422425099995,5.2,0.342096144999986));
#345751=CARTESIAN_POINT('Ctrl Pts',(4.20422425099995,2.2,0.342096144999986));
#345752=CARTESIAN_POINT('Ctrl Pts',(4.20269929299994,12.2,0.342478876999985));
#345753=CARTESIAN_POINT('Ctrl Pts',(4.20269929299994,5.2,0.342478876999985));
#345754=CARTESIAN_POINT('Ctrl Pts',(4.20269929299994,2.2,0.342478876999985));
#345755=CARTESIAN_POINT('Ctrl Pts',(4.20117837399994,12.2,0.342858717999985));
#345756=CARTESIAN_POINT('Ctrl Pts',(4.20117837399994,5.2,0.342858717999985));
#345757=CARTESIAN_POINT('Ctrl Pts',(4.20117837399994,2.2,0.342858717999985));
#345758=CARTESIAN_POINT('Ctrl Pts',(4.19966150399994,12.2,0.343235676999987));
#345759=CARTESIAN_POINT('Ctrl Pts',(4.19966150399994,5.2,0.343235676999987));
#345760=CARTESIAN_POINT('Ctrl Pts',(4.19966150399994,2.2,0.343235676999987));
#345761=CARTESIAN_POINT('Ctrl Pts',(4.19814869599994,12.2,0.343609762999986));
#345762=CARTESIAN_POINT('Ctrl Pts',(4.19814869599994,5.2,0.343609762999986));
#345763=CARTESIAN_POINT('Ctrl Pts',(4.19814869599994,2.2,0.343609762999986));
#345764=CARTESIAN_POINT('Ctrl Pts',(4.19663995799994,12.2,0.343980981999987));
#345765=CARTESIAN_POINT('Ctrl Pts',(4.19663995799994,5.2,0.343980981999987));
#345766=CARTESIAN_POINT('Ctrl Pts',(4.19663995799994,2.2,0.343980981999987));
#345767=CARTESIAN_POINT('Ctrl Pts',(4.19513530099994,12.2,0.344349341999983));
#345768=CARTESIAN_POINT('Ctrl Pts',(4.19513530099994,5.2,0.344349341999983));
#345769=CARTESIAN_POINT('Ctrl Pts',(4.19513530099994,2.2,0.344349341999983));
#345770=CARTESIAN_POINT('Ctrl Pts',(4.19363473699994,12.2,0.344714848999987));
#345771=CARTESIAN_POINT('Ctrl Pts',(4.19363473699994,5.2,0.344714848999987));
#345772=CARTESIAN_POINT('Ctrl Pts',(4.19363473699994,2.2,0.344714848999987));
#345773=CARTESIAN_POINT('Ctrl Pts',(4.19213827599994,12.2,0.345077513999983));
#345774=CARTESIAN_POINT('Ctrl Pts',(4.19213827599994,5.2,0.345077513999983));
#345775=CARTESIAN_POINT('Ctrl Pts',(4.19213827599994,2.2,0.345077513999983));
#345776=CARTESIAN_POINT('Ctrl Pts',(4.19064592699994,12.2,0.345437342999984));
#345777=CARTESIAN_POINT('Ctrl Pts',(4.19064592699994,5.2,0.345437342999984));
#345778=CARTESIAN_POINT('Ctrl Pts',(4.19064592699994,2.2,0.345437342999984));
#345779=CARTESIAN_POINT('Ctrl Pts',(4.18915770399995,12.2,0.345794341999985));
#345780=CARTESIAN_POINT('Ctrl Pts',(4.18915770399995,5.2,0.345794341999985));
#345781=CARTESIAN_POINT('Ctrl Pts',(4.18915770399995,2.2,0.345794341999985));
#345782=CARTESIAN_POINT('Ctrl Pts',(4.18767361599994,12.2,0.346148521999985));
#345783=CARTESIAN_POINT('Ctrl Pts',(4.18767361599994,5.2,0.346148521999985));
#345784=CARTESIAN_POINT('Ctrl Pts',(4.18767361599994,2.2,0.346148521999985));
#345785=CARTESIAN_POINT('Ctrl Pts',(4.18619367199994,12.2,0.346499887999983));
#345786=CARTESIAN_POINT('Ctrl Pts',(4.18619367199994,5.2,0.346499887999983));
#345787=CARTESIAN_POINT('Ctrl Pts',(4.18619367199994,2.2,0.346499887999983));
#345788=CARTESIAN_POINT('Ctrl Pts',(4.18471788499994,12.2,0.346848449999988));
#345789=CARTESIAN_POINT('Ctrl Pts',(4.18471788499994,5.2,0.346848449999988));
#345790=CARTESIAN_POINT('Ctrl Pts',(4.18471788499994,2.2,0.346848449999988));
#345791=CARTESIAN_POINT('Ctrl Pts',(4.18324626499994,12.2,0.347194214999984));
#345792=CARTESIAN_POINT('Ctrl Pts',(4.18324626499994,5.2,0.347194214999984));
#345793=CARTESIAN_POINT('Ctrl Pts',(4.18324626499994,2.2,0.347194214999984));
#345794=CARTESIAN_POINT('Ctrl Pts',(4.18177882199994,12.2,0.347537189999985));
#345795=CARTESIAN_POINT('Ctrl Pts',(4.18177882199994,5.2,0.347537189999985));
#345796=CARTESIAN_POINT('Ctrl Pts',(4.18177882199994,2.2,0.347537189999985));
#345797=CARTESIAN_POINT('Ctrl Pts',(4.18031556799995,12.2,0.347877382999986));
#345798=CARTESIAN_POINT('Ctrl Pts',(4.18031556799995,5.2,0.347877382999986));
#345799=CARTESIAN_POINT('Ctrl Pts',(4.18031556799995,2.2,0.347877382999986));
#345800=CARTESIAN_POINT('Ctrl Pts',(4.17885651199995,12.2,0.348214803999984));
#345801=CARTESIAN_POINT('Ctrl Pts',(4.17885651199995,5.2,0.348214803999984));
#345802=CARTESIAN_POINT('Ctrl Pts',(4.17885651199995,2.2,0.348214803999984));
#345803=CARTESIAN_POINT('Ctrl Pts',(4.17740166699994,12.2,0.348549458999985));
#345804=CARTESIAN_POINT('Ctrl Pts',(4.17740166699994,5.2,0.348549458999985));
#345805=CARTESIAN_POINT('Ctrl Pts',(4.17740166699994,2.2,0.348549458999985));
#345806=CARTESIAN_POINT('Ctrl Pts',(4.17595104199994,12.2,0.348881354999988));
#345807=CARTESIAN_POINT('Ctrl Pts',(4.17595104199994,5.2,0.348881354999988));
#345808=CARTESIAN_POINT('Ctrl Pts',(4.17595104199994,2.2,0.348881354999988));
#345809=CARTESIAN_POINT('Ctrl Pts',(4.17450464799995,12.2,0.349210502999986));
#345810=CARTESIAN_POINT('Ctrl Pts',(4.17450464799995,5.2,0.349210502999986));
#345811=CARTESIAN_POINT('Ctrl Pts',(4.17450464799995,2.2,0.349210502999986));
#345812=CARTESIAN_POINT('Ctrl Pts',(4.17306249699995,12.2,0.349536908999983));
#345813=CARTESIAN_POINT('Ctrl Pts',(4.17306249699995,5.2,0.349536908999983));
#345814=CARTESIAN_POINT('Ctrl Pts',(4.17306249699995,2.2,0.349536908999983));
#345815=CARTESIAN_POINT('Ctrl Pts',(4.17162459799994,12.2,0.349860581999986));
#345816=CARTESIAN_POINT('Ctrl Pts',(4.17162459799994,5.2,0.349860581999986));
#345817=CARTESIAN_POINT('Ctrl Pts',(4.17162459799994,2.2,0.349860581999986));
#345818=CARTESIAN_POINT('Ctrl Pts',(4.17019096299994,12.2,0.350181528999984));
#345819=CARTESIAN_POINT('Ctrl Pts',(4.17019096299994,5.2,0.350181528999984));
#345820=CARTESIAN_POINT('Ctrl Pts',(4.17019096299994,2.2,0.350181528999984));
#345821=CARTESIAN_POINT('Ctrl Pts',(4.16876160299995,12.2,0.350499758999985));
#345822=CARTESIAN_POINT('Ctrl Pts',(4.16876160299995,5.2,0.350499758999985));
#345823=CARTESIAN_POINT('Ctrl Pts',(4.16876160299995,2.2,0.350499758999985));
#345824=CARTESIAN_POINT('Ctrl Pts',(4.16733652799994,12.2,0.350815279999988));
#345825=CARTESIAN_POINT('Ctrl Pts',(4.16733652799994,5.2,0.350815279999988));
#345826=CARTESIAN_POINT('Ctrl Pts',(4.16733652799994,2.2,0.350815279999988));
#345827=CARTESIAN_POINT('Ctrl Pts',(4.16591574799994,12.2,0.351128100999984));
#345828=CARTESIAN_POINT('Ctrl Pts',(4.16591574799994,5.2,0.351128100999984));
#345829=CARTESIAN_POINT('Ctrl Pts',(4.16591574799994,2.2,0.351128100999984));
#345830=CARTESIAN_POINT('Ctrl Pts',(4.16449927599994,12.2,0.351438228999985));
#345831=CARTESIAN_POINT('Ctrl Pts',(4.16449927599994,5.2,0.351438228999985));
#345832=CARTESIAN_POINT('Ctrl Pts',(4.16449927599994,2.2,0.351438228999985));
#345833=CARTESIAN_POINT('Ctrl Pts',(4.16308712199995,12.2,0.351745671999986));
#345834=CARTESIAN_POINT('Ctrl Pts',(4.16308712199995,5.2,0.351745671999986));
#345835=CARTESIAN_POINT('Ctrl Pts',(4.16308712199995,2.2,0.351745671999986));
#345836=CARTESIAN_POINT('Ctrl Pts',(4.16167929599994,12.2,0.352050439999987));
#345837=CARTESIAN_POINT('Ctrl Pts',(4.16167929599994,5.2,0.352050439999987));
#345838=CARTESIAN_POINT('Ctrl Pts',(4.16167929599994,2.2,0.352050439999987));
#345839=CARTESIAN_POINT('Ctrl Pts',(4.16027580999994,12.2,0.352352540999985));
#345840=CARTESIAN_POINT('Ctrl Pts',(4.16027580999994,5.2,0.352352540999985));
#345841=CARTESIAN_POINT('Ctrl Pts',(4.16027580999994,2.2,0.352352540999985));
#345842=CARTESIAN_POINT('Ctrl Pts',(4.15887667599994,12.2,0.352651980999985));
#345843=CARTESIAN_POINT('Ctrl Pts',(4.15887667599994,5.2,0.352651980999985));
#345844=CARTESIAN_POINT('Ctrl Pts',(4.15887667599994,2.2,0.352651980999985));
#345845=CARTESIAN_POINT('Ctrl Pts',(4.15748190099994,12.2,0.352948770999983));
#345846=CARTESIAN_POINT('Ctrl Pts',(4.15748190099994,5.2,0.352948770999983));
#345847=CARTESIAN_POINT('Ctrl Pts',(4.15748190099994,2.2,0.352948770999983));
#345848=CARTESIAN_POINT('Ctrl Pts',(4.15609149899994,12.2,0.353242917999985));
#345849=CARTESIAN_POINT('Ctrl Pts',(4.15609149899994,5.2,0.353242917999985));
#345850=CARTESIAN_POINT('Ctrl Pts',(4.15609149899994,2.2,0.353242917999985));
#345851=CARTESIAN_POINT('Ctrl Pts',(4.15470548099994,12.2,0.353534431999982));
#345852=CARTESIAN_POINT('Ctrl Pts',(4.15470548099994,5.2,0.353534431999982));
#345853=CARTESIAN_POINT('Ctrl Pts',(4.15470548099994,2.2,0.353534431999982));
#345854=CARTESIAN_POINT('Ctrl Pts',(4.15332385599995,12.2,0.353823319999984));
#345855=CARTESIAN_POINT('Ctrl Pts',(4.15332385599995,5.2,0.353823319999984));
#345856=CARTESIAN_POINT('Ctrl Pts',(4.15332385599995,2.2,0.353823319999984));
#345857=CARTESIAN_POINT('Ctrl Pts',(4.15194663699994,12.2,0.354109590999983));
#345858=CARTESIAN_POINT('Ctrl Pts',(4.15194663699994,5.2,0.354109590999983));
#345859=CARTESIAN_POINT('Ctrl Pts',(4.15194663699994,2.2,0.354109590999983));
#345860=CARTESIAN_POINT('Ctrl Pts',(4.15057383399995,12.2,0.354393252999987));
#345861=CARTESIAN_POINT('Ctrl Pts',(4.15057383399995,5.2,0.354393252999987));
#345862=CARTESIAN_POINT('Ctrl Pts',(4.15057383399995,2.2,0.354393252999987));
#345863=CARTESIAN_POINT('Ctrl Pts',(4.14920545699994,12.2,0.354674315999985));
#345864=CARTESIAN_POINT('Ctrl Pts',(4.14920545699994,5.2,0.354674315999985));
#345865=CARTESIAN_POINT('Ctrl Pts',(4.14920545699994,2.2,0.354674315999985));
#345866=CARTESIAN_POINT('Ctrl Pts',(4.14784151899994,12.2,0.354952786999987));
#345867=CARTESIAN_POINT('Ctrl Pts',(4.14784151899994,5.2,0.354952786999987));
#345868=CARTESIAN_POINT('Ctrl Pts',(4.14784151899994,2.2,0.354952786999987));
#345869=CARTESIAN_POINT('Ctrl Pts',(4.14648202999994,12.2,0.355228675999988));
#345870=CARTESIAN_POINT('Ctrl Pts',(4.14648202999994,5.2,0.355228675999988));
#345871=CARTESIAN_POINT('Ctrl Pts',(4.14648202999994,2.2,0.355228675999988));
#345872=CARTESIAN_POINT('Ctrl Pts',(4.14512700099994,12.2,0.355501990999985));
#345873=CARTESIAN_POINT('Ctrl Pts',(4.14512700099994,5.2,0.355501990999985));
#345874=CARTESIAN_POINT('Ctrl Pts',(4.14512700099994,2.2,0.355501990999985));
#345875=CARTESIAN_POINT('Ctrl Pts',(4.14377644299995,12.2,0.355772740999987));
#345876=CARTESIAN_POINT('Ctrl Pts',(4.14377644299995,5.2,0.355772740999987));
#345877=CARTESIAN_POINT('Ctrl Pts',(4.14377644299995,2.2,0.355772740999987));
#345878=CARTESIAN_POINT('Ctrl Pts',(4.14243036799994,12.2,0.356040933999986));
#345879=CARTESIAN_POINT('Ctrl Pts',(4.14243036799994,5.2,0.356040933999986));
#345880=CARTESIAN_POINT('Ctrl Pts',(4.14243036799994,2.2,0.356040933999986));
#345881=CARTESIAN_POINT('Ctrl Pts',(4.14108878399994,12.2,0.356306579999988));
#345882=CARTESIAN_POINT('Ctrl Pts',(4.14108878399994,5.2,0.356306579999988));
#345883=CARTESIAN_POINT('Ctrl Pts',(4.14108878399994,2.2,0.356306579999988));
#345884=CARTESIAN_POINT('Ctrl Pts',(4.13975170499994,12.2,0.356569686999983));
#345885=CARTESIAN_POINT('Ctrl Pts',(4.13975170499994,5.2,0.356569686999983));
#345886=CARTESIAN_POINT('Ctrl Pts',(4.13975170499994,2.2,0.356569686999983));
#345887=CARTESIAN_POINT('Ctrl Pts',(4.13841914099994,12.2,0.356830263999988));
#345888=CARTESIAN_POINT('Ctrl Pts',(4.13841914099994,5.2,0.356830263999988));
#345889=CARTESIAN_POINT('Ctrl Pts',(4.13841914099994,2.2,0.356830263999988));
#345890=CARTESIAN_POINT('Ctrl Pts',(4.13709110399994,12.2,0.357088320999988));
#345891=CARTESIAN_POINT('Ctrl Pts',(4.13709110399994,5.2,0.357088320999988));
#345892=CARTESIAN_POINT('Ctrl Pts',(4.13709110399994,2.2,0.357088320999988));
#345893=CARTESIAN_POINT('Ctrl Pts',(4.13576760499994,12.2,0.357343863999984));
#345894=CARTESIAN_POINT('Ctrl Pts',(4.13576760499994,5.2,0.357343863999984));
#345895=CARTESIAN_POINT('Ctrl Pts',(4.13576760499994,2.2,0.357343863999984));
#345896=CARTESIAN_POINT('Ctrl Pts',(4.13444865299994,12.2,0.357596904999986));
#345897=CARTESIAN_POINT('Ctrl Pts',(4.13444865299994,5.2,0.357596904999986));
#345898=CARTESIAN_POINT('Ctrl Pts',(4.13444865299994,2.2,0.357596904999986));
#345899=CARTESIAN_POINT('Ctrl Pts',(4.13313426199994,12.2,0.357847450999986));
#345900=CARTESIAN_POINT('Ctrl Pts',(4.13313426199994,5.2,0.357847450999986));
#345901=CARTESIAN_POINT('Ctrl Pts',(4.13313426199994,2.2,0.357847450999986));
#345902=CARTESIAN_POINT('Ctrl Pts',(4.13182443999994,12.2,0.358095511999985));
#345903=CARTESIAN_POINT('Ctrl Pts',(4.13182443999994,5.2,0.358095511999985));
#345904=CARTESIAN_POINT('Ctrl Pts',(4.13182443999994,2.2,0.358095511999985));
#345905=CARTESIAN_POINT('Ctrl Pts',(4.13051920099995,12.2,0.358341096999983));
#345906=CARTESIAN_POINT('Ctrl Pts',(4.13051920099995,5.2,0.358341096999983));
#345907=CARTESIAN_POINT('Ctrl Pts',(4.13051920099995,2.2,0.358341096999983));
#345908=CARTESIAN_POINT('Ctrl Pts',(4.12921855399994,12.2,0.358584215999986));
#345909=CARTESIAN_POINT('Ctrl Pts',(4.12921855399994,5.2,0.358584215999986));
#345910=CARTESIAN_POINT('Ctrl Pts',(4.12921855399994,2.2,0.358584215999986));
#345911=CARTESIAN_POINT('Ctrl Pts',(4.12792251299994,12.2,0.358824875999986));
#345912=CARTESIAN_POINT('Ctrl Pts',(4.12792251299994,5.2,0.358824875999986));
#345913=CARTESIAN_POINT('Ctrl Pts',(4.12792251299994,2.2,0.358824875999986));
#345914=CARTESIAN_POINT('Ctrl Pts',(4.12663108599994,12.2,0.359063086999987));
#345915=CARTESIAN_POINT('Ctrl Pts',(4.12663108599994,5.2,0.359063086999987));
#345916=CARTESIAN_POINT('Ctrl Pts',(4.12663108599994,2.2,0.359063086999987));
#345917=CARTESIAN_POINT('Ctrl Pts',(4.12534428599994,12.2,0.359298858999986));
#345918=CARTESIAN_POINT('Ctrl Pts',(4.12534428599994,5.2,0.359298858999986));
#345919=CARTESIAN_POINT('Ctrl Pts',(4.12534428599994,2.2,0.359298858999986));
#345920=CARTESIAN_POINT('Ctrl Pts',(4.12406212399994,12.2,0.359532199999983));
#345921=CARTESIAN_POINT('Ctrl Pts',(4.12406212399994,5.2,0.359532199999983));
#345922=CARTESIAN_POINT('Ctrl Pts',(4.12406212399994,2.2,0.359532199999983));
#345923=CARTESIAN_POINT('Ctrl Pts',(4.12278461099994,12.2,0.359763120999985));
#345924=CARTESIAN_POINT('Ctrl Pts',(4.12278461099994,5.2,0.359763120999985));
#345925=CARTESIAN_POINT('Ctrl Pts',(4.12278461099994,2.2,0.359763120999985));
#345926=CARTESIAN_POINT('Ctrl Pts',(4.12151175799994,12.2,0.359991628999987));
#345927=CARTESIAN_POINT('Ctrl Pts',(4.12151175799994,5.2,0.359991628999987));
#345928=CARTESIAN_POINT('Ctrl Pts',(4.12151175799994,2.2,0.359991628999987));
#345929=CARTESIAN_POINT('Ctrl Pts',(4.12024357499994,12.2,0.360217734999986));
#345930=CARTESIAN_POINT('Ctrl Pts',(4.12024357499994,5.2,0.360217734999986));
#345931=CARTESIAN_POINT('Ctrl Pts',(4.12024357499994,2.2,0.360217734999986));
#345932=CARTESIAN_POINT('Ctrl Pts',(4.11898007599994,12.2,0.360441448999986));
#345933=CARTESIAN_POINT('Ctrl Pts',(4.11898007599994,5.2,0.360441448999986));
#345934=CARTESIAN_POINT('Ctrl Pts',(4.11898007599994,2.2,0.360441448999986));
#345935=CARTESIAN_POINT('Ctrl Pts',(4.11772127099994,12.2,0.360662777999985));
#345936=CARTESIAN_POINT('Ctrl Pts',(4.11772127099994,5.2,0.360662777999985));
#345937=CARTESIAN_POINT('Ctrl Pts',(4.11772127099994,2.2,0.360662777999985));
#345938=CARTESIAN_POINT('Ctrl Pts',(4.11646717199995,12.2,0.360881732999987));
#345939=CARTESIAN_POINT('Ctrl Pts',(4.11646717199995,5.2,0.360881732999987));
#345940=CARTESIAN_POINT('Ctrl Pts',(4.11646717199995,2.2,0.360881732999987));
#345941=CARTESIAN_POINT('Ctrl Pts',(4.11521778799994,12.2,0.361098323999984));
#345942=CARTESIAN_POINT('Ctrl Pts',(4.11521778799994,5.2,0.361098323999984));
#345943=CARTESIAN_POINT('Ctrl Pts',(4.11521778799994,2.2,0.361098323999984));
#345944=CARTESIAN_POINT('Ctrl Pts',(4.11397313199994,12.2,0.361312558999987));
#345945=CARTESIAN_POINT('Ctrl Pts',(4.11397313199994,5.2,0.361312558999987));
#345946=CARTESIAN_POINT('Ctrl Pts',(4.11397313199994,2.2,0.361312558999987));
#345947=CARTESIAN_POINT('Ctrl Pts',(4.11273321599994,12.2,0.361524448999986));
#345948=CARTESIAN_POINT('Ctrl Pts',(4.11273321599994,5.2,0.361524448999986));
#345949=CARTESIAN_POINT('Ctrl Pts',(4.11273321599994,2.2,0.361524448999986));
#345950=CARTESIAN_POINT('Ctrl Pts',(4.11149805099994,12.2,0.361734002999987));
#345951=CARTESIAN_POINT('Ctrl Pts',(4.11149805099994,5.2,0.361734002999987));
#345952=CARTESIAN_POINT('Ctrl Pts',(4.11149805099994,2.2,0.361734002999987));
#345953=CARTESIAN_POINT('Ctrl Pts',(4.11026764599994,12.2,0.361941229999987));
#345954=CARTESIAN_POINT('Ctrl Pts',(4.11026764599994,5.2,0.361941229999987));
#345955=CARTESIAN_POINT('Ctrl Pts',(4.11026764599994,2.2,0.361941229999987));
#345956=CARTESIAN_POINT('Ctrl Pts',(4.10904201499994,12.2,0.362146139999986));
#345957=CARTESIAN_POINT('Ctrl Pts',(4.10904201499994,5.2,0.362146139999986));
#345958=CARTESIAN_POINT('Ctrl Pts',(4.10904201499994,2.2,0.362146139999986));
#345959=CARTESIAN_POINT('Ctrl Pts',(4.10782116899994,12.2,0.362348742999985));
#345960=CARTESIAN_POINT('Ctrl Pts',(4.10782116899994,5.2,0.362348742999985));
#345961=CARTESIAN_POINT('Ctrl Pts',(4.10782116899994,2.2,0.362348742999985));
#345962=CARTESIAN_POINT('Ctrl Pts',(4.10660511699994,12.2,0.362549048999985));
#345963=CARTESIAN_POINT('Ctrl Pts',(4.10660511699994,5.2,0.362549048999985));
#345964=CARTESIAN_POINT('Ctrl Pts',(4.10660511699994,2.2,0.362549048999985));
#345965=CARTESIAN_POINT('Ctrl Pts',(4.10539387399994,12.2,0.362747067999987));
#345966=CARTESIAN_POINT('Ctrl Pts',(4.10539387399994,5.2,0.362747067999987));
#345967=CARTESIAN_POINT('Ctrl Pts',(4.10539387399994,2.2,0.362747067999987));
#345968=CARTESIAN_POINT('Ctrl Pts',(4.10418744999994,12.2,0.362942807999986));
#345969=CARTESIAN_POINT('Ctrl Pts',(4.10418744999994,5.2,0.362942807999986));
#345970=CARTESIAN_POINT('Ctrl Pts',(4.10418744999994,2.2,0.362942807999986));
#345971=CARTESIAN_POINT('Ctrl Pts',(4.10298585499994,12.2,0.363136280999985));
#345972=CARTESIAN_POINT('Ctrl Pts',(4.10298585499994,5.2,0.363136280999985));
#345973=CARTESIAN_POINT('Ctrl Pts',(4.10298585499994,2.2,0.363136280999985));
#345974=CARTESIAN_POINT('Ctrl Pts',(4.10178910199994,12.2,0.363327494999983));
#345975=CARTESIAN_POINT('Ctrl Pts',(4.10178910199994,5.2,0.363327494999983));
#345976=CARTESIAN_POINT('Ctrl Pts',(4.10178910199994,2.2,0.363327494999983));
#345977=CARTESIAN_POINT('Ctrl Pts',(4.10059720199994,12.2,0.363516460999986));
#345978=CARTESIAN_POINT('Ctrl Pts',(4.10059720199994,5.2,0.363516460999986));
#345979=CARTESIAN_POINT('Ctrl Pts',(4.10059720199994,2.2,0.363516460999986));
#345980=CARTESIAN_POINT('Ctrl Pts',(4.09941016599995,12.2,0.363703188999986));
#345981=CARTESIAN_POINT('Ctrl Pts',(4.09941016599995,5.2,0.363703188999986));
#345982=CARTESIAN_POINT('Ctrl Pts',(4.09941016599995,2.2,0.363703188999986));
#345983=CARTESIAN_POINT('Ctrl Pts',(4.09822800699995,12.2,0.363887689999984));
#345984=CARTESIAN_POINT('Ctrl Pts',(4.09822800699995,5.2,0.363887689999984));
#345985=CARTESIAN_POINT('Ctrl Pts',(4.09822800699995,2.2,0.363887689999984));
#345986=CARTESIAN_POINT('Ctrl Pts',(4.09705073399994,12.2,0.364069971999985));
#345987=CARTESIAN_POINT('Ctrl Pts',(4.09705073399994,5.2,0.364069971999985));
#345988=CARTESIAN_POINT('Ctrl Pts',(4.09705073399994,2.2,0.364069971999985));
#345989=CARTESIAN_POINT('Ctrl Pts',(4.09587836199994,12.2,0.364250044999985));
#345990=CARTESIAN_POINT('Ctrl Pts',(4.09587836199994,5.2,0.364250044999985));
#345991=CARTESIAN_POINT('Ctrl Pts',(4.09587836199994,2.2,0.364250044999985));
#345992=CARTESIAN_POINT('Ctrl Pts',(4.09471089799994,12.2,0.364427920999986));
#345993=CARTESIAN_POINT('Ctrl Pts',(4.09471089799994,5.2,0.364427920999986));
#345994=CARTESIAN_POINT('Ctrl Pts',(4.09471089799994,2.2,0.364427920999986));
#345995=CARTESIAN_POINT('Ctrl Pts',(4.09354835799994,12.2,0.364603608999987));
#345996=CARTESIAN_POINT('Ctrl Pts',(4.09354835799994,5.2,0.364603608999987));
#345997=CARTESIAN_POINT('Ctrl Pts',(4.09354835799994,2.2,0.364603608999987));
#345998=CARTESIAN_POINT('Ctrl Pts',(4.09239074999994,12.2,0.364777118999986));
#345999=CARTESIAN_POINT('Ctrl Pts',(4.09239074999994,5.2,0.364777118999986));
#346000=CARTESIAN_POINT('Ctrl Pts',(4.09239074999994,2.2,0.364777118999986));
#346001=CARTESIAN_POINT('Ctrl Pts',(4.09123808799994,12.2,0.364948461999983));
#346002=CARTESIAN_POINT('Ctrl Pts',(4.09123808799994,5.2,0.364948461999983));
#346003=CARTESIAN_POINT('Ctrl Pts',(4.09123808799994,2.2,0.364948461999983));
#346004=CARTESIAN_POINT('Ctrl Pts',(4.09009038199994,12.2,0.365117647999984));
#346005=CARTESIAN_POINT('Ctrl Pts',(4.09009038199994,5.2,0.365117647999984));
#346006=CARTESIAN_POINT('Ctrl Pts',(4.09009038199994,2.2,0.365117647999984));
#346007=CARTESIAN_POINT('Ctrl Pts',(4.08894764399994,12.2,0.365284685999985));
#346008=CARTESIAN_POINT('Ctrl Pts',(4.08894764399994,5.2,0.365284685999985));
#346009=CARTESIAN_POINT('Ctrl Pts',(4.08894764399994,2.2,0.365284685999985));
#346010=CARTESIAN_POINT('Ctrl Pts',(4.08780988599994,12.2,0.365449588999986));
#346011=CARTESIAN_POINT('Ctrl Pts',(4.08780988599994,5.2,0.365449588999986));
#346012=CARTESIAN_POINT('Ctrl Pts',(4.08780988599994,2.2,0.365449588999986));
#346013=CARTESIAN_POINT('Ctrl Pts',(4.08667711999994,12.2,0.365612363999985));
#346014=CARTESIAN_POINT('Ctrl Pts',(4.08667711999994,5.2,0.365612363999985));
#346015=CARTESIAN_POINT('Ctrl Pts',(4.08667711999994,2.2,0.365612363999985));
#346016=CARTESIAN_POINT('Ctrl Pts',(4.08554935699994,12.2,0.365773025999987));
#346017=CARTESIAN_POINT('Ctrl Pts',(4.08554935699994,5.2,0.365773025999987));
#346018=CARTESIAN_POINT('Ctrl Pts',(4.08554935699994,2.2,0.365773025999987));
#346019=CARTESIAN_POINT('Ctrl Pts',(4.08442660799994,12.2,0.365931580999987));
#346020=CARTESIAN_POINT('Ctrl Pts',(4.08442660799994,5.2,0.365931580999987));
#346021=CARTESIAN_POINT('Ctrl Pts',(4.08442660799994,2.2,0.365931580999987));
#346022=CARTESIAN_POINT('Ctrl Pts',(4.08330888599994,12.2,0.366088040999983));
#346023=CARTESIAN_POINT('Ctrl Pts',(4.08330888599994,5.2,0.366088040999983));
#346024=CARTESIAN_POINT('Ctrl Pts',(4.08330888599994,2.2,0.366088040999983));
#346025=CARTESIAN_POINT('Ctrl Pts',(4.08219620099994,12.2,0.366242417999985));
#346026=CARTESIAN_POINT('Ctrl Pts',(4.08219620099994,5.2,0.366242417999985));
#346027=CARTESIAN_POINT('Ctrl Pts',(4.08219620099994,2.2,0.366242417999985));
#346028=CARTESIAN_POINT('Ctrl Pts',(4.08108856699995,12.2,0.366394719999987));
#346029=CARTESIAN_POINT('Ctrl Pts',(4.08108856699995,5.2,0.366394719999987));
#346030=CARTESIAN_POINT('Ctrl Pts',(4.08108856699995,2.2,0.366394719999987));
#346031=CARTESIAN_POINT('Ctrl Pts',(4.07998599399995,12.2,0.366544959999988));
#346032=CARTESIAN_POINT('Ctrl Pts',(4.07998599399995,5.2,0.366544959999988));
#346033=CARTESIAN_POINT('Ctrl Pts',(4.07998599399995,2.2,0.366544959999988));
#346034=CARTESIAN_POINT('Ctrl Pts',(4.07888849299994,12.2,0.366693146999988));
#346035=CARTESIAN_POINT('Ctrl Pts',(4.07888849299994,5.2,0.366693146999988));
#346036=CARTESIAN_POINT('Ctrl Pts',(4.07888849299994,2.2,0.366693146999988));
#346037=CARTESIAN_POINT('Ctrl Pts',(4.07779607799994,12.2,0.366839292999988));
#346038=CARTESIAN_POINT('Ctrl Pts',(4.07779607799994,5.2,0.366839292999988));
#346039=CARTESIAN_POINT('Ctrl Pts',(4.07779607799994,2.2,0.366839292999988));
#346040=CARTESIAN_POINT('Ctrl Pts',(4.07670875899994,12.2,0.366983407999988));
#346041=CARTESIAN_POINT('Ctrl Pts',(4.07670875899994,5.2,0.366983407999988));
#346042=CARTESIAN_POINT('Ctrl Pts',(4.07670875899994,2.2,0.366983407999988));
#346043=CARTESIAN_POINT('Ctrl Pts',(4.07562654799994,12.2,0.367125501999985));
#346044=CARTESIAN_POINT('Ctrl Pts',(4.07562654799994,5.2,0.367125501999985));
#346045=CARTESIAN_POINT('Ctrl Pts',(4.07562654799994,2.2,0.367125501999985));
#346046=CARTESIAN_POINT('Ctrl Pts',(4.07454945699994,12.2,0.367265587999985));
#346047=CARTESIAN_POINT('Ctrl Pts',(4.07454945699994,5.2,0.367265587999985));
#346048=CARTESIAN_POINT('Ctrl Pts',(4.07454945699994,2.2,0.367265587999985));
#346049=CARTESIAN_POINT('Ctrl Pts',(4.07347749899994,12.2,0.367403674999984));
#346050=CARTESIAN_POINT('Ctrl Pts',(4.07347749899994,5.2,0.367403674999984));
#346051=CARTESIAN_POINT('Ctrl Pts',(4.07347749899994,2.2,0.367403674999984));
#346052=CARTESIAN_POINT('Ctrl Pts',(4.07241068399994,12.2,0.367539774999983));
#346053=CARTESIAN_POINT('Ctrl Pts',(4.07241068399994,5.2,0.367539774999983));
#346054=CARTESIAN_POINT('Ctrl Pts',(4.07241068399994,2.2,0.367539774999983));
#346055=CARTESIAN_POINT('Ctrl Pts',(4.07134902399994,12.2,0.367673896999987));
#346056=CARTESIAN_POINT('Ctrl Pts',(4.07134902399994,5.2,0.367673896999987));
#346057=CARTESIAN_POINT('Ctrl Pts',(4.07134902399994,2.2,0.367673896999987));
#346058=CARTESIAN_POINT('Ctrl Pts',(4.07029253099994,12.2,0.367806055999989));
#346059=CARTESIAN_POINT('Ctrl Pts',(4.07029253099994,5.2,0.367806055999989));
#346060=CARTESIAN_POINT('Ctrl Pts',(4.07029253099994,2.2,0.367806055999989));
#346061=CARTESIAN_POINT('Ctrl Pts',(4.06924121799995,12.2,0.367936258999984));
#346062=CARTESIAN_POINT('Ctrl Pts',(4.06924121799995,5.2,0.367936258999984));
#346063=CARTESIAN_POINT('Ctrl Pts',(4.06924121799995,2.2,0.367936258999984));
#346064=CARTESIAN_POINT('Ctrl Pts',(4.06819509499995,12.2,0.368064516999986));
#346065=CARTESIAN_POINT('Ctrl Pts',(4.06819509499995,5.2,0.368064516999986));
#346066=CARTESIAN_POINT('Ctrl Pts',(4.06819509499995,2.2,0.368064516999986));
#346067=CARTESIAN_POINT('Ctrl Pts',(4.06715417699994,12.2,0.368190844999985));
#346068=CARTESIAN_POINT('Ctrl Pts',(4.06715417699994,5.2,0.368190844999985));
#346069=CARTESIAN_POINT('Ctrl Pts',(4.06715417699994,2.2,0.368190844999985));
#346070=CARTESIAN_POINT('Ctrl Pts',(4.06611847099995,12.2,0.368315250999984));
#346071=CARTESIAN_POINT('Ctrl Pts',(4.06611847099995,5.2,0.368315250999984));
#346072=CARTESIAN_POINT('Ctrl Pts',(4.06611847099995,2.2,0.368315250999984));
#346073=CARTESIAN_POINT('Ctrl Pts',(4.06508799299994,12.2,0.368437746999986));
#346074=CARTESIAN_POINT('Ctrl Pts',(4.06508799299994,5.2,0.368437746999986));
#346075=CARTESIAN_POINT('Ctrl Pts',(4.06508799299994,2.2,0.368437746999986));
#346076=CARTESIAN_POINT('Ctrl Pts',(4.06406275399994,12.2,0.368558344999985));
#346077=CARTESIAN_POINT('Ctrl Pts',(4.06406275399994,5.2,0.368558344999985));
#346078=CARTESIAN_POINT('Ctrl Pts',(4.06406275399994,2.2,0.368558344999985));
#346079=CARTESIAN_POINT('Ctrl Pts',(4.06304276399994,12.2,0.368677054999988));
#346080=CARTESIAN_POINT('Ctrl Pts',(4.06304276399994,5.2,0.368677054999988));
#346081=CARTESIAN_POINT('Ctrl Pts',(4.06304276399994,2.2,0.368677054999988));
#346082=CARTESIAN_POINT('Ctrl Pts',(4.06202803699994,12.2,0.368793888999988));
#346083=CARTESIAN_POINT('Ctrl Pts',(4.06202803699994,5.2,0.368793888999988));
#346084=CARTESIAN_POINT('Ctrl Pts',(4.06202803699994,2.2,0.368793888999988));
#346085=CARTESIAN_POINT('Ctrl Pts',(4.06101858399994,12.2,0.368908857999983));
#346086=CARTESIAN_POINT('Ctrl Pts',(4.06101858399994,5.2,0.368908857999983));
#346087=CARTESIAN_POINT('Ctrl Pts',(4.06101858399994,2.2,0.368908857999983));
#346088=CARTESIAN_POINT('Ctrl Pts',(4.06001441899994,12.2,0.369021973999986));
#346089=CARTESIAN_POINT('Ctrl Pts',(4.06001441899994,5.2,0.369021973999986));
#346090=CARTESIAN_POINT('Ctrl Pts',(4.06001441899994,2.2,0.369021973999986));
#346091=CARTESIAN_POINT('Ctrl Pts',(4.05901555099994,12.2,0.369133247999986));
#346092=CARTESIAN_POINT('Ctrl Pts',(4.05901555099994,5.2,0.369133247999986));
#346093=CARTESIAN_POINT('Ctrl Pts',(4.05901555099994,2.2,0.369133247999986));
#346094=CARTESIAN_POINT('Ctrl Pts',(4.05802199399994,12.2,0.369242691999982));
#346095=CARTESIAN_POINT('Ctrl Pts',(4.05802199399994,5.2,0.369242691999982));
#346096=CARTESIAN_POINT('Ctrl Pts',(4.05802199399994,2.2,0.369242691999982));
#346097=CARTESIAN_POINT('Ctrl Pts',(4.05703375799995,12.2,0.369350315999988));
#346098=CARTESIAN_POINT('Ctrl Pts',(4.05703375799995,5.2,0.369350315999988));
#346099=CARTESIAN_POINT('Ctrl Pts',(4.05703375799995,2.2,0.369350315999988));
#346100=CARTESIAN_POINT('Ctrl Pts',(4.05605085799994,12.2,0.369456134999986));
#346101=CARTESIAN_POINT('Ctrl Pts',(4.05605085799994,5.2,0.369456134999986));
#346102=CARTESIAN_POINT('Ctrl Pts',(4.05605085799994,2.2,0.369456134999986));
#346103=CARTESIAN_POINT('Ctrl Pts',(4.05507330299994,12.2,0.369560156999986));
#346104=CARTESIAN_POINT('Ctrl Pts',(4.05507330299994,5.2,0.369560156999986));
#346105=CARTESIAN_POINT('Ctrl Pts',(4.05507330299994,2.2,0.369560156999986));
#346106=CARTESIAN_POINT('Ctrl Pts',(4.05410110799994,12.2,0.369662395999986));
#346107=CARTESIAN_POINT('Ctrl Pts',(4.05410110799994,5.2,0.369662395999986));
#346108=CARTESIAN_POINT('Ctrl Pts',(4.05410110799994,2.2,0.369662395999986));
#346109=CARTESIAN_POINT('Ctrl Pts',(4.05313428299995,12.2,0.369762862999985));
#346110=CARTESIAN_POINT('Ctrl Pts',(4.05313428299995,5.2,0.369762862999985));
#346111=CARTESIAN_POINT('Ctrl Pts',(4.05313428299995,2.2,0.369762862999985));
#346112=CARTESIAN_POINT('Ctrl Pts',(4.05217283999994,12.2,0.369861568999985));
#346113=CARTESIAN_POINT('Ctrl Pts',(4.05217283999994,5.2,0.369861568999985));
#346114=CARTESIAN_POINT('Ctrl Pts',(4.05217283999994,2.2,0.369861568999985));
#346115=CARTESIAN_POINT('Ctrl Pts',(4.05121679299994,12.2,0.369958526999987));
#346116=CARTESIAN_POINT('Ctrl Pts',(4.05121679299994,5.2,0.369958526999987));
#346117=CARTESIAN_POINT('Ctrl Pts',(4.05121679299994,2.2,0.369958526999987));
#346118=CARTESIAN_POINT('Ctrl Pts',(4.05026615299994,12.2,0.370053747999983));
#346119=CARTESIAN_POINT('Ctrl Pts',(4.05026615299994,5.2,0.370053747999983));
#346120=CARTESIAN_POINT('Ctrl Pts',(4.05026615299994,2.2,0.370053747999983));
#346121=CARTESIAN_POINT('Ctrl Pts',(4.04932093099994,12.2,0.370147244999988));
#346122=CARTESIAN_POINT('Ctrl Pts',(4.04932093099994,5.2,0.370147244999988));
#346123=CARTESIAN_POINT('Ctrl Pts',(4.04932093099994,2.2,0.370147244999988));
#346124=CARTESIAN_POINT('Ctrl Pts',(4.04838114099995,12.2,0.370239027999983));
#346125=CARTESIAN_POINT('Ctrl Pts',(4.04838114099995,5.2,0.370239027999983));
#346126=CARTESIAN_POINT('Ctrl Pts',(4.04838114099995,2.2,0.370239027999983));
#346127=CARTESIAN_POINT('Ctrl Pts',(4.04744679499994,12.2,0.370329110999985));
#346128=CARTESIAN_POINT('Ctrl Pts',(4.04744679499994,5.2,0.370329110999985));
#346129=CARTESIAN_POINT('Ctrl Pts',(4.04744679499994,2.2,0.370329110999985));
#346130=CARTESIAN_POINT('Ctrl Pts',(4.04651790299994,12.2,0.370417505999985));
#346131=CARTESIAN_POINT('Ctrl Pts',(4.04651790299994,5.2,0.370417505999985));
#346132=CARTESIAN_POINT('Ctrl Pts',(4.04651790299994,2.2,0.370417505999985));
#346133=CARTESIAN_POINT('Ctrl Pts',(4.04559448099994,12.2,0.370504222999983));
#346134=CARTESIAN_POINT('Ctrl Pts',(4.04559448099994,5.2,0.370504222999983));
#346135=CARTESIAN_POINT('Ctrl Pts',(4.04559448099994,2.2,0.370504222999983));
#346136=CARTESIAN_POINT('Ctrl Pts',(4.04467653799994,12.2,0.370589276999986));
#346137=CARTESIAN_POINT('Ctrl Pts',(4.04467653799994,5.2,0.370589276999986));
#346138=CARTESIAN_POINT('Ctrl Pts',(4.04467653799994,2.2,0.370589276999986));
#346139=CARTESIAN_POINT('Ctrl Pts',(4.04376408699994,12.2,0.370672677999986));
#346140=CARTESIAN_POINT('Ctrl Pts',(4.04376408699994,5.2,0.370672677999986));
#346141=CARTESIAN_POINT('Ctrl Pts',(4.04376408699994,2.2,0.370672677999986));
#346142=CARTESIAN_POINT('Ctrl Pts',(4.04285714099994,12.2,0.370754438999987));
#346143=CARTESIAN_POINT('Ctrl Pts',(4.04285714099994,5.2,0.370754438999987));
#346144=CARTESIAN_POINT('Ctrl Pts',(4.04285714099994,2.2,0.370754438999987));
#346145=CARTESIAN_POINT('Ctrl Pts',(4.04195571199994,12.2,0.370834572999983));
#346146=CARTESIAN_POINT('Ctrl Pts',(4.04195571199994,5.2,0.370834572999983));
#346147=CARTESIAN_POINT('Ctrl Pts',(4.04195571199994,2.2,0.370834572999983));
#346148=CARTESIAN_POINT('Ctrl Pts',(4.04105981299994,12.2,0.370913090999987));
#346149=CARTESIAN_POINT('Ctrl Pts',(4.04105981299994,5.2,0.370913090999987));
#346150=CARTESIAN_POINT('Ctrl Pts',(4.04105981299994,2.2,0.370913090999987));
#346151=CARTESIAN_POINT('Ctrl Pts',(4.04016945399994,12.2,0.370990005999987));
#346152=CARTESIAN_POINT('Ctrl Pts',(4.04016945399994,5.2,0.370990005999987));
#346153=CARTESIAN_POINT('Ctrl Pts',(4.04016945399994,2.2,0.370990005999987));
#346154=CARTESIAN_POINT('Ctrl Pts',(4.03928464999994,12.2,0.371065330999985));
#346155=CARTESIAN_POINT('Ctrl Pts',(4.03928464999994,5.2,0.371065330999985));
#346156=CARTESIAN_POINT('Ctrl Pts',(4.03928464999994,2.2,0.371065330999985));
#346157=CARTESIAN_POINT('Ctrl Pts',(4.03840541199994,12.2,0.371139076999984));
#346158=CARTESIAN_POINT('Ctrl Pts',(4.03840541199994,5.2,0.371139076999984));
#346159=CARTESIAN_POINT('Ctrl Pts',(4.03840541199994,2.2,0.371139076999984));
#346160=CARTESIAN_POINT('Ctrl Pts',(4.03753175299994,12.2,0.371211257999988));
#346161=CARTESIAN_POINT('Ctrl Pts',(4.03753175299994,5.2,0.371211257999988));
#346162=CARTESIAN_POINT('Ctrl Pts',(4.03753175299994,2.2,0.371211257999988));
#346163=CARTESIAN_POINT('Ctrl Pts',(4.03666368399994,12.2,0.371281886999988));
#346164=CARTESIAN_POINT('Ctrl Pts',(4.03666368399994,5.2,0.371281886999988));
#346165=CARTESIAN_POINT('Ctrl Pts',(4.03666368399994,2.2,0.371281886999988));
#346166=CARTESIAN_POINT('Ctrl Pts',(4.03580121899994,12.2,0.371350974999984));
#346167=CARTESIAN_POINT('Ctrl Pts',(4.03580121899994,5.2,0.371350974999984));
#346168=CARTESIAN_POINT('Ctrl Pts',(4.03580121899994,2.2,0.371350974999984));
#346169=CARTESIAN_POINT('Ctrl Pts',(4.03494436999994,12.2,0.371418534999983));
#346170=CARTESIAN_POINT('Ctrl Pts',(4.03494436999994,5.2,0.371418534999983));
#346171=CARTESIAN_POINT('Ctrl Pts',(4.03494436999994,2.2,0.371418534999983));
#346172=CARTESIAN_POINT('Ctrl Pts',(4.03409314899995,12.2,0.371484579999986));
#346173=CARTESIAN_POINT('Ctrl Pts',(4.03409314899995,5.2,0.371484579999986));
#346174=CARTESIAN_POINT('Ctrl Pts',(4.03409314899995,2.2,0.371484579999986));
#346175=CARTESIAN_POINT('Ctrl Pts',(4.03324756799995,12.2,0.371549123999984));
#346176=CARTESIAN_POINT('Ctrl Pts',(4.03324756799995,5.2,0.371549123999984));
#346177=CARTESIAN_POINT('Ctrl Pts',(4.03324756799995,2.2,0.371549123999984));
#346178=CARTESIAN_POINT('Ctrl Pts',(4.03240764099994,12.2,0.371612176999987));
#346179=CARTESIAN_POINT('Ctrl Pts',(4.03240764099994,5.2,0.371612176999987));
#346180=CARTESIAN_POINT('Ctrl Pts',(4.03240764099994,2.2,0.371612176999987));
#346181=CARTESIAN_POINT('Ctrl Pts',(4.03157337899995,12.2,0.371673753999988));
#346182=CARTESIAN_POINT('Ctrl Pts',(4.03157337899995,5.2,0.371673753999988));
#346183=CARTESIAN_POINT('Ctrl Pts',(4.03157337899995,2.2,0.371673753999988));
#346184=CARTESIAN_POINT('Ctrl Pts',(4.03074479599994,12.2,0.371733868999984));
#346185=CARTESIAN_POINT('Ctrl Pts',(4.03074479599994,5.2,0.371733868999984));
#346186=CARTESIAN_POINT('Ctrl Pts',(4.03074479599994,2.2,0.371733868999984));
#346187=CARTESIAN_POINT('Ctrl Pts',(4.02992190299994,12.2,0.371792531999984));
#346188=CARTESIAN_POINT('Ctrl Pts',(4.02992190299994,5.2,0.371792531999984));
#346189=CARTESIAN_POINT('Ctrl Pts',(4.02992190299994,2.2,0.371792531999984));
#346190=CARTESIAN_POINT('Ctrl Pts',(4.02910471299994,12.2,0.371849756999989));
#346191=CARTESIAN_POINT('Ctrl Pts',(4.02910471299994,5.2,0.371849756999989));
#346192=CARTESIAN_POINT('Ctrl Pts',(4.02910471299994,2.2,0.371849756999989));
#346193=CARTESIAN_POINT('Ctrl Pts',(4.02829323899994,12.2,0.371905558999988));
#346194=CARTESIAN_POINT('Ctrl Pts',(4.02829323899994,5.2,0.371905558999988));
#346195=CARTESIAN_POINT('Ctrl Pts',(4.02829323899994,2.2,0.371905558999988));
#346196=CARTESIAN_POINT('Ctrl Pts',(4.02748749399994,12.2,0.371959948999985));
#346197=CARTESIAN_POINT('Ctrl Pts',(4.02748749399994,5.2,0.371959948999985));
#346198=CARTESIAN_POINT('Ctrl Pts',(4.02748749399994,2.2,0.371959948999985));
#346199=CARTESIAN_POINT('Ctrl Pts',(4.02668748999994,12.2,0.372012940999986));
#346200=CARTESIAN_POINT('Ctrl Pts',(4.02668748999994,5.2,0.372012940999986));
#346201=CARTESIAN_POINT('Ctrl Pts',(4.02668748999994,2.2,0.372012940999986));
#346202=CARTESIAN_POINT('Ctrl Pts',(4.02589323899995,12.2,0.372064548999984));
#346203=CARTESIAN_POINT('Ctrl Pts',(4.02589323899995,5.2,0.372064548999984));
#346204=CARTESIAN_POINT('Ctrl Pts',(4.02589323899995,2.2,0.372064548999984));
#346205=CARTESIAN_POINT('Ctrl Pts',(4.02510475399994,12.2,0.372114783999984));
#346206=CARTESIAN_POINT('Ctrl Pts',(4.02510475399994,5.2,0.372114783999984));
#346207=CARTESIAN_POINT('Ctrl Pts',(4.02510475399994,2.2,0.372114783999984));
#346208=CARTESIAN_POINT('Ctrl Pts',(4.02432204899995,12.2,0.372163661999987));
#346209=CARTESIAN_POINT('Ctrl Pts',(4.02432204899995,5.2,0.372163661999987));
#346210=CARTESIAN_POINT('Ctrl Pts',(4.02432204899995,2.2,0.372163661999987));
#346211=CARTESIAN_POINT('Ctrl Pts',(4.02354513399994,12.2,0.372211193999985));
#346212=CARTESIAN_POINT('Ctrl Pts',(4.02354513399994,5.2,0.372211193999985));
#346213=CARTESIAN_POINT('Ctrl Pts',(4.02354513399994,2.2,0.372211193999985));
#346214=CARTESIAN_POINT('Ctrl Pts',(4.02277402399995,12.2,0.372257394999984));
#346215=CARTESIAN_POINT('Ctrl Pts',(4.02277402399995,5.2,0.372257394999984));
#346216=CARTESIAN_POINT('Ctrl Pts',(4.02277402399995,2.2,0.372257394999984));
#346217=CARTESIAN_POINT('Ctrl Pts',(4.02200873099994,12.2,0.372302277999985));
#346218=CARTESIAN_POINT('Ctrl Pts',(4.02200873099994,5.2,0.372302277999985));
#346219=CARTESIAN_POINT('Ctrl Pts',(4.02200873099994,2.2,0.372302277999985));
#346220=CARTESIAN_POINT('Ctrl Pts',(4.02124926799994,12.2,0.372345856999985));
#346221=CARTESIAN_POINT('Ctrl Pts',(4.02124926799994,5.2,0.372345856999985));
#346222=CARTESIAN_POINT('Ctrl Pts',(4.02124926799994,2.2,0.372345856999985));
#346223=CARTESIAN_POINT('Ctrl Pts',(4.02049564699994,12.2,0.372388144999984));
#346224=CARTESIAN_POINT('Ctrl Pts',(4.02049564699994,5.2,0.372388144999984));
#346225=CARTESIAN_POINT('Ctrl Pts',(4.02049564699994,2.2,0.372388144999984));
#346226=CARTESIAN_POINT('Ctrl Pts',(4.01974787999994,12.2,0.372429155999985));
#346227=CARTESIAN_POINT('Ctrl Pts',(4.01974787999994,5.2,0.372429155999985));
#346228=CARTESIAN_POINT('Ctrl Pts',(4.01974787999994,2.2,0.372429155999985));
#346229=CARTESIAN_POINT('Ctrl Pts',(4.01900598299994,12.2,0.372468902999987));
#346230=CARTESIAN_POINT('Ctrl Pts',(4.01900598299994,5.2,0.372468902999987));
#346231=CARTESIAN_POINT('Ctrl Pts',(4.01900598299994,2.2,0.372468902999987));
#346232=CARTESIAN_POINT('Ctrl Pts',(4.01826996599994,12.2,0.372507400999984));
#346233=CARTESIAN_POINT('Ctrl Pts',(4.01826996599994,5.2,0.372507400999984));
#346234=CARTESIAN_POINT('Ctrl Pts',(4.01826996599994,2.2,0.372507400999984));
#346235=CARTESIAN_POINT('Ctrl Pts',(4.01753984299994,12.2,0.372544663999985));
#346236=CARTESIAN_POINT('Ctrl Pts',(4.01753984299994,5.2,0.372544663999985));
#346237=CARTESIAN_POINT('Ctrl Pts',(4.01753984299994,2.2,0.372544663999985));
#346238=CARTESIAN_POINT('Ctrl Pts',(4.01681562499994,12.2,0.372580703999983));
#346239=CARTESIAN_POINT('Ctrl Pts',(4.01681562499994,5.2,0.372580703999983));
#346240=CARTESIAN_POINT('Ctrl Pts',(4.01681562499994,2.2,0.372580703999983));
#346241=CARTESIAN_POINT('Ctrl Pts',(4.01609732699994,12.2,0.372615535999987));
#346242=CARTESIAN_POINT('Ctrl Pts',(4.01609732699994,5.2,0.372615535999987));
#346243=CARTESIAN_POINT('Ctrl Pts',(4.01609732699994,2.2,0.372615535999987));
#346244=CARTESIAN_POINT('Ctrl Pts',(4.01538496099994,12.2,0.372649174999986));
#346245=CARTESIAN_POINT('Ctrl Pts',(4.01538496099994,5.2,0.372649174999986));
#346246=CARTESIAN_POINT('Ctrl Pts',(4.01538496099994,2.2,0.372649174999986));
#346247=CARTESIAN_POINT('Ctrl Pts',(4.01467854099994,12.2,0.372681631999985));
#346248=CARTESIAN_POINT('Ctrl Pts',(4.01467854099994,5.2,0.372681631999985));
#346249=CARTESIAN_POINT('Ctrl Pts',(4.01467854099994,2.2,0.372681631999985));
#346250=CARTESIAN_POINT('Ctrl Pts',(4.01397807799994,12.2,0.372712924999985));
#346251=CARTESIAN_POINT('Ctrl Pts',(4.01397807799994,5.2,0.372712924999985));
#346252=CARTESIAN_POINT('Ctrl Pts',(4.01397807799994,2.2,0.372712924999985));
#346253=CARTESIAN_POINT('Ctrl Pts',(4.01328358599994,12.2,0.372743064999987));
#346254=CARTESIAN_POINT('Ctrl Pts',(4.01328358599994,5.2,0.372743064999987));
#346255=CARTESIAN_POINT('Ctrl Pts',(4.01328358599994,2.2,0.372743064999987));
#346256=CARTESIAN_POINT('Ctrl Pts',(4.01259507899994,12.2,0.372772067999985));
#346257=CARTESIAN_POINT('Ctrl Pts',(4.01259507899994,5.2,0.372772067999985));
#346258=CARTESIAN_POINT('Ctrl Pts',(4.01259507899994,2.2,0.372772067999985));
#346259=CARTESIAN_POINT('Ctrl Pts',(4.01191256799994,12.2,0.372799947999987));
#346260=CARTESIAN_POINT('Ctrl Pts',(4.01191256799994,5.2,0.372799947999987));
#346261=CARTESIAN_POINT('Ctrl Pts',(4.01191256799994,2.2,0.372799947999987));
#346262=CARTESIAN_POINT('Ctrl Pts',(4.01123606699994,12.2,0.372826718999986));
#346263=CARTESIAN_POINT('Ctrl Pts',(4.01123606699994,5.2,0.372826718999986));
#346264=CARTESIAN_POINT('Ctrl Pts',(4.01123606699994,2.2,0.372826718999986));
#346265=CARTESIAN_POINT('Ctrl Pts',(4.01056558899994,12.2,0.372852395999987));
#346266=CARTESIAN_POINT('Ctrl Pts',(4.01056558899994,5.2,0.372852395999987));
#346267=CARTESIAN_POINT('Ctrl Pts',(4.01056558899994,2.2,0.372852395999987));
#346268=CARTESIAN_POINT('Ctrl Pts',(4.00990114699994,12.2,0.372876991999984));
#346269=CARTESIAN_POINT('Ctrl Pts',(4.00990114699994,5.2,0.372876991999984));
#346270=CARTESIAN_POINT('Ctrl Pts',(4.00990114699994,2.2,0.372876991999984));
#346271=CARTESIAN_POINT('Ctrl Pts',(4.00924275299994,12.2,0.372900522999986));
#346272=CARTESIAN_POINT('Ctrl Pts',(4.00924275299994,5.2,0.372900522999986));
#346273=CARTESIAN_POINT('Ctrl Pts',(4.00924275299994,2.2,0.372900522999986));
#346274=CARTESIAN_POINT('Ctrl Pts',(4.00859042199994,12.2,0.372923001999985));
#346275=CARTESIAN_POINT('Ctrl Pts',(4.00859042199994,5.2,0.372923001999985));
#346276=CARTESIAN_POINT('Ctrl Pts',(4.00859042199994,2.2,0.372923001999985));
#346277=CARTESIAN_POINT('Ctrl Pts',(4.00794416599994,12.2,0.372944444999987));
#346278=CARTESIAN_POINT('Ctrl Pts',(4.00794416599994,5.2,0.372944444999987));
#346279=CARTESIAN_POINT('Ctrl Pts',(4.00794416599994,2.2,0.372944444999987));
#346280=CARTESIAN_POINT('Ctrl Pts',(4.00730399899994,12.2,0.372964865999985));
#346281=CARTESIAN_POINT('Ctrl Pts',(4.00730399899994,5.2,0.372964865999985));
#346282=CARTESIAN_POINT('Ctrl Pts',(4.00730399899994,2.2,0.372964865999985));
#346283=CARTESIAN_POINT('Ctrl Pts',(4.00666993199995,12.2,0.372984279999984));
#346284=CARTESIAN_POINT('Ctrl Pts',(4.00666993199995,5.2,0.372984279999984));
#346285=CARTESIAN_POINT('Ctrl Pts',(4.00666993199995,2.2,0.372984279999984));
#346286=CARTESIAN_POINT('Ctrl Pts',(4.00604197999994,12.2,0.373002701999985));
#346287=CARTESIAN_POINT('Ctrl Pts',(4.00604197999994,5.2,0.373002701999985));
#346288=CARTESIAN_POINT('Ctrl Pts',(4.00604197999994,2.2,0.373002701999985));
#346289=CARTESIAN_POINT('Ctrl Pts',(4.00542015699994,12.2,0.373020146999985));
#346290=CARTESIAN_POINT('Ctrl Pts',(4.00542015699994,5.2,0.373020146999985));
#346291=CARTESIAN_POINT('Ctrl Pts',(4.00542015699994,2.2,0.373020146999985));
#346292=CARTESIAN_POINT('Ctrl Pts',(4.00480447399994,12.2,0.373036628999985));
#346293=CARTESIAN_POINT('Ctrl Pts',(4.00480447399994,5.2,0.373036628999985));
#346294=CARTESIAN_POINT('Ctrl Pts',(4.00480447399994,2.2,0.373036628999985));
#346295=CARTESIAN_POINT('Ctrl Pts',(4.00419494499994,12.2,0.373052163999983));
#346296=CARTESIAN_POINT('Ctrl Pts',(4.00419494499994,5.2,0.373052163999983));
#346297=CARTESIAN_POINT('Ctrl Pts',(4.00419494499994,2.2,0.373052163999983));
#346298=CARTESIAN_POINT('Ctrl Pts',(4.00359158399994,12.2,0.373066765999983));
#346299=CARTESIAN_POINT('Ctrl Pts',(4.00359158399994,5.2,0.373066765999983));
#346300=CARTESIAN_POINT('Ctrl Pts',(4.00359158399994,2.2,0.373066765999983));
#346301=CARTESIAN_POINT('Ctrl Pts',(4.00299440399994,12.2,0.373080450999983));
#346302=CARTESIAN_POINT('Ctrl Pts',(4.00299440399994,5.2,0.373080450999983));
#346303=CARTESIAN_POINT('Ctrl Pts',(4.00299440399994,2.2,0.373080450999983));
#346304=CARTESIAN_POINT('Ctrl Pts',(4.00240341799995,12.2,0.373093232999988));
#346305=CARTESIAN_POINT('Ctrl Pts',(4.00240341799995,5.2,0.373093232999988));
#346306=CARTESIAN_POINT('Ctrl Pts',(4.00240341799995,2.2,0.373093232999988));
#346307=CARTESIAN_POINT('Ctrl Pts',(4.00181863899994,12.2,0.373105127999986));
#346308=CARTESIAN_POINT('Ctrl Pts',(4.00181863899994,5.2,0.373105127999986));
#346309=CARTESIAN_POINT('Ctrl Pts',(4.00181863899994,2.2,0.373105127999986));
#346310=CARTESIAN_POINT('Ctrl Pts',(4.00124008099994,12.2,0.373116152999984));
#346311=CARTESIAN_POINT('Ctrl Pts',(4.00124008099994,5.2,0.373116152999984));
#346312=CARTESIAN_POINT('Ctrl Pts',(4.00124008099994,2.2,0.373116152999984));
#346313=CARTESIAN_POINT('Ctrl Pts',(4.00066775699994,12.2,0.373126319999986));
#346314=CARTESIAN_POINT('Ctrl Pts',(4.00066775699994,5.2,0.373126319999986));
#346315=CARTESIAN_POINT('Ctrl Pts',(4.00066775699994,2.2,0.373126319999986));
#346316=CARTESIAN_POINT('Ctrl Pts',(4.00010167999994,12.2,0.373135644999985));
#346317=CARTESIAN_POINT('Ctrl Pts',(4.00010167999994,5.2,0.373135644999985));
#346318=CARTESIAN_POINT('Ctrl Pts',(4.00010167999994,2.2,0.373135644999985));
#346319=CARTESIAN_POINT('Ctrl Pts',(3.99954186399994,12.2,0.373144146999986));
#346320=CARTESIAN_POINT('Ctrl Pts',(3.99954186399994,5.2,0.373144146999986));
#346321=CARTESIAN_POINT('Ctrl Pts',(3.99954186399994,2.2,0.373144146999986));
#346322=CARTESIAN_POINT('Ctrl Pts',(3.99898832299994,12.2,0.373151836999988));
#346323=CARTESIAN_POINT('Ctrl Pts',(3.99898832299994,5.2,0.373151836999988));
#346324=CARTESIAN_POINT('Ctrl Pts',(3.99898832299994,2.2,0.373151836999988));
#346325=CARTESIAN_POINT('Ctrl Pts',(3.99844106899994,12.2,0.373158732999985));
#346326=CARTESIAN_POINT('Ctrl Pts',(3.99844106899994,5.2,0.373158732999985));
#346327=CARTESIAN_POINT('Ctrl Pts',(3.99844106899994,2.2,0.373158732999985));
#346328=CARTESIAN_POINT('Ctrl Pts',(3.99790011699994,12.2,0.373164850999985));
#346329=CARTESIAN_POINT('Ctrl Pts',(3.99790011699994,5.2,0.373164850999985));
#346330=CARTESIAN_POINT('Ctrl Pts',(3.99790011699994,2.2,0.373164850999985));
#346331=CARTESIAN_POINT('Ctrl Pts',(3.99736547899994,12.2,0.373170204999984));
#346332=CARTESIAN_POINT('Ctrl Pts',(3.99736547899994,5.2,0.373170204999984));
#346333=CARTESIAN_POINT('Ctrl Pts',(3.99736547899994,2.2,0.373170204999984));
#346334=CARTESIAN_POINT('Ctrl Pts',(3.99683716899994,12.2,0.373174810999988));
#346335=CARTESIAN_POINT('Ctrl Pts',(3.99683716899994,5.2,0.373174810999988));
#346336=CARTESIAN_POINT('Ctrl Pts',(3.99683716899994,2.2,0.373174810999988));
#346337=CARTESIAN_POINT('Ctrl Pts',(3.99631520299994,12.2,0.373178685999989));
#346338=CARTESIAN_POINT('Ctrl Pts',(3.99631520299994,5.2,0.373178685999989));
#346339=CARTESIAN_POINT('Ctrl Pts',(3.99631520299994,2.2,0.373178685999989));
#346340=CARTESIAN_POINT('Ctrl Pts',(3.99579958899994,12.2,0.373181846999984));
#346341=CARTESIAN_POINT('Ctrl Pts',(3.99579958899994,5.2,0.373181846999984));
#346342=CARTESIAN_POINT('Ctrl Pts',(3.99579958899994,2.2,0.373181846999984));
#346343=CARTESIAN_POINT('Ctrl Pts',(3.99529034599994,12.2,0.373184306999987));
#346344=CARTESIAN_POINT('Ctrl Pts',(3.99529034599994,5.2,0.373184306999987));
#346345=CARTESIAN_POINT('Ctrl Pts',(3.99529034599994,2.2,0.373184306999987));
#346346=CARTESIAN_POINT('Ctrl Pts',(3.99478748599994,12.2,0.373186083999983));
#346347=CARTESIAN_POINT('Ctrl Pts',(3.99478748599994,5.2,0.373186083999983));
#346348=CARTESIAN_POINT('Ctrl Pts',(3.99478748599994,2.2,0.373186083999983));
#346349=CARTESIAN_POINT('Ctrl Pts',(3.99429102099994,12.2,0.373187192999982));
#346350=CARTESIAN_POINT('Ctrl Pts',(3.99429102099994,5.2,0.373187192999982));
#346351=CARTESIAN_POINT('Ctrl Pts',(3.99429102099994,2.2,0.373187192999982));
#346352=CARTESIAN_POINT('Ctrl Pts',(3.99380096699994,12.2,0.373187650999984));
#346353=CARTESIAN_POINT('Ctrl Pts',(3.99380096699994,5.2,0.373187650999984));
#346354=CARTESIAN_POINT('Ctrl Pts',(3.99380096699994,2.2,0.373187650999984));
#346355=CARTESIAN_POINT('Ctrl Pts',(3.99331733399995,12.2,0.373187473999987));
#346356=CARTESIAN_POINT('Ctrl Pts',(3.99331733399995,5.2,0.373187473999987));
#346357=CARTESIAN_POINT('Ctrl Pts',(3.99331733399995,2.2,0.373187473999987));
#346358=CARTESIAN_POINT('Ctrl Pts',(3.99284013999994,12.2,0.373186677999984));
#346359=CARTESIAN_POINT('Ctrl Pts',(3.99284013999994,5.2,0.373186677999984));
#346360=CARTESIAN_POINT('Ctrl Pts',(3.99284013999994,2.2,0.373186677999984));
#346361=CARTESIAN_POINT('Ctrl Pts',(3.99236939699994,12.2,0.373185279999984));
#346362=CARTESIAN_POINT('Ctrl Pts',(3.99236939699994,5.2,0.373185279999984));
#346363=CARTESIAN_POINT('Ctrl Pts',(3.99236939699994,2.2,0.373185279999984));
#346364=CARTESIAN_POINT('Ctrl Pts',(3.99190511899994,12.2,0.373183295999984));
#346365=CARTESIAN_POINT('Ctrl Pts',(3.99190511899994,5.2,0.373183295999984));
#346366=CARTESIAN_POINT('Ctrl Pts',(3.99190511899994,2.2,0.373183295999984));
#346367=CARTESIAN_POINT('Ctrl Pts',(3.99144731899994,12.2,0.373180742999986));
#346368=CARTESIAN_POINT('Ctrl Pts',(3.99144731899994,5.2,0.373180742999986));
#346369=CARTESIAN_POINT('Ctrl Pts',(3.99144731899994,2.2,0.373180742999986));
#346370=CARTESIAN_POINT('Ctrl Pts',(3.99099601199994,12.2,0.373177636999986));
#346371=CARTESIAN_POINT('Ctrl Pts',(3.99099601199994,5.2,0.373177636999986));
#346372=CARTESIAN_POINT('Ctrl Pts',(3.99099601199994,2.2,0.373177636999986));
#346373=CARTESIAN_POINT('Ctrl Pts',(3.99055120999994,12.2,0.373173994999987));
#346374=CARTESIAN_POINT('Ctrl Pts',(3.99055120999994,5.2,0.373173994999987));
#346375=CARTESIAN_POINT('Ctrl Pts',(3.99055120999994,2.2,0.373173994999987));
#346376=CARTESIAN_POINT('Ctrl Pts',(3.99011292899994,12.2,0.373169832999984));
#346377=CARTESIAN_POINT('Ctrl Pts',(3.99011292899994,5.2,0.373169832999984));
#346378=CARTESIAN_POINT('Ctrl Pts',(3.99011292899994,2.2,0.373169832999984));
#346379=CARTESIAN_POINT('Ctrl Pts',(3.98968118199994,12.2,0.373165167999985));
#346380=CARTESIAN_POINT('Ctrl Pts',(3.98968118199994,5.2,0.373165167999985));
#346381=CARTESIAN_POINT('Ctrl Pts',(3.98968118199994,2.2,0.373165167999985));
#346382=CARTESIAN_POINT('Ctrl Pts',(3.98925598199994,12.2,0.373160018999985));
#346383=CARTESIAN_POINT('Ctrl Pts',(3.98925598199994,5.2,0.373160018999985));
#346384=CARTESIAN_POINT('Ctrl Pts',(3.98925598199994,2.2,0.373160018999985));
#346385=CARTESIAN_POINT('Ctrl Pts',(3.98883734399994,12.2,0.373154398999986));
#346386=CARTESIAN_POINT('Ctrl Pts',(3.98883734399994,5.2,0.373154398999986));
#346387=CARTESIAN_POINT('Ctrl Pts',(3.98883734399994,2.2,0.373154398999986));
#346388=CARTESIAN_POINT('Ctrl Pts',(3.98842528099994,12.2,0.373148327999986));
#346389=CARTESIAN_POINT('Ctrl Pts',(3.98842528099994,5.2,0.373148327999986));
#346390=CARTESIAN_POINT('Ctrl Pts',(3.98842528099994,2.2,0.373148327999986));
#346391=CARTESIAN_POINT('Ctrl Pts',(3.98801980899994,12.2,0.373141822999985));
#346392=CARTESIAN_POINT('Ctrl Pts',(3.98801980899994,5.2,0.373141822999985));
#346393=CARTESIAN_POINT('Ctrl Pts',(3.98801980899994,2.2,0.373141822999985));
#346394=CARTESIAN_POINT('Ctrl Pts',(3.98762093899994,12.2,0.373134899999985));
#346395=CARTESIAN_POINT('Ctrl Pts',(3.98762093899994,5.2,0.373134899999985));
#346396=CARTESIAN_POINT('Ctrl Pts',(3.98762093899994,2.2,0.373134899999985));
#346397=CARTESIAN_POINT('Ctrl Pts',(3.98722868799994,12.2,0.373127575999987));
#346398=CARTESIAN_POINT('Ctrl Pts',(3.98722868799994,5.2,0.373127575999987));
#346399=CARTESIAN_POINT('Ctrl Pts',(3.98722868799994,2.2,0.373127575999987));
#346400=CARTESIAN_POINT('Ctrl Pts',(3.98684306899994,12.2,0.373119868999985));
#346401=CARTESIAN_POINT('Ctrl Pts',(3.98684306899994,5.2,0.373119868999985));
#346402=CARTESIAN_POINT('Ctrl Pts',(3.98684306899994,2.2,0.373119868999985));
#346403=CARTESIAN_POINT('Ctrl Pts',(3.98646409499994,12.2,0.373111795999983));
#346404=CARTESIAN_POINT('Ctrl Pts',(3.98646409499994,5.2,0.373111795999983));
#346405=CARTESIAN_POINT('Ctrl Pts',(3.98646409499994,2.2,0.373111795999983));
#346406=CARTESIAN_POINT('Ctrl Pts',(3.98609178199994,12.2,0.373103375999988));
#346407=CARTESIAN_POINT('Ctrl Pts',(3.98609178199994,5.2,0.373103375999988));
#346408=CARTESIAN_POINT('Ctrl Pts',(3.98609178199994,2.2,0.373103375999988));
#346409=CARTESIAN_POINT('Ctrl Pts',(3.98572614199994,12.2,0.373094623999983));
#346410=CARTESIAN_POINT('Ctrl Pts',(3.98572614199994,5.2,0.373094623999983));
#346411=CARTESIAN_POINT('Ctrl Pts',(3.98572614199994,2.2,0.373094623999983));
#346412=CARTESIAN_POINT('Ctrl Pts',(3.98536718999994,12.2,0.373085557999988));
#346413=CARTESIAN_POINT('Ctrl Pts',(3.98536718999994,5.2,0.373085557999988));
#346414=CARTESIAN_POINT('Ctrl Pts',(3.98536718999994,2.2,0.373085557999988));
#346415=CARTESIAN_POINT('Ctrl Pts',(3.98501494199994,12.2,0.373076197999986));
#346416=CARTESIAN_POINT('Ctrl Pts',(3.98501494199994,5.2,0.373076197999986));
#346417=CARTESIAN_POINT('Ctrl Pts',(3.98501494199994,2.2,0.373076197999986));
#346418=CARTESIAN_POINT('Ctrl Pts',(3.98466940899994,12.2,0.373066557999984));
#346419=CARTESIAN_POINT('Ctrl Pts',(3.98466940899994,5.2,0.373066557999984));
#346420=CARTESIAN_POINT('Ctrl Pts',(3.98466940899994,2.2,0.373066557999984));
#346421=CARTESIAN_POINT('Ctrl Pts',(3.98433060799994,12.2,0.373056658999986));
#346422=CARTESIAN_POINT('Ctrl Pts',(3.98433060799994,5.2,0.373056658999986));
#346423=CARTESIAN_POINT('Ctrl Pts',(3.98433060799994,2.2,0.373056658999986));
#346424=CARTESIAN_POINT('Ctrl Pts',(3.98399855199994,12.2,0.373046518999987));
#346425=CARTESIAN_POINT('Ctrl Pts',(3.98399855199994,5.2,0.373046518999987));
#346426=CARTESIAN_POINT('Ctrl Pts',(3.98399855199994,2.2,0.373046518999987));
#346427=CARTESIAN_POINT('Ctrl Pts',(3.98367325499994,12.2,0.373036153999986));
#346428=CARTESIAN_POINT('Ctrl Pts',(3.98367325499994,5.2,0.373036153999986));
#346429=CARTESIAN_POINT('Ctrl Pts',(3.98367325499994,2.2,0.373036153999986));
#346430=CARTESIAN_POINT('Ctrl Pts',(3.98335473199994,12.2,0.373025581999986));
#346431=CARTESIAN_POINT('Ctrl Pts',(3.98335473199994,5.2,0.373025581999986));
#346432=CARTESIAN_POINT('Ctrl Pts',(3.98335473199994,2.2,0.373025581999986));
#346433=CARTESIAN_POINT('Ctrl Pts',(3.98304299799995,12.2,0.373014822999984));
#346434=CARTESIAN_POINT('Ctrl Pts',(3.98304299799995,5.2,0.373014822999984));
#346435=CARTESIAN_POINT('Ctrl Pts',(3.98304299799995,2.2,0.373014822999984));
#346436=CARTESIAN_POINT('Ctrl Pts',(3.98273806599994,12.2,0.373003892999986));
#346437=CARTESIAN_POINT('Ctrl Pts',(3.98273806599994,5.2,0.373003892999986));
#346438=CARTESIAN_POINT('Ctrl Pts',(3.98273806599994,2.2,0.373003892999986));
#346439=CARTESIAN_POINT('Ctrl Pts',(3.98243995099994,12.2,0.372992811999988));
#346440=CARTESIAN_POINT('Ctrl Pts',(3.98243995099994,5.2,0.372992811999988));
#346441=CARTESIAN_POINT('Ctrl Pts',(3.98243995099994,2.2,0.372992811999988));
#346442=CARTESIAN_POINT('Ctrl Pts',(3.98214866699994,12.2,0.372981597999988));
#346443=CARTESIAN_POINT('Ctrl Pts',(3.98214866699994,5.2,0.372981597999988));
#346444=CARTESIAN_POINT('Ctrl Pts',(3.98214866699994,2.2,0.372981597999988));
#346445=CARTESIAN_POINT('Ctrl Pts',(3.98186422899994,12.2,0.372970267999988));
#346446=CARTESIAN_POINT('Ctrl Pts',(3.98186422899994,5.2,0.372970267999988));
#346447=CARTESIAN_POINT('Ctrl Pts',(3.98186422899994,2.2,0.372970267999988));
#346448=CARTESIAN_POINT('Ctrl Pts',(3.98158665199994,12.2,0.372958841999989));
#346449=CARTESIAN_POINT('Ctrl Pts',(3.98158665199994,5.2,0.372958841999989));
#346450=CARTESIAN_POINT('Ctrl Pts',(3.98158665199994,2.2,0.372958841999989));
#346451=CARTESIAN_POINT('Ctrl Pts',(3.98131594999994,12.2,0.372947338999987));
#346452=CARTESIAN_POINT('Ctrl Pts',(3.98131594999994,5.2,0.372947338999987));
#346453=CARTESIAN_POINT('Ctrl Pts',(3.98131594999994,2.2,0.372947338999987));
#346454=CARTESIAN_POINT('Ctrl Pts',(3.98105213699994,12.2,0.372935775999985));
#346455=CARTESIAN_POINT('Ctrl Pts',(3.98105213699994,5.2,0.372935775999985));
#346456=CARTESIAN_POINT('Ctrl Pts',(3.98105213699994,2.2,0.372935775999985));
#346457=CARTESIAN_POINT('Ctrl Pts',(3.98079522899994,12.2,0.372924173999984));
#346458=CARTESIAN_POINT('Ctrl Pts',(3.98079522899994,5.2,0.372924173999984));
#346459=CARTESIAN_POINT('Ctrl Pts',(3.98079522899994,2.2,0.372924173999984));
#346460=CARTESIAN_POINT('Ctrl Pts',(3.98054523899994,12.2,0.372912548999986));
#346461=CARTESIAN_POINT('Ctrl Pts',(3.98054523899994,5.2,0.372912548999986));
#346462=CARTESIAN_POINT('Ctrl Pts',(3.98054523899994,2.2,0.372912548999986));
#346463=CARTESIAN_POINT('Ctrl Pts',(3.98030218199994,12.2,0.372900921999988));
#346464=CARTESIAN_POINT('Ctrl Pts',(3.98030218199994,5.2,0.372900921999988));
#346465=CARTESIAN_POINT('Ctrl Pts',(3.98030218199994,2.2,0.372900921999988));
#346466=CARTESIAN_POINT('Ctrl Pts',(3.98006607399994,12.2,0.372889311999987));
#346467=CARTESIAN_POINT('Ctrl Pts',(3.98006607399994,5.2,0.372889311999987));
#346468=CARTESIAN_POINT('Ctrl Pts',(3.98006607399994,2.2,0.372889311999987));
#346469=CARTESIAN_POINT('Ctrl Pts',(3.97983692799994,12.2,0.372877735999988));
#346470=CARTESIAN_POINT('Ctrl Pts',(3.97983692799994,5.2,0.372877735999988));
#346471=CARTESIAN_POINT('Ctrl Pts',(3.97983692799994,2.2,0.372877735999988));
#346472=CARTESIAN_POINT('Ctrl Pts',(3.97961475899994,12.2,0.372866213999985));
#346473=CARTESIAN_POINT('Ctrl Pts',(3.97961475899994,5.2,0.372866213999985));
#346474=CARTESIAN_POINT('Ctrl Pts',(3.97961475899994,2.2,0.372866213999985));
#346475=CARTESIAN_POINT('Ctrl Pts',(3.97939958299994,12.2,0.372854766999984));
#346476=CARTESIAN_POINT('Ctrl Pts',(3.97939958299994,5.2,0.372854766999984));
#346477=CARTESIAN_POINT('Ctrl Pts',(3.97939958299994,2.2,0.372854766999984));
#346478=CARTESIAN_POINT('Ctrl Pts',(3.97919141399994,12.2,0.372843411999986));
#346479=CARTESIAN_POINT('Ctrl Pts',(3.97919141399994,5.2,0.372843411999986));
#346480=CARTESIAN_POINT('Ctrl Pts',(3.97919141399994,2.2,0.372843411999986));
#346481=CARTESIAN_POINT('Ctrl Pts',(3.97899026699994,12.2,0.372832170999988));
#346482=CARTESIAN_POINT('Ctrl Pts',(3.97899026699994,5.2,0.372832170999988));
#346483=CARTESIAN_POINT('Ctrl Pts',(3.97899026699994,2.2,0.372832170999988));
#346484=CARTESIAN_POINT('Ctrl Pts',(3.97879615699994,12.2,0.372821060999984));
#346485=CARTESIAN_POINT('Ctrl Pts',(3.97879615699994,5.2,0.372821060999984));
#346486=CARTESIAN_POINT('Ctrl Pts',(3.97879615699994,2.2,0.372821060999984));
#346487=CARTESIAN_POINT('Ctrl Pts',(3.97860909799994,12.2,0.372810104999988));
#346488=CARTESIAN_POINT('Ctrl Pts',(3.97860909799994,5.2,0.372810104999988));
#346489=CARTESIAN_POINT('Ctrl Pts',(3.97860909799994,2.2,0.372810104999988));
#346490=CARTESIAN_POINT('Ctrl Pts',(3.97842910699994,12.2,0.372799318999988));
#346491=CARTESIAN_POINT('Ctrl Pts',(3.97842910699994,5.2,0.372799318999988));
#346492=CARTESIAN_POINT('Ctrl Pts',(3.97842910699994,2.2,0.372799318999988));
#346493=CARTESIAN_POINT('Ctrl Pts',(3.97825619699994,12.2,0.372788722999986));
#346494=CARTESIAN_POINT('Ctrl Pts',(3.97825619699994,5.2,0.372788722999986));
#346495=CARTESIAN_POINT('Ctrl Pts',(3.97825619699994,2.2,0.372788722999986));
#346496=CARTESIAN_POINT('Ctrl Pts',(3.97809038299994,12.2,0.372778337999984));
#346497=CARTESIAN_POINT('Ctrl Pts',(3.97809038299994,5.2,0.372778337999984));
#346498=CARTESIAN_POINT('Ctrl Pts',(3.97809038299994,2.2,0.372778337999984));
#346499=CARTESIAN_POINT('Ctrl Pts',(3.97793167899994,12.2,0.372768182999987));
#346500=CARTESIAN_POINT('Ctrl Pts',(3.97793167899994,5.2,0.372768182999987));
#346501=CARTESIAN_POINT('Ctrl Pts',(3.97793167899994,2.2,0.372768182999987));
#346502=CARTESIAN_POINT('Ctrl Pts',(3.97778010099994,12.2,0.372758277999985));
#346503=CARTESIAN_POINT('Ctrl Pts',(3.97778010099994,5.2,0.372758277999985));
#346504=CARTESIAN_POINT('Ctrl Pts',(3.97778010099994,2.2,0.372758277999985));
#346505=CARTESIAN_POINT('Ctrl Pts',(3.97763566599994,12.2,0.372748643999987));
#346506=CARTESIAN_POINT('Ctrl Pts',(3.97763566599994,5.2,0.372748643999987));
#346507=CARTESIAN_POINT('Ctrl Pts',(3.97763566599994,2.2,0.372748643999987));
#346508=CARTESIAN_POINT('Ctrl Pts',(3.97749838899994,12.2,0.372739301999987));
#346509=CARTESIAN_POINT('Ctrl Pts',(3.97749838899994,5.2,0.372739301999987));
#346510=CARTESIAN_POINT('Ctrl Pts',(3.97749838899994,2.2,0.372739301999987));
#346511=CARTESIAN_POINT('Ctrl Pts',(3.97736828499994,12.2,0.372730274999986));
#346512=CARTESIAN_POINT('Ctrl Pts',(3.97736828499994,5.2,0.372730274999986));
#346513=CARTESIAN_POINT('Ctrl Pts',(3.97736828499994,2.2,0.372730274999986));
#346514=CARTESIAN_POINT('Ctrl Pts',(3.97724536999994,12.2,0.372721580999986));
#346515=CARTESIAN_POINT('Ctrl Pts',(3.97724536999994,5.2,0.372721580999986));
#346516=CARTESIAN_POINT('Ctrl Pts',(3.97724536999994,2.2,0.372721580999986));
#346517=CARTESIAN_POINT('Ctrl Pts',(3.97712965699994,12.2,0.372713236999989));
#346518=CARTESIAN_POINT('Ctrl Pts',(3.97712965699994,5.2,0.372713236999989));
#346519=CARTESIAN_POINT('Ctrl Pts',(3.97712965699994,2.2,0.372713236999989));
#346520=CARTESIAN_POINT('Ctrl Pts',(3.97702115899994,12.2,0.372705264999986));
#346521=CARTESIAN_POINT('Ctrl Pts',(3.97702115899994,5.2,0.372705264999986));
#346522=CARTESIAN_POINT('Ctrl Pts',(3.97702115899994,2.2,0.372705264999986));
#346523=CARTESIAN_POINT('Ctrl Pts',(3.97691989099994,12.2,0.372697680999985));
#346524=CARTESIAN_POINT('Ctrl Pts',(3.97691989099994,5.2,0.372697680999985));
#346525=CARTESIAN_POINT('Ctrl Pts',(3.97691989099994,2.2,0.372697680999985));
#346526=CARTESIAN_POINT('Ctrl Pts',(3.97682586699994,12.2,0.372690505999986));
#346527=CARTESIAN_POINT('Ctrl Pts',(3.97682586699994,5.2,0.372690505999986));
#346528=CARTESIAN_POINT('Ctrl Pts',(3.97682586699994,2.2,0.372690505999986));
#346529=CARTESIAN_POINT('Ctrl Pts',(3.97673910699994,12.2,0.372683765999984));
#346530=CARTESIAN_POINT('Ctrl Pts',(3.97673910699994,5.2,0.372683765999984));
#346531=CARTESIAN_POINT('Ctrl Pts',(3.97673910699994,2.2,0.372683765999984));
#346532=CARTESIAN_POINT('Ctrl Pts',(3.97665962899994,12.2,0.372677485999984));
#346533=CARTESIAN_POINT('Ctrl Pts',(3.97665962899994,5.2,0.372677485999984));
#346534=CARTESIAN_POINT('Ctrl Pts',(3.97665962899994,2.2,0.372677485999984));
#346535=CARTESIAN_POINT('Ctrl Pts',(3.97658745199994,12.2,0.372671693999984));
#346536=CARTESIAN_POINT('Ctrl Pts',(3.97658745199994,5.2,0.372671693999984));
#346537=CARTESIAN_POINT('Ctrl Pts',(3.97658745199994,2.2,0.372671693999984));
#346538=CARTESIAN_POINT('Ctrl Pts',(3.97652259499994,12.2,0.372666410999987));
#346539=CARTESIAN_POINT('Ctrl Pts',(3.97652259499994,5.2,0.372666410999987));
#346540=CARTESIAN_POINT('Ctrl Pts',(3.97652259499994,2.2,0.372666410999987));
#346541=CARTESIAN_POINT('Ctrl Pts',(3.97646506799994,12.2,0.372661654999984));
#346542=CARTESIAN_POINT('Ctrl Pts',(3.97646506799994,5.2,0.372661654999984));
#346543=CARTESIAN_POINT('Ctrl Pts',(3.97646506799994,2.2,0.372661654999984));
#346544=CARTESIAN_POINT('Ctrl Pts',(3.97640950604921,12.2,0.372656984337683));
#346545=CARTESIAN_POINT('Ctrl Pts',(3.97640950604921,5.2,0.372656984337683));
#346546=CARTESIAN_POINT('Ctrl Pts',(3.97640950604921,2.2,0.372656984337683));
#346547=CARTESIAN_POINT('Ctrl Pts',(3.97637153472191,12.2,0.372653714372708));
#346548=CARTESIAN_POINT('Ctrl Pts',(3.97637153472191,5.2,0.372653714372708));
#346549=CARTESIAN_POINT('Ctrl Pts',(3.97637153472191,2.2,0.372653714372708));
#346550=CARTESIAN_POINT('Ctrl Pts',(3.97634652385127,12.2,0.372651508425408));
#346551=CARTESIAN_POINT('Ctrl Pts',(3.97634652385127,5.2,0.372651508425408));
#346552=CARTESIAN_POINT('Ctrl Pts',(3.97634652385127,2.2,0.372651508425408));
#346553=CARTESIAN_POINT('Ctrl Pts',(3.97633094703549,12.2,0.372650094949822));
#346554=CARTESIAN_POINT('Ctrl Pts',(3.97633094703549,5.2,0.372650094949822));
#346555=CARTESIAN_POINT('Ctrl Pts',(3.97633094703549,2.2,0.372650094949822));
#346556=CARTESIAN_POINT('Ctrl Pts',(3.97632132799994,12.2,0.372649231999986));
#346557=CARTESIAN_POINT('Ctrl Pts',(3.97632132799994,5.2,0.372649231999986));
#346558=CARTESIAN_POINT('Ctrl Pts',(3.97632132799994,2.2,0.372649231999986));
#346559=CARTESIAN_POINT('',(4.74889012999994,12.2,0.102676828999986));
#346560=CARTESIAN_POINT('Origin',(-5.66300478732629E-14,15.2,-1.77635683940025E-14));
#346561=CARTESIAN_POINT('',(4.74421990499994,12.2,-0.234259451000014));
#346562=CARTESIAN_POINT('Ctrl Pts',(3.96444825599994,12.2,-0.482713322000015));
#346563=CARTESIAN_POINT('Ctrl Pts',(3.96444825599994,5.2,-0.482713322000015));
#346564=CARTESIAN_POINT('Ctrl Pts',(3.96444825599994,2.2,-0.482713322000015));
#346565=CARTESIAN_POINT('Ctrl Pts',(3.9644550525987,12.2,-0.482714122952763));
#346566=CARTESIAN_POINT('Ctrl Pts',(3.9644550525987,5.2,-0.482714122952763));
#346567=CARTESIAN_POINT('Ctrl Pts',(3.9644550525987,2.2,-0.482714122952763));
#346568=CARTESIAN_POINT('Ctrl Pts',(3.96446819348808,12.2,-0.482715670305005));
#346569=CARTESIAN_POINT('Ctrl Pts',(3.96446819348808,5.2,-0.482715670305005));
#346570=CARTESIAN_POINT('Ctrl Pts',(3.96446819348808,2.2,-0.482715670305005));
#346571=CARTESIAN_POINT('Ctrl Pts',(3.9644876922665,12.2,-0.482717970545998));
#346572=CARTESIAN_POINT('Ctrl Pts',(3.9644876922665,5.2,-0.482717970545998));
#346573=CARTESIAN_POINT('Ctrl Pts',(3.9644876922665,2.2,-0.482717970545998));
#346574=CARTESIAN_POINT('Ctrl Pts',(3.96451349997268,12.2,-0.482721030842654));
#346575=CARTESIAN_POINT('Ctrl Pts',(3.96451349997268,5.2,-0.482721030842654));
#346576=CARTESIAN_POINT('Ctrl Pts',(3.96451349997268,2.2,-0.482721030842654));
#346577=CARTESIAN_POINT('Ctrl Pts',(3.96455853299994,12.2,-0.482726117000016));
#346578=CARTESIAN_POINT('Ctrl Pts',(3.96455853299994,5.2,-0.482726117000016));
#346579=CARTESIAN_POINT('Ctrl Pts',(3.96455853299994,2.2,-0.482726117000016));
#346580=CARTESIAN_POINT('Ctrl Pts',(3.96460858399994,12.2,-0.482731726000014));
#346581=CARTESIAN_POINT('Ctrl Pts',(3.96460858399994,5.2,-0.482731726000014));
#346582=CARTESIAN_POINT('Ctrl Pts',(3.96460858399994,2.2,-0.482731726000014));
#346583=CARTESIAN_POINT('Ctrl Pts',(3.96466595699994,12.2,-0.482738075000011));
#346584=CARTESIAN_POINT('Ctrl Pts',(3.96466595699994,5.2,-0.482738075000011));
#346585=CARTESIAN_POINT('Ctrl Pts',(3.96466595699994,2.2,-0.482738075000011));
#346586=CARTESIAN_POINT('Ctrl Pts',(3.96473064299994,12.2,-0.482745154000015));
#346587=CARTESIAN_POINT('Ctrl Pts',(3.96473064299994,5.2,-0.482745154000015));
#346588=CARTESIAN_POINT('Ctrl Pts',(3.96473064299994,2.2,-0.482745154000015));
#346589=CARTESIAN_POINT('Ctrl Pts',(3.96480263099994,12.2,-0.482752944000016));
#346590=CARTESIAN_POINT('Ctrl Pts',(3.96480263099994,5.2,-0.482752944000016));
#346591=CARTESIAN_POINT('Ctrl Pts',(3.96480263099994,2.2,-0.482752944000016));
#346592=CARTESIAN_POINT('Ctrl Pts',(3.96488190499994,12.2,-0.482761424000016));
#346593=CARTESIAN_POINT('Ctrl Pts',(3.96488190499994,5.2,-0.482761424000016));
#346594=CARTESIAN_POINT('Ctrl Pts',(3.96488190499994,2.2,-0.482761424000016));
#346595=CARTESIAN_POINT('Ctrl Pts',(3.96496844499994,12.2,-0.482770567000017));
#346596=CARTESIAN_POINT('Ctrl Pts',(3.96496844499994,5.2,-0.482770567000017));
#346597=CARTESIAN_POINT('Ctrl Pts',(3.96496844499994,2.2,-0.482770567000017));
#346598=CARTESIAN_POINT('Ctrl Pts',(3.96506223299994,12.2,-0.482780345000013));
#346599=CARTESIAN_POINT('Ctrl Pts',(3.96506223299994,5.2,-0.482780345000013));
#346600=CARTESIAN_POINT('Ctrl Pts',(3.96506223299994,2.2,-0.482780345000013));
#346601=CARTESIAN_POINT('Ctrl Pts',(3.96516325199994,12.2,-0.482790732000016));
#346602=CARTESIAN_POINT('Ctrl Pts',(3.96516325199994,5.2,-0.482790732000016));
#346603=CARTESIAN_POINT('Ctrl Pts',(3.96516325199994,2.2,-0.482790732000016));
#346604=CARTESIAN_POINT('Ctrl Pts',(3.96527148799994,12.2,-0.482801710000014));
#346605=CARTESIAN_POINT('Ctrl Pts',(3.96527148799994,5.2,-0.482801710000014));
#346606=CARTESIAN_POINT('Ctrl Pts',(3.96527148799994,2.2,-0.482801710000014));
#346607=CARTESIAN_POINT('Ctrl Pts',(3.96538692599994,12.2,-0.482813256000014));
#346608=CARTESIAN_POINT('Ctrl Pts',(3.96538692599994,5.2,-0.482813256000014));
#346609=CARTESIAN_POINT('Ctrl Pts',(3.96538692599994,2.2,-0.482813256000014));
#346610=CARTESIAN_POINT('Ctrl Pts',(3.96550955299994,12.2,-0.482825354000016));
#346611=CARTESIAN_POINT('Ctrl Pts',(3.96550955299994,5.2,-0.482825354000016));
#346612=CARTESIAN_POINT('Ctrl Pts',(3.96550955299994,2.2,-0.482825354000016));
#346613=CARTESIAN_POINT('Ctrl Pts',(3.96563935599994,12.2,-0.482837984000017));
#346614=CARTESIAN_POINT('Ctrl Pts',(3.96563935599994,5.2,-0.482837984000017));
#346615=CARTESIAN_POINT('Ctrl Pts',(3.96563935599994,2.2,-0.482837984000017));
#346616=CARTESIAN_POINT('Ctrl Pts',(3.96577632199994,12.2,-0.482851127000017));
#346617=CARTESIAN_POINT('Ctrl Pts',(3.96577632199994,5.2,-0.482851127000017));
#346618=CARTESIAN_POINT('Ctrl Pts',(3.96577632199994,2.2,-0.482851127000017));
#346619=CARTESIAN_POINT('Ctrl Pts',(3.96592043499994,12.2,-0.482864759000012));
#346620=CARTESIAN_POINT('Ctrl Pts',(3.96592043499994,5.2,-0.482864759000012));
#346621=CARTESIAN_POINT('Ctrl Pts',(3.96592043499994,2.2,-0.482864759000012));
#346622=CARTESIAN_POINT('Ctrl Pts',(3.96607167899994,12.2,-0.482878862000016));
#346623=CARTESIAN_POINT('Ctrl Pts',(3.96607167899994,5.2,-0.482878862000016));
#346624=CARTESIAN_POINT('Ctrl Pts',(3.96607167899994,2.2,-0.482878862000016));
#346625=CARTESIAN_POINT('Ctrl Pts',(3.96623003999994,12.2,-0.482893412000016));
#346626=CARTESIAN_POINT('Ctrl Pts',(3.96623003999994,5.2,-0.482893412000016));
#346627=CARTESIAN_POINT('Ctrl Pts',(3.96623003999994,2.2,-0.482893412000016));
#346628=CARTESIAN_POINT('Ctrl Pts',(3.96639550299994,12.2,-0.482908389000016));
#346629=CARTESIAN_POINT('Ctrl Pts',(3.96639550299994,5.2,-0.482908389000016));
#346630=CARTESIAN_POINT('Ctrl Pts',(3.96639550299994,2.2,-0.482908389000016));
#346631=CARTESIAN_POINT('Ctrl Pts',(3.96656805299994,12.2,-0.482923774000015));
#346632=CARTESIAN_POINT('Ctrl Pts',(3.96656805299994,5.2,-0.482923774000015));
#346633=CARTESIAN_POINT('Ctrl Pts',(3.96656805299994,2.2,-0.482923774000015));
#346634=CARTESIAN_POINT('Ctrl Pts',(3.96674767599994,12.2,-0.482939544000014));
#346635=CARTESIAN_POINT('Ctrl Pts',(3.96674767599994,5.2,-0.482939544000014));
#346636=CARTESIAN_POINT('Ctrl Pts',(3.96674767599994,2.2,-0.482939544000014));
#346637=CARTESIAN_POINT('Ctrl Pts',(3.96693435899994,12.2,-0.482955682000017));
#346638=CARTESIAN_POINT('Ctrl Pts',(3.96693435899994,5.2,-0.482955682000017));
#346639=CARTESIAN_POINT('Ctrl Pts',(3.96693435899994,2.2,-0.482955682000017));
#346640=CARTESIAN_POINT('Ctrl Pts',(3.96712808699994,12.2,-0.482972166000017));
#346641=CARTESIAN_POINT('Ctrl Pts',(3.96712808699994,5.2,-0.482972166000017));
#346642=CARTESIAN_POINT('Ctrl Pts',(3.96712808699994,2.2,-0.482972166000017));
#346643=CARTESIAN_POINT('Ctrl Pts',(3.96732884499994,12.2,-0.482988979000014));
#346644=CARTESIAN_POINT('Ctrl Pts',(3.96732884499994,5.2,-0.482988979000014));
#346645=CARTESIAN_POINT('Ctrl Pts',(3.96732884499994,2.2,-0.482988979000014));
#346646=CARTESIAN_POINT('Ctrl Pts',(3.96753661899994,12.2,-0.483006098000014));
#346647=CARTESIAN_POINT('Ctrl Pts',(3.96753661899994,5.2,-0.483006098000014));
#346648=CARTESIAN_POINT('Ctrl Pts',(3.96753661899994,2.2,-0.483006098000014));
#346649=CARTESIAN_POINT('Ctrl Pts',(3.96775139599994,12.2,-0.483023505000015));
#346650=CARTESIAN_POINT('Ctrl Pts',(3.96775139599994,5.2,-0.483023505000015));
#346651=CARTESIAN_POINT('Ctrl Pts',(3.96775139599994,2.2,-0.483023505000015));
#346652=CARTESIAN_POINT('Ctrl Pts',(3.96797315999994,12.2,-0.483041180000012));
#346653=CARTESIAN_POINT('Ctrl Pts',(3.96797315999994,5.2,-0.483041180000012));
#346654=CARTESIAN_POINT('Ctrl Pts',(3.96797315999994,2.2,-0.483041180000012));
#346655=CARTESIAN_POINT('Ctrl Pts',(3.96820189699994,12.2,-0.483059102000016));
#346656=CARTESIAN_POINT('Ctrl Pts',(3.96820189699994,5.2,-0.483059102000016));
#346657=CARTESIAN_POINT('Ctrl Pts',(3.96820189699994,2.2,-0.483059102000016));
#346658=CARTESIAN_POINT('Ctrl Pts',(3.96843759299994,12.2,-0.483077252000013));
#346659=CARTESIAN_POINT('Ctrl Pts',(3.96843759299994,5.2,-0.483077252000013));
#346660=CARTESIAN_POINT('Ctrl Pts',(3.96843759299994,2.2,-0.483077252000013));
#346661=CARTESIAN_POINT('Ctrl Pts',(3.96868023399994,12.2,-0.483095611000017));
#346662=CARTESIAN_POINT('Ctrl Pts',(3.96868023399994,5.2,-0.483095611000017));
#346663=CARTESIAN_POINT('Ctrl Pts',(3.96868023399994,2.2,-0.483095611000017));
#346664=CARTESIAN_POINT('Ctrl Pts',(3.96892980499994,12.2,-0.483114161000016));
#346665=CARTESIAN_POINT('Ctrl Pts',(3.96892980499994,5.2,-0.483114161000016));
#346666=CARTESIAN_POINT('Ctrl Pts',(3.96892980499994,2.2,-0.483114161000016));
#346667=CARTESIAN_POINT('Ctrl Pts',(3.96918629399994,12.2,-0.483132879000014));
#346668=CARTESIAN_POINT('Ctrl Pts',(3.96918629399994,5.2,-0.483132879000014));
#346669=CARTESIAN_POINT('Ctrl Pts',(3.96918629399994,2.2,-0.483132879000014));
#346670=CARTESIAN_POINT('Ctrl Pts',(3.96944968499994,12.2,-0.483151750000013));
#346671=CARTESIAN_POINT('Ctrl Pts',(3.96944968499994,5.2,-0.483151750000013));
#346672=CARTESIAN_POINT('Ctrl Pts',(3.96944968499994,2.2,-0.483151750000013));
#346673=CARTESIAN_POINT('Ctrl Pts',(3.96971996399994,12.2,-0.483170752000017));
#346674=CARTESIAN_POINT('Ctrl Pts',(3.96971996399994,5.2,-0.483170752000017));
#346675=CARTESIAN_POINT('Ctrl Pts',(3.96971996399994,2.2,-0.483170752000017));
#346676=CARTESIAN_POINT('Ctrl Pts',(3.96999711799995,12.2,-0.483189867000018));
#346677=CARTESIAN_POINT('Ctrl Pts',(3.96999711799995,5.2,-0.483189867000018));
#346678=CARTESIAN_POINT('Ctrl Pts',(3.96999711799995,2.2,-0.483189867000018));
#346679=CARTESIAN_POINT('Ctrl Pts',(3.97028113299994,12.2,-0.483209075000013));
#346680=CARTESIAN_POINT('Ctrl Pts',(3.97028113299994,5.2,-0.483209075000013));
#346681=CARTESIAN_POINT('Ctrl Pts',(3.97028113299994,2.2,-0.483209075000013));
#346682=CARTESIAN_POINT('Ctrl Pts',(3.97057199299994,12.2,-0.483228358000014));
#346683=CARTESIAN_POINT('Ctrl Pts',(3.97057199299994,5.2,-0.483228358000014));
#346684=CARTESIAN_POINT('Ctrl Pts',(3.97057199299994,2.2,-0.483228358000014));
#346685=CARTESIAN_POINT('Ctrl Pts',(3.97086968699994,12.2,-0.483247698000016));
#346686=CARTESIAN_POINT('Ctrl Pts',(3.97086968699994,5.2,-0.483247698000016));
#346687=CARTESIAN_POINT('Ctrl Pts',(3.97086968699994,2.2,-0.483247698000016));
#346688=CARTESIAN_POINT('Ctrl Pts',(3.97117419799994,12.2,-0.483267075000011));
#346689=CARTESIAN_POINT('Ctrl Pts',(3.97117419799994,5.2,-0.483267075000011));
#346690=CARTESIAN_POINT('Ctrl Pts',(3.97117419799994,2.2,-0.483267075000011));
#346691=CARTESIAN_POINT('Ctrl Pts',(3.97148551499994,12.2,-0.483286471000017));
#346692=CARTESIAN_POINT('Ctrl Pts',(3.97148551499994,5.2,-0.483286471000017));
#346693=CARTESIAN_POINT('Ctrl Pts',(3.97148551499994,2.2,-0.483286471000017));
#346694=CARTESIAN_POINT('Ctrl Pts',(3.97180362299994,12.2,-0.483305866000014));
#346695=CARTESIAN_POINT('Ctrl Pts',(3.97180362299994,5.2,-0.483305866000014));
#346696=CARTESIAN_POINT('Ctrl Pts',(3.97180362299994,2.2,-0.483305866000014));
#346697=CARTESIAN_POINT('Ctrl Pts',(3.97212850699994,12.2,-0.483325243000015));
#346698=CARTESIAN_POINT('Ctrl Pts',(3.97212850699994,5.2,-0.483325243000015));
#346699=CARTESIAN_POINT('Ctrl Pts',(3.97212850699994,2.2,-0.483325243000015));
#346700=CARTESIAN_POINT('Ctrl Pts',(3.97246015499995,12.2,-0.483344584000012));
#346701=CARTESIAN_POINT('Ctrl Pts',(3.97246015499995,5.2,-0.483344584000012));
#346702=CARTESIAN_POINT('Ctrl Pts',(3.97246015499995,2.2,-0.483344584000012));
#346703=CARTESIAN_POINT('Ctrl Pts',(3.97279855099994,12.2,-0.483363869000013));
#346704=CARTESIAN_POINT('Ctrl Pts',(3.97279855099994,5.2,-0.483363869000013));
#346705=CARTESIAN_POINT('Ctrl Pts',(3.97279855099994,2.2,-0.483363869000013));
#346706=CARTESIAN_POINT('Ctrl Pts',(3.97314368299994,12.2,-0.483383081000017));
#346707=CARTESIAN_POINT('Ctrl Pts',(3.97314368299994,5.2,-0.483383081000017));
#346708=CARTESIAN_POINT('Ctrl Pts',(3.97314368299994,2.2,-0.483383081000017));
#346709=CARTESIAN_POINT('Ctrl Pts',(3.97349553699994,12.2,-0.483402201000014));
#346710=CARTESIAN_POINT('Ctrl Pts',(3.97349553699994,5.2,-0.483402201000014));
#346711=CARTESIAN_POINT('Ctrl Pts',(3.97349553699994,2.2,-0.483402201000014));
#346712=CARTESIAN_POINT('Ctrl Pts',(3.97385409999994,12.2,-0.483421212000015));
#346713=CARTESIAN_POINT('Ctrl Pts',(3.97385409999994,5.2,-0.483421212000015));
#346714=CARTESIAN_POINT('Ctrl Pts',(3.97385409999994,2.2,-0.483421212000015));
#346715=CARTESIAN_POINT('Ctrl Pts',(3.97421935599994,12.2,-0.483440095000014));
#346716=CARTESIAN_POINT('Ctrl Pts',(3.97421935599994,5.2,-0.483440095000014));
#346717=CARTESIAN_POINT('Ctrl Pts',(3.97421935599994,2.2,-0.483440095000014));
#346718=CARTESIAN_POINT('Ctrl Pts',(3.97459129399994,12.2,-0.483458832000014));
#346719=CARTESIAN_POINT('Ctrl Pts',(3.97459129399994,5.2,-0.483458832000014));
#346720=CARTESIAN_POINT('Ctrl Pts',(3.97459129399994,2.2,-0.483458832000014));
#346721=CARTESIAN_POINT('Ctrl Pts',(3.97496989799994,12.2,-0.483477405000015));
#346722=CARTESIAN_POINT('Ctrl Pts',(3.97496989799994,5.2,-0.483477405000015));
#346723=CARTESIAN_POINT('Ctrl Pts',(3.97496989799994,2.2,-0.483477405000015));
#346724=CARTESIAN_POINT('Ctrl Pts',(3.97535515599994,12.2,-0.483495797000018));
#346725=CARTESIAN_POINT('Ctrl Pts',(3.97535515599994,5.2,-0.483495797000018));
#346726=CARTESIAN_POINT('Ctrl Pts',(3.97535515599994,2.2,-0.483495797000018));
#346727=CARTESIAN_POINT('Ctrl Pts',(3.97574705299994,12.2,-0.483513990000013));
#346728=CARTESIAN_POINT('Ctrl Pts',(3.97574705299994,5.2,-0.483513990000013));
#346729=CARTESIAN_POINT('Ctrl Pts',(3.97574705299994,2.2,-0.483513990000013));
#346730=CARTESIAN_POINT('Ctrl Pts',(3.97614557699994,12.2,-0.483531966000013));
#346731=CARTESIAN_POINT('Ctrl Pts',(3.97614557699994,5.2,-0.483531966000013));
#346732=CARTESIAN_POINT('Ctrl Pts',(3.97614557699994,2.2,-0.483531966000013));
#346733=CARTESIAN_POINT('Ctrl Pts',(3.97655071399994,12.2,-0.483549707000015));
#346734=CARTESIAN_POINT('Ctrl Pts',(3.97655071399994,5.2,-0.483549707000015));
#346735=CARTESIAN_POINT('Ctrl Pts',(3.97655071399994,2.2,-0.483549707000015));
#346736=CARTESIAN_POINT('Ctrl Pts',(3.97696244899994,12.2,-0.483567197000014));
#346737=CARTESIAN_POINT('Ctrl Pts',(3.97696244899994,5.2,-0.483567197000014));
#346738=CARTESIAN_POINT('Ctrl Pts',(3.97696244899994,2.2,-0.483567197000014));
#346739=CARTESIAN_POINT('Ctrl Pts',(3.97738077099994,12.2,-0.483584416000014));
#346740=CARTESIAN_POINT('Ctrl Pts',(3.97738077099994,5.2,-0.483584416000014));
#346741=CARTESIAN_POINT('Ctrl Pts',(3.97738077099994,2.2,-0.483584416000014));
#346742=CARTESIAN_POINT('Ctrl Pts',(3.97780566499994,12.2,-0.483601350000011));
#346743=CARTESIAN_POINT('Ctrl Pts',(3.97780566499994,5.2,-0.483601350000011));
#346744=CARTESIAN_POINT('Ctrl Pts',(3.97780566499994,2.2,-0.483601350000011));
#346745=CARTESIAN_POINT('Ctrl Pts',(3.97823711799994,12.2,-0.483617978000015));
#346746=CARTESIAN_POINT('Ctrl Pts',(3.97823711799994,5.2,-0.483617978000015));
#346747=CARTESIAN_POINT('Ctrl Pts',(3.97823711799994,2.2,-0.483617978000015));
#346748=CARTESIAN_POINT('Ctrl Pts',(3.97867511499994,12.2,-0.483634286000014));
#346749=CARTESIAN_POINT('Ctrl Pts',(3.97867511499994,5.2,-0.483634286000014));
#346750=CARTESIAN_POINT('Ctrl Pts',(3.97867511499994,2.2,-0.483634286000014));
#346751=CARTESIAN_POINT('Ctrl Pts',(3.97911964499994,12.2,-0.483650256000012));
#346752=CARTESIAN_POINT('Ctrl Pts',(3.97911964499994,5.2,-0.483650256000012));
#346753=CARTESIAN_POINT('Ctrl Pts',(3.97911964499994,2.2,-0.483650256000012));
#346754=CARTESIAN_POINT('Ctrl Pts',(3.97957069299994,12.2,-0.483665869000016));
#346755=CARTESIAN_POINT('Ctrl Pts',(3.97957069299994,5.2,-0.483665869000016));
#346756=CARTESIAN_POINT('Ctrl Pts',(3.97957069299994,2.2,-0.483665869000016));
#346757=CARTESIAN_POINT('Ctrl Pts',(3.98002824599994,12.2,-0.483681109000016));
#346758=CARTESIAN_POINT('Ctrl Pts',(3.98002824599994,5.2,-0.483681109000016));
#346759=CARTESIAN_POINT('Ctrl Pts',(3.98002824599994,2.2,-0.483681109000016));
#346760=CARTESIAN_POINT('Ctrl Pts',(3.98049229099994,12.2,-0.483695961000015));
#346761=CARTESIAN_POINT('Ctrl Pts',(3.98049229099994,5.2,-0.483695961000015));
#346762=CARTESIAN_POINT('Ctrl Pts',(3.98049229099994,2.2,-0.483695961000015));
#346763=CARTESIAN_POINT('Ctrl Pts',(3.98096281399994,12.2,-0.483710406000015));
#346764=CARTESIAN_POINT('Ctrl Pts',(3.98096281399994,5.2,-0.483710406000015));
#346765=CARTESIAN_POINT('Ctrl Pts',(3.98096281399994,2.2,-0.483710406000015));
#346766=CARTESIAN_POINT('Ctrl Pts',(3.98143980299994,12.2,-0.483724427000016));
#346767=CARTESIAN_POINT('Ctrl Pts',(3.98143980299994,5.2,-0.483724427000016));
#346768=CARTESIAN_POINT('Ctrl Pts',(3.98143980299994,2.2,-0.483724427000016));
#346769=CARTESIAN_POINT('Ctrl Pts',(3.98192324299994,12.2,-0.483738009000017));
#346770=CARTESIAN_POINT('Ctrl Pts',(3.98192324299994,5.2,-0.483738009000017));
#346771=CARTESIAN_POINT('Ctrl Pts',(3.98192324299994,2.2,-0.483738009000017));
#346772=CARTESIAN_POINT('Ctrl Pts',(3.98241312199994,12.2,-0.483751134000014));
#346773=CARTESIAN_POINT('Ctrl Pts',(3.98241312199994,5.2,-0.483751134000014));
#346774=CARTESIAN_POINT('Ctrl Pts',(3.98241312199994,2.2,-0.483751134000014));
#346775=CARTESIAN_POINT('Ctrl Pts',(3.98290942699994,12.2,-0.483763784000013));
#346776=CARTESIAN_POINT('Ctrl Pts',(3.98290942699994,5.2,-0.483763784000013));
#346777=CARTESIAN_POINT('Ctrl Pts',(3.98290942699994,2.2,-0.483763784000013));
#346778=CARTESIAN_POINT('Ctrl Pts',(3.98341214399994,12.2,-0.483775947000016));
#346779=CARTESIAN_POINT('Ctrl Pts',(3.98341214399994,5.2,-0.483775947000016));
#346780=CARTESIAN_POINT('Ctrl Pts',(3.98341214399994,2.2,-0.483775947000016));
#346781=CARTESIAN_POINT('Ctrl Pts',(3.98392125999994,12.2,-0.483787602000016));
#346782=CARTESIAN_POINT('Ctrl Pts',(3.98392125999994,5.2,-0.483787602000016));
#346783=CARTESIAN_POINT('Ctrl Pts',(3.98392125999994,2.2,-0.483787602000016));
#346784=CARTESIAN_POINT('Ctrl Pts',(3.98443676199994,12.2,-0.483798734000014));
#346785=CARTESIAN_POINT('Ctrl Pts',(3.98443676199994,5.2,-0.483798734000014));
#346786=CARTESIAN_POINT('Ctrl Pts',(3.98443676199994,2.2,-0.483798734000014));
#346787=CARTESIAN_POINT('Ctrl Pts',(3.98495863699994,12.2,-0.483809327000015));
#346788=CARTESIAN_POINT('Ctrl Pts',(3.98495863699994,5.2,-0.483809327000015));
#346789=CARTESIAN_POINT('Ctrl Pts',(3.98495863699994,2.2,-0.483809327000015));
#346790=CARTESIAN_POINT('Ctrl Pts',(3.98548687099994,12.2,-0.483819364000015));
#346791=CARTESIAN_POINT('Ctrl Pts',(3.98548687099994,5.2,-0.483819364000015));
#346792=CARTESIAN_POINT('Ctrl Pts',(3.98548687099994,2.2,-0.483819364000015));
#346793=CARTESIAN_POINT('Ctrl Pts',(3.98602145199995,12.2,-0.483828830000017));
#346794=CARTESIAN_POINT('Ctrl Pts',(3.98602145199995,5.2,-0.483828830000017));
#346795=CARTESIAN_POINT('Ctrl Pts',(3.98602145199995,2.2,-0.483828830000017));
#346796=CARTESIAN_POINT('Ctrl Pts',(3.98656236599995,12.2,-0.483837709000015));
#346797=CARTESIAN_POINT('Ctrl Pts',(3.98656236599995,5.2,-0.483837709000015));
#346798=CARTESIAN_POINT('Ctrl Pts',(3.98656236599995,2.2,-0.483837709000015));
#346799=CARTESIAN_POINT('Ctrl Pts',(3.98710959999994,12.2,-0.483845983000015));
#346800=CARTESIAN_POINT('Ctrl Pts',(3.98710959999994,5.2,-0.483845983000015));
#346801=CARTESIAN_POINT('Ctrl Pts',(3.98710959999994,2.2,-0.483845983000015));
#346802=CARTESIAN_POINT('Ctrl Pts',(3.98766314199994,12.2,-0.483853638000014));
#346803=CARTESIAN_POINT('Ctrl Pts',(3.98766314199994,5.2,-0.483853638000014));
#346804=CARTESIAN_POINT('Ctrl Pts',(3.98766314199994,2.2,-0.483853638000014));
#346805=CARTESIAN_POINT('Ctrl Pts',(3.98822297899994,12.2,-0.483860657000013));
#346806=CARTESIAN_POINT('Ctrl Pts',(3.98822297899994,5.2,-0.483860657000013));
#346807=CARTESIAN_POINT('Ctrl Pts',(3.98822297899994,2.2,-0.483860657000013));
#346808=CARTESIAN_POINT('Ctrl Pts',(3.98878909599994,12.2,-0.483867023000015));
#346809=CARTESIAN_POINT('Ctrl Pts',(3.98878909599994,5.2,-0.483867023000015));
#346810=CARTESIAN_POINT('Ctrl Pts',(3.98878909599994,2.2,-0.483867023000015));
#346811=CARTESIAN_POINT('Ctrl Pts',(3.98936148199994,12.2,-0.483872724000012));
#346812=CARTESIAN_POINT('Ctrl Pts',(3.98936148199994,5.2,-0.483872724000012));
#346813=CARTESIAN_POINT('Ctrl Pts',(3.98936148199994,2.2,-0.483872724000012));
#346814=CARTESIAN_POINT('Ctrl Pts',(3.98994012399994,12.2,-0.483877739000014));
#346815=CARTESIAN_POINT('Ctrl Pts',(3.98994012399994,5.2,-0.483877739000014));
#346816=CARTESIAN_POINT('Ctrl Pts',(3.98994012399994,2.2,-0.483877739000014));
#346817=CARTESIAN_POINT('Ctrl Pts',(3.99052500699994,12.2,-0.483882056000016));
#346818=CARTESIAN_POINT('Ctrl Pts',(3.99052500699994,5.2,-0.483882056000016));
#346819=CARTESIAN_POINT('Ctrl Pts',(3.99052500699994,2.2,-0.483882056000016));
#346820=CARTESIAN_POINT('Ctrl Pts',(3.99111612099994,12.2,-0.483885659000016));
#346821=CARTESIAN_POINT('Ctrl Pts',(3.99111612099994,5.2,-0.483885659000016));
#346822=CARTESIAN_POINT('Ctrl Pts',(3.99111612099994,2.2,-0.483885659000016));
#346823=CARTESIAN_POINT('Ctrl Pts',(3.99171345099994,12.2,-0.483888531000014));
#346824=CARTESIAN_POINT('Ctrl Pts',(3.99171345099994,5.2,-0.483888531000014));
#346825=CARTESIAN_POINT('Ctrl Pts',(3.99171345099994,2.2,-0.483888531000014));
#346826=CARTESIAN_POINT('Ctrl Pts',(3.99231698499994,12.2,-0.483890657000017));
#346827=CARTESIAN_POINT('Ctrl Pts',(3.99231698499994,5.2,-0.483890657000017));
#346828=CARTESIAN_POINT('Ctrl Pts',(3.99231698499994,2.2,-0.483890657000017));
#346829=CARTESIAN_POINT('Ctrl Pts',(3.99292670999994,12.2,-0.483892023000014));
#346830=CARTESIAN_POINT('Ctrl Pts',(3.99292670999994,5.2,-0.483892023000014));
#346831=CARTESIAN_POINT('Ctrl Pts',(3.99292670999994,2.2,-0.483892023000014));
#346832=CARTESIAN_POINT('Ctrl Pts',(3.99354261299994,12.2,-0.483892612000014));
#346833=CARTESIAN_POINT('Ctrl Pts',(3.99354261299994,5.2,-0.483892612000014));
#346834=CARTESIAN_POINT('Ctrl Pts',(3.99354261299994,2.2,-0.483892612000014));
#346835=CARTESIAN_POINT('Ctrl Pts',(3.99416468199994,12.2,-0.483892409000015));
#346836=CARTESIAN_POINT('Ctrl Pts',(3.99416468199994,5.2,-0.483892409000015));
#346837=CARTESIAN_POINT('Ctrl Pts',(3.99416468199994,2.2,-0.483892409000015));
#346838=CARTESIAN_POINT('Ctrl Pts',(3.99479290299994,12.2,-0.483891397000011));
#346839=CARTESIAN_POINT('Ctrl Pts',(3.99479290299994,5.2,-0.483891397000011));
#346840=CARTESIAN_POINT('Ctrl Pts',(3.99479290299994,2.2,-0.483891397000011));
#346841=CARTESIAN_POINT('Ctrl Pts',(3.99542726299994,12.2,-0.483889565000015));
#346842=CARTESIAN_POINT('Ctrl Pts',(3.99542726299994,5.2,-0.483889565000015));
#346843=CARTESIAN_POINT('Ctrl Pts',(3.99542726299994,2.2,-0.483889565000015));
#346844=CARTESIAN_POINT('Ctrl Pts',(3.99606775099994,12.2,-0.483886895000012));
#346845=CARTESIAN_POINT('Ctrl Pts',(3.99606775099994,5.2,-0.483886895000012));
#346846=CARTESIAN_POINT('Ctrl Pts',(3.99606775099994,2.2,-0.483886895000012));
#346847=CARTESIAN_POINT('Ctrl Pts',(3.99671435299994,12.2,-0.483883372000014));
#346848=CARTESIAN_POINT('Ctrl Pts',(3.99671435299994,5.2,-0.483883372000014));
#346849=CARTESIAN_POINT('Ctrl Pts',(3.99671435299994,2.2,-0.483883372000014));
#346850=CARTESIAN_POINT('Ctrl Pts',(3.99736705599994,12.2,-0.483878981000014));
#346851=CARTESIAN_POINT('Ctrl Pts',(3.99736705599994,5.2,-0.483878981000014));
#346852=CARTESIAN_POINT('Ctrl Pts',(3.99736705599994,2.2,-0.483878981000014));
#346853=CARTESIAN_POINT('Ctrl Pts',(3.99802584899994,12.2,-0.483873708000013));
#346854=CARTESIAN_POINT('Ctrl Pts',(3.99802584899994,5.2,-0.483873708000013));
#346855=CARTESIAN_POINT('Ctrl Pts',(3.99802584899994,2.2,-0.483873708000013));
#346856=CARTESIAN_POINT('Ctrl Pts',(3.99869071799994,12.2,-0.483867537000013));
#346857=CARTESIAN_POINT('Ctrl Pts',(3.99869071799994,5.2,-0.483867537000013));
#346858=CARTESIAN_POINT('Ctrl Pts',(3.99869071799994,2.2,-0.483867537000013));
#346859=CARTESIAN_POINT('Ctrl Pts',(3.99936164999994,12.2,-0.483860454000014));
#346860=CARTESIAN_POINT('Ctrl Pts',(3.99936164999994,5.2,-0.483860454000014));
#346861=CARTESIAN_POINT('Ctrl Pts',(3.99936164999994,2.2,-0.483860454000014));
#346862=CARTESIAN_POINT('Ctrl Pts',(4.00003863299994,12.2,-0.483852443000017));
#346863=CARTESIAN_POINT('Ctrl Pts',(4.00003863299994,5.2,-0.483852443000017));
#346864=CARTESIAN_POINT('Ctrl Pts',(4.00003863299994,2.2,-0.483852443000017));
#346865=CARTESIAN_POINT('Ctrl Pts',(4.00072165499994,12.2,-0.483843491000013));
#346866=CARTESIAN_POINT('Ctrl Pts',(4.00072165499994,5.2,-0.483843491000013));
#346867=CARTESIAN_POINT('Ctrl Pts',(4.00072165499994,2.2,-0.483843491000013));
#346868=CARTESIAN_POINT('Ctrl Pts',(4.00141070199994,12.2,-0.483833582000015));
#346869=CARTESIAN_POINT('Ctrl Pts',(4.00141070199994,5.2,-0.483833582000015));
#346870=CARTESIAN_POINT('Ctrl Pts',(4.00141070199994,2.2,-0.483833582000015));
#346871=CARTESIAN_POINT('Ctrl Pts',(4.00210576199994,12.2,-0.483822701000012));
#346872=CARTESIAN_POINT('Ctrl Pts',(4.00210576199994,5.2,-0.483822701000012));
#346873=CARTESIAN_POINT('Ctrl Pts',(4.00210576199994,2.2,-0.483822701000012));
#346874=CARTESIAN_POINT('Ctrl Pts',(4.00280682299995,12.2,-0.483810836000016));
#346875=CARTESIAN_POINT('Ctrl Pts',(4.00280682299995,5.2,-0.483810836000016));
#346876=CARTESIAN_POINT('Ctrl Pts',(4.00280682299995,2.2,-0.483810836000016));
#346877=CARTESIAN_POINT('Ctrl Pts',(4.00351387199995,12.2,-0.483797969000013));
#346878=CARTESIAN_POINT('Ctrl Pts',(4.00351387199995,5.2,-0.483797969000013));
#346879=CARTESIAN_POINT('Ctrl Pts',(4.00351387199995,2.2,-0.483797969000013));
#346880=CARTESIAN_POINT('Ctrl Pts',(4.00422689599994,12.2,-0.483784088000014));
#346881=CARTESIAN_POINT('Ctrl Pts',(4.00422689599994,5.2,-0.483784088000014));
#346882=CARTESIAN_POINT('Ctrl Pts',(4.00422689599994,2.2,-0.483784088000014));
#346883=CARTESIAN_POINT('Ctrl Pts',(4.00494588399994,12.2,-0.483769178000015));
#346884=CARTESIAN_POINT('Ctrl Pts',(4.00494588399994,5.2,-0.483769178000015));
#346885=CARTESIAN_POINT('Ctrl Pts',(4.00494588399994,2.2,-0.483769178000015));
#346886=CARTESIAN_POINT('Ctrl Pts',(4.00567082099994,12.2,-0.483753224000014));
#346887=CARTESIAN_POINT('Ctrl Pts',(4.00567082099994,5.2,-0.483753224000014));
#346888=CARTESIAN_POINT('Ctrl Pts',(4.00567082099994,2.2,-0.483753224000014));
#346889=CARTESIAN_POINT('Ctrl Pts',(4.00640169699995,12.2,-0.483736213000014));
#346890=CARTESIAN_POINT('Ctrl Pts',(4.00640169699995,5.2,-0.483736213000014));
#346891=CARTESIAN_POINT('Ctrl Pts',(4.00640169699995,2.2,-0.483736213000014));
#346892=CARTESIAN_POINT('Ctrl Pts',(4.00713849899994,12.2,-0.483718129000015));
#346893=CARTESIAN_POINT('Ctrl Pts',(4.00713849899994,5.2,-0.483718129000015));
#346894=CARTESIAN_POINT('Ctrl Pts',(4.00713849899994,2.2,-0.483718129000015));
#346895=CARTESIAN_POINT('Ctrl Pts',(4.00788121299995,12.2,-0.483698960000014));
#346896=CARTESIAN_POINT('Ctrl Pts',(4.00788121299995,5.2,-0.483698960000014));
#346897=CARTESIAN_POINT('Ctrl Pts',(4.00788121299995,2.2,-0.483698960000014));
#346898=CARTESIAN_POINT('Ctrl Pts',(4.00862982799994,12.2,-0.483678690000016));
#346899=CARTESIAN_POINT('Ctrl Pts',(4.00862982799994,5.2,-0.483678690000016));
#346900=CARTESIAN_POINT('Ctrl Pts',(4.00862982799994,2.2,-0.483678690000016));
#346901=CARTESIAN_POINT('Ctrl Pts',(4.00938433099994,12.2,-0.483657306000014));
#346902=CARTESIAN_POINT('Ctrl Pts',(4.00938433099994,5.2,-0.483657306000014));
#346903=CARTESIAN_POINT('Ctrl Pts',(4.00938433099994,2.2,-0.483657306000014));
#346904=CARTESIAN_POINT('Ctrl Pts',(4.01014471099994,12.2,-0.483634794000012));
#346905=CARTESIAN_POINT('Ctrl Pts',(4.01014471099994,5.2,-0.483634794000012));
#346906=CARTESIAN_POINT('Ctrl Pts',(4.01014471099994,2.2,-0.483634794000012));
#346907=CARTESIAN_POINT('Ctrl Pts',(4.01091095499994,12.2,-0.483611138000013));
#346908=CARTESIAN_POINT('Ctrl Pts',(4.01091095499994,5.2,-0.483611138000013));
#346909=CARTESIAN_POINT('Ctrl Pts',(4.01091095499994,2.2,-0.483611138000013));
#346910=CARTESIAN_POINT('Ctrl Pts',(4.01168304899994,12.2,-0.483586328000012));
#346911=CARTESIAN_POINT('Ctrl Pts',(4.01168304899994,5.2,-0.483586328000012));
#346912=CARTESIAN_POINT('Ctrl Pts',(4.01168304899994,2.2,-0.483586328000012));
#346913=CARTESIAN_POINT('Ctrl Pts',(4.01246098199994,12.2,-0.483560347000012));
#346914=CARTESIAN_POINT('Ctrl Pts',(4.01246098199994,5.2,-0.483560347000012));
#346915=CARTESIAN_POINT('Ctrl Pts',(4.01246098199994,2.2,-0.483560347000012));
#346916=CARTESIAN_POINT('Ctrl Pts',(4.01324474199994,12.2,-0.483533182000015));
#346917=CARTESIAN_POINT('Ctrl Pts',(4.01324474199994,5.2,-0.483533182000015));
#346918=CARTESIAN_POINT('Ctrl Pts',(4.01324474199994,2.2,-0.483533182000015));
#346919=CARTESIAN_POINT('Ctrl Pts',(4.01403431599994,12.2,-0.483504820000018));
#346920=CARTESIAN_POINT('Ctrl Pts',(4.01403431599994,5.2,-0.483504820000018));
#346921=CARTESIAN_POINT('Ctrl Pts',(4.01403431599994,2.2,-0.483504820000018));
#346922=CARTESIAN_POINT('Ctrl Pts',(4.01482969199995,12.2,-0.483475246000014));
#346923=CARTESIAN_POINT('Ctrl Pts',(4.01482969199995,5.2,-0.483475246000014));
#346924=CARTESIAN_POINT('Ctrl Pts',(4.01482969199995,2.2,-0.483475246000014));
#346925=CARTESIAN_POINT('Ctrl Pts',(4.01563085799994,12.2,-0.483444448000014));
#346926=CARTESIAN_POINT('Ctrl Pts',(4.01563085799994,5.2,-0.483444448000014));
#346927=CARTESIAN_POINT('Ctrl Pts',(4.01563085799994,2.2,-0.483444448000014));
#346928=CARTESIAN_POINT('Ctrl Pts',(4.01643780099994,12.2,-0.483412411000015));
#346929=CARTESIAN_POINT('Ctrl Pts',(4.01643780099994,5.2,-0.483412411000015));
#346930=CARTESIAN_POINT('Ctrl Pts',(4.01643780099994,2.2,-0.483412411000015));
#346931=CARTESIAN_POINT('Ctrl Pts',(4.01725050999994,12.2,-0.483379121000014));
#346932=CARTESIAN_POINT('Ctrl Pts',(4.01725050999994,5.2,-0.483379121000014));
#346933=CARTESIAN_POINT('Ctrl Pts',(4.01725050999994,2.2,-0.483379121000014));
#346934=CARTESIAN_POINT('Ctrl Pts',(4.01806897099994,12.2,-0.483344567000015));
#346935=CARTESIAN_POINT('Ctrl Pts',(4.01806897099994,5.2,-0.483344567000015));
#346936=CARTESIAN_POINT('Ctrl Pts',(4.01806897099994,2.2,-0.483344567000015));
#346937=CARTESIAN_POINT('Ctrl Pts',(4.01889317399994,12.2,-0.483308734000012));
#346938=CARTESIAN_POINT('Ctrl Pts',(4.01889317399994,5.2,-0.483308734000012));
#346939=CARTESIAN_POINT('Ctrl Pts',(4.01889317399994,2.2,-0.483308734000012));
#346940=CARTESIAN_POINT('Ctrl Pts',(4.01972310599994,12.2,-0.483271609000013));
#346941=CARTESIAN_POINT('Ctrl Pts',(4.01972310599994,5.2,-0.483271609000013));
#346942=CARTESIAN_POINT('Ctrl Pts',(4.01972310599994,2.2,-0.483271609000013));
#346943=CARTESIAN_POINT('Ctrl Pts',(4.02055875299994,12.2,-0.483233178000013));
#346944=CARTESIAN_POINT('Ctrl Pts',(4.02055875299994,5.2,-0.483233178000013));
#346945=CARTESIAN_POINT('Ctrl Pts',(4.02055875299994,2.2,-0.483233178000013));
#346946=CARTESIAN_POINT('Ctrl Pts',(4.02140010499994,12.2,-0.483193427000015));
#346947=CARTESIAN_POINT('Ctrl Pts',(4.02140010499994,5.2,-0.483193427000015));
#346948=CARTESIAN_POINT('Ctrl Pts',(4.02140010499994,2.2,-0.483193427000015));
#346949=CARTESIAN_POINT('Ctrl Pts',(4.02224714999995,12.2,-0.483152346000013));
#346950=CARTESIAN_POINT('Ctrl Pts',(4.02224714999995,5.2,-0.483152346000013));
#346951=CARTESIAN_POINT('Ctrl Pts',(4.02224714999995,2.2,-0.483152346000013));
#346952=CARTESIAN_POINT('Ctrl Pts',(4.02309987399994,12.2,-0.483109919000011));
#346953=CARTESIAN_POINT('Ctrl Pts',(4.02309987399994,5.2,-0.483109919000011));
#346954=CARTESIAN_POINT('Ctrl Pts',(4.02309987399994,2.2,-0.483109919000011));
#346955=CARTESIAN_POINT('Ctrl Pts',(4.02395826699994,12.2,-0.483066133000012));
#346956=CARTESIAN_POINT('Ctrl Pts',(4.02395826699994,5.2,-0.483066133000012));
#346957=CARTESIAN_POINT('Ctrl Pts',(4.02395826699994,2.2,-0.483066133000012));
#346958=CARTESIAN_POINT('Ctrl Pts',(4.02482231599994,12.2,-0.483020976000015));
#346959=CARTESIAN_POINT('Ctrl Pts',(4.02482231599994,5.2,-0.483020976000015));
#346960=CARTESIAN_POINT('Ctrl Pts',(4.02482231599994,2.2,-0.483020976000015));
#346961=CARTESIAN_POINT('Ctrl Pts',(4.02569200799994,12.2,-0.482974435000014));
#346962=CARTESIAN_POINT('Ctrl Pts',(4.02569200799994,5.2,-0.482974435000014));
#346963=CARTESIAN_POINT('Ctrl Pts',(4.02569200799994,2.2,-0.482974435000014));
#346964=CARTESIAN_POINT('Ctrl Pts',(4.02656733299994,12.2,-0.482926497000014));
#346965=CARTESIAN_POINT('Ctrl Pts',(4.02656733299994,5.2,-0.482926497000014));
#346966=CARTESIAN_POINT('Ctrl Pts',(4.02656733299994,2.2,-0.482926497000014));
#346967=CARTESIAN_POINT('Ctrl Pts',(4.02744827799994,12.2,-0.482877148000016));
#346968=CARTESIAN_POINT('Ctrl Pts',(4.02744827799994,5.2,-0.482877148000016));
#346969=CARTESIAN_POINT('Ctrl Pts',(4.02744827799994,2.2,-0.482877148000016));
#346970=CARTESIAN_POINT('Ctrl Pts',(4.02833482899995,12.2,-0.482826375000016));
#346971=CARTESIAN_POINT('Ctrl Pts',(4.02833482899995,5.2,-0.482826375000016));
#346972=CARTESIAN_POINT('Ctrl Pts',(4.02833482899995,2.2,-0.482826375000016));
#346973=CARTESIAN_POINT('Ctrl Pts',(4.02922697699994,12.2,-0.482774167000013));
#346974=CARTESIAN_POINT('Ctrl Pts',(4.02922697699994,5.2,-0.482774167000013));
#346975=CARTESIAN_POINT('Ctrl Pts',(4.02922697699994,2.2,-0.482774167000013));
#346976=CARTESIAN_POINT('Ctrl Pts',(4.03012470899994,12.2,-0.482720510000014));
#346977=CARTESIAN_POINT('Ctrl Pts',(4.03012470899994,5.2,-0.482720510000014));
#346978=CARTESIAN_POINT('Ctrl Pts',(4.03012470899994,2.2,-0.482720510000014));
#346979=CARTESIAN_POINT('Ctrl Pts',(4.03102801199995,12.2,-0.482665392000015));
#346980=CARTESIAN_POINT('Ctrl Pts',(4.03102801199995,5.2,-0.482665392000015));
#346981=CARTESIAN_POINT('Ctrl Pts',(4.03102801199995,2.2,-0.482665392000015));
#346982=CARTESIAN_POINT('Ctrl Pts',(4.03193687599994,12.2,-0.482608799000013));
#346983=CARTESIAN_POINT('Ctrl Pts',(4.03193687599994,5.2,-0.482608799000013));
#346984=CARTESIAN_POINT('Ctrl Pts',(4.03193687599994,2.2,-0.482608799000013));
#346985=CARTESIAN_POINT('Ctrl Pts',(4.03285128799994,12.2,-0.482550720000017));
#346986=CARTESIAN_POINT('Ctrl Pts',(4.03285128799994,5.2,-0.482550720000017));
#346987=CARTESIAN_POINT('Ctrl Pts',(4.03285128799994,2.2,-0.482550720000017));
#346988=CARTESIAN_POINT('Ctrl Pts',(4.03377123599994,12.2,-0.482491142000012));
#346989=CARTESIAN_POINT('Ctrl Pts',(4.03377123599994,5.2,-0.482491142000012));
#346990=CARTESIAN_POINT('Ctrl Pts',(4.03377123599994,2.2,-0.482491142000012));
#346991=CARTESIAN_POINT('Ctrl Pts',(4.03469670699994,12.2,-0.482430050000016));
#346992=CARTESIAN_POINT('Ctrl Pts',(4.03469670699994,5.2,-0.482430050000016));
#346993=CARTESIAN_POINT('Ctrl Pts',(4.03469670699994,2.2,-0.482430050000016));
#346994=CARTESIAN_POINT('Ctrl Pts',(4.03562769099994,12.2,-0.482367436000013));
#346995=CARTESIAN_POINT('Ctrl Pts',(4.03562769099994,5.2,-0.482367436000013));
#346996=CARTESIAN_POINT('Ctrl Pts',(4.03562769099994,2.2,-0.482367436000013));
#346997=CARTESIAN_POINT('Ctrl Pts',(4.03656417599994,12.2,-0.482303284000012));
#346998=CARTESIAN_POINT('Ctrl Pts',(4.03656417599994,5.2,-0.482303284000012));
#346999=CARTESIAN_POINT('Ctrl Pts',(4.03656417599994,2.2,-0.482303284000012));
#347000=CARTESIAN_POINT('Ctrl Pts',(4.03750614799994,12.2,-0.482237583000016));
#347001=CARTESIAN_POINT('Ctrl Pts',(4.03750614799994,5.2,-0.482237583000016));
#347002=CARTESIAN_POINT('Ctrl Pts',(4.03750614799994,2.2,-0.482237583000016));
#347003=CARTESIAN_POINT('Ctrl Pts',(4.03845359799995,12.2,-0.482170321000015));
#347004=CARTESIAN_POINT('Ctrl Pts',(4.03845359799995,5.2,-0.482170321000015));
#347005=CARTESIAN_POINT('Ctrl Pts',(4.03845359799995,2.2,-0.482170321000015));
#347006=CARTESIAN_POINT('Ctrl Pts',(4.03940651299994,12.2,-0.482101484000013));
#347007=CARTESIAN_POINT('Ctrl Pts',(4.03940651299994,5.2,-0.482101484000013));
#347008=CARTESIAN_POINT('Ctrl Pts',(4.03940651299994,2.2,-0.482101484000013));
#347009=CARTESIAN_POINT('Ctrl Pts',(4.04036487999995,12.2,-0.482031062000012));
#347010=CARTESIAN_POINT('Ctrl Pts',(4.04036487999995,5.2,-0.482031062000012));
#347011=CARTESIAN_POINT('Ctrl Pts',(4.04036487999995,2.2,-0.482031062000012));
#347012=CARTESIAN_POINT('Ctrl Pts',(4.04132868899994,12.2,-0.481959041000017));
#347013=CARTESIAN_POINT('Ctrl Pts',(4.04132868899994,5.2,-0.481959041000017));
#347014=CARTESIAN_POINT('Ctrl Pts',(4.04132868899994,2.2,-0.481959041000017));
#347015=CARTESIAN_POINT('Ctrl Pts',(4.04229792699994,12.2,-0.481885410000018));
#347016=CARTESIAN_POINT('Ctrl Pts',(4.04229792699994,5.2,-0.481885410000018));
#347017=CARTESIAN_POINT('Ctrl Pts',(4.04229792699994,2.2,-0.481885410000018));
#347018=CARTESIAN_POINT('Ctrl Pts',(4.04327258299995,12.2,-0.481810156000013));
#347019=CARTESIAN_POINT('Ctrl Pts',(4.04327258299995,5.2,-0.481810156000013));
#347020=CARTESIAN_POINT('Ctrl Pts',(4.04327258299995,2.2,-0.481810156000013));
#347021=CARTESIAN_POINT('Ctrl Pts',(4.04425264399995,12.2,-0.481733268000015));
#347022=CARTESIAN_POINT('Ctrl Pts',(4.04425264399995,5.2,-0.481733268000015));
#347023=CARTESIAN_POINT('Ctrl Pts',(4.04425264399995,2.2,-0.481733268000015));
#347024=CARTESIAN_POINT('Ctrl Pts',(4.04523810099994,12.2,-0.481654733000014));
#347025=CARTESIAN_POINT('Ctrl Pts',(4.04523810099994,5.2,-0.481654733000014));
#347026=CARTESIAN_POINT('Ctrl Pts',(4.04523810099994,2.2,-0.481654733000014));
#347027=CARTESIAN_POINT('Ctrl Pts',(4.04622893899994,12.2,-0.481574540000014));
#347028=CARTESIAN_POINT('Ctrl Pts',(4.04622893899994,5.2,-0.481574540000014));
#347029=CARTESIAN_POINT('Ctrl Pts',(4.04622893899994,2.2,-0.481574540000014));
#347030=CARTESIAN_POINT('Ctrl Pts',(4.04722514799994,12.2,-0.481492676000013));
#347031=CARTESIAN_POINT('Ctrl Pts',(4.04722514799994,5.2,-0.481492676000013));
#347032=CARTESIAN_POINT('Ctrl Pts',(4.04722514799994,2.2,-0.481492676000013));
#347033=CARTESIAN_POINT('Ctrl Pts',(4.04822671599994,12.2,-0.481409130000015));
#347034=CARTESIAN_POINT('Ctrl Pts',(4.04822671599994,5.2,-0.481409130000015));
#347035=CARTESIAN_POINT('Ctrl Pts',(4.04822671599994,2.2,-0.481409130000015));
#347036=CARTESIAN_POINT('Ctrl Pts',(4.04923363199994,12.2,-0.481323889000014));
#347037=CARTESIAN_POINT('Ctrl Pts',(4.04923363199994,5.2,-0.481323889000014));
#347038=CARTESIAN_POINT('Ctrl Pts',(4.04923363199994,2.2,-0.481323889000014));
#347039=CARTESIAN_POINT('Ctrl Pts',(4.05024588299994,12.2,-0.481236942000014));
#347040=CARTESIAN_POINT('Ctrl Pts',(4.05024588299994,5.2,-0.481236942000014));
#347041=CARTESIAN_POINT('Ctrl Pts',(4.05024588299994,2.2,-0.481236942000014));
#347042=CARTESIAN_POINT('Ctrl Pts',(4.05126345799994,12.2,-0.481148277000014));
#347043=CARTESIAN_POINT('Ctrl Pts',(4.05126345799994,5.2,-0.481148277000014));
#347044=CARTESIAN_POINT('Ctrl Pts',(4.05126345799994,2.2,-0.481148277000014));
#347045=CARTESIAN_POINT('Ctrl Pts',(4.05228634599994,12.2,-0.481057884000013));
#347046=CARTESIAN_POINT('Ctrl Pts',(4.05228634599994,5.2,-0.481057884000013));
#347047=CARTESIAN_POINT('Ctrl Pts',(4.05228634599994,2.2,-0.481057884000013));
#347048=CARTESIAN_POINT('Ctrl Pts',(4.05331453399994,12.2,-0.480965749000015));
#347049=CARTESIAN_POINT('Ctrl Pts',(4.05331453399994,5.2,-0.480965749000015));
#347050=CARTESIAN_POINT('Ctrl Pts',(4.05331453399994,2.2,-0.480965749000015));
#347051=CARTESIAN_POINT('Ctrl Pts',(4.05434801099995,12.2,-0.480871860000014));
#347052=CARTESIAN_POINT('Ctrl Pts',(4.05434801099995,5.2,-0.480871860000014));
#347053=CARTESIAN_POINT('Ctrl Pts',(4.05434801099995,2.2,-0.480871860000014));
#347054=CARTESIAN_POINT('Ctrl Pts',(4.05538676699994,12.2,-0.480776208000013));
#347055=CARTESIAN_POINT('Ctrl Pts',(4.05538676699994,5.2,-0.480776208000013));
#347056=CARTESIAN_POINT('Ctrl Pts',(4.05538676699994,2.2,-0.480776208000013));
#347057=CARTESIAN_POINT('Ctrl Pts',(4.05643078799994,12.2,-0.480678780000012));
#347058=CARTESIAN_POINT('Ctrl Pts',(4.05643078799994,5.2,-0.480678780000012));
#347059=CARTESIAN_POINT('Ctrl Pts',(4.05643078799994,2.2,-0.480678780000012));
#347060=CARTESIAN_POINT('Ctrl Pts',(4.05748006299994,12.2,-0.480579565000014));
#347061=CARTESIAN_POINT('Ctrl Pts',(4.05748006299994,5.2,-0.480579565000014));
#347062=CARTESIAN_POINT('Ctrl Pts',(4.05748006299994,2.2,-0.480579565000014));
#347063=CARTESIAN_POINT('Ctrl Pts',(4.05853458199994,12.2,-0.480478550000014));
#347064=CARTESIAN_POINT('Ctrl Pts',(4.05853458199994,5.2,-0.480478550000014));
#347065=CARTESIAN_POINT('Ctrl Pts',(4.05853458199994,2.2,-0.480478550000014));
#347066=CARTESIAN_POINT('Ctrl Pts',(4.05959433099994,12.2,-0.480375726000015));
#347067=CARTESIAN_POINT('Ctrl Pts',(4.05959433099994,5.2,-0.480375726000015));
#347068=CARTESIAN_POINT('Ctrl Pts',(4.05959433099994,2.2,-0.480375726000015));
#347069=CARTESIAN_POINT('Ctrl Pts',(4.06065929999994,12.2,-0.480271080000012));
#347070=CARTESIAN_POINT('Ctrl Pts',(4.06065929999994,5.2,-0.480271080000012));
#347071=CARTESIAN_POINT('Ctrl Pts',(4.06065929999994,2.2,-0.480271080000012));
#347072=CARTESIAN_POINT('Ctrl Pts',(4.06172947699995,12.2,-0.480164600000013));
#347073=CARTESIAN_POINT('Ctrl Pts',(4.06172947699995,5.2,-0.480164600000013));
#347074=CARTESIAN_POINT('Ctrl Pts',(4.06172947699995,2.2,-0.480164600000013));
#347075=CARTESIAN_POINT('Ctrl Pts',(4.06280485199995,12.2,-0.480056278000016));
#347076=CARTESIAN_POINT('Ctrl Pts',(4.06280485199995,5.2,-0.480056278000016));
#347077=CARTESIAN_POINT('Ctrl Pts',(4.06280485199995,2.2,-0.480056278000016));
#347078=CARTESIAN_POINT('Ctrl Pts',(4.06388541099994,12.2,-0.479946099000017));
#347079=CARTESIAN_POINT('Ctrl Pts',(4.06388541099994,5.2,-0.479946099000017));
#347080=CARTESIAN_POINT('Ctrl Pts',(4.06388541099994,2.2,-0.479946099000017));
#347081=CARTESIAN_POINT('Ctrl Pts',(4.06497114499994,12.2,-0.479834053000014));
#347082=CARTESIAN_POINT('Ctrl Pts',(4.06497114499994,5.2,-0.479834053000014));
#347083=CARTESIAN_POINT('Ctrl Pts',(4.06497114499994,2.2,-0.479834053000014));
#347084=CARTESIAN_POINT('Ctrl Pts',(4.06606203999995,12.2,-0.479720131000012));
#347085=CARTESIAN_POINT('Ctrl Pts',(4.06606203999995,5.2,-0.479720131000012));
#347086=CARTESIAN_POINT('Ctrl Pts',(4.06606203999995,2.2,-0.479720131000012));
#347087=CARTESIAN_POINT('Ctrl Pts',(4.06715808699994,12.2,-0.479604318000018));
#347088=CARTESIAN_POINT('Ctrl Pts',(4.06715808699994,5.2,-0.479604318000018));
#347089=CARTESIAN_POINT('Ctrl Pts',(4.06715808699994,2.2,-0.479604318000018));
#347090=CARTESIAN_POINT('Ctrl Pts',(4.06825927299994,12.2,-0.479486607000013));
#347091=CARTESIAN_POINT('Ctrl Pts',(4.06825927299994,5.2,-0.479486607000013));
#347092=CARTESIAN_POINT('Ctrl Pts',(4.06825927299994,2.2,-0.479486607000013));
#347093=CARTESIAN_POINT('Ctrl Pts',(4.06936558599994,12.2,-0.479366984000014));
#347094=CARTESIAN_POINT('Ctrl Pts',(4.06936558599994,5.2,-0.479366984000014));
#347095=CARTESIAN_POINT('Ctrl Pts',(4.06936558599994,2.2,-0.479366984000014));
#347096=CARTESIAN_POINT('Ctrl Pts',(4.07047701699994,12.2,-0.479245440000016));
#347097=CARTESIAN_POINT('Ctrl Pts',(4.07047701699994,5.2,-0.479245440000016));
#347098=CARTESIAN_POINT('Ctrl Pts',(4.07047701699994,2.2,-0.479245440000016));
#347099=CARTESIAN_POINT('Ctrl Pts',(4.07159355199994,12.2,-0.479121962000013));
#347100=CARTESIAN_POINT('Ctrl Pts',(4.07159355199994,5.2,-0.479121962000013));
#347101=CARTESIAN_POINT('Ctrl Pts',(4.07159355199994,2.2,-0.479121962000013));
#347102=CARTESIAN_POINT('Ctrl Pts',(4.07271518199994,12.2,-0.478996541000014));
#347103=CARTESIAN_POINT('Ctrl Pts',(4.07271518199994,5.2,-0.478996541000014));
#347104=CARTESIAN_POINT('Ctrl Pts',(4.07271518199994,2.2,-0.478996541000014));
#347105=CARTESIAN_POINT('Ctrl Pts',(4.07384189399994,12.2,-0.478869166000013));
#347106=CARTESIAN_POINT('Ctrl Pts',(4.07384189399994,5.2,-0.478869166000013));
#347107=CARTESIAN_POINT('Ctrl Pts',(4.07384189399994,2.2,-0.478869166000013));
#347108=CARTESIAN_POINT('Ctrl Pts',(4.07497367699994,12.2,-0.478739825000014));
#347109=CARTESIAN_POINT('Ctrl Pts',(4.07497367699994,5.2,-0.478739825000014));
#347110=CARTESIAN_POINT('Ctrl Pts',(4.07497367699994,2.2,-0.478739825000014));
#347111=CARTESIAN_POINT('Ctrl Pts',(4.07611051999995,12.2,-0.478608507000011));
#347112=CARTESIAN_POINT('Ctrl Pts',(4.07611051999995,5.2,-0.478608507000011));
#347113=CARTESIAN_POINT('Ctrl Pts',(4.07611051999995,2.2,-0.478608507000011));
#347114=CARTESIAN_POINT('Ctrl Pts',(4.07725240999994,12.2,-0.478475202000013));
#347115=CARTESIAN_POINT('Ctrl Pts',(4.07725240999994,5.2,-0.478475202000013));
#347116=CARTESIAN_POINT('Ctrl Pts',(4.07725240999994,2.2,-0.478475202000013));
#347117=CARTESIAN_POINT('Ctrl Pts',(4.07839933899994,12.2,-0.478339900000013));
#347118=CARTESIAN_POINT('Ctrl Pts',(4.07839933899994,5.2,-0.478339900000013));
#347119=CARTESIAN_POINT('Ctrl Pts',(4.07839933899994,2.2,-0.478339900000013));
#347120=CARTESIAN_POINT('Ctrl Pts',(4.07955129299994,12.2,-0.478202590000016));
#347121=CARTESIAN_POINT('Ctrl Pts',(4.07955129299994,5.2,-0.478202590000016));
#347122=CARTESIAN_POINT('Ctrl Pts',(4.07955129299994,2.2,-0.478202590000016));
#347123=CARTESIAN_POINT('Ctrl Pts',(4.08070826099994,12.2,-0.478063260000017));
#347124=CARTESIAN_POINT('Ctrl Pts',(4.08070826099994,5.2,-0.478063260000017));
#347125=CARTESIAN_POINT('Ctrl Pts',(4.08070826099994,2.2,-0.478063260000017));
#347126=CARTESIAN_POINT('Ctrl Pts',(4.08187023299995,12.2,-0.477921902000014));
#347127=CARTESIAN_POINT('Ctrl Pts',(4.08187023299995,5.2,-0.477921902000014));
#347128=CARTESIAN_POINT('Ctrl Pts',(4.08187023299995,2.2,-0.477921902000014));
#347129=CARTESIAN_POINT('Ctrl Pts',(4.08303719699994,12.2,-0.477778502000015));
#347130=CARTESIAN_POINT('Ctrl Pts',(4.08303719699994,5.2,-0.477778502000015));
#347131=CARTESIAN_POINT('Ctrl Pts',(4.08303719699994,2.2,-0.477778502000015));
#347132=CARTESIAN_POINT('Ctrl Pts',(4.08420914199994,12.2,-0.477633053000015));
#347133=CARTESIAN_POINT('Ctrl Pts',(4.08420914199994,5.2,-0.477633053000015));
#347134=CARTESIAN_POINT('Ctrl Pts',(4.08420914199994,2.2,-0.477633053000015));
#347135=CARTESIAN_POINT('Ctrl Pts',(4.08538605599994,12.2,-0.477485542000018));
#347136=CARTESIAN_POINT('Ctrl Pts',(4.08538605599994,5.2,-0.477485542000018));
#347137=CARTESIAN_POINT('Ctrl Pts',(4.08538605599994,2.2,-0.477485542000018));
#347138=CARTESIAN_POINT('Ctrl Pts',(4.08656792799994,12.2,-0.477335960000014));
#347139=CARTESIAN_POINT('Ctrl Pts',(4.08656792799994,5.2,-0.477335960000014));
#347140=CARTESIAN_POINT('Ctrl Pts',(4.08656792799994,2.2,-0.477335960000014));
#347141=CARTESIAN_POINT('Ctrl Pts',(4.08775474699994,12.2,-0.477184296000015));
#347142=CARTESIAN_POINT('Ctrl Pts',(4.08775474699994,5.2,-0.477184296000015));
#347143=CARTESIAN_POINT('Ctrl Pts',(4.08775474699994,2.2,-0.477184296000015));
#347144=CARTESIAN_POINT('Ctrl Pts',(4.08894650199994,12.2,-0.477030541000012));
#347145=CARTESIAN_POINT('Ctrl Pts',(4.08894650199994,5.2,-0.477030541000012));
#347146=CARTESIAN_POINT('Ctrl Pts',(4.08894650199994,2.2,-0.477030541000012));
#347147=CARTESIAN_POINT('Ctrl Pts',(4.09014318199994,12.2,-0.476874682000012));
#347148=CARTESIAN_POINT('Ctrl Pts',(4.09014318199994,5.2,-0.476874682000012));
#347149=CARTESIAN_POINT('Ctrl Pts',(4.09014318199994,2.2,-0.476874682000012));
#347150=CARTESIAN_POINT('Ctrl Pts',(4.09134477499994,12.2,-0.476716711000016));
#347151=CARTESIAN_POINT('Ctrl Pts',(4.09134477499994,5.2,-0.476716711000016));
#347152=CARTESIAN_POINT('Ctrl Pts',(4.09134477499994,2.2,-0.476716711000016));
#347153=CARTESIAN_POINT('Ctrl Pts',(4.09255126999994,12.2,-0.476556616000017));
#347154=CARTESIAN_POINT('Ctrl Pts',(4.09255126999994,5.2,-0.476556616000017));
#347155=CARTESIAN_POINT('Ctrl Pts',(4.09255126999994,2.2,-0.476556616000017));
#347156=CARTESIAN_POINT('Ctrl Pts',(4.09376265599994,12.2,-0.476394388000014));
#347157=CARTESIAN_POINT('Ctrl Pts',(4.09376265599994,5.2,-0.476394388000014));
#347158=CARTESIAN_POINT('Ctrl Pts',(4.09376265599994,2.2,-0.476394388000014));
#347159=CARTESIAN_POINT('Ctrl Pts',(4.09497892299994,12.2,-0.476230018000017));
#347160=CARTESIAN_POINT('Ctrl Pts',(4.09497892299994,5.2,-0.476230018000017));
#347161=CARTESIAN_POINT('Ctrl Pts',(4.09497892299994,2.2,-0.476230018000017));
#347162=CARTESIAN_POINT('Ctrl Pts',(4.09620005699994,12.2,-0.476063493000014));
#347163=CARTESIAN_POINT('Ctrl Pts',(4.09620005699994,5.2,-0.476063493000014));
#347164=CARTESIAN_POINT('Ctrl Pts',(4.09620005699994,2.2,-0.476063493000014));
#347165=CARTESIAN_POINT('Ctrl Pts',(4.09742605099995,12.2,-0.475894805000014));
#347166=CARTESIAN_POINT('Ctrl Pts',(4.09742605099995,5.2,-0.475894805000014));
#347167=CARTESIAN_POINT('Ctrl Pts',(4.09742605099995,2.2,-0.475894805000014));
#347168=CARTESIAN_POINT('Ctrl Pts',(4.09865689099994,12.2,-0.475723944000013));
#347169=CARTESIAN_POINT('Ctrl Pts',(4.09865689099994,5.2,-0.475723944000013));
#347170=CARTESIAN_POINT('Ctrl Pts',(4.09865689099994,2.2,-0.475723944000013));
#347171=CARTESIAN_POINT('Ctrl Pts',(4.09989256499994,12.2,-0.475550898000012));
#347172=CARTESIAN_POINT('Ctrl Pts',(4.09989256499994,5.2,-0.475550898000012));
#347173=CARTESIAN_POINT('Ctrl Pts',(4.09989256499994,2.2,-0.475550898000012));
#347174=CARTESIAN_POINT('Ctrl Pts',(4.10113306499994,12.2,-0.475375660000013));
#347175=CARTESIAN_POINT('Ctrl Pts',(4.10113306499994,5.2,-0.475375660000013));
#347176=CARTESIAN_POINT('Ctrl Pts',(4.10113306499994,2.2,-0.475375660000013));
#347177=CARTESIAN_POINT('Ctrl Pts',(4.10237837799994,12.2,-0.475198217000017));
#347178=CARTESIAN_POINT('Ctrl Pts',(4.10237837799994,5.2,-0.475198217000017));
#347179=CARTESIAN_POINT('Ctrl Pts',(4.10237837799994,2.2,-0.475198217000017));
#347180=CARTESIAN_POINT('Ctrl Pts',(4.10362849299994,12.2,-0.475018562000016));
#347181=CARTESIAN_POINT('Ctrl Pts',(4.10362849299994,5.2,-0.475018562000016));
#347182=CARTESIAN_POINT('Ctrl Pts',(4.10362849299994,2.2,-0.475018562000016));
#347183=CARTESIAN_POINT('Ctrl Pts',(4.10488339999994,12.2,-0.474836683000017));
#347184=CARTESIAN_POINT('Ctrl Pts',(4.10488339999994,5.2,-0.474836683000017));
#347185=CARTESIAN_POINT('Ctrl Pts',(4.10488339999994,2.2,-0.474836683000017));
#347186=CARTESIAN_POINT('Ctrl Pts',(4.10614308599994,12.2,-0.474652570000016));
#347187=CARTESIAN_POINT('Ctrl Pts',(4.10614308599994,5.2,-0.474652570000016));
#347188=CARTESIAN_POINT('Ctrl Pts',(4.10614308599994,2.2,-0.474652570000016));
#347189=CARTESIAN_POINT('Ctrl Pts',(4.10740754199994,12.2,-0.474466215000016));
#347190=CARTESIAN_POINT('Ctrl Pts',(4.10740754199994,5.2,-0.474466215000016));
#347191=CARTESIAN_POINT('Ctrl Pts',(4.10740754199994,2.2,-0.474466215000016));
#347192=CARTESIAN_POINT('Ctrl Pts',(4.10867675699994,12.2,-0.474277608000016));
#347193=CARTESIAN_POINT('Ctrl Pts',(4.10867675699994,5.2,-0.474277608000016));
#347194=CARTESIAN_POINT('Ctrl Pts',(4.10867675699994,2.2,-0.474277608000016));
#347195=CARTESIAN_POINT('Ctrl Pts',(4.10995071699995,12.2,-0.474086738000015));
#347196=CARTESIAN_POINT('Ctrl Pts',(4.10995071699995,5.2,-0.474086738000015));
#347197=CARTESIAN_POINT('Ctrl Pts',(4.10995071699995,2.2,-0.474086738000015));
#347198=CARTESIAN_POINT('Ctrl Pts',(4.11122941499994,12.2,-0.473893597000017));
#347199=CARTESIAN_POINT('Ctrl Pts',(4.11122941499994,5.2,-0.473893597000017));
#347200=CARTESIAN_POINT('Ctrl Pts',(4.11122941499994,2.2,-0.473893597000017));
#347201=CARTESIAN_POINT('Ctrl Pts',(4.11251283799994,12.2,-0.473698173000017));
#347202=CARTESIAN_POINT('Ctrl Pts',(4.11251283799994,5.2,-0.473698173000017));
#347203=CARTESIAN_POINT('Ctrl Pts',(4.11251283799994,2.2,-0.473698173000017));
#347204=CARTESIAN_POINT('Ctrl Pts',(4.11380097599995,12.2,-0.473500458000018));
#347205=CARTESIAN_POINT('Ctrl Pts',(4.11380097599995,5.2,-0.473500458000018));
#347206=CARTESIAN_POINT('Ctrl Pts',(4.11380097599995,2.2,-0.473500458000018));
#347207=CARTESIAN_POINT('Ctrl Pts',(4.11509381599994,12.2,-0.473300442000015));
#347208=CARTESIAN_POINT('Ctrl Pts',(4.11509381599994,5.2,-0.473300442000015));
#347209=CARTESIAN_POINT('Ctrl Pts',(4.11509381599994,2.2,-0.473300442000015));
#347210=CARTESIAN_POINT('Ctrl Pts',(4.11639134899994,12.2,-0.473098116000017));
#347211=CARTESIAN_POINT('Ctrl Pts',(4.11639134899994,5.2,-0.473098116000017));
#347212=CARTESIAN_POINT('Ctrl Pts',(4.11639134899994,2.2,-0.473098116000017));
#347213=CARTESIAN_POINT('Ctrl Pts',(4.11769356299994,12.2,-0.472893470000013));
#347214=CARTESIAN_POINT('Ctrl Pts',(4.11769356299994,5.2,-0.472893470000013));
#347215=CARTESIAN_POINT('Ctrl Pts',(4.11769356299994,2.2,-0.472893470000013));
#347216=CARTESIAN_POINT('Ctrl Pts',(4.11900044799994,12.2,-0.472686494000012));
#347217=CARTESIAN_POINT('Ctrl Pts',(4.11900044799994,5.2,-0.472686494000012));
#347218=CARTESIAN_POINT('Ctrl Pts',(4.11900044799994,2.2,-0.472686494000012));
#347219=CARTESIAN_POINT('Ctrl Pts',(4.12031199199994,12.2,-0.472477180000013));
#347220=CARTESIAN_POINT('Ctrl Pts',(4.12031199199994,5.2,-0.472477180000013));
#347221=CARTESIAN_POINT('Ctrl Pts',(4.12031199199994,2.2,-0.472477180000013));
#347222=CARTESIAN_POINT('Ctrl Pts',(4.12162818599994,12.2,-0.472265517000015));
#347223=CARTESIAN_POINT('Ctrl Pts',(4.12162818599994,5.2,-0.472265517000015));
#347224=CARTESIAN_POINT('Ctrl Pts',(4.12162818599994,2.2,-0.472265517000015));
#347225=CARTESIAN_POINT('Ctrl Pts',(4.12294901699994,12.2,-0.472051498000017));
#347226=CARTESIAN_POINT('Ctrl Pts',(4.12294901699994,5.2,-0.472051498000017));
#347227=CARTESIAN_POINT('Ctrl Pts',(4.12294901699994,2.2,-0.472051498000017));
#347228=CARTESIAN_POINT('Ctrl Pts',(4.12427447499994,12.2,-0.471835110000014));
#347229=CARTESIAN_POINT('Ctrl Pts',(4.12427447499994,5.2,-0.471835110000014));
#347230=CARTESIAN_POINT('Ctrl Pts',(4.12427447499994,2.2,-0.471835110000014));
#347231=CARTESIAN_POINT('Ctrl Pts',(4.12560454899995,12.2,-0.471616347000015));
#347232=CARTESIAN_POINT('Ctrl Pts',(4.12560454899995,5.2,-0.471616347000015));
#347233=CARTESIAN_POINT('Ctrl Pts',(4.12560454899995,2.2,-0.471616347000015));
#347234=CARTESIAN_POINT('Ctrl Pts',(4.12693922899994,12.2,-0.471395199000018));
#347235=CARTESIAN_POINT('Ctrl Pts',(4.12693922899994,5.2,-0.471395199000018));
#347236=CARTESIAN_POINT('Ctrl Pts',(4.12693922899994,2.2,-0.471395199000018));
#347237=CARTESIAN_POINT('Ctrl Pts',(4.12827850199994,12.2,-0.471171656000013));
#347238=CARTESIAN_POINT('Ctrl Pts',(4.12827850199994,5.2,-0.471171656000013));
#347239=CARTESIAN_POINT('Ctrl Pts',(4.12827850199994,2.2,-0.471171656000013));
#347240=CARTESIAN_POINT('Ctrl Pts',(4.12962235999994,12.2,-0.470945710000015));
#347241=CARTESIAN_POINT('Ctrl Pts',(4.12962235999994,5.2,-0.470945710000015));
#347242=CARTESIAN_POINT('Ctrl Pts',(4.12962235999994,2.2,-0.470945710000015));
#347243=CARTESIAN_POINT('Ctrl Pts',(4.13097078999995,12.2,-0.470717349000012));
#347244=CARTESIAN_POINT('Ctrl Pts',(4.13097078999995,5.2,-0.470717349000012));
#347245=CARTESIAN_POINT('Ctrl Pts',(4.13097078999995,2.2,-0.470717349000012));
#347246=CARTESIAN_POINT('Ctrl Pts',(4.13232378199995,12.2,-0.470486567000012));
#347247=CARTESIAN_POINT('Ctrl Pts',(4.13232378199995,5.2,-0.470486567000012));
#347248=CARTESIAN_POINT('Ctrl Pts',(4.13232378199995,2.2,-0.470486567000012));
#347249=CARTESIAN_POINT('Ctrl Pts',(4.13368132599994,12.2,-0.470253354000012));
#347250=CARTESIAN_POINT('Ctrl Pts',(4.13368132599994,5.2,-0.470253354000012));
#347251=CARTESIAN_POINT('Ctrl Pts',(4.13368132599994,2.2,-0.470253354000012));
#347252=CARTESIAN_POINT('Ctrl Pts',(4.13504340999994,12.2,-0.470017700000014));
#347253=CARTESIAN_POINT('Ctrl Pts',(4.13504340999994,5.2,-0.470017700000014));
#347254=CARTESIAN_POINT('Ctrl Pts',(4.13504340999994,2.2,-0.470017700000014));
#347255=CARTESIAN_POINT('Ctrl Pts',(4.13641002299994,12.2,-0.469779598000013));
#347256=CARTESIAN_POINT('Ctrl Pts',(4.13641002299994,5.2,-0.469779598000013));
#347257=CARTESIAN_POINT('Ctrl Pts',(4.13641002299994,2.2,-0.469779598000013));
#347258=CARTESIAN_POINT('Ctrl Pts',(4.13778115599994,12.2,-0.469539037000013));
#347259=CARTESIAN_POINT('Ctrl Pts',(4.13778115599994,5.2,-0.469539037000013));
#347260=CARTESIAN_POINT('Ctrl Pts',(4.13778115599994,2.2,-0.469539037000013));
#347261=CARTESIAN_POINT('Ctrl Pts',(4.13915679599994,12.2,-0.469296008000013));
#347262=CARTESIAN_POINT('Ctrl Pts',(4.13915679599994,5.2,-0.469296008000013));
#347263=CARTESIAN_POINT('Ctrl Pts',(4.13915679599994,2.2,-0.469296008000013));
#347264=CARTESIAN_POINT('Ctrl Pts',(4.14053693499994,12.2,-0.469050504000013));
#347265=CARTESIAN_POINT('Ctrl Pts',(4.14053693499994,5.2,-0.469050504000013));
#347266=CARTESIAN_POINT('Ctrl Pts',(4.14053693499994,2.2,-0.469050504000013));
#347267=CARTESIAN_POINT('Ctrl Pts',(4.14192155899994,12.2,-0.468802514000015));
#347268=CARTESIAN_POINT('Ctrl Pts',(4.14192155899994,5.2,-0.468802514000015));
#347269=CARTESIAN_POINT('Ctrl Pts',(4.14192155899994,2.2,-0.468802514000015));
#347270=CARTESIAN_POINT('Ctrl Pts',(4.14331065899994,12.2,-0.468552031000016));
#347271=CARTESIAN_POINT('Ctrl Pts',(4.14331065899994,5.2,-0.468552031000016));
#347272=CARTESIAN_POINT('Ctrl Pts',(4.14331065899994,2.2,-0.468552031000016));
#347273=CARTESIAN_POINT('Ctrl Pts',(4.14470422499994,12.2,-0.468299046000014));
#347274=CARTESIAN_POINT('Ctrl Pts',(4.14470422499994,5.2,-0.468299046000014));
#347275=CARTESIAN_POINT('Ctrl Pts',(4.14470422499994,2.2,-0.468299046000014));
#347276=CARTESIAN_POINT('Ctrl Pts',(4.14610224599994,12.2,-0.468043548000012));
#347277=CARTESIAN_POINT('Ctrl Pts',(4.14610224599994,5.2,-0.468043548000012));
#347278=CARTESIAN_POINT('Ctrl Pts',(4.14610224599994,2.2,-0.468043548000012));
#347279=CARTESIAN_POINT('Ctrl Pts',(4.14750470899994,12.2,-0.467785530000011));
#347280=CARTESIAN_POINT('Ctrl Pts',(4.14750470899994,5.2,-0.467785530000011));
#347281=CARTESIAN_POINT('Ctrl Pts',(4.14750470899994,2.2,-0.467785530000011));
#347282=CARTESIAN_POINT('Ctrl Pts',(4.14891160699994,12.2,-0.467524983000014));
#347283=CARTESIAN_POINT('Ctrl Pts',(4.14891160699994,5.2,-0.467524983000014));
#347284=CARTESIAN_POINT('Ctrl Pts',(4.14891160699994,2.2,-0.467524983000014));
#347285=CARTESIAN_POINT('Ctrl Pts',(4.15032292699994,12.2,-0.467261899000011));
#347286=CARTESIAN_POINT('Ctrl Pts',(4.15032292699994,5.2,-0.467261899000011));
#347287=CARTESIAN_POINT('Ctrl Pts',(4.15032292699994,2.2,-0.467261899000011));
#347288=CARTESIAN_POINT('Ctrl Pts',(4.15173865799995,12.2,-0.466996269000015));
#347289=CARTESIAN_POINT('Ctrl Pts',(4.15173865799995,5.2,-0.466996269000015));
#347290=CARTESIAN_POINT('Ctrl Pts',(4.15173865799995,2.2,-0.466996269000015));
#347291=CARTESIAN_POINT('Ctrl Pts',(4.15315879199994,12.2,-0.466728082000016));
#347292=CARTESIAN_POINT('Ctrl Pts',(4.15315879199994,5.2,-0.466728082000016));
#347293=CARTESIAN_POINT('Ctrl Pts',(4.15315879199994,2.2,-0.466728082000016));
#347294=CARTESIAN_POINT('Ctrl Pts',(4.15458331499994,12.2,-0.466457333000014));
#347295=CARTESIAN_POINT('Ctrl Pts',(4.15458331499994,5.2,-0.466457333000014));
#347296=CARTESIAN_POINT('Ctrl Pts',(4.15458331499994,2.2,-0.466457333000014));
#347297=CARTESIAN_POINT('Ctrl Pts',(4.15601221799994,12.2,-0.466184012000017));
#347298=CARTESIAN_POINT('Ctrl Pts',(4.15601221799994,5.2,-0.466184012000017));
#347299=CARTESIAN_POINT('Ctrl Pts',(4.15601221799994,2.2,-0.466184012000017));
#347300=CARTESIAN_POINT('Ctrl Pts',(4.15744549099994,12.2,-0.465908110000015));
#347301=CARTESIAN_POINT('Ctrl Pts',(4.15744549099994,5.2,-0.465908110000015));
#347302=CARTESIAN_POINT('Ctrl Pts',(4.15744549099994,2.2,-0.465908110000015));
#347303=CARTESIAN_POINT('Ctrl Pts',(4.15888312199994,12.2,-0.465629618000012));
#347304=CARTESIAN_POINT('Ctrl Pts',(4.15888312199994,5.2,-0.465629618000012));
#347305=CARTESIAN_POINT('Ctrl Pts',(4.15888312199994,2.2,-0.465629618000012));
#347306=CARTESIAN_POINT('Ctrl Pts',(4.16032510199994,12.2,-0.465348529000016));
#347307=CARTESIAN_POINT('Ctrl Pts',(4.16032510199994,5.2,-0.465348529000016));
#347308=CARTESIAN_POINT('Ctrl Pts',(4.16032510199994,2.2,-0.465348529000016));
#347309=CARTESIAN_POINT('Ctrl Pts',(4.16177141899994,12.2,-0.465064834000017));
#347310=CARTESIAN_POINT('Ctrl Pts',(4.16177141899994,5.2,-0.465064834000017));
#347311=CARTESIAN_POINT('Ctrl Pts',(4.16177141899994,2.2,-0.465064834000017));
#347312=CARTESIAN_POINT('Ctrl Pts',(4.16322206499994,12.2,-0.464778525000016));
#347313=CARTESIAN_POINT('Ctrl Pts',(4.16322206499994,5.2,-0.464778525000016));
#347314=CARTESIAN_POINT('Ctrl Pts',(4.16322206499994,2.2,-0.464778525000016));
#347315=CARTESIAN_POINT('Ctrl Pts',(4.16467702499994,12.2,-0.464489593000015));
#347316=CARTESIAN_POINT('Ctrl Pts',(4.16467702499994,5.2,-0.464489593000015));
#347317=CARTESIAN_POINT('Ctrl Pts',(4.16467702499994,2.2,-0.464489593000015));
#347318=CARTESIAN_POINT('Ctrl Pts',(4.16613629199994,12.2,-0.464198030000014));
#347319=CARTESIAN_POINT('Ctrl Pts',(4.16613629199994,5.2,-0.464198030000014));
#347320=CARTESIAN_POINT('Ctrl Pts',(4.16613629199994,2.2,-0.464198030000014));
#347321=CARTESIAN_POINT('Ctrl Pts',(4.16759985399994,12.2,-0.463903826000016));
#347322=CARTESIAN_POINT('Ctrl Pts',(4.16759985399994,5.2,-0.463903826000016));
#347323=CARTESIAN_POINT('Ctrl Pts',(4.16759985399994,2.2,-0.463903826000016));
#347324=CARTESIAN_POINT('Ctrl Pts',(4.16906769999995,12.2,-0.463606975000013));
#347325=CARTESIAN_POINT('Ctrl Pts',(4.16906769999995,5.2,-0.463606975000013));
#347326=CARTESIAN_POINT('Ctrl Pts',(4.16906769999995,2.2,-0.463606975000013));
#347327=CARTESIAN_POINT('Ctrl Pts',(4.17053982099994,12.2,-0.463307468000016));
#347328=CARTESIAN_POINT('Ctrl Pts',(4.17053982099994,5.2,-0.463307468000016));
#347329=CARTESIAN_POINT('Ctrl Pts',(4.17053982099994,2.2,-0.463307468000016));
#347330=CARTESIAN_POINT('Ctrl Pts',(4.17201620699994,12.2,-0.463005298000017));
#347331=CARTESIAN_POINT('Ctrl Pts',(4.17201620699994,5.2,-0.463005298000017));
#347332=CARTESIAN_POINT('Ctrl Pts',(4.17201620699994,2.2,-0.463005298000017));
#347333=CARTESIAN_POINT('Ctrl Pts',(4.17349684399994,12.2,-0.462700453000018));
#347334=CARTESIAN_POINT('Ctrl Pts',(4.17349684399994,5.2,-0.462700453000018));
#347335=CARTESIAN_POINT('Ctrl Pts',(4.17349684399994,2.2,-0.462700453000018));
#347336=CARTESIAN_POINT('Ctrl Pts',(4.17498172499995,12.2,-0.462392929000015));
#347337=CARTESIAN_POINT('Ctrl Pts',(4.17498172499995,5.2,-0.462392929000015));
#347338=CARTESIAN_POINT('Ctrl Pts',(4.17498172499995,2.2,-0.462392929000015));
#347339=CARTESIAN_POINT('Ctrl Pts',(4.17647083799995,12.2,-0.462082716000012));
#347340=CARTESIAN_POINT('Ctrl Pts',(4.17647083799995,5.2,-0.462082716000012));
#347341=CARTESIAN_POINT('Ctrl Pts',(4.17647083799995,2.2,-0.462082716000012));
#347342=CARTESIAN_POINT('Ctrl Pts',(4.17796417399994,12.2,-0.461769807000016));
#347343=CARTESIAN_POINT('Ctrl Pts',(4.17796417399994,5.2,-0.461769807000016));
#347344=CARTESIAN_POINT('Ctrl Pts',(4.17796417399994,2.2,-0.461769807000016));
#347345=CARTESIAN_POINT('Ctrl Pts',(4.17946172099994,12.2,-0.461454192000015));
#347346=CARTESIAN_POINT('Ctrl Pts',(4.17946172099994,5.2,-0.461454192000015));
#347347=CARTESIAN_POINT('Ctrl Pts',(4.17946172099994,2.2,-0.461454192000015));
#347348=CARTESIAN_POINT('Ctrl Pts',(4.18096346899994,12.2,-0.461135864000015));
#347349=CARTESIAN_POINT('Ctrl Pts',(4.18096346899994,5.2,-0.461135864000015));
#347350=CARTESIAN_POINT('Ctrl Pts',(4.18096346899994,2.2,-0.461135864000015));
#347351=CARTESIAN_POINT('Ctrl Pts',(4.18246940699994,12.2,-0.460814815000017));
#347352=CARTESIAN_POINT('Ctrl Pts',(4.18246940699994,5.2,-0.460814815000017));
#347353=CARTESIAN_POINT('Ctrl Pts',(4.18246940699994,2.2,-0.460814815000017));
#347354=CARTESIAN_POINT('Ctrl Pts',(4.18397952499994,12.2,-0.460491039000015));
#347355=CARTESIAN_POINT('Ctrl Pts',(4.18397952499994,5.2,-0.460491039000015));
#347356=CARTESIAN_POINT('Ctrl Pts',(4.18397952499994,2.2,-0.460491039000015));
#347357=CARTESIAN_POINT('Ctrl Pts',(4.18549381299994,12.2,-0.460164523000017));
#347358=CARTESIAN_POINT('Ctrl Pts',(4.18549381299994,5.2,-0.460164523000017));
#347359=CARTESIAN_POINT('Ctrl Pts',(4.18549381299994,2.2,-0.460164523000017));
#347360=CARTESIAN_POINT('Ctrl Pts',(4.18701225999994,12.2,-0.459835264000015));
#347361=CARTESIAN_POINT('Ctrl Pts',(4.18701225999994,5.2,-0.459835264000015));
#347362=CARTESIAN_POINT('Ctrl Pts',(4.18701225999994,2.2,-0.459835264000015));
#347363=CARTESIAN_POINT('Ctrl Pts',(4.18853485599994,12.2,-0.459503253000015));
#347364=CARTESIAN_POINT('Ctrl Pts',(4.18853485599994,5.2,-0.459503253000015));
#347365=CARTESIAN_POINT('Ctrl Pts',(4.18853485599994,2.2,-0.459503253000015));
#347366=CARTESIAN_POINT('Ctrl Pts',(4.19006159099994,12.2,-0.459168479000014));
#347367=CARTESIAN_POINT('Ctrl Pts',(4.19006159099994,5.2,-0.459168479000014));
#347368=CARTESIAN_POINT('Ctrl Pts',(4.19006159099994,2.2,-0.459168479000014));
#347369=CARTESIAN_POINT('Ctrl Pts',(4.19159245399995,12.2,-0.458830938000014));
#347370=CARTESIAN_POINT('Ctrl Pts',(4.19159245399995,5.2,-0.458830938000014));
#347371=CARTESIAN_POINT('Ctrl Pts',(4.19159245399995,2.2,-0.458830938000014));
#347372=CARTESIAN_POINT('Ctrl Pts',(4.19312743399994,12.2,-0.458490621000016));
#347373=CARTESIAN_POINT('Ctrl Pts',(4.19312743399994,5.2,-0.458490621000016));
#347374=CARTESIAN_POINT('Ctrl Pts',(4.19312743399994,2.2,-0.458490621000016));
#347375=CARTESIAN_POINT('Ctrl Pts',(4.19466652199994,12.2,-0.458147520000014));
#347376=CARTESIAN_POINT('Ctrl Pts',(4.19466652199994,5.2,-0.458147520000014));
#347377=CARTESIAN_POINT('Ctrl Pts',(4.19466652199994,2.2,-0.458147520000014));
#347378=CARTESIAN_POINT('Ctrl Pts',(4.19620970699994,12.2,-0.457801626000016));
#347379=CARTESIAN_POINT('Ctrl Pts',(4.19620970699994,5.2,-0.457801626000016));
#347380=CARTESIAN_POINT('Ctrl Pts',(4.19620970699994,2.2,-0.457801626000016));
#347381=CARTESIAN_POINT('Ctrl Pts',(4.19775697799994,12.2,-0.457452935000013));
#347382=CARTESIAN_POINT('Ctrl Pts',(4.19775697799994,5.2,-0.457452935000013));
#347383=CARTESIAN_POINT('Ctrl Pts',(4.19775697799994,2.2,-0.457452935000013));
#347384=CARTESIAN_POINT('Ctrl Pts',(4.19930832699994,12.2,-0.457101434000013));
#347385=CARTESIAN_POINT('Ctrl Pts',(4.19930832699994,5.2,-0.457101434000013));
#347386=CARTESIAN_POINT('Ctrl Pts',(4.19930832699994,2.2,-0.457101434000013));
#347387=CARTESIAN_POINT('Ctrl Pts',(4.20086373999994,12.2,-0.456747121000016));
#347388=CARTESIAN_POINT('Ctrl Pts',(4.20086373999994,5.2,-0.456747121000016));
#347389=CARTESIAN_POINT('Ctrl Pts',(4.20086373999994,2.2,-0.456747121000016));
#347390=CARTESIAN_POINT('Ctrl Pts',(4.20242320999995,12.2,-0.456389984000012));
#347391=CARTESIAN_POINT('Ctrl Pts',(4.20242320999995,5.2,-0.456389984000012));
#347392=CARTESIAN_POINT('Ctrl Pts',(4.20242320999995,2.2,-0.456389984000012));
#347393=CARTESIAN_POINT('Ctrl Pts',(4.20398672499994,12.2,-0.456030016000017));
#347394=CARTESIAN_POINT('Ctrl Pts',(4.20398672499994,5.2,-0.456030016000017));
#347395=CARTESIAN_POINT('Ctrl Pts',(4.20398672499994,2.2,-0.456030016000017));
#347396=CARTESIAN_POINT('Ctrl Pts',(4.20555427599994,12.2,-0.455667212000015));
#347397=CARTESIAN_POINT('Ctrl Pts',(4.20555427599994,5.2,-0.455667212000015));
#347398=CARTESIAN_POINT('Ctrl Pts',(4.20555427599994,2.2,-0.455667212000015));
#347399=CARTESIAN_POINT('Ctrl Pts',(4.20712585099994,12.2,-0.455301563000017));
#347400=CARTESIAN_POINT('Ctrl Pts',(4.20712585099994,5.2,-0.455301563000017));
#347401=CARTESIAN_POINT('Ctrl Pts',(4.20712585099994,2.2,-0.455301563000017));
#347402=CARTESIAN_POINT('Ctrl Pts',(4.20870143999994,12.2,-0.454933060000013));
#347403=CARTESIAN_POINT('Ctrl Pts',(4.20870143999994,5.2,-0.454933060000013));
#347404=CARTESIAN_POINT('Ctrl Pts',(4.20870143999994,2.2,-0.454933060000013));
#347405=CARTESIAN_POINT('Ctrl Pts',(4.21028103499994,12.2,-0.454561698000013));
#347406=CARTESIAN_POINT('Ctrl Pts',(4.21028103499994,5.2,-0.454561698000013));
#347407=CARTESIAN_POINT('Ctrl Pts',(4.21028103499994,2.2,-0.454561698000013));
#347408=CARTESIAN_POINT('Ctrl Pts',(4.21186462299994,12.2,-0.454187467000011));
#347409=CARTESIAN_POINT('Ctrl Pts',(4.21186462299994,5.2,-0.454187467000011));
#347410=CARTESIAN_POINT('Ctrl Pts',(4.21186462299994,2.2,-0.454187467000011));
#347411=CARTESIAN_POINT('Ctrl Pts',(4.21345219499994,12.2,-0.453810363000016));
#347412=CARTESIAN_POINT('Ctrl Pts',(4.21345219499994,5.2,-0.453810363000016));
#347413=CARTESIAN_POINT('Ctrl Pts',(4.21345219499994,2.2,-0.453810363000016));
#347414=CARTESIAN_POINT('Ctrl Pts',(4.21504373999994,12.2,-0.453430375000017));
#347415=CARTESIAN_POINT('Ctrl Pts',(4.21504373999994,5.2,-0.453430375000017));
#347416=CARTESIAN_POINT('Ctrl Pts',(4.21504373999994,2.2,-0.453430375000017));
#347417=CARTESIAN_POINT('Ctrl Pts',(4.21663924899994,12.2,-0.453047497000014));
#347418=CARTESIAN_POINT('Ctrl Pts',(4.21663924899994,5.2,-0.453047497000014));
#347419=CARTESIAN_POINT('Ctrl Pts',(4.21663924899994,2.2,-0.453047497000014));
#347420=CARTESIAN_POINT('Ctrl Pts',(4.21823871099994,12.2,-0.452661723000016));
#347421=CARTESIAN_POINT('Ctrl Pts',(4.21823871099994,5.2,-0.452661723000016));
#347422=CARTESIAN_POINT('Ctrl Pts',(4.21823871099994,2.2,-0.452661723000016));
#347423=CARTESIAN_POINT('Ctrl Pts',(4.21984211599994,12.2,-0.452273044000013));
#347424=CARTESIAN_POINT('Ctrl Pts',(4.21984211599994,5.2,-0.452273044000013));
#347425=CARTESIAN_POINT('Ctrl Pts',(4.21984211599994,2.2,-0.452273044000013));
#347426=CARTESIAN_POINT('Ctrl Pts',(4.22144945399994,12.2,-0.451881453000014));
#347427=CARTESIAN_POINT('Ctrl Pts',(4.22144945399994,5.2,-0.451881453000014));
#347428=CARTESIAN_POINT('Ctrl Pts',(4.22144945399994,2.2,-0.451881453000014));
#347429=CARTESIAN_POINT('Ctrl Pts',(4.22306071499994,12.2,-0.451486943000017));
#347430=CARTESIAN_POINT('Ctrl Pts',(4.22306071499994,5.2,-0.451486943000017));
#347431=CARTESIAN_POINT('Ctrl Pts',(4.22306071499994,2.2,-0.451486943000017));
#347432=CARTESIAN_POINT('Ctrl Pts',(4.22467588799995,12.2,-0.451089507000013));
#347433=CARTESIAN_POINT('Ctrl Pts',(4.22467588799995,5.2,-0.451089507000013));
#347434=CARTESIAN_POINT('Ctrl Pts',(4.22467588799995,2.2,-0.451089507000013));
#347435=CARTESIAN_POINT('Ctrl Pts',(4.22629496199994,12.2,-0.450689138000016));
#347436=CARTESIAN_POINT('Ctrl Pts',(4.22629496199994,5.2,-0.450689138000016));
#347437=CARTESIAN_POINT('Ctrl Pts',(4.22629496199994,2.2,-0.450689138000016));
#347438=CARTESIAN_POINT('Ctrl Pts',(4.22791792999995,12.2,-0.450285826000014));
#347439=CARTESIAN_POINT('Ctrl Pts',(4.22791792999995,5.2,-0.450285826000014));
#347440=CARTESIAN_POINT('Ctrl Pts',(4.22791792999995,2.2,-0.450285826000014));
#347441=CARTESIAN_POINT('Ctrl Pts',(4.22954477799994,12.2,-0.449879568000018));
#347442=CARTESIAN_POINT('Ctrl Pts',(4.22954477799994,5.2,-0.449879568000018));
#347443=CARTESIAN_POINT('Ctrl Pts',(4.22954477799994,2.2,-0.449879568000018));
#347444=CARTESIAN_POINT('Ctrl Pts',(4.23117549899994,12.2,-0.449470355000017));
#347445=CARTESIAN_POINT('Ctrl Pts',(4.23117549899994,5.2,-0.449470355000017));
#347446=CARTESIAN_POINT('Ctrl Pts',(4.23117549899994,2.2,-0.449470355000017));
#347447=CARTESIAN_POINT('Ctrl Pts',(4.23281008199995,12.2,-0.449058180000015));
#347448=CARTESIAN_POINT('Ctrl Pts',(4.23281008199995,5.2,-0.449058180000015));
#347449=CARTESIAN_POINT('Ctrl Pts',(4.23281008199995,2.2,-0.449058180000015));
#347450=CARTESIAN_POINT('Ctrl Pts',(4.23444851499994,12.2,-0.448643035000016));
#347451=CARTESIAN_POINT('Ctrl Pts',(4.23444851499994,5.2,-0.448643035000016));
#347452=CARTESIAN_POINT('Ctrl Pts',(4.23444851499994,2.2,-0.448643035000016));
#347453=CARTESIAN_POINT('Ctrl Pts',(4.23609078999994,12.2,-0.448224914000015));
#347454=CARTESIAN_POINT('Ctrl Pts',(4.23609078999994,5.2,-0.448224914000015));
#347455=CARTESIAN_POINT('Ctrl Pts',(4.23609078999994,2.2,-0.448224914000015));
#347456=CARTESIAN_POINT('Ctrl Pts',(4.23773689699994,12.2,-0.447803810000016));
#347457=CARTESIAN_POINT('Ctrl Pts',(4.23773689699994,5.2,-0.447803810000016));
#347458=CARTESIAN_POINT('Ctrl Pts',(4.23773689699994,2.2,-0.447803810000016));
#347459=CARTESIAN_POINT('Ctrl Pts',(4.23938682399995,12.2,-0.447379715000018));
#347460=CARTESIAN_POINT('Ctrl Pts',(4.23938682399995,5.2,-0.447379715000018));
#347461=CARTESIAN_POINT('Ctrl Pts',(4.23938682399995,2.2,-0.447379715000018));
#347462=CARTESIAN_POINT('Ctrl Pts',(4.24104056399994,12.2,-0.446952624000012));
#347463=CARTESIAN_POINT('Ctrl Pts',(4.24104056399994,5.2,-0.446952624000012));
#347464=CARTESIAN_POINT('Ctrl Pts',(4.24104056399994,2.2,-0.446952624000012));
#347465=CARTESIAN_POINT('Ctrl Pts',(4.24269810399994,12.2,-0.446522529000015));
#347466=CARTESIAN_POINT('Ctrl Pts',(4.24269810399994,5.2,-0.446522529000015));
#347467=CARTESIAN_POINT('Ctrl Pts',(4.24269810399994,2.2,-0.446522529000015));
#347468=CARTESIAN_POINT('Ctrl Pts',(4.24435943499994,12.2,-0.446089421000018));
#347469=CARTESIAN_POINT('Ctrl Pts',(4.24435943499994,5.2,-0.446089421000018));
#347470=CARTESIAN_POINT('Ctrl Pts',(4.24435943499994,2.2,-0.446089421000018));
#347471=CARTESIAN_POINT('Ctrl Pts',(4.24602454599994,12.2,-0.445653297000015));
#347472=CARTESIAN_POINT('Ctrl Pts',(4.24602454599994,5.2,-0.445653297000015));
#347473=CARTESIAN_POINT('Ctrl Pts',(4.24602454599994,2.2,-0.445653297000015));
#347474=CARTESIAN_POINT('Ctrl Pts',(4.24769342899994,12.2,-0.445214148000015));
#347475=CARTESIAN_POINT('Ctrl Pts',(4.24769342899994,5.2,-0.445214148000015));
#347476=CARTESIAN_POINT('Ctrl Pts',(4.24769342899994,2.2,-0.445214148000015));
#347477=CARTESIAN_POINT('Ctrl Pts',(4.24936607299994,12.2,-0.444771966000013));
#347478=CARTESIAN_POINT('Ctrl Pts',(4.24936607299994,5.2,-0.444771966000013));
#347479=CARTESIAN_POINT('Ctrl Pts',(4.24936607299994,2.2,-0.444771966000013));
#347480=CARTESIAN_POINT('Ctrl Pts',(4.25104246699994,12.2,-0.444326746000012));
#347481=CARTESIAN_POINT('Ctrl Pts',(4.25104246699994,5.2,-0.444326746000012));
#347482=CARTESIAN_POINT('Ctrl Pts',(4.25104246699994,2.2,-0.444326746000012));
#347483=CARTESIAN_POINT('Ctrl Pts',(4.25272260199994,12.2,-0.443878482000013));
#347484=CARTESIAN_POINT('Ctrl Pts',(4.25272260199994,5.2,-0.443878482000013));
#347485=CARTESIAN_POINT('Ctrl Pts',(4.25272260199994,2.2,-0.443878482000013));
#347486=CARTESIAN_POINT('Ctrl Pts',(4.25440646699994,12.2,-0.443427164000014));
#347487=CARTESIAN_POINT('Ctrl Pts',(4.25440646699994,5.2,-0.443427164000014));
#347488=CARTESIAN_POINT('Ctrl Pts',(4.25440646699994,2.2,-0.443427164000014));
#347489=CARTESIAN_POINT('Ctrl Pts',(4.25609405399995,12.2,-0.442972788000016));
#347490=CARTESIAN_POINT('Ctrl Pts',(4.25609405399995,5.2,-0.442972788000016));
#347491=CARTESIAN_POINT('Ctrl Pts',(4.25609405399995,2.2,-0.442972788000016));
#347492=CARTESIAN_POINT('Ctrl Pts',(4.25778535099994,12.2,-0.442515347000012));
#347493=CARTESIAN_POINT('Ctrl Pts',(4.25778535099994,5.2,-0.442515347000012));
#347494=CARTESIAN_POINT('Ctrl Pts',(4.25778535099994,2.2,-0.442515347000012));
#347495=CARTESIAN_POINT('Ctrl Pts',(4.25948034899994,12.2,-0.442054834000012));
#347496=CARTESIAN_POINT('Ctrl Pts',(4.25948034899994,5.2,-0.442054834000012));
#347497=CARTESIAN_POINT('Ctrl Pts',(4.25948034899994,2.2,-0.442054834000012));
#347498=CARTESIAN_POINT('Ctrl Pts',(4.26117903799994,12.2,-0.441591242000015));
#347499=CARTESIAN_POINT('Ctrl Pts',(4.26117903799994,5.2,-0.441591242000015));
#347500=CARTESIAN_POINT('Ctrl Pts',(4.26117903799994,2.2,-0.441591242000015));
#347501=CARTESIAN_POINT('Ctrl Pts',(4.26288140799994,12.2,-0.441124564000015));
#347502=CARTESIAN_POINT('Ctrl Pts',(4.26288140799994,5.2,-0.441124564000015));
#347503=CARTESIAN_POINT('Ctrl Pts',(4.26288140799994,2.2,-0.441124564000015));
#347504=CARTESIAN_POINT('Ctrl Pts',(4.26458744799994,12.2,-0.440654794000017));
#347505=CARTESIAN_POINT('Ctrl Pts',(4.26458744799994,5.2,-0.440654794000017));
#347506=CARTESIAN_POINT('Ctrl Pts',(4.26458744799994,2.2,-0.440654794000017));
#347507=CARTESIAN_POINT('Ctrl Pts',(4.26629714899994,12.2,-0.440181925000012));
#347508=CARTESIAN_POINT('Ctrl Pts',(4.26629714899994,5.2,-0.440181925000012));
#347509=CARTESIAN_POINT('Ctrl Pts',(4.26629714899994,2.2,-0.440181925000012));
#347510=CARTESIAN_POINT('Ctrl Pts',(4.26801050199995,12.2,-0.439705951000011));
#347511=CARTESIAN_POINT('Ctrl Pts',(4.26801050199995,5.2,-0.439705951000011));
#347512=CARTESIAN_POINT('Ctrl Pts',(4.26801050199995,2.2,-0.439705951000011));
#347513=CARTESIAN_POINT('Ctrl Pts',(4.26972749499994,12.2,-0.439226866000015));
#347514=CARTESIAN_POINT('Ctrl Pts',(4.26972749499994,5.2,-0.439226866000015));
#347515=CARTESIAN_POINT('Ctrl Pts',(4.26972749499994,2.2,-0.439226866000015));
#347516=CARTESIAN_POINT('Ctrl Pts',(4.27144811999994,12.2,-0.438744662000015));
#347517=CARTESIAN_POINT('Ctrl Pts',(4.27144811999994,5.2,-0.438744662000015));
#347518=CARTESIAN_POINT('Ctrl Pts',(4.27144811999994,2.2,-0.438744662000015));
#347519=CARTESIAN_POINT('Ctrl Pts',(4.27317236499994,12.2,-0.438259334000013));
#347520=CARTESIAN_POINT('Ctrl Pts',(4.27317236499994,5.2,-0.438259334000013));
#347521=CARTESIAN_POINT('Ctrl Pts',(4.27317236499994,2.2,-0.438259334000013));
#347522=CARTESIAN_POINT('Ctrl Pts',(4.27490022199995,12.2,-0.437770874000014));
#347523=CARTESIAN_POINT('Ctrl Pts',(4.27490022199995,5.2,-0.437770874000014));
#347524=CARTESIAN_POINT('Ctrl Pts',(4.27490022199995,2.2,-0.437770874000014));
#347525=CARTESIAN_POINT('Ctrl Pts',(4.27663167999994,12.2,-0.437279276000013));
#347526=CARTESIAN_POINT('Ctrl Pts',(4.27663167999994,5.2,-0.437279276000013));
#347527=CARTESIAN_POINT('Ctrl Pts',(4.27663167999994,2.2,-0.437279276000013));
#347528=CARTESIAN_POINT('Ctrl Pts',(4.27836672999994,12.2,-0.436784535000014));
#347529=CARTESIAN_POINT('Ctrl Pts',(4.27836672999994,5.2,-0.436784535000014));
#347530=CARTESIAN_POINT('Ctrl Pts',(4.27836672999994,2.2,-0.436784535000014));
#347531=CARTESIAN_POINT('Ctrl Pts',(4.28010536099994,12.2,-0.436286643000017));
#347532=CARTESIAN_POINT('Ctrl Pts',(4.28010536099994,5.2,-0.436286643000017));
#347533=CARTESIAN_POINT('Ctrl Pts',(4.28010536099994,2.2,-0.436286643000017));
#347534=CARTESIAN_POINT('Ctrl Pts',(4.28184756399994,12.2,-0.435785595000016));
#347535=CARTESIAN_POINT('Ctrl Pts',(4.28184756399994,5.2,-0.435785595000016));
#347536=CARTESIAN_POINT('Ctrl Pts',(4.28184756399994,2.2,-0.435785595000016));
#347537=CARTESIAN_POINT('Ctrl Pts',(4.28359332899995,12.2,-0.435281384000015));
#347538=CARTESIAN_POINT('Ctrl Pts',(4.28359332899995,5.2,-0.435281384000015));
#347539=CARTESIAN_POINT('Ctrl Pts',(4.28359332899995,2.2,-0.435281384000015));
#347540=CARTESIAN_POINT('Ctrl Pts',(4.28534264599994,12.2,-0.434774002000013));
#347541=CARTESIAN_POINT('Ctrl Pts',(4.28534264599994,5.2,-0.434774002000013));
#347542=CARTESIAN_POINT('Ctrl Pts',(4.28534264599994,2.2,-0.434774002000013));
#347543=CARTESIAN_POINT('Ctrl Pts',(4.28709550499994,12.2,-0.434263445000016));
#347544=CARTESIAN_POINT('Ctrl Pts',(4.28709550499994,5.2,-0.434263445000016));
#347545=CARTESIAN_POINT('Ctrl Pts',(4.28709550499994,2.2,-0.434263445000016));
#347546=CARTESIAN_POINT('Ctrl Pts',(4.28885189599994,12.2,-0.433749706000013));
#347547=CARTESIAN_POINT('Ctrl Pts',(4.28885189599994,5.2,-0.433749706000013));
#347548=CARTESIAN_POINT('Ctrl Pts',(4.28885189599994,2.2,-0.433749706000013));
#347549=CARTESIAN_POINT('Ctrl Pts',(4.29061181099994,12.2,-0.433232780000012));
#347550=CARTESIAN_POINT('Ctrl Pts',(4.29061181099994,5.2,-0.433232780000012));
#347551=CARTESIAN_POINT('Ctrl Pts',(4.29061181099994,2.2,-0.433232780000012));
#347552=CARTESIAN_POINT('Ctrl Pts',(4.29237523699994,12.2,-0.432712658000014));
#347553=CARTESIAN_POINT('Ctrl Pts',(4.29237523699994,5.2,-0.432712658000014));
#347554=CARTESIAN_POINT('Ctrl Pts',(4.29237523699994,2.2,-0.432712658000014));
#347555=CARTESIAN_POINT('Ctrl Pts',(4.29414216599994,12.2,-0.432189335000013));
#347556=CARTESIAN_POINT('Ctrl Pts',(4.29414216599994,5.2,-0.432189335000013));
#347557=CARTESIAN_POINT('Ctrl Pts',(4.29414216599994,2.2,-0.432189335000013));
#347558=CARTESIAN_POINT('Ctrl Pts',(4.29591258899995,12.2,-0.431662807000013));
#347559=CARTESIAN_POINT('Ctrl Pts',(4.29591258899995,5.2,-0.431662807000013));
#347560=CARTESIAN_POINT('Ctrl Pts',(4.29591258899995,2.2,-0.431662807000013));
#347561=CARTESIAN_POINT('Ctrl Pts',(4.29768649499994,12.2,-0.431133065000013));
#347562=CARTESIAN_POINT('Ctrl Pts',(4.29768649499994,5.2,-0.431133065000013));
#347563=CARTESIAN_POINT('Ctrl Pts',(4.29768649499994,2.2,-0.431133065000013));
#347564=CARTESIAN_POINT('Ctrl Pts',(4.29946387299994,12.2,-0.430600104000014));
#347565=CARTESIAN_POINT('Ctrl Pts',(4.29946387299994,5.2,-0.430600104000014));
#347566=CARTESIAN_POINT('Ctrl Pts',(4.29946387299994,2.2,-0.430600104000014));
#347567=CARTESIAN_POINT('Ctrl Pts',(4.30124471599994,12.2,-0.430063918000014));
#347568=CARTESIAN_POINT('Ctrl Pts',(4.30124471599994,5.2,-0.430063918000014));
#347569=CARTESIAN_POINT('Ctrl Pts',(4.30124471599994,2.2,-0.430063918000014));
#347570=CARTESIAN_POINT('Ctrl Pts',(4.30302901299994,12.2,-0.429524501000014));
#347571=CARTESIAN_POINT('Ctrl Pts',(4.30302901299994,5.2,-0.429524501000014));
#347572=CARTESIAN_POINT('Ctrl Pts',(4.30302901299994,2.2,-0.429524501000014));
#347573=CARTESIAN_POINT('Ctrl Pts',(4.30481675399994,12.2,-0.428981846000016));
#347574=CARTESIAN_POINT('Ctrl Pts',(4.30481675399994,5.2,-0.428981846000016));
#347575=CARTESIAN_POINT('Ctrl Pts',(4.30481675399994,2.2,-0.428981846000016));
#347576=CARTESIAN_POINT('Ctrl Pts',(4.30660792899995,12.2,-0.428435948000012));
#347577=CARTESIAN_POINT('Ctrl Pts',(4.30660792899995,5.2,-0.428435948000012));
#347578=CARTESIAN_POINT('Ctrl Pts',(4.30660792899995,2.2,-0.428435948000012));
#347579=CARTESIAN_POINT('Ctrl Pts',(4.30840252899995,12.2,-0.427886801000015));
#347580=CARTESIAN_POINT('Ctrl Pts',(4.30840252899995,5.2,-0.427886801000015));
#347581=CARTESIAN_POINT('Ctrl Pts',(4.30840252899995,2.2,-0.427886801000015));
#347582=CARTESIAN_POINT('Ctrl Pts',(4.31020054399994,12.2,-0.427334398000014));
#347583=CARTESIAN_POINT('Ctrl Pts',(4.31020054399994,5.2,-0.427334398000014));
#347584=CARTESIAN_POINT('Ctrl Pts',(4.31020054399994,2.2,-0.427334398000014));
#347585=CARTESIAN_POINT('Ctrl Pts',(4.31200196399994,12.2,-0.426778735000015));
#347586=CARTESIAN_POINT('Ctrl Pts',(4.31200196399994,5.2,-0.426778735000015));
#347587=CARTESIAN_POINT('Ctrl Pts',(4.31200196399994,2.2,-0.426778735000015));
#347588=CARTESIAN_POINT('Ctrl Pts',(4.31380677899995,12.2,-0.426219804000016));
#347589=CARTESIAN_POINT('Ctrl Pts',(4.31380677899995,5.2,-0.426219804000016));
#347590=CARTESIAN_POINT('Ctrl Pts',(4.31380677899995,2.2,-0.426219804000016));
#347591=CARTESIAN_POINT('Ctrl Pts',(4.31561497899995,12.2,-0.425657600000013));
#347592=CARTESIAN_POINT('Ctrl Pts',(4.31561497899995,5.2,-0.425657600000013));
#347593=CARTESIAN_POINT('Ctrl Pts',(4.31561497899995,2.2,-0.425657600000013));
#347594=CARTESIAN_POINT('Ctrl Pts',(4.31742655599994,12.2,-0.425092117000014));
#347595=CARTESIAN_POINT('Ctrl Pts',(4.31742655599994,5.2,-0.425092117000014));
#347596=CARTESIAN_POINT('Ctrl Pts',(4.31742655599994,2.2,-0.425092117000014));
#347597=CARTESIAN_POINT('Ctrl Pts',(4.31924149999994,12.2,-0.424523350000015));
#347598=CARTESIAN_POINT('Ctrl Pts',(4.31924149999994,5.2,-0.424523350000015));
#347599=CARTESIAN_POINT('Ctrl Pts',(4.31924149999994,2.2,-0.424523350000015));
#347600=CARTESIAN_POINT('Ctrl Pts',(4.32105979999994,12.2,-0.423951292000013));
#347601=CARTESIAN_POINT('Ctrl Pts',(4.32105979999994,5.2,-0.423951292000013));
#347602=CARTESIAN_POINT('Ctrl Pts',(4.32105979999994,2.2,-0.423951292000013));
#347603=CARTESIAN_POINT('Ctrl Pts',(4.32288144699995,12.2,-0.423375938000015));
#347604=CARTESIAN_POINT('Ctrl Pts',(4.32288144699995,5.2,-0.423375938000015));
#347605=CARTESIAN_POINT('Ctrl Pts',(4.32288144699995,2.2,-0.423375938000015));
#347606=CARTESIAN_POINT('Ctrl Pts',(4.32470643099994,12.2,-0.422797280000013));
#347607=CARTESIAN_POINT('Ctrl Pts',(4.32470643099994,5.2,-0.422797280000013));
#347608=CARTESIAN_POINT('Ctrl Pts',(4.32470643099994,2.2,-0.422797280000013));
#347609=CARTESIAN_POINT('Ctrl Pts',(4.32653474299994,12.2,-0.422215316000014));
#347610=CARTESIAN_POINT('Ctrl Pts',(4.32653474299994,5.2,-0.422215316000014));
#347611=CARTESIAN_POINT('Ctrl Pts',(4.32653474299994,2.2,-0.422215316000014));
#347612=CARTESIAN_POINT('Ctrl Pts',(4.32836637299994,12.2,-0.421630037000016));
#347613=CARTESIAN_POINT('Ctrl Pts',(4.32836637299994,5.2,-0.421630037000016));
#347614=CARTESIAN_POINT('Ctrl Pts',(4.32836637299994,2.2,-0.421630037000016));
#347615=CARTESIAN_POINT('Ctrl Pts',(4.33020131099994,12.2,-0.421041438000014));
#347616=CARTESIAN_POINT('Ctrl Pts',(4.33020131099994,5.2,-0.421041438000014));
#347617=CARTESIAN_POINT('Ctrl Pts',(4.33020131099994,2.2,-0.421041438000014));
#347618=CARTESIAN_POINT('Ctrl Pts',(4.33203954699994,12.2,-0.420449516000012));
#347619=CARTESIAN_POINT('Ctrl Pts',(4.33203954699994,5.2,-0.420449516000012));
#347620=CARTESIAN_POINT('Ctrl Pts',(4.33203954699994,2.2,-0.420449516000012));
#347621=CARTESIAN_POINT('Ctrl Pts',(4.33388107299994,12.2,-0.419854261000014));
#347622=CARTESIAN_POINT('Ctrl Pts',(4.33388107299994,5.2,-0.419854261000014));
#347623=CARTESIAN_POINT('Ctrl Pts',(4.33388107299994,2.2,-0.419854261000014));
#347624=CARTESIAN_POINT('Ctrl Pts',(4.33572587799994,12.2,-0.419255671000016));
#347625=CARTESIAN_POINT('Ctrl Pts',(4.33572587799994,5.2,-0.419255671000016));
#347626=CARTESIAN_POINT('Ctrl Pts',(4.33572587799994,2.2,-0.419255671000016));
#347627=CARTESIAN_POINT('Ctrl Pts',(4.33757395399994,12.2,-0.418653738000017));
#347628=CARTESIAN_POINT('Ctrl Pts',(4.33757395399994,5.2,-0.418653738000017));
#347629=CARTESIAN_POINT('Ctrl Pts',(4.33757395399994,2.2,-0.418653738000017));
#347630=CARTESIAN_POINT('Ctrl Pts',(4.33942528899994,12.2,-0.418048457000015));
#347631=CARTESIAN_POINT('Ctrl Pts',(4.33942528899994,5.2,-0.418048457000015));
#347632=CARTESIAN_POINT('Ctrl Pts',(4.33942528899994,2.2,-0.418048457000015));
#347633=CARTESIAN_POINT('Ctrl Pts',(4.34127987499994,12.2,-0.417439823000016));
#347634=CARTESIAN_POINT('Ctrl Pts',(4.34127987499994,5.2,-0.417439823000016));
#347635=CARTESIAN_POINT('Ctrl Pts',(4.34127987499994,2.2,-0.417439823000016));
#347636=CARTESIAN_POINT('Ctrl Pts',(4.34313770199994,12.2,-0.416827830000015));
#347637=CARTESIAN_POINT('Ctrl Pts',(4.34313770199994,5.2,-0.416827830000015));
#347638=CARTESIAN_POINT('Ctrl Pts',(4.34313770199994,2.2,-0.416827830000015));
#347639=CARTESIAN_POINT('Ctrl Pts',(4.34499875999994,12.2,-0.416212473000015));
#347640=CARTESIAN_POINT('Ctrl Pts',(4.34499875999994,5.2,-0.416212473000015));
#347641=CARTESIAN_POINT('Ctrl Pts',(4.34499875999994,2.2,-0.416212473000015));
#347642=CARTESIAN_POINT('Ctrl Pts',(4.34686303899994,12.2,-0.415593746000016));
#347643=CARTESIAN_POINT('Ctrl Pts',(4.34686303899994,5.2,-0.415593746000016));
#347644=CARTESIAN_POINT('Ctrl Pts',(4.34686303899994,2.2,-0.415593746000016));
#347645=CARTESIAN_POINT('Ctrl Pts',(4.34873053199994,12.2,-0.414971643000013));
#347646=CARTESIAN_POINT('Ctrl Pts',(4.34873053199994,5.2,-0.414971643000013));
#347647=CARTESIAN_POINT('Ctrl Pts',(4.34873053199994,2.2,-0.414971643000013));
#347648=CARTESIAN_POINT('Ctrl Pts',(4.35060122699995,12.2,-0.414346159000014));
#347649=CARTESIAN_POINT('Ctrl Pts',(4.35060122699995,5.2,-0.414346159000014));
#347650=CARTESIAN_POINT('Ctrl Pts',(4.35060122699995,2.2,-0.414346159000014));
#347651=CARTESIAN_POINT('Ctrl Pts',(4.35247511499994,12.2,-0.413717289000015));
#347652=CARTESIAN_POINT('Ctrl Pts',(4.35247511499994,5.2,-0.413717289000015));
#347653=CARTESIAN_POINT('Ctrl Pts',(4.35247511499994,2.2,-0.413717289000015));
#347654=CARTESIAN_POINT('Ctrl Pts',(4.35435218699994,12.2,-0.413085027000015));
#347655=CARTESIAN_POINT('Ctrl Pts',(4.35435218699994,5.2,-0.413085027000015));
#347656=CARTESIAN_POINT('Ctrl Pts',(4.35435218699994,2.2,-0.413085027000015));
#347657=CARTESIAN_POINT('Ctrl Pts',(4.35623243299994,12.2,-0.412449368000014));
#347658=CARTESIAN_POINT('Ctrl Pts',(4.35623243299994,5.2,-0.412449368000014));
#347659=CARTESIAN_POINT('Ctrl Pts',(4.35623243299994,2.2,-0.412449368000014));
#347660=CARTESIAN_POINT('Ctrl Pts',(4.35811584299994,12.2,-0.411810305000015));
#347661=CARTESIAN_POINT('Ctrl Pts',(4.35811584299994,5.2,-0.411810305000015));
#347662=CARTESIAN_POINT('Ctrl Pts',(4.35811584299994,2.2,-0.411810305000015));
#347663=CARTESIAN_POINT('Ctrl Pts',(4.36000240899994,12.2,-0.411167836000015));
#347664=CARTESIAN_POINT('Ctrl Pts',(4.36000240899994,5.2,-0.411167836000015));
#347665=CARTESIAN_POINT('Ctrl Pts',(4.36000240899994,2.2,-0.411167836000015));
#347666=CARTESIAN_POINT('Ctrl Pts',(4.36189211999995,12.2,-0.410521953000016));
#347667=CARTESIAN_POINT('Ctrl Pts',(4.36189211999995,5.2,-0.410521953000016));
#347668=CARTESIAN_POINT('Ctrl Pts',(4.36189211999995,2.2,-0.410521953000016));
#347669=CARTESIAN_POINT('Ctrl Pts',(4.36378496799994,12.2,-0.409872651000014));
#347670=CARTESIAN_POINT('Ctrl Pts',(4.36378496799994,5.2,-0.409872651000014));
#347671=CARTESIAN_POINT('Ctrl Pts',(4.36378496799994,2.2,-0.409872651000014));
#347672=CARTESIAN_POINT('Ctrl Pts',(4.36568093999994,12.2,-0.409219925000013));
#347673=CARTESIAN_POINT('Ctrl Pts',(4.36568093999994,5.2,-0.409219925000013));
#347674=CARTESIAN_POINT('Ctrl Pts',(4.36568093999994,2.2,-0.409219925000013));
#347675=CARTESIAN_POINT('Ctrl Pts',(4.36758003099994,12.2,-0.408563769000012));
#347676=CARTESIAN_POINT('Ctrl Pts',(4.36758003099994,5.2,-0.408563769000012));
#347677=CARTESIAN_POINT('Ctrl Pts',(4.36758003099994,2.2,-0.408563769000012));
#347678=CARTESIAN_POINT('Ctrl Pts',(4.36948222999994,12.2,-0.407904179000016));
#347679=CARTESIAN_POINT('Ctrl Pts',(4.36948222999994,5.2,-0.407904179000016));
#347680=CARTESIAN_POINT('Ctrl Pts',(4.36948222999994,2.2,-0.407904179000016));
#347681=CARTESIAN_POINT('Ctrl Pts',(4.37138752599994,12.2,-0.407241150000015));
#347682=CARTESIAN_POINT('Ctrl Pts',(4.37138752599994,5.2,-0.407241150000015));
#347683=CARTESIAN_POINT('Ctrl Pts',(4.37138752599994,2.2,-0.407241150000015));
#347684=CARTESIAN_POINT('Ctrl Pts',(4.37329590999994,12.2,-0.406574675000013));
#347685=CARTESIAN_POINT('Ctrl Pts',(4.37329590999994,5.2,-0.406574675000013));
#347686=CARTESIAN_POINT('Ctrl Pts',(4.37329590999994,2.2,-0.406574675000013));
#347687=CARTESIAN_POINT('Ctrl Pts',(4.37520737499994,12.2,-0.405904750000015));
#347688=CARTESIAN_POINT('Ctrl Pts',(4.37520737499994,5.2,-0.405904750000015));
#347689=CARTESIAN_POINT('Ctrl Pts',(4.37520737499994,2.2,-0.405904750000015));
#347690=CARTESIAN_POINT('Ctrl Pts',(4.37712190899994,12.2,-0.405231370000014));
#347691=CARTESIAN_POINT('Ctrl Pts',(4.37712190899994,5.2,-0.405231370000014));
#347692=CARTESIAN_POINT('Ctrl Pts',(4.37712190899994,2.2,-0.405231370000014));
#347693=CARTESIAN_POINT('Ctrl Pts',(4.37903950299994,12.2,-0.404554529000016));
#347694=CARTESIAN_POINT('Ctrl Pts',(4.37903950299994,5.2,-0.404554529000016));
#347695=CARTESIAN_POINT('Ctrl Pts',(4.37903950299994,2.2,-0.404554529000016));
#347696=CARTESIAN_POINT('Ctrl Pts',(4.38096014699994,12.2,-0.403874222000016));
#347697=CARTESIAN_POINT('Ctrl Pts',(4.38096014699994,5.2,-0.403874222000016));
#347698=CARTESIAN_POINT('Ctrl Pts',(4.38096014699994,2.2,-0.403874222000016));
#347699=CARTESIAN_POINT('Ctrl Pts',(4.38288383399995,12.2,-0.403190444000017));
#347700=CARTESIAN_POINT('Ctrl Pts',(4.38288383399995,5.2,-0.403190444000017));
#347701=CARTESIAN_POINT('Ctrl Pts',(4.38288383399995,2.2,-0.403190444000017));
#347702=CARTESIAN_POINT('Ctrl Pts',(4.38481055199994,12.2,-0.402503192000014));
#347703=CARTESIAN_POINT('Ctrl Pts',(4.38481055199994,5.2,-0.402503192000014));
#347704=CARTESIAN_POINT('Ctrl Pts',(4.38481055199994,2.2,-0.402503192000014));
#347705=CARTESIAN_POINT('Ctrl Pts',(4.38674029299994,12.2,-0.401812457000013));
#347706=CARTESIAN_POINT('Ctrl Pts',(4.38674029299994,5.2,-0.401812457000013));
#347707=CARTESIAN_POINT('Ctrl Pts',(4.38674029299994,2.2,-0.401812457000013));
#347708=CARTESIAN_POINT('Ctrl Pts',(4.38867304799994,12.2,-0.401118237000015));
#347709=CARTESIAN_POINT('Ctrl Pts',(4.38867304799994,5.2,-0.401118237000015));
#347710=CARTESIAN_POINT('Ctrl Pts',(4.38867304799994,2.2,-0.401118237000015));
#347711=CARTESIAN_POINT('Ctrl Pts',(4.39060880499994,12.2,-0.400420526000014));
#347712=CARTESIAN_POINT('Ctrl Pts',(4.39060880499994,5.2,-0.400420526000014));
#347713=CARTESIAN_POINT('Ctrl Pts',(4.39060880499994,2.2,-0.400420526000014));
#347714=CARTESIAN_POINT('Ctrl Pts',(4.39254755799994,12.2,-0.399719319000016));
#347715=CARTESIAN_POINT('Ctrl Pts',(4.39254755799994,5.2,-0.399719319000016));
#347716=CARTESIAN_POINT('Ctrl Pts',(4.39254755799994,2.2,-0.399719319000016));
#347717=CARTESIAN_POINT('Ctrl Pts',(4.39448929499994,12.2,-0.399014611000013));
#347718=CARTESIAN_POINT('Ctrl Pts',(4.39448929499994,5.2,-0.399014611000013));
#347719=CARTESIAN_POINT('Ctrl Pts',(4.39448929499994,2.2,-0.399014611000013));
#347720=CARTESIAN_POINT('Ctrl Pts',(4.39643400699994,12.2,-0.398306396000017));
#347721=CARTESIAN_POINT('Ctrl Pts',(4.39643400699994,5.2,-0.398306396000017));
#347722=CARTESIAN_POINT('Ctrl Pts',(4.39643400699994,2.2,-0.398306396000017));
#347723=CARTESIAN_POINT('Ctrl Pts',(4.39838168799994,12.2,-0.397594671000014));
#347724=CARTESIAN_POINT('Ctrl Pts',(4.39838168799994,5.2,-0.397594671000014));
#347725=CARTESIAN_POINT('Ctrl Pts',(4.39838168799994,2.2,-0.397594671000014));
#347726=CARTESIAN_POINT('Ctrl Pts',(4.40033232399994,12.2,-0.396879430000014));
#347727=CARTESIAN_POINT('Ctrl Pts',(4.40033232399994,5.2,-0.396879430000014));
#347728=CARTESIAN_POINT('Ctrl Pts',(4.40033232399994,2.2,-0.396879430000014));
#347729=CARTESIAN_POINT('Ctrl Pts',(4.40228590799994,12.2,-0.396160667000016));
#347730=CARTESIAN_POINT('Ctrl Pts',(4.40228590799994,5.2,-0.396160667000016));
#347731=CARTESIAN_POINT('Ctrl Pts',(4.40228590799994,2.2,-0.396160667000016));
#347732=CARTESIAN_POINT('Ctrl Pts',(4.40424242999994,12.2,-0.395438380000015));
#347733=CARTESIAN_POINT('Ctrl Pts',(4.40424242999994,5.2,-0.395438380000015));
#347734=CARTESIAN_POINT('Ctrl Pts',(4.40424242999994,2.2,-0.395438380000015));
#347735=CARTESIAN_POINT('Ctrl Pts',(4.40620187999994,12.2,-0.394712561000015));
#347736=CARTESIAN_POINT('Ctrl Pts',(4.40620187999994,5.2,-0.394712561000015));
#347737=CARTESIAN_POINT('Ctrl Pts',(4.40620187999994,2.2,-0.394712561000015));
#347738=CARTESIAN_POINT('Ctrl Pts',(4.40816425099994,12.2,-0.393983207000015));
#347739=CARTESIAN_POINT('Ctrl Pts',(4.40816425099994,5.2,-0.393983207000015));
#347740=CARTESIAN_POINT('Ctrl Pts',(4.40816425099994,2.2,-0.393983207000015));
#347741=CARTESIAN_POINT('Ctrl Pts',(4.41012953199994,12.2,-0.393250314000015));
#347742=CARTESIAN_POINT('Ctrl Pts',(4.41012953199994,5.2,-0.393250314000015));
#347743=CARTESIAN_POINT('Ctrl Pts',(4.41012953199994,2.2,-0.393250314000015));
#347744=CARTESIAN_POINT('Ctrl Pts',(4.41209771399994,12.2,-0.392513875000016));
#347745=CARTESIAN_POINT('Ctrl Pts',(4.41209771399994,5.2,-0.392513875000016));
#347746=CARTESIAN_POINT('Ctrl Pts',(4.41209771399994,2.2,-0.392513875000016));
#347747=CARTESIAN_POINT('Ctrl Pts',(4.41406878699994,12.2,-0.391773886000015));
#347748=CARTESIAN_POINT('Ctrl Pts',(4.41406878699994,5.2,-0.391773886000015));
#347749=CARTESIAN_POINT('Ctrl Pts',(4.41406878699994,2.2,-0.391773886000015));
#347750=CARTESIAN_POINT('Ctrl Pts',(4.41604274299995,12.2,-0.391030343000014));
#347751=CARTESIAN_POINT('Ctrl Pts',(4.41604274299995,5.2,-0.391030343000014));
#347752=CARTESIAN_POINT('Ctrl Pts',(4.41604274299995,2.2,-0.391030343000014));
#347753=CARTESIAN_POINT('Ctrl Pts',(4.41801957099995,12.2,-0.390283240000016));
#347754=CARTESIAN_POINT('Ctrl Pts',(4.41801957099995,5.2,-0.390283240000016));
#347755=CARTESIAN_POINT('Ctrl Pts',(4.41801957099995,2.2,-0.390283240000016));
#347756=CARTESIAN_POINT('Ctrl Pts',(4.41999926399994,12.2,-0.389532573000011));
#347757=CARTESIAN_POINT('Ctrl Pts',(4.41999926399994,5.2,-0.389532573000011));
#347758=CARTESIAN_POINT('Ctrl Pts',(4.41999926399994,2.2,-0.389532573000011));
#347759=CARTESIAN_POINT('Ctrl Pts',(4.42198181199995,12.2,-0.388778337000013));
#347760=CARTESIAN_POINT('Ctrl Pts',(4.42198181199995,5.2,-0.388778337000013));
#347761=CARTESIAN_POINT('Ctrl Pts',(4.42198181199995,2.2,-0.388778337000013));
#347762=CARTESIAN_POINT('Ctrl Pts',(4.42396720399994,12.2,-0.388020528000013));
#347763=CARTESIAN_POINT('Ctrl Pts',(4.42396720399994,5.2,-0.388020528000013));
#347764=CARTESIAN_POINT('Ctrl Pts',(4.42396720399994,2.2,-0.388020528000013));
#347765=CARTESIAN_POINT('Ctrl Pts',(4.42595543299994,12.2,-0.387259141000014));
#347766=CARTESIAN_POINT('Ctrl Pts',(4.42595543299994,5.2,-0.387259141000014));
#347767=CARTESIAN_POINT('Ctrl Pts',(4.42595543299994,2.2,-0.387259141000014));
#347768=CARTESIAN_POINT('Ctrl Pts',(4.42794648799994,12.2,-0.386494172000016));
#347769=CARTESIAN_POINT('Ctrl Pts',(4.42794648799994,5.2,-0.386494172000016));
#347770=CARTESIAN_POINT('Ctrl Pts',(4.42794648799994,2.2,-0.386494172000016));
#347771=CARTESIAN_POINT('Ctrl Pts',(4.42994036099994,12.2,-0.385725614000014));
#347772=CARTESIAN_POINT('Ctrl Pts',(4.42994036099994,5.2,-0.385725614000014));
#347773=CARTESIAN_POINT('Ctrl Pts',(4.42994036099994,2.2,-0.385725614000014));
#347774=CARTESIAN_POINT('Ctrl Pts',(4.43193704199994,12.2,-0.384953465000013));
#347775=CARTESIAN_POINT('Ctrl Pts',(4.43193704199994,5.2,-0.384953465000013));
#347776=CARTESIAN_POINT('Ctrl Pts',(4.43193704199994,2.2,-0.384953465000013));
#347777=CARTESIAN_POINT('Ctrl Pts',(4.43393652199994,12.2,-0.384177719000016));
#347778=CARTESIAN_POINT('Ctrl Pts',(4.43393652199994,5.2,-0.384177719000016));
#347779=CARTESIAN_POINT('Ctrl Pts',(4.43393652199994,2.2,-0.384177719000016));
#347780=CARTESIAN_POINT('Ctrl Pts',(4.43593879199994,12.2,-0.383398371000014));
#347781=CARTESIAN_POINT('Ctrl Pts',(4.43593879199994,5.2,-0.383398371000014));
#347782=CARTESIAN_POINT('Ctrl Pts',(4.43593879199994,2.2,-0.383398371000014));
#347783=CARTESIAN_POINT('Ctrl Pts',(4.43794384199994,12.2,-0.382615419000012));
#347784=CARTESIAN_POINT('Ctrl Pts',(4.43794384199994,5.2,-0.382615419000012));
#347785=CARTESIAN_POINT('Ctrl Pts',(4.43794384199994,2.2,-0.382615419000012));
#347786=CARTESIAN_POINT('Ctrl Pts',(4.43995166399994,12.2,-0.381828856000013));
#347787=CARTESIAN_POINT('Ctrl Pts',(4.43995166399994,5.2,-0.381828856000013));
#347788=CARTESIAN_POINT('Ctrl Pts',(4.43995166399994,2.2,-0.381828856000013));
#347789=CARTESIAN_POINT('Ctrl Pts',(4.44196224799995,12.2,-0.381038678000016));
#347790=CARTESIAN_POINT('Ctrl Pts',(4.44196224799995,5.2,-0.381038678000016));
#347791=CARTESIAN_POINT('Ctrl Pts',(4.44196224799995,2.2,-0.381038678000016));
#347792=CARTESIAN_POINT('Ctrl Pts',(4.44397558499994,12.2,-0.380244880000014));
#347793=CARTESIAN_POINT('Ctrl Pts',(4.44397558499994,5.2,-0.380244880000014));
#347794=CARTESIAN_POINT('Ctrl Pts',(4.44397558499994,2.2,-0.380244880000014));
#347795=CARTESIAN_POINT('Ctrl Pts',(4.44599166599995,12.2,-0.379447460000013));
#347796=CARTESIAN_POINT('Ctrl Pts',(4.44599166599995,5.2,-0.379447460000013));
#347797=CARTESIAN_POINT('Ctrl Pts',(4.44599166599995,2.2,-0.379447460000013));
#347798=CARTESIAN_POINT('Ctrl Pts',(4.44801048099994,12.2,-0.378646411000014));
#347799=CARTESIAN_POINT('Ctrl Pts',(4.44801048099994,5.2,-0.378646411000014));
#347800=CARTESIAN_POINT('Ctrl Pts',(4.44801048099994,2.2,-0.378646411000014));
#347801=CARTESIAN_POINT('Ctrl Pts',(4.45003202299994,12.2,-0.377841729000017));
#347802=CARTESIAN_POINT('Ctrl Pts',(4.45003202299994,5.2,-0.377841729000017));
#347803=CARTESIAN_POINT('Ctrl Pts',(4.45003202299994,2.2,-0.377841729000017));
#347804=CARTESIAN_POINT('Ctrl Pts',(4.45205627999994,12.2,-0.377033410000016));
#347805=CARTESIAN_POINT('Ctrl Pts',(4.45205627999994,5.2,-0.377033410000016));
#347806=CARTESIAN_POINT('Ctrl Pts',(4.45205627999994,2.2,-0.377033410000016));
#347807=CARTESIAN_POINT('Ctrl Pts',(4.45408324399994,12.2,-0.376221450000016));
#347808=CARTESIAN_POINT('Ctrl Pts',(4.45408324399994,5.2,-0.376221450000016));
#347809=CARTESIAN_POINT('Ctrl Pts',(4.45408324399994,2.2,-0.376221450000016));
#347810=CARTESIAN_POINT('Ctrl Pts',(4.45611290699994,12.2,-0.375405844000016));
#347811=CARTESIAN_POINT('Ctrl Pts',(4.45611290699994,5.2,-0.375405844000016));
#347812=CARTESIAN_POINT('Ctrl Pts',(4.45611290699994,2.2,-0.375405844000016));
#347813=CARTESIAN_POINT('Ctrl Pts',(4.45814525899995,12.2,-0.374586587000016));
#347814=CARTESIAN_POINT('Ctrl Pts',(4.45814525899995,5.2,-0.374586587000016));
#347815=CARTESIAN_POINT('Ctrl Pts',(4.45814525899995,2.2,-0.374586587000016));
#347816=CARTESIAN_POINT('Ctrl Pts',(4.46018028999995,12.2,-0.373763677000016));
#347817=CARTESIAN_POINT('Ctrl Pts',(4.46018028999995,5.2,-0.373763677000016));
#347818=CARTESIAN_POINT('Ctrl Pts',(4.46018028999995,2.2,-0.373763677000016));
#347819=CARTESIAN_POINT('Ctrl Pts',(4.46221799099995,12.2,-0.372937107000015));
#347820=CARTESIAN_POINT('Ctrl Pts',(4.46221799099995,5.2,-0.372937107000015));
#347821=CARTESIAN_POINT('Ctrl Pts',(4.46221799099995,2.2,-0.372937107000015));
#347822=CARTESIAN_POINT('Ctrl Pts',(4.46425835499995,12.2,-0.372106875000018));
#347823=CARTESIAN_POINT('Ctrl Pts',(4.46425835499995,5.2,-0.372106875000018));
#347824=CARTESIAN_POINT('Ctrl Pts',(4.46425835499995,2.2,-0.372106875000018));
#347825=CARTESIAN_POINT('Ctrl Pts',(4.46630137099994,12.2,-0.371272974000014));
#347826=CARTESIAN_POINT('Ctrl Pts',(4.46630137099994,5.2,-0.371272974000014));
#347827=CARTESIAN_POINT('Ctrl Pts',(4.46630137099994,2.2,-0.371272974000014));
#347828=CARTESIAN_POINT('Ctrl Pts',(4.46834702999995,12.2,-0.370435403000013));
#347829=CARTESIAN_POINT('Ctrl Pts',(4.46834702999995,5.2,-0.370435403000013));
#347830=CARTESIAN_POINT('Ctrl Pts',(4.46834702999995,2.2,-0.370435403000013));
#347831=CARTESIAN_POINT('Ctrl Pts',(4.47039532399994,12.2,-0.369594155000015));
#347832=CARTESIAN_POINT('Ctrl Pts',(4.47039532399994,5.2,-0.369594155000015));
#347833=CARTESIAN_POINT('Ctrl Pts',(4.47039532399994,2.2,-0.369594155000015));
#347834=CARTESIAN_POINT('Ctrl Pts',(4.47244624199994,12.2,-0.368749227000014));
#347835=CARTESIAN_POINT('Ctrl Pts',(4.47244624199994,5.2,-0.368749227000014));
#347836=CARTESIAN_POINT('Ctrl Pts',(4.47244624199994,2.2,-0.368749227000014));
#347837=CARTESIAN_POINT('Ctrl Pts',(4.47449977699994,12.2,-0.367900614000014));
#347838=CARTESIAN_POINT('Ctrl Pts',(4.47449977699994,5.2,-0.367900614000014));
#347839=CARTESIAN_POINT('Ctrl Pts',(4.47449977699994,2.2,-0.367900614000014));
#347840=CARTESIAN_POINT('Ctrl Pts',(4.47655591799994,12.2,-0.367048314000016));
#347841=CARTESIAN_POINT('Ctrl Pts',(4.47655591799994,5.2,-0.367048314000016));
#347842=CARTESIAN_POINT('Ctrl Pts',(4.47655591799994,2.2,-0.367048314000016));
#347843=CARTESIAN_POINT('Ctrl Pts',(4.47861465699994,12.2,-0.366192320000014));
#347844=CARTESIAN_POINT('Ctrl Pts',(4.47861465699994,5.2,-0.366192320000014));
#347845=CARTESIAN_POINT('Ctrl Pts',(4.47861465699994,2.2,-0.366192320000014));
#347846=CARTESIAN_POINT('Ctrl Pts',(4.48067598499994,12.2,-0.365332629000013));
#347847=CARTESIAN_POINT('Ctrl Pts',(4.48067598499994,5.2,-0.365332629000013));
#347848=CARTESIAN_POINT('Ctrl Pts',(4.48067598499994,2.2,-0.365332629000013));
#347849=CARTESIAN_POINT('Ctrl Pts',(4.48273989399994,12.2,-0.364469238000016));
#347850=CARTESIAN_POINT('Ctrl Pts',(4.48273989399994,5.2,-0.364469238000016));
#347851=CARTESIAN_POINT('Ctrl Pts',(4.48273989399994,2.2,-0.364469238000016));
#347852=CARTESIAN_POINT('Ctrl Pts',(4.48480637199994,12.2,-0.363602142000015));
#347853=CARTESIAN_POINT('Ctrl Pts',(4.48480637199994,5.2,-0.363602142000015));
#347854=CARTESIAN_POINT('Ctrl Pts',(4.48480637199994,2.2,-0.363602142000015));
#347855=CARTESIAN_POINT('Ctrl Pts',(4.48687541199994,12.2,-0.362731335000017));
#347856=CARTESIAN_POINT('Ctrl Pts',(4.48687541199994,5.2,-0.362731335000017));
#347857=CARTESIAN_POINT('Ctrl Pts',(4.48687541199994,2.2,-0.362731335000017));
#347858=CARTESIAN_POINT('Ctrl Pts',(4.48894700499994,12.2,-0.361856816000015));
#347859=CARTESIAN_POINT('Ctrl Pts',(4.48894700499994,5.2,-0.361856816000015));
#347860=CARTESIAN_POINT('Ctrl Pts',(4.48894700499994,2.2,-0.361856816000015));
#347861=CARTESIAN_POINT('Ctrl Pts',(4.49102114199994,12.2,-0.360978579000015));
#347862=CARTESIAN_POINT('Ctrl Pts',(4.49102114199994,5.2,-0.360978579000015));
#347863=CARTESIAN_POINT('Ctrl Pts',(4.49102114199994,2.2,-0.360978579000015));
#347864=CARTESIAN_POINT('Ctrl Pts',(4.49309781399994,12.2,-0.360096621000014));
#347865=CARTESIAN_POINT('Ctrl Pts',(4.49309781399994,5.2,-0.360096621000014));
#347866=CARTESIAN_POINT('Ctrl Pts',(4.49309781399994,2.2,-0.360096621000014));
#347867=CARTESIAN_POINT('Ctrl Pts',(4.49517701099994,12.2,-0.359210937000016));
#347868=CARTESIAN_POINT('Ctrl Pts',(4.49517701099994,5.2,-0.359210937000016));
#347869=CARTESIAN_POINT('Ctrl Pts',(4.49517701099994,2.2,-0.359210937000016));
#347870=CARTESIAN_POINT('Ctrl Pts',(4.49725872399994,12.2,-0.358321524000011));
#347871=CARTESIAN_POINT('Ctrl Pts',(4.49725872399994,5.2,-0.358321524000011));
#347872=CARTESIAN_POINT('Ctrl Pts',(4.49725872399994,2.2,-0.358321524000011));
#347873=CARTESIAN_POINT('Ctrl Pts',(4.49934294599994,12.2,-0.357428377000013));
#347874=CARTESIAN_POINT('Ctrl Pts',(4.49934294599994,5.2,-0.357428377000013));
#347875=CARTESIAN_POINT('Ctrl Pts',(4.49934294599994,2.2,-0.357428377000013));
#347876=CARTESIAN_POINT('Ctrl Pts',(4.50142966599994,12.2,-0.356531493000016));
#347877=CARTESIAN_POINT('Ctrl Pts',(4.50142966599994,5.2,-0.356531493000016));
#347878=CARTESIAN_POINT('Ctrl Pts',(4.50142966599994,2.2,-0.356531493000016));
#347879=CARTESIAN_POINT('Ctrl Pts',(4.50351887499994,12.2,-0.355630868000016));
#347880=CARTESIAN_POINT('Ctrl Pts',(4.50351887499994,5.2,-0.355630868000016));
#347881=CARTESIAN_POINT('Ctrl Pts',(4.50351887499994,2.2,-0.355630868000016));
#347882=CARTESIAN_POINT('Ctrl Pts',(4.50561056499994,12.2,-0.354726498000013));
#347883=CARTESIAN_POINT('Ctrl Pts',(4.50561056499994,5.2,-0.354726498000013));
#347884=CARTESIAN_POINT('Ctrl Pts',(4.50561056499994,2.2,-0.354726498000013));
#347885=CARTESIAN_POINT('Ctrl Pts',(4.50770472699994,12.2,-0.353818377000015));
#347886=CARTESIAN_POINT('Ctrl Pts',(4.50770472699994,5.2,-0.353818377000015));
#347887=CARTESIAN_POINT('Ctrl Pts',(4.50770472699994,2.2,-0.353818377000015));
#347888=CARTESIAN_POINT('Ctrl Pts',(4.50980135199994,12.2,-0.352906504000017));
#347889=CARTESIAN_POINT('Ctrl Pts',(4.50980135199994,5.2,-0.352906504000017));
#347890=CARTESIAN_POINT('Ctrl Pts',(4.50980135199994,2.2,-0.352906504000017));
#347891=CARTESIAN_POINT('Ctrl Pts',(4.51190043099994,12.2,-0.351990873000014));
#347892=CARTESIAN_POINT('Ctrl Pts',(4.51190043099994,5.2,-0.351990873000014));
#347893=CARTESIAN_POINT('Ctrl Pts',(4.51190043099994,2.2,-0.351990873000014));
#347894=CARTESIAN_POINT('Ctrl Pts',(4.51400195399994,12.2,-0.351071482000016));
#347895=CARTESIAN_POINT('Ctrl Pts',(4.51400195399994,5.2,-0.351071482000016));
#347896=CARTESIAN_POINT('Ctrl Pts',(4.51400195399994,2.2,-0.351071482000016));
#347897=CARTESIAN_POINT('Ctrl Pts',(4.51610591499994,12.2,-0.350148326000017));
#347898=CARTESIAN_POINT('Ctrl Pts',(4.51610591499994,5.2,-0.350148326000017));
#347899=CARTESIAN_POINT('Ctrl Pts',(4.51610591499994,2.2,-0.350148326000017));
#347900=CARTESIAN_POINT('Ctrl Pts',(4.51821229999995,12.2,-0.349221402000013));
#347901=CARTESIAN_POINT('Ctrl Pts',(4.51821229999995,5.2,-0.349221402000013));
#347902=CARTESIAN_POINT('Ctrl Pts',(4.51821229999995,2.2,-0.349221402000013));
#347903=CARTESIAN_POINT('Ctrl Pts',(4.52032110499994,12.2,-0.348290705000016));
#347904=CARTESIAN_POINT('Ctrl Pts',(4.52032110499994,5.2,-0.348290705000016));
#347905=CARTESIAN_POINT('Ctrl Pts',(4.52032110499994,2.2,-0.348290705000016));
#347906=CARTESIAN_POINT('Ctrl Pts',(4.52243231899994,12.2,-0.347356232000013));
#347907=CARTESIAN_POINT('Ctrl Pts',(4.52243231899994,5.2,-0.347356232000013));
#347908=CARTESIAN_POINT('Ctrl Pts',(4.52243231899994,2.2,-0.347356232000013));
#347909=CARTESIAN_POINT('Ctrl Pts',(4.52454593299994,12.2,-0.346417978000013));
#347910=CARTESIAN_POINT('Ctrl Pts',(4.52454593299994,5.2,-0.346417978000013));
#347911=CARTESIAN_POINT('Ctrl Pts',(4.52454593299994,2.2,-0.346417978000013));
#347912=CARTESIAN_POINT('Ctrl Pts',(4.52666193799994,12.2,-0.345475941000015));
#347913=CARTESIAN_POINT('Ctrl Pts',(4.52666193799994,5.2,-0.345475941000015));
#347914=CARTESIAN_POINT('Ctrl Pts',(4.52666193799994,2.2,-0.345475941000015));
#347915=CARTESIAN_POINT('Ctrl Pts',(4.52878032599994,12.2,-0.344530117000015));
#347916=CARTESIAN_POINT('Ctrl Pts',(4.52878032599994,5.2,-0.344530117000015));
#347917=CARTESIAN_POINT('Ctrl Pts',(4.52878032599994,2.2,-0.344530117000015));
#347918=CARTESIAN_POINT('Ctrl Pts',(4.53090108699994,12.2,-0.343580501000016));
#347919=CARTESIAN_POINT('Ctrl Pts',(4.53090108699994,5.2,-0.343580501000016));
#347920=CARTESIAN_POINT('Ctrl Pts',(4.53090108699994,2.2,-0.343580501000016));
#347921=CARTESIAN_POINT('Ctrl Pts',(4.53302421399994,12.2,-0.342627090000014));
#347922=CARTESIAN_POINT('Ctrl Pts',(4.53302421399994,5.2,-0.342627090000014));
#347923=CARTESIAN_POINT('Ctrl Pts',(4.53302421399994,2.2,-0.342627090000014));
#347924=CARTESIAN_POINT('Ctrl Pts',(4.53514969499994,12.2,-0.341669881000013));
#347925=CARTESIAN_POINT('Ctrl Pts',(4.53514969499994,5.2,-0.341669881000013));
#347926=CARTESIAN_POINT('Ctrl Pts',(4.53514969499994,2.2,-0.341669881000013));
#347927=CARTESIAN_POINT('Ctrl Pts',(4.53727752399994,12.2,-0.340708870000017));
#347928=CARTESIAN_POINT('Ctrl Pts',(4.53727752399994,5.2,-0.340708870000017));
#347929=CARTESIAN_POINT('Ctrl Pts',(4.53727752399994,2.2,-0.340708870000017));
#347930=CARTESIAN_POINT('Ctrl Pts',(4.53940769099995,12.2,-0.339744052000013));
#347931=CARTESIAN_POINT('Ctrl Pts',(4.53940769099995,5.2,-0.339744052000013));
#347932=CARTESIAN_POINT('Ctrl Pts',(4.53940769099995,2.2,-0.339744052000013));
#347933=CARTESIAN_POINT('Ctrl Pts',(4.54154018699994,12.2,-0.338775425000013));
#347934=CARTESIAN_POINT('Ctrl Pts',(4.54154018699994,5.2,-0.338775425000013));
#347935=CARTESIAN_POINT('Ctrl Pts',(4.54154018699994,2.2,-0.338775425000013));
#347936=CARTESIAN_POINT('Ctrl Pts',(4.54367500399994,12.2,-0.337802984000017));
#347937=CARTESIAN_POINT('Ctrl Pts',(4.54367500399994,5.2,-0.337802984000017));
#347938=CARTESIAN_POINT('Ctrl Pts',(4.54367500399994,2.2,-0.337802984000017));
#347939=CARTESIAN_POINT('Ctrl Pts',(4.54581213099994,12.2,-0.336826727000012));
#347940=CARTESIAN_POINT('Ctrl Pts',(4.54581213099994,5.2,-0.336826727000012));
#347941=CARTESIAN_POINT('Ctrl Pts',(4.54581213099994,2.2,-0.336826727000012));
#347942=CARTESIAN_POINT('Ctrl Pts',(4.54795156299994,12.2,-0.335846649000011));
#347943=CARTESIAN_POINT('Ctrl Pts',(4.54795156299994,5.2,-0.335846649000011));
#347944=CARTESIAN_POINT('Ctrl Pts',(4.54795156299994,2.2,-0.335846649000011));
#347945=CARTESIAN_POINT('Ctrl Pts',(4.55009328699994,12.2,-0.334862747000013));
#347946=CARTESIAN_POINT('Ctrl Pts',(4.55009328699994,5.2,-0.334862747000013));
#347947=CARTESIAN_POINT('Ctrl Pts',(4.55009328699994,2.2,-0.334862747000013));
#347948=CARTESIAN_POINT('Ctrl Pts',(4.55223729599994,12.2,-0.333875018000014));
#347949=CARTESIAN_POINT('Ctrl Pts',(4.55223729599994,5.2,-0.333875018000014));
#347950=CARTESIAN_POINT('Ctrl Pts',(4.55223729599994,2.2,-0.333875018000014));
#347951=CARTESIAN_POINT('Ctrl Pts',(4.55438358299994,12.2,-0.332883458000013));
#347952=CARTESIAN_POINT('Ctrl Pts',(4.55438358299994,5.2,-0.332883458000013));
#347953=CARTESIAN_POINT('Ctrl Pts',(4.55438358299994,2.2,-0.332883458000013));
#347954=CARTESIAN_POINT('Ctrl Pts',(4.55653213599994,12.2,-0.331888063000014));
#347955=CARTESIAN_POINT('Ctrl Pts',(4.55653213599994,5.2,-0.331888063000014));
#347956=CARTESIAN_POINT('Ctrl Pts',(4.55653213599994,2.2,-0.331888063000014));
#347957=CARTESIAN_POINT('Ctrl Pts',(4.55868294799994,12.2,-0.330888829000013));
#347958=CARTESIAN_POINT('Ctrl Pts',(4.55868294799994,5.2,-0.330888829000013));
#347959=CARTESIAN_POINT('Ctrl Pts',(4.55868294799994,2.2,-0.330888829000013));
#347960=CARTESIAN_POINT('Ctrl Pts',(4.56083600999994,12.2,-0.329885755000014));
#347961=CARTESIAN_POINT('Ctrl Pts',(4.56083600999994,5.2,-0.329885755000014));
#347962=CARTESIAN_POINT('Ctrl Pts',(4.56083600999994,2.2,-0.329885755000014));
#347963=CARTESIAN_POINT('Ctrl Pts',(4.56299131399994,12.2,-0.328878835000013));
#347964=CARTESIAN_POINT('Ctrl Pts',(4.56299131399994,5.2,-0.328878835000013));
#347965=CARTESIAN_POINT('Ctrl Pts',(4.56299131399994,2.2,-0.328878835000013));
#347966=CARTESIAN_POINT('Ctrl Pts',(4.56514884899994,12.2,-0.327868067000012));
#347967=CARTESIAN_POINT('Ctrl Pts',(4.56514884899994,5.2,-0.327868067000012));
#347968=CARTESIAN_POINT('Ctrl Pts',(4.56514884899994,2.2,-0.327868067000012));
#347969=CARTESIAN_POINT('Ctrl Pts',(4.56730860799994,12.2,-0.326853447000013));
#347970=CARTESIAN_POINT('Ctrl Pts',(4.56730860799994,5.2,-0.326853447000013));
#347971=CARTESIAN_POINT('Ctrl Pts',(4.56730860799994,2.2,-0.326853447000013));
#347972=CARTESIAN_POINT('Ctrl Pts',(4.56947058099994,12.2,-0.325834970000014));
#347973=CARTESIAN_POINT('Ctrl Pts',(4.56947058099994,5.2,-0.325834970000014));
#347974=CARTESIAN_POINT('Ctrl Pts',(4.56947058099994,2.2,-0.325834970000014));
#347975=CARTESIAN_POINT('Ctrl Pts',(4.57163476099994,12.2,-0.324812636000011));
#347976=CARTESIAN_POINT('Ctrl Pts',(4.57163476099994,5.2,-0.324812636000011));
#347977=CARTESIAN_POINT('Ctrl Pts',(4.57163476099994,2.2,-0.324812636000011));
#347978=CARTESIAN_POINT('Ctrl Pts',(4.57380113799994,12.2,-0.323786439000013));
#347979=CARTESIAN_POINT('Ctrl Pts',(4.57380113799994,5.2,-0.323786439000013));
#347980=CARTESIAN_POINT('Ctrl Pts',(4.57380113799994,2.2,-0.323786439000013));
#347981=CARTESIAN_POINT('Ctrl Pts',(4.57596970299994,12.2,-0.322756377000015));
#347982=CARTESIAN_POINT('Ctrl Pts',(4.57596970299994,5.2,-0.322756377000015));
#347983=CARTESIAN_POINT('Ctrl Pts',(4.57596970299994,2.2,-0.322756377000015));
#347984=CARTESIAN_POINT('Ctrl Pts',(4.57814044899994,12.2,-0.321722446000017));
#347985=CARTESIAN_POINT('Ctrl Pts',(4.57814044899994,5.2,-0.321722446000017));
#347986=CARTESIAN_POINT('Ctrl Pts',(4.57814044899994,2.2,-0.321722446000017));
#347987=CARTESIAN_POINT('Ctrl Pts',(4.58031336499994,12.2,-0.320684641000017));
#347988=CARTESIAN_POINT('Ctrl Pts',(4.58031336499994,5.2,-0.320684641000017));
#347989=CARTESIAN_POINT('Ctrl Pts',(4.58031336499994,2.2,-0.320684641000017));
#347990=CARTESIAN_POINT('Ctrl Pts',(4.58248844399994,12.2,-0.319642962000017));
#347991=CARTESIAN_POINT('Ctrl Pts',(4.58248844399994,5.2,-0.319642962000017));
#347992=CARTESIAN_POINT('Ctrl Pts',(4.58248844399994,2.2,-0.319642962000017));
#347993=CARTESIAN_POINT('Ctrl Pts',(4.58466567599994,12.2,-0.318597404000016));
#347994=CARTESIAN_POINT('Ctrl Pts',(4.58466567599994,5.2,-0.318597404000016));
#347995=CARTESIAN_POINT('Ctrl Pts',(4.58466567599994,2.2,-0.318597404000016));
#347996=CARTESIAN_POINT('Ctrl Pts',(4.58684505399994,12.2,-0.317547963000013));
#347997=CARTESIAN_POINT('Ctrl Pts',(4.58684505399994,5.2,-0.317547963000013));
#347998=CARTESIAN_POINT('Ctrl Pts',(4.58684505399994,2.2,-0.317547963000013));
#347999=CARTESIAN_POINT('Ctrl Pts',(4.58902656699994,12.2,-0.316494638000013));
#348000=CARTESIAN_POINT('Ctrl Pts',(4.58902656699994,5.2,-0.316494638000013));
#348001=CARTESIAN_POINT('Ctrl Pts',(4.58902656699994,2.2,-0.316494638000013));
#348002=CARTESIAN_POINT('Ctrl Pts',(4.59121020699994,12.2,-0.315437423000016));
#348003=CARTESIAN_POINT('Ctrl Pts',(4.59121020699994,5.2,-0.315437423000016));
#348004=CARTESIAN_POINT('Ctrl Pts',(4.59121020699994,2.2,-0.315437423000016));
#348005=CARTESIAN_POINT('Ctrl Pts',(4.59339596799994,12.2,-0.314376316000011));
#348006=CARTESIAN_POINT('Ctrl Pts',(4.59339596799994,5.2,-0.314376316000011));
#348007=CARTESIAN_POINT('Ctrl Pts',(4.59339596799994,2.2,-0.314376316000011));
#348008=CARTESIAN_POINT('Ctrl Pts',(4.59558383799994,12.2,-0.313311314000018));
#348009=CARTESIAN_POINT('Ctrl Pts',(4.59558383799994,5.2,-0.313311314000018));
#348010=CARTESIAN_POINT('Ctrl Pts',(4.59558383799994,2.2,-0.313311314000018));
#348011=CARTESIAN_POINT('Ctrl Pts',(4.59777380999994,12.2,-0.312242414000017));
#348012=CARTESIAN_POINT('Ctrl Pts',(4.59777380999994,5.2,-0.312242414000017));
#348013=CARTESIAN_POINT('Ctrl Pts',(4.59777380999994,2.2,-0.312242414000017));
#348014=CARTESIAN_POINT('Ctrl Pts',(4.59996587399994,12.2,-0.311169612000013));
#348015=CARTESIAN_POINT('Ctrl Pts',(4.59996587399994,5.2,-0.311169612000013));
#348016=CARTESIAN_POINT('Ctrl Pts',(4.59996587399994,2.2,-0.311169612000013));
#348017=CARTESIAN_POINT('Ctrl Pts',(4.60216002199994,12.2,-0.310092905000015));
#348018=CARTESIAN_POINT('Ctrl Pts',(4.60216002199994,5.2,-0.310092905000015));
#348019=CARTESIAN_POINT('Ctrl Pts',(4.60216002199994,2.2,-0.310092905000015));
#348020=CARTESIAN_POINT('Ctrl Pts',(4.60435624599994,12.2,-0.309012290000013));
#348021=CARTESIAN_POINT('Ctrl Pts',(4.60435624599994,5.2,-0.309012290000013));
#348022=CARTESIAN_POINT('Ctrl Pts',(4.60435624599994,2.2,-0.309012290000013));
#348023=CARTESIAN_POINT('Ctrl Pts',(4.60655453599994,12.2,-0.307927764000016));
#348024=CARTESIAN_POINT('Ctrl Pts',(4.60655453599994,5.2,-0.307927764000016));
#348025=CARTESIAN_POINT('Ctrl Pts',(4.60655453599994,2.2,-0.307927764000016));
#348026=CARTESIAN_POINT('Ctrl Pts',(4.60875488599994,12.2,-0.306839323000014));
#348027=CARTESIAN_POINT('Ctrl Pts',(4.60875488599994,5.2,-0.306839323000014));
#348028=CARTESIAN_POINT('Ctrl Pts',(4.60875488599994,2.2,-0.306839323000014));
#348029=CARTESIAN_POINT('Ctrl Pts',(4.61095728299994,12.2,-0.305746966000013));
#348030=CARTESIAN_POINT('Ctrl Pts',(4.61095728299994,5.2,-0.305746966000013));
#348031=CARTESIAN_POINT('Ctrl Pts',(4.61095728299994,2.2,-0.305746966000013));
#348032=CARTESIAN_POINT('Ctrl Pts',(4.61316172299994,12.2,-0.304650688000017));
#348033=CARTESIAN_POINT('Ctrl Pts',(4.61316172299994,5.2,-0.304650688000017));
#348034=CARTESIAN_POINT('Ctrl Pts',(4.61316172299994,2.2,-0.304650688000017));
#348035=CARTESIAN_POINT('Ctrl Pts',(4.61536819599994,12.2,-0.303550486000015));
#348036=CARTESIAN_POINT('Ctrl Pts',(4.61536819599994,5.2,-0.303550486000015));
#348037=CARTESIAN_POINT('Ctrl Pts',(4.61536819599994,2.2,-0.303550486000015));
#348038=CARTESIAN_POINT('Ctrl Pts',(4.61757669099994,12.2,-0.302446358000013));
#348039=CARTESIAN_POINT('Ctrl Pts',(4.61757669099994,5.2,-0.302446358000013));
#348040=CARTESIAN_POINT('Ctrl Pts',(4.61757669099994,2.2,-0.302446358000013));
#348041=CARTESIAN_POINT('Ctrl Pts',(4.61978720099994,12.2,-0.301338300000014));
#348042=CARTESIAN_POINT('Ctrl Pts',(4.61978720099994,5.2,-0.301338300000014));
#348043=CARTESIAN_POINT('Ctrl Pts',(4.61978720099994,2.2,-0.301338300000014));
#348044=CARTESIAN_POINT('Ctrl Pts',(4.62199971899994,12.2,-0.300226309000013));
#348045=CARTESIAN_POINT('Ctrl Pts',(4.62199971899994,5.2,-0.300226309000013));
#348046=CARTESIAN_POINT('Ctrl Pts',(4.62199971899994,2.2,-0.300226309000013));
#348047=CARTESIAN_POINT('Ctrl Pts',(4.62421423299994,12.2,-0.299110383000016));
#348048=CARTESIAN_POINT('Ctrl Pts',(4.62421423299994,5.2,-0.299110383000016));
#348049=CARTESIAN_POINT('Ctrl Pts',(4.62421423299994,2.2,-0.299110383000016));
#348050=CARTESIAN_POINT('Ctrl Pts',(4.62643073799994,12.2,-0.297990517000013));
#348051=CARTESIAN_POINT('Ctrl Pts',(4.62643073799994,5.2,-0.297990517000013));
#348052=CARTESIAN_POINT('Ctrl Pts',(4.62643073799994,2.2,-0.297990517000013));
#348053=CARTESIAN_POINT('Ctrl Pts',(4.62864922299994,12.2,-0.296866710000017));
#348054=CARTESIAN_POINT('Ctrl Pts',(4.62864922299994,5.2,-0.296866710000017));
#348055=CARTESIAN_POINT('Ctrl Pts',(4.62864922299994,2.2,-0.296866710000017));
#348056=CARTESIAN_POINT('Ctrl Pts',(4.63086967999994,12.2,-0.295738958000014));
#348057=CARTESIAN_POINT('Ctrl Pts',(4.63086967999994,5.2,-0.295738958000014));
#348058=CARTESIAN_POINT('Ctrl Pts',(4.63086967999994,2.2,-0.295738958000014));
#348059=CARTESIAN_POINT('Ctrl Pts',(4.63309210099994,12.2,-0.294607259000017));
#348060=CARTESIAN_POINT('Ctrl Pts',(4.63309210099994,5.2,-0.294607259000017));
#348061=CARTESIAN_POINT('Ctrl Pts',(4.63309210099994,2.2,-0.294607259000017));
#348062=CARTESIAN_POINT('Ctrl Pts',(4.63531647699994,12.2,-0.293471608000013));
#348063=CARTESIAN_POINT('Ctrl Pts',(4.63531647699994,5.2,-0.293471608000013));
#348064=CARTESIAN_POINT('Ctrl Pts',(4.63531647699994,2.2,-0.293471608000013));
#348065=CARTESIAN_POINT('Ctrl Pts',(4.63754279899994,12.2,-0.292332005000016));
#348066=CARTESIAN_POINT('Ctrl Pts',(4.63754279899994,5.2,-0.292332005000016));
#348067=CARTESIAN_POINT('Ctrl Pts',(4.63754279899994,2.2,-0.292332005000016));
#348068=CARTESIAN_POINT('Ctrl Pts',(4.63977105899995,12.2,-0.291188445000015));
#348069=CARTESIAN_POINT('Ctrl Pts',(4.63977105899995,5.2,-0.291188445000015));
#348070=CARTESIAN_POINT('Ctrl Pts',(4.63977105899995,2.2,-0.291188445000015));
#348071=CARTESIAN_POINT('Ctrl Pts',(4.64200124899994,12.2,-0.290040925000015));
#348072=CARTESIAN_POINT('Ctrl Pts',(4.64200124899994,5.2,-0.290040925000015));
#348073=CARTESIAN_POINT('Ctrl Pts',(4.64200124899994,2.2,-0.290040925000015));
#348074=CARTESIAN_POINT('Ctrl Pts',(4.64423335999994,12.2,-0.288889443000016));
#348075=CARTESIAN_POINT('Ctrl Pts',(4.64423335999994,5.2,-0.288889443000016));
#348076=CARTESIAN_POINT('Ctrl Pts',(4.64423335999994,2.2,-0.288889443000016));
#348077=CARTESIAN_POINT('Ctrl Pts',(4.64646738299994,12.2,-0.287733996000017));
#348078=CARTESIAN_POINT('Ctrl Pts',(4.64646738299994,5.2,-0.287733996000017));
#348079=CARTESIAN_POINT('Ctrl Pts',(4.64646738299994,2.2,-0.287733996000017));
#348080=CARTESIAN_POINT('Ctrl Pts',(4.64870330999994,12.2,-0.286574581000014));
#348081=CARTESIAN_POINT('Ctrl Pts',(4.64870330999994,5.2,-0.286574581000014));
#348082=CARTESIAN_POINT('Ctrl Pts',(4.64870330999994,2.2,-0.286574581000014));
#348083=CARTESIAN_POINT('Ctrl Pts',(4.65094113199994,12.2,-0.285411196000016));
#348084=CARTESIAN_POINT('Ctrl Pts',(4.65094113199994,5.2,-0.285411196000016));
#348085=CARTESIAN_POINT('Ctrl Pts',(4.65094113199994,2.2,-0.285411196000016));
#348086=CARTESIAN_POINT('Ctrl Pts',(4.65318083999995,12.2,-0.284243837000013));
#348087=CARTESIAN_POINT('Ctrl Pts',(4.65318083999995,5.2,-0.284243837000013));
#348088=CARTESIAN_POINT('Ctrl Pts',(4.65318083999995,2.2,-0.284243837000013));
#348089=CARTESIAN_POINT('Ctrl Pts',(4.65542242799994,12.2,-0.283072500000014));
#348090=CARTESIAN_POINT('Ctrl Pts',(4.65542242799994,5.2,-0.283072500000014));
#348091=CARTESIAN_POINT('Ctrl Pts',(4.65542242799994,2.2,-0.283072500000014));
#348092=CARTESIAN_POINT('Ctrl Pts',(4.65766588499995,12.2,-0.281897186000015));
#348093=CARTESIAN_POINT('Ctrl Pts',(4.65766588499995,5.2,-0.281897186000015));
#348094=CARTESIAN_POINT('Ctrl Pts',(4.65766588499995,2.2,-0.281897186000015));
#348095=CARTESIAN_POINT('Ctrl Pts',(4.65991120199994,12.2,-0.280717888000015));
#348096=CARTESIAN_POINT('Ctrl Pts',(4.65991120199994,5.2,-0.280717888000015));
#348097=CARTESIAN_POINT('Ctrl Pts',(4.65991120199994,2.2,-0.280717888000015));
#348098=CARTESIAN_POINT('Ctrl Pts',(4.66215837399994,12.2,-0.279534606000014));
#348099=CARTESIAN_POINT('Ctrl Pts',(4.66215837399994,5.2,-0.279534606000014));
#348100=CARTESIAN_POINT('Ctrl Pts',(4.66215837399994,2.2,-0.279534606000014));
#348101=CARTESIAN_POINT('Ctrl Pts',(4.66440738899994,12.2,-0.278347336000015));
#348102=CARTESIAN_POINT('Ctrl Pts',(4.66440738899994,5.2,-0.278347336000015));
#348103=CARTESIAN_POINT('Ctrl Pts',(4.66440738899994,2.2,-0.278347336000015));
#348104=CARTESIAN_POINT('Ctrl Pts',(4.66665823999994,12.2,-0.277156077000011));
#348105=CARTESIAN_POINT('Ctrl Pts',(4.66665823999994,5.2,-0.277156077000011));
#348106=CARTESIAN_POINT('Ctrl Pts',(4.66665823999994,2.2,-0.277156077000011));
#348107=CARTESIAN_POINT('Ctrl Pts',(4.66891091999995,12.2,-0.275960824000014));
#348108=CARTESIAN_POINT('Ctrl Pts',(4.66891091999995,5.2,-0.275960824000014));
#348109=CARTESIAN_POINT('Ctrl Pts',(4.66891091999995,2.2,-0.275960824000014));
#348110=CARTESIAN_POINT('Ctrl Pts',(4.67116541799994,12.2,-0.274761575000015));
#348111=CARTESIAN_POINT('Ctrl Pts',(4.67116541799994,5.2,-0.274761575000015));
#348112=CARTESIAN_POINT('Ctrl Pts',(4.67116541799994,2.2,-0.274761575000015));
#348113=CARTESIAN_POINT('Ctrl Pts',(4.67342172599994,12.2,-0.273558329000014));
#348114=CARTESIAN_POINT('Ctrl Pts',(4.67342172599994,5.2,-0.273558329000014));
#348115=CARTESIAN_POINT('Ctrl Pts',(4.67342172599994,2.2,-0.273558329000014));
#348116=CARTESIAN_POINT('Ctrl Pts',(4.67567983699994,12.2,-0.272351081000015));
#348117=CARTESIAN_POINT('Ctrl Pts',(4.67567983699994,5.2,-0.272351081000015));
#348118=CARTESIAN_POINT('Ctrl Pts',(4.67567983699994,2.2,-0.272351081000015));
#348119=CARTESIAN_POINT('Ctrl Pts',(4.67793973999994,12.2,-0.271139829000013));
#348120=CARTESIAN_POINT('Ctrl Pts',(4.67793973999994,5.2,-0.271139829000013));
#348121=CARTESIAN_POINT('Ctrl Pts',(4.67793973999994,2.2,-0.271139829000013));
#348122=CARTESIAN_POINT('Ctrl Pts',(4.68020142899994,12.2,-0.269924571000013));
#348123=CARTESIAN_POINT('Ctrl Pts',(4.68020142899994,5.2,-0.269924571000013));
#348124=CARTESIAN_POINT('Ctrl Pts',(4.68020142899994,2.2,-0.269924571000013));
#348125=CARTESIAN_POINT('Ctrl Pts',(4.68246489399994,12.2,-0.268705303000014));
#348126=CARTESIAN_POINT('Ctrl Pts',(4.68246489399994,5.2,-0.268705303000014));
#348127=CARTESIAN_POINT('Ctrl Pts',(4.68246489399994,2.2,-0.268705303000014));
#348128=CARTESIAN_POINT('Ctrl Pts',(4.68473012899994,12.2,-0.267482024000016));
#348129=CARTESIAN_POINT('Ctrl Pts',(4.68473012899994,5.2,-0.267482024000016));
#348130=CARTESIAN_POINT('Ctrl Pts',(4.68473012899994,2.2,-0.267482024000016));
#348131=CARTESIAN_POINT('Ctrl Pts',(4.68699712299994,12.2,-0.266254731000015));
#348132=CARTESIAN_POINT('Ctrl Pts',(4.68699712299994,5.2,-0.266254731000015));
#348133=CARTESIAN_POINT('Ctrl Pts',(4.68699712299994,2.2,-0.266254731000015));
#348134=CARTESIAN_POINT('Ctrl Pts',(4.68926586999994,12.2,-0.265023422000015));
#348135=CARTESIAN_POINT('Ctrl Pts',(4.68926586999994,5.2,-0.265023422000015));
#348136=CARTESIAN_POINT('Ctrl Pts',(4.68926586999994,2.2,-0.265023422000015));
#348137=CARTESIAN_POINT('Ctrl Pts',(4.69153635799994,12.2,-0.263788092000015));
#348138=CARTESIAN_POINT('Ctrl Pts',(4.69153635799994,5.2,-0.263788092000015));
#348139=CARTESIAN_POINT('Ctrl Pts',(4.69153635799994,2.2,-0.263788092000015));
#348140=CARTESIAN_POINT('Ctrl Pts',(4.69380858299994,12.2,-0.262548742000015));
#348141=CARTESIAN_POINT('Ctrl Pts',(4.69380858299994,5.2,-0.262548742000015));
#348142=CARTESIAN_POINT('Ctrl Pts',(4.69380858299994,2.2,-0.262548742000015));
#348143=CARTESIAN_POINT('Ctrl Pts',(4.69608253499994,12.2,-0.261305367000015));
#348144=CARTESIAN_POINT('Ctrl Pts',(4.69608253499994,5.2,-0.261305367000015));
#348145=CARTESIAN_POINT('Ctrl Pts',(4.69608253499994,2.2,-0.261305367000015));
#348146=CARTESIAN_POINT('Ctrl Pts',(4.69835820499994,12.2,-0.260057964000016));
#348147=CARTESIAN_POINT('Ctrl Pts',(4.69835820499994,5.2,-0.260057964000016));
#348148=CARTESIAN_POINT('Ctrl Pts',(4.69835820499994,2.2,-0.260057964000016));
#348149=CARTESIAN_POINT('Ctrl Pts',(4.70063558299994,12.2,-0.258806532000015));
#348150=CARTESIAN_POINT('Ctrl Pts',(4.70063558299994,5.2,-0.258806532000015));
#348151=CARTESIAN_POINT('Ctrl Pts',(4.70063558299994,2.2,-0.258806532000015));
#348152=CARTESIAN_POINT('Ctrl Pts',(4.70291466199994,12.2,-0.257551068000015));
#348153=CARTESIAN_POINT('Ctrl Pts',(4.70291466199994,5.2,-0.257551068000015));
#348154=CARTESIAN_POINT('Ctrl Pts',(4.70291466199994,2.2,-0.257551068000015));
#348155=CARTESIAN_POINT('Ctrl Pts',(4.70519543299995,12.2,-0.256291568000013));
#348156=CARTESIAN_POINT('Ctrl Pts',(4.70519543299995,5.2,-0.256291568000013));
#348157=CARTESIAN_POINT('Ctrl Pts',(4.70519543299995,2.2,-0.256291568000013));
#348158=CARTESIAN_POINT('Ctrl Pts',(4.70747788699994,12.2,-0.255028032000015));
#348159=CARTESIAN_POINT('Ctrl Pts',(4.70747788699994,5.2,-0.255028032000015));
#348160=CARTESIAN_POINT('Ctrl Pts',(4.70747788699994,2.2,-0.255028032000015));
#348161=CARTESIAN_POINT('Ctrl Pts',(4.70976201899994,12.2,-0.253760456000016));
#348162=CARTESIAN_POINT('Ctrl Pts',(4.70976201899994,5.2,-0.253760456000016));
#348163=CARTESIAN_POINT('Ctrl Pts',(4.70976201899994,2.2,-0.253760456000016));
#348164=CARTESIAN_POINT('Ctrl Pts',(4.71204781699994,12.2,-0.252488839000016));
#348165=CARTESIAN_POINT('Ctrl Pts',(4.71204781699994,5.2,-0.252488839000016));
#348166=CARTESIAN_POINT('Ctrl Pts',(4.71204781699994,2.2,-0.252488839000016));
#348167=CARTESIAN_POINT('Ctrl Pts',(4.71433527799995,12.2,-0.251213177000014));
#348168=CARTESIAN_POINT('Ctrl Pts',(4.71433527799995,5.2,-0.251213177000014));
#348169=CARTESIAN_POINT('Ctrl Pts',(4.71433527799995,2.2,-0.251213177000014));
#348170=CARTESIAN_POINT('Ctrl Pts',(4.71662439299994,12.2,-0.249933470000014));
#348171=CARTESIAN_POINT('Ctrl Pts',(4.71662439299994,5.2,-0.249933470000014));
#348172=CARTESIAN_POINT('Ctrl Pts',(4.71662439299994,2.2,-0.249933470000014));
#348173=CARTESIAN_POINT('Ctrl Pts',(4.71891515199994,12.2,-0.248649714000013));
#348174=CARTESIAN_POINT('Ctrl Pts',(4.71891515199994,5.2,-0.248649714000013));
#348175=CARTESIAN_POINT('Ctrl Pts',(4.71891515199994,2.2,-0.248649714000013));
#348176=CARTESIAN_POINT('Ctrl Pts',(4.72120754799994,12.2,-0.247361908000014));
#348177=CARTESIAN_POINT('Ctrl Pts',(4.72120754799994,5.2,-0.247361908000014));
#348178=CARTESIAN_POINT('Ctrl Pts',(4.72120754799994,2.2,-0.247361908000014));
#348179=CARTESIAN_POINT('Ctrl Pts',(4.72350156999994,12.2,-0.246070046000018));
#348180=CARTESIAN_POINT('Ctrl Pts',(4.72350156999994,5.2,-0.246070046000018));
#348181=CARTESIAN_POINT('Ctrl Pts',(4.72350156999994,2.2,-0.246070046000018));
#348182=CARTESIAN_POINT('Ctrl Pts',(4.72579720499995,12.2,-0.244774128000014));
#348183=CARTESIAN_POINT('Ctrl Pts',(4.72579720499995,5.2,-0.244774128000014));
#348184=CARTESIAN_POINT('Ctrl Pts',(4.72579720499995,2.2,-0.244774128000014));
#348185=CARTESIAN_POINT('Ctrl Pts',(4.72809444799994,12.2,-0.243474151000012));
#348186=CARTESIAN_POINT('Ctrl Pts',(4.72809444799994,5.2,-0.243474151000012));
#348187=CARTESIAN_POINT('Ctrl Pts',(4.72809444799994,2.2,-0.243474151000012));
#348188=CARTESIAN_POINT('Ctrl Pts',(4.73039328499994,12.2,-0.242170110000015));
#348189=CARTESIAN_POINT('Ctrl Pts',(4.73039328499994,5.2,-0.242170110000015));
#348190=CARTESIAN_POINT('Ctrl Pts',(4.73039328499994,2.2,-0.242170110000015));
#348191=CARTESIAN_POINT('Ctrl Pts',(4.73269371199994,12.2,-0.240862004000015));
#348192=CARTESIAN_POINT('Ctrl Pts',(4.73269371199994,5.2,-0.240862004000015));
#348193=CARTESIAN_POINT('Ctrl Pts',(4.73269371199994,2.2,-0.240862004000015));
#348194=CARTESIAN_POINT('Ctrl Pts',(4.73499571799994,12.2,-0.239549833000012));
#348195=CARTESIAN_POINT('Ctrl Pts',(4.73499571799994,5.2,-0.239549833000012));
#348196=CARTESIAN_POINT('Ctrl Pts',(4.73499571799994,2.2,-0.239549833000012));
#348197=CARTESIAN_POINT('Ctrl Pts',(4.73729930399994,12.2,-0.238233593000015));
#348198=CARTESIAN_POINT('Ctrl Pts',(4.73729930399994,5.2,-0.238233593000015));
#348199=CARTESIAN_POINT('Ctrl Pts',(4.73729930399994,2.2,-0.238233593000015));
#348200=CARTESIAN_POINT('Ctrl Pts',(4.73960446599994,12.2,-0.236913286000018));
#348201=CARTESIAN_POINT('Ctrl Pts',(4.73960446599994,5.2,-0.236913286000018));
#348202=CARTESIAN_POINT('Ctrl Pts',(4.73960446599994,2.2,-0.236913286000018));
#348203=CARTESIAN_POINT('Ctrl Pts',(4.74144985399994,12.2,-0.235853787000018));
#348204=CARTESIAN_POINT('Ctrl Pts',(4.74144985399994,5.2,-0.235853787000018));
#348205=CARTESIAN_POINT('Ctrl Pts',(4.74144985399994,2.2,-0.235853787000018));
#348206=CARTESIAN_POINT('Ctrl Pts',(4.74283460399994,12.2,-0.235057331000017));
#348207=CARTESIAN_POINT('Ctrl Pts',(4.74283460399994,5.2,-0.235057331000017));
#348208=CARTESIAN_POINT('Ctrl Pts',(4.74283460399994,2.2,-0.235057331000017));
#348209=CARTESIAN_POINT('Ctrl Pts',(4.74375808599994,12.2,-0.234525546000013));
#348210=CARTESIAN_POINT('Ctrl Pts',(4.74375808599994,5.2,-0.234525546000013));
#348211=CARTESIAN_POINT('Ctrl Pts',(4.74375808599994,2.2,-0.234525546000013));
#348212=CARTESIAN_POINT('Ctrl Pts',(4.74421990499994,12.2,-0.234259451000014));
#348213=CARTESIAN_POINT('Ctrl Pts',(4.74421990499994,5.2,-0.234259451000014));
#348214=CARTESIAN_POINT('Ctrl Pts',(4.74421990499994,2.2,-0.234259451000014));
#348215=CARTESIAN_POINT('Origin',(3.84237632699994,15.2,-1.08891369700002));
#348216=CARTESIAN_POINT('',(3.48765214499994,2.2,-0.988386318000014));
#348217=CARTESIAN_POINT('',(3.84242569899994,12.2,-1.08892768900001));
#348218=CARTESIAN_POINT('Origin',(-5.66300478732629E-14,15.2,-1.77635683940025E-14));
#348219=CARTESIAN_POINT('',(3.52236167599994,12.2,-1.88224078000002));
#348220=CARTESIAN_POINT('',(3.19715352599995,12.2,-1.70845963700001));
#348221=CARTESIAN_POINT('Ctrl Pts',(4.46529931499995,12.2,-1.61975369200002));
#348222=CARTESIAN_POINT('Ctrl Pts',(4.46529931499995,5.2,-1.61975369200002));
#348223=CARTESIAN_POINT('Ctrl Pts',(4.46529931499995,2.2,-1.61975369200002));
#348224=CARTESIAN_POINT('Ctrl Pts',(4.46497643499994,12.2,-1.61932962500002));
#348225=CARTESIAN_POINT('Ctrl Pts',(4.46497643499994,5.2,-1.61932962500002));
#348226=CARTESIAN_POINT('Ctrl Pts',(4.46497643499994,2.2,-1.61932962500002));
#348227=CARTESIAN_POINT('Ctrl Pts',(4.46433066499995,12.2,-1.61848192700001));
#348228=CARTESIAN_POINT('Ctrl Pts',(4.46433066499995,5.2,-1.61848192700001));
#348229=CARTESIAN_POINT('Ctrl Pts',(4.46433066499995,2.2,-1.61848192700001));
#348230=CARTESIAN_POINT('Ctrl Pts',(4.46336197099995,12.2,-1.61721168800002));
#348231=CARTESIAN_POINT('Ctrl Pts',(4.46336197099995,5.2,-1.61721168800002));
#348232=CARTESIAN_POINT('Ctrl Pts',(4.46336197099995,2.2,-1.61721168800002));
#348233=CARTESIAN_POINT('Ctrl Pts',(4.46207030599994,12.2,-1.61552065300001));
#348234=CARTESIAN_POINT('Ctrl Pts',(4.46207030599994,5.2,-1.61552065300001));
#348235=CARTESIAN_POINT('Ctrl Pts',(4.46207030599994,2.2,-1.61552065300001));
#348236=CARTESIAN_POINT('Ctrl Pts',(4.46045560299994,12.2,-1.61341121800001));
#348237=CARTESIAN_POINT('Ctrl Pts',(4.46045560299994,5.2,-1.61341121800001));
#348238=CARTESIAN_POINT('Ctrl Pts',(4.46045560299994,2.2,-1.61341121800001));
#348239=CARTESIAN_POINT('Ctrl Pts',(4.45884077799994,12.2,-1.61130614500001));
#348240=CARTESIAN_POINT('Ctrl Pts',(4.45884077799994,5.2,-1.61130614500001));
#348241=CARTESIAN_POINT('Ctrl Pts',(4.45884077799994,2.2,-1.61130614500001));
#348242=CARTESIAN_POINT('Ctrl Pts',(4.45722583399994,12.2,-1.60920543300001));
#348243=CARTESIAN_POINT('Ctrl Pts',(4.45722583399994,5.2,-1.60920543300001));
#348244=CARTESIAN_POINT('Ctrl Pts',(4.45722583399994,2.2,-1.60920543300001));
#348245=CARTESIAN_POINT('Ctrl Pts',(4.45561077699994,12.2,-1.60710908300001));
#348246=CARTESIAN_POINT('Ctrl Pts',(4.45561077699994,5.2,-1.60710908300001));
#348247=CARTESIAN_POINT('Ctrl Pts',(4.45561077699994,2.2,-1.60710908300001));
#348248=CARTESIAN_POINT('Ctrl Pts',(4.45399560999994,12.2,-1.60501709500001));
#348249=CARTESIAN_POINT('Ctrl Pts',(4.45399560999994,5.2,-1.60501709500001));
#348250=CARTESIAN_POINT('Ctrl Pts',(4.45399560999994,2.2,-1.60501709500001));
#348251=CARTESIAN_POINT('Ctrl Pts',(4.45238034299994,12.2,-1.60292947100002));
#348252=CARTESIAN_POINT('Ctrl Pts',(4.45238034299994,5.2,-1.60292947100002));
#348253=CARTESIAN_POINT('Ctrl Pts',(4.45238034299994,2.2,-1.60292947100002));
#348254=CARTESIAN_POINT('Ctrl Pts',(4.45076498499995,12.2,-1.60084621100001));
#348255=CARTESIAN_POINT('Ctrl Pts',(4.45076498499995,5.2,-1.60084621100001));
#348256=CARTESIAN_POINT('Ctrl Pts',(4.45076498499995,2.2,-1.60084621100001));
#348257=CARTESIAN_POINT('Ctrl Pts',(4.44914954699995,12.2,-1.59876731800002));
#348258=CARTESIAN_POINT('Ctrl Pts',(4.44914954699995,5.2,-1.59876731800002));
#348259=CARTESIAN_POINT('Ctrl Pts',(4.44914954699995,2.2,-1.59876731800002));
#348260=CARTESIAN_POINT('Ctrl Pts',(4.44753403899994,12.2,-1.59669279200001));
#348261=CARTESIAN_POINT('Ctrl Pts',(4.44753403899994,5.2,-1.59669279200001));
#348262=CARTESIAN_POINT('Ctrl Pts',(4.44753403899994,2.2,-1.59669279200001));
#348263=CARTESIAN_POINT('Ctrl Pts',(4.44591847199994,12.2,-1.59462263400002));
#348264=CARTESIAN_POINT('Ctrl Pts',(4.44591847199994,5.2,-1.59462263400002));
#348265=CARTESIAN_POINT('Ctrl Pts',(4.44591847199994,2.2,-1.59462263400002));
#348266=CARTESIAN_POINT('Ctrl Pts',(4.44430285599995,12.2,-1.59255684700002));
#348267=CARTESIAN_POINT('Ctrl Pts',(4.44430285599995,5.2,-1.59255684700002));
#348268=CARTESIAN_POINT('Ctrl Pts',(4.44430285599995,2.2,-1.59255684700002));
#348269=CARTESIAN_POINT('Ctrl Pts',(4.44268719799994,12.2,-1.59049542900001));
#348270=CARTESIAN_POINT('Ctrl Pts',(4.44268719799994,5.2,-1.59049542900001));
#348271=CARTESIAN_POINT('Ctrl Pts',(4.44268719799994,2.2,-1.59049542900001));
#348272=CARTESIAN_POINT('Ctrl Pts',(4.44107150699994,12.2,-1.58843838400001));
#348273=CARTESIAN_POINT('Ctrl Pts',(4.44107150699994,5.2,-1.58843838400001));
#348274=CARTESIAN_POINT('Ctrl Pts',(4.44107150699994,2.2,-1.58843838400001));
#348275=CARTESIAN_POINT('Ctrl Pts',(4.43945579199994,12.2,-1.58638571200001));
#348276=CARTESIAN_POINT('Ctrl Pts',(4.43945579199994,5.2,-1.58638571200001));
#348277=CARTESIAN_POINT('Ctrl Pts',(4.43945579199994,2.2,-1.58638571200001));
#348278=CARTESIAN_POINT('Ctrl Pts',(4.43784005899994,12.2,-1.58433741300001));
#348279=CARTESIAN_POINT('Ctrl Pts',(4.43784005899994,5.2,-1.58433741300001));
#348280=CARTESIAN_POINT('Ctrl Pts',(4.43784005899994,2.2,-1.58433741300001));
#348281=CARTESIAN_POINT('Ctrl Pts',(4.43622431699994,12.2,-1.58229348700001));
#348282=CARTESIAN_POINT('Ctrl Pts',(4.43622431699994,5.2,-1.58229348700001));
#348283=CARTESIAN_POINT('Ctrl Pts',(4.43622431699994,2.2,-1.58229348700001));
#348284=CARTESIAN_POINT('Ctrl Pts',(4.43460857399994,12.2,-1.58025393700001));
#348285=CARTESIAN_POINT('Ctrl Pts',(4.43460857399994,5.2,-1.58025393700001));
#348286=CARTESIAN_POINT('Ctrl Pts',(4.43460857399994,2.2,-1.58025393700001));
#348287=CARTESIAN_POINT('Ctrl Pts',(4.43299283799994,12.2,-1.57821876300002));
#348288=CARTESIAN_POINT('Ctrl Pts',(4.43299283799994,5.2,-1.57821876300002));
#348289=CARTESIAN_POINT('Ctrl Pts',(4.43299283799994,2.2,-1.57821876300002));
#348290=CARTESIAN_POINT('Ctrl Pts',(4.43137711899994,12.2,-1.57618796700001));
#348291=CARTESIAN_POINT('Ctrl Pts',(4.43137711899994,5.2,-1.57618796700001));
#348292=CARTESIAN_POINT('Ctrl Pts',(4.43137711899994,2.2,-1.57618796700001));
#348293=CARTESIAN_POINT('Ctrl Pts',(4.42976142499994,12.2,-1.57416154700002));
#348294=CARTESIAN_POINT('Ctrl Pts',(4.42976142499994,5.2,-1.57416154700002));
#348295=CARTESIAN_POINT('Ctrl Pts',(4.42976142499994,2.2,-1.57416154700002));
#348296=CARTESIAN_POINT('Ctrl Pts',(4.42814576699995,12.2,-1.57213950800001));
#348297=CARTESIAN_POINT('Ctrl Pts',(4.42814576699995,5.2,-1.57213950800001));
#348298=CARTESIAN_POINT('Ctrl Pts',(4.42814576699995,2.2,-1.57213950800001));
#348299=CARTESIAN_POINT('Ctrl Pts',(4.42653015199994,12.2,-1.57012184800001));
#348300=CARTESIAN_POINT('Ctrl Pts',(4.42653015199994,5.2,-1.57012184800001));
#348301=CARTESIAN_POINT('Ctrl Pts',(4.42653015199994,2.2,-1.57012184800001));
#348302=CARTESIAN_POINT('Ctrl Pts',(4.42491458999995,12.2,-1.56810856900002));
#348303=CARTESIAN_POINT('Ctrl Pts',(4.42491458999995,5.2,-1.56810856900002));
#348304=CARTESIAN_POINT('Ctrl Pts',(4.42491458999995,2.2,-1.56810856900002));
#348305=CARTESIAN_POINT('Ctrl Pts',(4.42329908899994,12.2,-1.56609967300001));
#348306=CARTESIAN_POINT('Ctrl Pts',(4.42329908899994,5.2,-1.56609967300001));
#348307=CARTESIAN_POINT('Ctrl Pts',(4.42329908899994,2.2,-1.56609967300001));
#348308=CARTESIAN_POINT('Ctrl Pts',(4.42168365699994,12.2,-1.56409515800001));
#348309=CARTESIAN_POINT('Ctrl Pts',(4.42168365699994,5.2,-1.56409515800001));
#348310=CARTESIAN_POINT('Ctrl Pts',(4.42168365699994,2.2,-1.56409515800001));
#348311=CARTESIAN_POINT('Ctrl Pts',(4.42006830399994,12.2,-1.56209502700001));
#348312=CARTESIAN_POINT('Ctrl Pts',(4.42006830399994,5.2,-1.56209502700001));
#348313=CARTESIAN_POINT('Ctrl Pts',(4.42006830399994,2.2,-1.56209502700001));
#348314=CARTESIAN_POINT('Ctrl Pts',(4.41845303799994,12.2,-1.56009928000001));
#348315=CARTESIAN_POINT('Ctrl Pts',(4.41845303799994,5.2,-1.56009928000001));
#348316=CARTESIAN_POINT('Ctrl Pts',(4.41845303799994,2.2,-1.56009928000001));
#348317=CARTESIAN_POINT('Ctrl Pts',(4.41683786899994,12.2,-1.55810791900001));
#348318=CARTESIAN_POINT('Ctrl Pts',(4.41683786899994,5.2,-1.55810791900001));
#348319=CARTESIAN_POINT('Ctrl Pts',(4.41683786899994,2.2,-1.55810791900001));
#348320=CARTESIAN_POINT('Ctrl Pts',(4.41522280299994,12.2,-1.55612094300002));
#348321=CARTESIAN_POINT('Ctrl Pts',(4.41522280299994,5.2,-1.55612094300002));
#348322=CARTESIAN_POINT('Ctrl Pts',(4.41522280299994,2.2,-1.55612094300002));
#348323=CARTESIAN_POINT('Ctrl Pts',(4.41360785099994,12.2,-1.55413835300001));
#348324=CARTESIAN_POINT('Ctrl Pts',(4.41360785099994,5.2,-1.55413835300001));
#348325=CARTESIAN_POINT('Ctrl Pts',(4.41360785099994,2.2,-1.55413835300001));
#348326=CARTESIAN_POINT('Ctrl Pts',(4.41199301999994,12.2,-1.55216015100001));
#348327=CARTESIAN_POINT('Ctrl Pts',(4.41199301999994,5.2,-1.55216015100001));
#348328=CARTESIAN_POINT('Ctrl Pts',(4.41199301999994,2.2,-1.55216015100001));
#348329=CARTESIAN_POINT('Ctrl Pts',(4.41037832099994,12.2,-1.55018633800001));
#348330=CARTESIAN_POINT('Ctrl Pts',(4.41037832099994,5.2,-1.55018633800001));
#348331=CARTESIAN_POINT('Ctrl Pts',(4.41037832099994,2.2,-1.55018633800001));
#348332=CARTESIAN_POINT('Ctrl Pts',(4.40876376299994,12.2,-1.54821691400001));
#348333=CARTESIAN_POINT('Ctrl Pts',(4.40876376299994,5.2,-1.54821691400001));
#348334=CARTESIAN_POINT('Ctrl Pts',(4.40876376299994,2.2,-1.54821691400001));
#348335=CARTESIAN_POINT('Ctrl Pts',(4.40714935399994,12.2,-1.54625187900002));
#348336=CARTESIAN_POINT('Ctrl Pts',(4.40714935399994,5.2,-1.54625187900002));
#348337=CARTESIAN_POINT('Ctrl Pts',(4.40714935399994,2.2,-1.54625187900002));
#348338=CARTESIAN_POINT('Ctrl Pts',(4.40553510099994,12.2,-1.54429123500002));
#348339=CARTESIAN_POINT('Ctrl Pts',(4.40553510099994,5.2,-1.54429123500002));
#348340=CARTESIAN_POINT('Ctrl Pts',(4.40553510099994,2.2,-1.54429123500002));
#348341=CARTESIAN_POINT('Ctrl Pts',(4.40392101499994,12.2,-1.54233498200002));
#348342=CARTESIAN_POINT('Ctrl Pts',(4.40392101499994,5.2,-1.54233498200002));
#348343=CARTESIAN_POINT('Ctrl Pts',(4.40392101499994,2.2,-1.54233498200002));
#348344=CARTESIAN_POINT('Ctrl Pts',(4.40230710599994,12.2,-1.54038312200001));
#348345=CARTESIAN_POINT('Ctrl Pts',(4.40230710599994,5.2,-1.54038312200001));
#348346=CARTESIAN_POINT('Ctrl Pts',(4.40230710599994,2.2,-1.54038312200001));
#348347=CARTESIAN_POINT('Ctrl Pts',(4.40069337999994,12.2,-1.53843565400001));
#348348=CARTESIAN_POINT('Ctrl Pts',(4.40069337999994,5.2,-1.53843565400001));
#348349=CARTESIAN_POINT('Ctrl Pts',(4.40069337999994,2.2,-1.53843565400001));
#348350=CARTESIAN_POINT('Ctrl Pts',(4.39907984799994,12.2,-1.53649258000002));
#348351=CARTESIAN_POINT('Ctrl Pts',(4.39907984799994,5.2,-1.53649258000002));
#348352=CARTESIAN_POINT('Ctrl Pts',(4.39907984799994,2.2,-1.53649258000002));
#348353=CARTESIAN_POINT('Ctrl Pts',(4.39746651799994,12.2,-1.53455390100001));
#348354=CARTESIAN_POINT('Ctrl Pts',(4.39746651799994,5.2,-1.53455390100001));
#348355=CARTESIAN_POINT('Ctrl Pts',(4.39746651799994,2.2,-1.53455390100001));
#348356=CARTESIAN_POINT('Ctrl Pts',(4.39585339899994,12.2,-1.53261961500001));
#348357=CARTESIAN_POINT('Ctrl Pts',(4.39585339899994,5.2,-1.53261961500001));
#348358=CARTESIAN_POINT('Ctrl Pts',(4.39585339899994,2.2,-1.53261961500001));
#348359=CARTESIAN_POINT('Ctrl Pts',(4.39424049999994,12.2,-1.53068972600002));
#348360=CARTESIAN_POINT('Ctrl Pts',(4.39424049999994,5.2,-1.53068972600002));
#348361=CARTESIAN_POINT('Ctrl Pts',(4.39424049999994,2.2,-1.53068972600002));
#348362=CARTESIAN_POINT('Ctrl Pts',(4.39262782999994,12.2,-1.52876423300001));
#348363=CARTESIAN_POINT('Ctrl Pts',(4.39262782999994,5.2,-1.52876423300001));
#348364=CARTESIAN_POINT('Ctrl Pts',(4.39262782999994,2.2,-1.52876423300001));
#348365=CARTESIAN_POINT('Ctrl Pts',(4.39101539899994,12.2,-1.52684313600002));
#348366=CARTESIAN_POINT('Ctrl Pts',(4.39101539899994,5.2,-1.52684313600002));
#348367=CARTESIAN_POINT('Ctrl Pts',(4.39101539899994,2.2,-1.52684313600002));
#348368=CARTESIAN_POINT('Ctrl Pts',(4.38940321399994,12.2,-1.52492643700001));
#348369=CARTESIAN_POINT('Ctrl Pts',(4.38940321399994,5.2,-1.52492643700001));
#348370=CARTESIAN_POINT('Ctrl Pts',(4.38940321399994,2.2,-1.52492643700001));
#348371=CARTESIAN_POINT('Ctrl Pts',(4.38779128499994,12.2,-1.52301413600001));
#348372=CARTESIAN_POINT('Ctrl Pts',(4.38779128499994,5.2,-1.52301413600001));
#348373=CARTESIAN_POINT('Ctrl Pts',(4.38779128499994,2.2,-1.52301413600001));
#348374=CARTESIAN_POINT('Ctrl Pts',(4.38617962199995,12.2,-1.52110623500001));
#348375=CARTESIAN_POINT('Ctrl Pts',(4.38617962199995,5.2,-1.52110623500001));
#348376=CARTESIAN_POINT('Ctrl Pts',(4.38617962199995,2.2,-1.52110623500001));
#348377=CARTESIAN_POINT('Ctrl Pts',(4.38456823199994,12.2,-1.51920273300002));
#348378=CARTESIAN_POINT('Ctrl Pts',(4.38456823199994,5.2,-1.51920273300002));
#348379=CARTESIAN_POINT('Ctrl Pts',(4.38456823199994,2.2,-1.51920273300002));
#348380=CARTESIAN_POINT('Ctrl Pts',(4.38295712499994,12.2,-1.51730363000001));
#348381=CARTESIAN_POINT('Ctrl Pts',(4.38295712499994,5.2,-1.51730363000001));
#348382=CARTESIAN_POINT('Ctrl Pts',(4.38295712499994,2.2,-1.51730363000001));
#348383=CARTESIAN_POINT('Ctrl Pts',(4.38134631099994,12.2,-1.51540892800002));
#348384=CARTESIAN_POINT('Ctrl Pts',(4.38134631099994,5.2,-1.51540892800002));
#348385=CARTESIAN_POINT('Ctrl Pts',(4.38134631099994,2.2,-1.51540892800002));
#348386=CARTESIAN_POINT('Ctrl Pts',(4.37973579799994,12.2,-1.51351862700002));
#348387=CARTESIAN_POINT('Ctrl Pts',(4.37973579799994,5.2,-1.51351862700002));
#348388=CARTESIAN_POINT('Ctrl Pts',(4.37973579799994,2.2,-1.51351862700002));
#348389=CARTESIAN_POINT('Ctrl Pts',(4.37812559599995,12.2,-1.51163272800002));
#348390=CARTESIAN_POINT('Ctrl Pts',(4.37812559599995,5.2,-1.51163272800002));
#348391=CARTESIAN_POINT('Ctrl Pts',(4.37812559599995,2.2,-1.51163272800002));
#348392=CARTESIAN_POINT('Ctrl Pts',(4.37651571199994,12.2,-1.50975123100002));
#348393=CARTESIAN_POINT('Ctrl Pts',(4.37651571199994,5.2,-1.50975123100002));
#348394=CARTESIAN_POINT('Ctrl Pts',(4.37651571199994,2.2,-1.50975123100002));
#348395=CARTESIAN_POINT('Ctrl Pts',(4.37490615699994,12.2,-1.50787413700002));
#348396=CARTESIAN_POINT('Ctrl Pts',(4.37490615699994,5.2,-1.50787413700002));
#348397=CARTESIAN_POINT('Ctrl Pts',(4.37490615699994,2.2,-1.50787413700002));
#348398=CARTESIAN_POINT('Ctrl Pts',(4.37329693899995,12.2,-1.50600144600002));
#348399=CARTESIAN_POINT('Ctrl Pts',(4.37329693899995,5.2,-1.50600144600002));
#348400=CARTESIAN_POINT('Ctrl Pts',(4.37329693899995,2.2,-1.50600144600002));
#348401=CARTESIAN_POINT('Ctrl Pts',(4.37168806799995,12.2,-1.50413316000002));
#348402=CARTESIAN_POINT('Ctrl Pts',(4.37168806799995,5.2,-1.50413316000002));
#348403=CARTESIAN_POINT('Ctrl Pts',(4.37168806799995,2.2,-1.50413316000002));
#348404=CARTESIAN_POINT('Ctrl Pts',(4.37007955299994,12.2,-1.50226927600002));
#348405=CARTESIAN_POINT('Ctrl Pts',(4.37007955299994,5.2,-1.50226927600002));
#348406=CARTESIAN_POINT('Ctrl Pts',(4.37007955299994,2.2,-1.50226927600002));
#348407=CARTESIAN_POINT('Ctrl Pts',(4.36847140299994,12.2,-1.50040979900002));
#348408=CARTESIAN_POINT('Ctrl Pts',(4.36847140299994,5.2,-1.50040979900002));
#348409=CARTESIAN_POINT('Ctrl Pts',(4.36847140299994,2.2,-1.50040979900002));
#348410=CARTESIAN_POINT('Ctrl Pts',(4.36686362699994,12.2,-1.49855472700001));
#348411=CARTESIAN_POINT('Ctrl Pts',(4.36686362699994,5.2,-1.49855472700001));
#348412=CARTESIAN_POINT('Ctrl Pts',(4.36686362699994,2.2,-1.49855472700001));
#348413=CARTESIAN_POINT('Ctrl Pts',(4.36525623399994,12.2,-1.49670406000002));
#348414=CARTESIAN_POINT('Ctrl Pts',(4.36525623399994,5.2,-1.49670406000002));
#348415=CARTESIAN_POINT('Ctrl Pts',(4.36525623399994,2.2,-1.49670406000002));
#348416=CARTESIAN_POINT('Ctrl Pts',(4.36364923399994,12.2,-1.49485779900001));
#348417=CARTESIAN_POINT('Ctrl Pts',(4.36364923399994,5.2,-1.49485779900001));
#348418=CARTESIAN_POINT('Ctrl Pts',(4.36364923399994,2.2,-1.49485779900001));
#348419=CARTESIAN_POINT('Ctrl Pts',(4.36204263499994,12.2,-1.49301594600002));
#348420=CARTESIAN_POINT('Ctrl Pts',(4.36204263499994,5.2,-1.49301594600002));
#348421=CARTESIAN_POINT('Ctrl Pts',(4.36204263499994,2.2,-1.49301594600002));
#348422=CARTESIAN_POINT('Ctrl Pts',(4.36043644699994,12.2,-1.49117849900001));
#348423=CARTESIAN_POINT('Ctrl Pts',(4.36043644699994,5.2,-1.49117849900001));
#348424=CARTESIAN_POINT('Ctrl Pts',(4.36043644699994,2.2,-1.49117849900001));
#348425=CARTESIAN_POINT('Ctrl Pts',(4.35883067899994,12.2,-1.48934546000001));
#348426=CARTESIAN_POINT('Ctrl Pts',(4.35883067899994,5.2,-1.48934546000001));
#348427=CARTESIAN_POINT('Ctrl Pts',(4.35883067899994,2.2,-1.48934546000001));
#348428=CARTESIAN_POINT('Ctrl Pts',(4.35722534099994,12.2,-1.48751682800001));
#348429=CARTESIAN_POINT('Ctrl Pts',(4.35722534099994,5.2,-1.48751682800001));
#348430=CARTESIAN_POINT('Ctrl Pts',(4.35722534099994,2.2,-1.48751682800001));
#348431=CARTESIAN_POINT('Ctrl Pts',(4.35562043999994,12.2,-1.48569260600001));
#348432=CARTESIAN_POINT('Ctrl Pts',(4.35562043999994,5.2,-1.48569260600001));
#348433=CARTESIAN_POINT('Ctrl Pts',(4.35562043999994,2.2,-1.48569260600001));
#348434=CARTESIAN_POINT('Ctrl Pts',(4.35401598799994,12.2,-1.48387279100001));
#348435=CARTESIAN_POINT('Ctrl Pts',(4.35401598799994,5.2,-1.48387279100001));
#348436=CARTESIAN_POINT('Ctrl Pts',(4.35401598799994,2.2,-1.48387279100001));
#348437=CARTESIAN_POINT('Ctrl Pts',(4.35241199299994,12.2,-1.48205738700002));
#348438=CARTESIAN_POINT('Ctrl Pts',(4.35241199299994,5.2,-1.48205738700002));
#348439=CARTESIAN_POINT('Ctrl Pts',(4.35241199299994,2.2,-1.48205738700002));
#348440=CARTESIAN_POINT('Ctrl Pts',(4.35080846399994,12.2,-1.48024639000001));
#348441=CARTESIAN_POINT('Ctrl Pts',(4.35080846399994,5.2,-1.48024639000001));
#348442=CARTESIAN_POINT('Ctrl Pts',(4.35080846399994,2.2,-1.48024639000001));
#348443=CARTESIAN_POINT('Ctrl Pts',(4.34920541099994,12.2,-1.47843980500001));
#348444=CARTESIAN_POINT('Ctrl Pts',(4.34920541099994,5.2,-1.47843980500001));
#348445=CARTESIAN_POINT('Ctrl Pts',(4.34920541099994,2.2,-1.47843980500001));
#348446=CARTESIAN_POINT('Ctrl Pts',(4.34760284299994,12.2,-1.47663762900001));
#348447=CARTESIAN_POINT('Ctrl Pts',(4.34760284299994,5.2,-1.47663762900001));
#348448=CARTESIAN_POINT('Ctrl Pts',(4.34760284299994,2.2,-1.47663762900001));
#348449=CARTESIAN_POINT('Ctrl Pts',(4.34600076899994,12.2,-1.47483986400001));
#348450=CARTESIAN_POINT('Ctrl Pts',(4.34600076899994,5.2,-1.47483986400001));
#348451=CARTESIAN_POINT('Ctrl Pts',(4.34600076899994,2.2,-1.47483986400001));
#348452=CARTESIAN_POINT('Ctrl Pts',(4.34439919799994,12.2,-1.47304650900002));
#348453=CARTESIAN_POINT('Ctrl Pts',(4.34439919799994,5.2,-1.47304650900002));
#348454=CARTESIAN_POINT('Ctrl Pts',(4.34439919799994,2.2,-1.47304650900002));
#348455=CARTESIAN_POINT('Ctrl Pts',(4.34279813999995,12.2,-1.47125756500001));
#348456=CARTESIAN_POINT('Ctrl Pts',(4.34279813999995,5.2,-1.47125756500001));
#348457=CARTESIAN_POINT('Ctrl Pts',(4.34279813999995,2.2,-1.47125756500001));
#348458=CARTESIAN_POINT('Ctrl Pts',(4.34119760499994,12.2,-1.46947303300001));
#348459=CARTESIAN_POINT('Ctrl Pts',(4.34119760499994,5.2,-1.46947303300001));
#348460=CARTESIAN_POINT('Ctrl Pts',(4.34119760499994,2.2,-1.46947303300001));
#348461=CARTESIAN_POINT('Ctrl Pts',(4.33959760099994,12.2,-1.46769291200001));
#348462=CARTESIAN_POINT('Ctrl Pts',(4.33959760099994,5.2,-1.46769291200001));
#348463=CARTESIAN_POINT('Ctrl Pts',(4.33959760099994,2.2,-1.46769291200001));
#348464=CARTESIAN_POINT('Ctrl Pts',(4.33799813899994,12.2,-1.46591720300002));
#348465=CARTESIAN_POINT('Ctrl Pts',(4.33799813899994,5.2,-1.46591720300002));
#348466=CARTESIAN_POINT('Ctrl Pts',(4.33799813899994,2.2,-1.46591720300002));
#348467=CARTESIAN_POINT('Ctrl Pts',(4.33639922599994,12.2,-1.46414590600001));
#348468=CARTESIAN_POINT('Ctrl Pts',(4.33639922599994,5.2,-1.46414590600001));
#348469=CARTESIAN_POINT('Ctrl Pts',(4.33639922599994,2.2,-1.46414590600001));
#348470=CARTESIAN_POINT('Ctrl Pts',(4.33480087399994,12.2,-1.46237902200001));
#348471=CARTESIAN_POINT('Ctrl Pts',(4.33480087399994,5.2,-1.46237902200001));
#348472=CARTESIAN_POINT('Ctrl Pts',(4.33480087399994,2.2,-1.46237902200001));
#348473=CARTESIAN_POINT('Ctrl Pts',(4.33320308999994,12.2,-1.46061655000001));
#348474=CARTESIAN_POINT('Ctrl Pts',(4.33320308999994,5.2,-1.46061655000001));
#348475=CARTESIAN_POINT('Ctrl Pts',(4.33320308999994,2.2,-1.46061655000001));
#348476=CARTESIAN_POINT('Ctrl Pts',(4.33160588499994,12.2,-1.45885849100001));
#348477=CARTESIAN_POINT('Ctrl Pts',(4.33160588499994,5.2,-1.45885849100001));
#348478=CARTESIAN_POINT('Ctrl Pts',(4.33160588499994,2.2,-1.45885849100001));
#348479=CARTESIAN_POINT('Ctrl Pts',(4.33000926899994,12.2,-1.45710484400002));
#348480=CARTESIAN_POINT('Ctrl Pts',(4.33000926899994,5.2,-1.45710484400002));
#348481=CARTESIAN_POINT('Ctrl Pts',(4.33000926899994,2.2,-1.45710484400002));
#348482=CARTESIAN_POINT('Ctrl Pts',(4.32841324999994,12.2,-1.45535561100001));
#348483=CARTESIAN_POINT('Ctrl Pts',(4.32841324999994,5.2,-1.45535561100001));
#348484=CARTESIAN_POINT('Ctrl Pts',(4.32841324999994,2.2,-1.45535561100001));
#348485=CARTESIAN_POINT('Ctrl Pts',(4.32681783699994,12.2,-1.45361079200002));
#348486=CARTESIAN_POINT('Ctrl Pts',(4.32681783699994,5.2,-1.45361079200002));
#348487=CARTESIAN_POINT('Ctrl Pts',(4.32681783699994,2.2,-1.45361079200002));
#348488=CARTESIAN_POINT('Ctrl Pts',(4.32522304199995,12.2,-1.45187038500001));
#348489=CARTESIAN_POINT('Ctrl Pts',(4.32522304199995,5.2,-1.45187038500001));
#348490=CARTESIAN_POINT('Ctrl Pts',(4.32522304199995,2.2,-1.45187038500001));
#348491=CARTESIAN_POINT('Ctrl Pts',(4.32362887299994,12.2,-1.45013439300001));
#348492=CARTESIAN_POINT('Ctrl Pts',(4.32362887299994,5.2,-1.45013439300001));
#348493=CARTESIAN_POINT('Ctrl Pts',(4.32362887299994,2.2,-1.45013439300001));
#348494=CARTESIAN_POINT('Ctrl Pts',(4.32203533899994,12.2,-1.44840281300001));
#348495=CARTESIAN_POINT('Ctrl Pts',(4.32203533899994,5.2,-1.44840281300001));
#348496=CARTESIAN_POINT('Ctrl Pts',(4.32203533899994,2.2,-1.44840281300001));
#348497=CARTESIAN_POINT('Ctrl Pts',(4.32044244999994,12.2,-1.44667564900002));
#348498=CARTESIAN_POINT('Ctrl Pts',(4.32044244999994,5.2,-1.44667564900002));
#348499=CARTESIAN_POINT('Ctrl Pts',(4.32044244999994,2.2,-1.44667564900002));
#348500=CARTESIAN_POINT('Ctrl Pts',(4.31885021599994,12.2,-1.44495289700002));
#348501=CARTESIAN_POINT('Ctrl Pts',(4.31885021599994,5.2,-1.44495289700002));
#348502=CARTESIAN_POINT('Ctrl Pts',(4.31885021599994,2.2,-1.44495289700002));
#348503=CARTESIAN_POINT('Ctrl Pts',(4.31725864499994,12.2,-1.44323456000001));
#348504=CARTESIAN_POINT('Ctrl Pts',(4.31725864499994,5.2,-1.44323456000001));
#348505=CARTESIAN_POINT('Ctrl Pts',(4.31725864499994,2.2,-1.44323456000001));
#348506=CARTESIAN_POINT('Ctrl Pts',(4.31566774799994,12.2,-1.44152063700002));
#348507=CARTESIAN_POINT('Ctrl Pts',(4.31566774799994,5.2,-1.44152063700002));
#348508=CARTESIAN_POINT('Ctrl Pts',(4.31566774799994,2.2,-1.44152063700002));
#348509=CARTESIAN_POINT('Ctrl Pts',(4.31407753499994,12.2,-1.43981112800001));
#348510=CARTESIAN_POINT('Ctrl Pts',(4.31407753499994,5.2,-1.43981112800001));
#348511=CARTESIAN_POINT('Ctrl Pts',(4.31407753499994,2.2,-1.43981112800001));
#348512=CARTESIAN_POINT('Ctrl Pts',(4.31248801499994,12.2,-1.43810603400001));
#348513=CARTESIAN_POINT('Ctrl Pts',(4.31248801499994,5.2,-1.43810603400001));
#348514=CARTESIAN_POINT('Ctrl Pts',(4.31248801499994,2.2,-1.43810603400001));
#348515=CARTESIAN_POINT('Ctrl Pts',(4.31089919699994,12.2,-1.43640535400001));
#348516=CARTESIAN_POINT('Ctrl Pts',(4.31089919699994,5.2,-1.43640535400001));
#348517=CARTESIAN_POINT('Ctrl Pts',(4.31089919699994,2.2,-1.43640535400001));
#348518=CARTESIAN_POINT('Ctrl Pts',(4.30931109099994,12.2,-1.43470908800001));
#348519=CARTESIAN_POINT('Ctrl Pts',(4.30931109099994,5.2,-1.43470908800001));
#348520=CARTESIAN_POINT('Ctrl Pts',(4.30931109099994,2.2,-1.43470908800001));
#348521=CARTESIAN_POINT('Ctrl Pts',(4.30772370599994,12.2,-1.43301723600001));
#348522=CARTESIAN_POINT('Ctrl Pts',(4.30772370599994,5.2,-1.43301723600001));
#348523=CARTESIAN_POINT('Ctrl Pts',(4.30772370599994,2.2,-1.43301723600001));
#348524=CARTESIAN_POINT('Ctrl Pts',(4.30613705299994,12.2,-1.43132979900002));
#348525=CARTESIAN_POINT('Ctrl Pts',(4.30613705299994,5.2,-1.43132979900002));
#348526=CARTESIAN_POINT('Ctrl Pts',(4.30613705299994,2.2,-1.43132979900002));
#348527=CARTESIAN_POINT('Ctrl Pts',(4.30455114099995,12.2,-1.42964677700002));
#348528=CARTESIAN_POINT('Ctrl Pts',(4.30455114099995,5.2,-1.42964677700002));
#348529=CARTESIAN_POINT('Ctrl Pts',(4.30455114099995,2.2,-1.42964677700002));
#348530=CARTESIAN_POINT('Ctrl Pts',(4.30296597899994,12.2,-1.42796816700002));
#348531=CARTESIAN_POINT('Ctrl Pts',(4.30296597899994,5.2,-1.42796816700002));
#348532=CARTESIAN_POINT('Ctrl Pts',(4.30296597899994,2.2,-1.42796816700002));
#348533=CARTESIAN_POINT('Ctrl Pts',(4.30138157799994,12.2,-1.42629397300002));
#348534=CARTESIAN_POINT('Ctrl Pts',(4.30138157799994,5.2,-1.42629397300002));
#348535=CARTESIAN_POINT('Ctrl Pts',(4.30138157799994,2.2,-1.42629397300002));
#348536=CARTESIAN_POINT('Ctrl Pts',(4.29979794699994,12.2,-1.42462419400001));
#348537=CARTESIAN_POINT('Ctrl Pts',(4.29979794699994,5.2,-1.42462419400001));
#348538=CARTESIAN_POINT('Ctrl Pts',(4.29979794699994,2.2,-1.42462419400001));
#348539=CARTESIAN_POINT('Ctrl Pts',(4.29821509599994,12.2,-1.42295882700001));
#348540=CARTESIAN_POINT('Ctrl Pts',(4.29821509599994,5.2,-1.42295882700001));
#348541=CARTESIAN_POINT('Ctrl Pts',(4.29821509599994,2.2,-1.42295882700001));
#348542=CARTESIAN_POINT('Ctrl Pts',(4.29663303399995,12.2,-1.42129787500001));
#348543=CARTESIAN_POINT('Ctrl Pts',(4.29663303399995,5.2,-1.42129787500001));
#348544=CARTESIAN_POINT('Ctrl Pts',(4.29663303399995,2.2,-1.42129787500001));
#348545=CARTESIAN_POINT('Ctrl Pts',(4.29505177099994,12.2,-1.41964133800002));
#348546=CARTESIAN_POINT('Ctrl Pts',(4.29505177099994,5.2,-1.41964133800002));
#348547=CARTESIAN_POINT('Ctrl Pts',(4.29505177099994,2.2,-1.41964133800002));
#348548=CARTESIAN_POINT('Ctrl Pts',(4.29347131599994,12.2,-1.41798921400001));
#348549=CARTESIAN_POINT('Ctrl Pts',(4.29347131599994,5.2,-1.41798921400001));
#348550=CARTESIAN_POINT('Ctrl Pts',(4.29347131599994,2.2,-1.41798921400001));
#348551=CARTESIAN_POINT('Ctrl Pts',(4.29189168099995,12.2,-1.41634150400002));
#348552=CARTESIAN_POINT('Ctrl Pts',(4.29189168099995,5.2,-1.41634150400002));
#348553=CARTESIAN_POINT('Ctrl Pts',(4.29189168099995,2.2,-1.41634150400002));
#348554=CARTESIAN_POINT('Ctrl Pts',(4.29031287399994,12.2,-1.41469820800001));
#348555=CARTESIAN_POINT('Ctrl Pts',(4.29031287399994,5.2,-1.41469820800001));
#348556=CARTESIAN_POINT('Ctrl Pts',(4.29031287399994,2.2,-1.41469820800001));
#348557=CARTESIAN_POINT('Ctrl Pts',(4.28873490499995,12.2,-1.41305932400002));
#348558=CARTESIAN_POINT('Ctrl Pts',(4.28873490499995,5.2,-1.41305932400002));
#348559=CARTESIAN_POINT('Ctrl Pts',(4.28873490499995,2.2,-1.41305932400002));
#348560=CARTESIAN_POINT('Ctrl Pts',(4.28715778399994,12.2,-1.41142485500001));
#348561=CARTESIAN_POINT('Ctrl Pts',(4.28715778399994,5.2,-1.41142485500001));
#348562=CARTESIAN_POINT('Ctrl Pts',(4.28715778399994,2.2,-1.41142485500001));
#348563=CARTESIAN_POINT('Ctrl Pts',(4.28558152199995,12.2,-1.40979479800002));
#348564=CARTESIAN_POINT('Ctrl Pts',(4.28558152199995,5.2,-1.40979479800002));
#348565=CARTESIAN_POINT('Ctrl Pts',(4.28558152199995,2.2,-1.40979479800002));
#348566=CARTESIAN_POINT('Ctrl Pts',(4.28400612599994,12.2,-1.40816915500002));
#348567=CARTESIAN_POINT('Ctrl Pts',(4.28400612599994,5.2,-1.40816915500002));
#348568=CARTESIAN_POINT('Ctrl Pts',(4.28400612599994,2.2,-1.40816915500002));
#348569=CARTESIAN_POINT('Ctrl Pts',(4.28243160799994,12.2,-1.40654792400001));
#348570=CARTESIAN_POINT('Ctrl Pts',(4.28243160799994,5.2,-1.40654792400001));
#348571=CARTESIAN_POINT('Ctrl Pts',(4.28243160799994,2.2,-1.40654792400001));
#348572=CARTESIAN_POINT('Ctrl Pts',(4.28085797699994,12.2,-1.40493110600001));
#348573=CARTESIAN_POINT('Ctrl Pts',(4.28085797699994,5.2,-1.40493110600001));
#348574=CARTESIAN_POINT('Ctrl Pts',(4.28085797699994,2.2,-1.40493110600001));
#348575=CARTESIAN_POINT('Ctrl Pts',(4.27928524499994,12.2,-1.40331870000002));
#348576=CARTESIAN_POINT('Ctrl Pts',(4.27928524499994,5.2,-1.40331870000002));
#348577=CARTESIAN_POINT('Ctrl Pts',(4.27928524499994,2.2,-1.40331870000002));
#348578=CARTESIAN_POINT('Ctrl Pts',(4.27771341799995,12.2,-1.40171070500001));
#348579=CARTESIAN_POINT('Ctrl Pts',(4.27771341799995,5.2,-1.40171070500001));
#348580=CARTESIAN_POINT('Ctrl Pts',(4.27771341799995,2.2,-1.40171070500001));
#348581=CARTESIAN_POINT('Ctrl Pts',(4.27614250899994,12.2,-1.40010712400001));
#348582=CARTESIAN_POINT('Ctrl Pts',(4.27614250899994,5.2,-1.40010712400001));
#348583=CARTESIAN_POINT('Ctrl Pts',(4.27614250899994,2.2,-1.40010712400001));
#348584=CARTESIAN_POINT('Ctrl Pts',(4.27457252599994,12.2,-1.39850795300001));
#348585=CARTESIAN_POINT('Ctrl Pts',(4.27457252599994,5.2,-1.39850795300001));
#348586=CARTESIAN_POINT('Ctrl Pts',(4.27457252599994,2.2,-1.39850795300001));
#348587=CARTESIAN_POINT('Ctrl Pts',(4.27300347999994,12.2,-1.39691319500002));
#348588=CARTESIAN_POINT('Ctrl Pts',(4.27300347999994,5.2,-1.39691319500002));
#348589=CARTESIAN_POINT('Ctrl Pts',(4.27300347999994,2.2,-1.39691319500002));
#348590=CARTESIAN_POINT('Ctrl Pts',(4.27143538199994,12.2,-1.39532284600001));
#348591=CARTESIAN_POINT('Ctrl Pts',(4.27143538199994,5.2,-1.39532284600001));
#348592=CARTESIAN_POINT('Ctrl Pts',(4.27143538199994,2.2,-1.39532284600001));
#348593=CARTESIAN_POINT('Ctrl Pts',(4.26986823899994,12.2,-1.39373690900001));
#348594=CARTESIAN_POINT('Ctrl Pts',(4.26986823899994,5.2,-1.39373690900001));
#348595=CARTESIAN_POINT('Ctrl Pts',(4.26986823899994,2.2,-1.39373690900001));
#348596=CARTESIAN_POINT('Ctrl Pts',(4.26830206399995,12.2,-1.39215538100002));
#348597=CARTESIAN_POINT('Ctrl Pts',(4.26830206399995,5.2,-1.39215538100002));
#348598=CARTESIAN_POINT('Ctrl Pts',(4.26830206399995,2.2,-1.39215538100002));
#348599=CARTESIAN_POINT('Ctrl Pts',(4.26673686399995,12.2,-1.39057826400002));
#348600=CARTESIAN_POINT('Ctrl Pts',(4.26673686399995,5.2,-1.39057826400002));
#348601=CARTESIAN_POINT('Ctrl Pts',(4.26673686399995,2.2,-1.39057826400002));
#348602=CARTESIAN_POINT('Ctrl Pts',(4.26517265199994,12.2,-1.38900555700001));
#348603=CARTESIAN_POINT('Ctrl Pts',(4.26517265199994,5.2,-1.38900555700001));
#348604=CARTESIAN_POINT('Ctrl Pts',(4.26517265199994,2.2,-1.38900555700001));
#348605=CARTESIAN_POINT('Ctrl Pts',(4.26360943599995,12.2,-1.38743725800001));
#348606=CARTESIAN_POINT('Ctrl Pts',(4.26360943599995,5.2,-1.38743725800001));
#348607=CARTESIAN_POINT('Ctrl Pts',(4.26360943599995,2.2,-1.38743725800001));
#348608=CARTESIAN_POINT('Ctrl Pts',(4.26204722699994,12.2,-1.38587336900001));
#348609=CARTESIAN_POINT('Ctrl Pts',(4.26204722699994,5.2,-1.38587336900001));
#348610=CARTESIAN_POINT('Ctrl Pts',(4.26204722699994,2.2,-1.38587336900001));
#348611=CARTESIAN_POINT('Ctrl Pts',(4.26048603399994,12.2,-1.38431388800001));
#348612=CARTESIAN_POINT('Ctrl Pts',(4.26048603399994,5.2,-1.38431388800001));
#348613=CARTESIAN_POINT('Ctrl Pts',(4.26048603399994,2.2,-1.38431388800001));
#348614=CARTESIAN_POINT('Ctrl Pts',(4.25892586799994,12.2,-1.38275881500002));
#348615=CARTESIAN_POINT('Ctrl Pts',(4.25892586799994,5.2,-1.38275881500002));
#348616=CARTESIAN_POINT('Ctrl Pts',(4.25892586799994,2.2,-1.38275881500002));
#348617=CARTESIAN_POINT('Ctrl Pts',(4.25736673899994,12.2,-1.38120815000002));
#348618=CARTESIAN_POINT('Ctrl Pts',(4.25736673899994,5.2,-1.38120815000002));
#348619=CARTESIAN_POINT('Ctrl Pts',(4.25736673899994,2.2,-1.38120815000002));
#348620=CARTESIAN_POINT('Ctrl Pts',(4.25580865599995,12.2,-1.37966189200001));
#348621=CARTESIAN_POINT('Ctrl Pts',(4.25580865599995,5.2,-1.37966189200001));
#348622=CARTESIAN_POINT('Ctrl Pts',(4.25580865599995,2.2,-1.37966189200001));
#348623=CARTESIAN_POINT('Ctrl Pts',(4.25425163099994,12.2,-1.37812004100001));
#348624=CARTESIAN_POINT('Ctrl Pts',(4.25425163099994,5.2,-1.37812004100001));
#348625=CARTESIAN_POINT('Ctrl Pts',(4.25425163099994,2.2,-1.37812004100001));
#348626=CARTESIAN_POINT('Ctrl Pts',(4.25269567199994,12.2,-1.37658259600002));
#348627=CARTESIAN_POINT('Ctrl Pts',(4.25269567199994,5.2,-1.37658259600002));
#348628=CARTESIAN_POINT('Ctrl Pts',(4.25269567199994,2.2,-1.37658259600002));
#348629=CARTESIAN_POINT('Ctrl Pts',(4.25114079099994,12.2,-1.37504955700001));
#348630=CARTESIAN_POINT('Ctrl Pts',(4.25114079099994,5.2,-1.37504955700001));
#348631=CARTESIAN_POINT('Ctrl Pts',(4.25114079099994,2.2,-1.37504955700001));
#348632=CARTESIAN_POINT('Ctrl Pts',(4.24958699699994,12.2,-1.37352092300001));
#348633=CARTESIAN_POINT('Ctrl Pts',(4.24958699699994,5.2,-1.37352092300001));
#348634=CARTESIAN_POINT('Ctrl Pts',(4.24958699699994,2.2,-1.37352092300001));
#348635=CARTESIAN_POINT('Ctrl Pts',(4.24803429999994,12.2,-1.37199669400002));
#348636=CARTESIAN_POINT('Ctrl Pts',(4.24803429999994,5.2,-1.37199669400002));
#348637=CARTESIAN_POINT('Ctrl Pts',(4.24803429999994,2.2,-1.37199669400002));
#348638=CARTESIAN_POINT('Ctrl Pts',(4.24648271099994,12.2,-1.37047686900001));
#348639=CARTESIAN_POINT('Ctrl Pts',(4.24648271099994,5.2,-1.37047686900001));
#348640=CARTESIAN_POINT('Ctrl Pts',(4.24648271099994,2.2,-1.37047686900001));
#348641=CARTESIAN_POINT('Ctrl Pts',(4.24493223999994,12.2,-1.36896144900001));
#348642=CARTESIAN_POINT('Ctrl Pts',(4.24493223999994,5.2,-1.36896144900001));
#348643=CARTESIAN_POINT('Ctrl Pts',(4.24493223999994,2.2,-1.36896144900001));
#348644=CARTESIAN_POINT('Ctrl Pts',(4.24338289699994,12.2,-1.36745043100001));
#348645=CARTESIAN_POINT('Ctrl Pts',(4.24338289699994,5.2,-1.36745043100001));
#348646=CARTESIAN_POINT('Ctrl Pts',(4.24338289699994,2.2,-1.36745043100001));
#348647=CARTESIAN_POINT('Ctrl Pts',(4.24183469099995,12.2,-1.36594381500001));
#348648=CARTESIAN_POINT('Ctrl Pts',(4.24183469099995,5.2,-1.36594381500001));
#348649=CARTESIAN_POINT('Ctrl Pts',(4.24183469099995,2.2,-1.36594381500001));
#348650=CARTESIAN_POINT('Ctrl Pts',(4.24028763399994,12.2,-1.36444160200002));
#348651=CARTESIAN_POINT('Ctrl Pts',(4.24028763399994,5.2,-1.36444160200002));
#348652=CARTESIAN_POINT('Ctrl Pts',(4.24028763399994,2.2,-1.36444160200002));
#348653=CARTESIAN_POINT('Ctrl Pts',(4.23874173499994,12.2,-1.36294379100002));
#348654=CARTESIAN_POINT('Ctrl Pts',(4.23874173499994,5.2,-1.36294379100002));
#348655=CARTESIAN_POINT('Ctrl Pts',(4.23874173499994,2.2,-1.36294379100002));
#348656=CARTESIAN_POINT('Ctrl Pts',(4.23719700499994,12.2,-1.36145038000001));
#348657=CARTESIAN_POINT('Ctrl Pts',(4.23719700499994,5.2,-1.36145038000001));
#348658=CARTESIAN_POINT('Ctrl Pts',(4.23719700499994,2.2,-1.36145038000001));
#348659=CARTESIAN_POINT('Ctrl Pts',(4.23565345399994,12.2,-1.35996136900001));
#348660=CARTESIAN_POINT('Ctrl Pts',(4.23565345399994,5.2,-1.35996136900001));
#348661=CARTESIAN_POINT('Ctrl Pts',(4.23565345399994,2.2,-1.35996136900001));
#348662=CARTESIAN_POINT('Ctrl Pts',(4.23411109299995,12.2,-1.35847675800001));
#348663=CARTESIAN_POINT('Ctrl Pts',(4.23411109299995,5.2,-1.35847675800001));
#348664=CARTESIAN_POINT('Ctrl Pts',(4.23411109299995,2.2,-1.35847675800001));
#348665=CARTESIAN_POINT('Ctrl Pts',(4.23256993099994,12.2,-1.35699654500002));
#348666=CARTESIAN_POINT('Ctrl Pts',(4.23256993099994,5.2,-1.35699654500002));
#348667=CARTESIAN_POINT('Ctrl Pts',(4.23256993099994,2.2,-1.35699654500002));
#348668=CARTESIAN_POINT('Ctrl Pts',(4.23102997899994,12.2,-1.35552073100001));
#348669=CARTESIAN_POINT('Ctrl Pts',(4.23102997899994,5.2,-1.35552073100001));
#348670=CARTESIAN_POINT('Ctrl Pts',(4.23102997899994,2.2,-1.35552073100001));
#348671=CARTESIAN_POINT('Ctrl Pts',(4.22949124699994,12.2,-1.35404931500001));
#348672=CARTESIAN_POINT('Ctrl Pts',(4.22949124699994,5.2,-1.35404931500001));
#348673=CARTESIAN_POINT('Ctrl Pts',(4.22949124699994,2.2,-1.35404931500001));
#348674=CARTESIAN_POINT('Ctrl Pts',(4.22795374499994,12.2,-1.35258229500002));
#348675=CARTESIAN_POINT('Ctrl Pts',(4.22795374499994,5.2,-1.35258229500002));
#348676=CARTESIAN_POINT('Ctrl Pts',(4.22795374499994,2.2,-1.35258229500002));
#348677=CARTESIAN_POINT('Ctrl Pts',(4.22641748499994,12.2,-1.35111967100002));
#348678=CARTESIAN_POINT('Ctrl Pts',(4.22641748499994,5.2,-1.35111967100002));
#348679=CARTESIAN_POINT('Ctrl Pts',(4.22641748499994,2.2,-1.35111967100002));
#348680=CARTESIAN_POINT('Ctrl Pts',(4.22488247499994,12.2,-1.34966144200002));
#348681=CARTESIAN_POINT('Ctrl Pts',(4.22488247499994,5.2,-1.34966144200002));
#348682=CARTESIAN_POINT('Ctrl Pts',(4.22488247499994,2.2,-1.34966144200002));
#348683=CARTESIAN_POINT('Ctrl Pts',(4.22334872799994,12.2,-1.34820760900002));
#348684=CARTESIAN_POINT('Ctrl Pts',(4.22334872799994,5.2,-1.34820760900002));
#348685=CARTESIAN_POINT('Ctrl Pts',(4.22334872799994,2.2,-1.34820760900002));
#348686=CARTESIAN_POINT('Ctrl Pts',(4.22181625199994,12.2,-1.34675816800002));
#348687=CARTESIAN_POINT('Ctrl Pts',(4.22181625199994,5.2,-1.34675816800002));
#348688=CARTESIAN_POINT('Ctrl Pts',(4.22181625199994,2.2,-1.34675816800002));
#348689=CARTESIAN_POINT('Ctrl Pts',(4.22028505899994,12.2,-1.34531312100002));
#348690=CARTESIAN_POINT('Ctrl Pts',(4.22028505899994,5.2,-1.34531312100002));
#348691=CARTESIAN_POINT('Ctrl Pts',(4.22028505899994,2.2,-1.34531312100002));
#348692=CARTESIAN_POINT('Ctrl Pts',(4.21875515899994,12.2,-1.34387246600001));
#348693=CARTESIAN_POINT('Ctrl Pts',(4.21875515899994,5.2,-1.34387246600001));
#348694=CARTESIAN_POINT('Ctrl Pts',(4.21875515899994,2.2,-1.34387246600001));
#348695=CARTESIAN_POINT('Ctrl Pts',(4.21722656199994,12.2,-1.34243620300001));
#348696=CARTESIAN_POINT('Ctrl Pts',(4.21722656199994,5.2,-1.34243620300001));
#348697=CARTESIAN_POINT('Ctrl Pts',(4.21722656199994,2.2,-1.34243620300001));
#348698=CARTESIAN_POINT('Ctrl Pts',(4.21569927799994,12.2,-1.34100433000001));
#348699=CARTESIAN_POINT('Ctrl Pts',(4.21569927799994,5.2,-1.34100433000001));
#348700=CARTESIAN_POINT('Ctrl Pts',(4.21569927799994,2.2,-1.34100433000001));
#348701=CARTESIAN_POINT('Ctrl Pts',(4.21417331899994,12.2,-1.33957684700002));
#348702=CARTESIAN_POINT('Ctrl Pts',(4.21417331899994,5.2,-1.33957684700002));
#348703=CARTESIAN_POINT('Ctrl Pts',(4.21417331899994,2.2,-1.33957684700002));
#348704=CARTESIAN_POINT('Ctrl Pts',(4.21264869399994,12.2,-1.33815375200002));
#348705=CARTESIAN_POINT('Ctrl Pts',(4.21264869399994,5.2,-1.33815375200002));
#348706=CARTESIAN_POINT('Ctrl Pts',(4.21264869399994,2.2,-1.33815375200002));
#348707=CARTESIAN_POINT('Ctrl Pts',(4.21112541399994,12.2,-1.33673504600001));
#348708=CARTESIAN_POINT('Ctrl Pts',(4.21112541399994,5.2,-1.33673504600001));
#348709=CARTESIAN_POINT('Ctrl Pts',(4.21112541399994,2.2,-1.33673504600001));
#348710=CARTESIAN_POINT('Ctrl Pts',(4.20960348999994,12.2,-1.33532072700001));
#348711=CARTESIAN_POINT('Ctrl Pts',(4.20960348999994,5.2,-1.33532072700001));
#348712=CARTESIAN_POINT('Ctrl Pts',(4.20960348999994,2.2,-1.33532072700001));
#348713=CARTESIAN_POINT('Ctrl Pts',(4.20808293199994,12.2,-1.33391079400001));
#348714=CARTESIAN_POINT('Ctrl Pts',(4.20808293199994,5.2,-1.33391079400001));
#348715=CARTESIAN_POINT('Ctrl Pts',(4.20808293199994,2.2,-1.33391079400001));
#348716=CARTESIAN_POINT('Ctrl Pts',(4.20656375099994,12.2,-1.33250524600002));
#348717=CARTESIAN_POINT('Ctrl Pts',(4.20656375099994,5.2,-1.33250524600002));
#348718=CARTESIAN_POINT('Ctrl Pts',(4.20656375099994,2.2,-1.33250524600002));
#348719=CARTESIAN_POINT('Ctrl Pts',(4.20504595699995,12.2,-1.33110408200002));
#348720=CARTESIAN_POINT('Ctrl Pts',(4.20504595699995,5.2,-1.33110408200002));
#348721=CARTESIAN_POINT('Ctrl Pts',(4.20504595699995,2.2,-1.33110408200002));
#348722=CARTESIAN_POINT('Ctrl Pts',(4.20352956099994,12.2,-1.32970730200002));
#348723=CARTESIAN_POINT('Ctrl Pts',(4.20352956099994,5.2,-1.32970730200002));
#348724=CARTESIAN_POINT('Ctrl Pts',(4.20352956099994,2.2,-1.32970730200002));
#348725=CARTESIAN_POINT('Ctrl Pts',(4.20201457299994,12.2,-1.32831490500001));
#348726=CARTESIAN_POINT('Ctrl Pts',(4.20201457299994,5.2,-1.32831490500001));
#348727=CARTESIAN_POINT('Ctrl Pts',(4.20201457299994,2.2,-1.32831490500001));
#348728=CARTESIAN_POINT('Ctrl Pts',(4.20050100399994,12.2,-1.32692688800002));
#348729=CARTESIAN_POINT('Ctrl Pts',(4.20050100399994,5.2,-1.32692688800002));
#348730=CARTESIAN_POINT('Ctrl Pts',(4.20050100399994,2.2,-1.32692688800002));
#348731=CARTESIAN_POINT('Ctrl Pts',(4.19898886499994,12.2,-1.32554325300001));
#348732=CARTESIAN_POINT('Ctrl Pts',(4.19898886499994,5.2,-1.32554325300001));
#348733=CARTESIAN_POINT('Ctrl Pts',(4.19898886499994,2.2,-1.32554325300001));
#348734=CARTESIAN_POINT('Ctrl Pts',(4.19747816499994,12.2,-1.32416399600002));
#348735=CARTESIAN_POINT('Ctrl Pts',(4.19747816499994,5.2,-1.32416399600002));
#348736=CARTESIAN_POINT('Ctrl Pts',(4.19747816499994,2.2,-1.32416399600002));
#348737=CARTESIAN_POINT('Ctrl Pts',(4.19596891699995,12.2,-1.32278911800002));
#348738=CARTESIAN_POINT('Ctrl Pts',(4.19596891699995,5.2,-1.32278911800002));
#348739=CARTESIAN_POINT('Ctrl Pts',(4.19596891699995,2.2,-1.32278911800002));
#348740=CARTESIAN_POINT('Ctrl Pts',(4.19446112999994,12.2,-1.32141861700001));
#348741=CARTESIAN_POINT('Ctrl Pts',(4.19446112999994,5.2,-1.32141861700001));
#348742=CARTESIAN_POINT('Ctrl Pts',(4.19446112999994,2.2,-1.32141861700001));
#348743=CARTESIAN_POINT('Ctrl Pts',(4.19295481499994,12.2,-1.32005249200001));
#348744=CARTESIAN_POINT('Ctrl Pts',(4.19295481499994,5.2,-1.32005249200001));
#348745=CARTESIAN_POINT('Ctrl Pts',(4.19295481499994,2.2,-1.32005249200001));
#348746=CARTESIAN_POINT('Ctrl Pts',(4.19144998399995,12.2,-1.31869074300001));
#348747=CARTESIAN_POINT('Ctrl Pts',(4.19144998399995,5.2,-1.31869074300001));
#348748=CARTESIAN_POINT('Ctrl Pts',(4.19144998399995,2.2,-1.31869074300001));
#348749=CARTESIAN_POINT('Ctrl Pts',(4.18994664499994,12.2,-1.31733336700002));
#348750=CARTESIAN_POINT('Ctrl Pts',(4.18994664499994,5.2,-1.31733336700002));
#348751=CARTESIAN_POINT('Ctrl Pts',(4.18994664499994,2.2,-1.31733336700002));
#348752=CARTESIAN_POINT('Ctrl Pts',(4.18844481099994,12.2,-1.31598036500002));
#348753=CARTESIAN_POINT('Ctrl Pts',(4.18844481099994,5.2,-1.31598036500002));
#348754=CARTESIAN_POINT('Ctrl Pts',(4.18844481099994,2.2,-1.31598036500002));
#348755=CARTESIAN_POINT('Ctrl Pts',(4.18694449099995,12.2,-1.31463173400002));
#348756=CARTESIAN_POINT('Ctrl Pts',(4.18694449099995,5.2,-1.31463173400002));
#348757=CARTESIAN_POINT('Ctrl Pts',(4.18694449099995,2.2,-1.31463173400002));
#348758=CARTESIAN_POINT('Ctrl Pts',(4.18544569799994,12.2,-1.31328747400001));
#348759=CARTESIAN_POINT('Ctrl Pts',(4.18544569799994,5.2,-1.31328747400001));
#348760=CARTESIAN_POINT('Ctrl Pts',(4.18544569799994,2.2,-1.31328747400001));
#348761=CARTESIAN_POINT('Ctrl Pts',(4.18394844199994,12.2,-1.31194758300001));
#348762=CARTESIAN_POINT('Ctrl Pts',(4.18394844199994,5.2,-1.31194758300001));
#348763=CARTESIAN_POINT('Ctrl Pts',(4.18394844199994,2.2,-1.31194758300001));
#348764=CARTESIAN_POINT('Ctrl Pts',(4.18245273199994,12.2,-1.31061206100001));
#348765=CARTESIAN_POINT('Ctrl Pts',(4.18245273199994,5.2,-1.31061206100001));
#348766=CARTESIAN_POINT('Ctrl Pts',(4.18245273199994,2.2,-1.31061206100001));
#348767=CARTESIAN_POINT('Ctrl Pts',(4.18095858099994,12.2,-1.30928090600001));
#348768=CARTESIAN_POINT('Ctrl Pts',(4.18095858099994,5.2,-1.30928090600001));
#348769=CARTESIAN_POINT('Ctrl Pts',(4.18095858099994,2.2,-1.30928090600001));
#348770=CARTESIAN_POINT('Ctrl Pts',(4.17946599699994,12.2,-1.30795411700001));
#348771=CARTESIAN_POINT('Ctrl Pts',(4.17946599699994,5.2,-1.30795411700001));
#348772=CARTESIAN_POINT('Ctrl Pts',(4.17946599699994,2.2,-1.30795411700001));
#348773=CARTESIAN_POINT('Ctrl Pts',(4.17797499499994,12.2,-1.30663169200002));
#348774=CARTESIAN_POINT('Ctrl Pts',(4.17797499499994,5.2,-1.30663169200002));
#348775=CARTESIAN_POINT('Ctrl Pts',(4.17797499499994,2.2,-1.30663169200002));
#348776=CARTESIAN_POINT('Ctrl Pts',(4.17648558199994,12.2,-1.30531363000001));
#348777=CARTESIAN_POINT('Ctrl Pts',(4.17648558199994,5.2,-1.30531363000001));
#348778=CARTESIAN_POINT('Ctrl Pts',(4.17648558199994,2.2,-1.30531363000001));
#348779=CARTESIAN_POINT('Ctrl Pts',(4.17499777099995,12.2,-1.30399993100001));
#348780=CARTESIAN_POINT('Ctrl Pts',(4.17499777099995,5.2,-1.30399993100001));
#348781=CARTESIAN_POINT('Ctrl Pts',(4.17499777099995,2.2,-1.30399993100001));
#348782=CARTESIAN_POINT('Ctrl Pts',(4.17351157199994,12.2,-1.30269059300002));
#348783=CARTESIAN_POINT('Ctrl Pts',(4.17351157199994,5.2,-1.30269059300002));
#348784=CARTESIAN_POINT('Ctrl Pts',(4.17351157199994,2.2,-1.30269059300002));
#348785=CARTESIAN_POINT('Ctrl Pts',(4.17202699599994,12.2,-1.30138561400001));
#348786=CARTESIAN_POINT('Ctrl Pts',(4.17202699599994,5.2,-1.30138561400001));
#348787=CARTESIAN_POINT('Ctrl Pts',(4.17202699599994,2.2,-1.30138561400001));
#348788=CARTESIAN_POINT('Ctrl Pts',(4.17054405399994,12.2,-1.30008499300001));
#348789=CARTESIAN_POINT('Ctrl Pts',(4.17054405399994,5.2,-1.30008499300001));
#348790=CARTESIAN_POINT('Ctrl Pts',(4.17054405399994,2.2,-1.30008499300001));
#348791=CARTESIAN_POINT('Ctrl Pts',(4.16906275799994,12.2,-1.29878873000001));
#348792=CARTESIAN_POINT('Ctrl Pts',(4.16906275799994,5.2,-1.29878873000001));
#348793=CARTESIAN_POINT('Ctrl Pts',(4.16906275799994,2.2,-1.29878873000001));
#348794=CARTESIAN_POINT('Ctrl Pts',(4.16758311699994,12.2,-1.29749682100002));
#348795=CARTESIAN_POINT('Ctrl Pts',(4.16758311699994,5.2,-1.29749682100002));
#348796=CARTESIAN_POINT('Ctrl Pts',(4.16758311699994,2.2,-1.29749682100002));
#348797=CARTESIAN_POINT('Ctrl Pts',(4.16610514399994,12.2,-1.29620926700001));
#348798=CARTESIAN_POINT('Ctrl Pts',(4.16610514399994,5.2,-1.29620926700001));
#348799=CARTESIAN_POINT('Ctrl Pts',(4.16610514399994,2.2,-1.29620926700001));
#348800=CARTESIAN_POINT('Ctrl Pts',(4.16462884799994,12.2,-1.29492606500001));
#348801=CARTESIAN_POINT('Ctrl Pts',(4.16462884799994,5.2,-1.29492606500001));
#348802=CARTESIAN_POINT('Ctrl Pts',(4.16462884799994,2.2,-1.29492606500001));
#348803=CARTESIAN_POINT('Ctrl Pts',(4.16315424099994,12.2,-1.29364721600002));
#348804=CARTESIAN_POINT('Ctrl Pts',(4.16315424099994,5.2,-1.29364721600002));
#348805=CARTESIAN_POINT('Ctrl Pts',(4.16315424099994,2.2,-1.29364721600002));
#348806=CARTESIAN_POINT('Ctrl Pts',(4.16168133299994,12.2,-1.29237271600001));
#348807=CARTESIAN_POINT('Ctrl Pts',(4.16168133299994,5.2,-1.29237271600001));
#348808=CARTESIAN_POINT('Ctrl Pts',(4.16168133299994,2.2,-1.29237271600001));
#348809=CARTESIAN_POINT('Ctrl Pts',(4.16021013599994,12.2,-1.29110256400002));
#348810=CARTESIAN_POINT('Ctrl Pts',(4.16021013599994,5.2,-1.29110256400002));
#348811=CARTESIAN_POINT('Ctrl Pts',(4.16021013599994,2.2,-1.29110256400002));
#348812=CARTESIAN_POINT('Ctrl Pts',(4.15874066199994,12.2,-1.28983676000002));
#348813=CARTESIAN_POINT('Ctrl Pts',(4.15874066199994,5.2,-1.28983676000002));
#348814=CARTESIAN_POINT('Ctrl Pts',(4.15874066199994,2.2,-1.28983676000002));
#348815=CARTESIAN_POINT('Ctrl Pts',(4.15727291999994,12.2,-1.28857530100001));
#348816=CARTESIAN_POINT('Ctrl Pts',(4.15727291999994,5.2,-1.28857530100001));
#348817=CARTESIAN_POINT('Ctrl Pts',(4.15727291999994,2.2,-1.28857530100001));
#348818=CARTESIAN_POINT('Ctrl Pts',(4.15580692199994,12.2,-1.28731818500002));
#348819=CARTESIAN_POINT('Ctrl Pts',(4.15580692199994,5.2,-1.28731818500002));
#348820=CARTESIAN_POINT('Ctrl Pts',(4.15580692199994,2.2,-1.28731818500002));
#348821=CARTESIAN_POINT('Ctrl Pts',(4.15434267899994,12.2,-1.28606541400002));
#348822=CARTESIAN_POINT('Ctrl Pts',(4.15434267899994,5.2,-1.28606541400002));
#348823=CARTESIAN_POINT('Ctrl Pts',(4.15434267899994,2.2,-1.28606541400002));
#348824=CARTESIAN_POINT('Ctrl Pts',(4.15288020299994,12.2,-1.28481698200002));
#348825=CARTESIAN_POINT('Ctrl Pts',(4.15288020299994,5.2,-1.28481698200002));
#348826=CARTESIAN_POINT('Ctrl Pts',(4.15288020299994,2.2,-1.28481698200002));
#348827=CARTESIAN_POINT('Ctrl Pts',(4.15141950299994,12.2,-1.28357289000002));
#348828=CARTESIAN_POINT('Ctrl Pts',(4.15141950299994,5.2,-1.28357289000002));
#348829=CARTESIAN_POINT('Ctrl Pts',(4.15141950299994,2.2,-1.28357289000002));
#348830=CARTESIAN_POINT('Ctrl Pts',(4.14996059099995,12.2,-1.28233313700001));
#348831=CARTESIAN_POINT('Ctrl Pts',(4.14996059099995,5.2,-1.28233313700001));
#348832=CARTESIAN_POINT('Ctrl Pts',(4.14996059099995,2.2,-1.28233313700001));
#348833=CARTESIAN_POINT('Ctrl Pts',(4.14850347999994,12.2,-1.28109772000002));
#348834=CARTESIAN_POINT('Ctrl Pts',(4.14850347999994,5.2,-1.28109772000002));
#348835=CARTESIAN_POINT('Ctrl Pts',(4.14850347999994,2.2,-1.28109772000002));
#348836=CARTESIAN_POINT('Ctrl Pts',(4.14704817999994,12.2,-1.27986663600002));
#348837=CARTESIAN_POINT('Ctrl Pts',(4.14704817999994,5.2,-1.27986663600002));
#348838=CARTESIAN_POINT('Ctrl Pts',(4.14704817999994,2.2,-1.27986663600002));
#348839=CARTESIAN_POINT('Ctrl Pts',(4.14559469999995,12.2,-1.27863988700001));
#348840=CARTESIAN_POINT('Ctrl Pts',(4.14559469999995,5.2,-1.27863988700001));
#348841=CARTESIAN_POINT('Ctrl Pts',(4.14559469999995,2.2,-1.27863988700001));
#348842=CARTESIAN_POINT('Ctrl Pts',(4.14414305399994,12.2,-1.27741746900002));
#348843=CARTESIAN_POINT('Ctrl Pts',(4.14414305399994,5.2,-1.27741746900002));
#348844=CARTESIAN_POINT('Ctrl Pts',(4.14414305399994,2.2,-1.27741746900002));
#348845=CARTESIAN_POINT('Ctrl Pts',(4.14269325199994,12.2,-1.27619938100001));
#348846=CARTESIAN_POINT('Ctrl Pts',(4.14269325199994,5.2,-1.27619938100001));
#348847=CARTESIAN_POINT('Ctrl Pts',(4.14269325199994,2.2,-1.27619938100001));
#348848=CARTESIAN_POINT('Ctrl Pts',(4.14124530599994,12.2,-1.27498562100001));
#348849=CARTESIAN_POINT('Ctrl Pts',(4.14124530599994,5.2,-1.27498562100001));
#348850=CARTESIAN_POINT('Ctrl Pts',(4.14124530599994,2.2,-1.27498562100001));
#348851=CARTESIAN_POINT('Ctrl Pts',(4.13979922699994,12.2,-1.27377618700002));
#348852=CARTESIAN_POINT('Ctrl Pts',(4.13979922699994,5.2,-1.27377618700002));
#348853=CARTESIAN_POINT('Ctrl Pts',(4.13979922699994,2.2,-1.27377618700002));
#348854=CARTESIAN_POINT('Ctrl Pts',(4.13835502499994,12.2,-1.27257107800002));
#348855=CARTESIAN_POINT('Ctrl Pts',(4.13835502499994,5.2,-1.27257107800002));
#348856=CARTESIAN_POINT('Ctrl Pts',(4.13835502499994,2.2,-1.27257107800002));
#348857=CARTESIAN_POINT('Ctrl Pts',(4.13691271299994,12.2,-1.27137029300001));
#348858=CARTESIAN_POINT('Ctrl Pts',(4.13691271299994,5.2,-1.27137029300001));
#348859=CARTESIAN_POINT('Ctrl Pts',(4.13691271299994,2.2,-1.27137029300001));
#348860=CARTESIAN_POINT('Ctrl Pts',(4.13547230099994,12.2,-1.27017382800001));
#348861=CARTESIAN_POINT('Ctrl Pts',(4.13547230099994,5.2,-1.27017382800001));
#348862=CARTESIAN_POINT('Ctrl Pts',(4.13547230099994,2.2,-1.27017382800001));
#348863=CARTESIAN_POINT('Ctrl Pts',(4.13403380099994,12.2,-1.26898168400002));
#348864=CARTESIAN_POINT('Ctrl Pts',(4.13403380099994,5.2,-1.26898168400002));
#348865=CARTESIAN_POINT('Ctrl Pts',(4.13403380099994,2.2,-1.26898168400002));
#348866=CARTESIAN_POINT('Ctrl Pts',(4.13259722399994,12.2,-1.26779385600001));
#348867=CARTESIAN_POINT('Ctrl Pts',(4.13259722399994,5.2,-1.26779385600001));
#348868=CARTESIAN_POINT('Ctrl Pts',(4.13259722399994,2.2,-1.26779385600001));
#348869=CARTESIAN_POINT('Ctrl Pts',(4.13116258199994,12.2,-1.26661034500001));
#348870=CARTESIAN_POINT('Ctrl Pts',(4.13116258199994,5.2,-1.26661034500001));
#348871=CARTESIAN_POINT('Ctrl Pts',(4.13116258199994,2.2,-1.26661034500001));
#348872=CARTESIAN_POINT('Ctrl Pts',(4.12972988599994,12.2,-1.26543114900001));
#348873=CARTESIAN_POINT('Ctrl Pts',(4.12972988599994,5.2,-1.26543114900001));
#348874=CARTESIAN_POINT('Ctrl Pts',(4.12972988599994,2.2,-1.26543114900001));
#348875=CARTESIAN_POINT('Ctrl Pts',(4.12829914699994,12.2,-1.26425626500001));
#348876=CARTESIAN_POINT('Ctrl Pts',(4.12829914699994,5.2,-1.26425626500001));
#348877=CARTESIAN_POINT('Ctrl Pts',(4.12829914699994,2.2,-1.26425626500001));
#348878=CARTESIAN_POINT('Ctrl Pts',(4.12687037699994,12.2,-1.26308569100001));
#348879=CARTESIAN_POINT('Ctrl Pts',(4.12687037699994,5.2,-1.26308569100001));
#348880=CARTESIAN_POINT('Ctrl Pts',(4.12687037699994,2.2,-1.26308569100001));
#348881=CARTESIAN_POINT('Ctrl Pts',(4.12544358599995,12.2,-1.26191942500002));
#348882=CARTESIAN_POINT('Ctrl Pts',(4.12544358599995,5.2,-1.26191942500002));
#348883=CARTESIAN_POINT('Ctrl Pts',(4.12544358599995,2.2,-1.26191942500002));
#348884=CARTESIAN_POINT('Ctrl Pts',(4.12401878699994,12.2,-1.26075746600002));
#348885=CARTESIAN_POINT('Ctrl Pts',(4.12401878699994,5.2,-1.26075746600002));
#348886=CARTESIAN_POINT('Ctrl Pts',(4.12401878699994,2.2,-1.26075746600002));
#348887=CARTESIAN_POINT('Ctrl Pts',(4.12259599199994,12.2,-1.25959981300001));
#348888=CARTESIAN_POINT('Ctrl Pts',(4.12259599199994,5.2,-1.25959981300001));
#348889=CARTESIAN_POINT('Ctrl Pts',(4.12259599199994,2.2,-1.25959981300001));
#348890=CARTESIAN_POINT('Ctrl Pts',(4.12117520999994,12.2,-1.25844646100001));
#348891=CARTESIAN_POINT('Ctrl Pts',(4.12117520999994,5.2,-1.25844646100001));
#348892=CARTESIAN_POINT('Ctrl Pts',(4.12117520999994,2.2,-1.25844646100001));
#348893=CARTESIAN_POINT('Ctrl Pts',(4.11975645499994,12.2,-1.25729741200002));
#348894=CARTESIAN_POINT('Ctrl Pts',(4.11975645499994,5.2,-1.25729741200002));
#348895=CARTESIAN_POINT('Ctrl Pts',(4.11975645499994,2.2,-1.25729741200002));
#348896=CARTESIAN_POINT('Ctrl Pts',(4.11833973699994,12.2,-1.25615266000001));
#348897=CARTESIAN_POINT('Ctrl Pts',(4.11833973699994,5.2,-1.25615266000001));
#348898=CARTESIAN_POINT('Ctrl Pts',(4.11833973699994,2.2,-1.25615266000001));
#348899=CARTESIAN_POINT('Ctrl Pts',(4.11692506799994,12.2,-1.25501220700002));
#348900=CARTESIAN_POINT('Ctrl Pts',(4.11692506799994,5.2,-1.25501220700002));
#348901=CARTESIAN_POINT('Ctrl Pts',(4.11692506799994,2.2,-1.25501220700002));
#348902=CARTESIAN_POINT('Ctrl Pts',(4.11551245899994,12.2,-1.25387604800002));
#348903=CARTESIAN_POINT('Ctrl Pts',(4.11551245899994,5.2,-1.25387604800002));
#348904=CARTESIAN_POINT('Ctrl Pts',(4.11551245899994,2.2,-1.25387604800002));
#348905=CARTESIAN_POINT('Ctrl Pts',(4.11410192199994,12.2,-1.25274418100001));
#348906=CARTESIAN_POINT('Ctrl Pts',(4.11410192199994,5.2,-1.25274418100001));
#348907=CARTESIAN_POINT('Ctrl Pts',(4.11410192199994,2.2,-1.25274418100001));
#348908=CARTESIAN_POINT('Ctrl Pts',(4.11269346899994,12.2,-1.25161660600002));
#348909=CARTESIAN_POINT('Ctrl Pts',(4.11269346899994,5.2,-1.25161660600002));
#348910=CARTESIAN_POINT('Ctrl Pts',(4.11269346899994,2.2,-1.25161660600002));
#348911=CARTESIAN_POINT('Ctrl Pts',(4.11128710999995,12.2,-1.25049332000001));
#348912=CARTESIAN_POINT('Ctrl Pts',(4.11128710999995,5.2,-1.25049332000001));
#348913=CARTESIAN_POINT('Ctrl Pts',(4.11128710999995,2.2,-1.25049332000001));
#348914=CARTESIAN_POINT('Ctrl Pts',(4.10988285899994,12.2,-1.24937432000001));
#348915=CARTESIAN_POINT('Ctrl Pts',(4.10988285899994,5.2,-1.24937432000001));
#348916=CARTESIAN_POINT('Ctrl Pts',(4.10988285899994,2.2,-1.24937432000001));
#348917=CARTESIAN_POINT('Ctrl Pts',(4.10848072599994,12.2,-1.24825960500001));
#348918=CARTESIAN_POINT('Ctrl Pts',(4.10848072599994,5.2,-1.24825960500001));
#348919=CARTESIAN_POINT('Ctrl Pts',(4.10848072599994,2.2,-1.24825960500001));
#348920=CARTESIAN_POINT('Ctrl Pts',(4.10708072299994,12.2,-1.24714917200002));
#348921=CARTESIAN_POINT('Ctrl Pts',(4.10708072299994,5.2,-1.24714917200002));
#348922=CARTESIAN_POINT('Ctrl Pts',(4.10708072299994,2.2,-1.24714917200002));
#348923=CARTESIAN_POINT('Ctrl Pts',(4.10568286099994,12.2,-1.24604302000002));
#348924=CARTESIAN_POINT('Ctrl Pts',(4.10568286099994,5.2,-1.24604302000002));
#348925=CARTESIAN_POINT('Ctrl Pts',(4.10568286099994,2.2,-1.24604302000002));
#348926=CARTESIAN_POINT('Ctrl Pts',(4.10428715299994,12.2,-1.24494114600001));
#348927=CARTESIAN_POINT('Ctrl Pts',(4.10428715299994,5.2,-1.24494114600001));
#348928=CARTESIAN_POINT('Ctrl Pts',(4.10428715299994,2.2,-1.24494114600001));
#348929=CARTESIAN_POINT('Ctrl Pts',(4.10289360999994,12.2,-1.24384354800001));
#348930=CARTESIAN_POINT('Ctrl Pts',(4.10289360999994,5.2,-1.24384354800001));
#348931=CARTESIAN_POINT('Ctrl Pts',(4.10289360999994,2.2,-1.24384354800001));
#348932=CARTESIAN_POINT('Ctrl Pts',(4.10150224399994,12.2,-1.24275022400001));
#348933=CARTESIAN_POINT('Ctrl Pts',(4.10150224399994,5.2,-1.24275022400001));
#348934=CARTESIAN_POINT('Ctrl Pts',(4.10150224399994,2.2,-1.24275022400001));
#348935=CARTESIAN_POINT('Ctrl Pts',(4.10011306599994,12.2,-1.24166117200001));
#348936=CARTESIAN_POINT('Ctrl Pts',(4.10011306599994,5.2,-1.24166117200001));
#348937=CARTESIAN_POINT('Ctrl Pts',(4.10011306599994,2.2,-1.24166117200001));
#348938=CARTESIAN_POINT('Ctrl Pts',(4.09872608799995,12.2,-1.24057638900001));
#348939=CARTESIAN_POINT('Ctrl Pts',(4.09872608799995,5.2,-1.24057638900001));
#348940=CARTESIAN_POINT('Ctrl Pts',(4.09872608799995,2.2,-1.24057638900001));
#348941=CARTESIAN_POINT('Ctrl Pts',(4.09734132199994,12.2,-1.23949587400002));
#348942=CARTESIAN_POINT('Ctrl Pts',(4.09734132199994,5.2,-1.23949587400002));
#348943=CARTESIAN_POINT('Ctrl Pts',(4.09734132199994,2.2,-1.23949587400002));
#348944=CARTESIAN_POINT('Ctrl Pts',(4.09595877899994,12.2,-1.23841962300002));
#348945=CARTESIAN_POINT('Ctrl Pts',(4.09595877899994,5.2,-1.23841962300002));
#348946=CARTESIAN_POINT('Ctrl Pts',(4.09595877899994,2.2,-1.23841962300002));
#348947=CARTESIAN_POINT('Ctrl Pts',(4.09457847299994,12.2,-1.23734763400002));
#348948=CARTESIAN_POINT('Ctrl Pts',(4.09457847299994,5.2,-1.23734763400002));
#348949=CARTESIAN_POINT('Ctrl Pts',(4.09457847299994,2.2,-1.23734763400002));
#348950=CARTESIAN_POINT('Ctrl Pts',(4.09320041299994,12.2,-1.23627990700002));
#348951=CARTESIAN_POINT('Ctrl Pts',(4.09320041299994,5.2,-1.23627990700002));
#348952=CARTESIAN_POINT('Ctrl Pts',(4.09320041299994,2.2,-1.23627990700002));
#348953=CARTESIAN_POINT('Ctrl Pts',(4.09182461299994,12.2,-1.23521643600002));
#348954=CARTESIAN_POINT('Ctrl Pts',(4.09182461299994,5.2,-1.23521643600002));
#348955=CARTESIAN_POINT('Ctrl Pts',(4.09182461299994,2.2,-1.23521643600002));
#348956=CARTESIAN_POINT('Ctrl Pts',(4.09045108399994,12.2,-1.23415722100002));
#348957=CARTESIAN_POINT('Ctrl Pts',(4.09045108399994,5.2,-1.23415722100002));
#348958=CARTESIAN_POINT('Ctrl Pts',(4.09045108399994,2.2,-1.23415722100002));
#348959=CARTESIAN_POINT('Ctrl Pts',(4.08907983799994,12.2,-1.23310226000001));
#348960=CARTESIAN_POINT('Ctrl Pts',(4.08907983799994,5.2,-1.23310226000001));
#348961=CARTESIAN_POINT('Ctrl Pts',(4.08907983799994,2.2,-1.23310226000001));
#348962=CARTESIAN_POINT('Ctrl Pts',(4.08771088599994,12.2,-1.23205154900001));
#348963=CARTESIAN_POINT('Ctrl Pts',(4.08771088599994,5.2,-1.23205154900001));
#348964=CARTESIAN_POINT('Ctrl Pts',(4.08771088599994,2.2,-1.23205154900001));
#348965=CARTESIAN_POINT('Ctrl Pts',(4.08634424099994,12.2,-1.23100508600002));
#348966=CARTESIAN_POINT('Ctrl Pts',(4.08634424099994,5.2,-1.23100508600002));
#348967=CARTESIAN_POINT('Ctrl Pts',(4.08634424099994,2.2,-1.23100508600002));
#348968=CARTESIAN_POINT('Ctrl Pts',(4.08497991499994,12.2,-1.22996287000001));
#348969=CARTESIAN_POINT('Ctrl Pts',(4.08497991499994,5.2,-1.22996287000001));
#348970=CARTESIAN_POINT('Ctrl Pts',(4.08497991499994,2.2,-1.22996287000001));
#348971=CARTESIAN_POINT('Ctrl Pts',(4.08361791899994,12.2,-1.22892489700002));
#348972=CARTESIAN_POINT('Ctrl Pts',(4.08361791899994,5.2,-1.22892489700002));
#348973=CARTESIAN_POINT('Ctrl Pts',(4.08361791899994,2.2,-1.22892489700002));
#348974=CARTESIAN_POINT('Ctrl Pts',(4.08225826499994,12.2,-1.22789116500002));
#348975=CARTESIAN_POINT('Ctrl Pts',(4.08225826499994,5.2,-1.22789116500002));
#348976=CARTESIAN_POINT('Ctrl Pts',(4.08225826499994,2.2,-1.22789116500002));
#348977=CARTESIAN_POINT('Ctrl Pts',(4.08090096699994,12.2,-1.22686167100001));
#348978=CARTESIAN_POINT('Ctrl Pts',(4.08090096699994,5.2,-1.22686167100001));
#348979=CARTESIAN_POINT('Ctrl Pts',(4.08090096699994,2.2,-1.22686167100001));
#348980=CARTESIAN_POINT('Ctrl Pts',(4.07954603499994,12.2,-1.22583641400002));
#348981=CARTESIAN_POINT('Ctrl Pts',(4.07954603499994,5.2,-1.22583641400002));
#348982=CARTESIAN_POINT('Ctrl Pts',(4.07954603499994,2.2,-1.22583641400002));
#348983=CARTESIAN_POINT('Ctrl Pts',(4.07819348099994,12.2,-1.22481538900002));
#348984=CARTESIAN_POINT('Ctrl Pts',(4.07819348099994,5.2,-1.22481538900002));
#348985=CARTESIAN_POINT('Ctrl Pts',(4.07819348099994,2.2,-1.22481538900002));
#348986=CARTESIAN_POINT('Ctrl Pts',(4.07684331699994,12.2,-1.22379859500001));
#348987=CARTESIAN_POINT('Ctrl Pts',(4.07684331699994,5.2,-1.22379859500001));
#348988=CARTESIAN_POINT('Ctrl Pts',(4.07684331699994,2.2,-1.22379859500001));
#348989=CARTESIAN_POINT('Ctrl Pts',(4.07549555599994,12.2,-1.22278602900002));
#348990=CARTESIAN_POINT('Ctrl Pts',(4.07549555599994,5.2,-1.22278602900002));
#348991=CARTESIAN_POINT('Ctrl Pts',(4.07549555599994,2.2,-1.22278602900002));
#348992=CARTESIAN_POINT('Ctrl Pts',(4.07415020999994,12.2,-1.22177768900002));
#348993=CARTESIAN_POINT('Ctrl Pts',(4.07415020999994,5.2,-1.22177768900002));
#348994=CARTESIAN_POINT('Ctrl Pts',(4.07415020999994,2.2,-1.22177768900002));
#348995=CARTESIAN_POINT('Ctrl Pts',(4.07280729099995,12.2,-1.22077357300002));
#348996=CARTESIAN_POINT('Ctrl Pts',(4.07280729099995,5.2,-1.22077357300002));
#348997=CARTESIAN_POINT('Ctrl Pts',(4.07280729099995,2.2,-1.22077357300002));
#348998=CARTESIAN_POINT('Ctrl Pts',(4.07146680999994,12.2,-1.21977367600001));
#348999=CARTESIAN_POINT('Ctrl Pts',(4.07146680999994,5.2,-1.21977367600001));
#349000=CARTESIAN_POINT('Ctrl Pts',(4.07146680999994,2.2,-1.21977367600001));
#349001=CARTESIAN_POINT('Ctrl Pts',(4.07012877999995,12.2,-1.21877799800002));
#349002=CARTESIAN_POINT('Ctrl Pts',(4.07012877999995,5.2,-1.21877799800002));
#349003=CARTESIAN_POINT('Ctrl Pts',(4.07012877999995,2.2,-1.21877799800002));
#349004=CARTESIAN_POINT('Ctrl Pts',(4.06879321399995,12.2,-1.21778653400002));
#349005=CARTESIAN_POINT('Ctrl Pts',(4.06879321399995,5.2,-1.21778653400002));
#349006=CARTESIAN_POINT('Ctrl Pts',(4.06879321399995,2.2,-1.21778653400002));
#349007=CARTESIAN_POINT('Ctrl Pts',(4.06746012299994,12.2,-1.21679928200002));
#349008=CARTESIAN_POINT('Ctrl Pts',(4.06746012299994,5.2,-1.21679928200002));
#349009=CARTESIAN_POINT('Ctrl Pts',(4.06746012299994,2.2,-1.21679928200002));
#349010=CARTESIAN_POINT('Ctrl Pts',(4.06612951899994,12.2,-1.21581624000001));
#349011=CARTESIAN_POINT('Ctrl Pts',(4.06612951899994,5.2,-1.21581624000001));
#349012=CARTESIAN_POINT('Ctrl Pts',(4.06612951899994,2.2,-1.21581624000001));
#349013=CARTESIAN_POINT('Ctrl Pts',(4.06480141499994,12.2,-1.21483740400001));
#349014=CARTESIAN_POINT('Ctrl Pts',(4.06480141499994,5.2,-1.21483740400001));
#349015=CARTESIAN_POINT('Ctrl Pts',(4.06480141499994,2.2,-1.21483740400001));
#349016=CARTESIAN_POINT('Ctrl Pts',(4.06347582299994,12.2,-1.21386277300001));
#349017=CARTESIAN_POINT('Ctrl Pts',(4.06347582299994,5.2,-1.21386277300001));
#349018=CARTESIAN_POINT('Ctrl Pts',(4.06347582299994,2.2,-1.21386277300001));
#349019=CARTESIAN_POINT('Ctrl Pts',(4.06215275499994,12.2,-1.21289234200002));
#349020=CARTESIAN_POINT('Ctrl Pts',(4.06215275499994,5.2,-1.21289234200002));
#349021=CARTESIAN_POINT('Ctrl Pts',(4.06215275499994,2.2,-1.21289234200002));
#349022=CARTESIAN_POINT('Ctrl Pts',(4.06083222399995,12.2,-1.21192611000001));
#349023=CARTESIAN_POINT('Ctrl Pts',(4.06083222399995,5.2,-1.21192611000001));
#349024=CARTESIAN_POINT('Ctrl Pts',(4.06083222399995,2.2,-1.21192611000001));
#349025=CARTESIAN_POINT('Ctrl Pts',(4.05951424099994,12.2,-1.21096407400001));
#349026=CARTESIAN_POINT('Ctrl Pts',(4.05951424099994,5.2,-1.21096407400001));
#349027=CARTESIAN_POINT('Ctrl Pts',(4.05951424099994,2.2,-1.21096407400001));
#349028=CARTESIAN_POINT('Ctrl Pts',(4.05819881799994,12.2,-1.21000623000001));
#349029=CARTESIAN_POINT('Ctrl Pts',(4.05819881799994,5.2,-1.21000623000001));
#349030=CARTESIAN_POINT('Ctrl Pts',(4.05819881799994,2.2,-1.21000623000001));
#349031=CARTESIAN_POINT('Ctrl Pts',(4.05688596999994,12.2,-1.20905257600001));
#349032=CARTESIAN_POINT('Ctrl Pts',(4.05688596999994,5.2,-1.20905257600001));
#349033=CARTESIAN_POINT('Ctrl Pts',(4.05688596999994,2.2,-1.20905257600001));
#349034=CARTESIAN_POINT('Ctrl Pts',(4.05557570699994,12.2,-1.20810310800001));
#349035=CARTESIAN_POINT('Ctrl Pts',(4.05557570699994,5.2,-1.20810310800001));
#349036=CARTESIAN_POINT('Ctrl Pts',(4.05557570699994,2.2,-1.20810310800001));
#349037=CARTESIAN_POINT('Ctrl Pts',(4.05426804299994,12.2,-1.20715782500001));
#349038=CARTESIAN_POINT('Ctrl Pts',(4.05426804299994,5.2,-1.20715782500001));
#349039=CARTESIAN_POINT('Ctrl Pts',(4.05426804299994,2.2,-1.20715782500001));
#349040=CARTESIAN_POINT('Ctrl Pts',(4.05296298799994,12.2,-1.20621672300001));
#349041=CARTESIAN_POINT('Ctrl Pts',(4.05296298799994,5.2,-1.20621672300001));
#349042=CARTESIAN_POINT('Ctrl Pts',(4.05296298799994,2.2,-1.20621672300001));
#349043=CARTESIAN_POINT('Ctrl Pts',(4.05166055699994,12.2,-1.20527979800002));
#349044=CARTESIAN_POINT('Ctrl Pts',(4.05166055699994,5.2,-1.20527979800002));
#349045=CARTESIAN_POINT('Ctrl Pts',(4.05166055699994,2.2,-1.20527979800002));
#349046=CARTESIAN_POINT('Ctrl Pts',(4.05036075999995,12.2,-1.20434704800001));
#349047=CARTESIAN_POINT('Ctrl Pts',(4.05036075999995,5.2,-1.20434704800001));
#349048=CARTESIAN_POINT('Ctrl Pts',(4.05036075999995,2.2,-1.20434704800001));
#349049=CARTESIAN_POINT('Ctrl Pts',(4.04906361199994,12.2,-1.20341847100002));
#349050=CARTESIAN_POINT('Ctrl Pts',(4.04906361199994,5.2,-1.20341847100002));
#349051=CARTESIAN_POINT('Ctrl Pts',(4.04906361199994,2.2,-1.20341847100002));
#349052=CARTESIAN_POINT('Ctrl Pts',(4.04776912299995,12.2,-1.20249406100001));
#349053=CARTESIAN_POINT('Ctrl Pts',(4.04776912299995,5.2,-1.20249406100001));
#349054=CARTESIAN_POINT('Ctrl Pts',(4.04776912299995,2.2,-1.20249406100001));
#349055=CARTESIAN_POINT('Ctrl Pts',(4.04647730599994,12.2,-1.20157381900002));
#349056=CARTESIAN_POINT('Ctrl Pts',(4.04647730599994,5.2,-1.20157381900002));
#349057=CARTESIAN_POINT('Ctrl Pts',(4.04647730599994,2.2,-1.20157381900002));
#349058=CARTESIAN_POINT('Ctrl Pts',(4.04518817599994,12.2,-1.20065773800001));
#349059=CARTESIAN_POINT('Ctrl Pts',(4.04518817599994,5.2,-1.20065773800001));
#349060=CARTESIAN_POINT('Ctrl Pts',(4.04518817599994,2.2,-1.20065773800001));
#349061=CARTESIAN_POINT('Ctrl Pts',(4.04390174199994,12.2,-1.19974581800002));
#349062=CARTESIAN_POINT('Ctrl Pts',(4.04390174199994,5.2,-1.19974581800002));
#349063=CARTESIAN_POINT('Ctrl Pts',(4.04390174199994,2.2,-1.19974581800002));
#349064=CARTESIAN_POINT('Ctrl Pts',(4.04261801999994,12.2,-1.19883805300002));
#349065=CARTESIAN_POINT('Ctrl Pts',(4.04261801999994,5.2,-1.19883805300002));
#349066=CARTESIAN_POINT('Ctrl Pts',(4.04261801999994,2.2,-1.19883805300002));
#349067=CARTESIAN_POINT('Ctrl Pts',(4.04133701899995,12.2,-1.19793444300001));
#349068=CARTESIAN_POINT('Ctrl Pts',(4.04133701899995,5.2,-1.19793444300001));
#349069=CARTESIAN_POINT('Ctrl Pts',(4.04133701899995,2.2,-1.19793444300001));
#349070=CARTESIAN_POINT('Ctrl Pts',(4.04005875299995,12.2,-1.19703498200002));
#349071=CARTESIAN_POINT('Ctrl Pts',(4.04005875299995,5.2,-1.19703498200002));
#349072=CARTESIAN_POINT('Ctrl Pts',(4.04005875299995,2.2,-1.19703498200002));
#349073=CARTESIAN_POINT('Ctrl Pts',(4.03878323699994,12.2,-1.19613966800001));
#349074=CARTESIAN_POINT('Ctrl Pts',(4.03878323699994,5.2,-1.19613966800001));
#349075=CARTESIAN_POINT('Ctrl Pts',(4.03878323699994,2.2,-1.19613966800001));
#349076=CARTESIAN_POINT('Ctrl Pts',(4.03751047999994,12.2,-1.19524849800001));
#349077=CARTESIAN_POINT('Ctrl Pts',(4.03751047999994,5.2,-1.19524849800001));
#349078=CARTESIAN_POINT('Ctrl Pts',(4.03751047999994,2.2,-1.19524849800001));
#349079=CARTESIAN_POINT('Ctrl Pts',(4.03624049699994,12.2,-1.19436146800001));
#349080=CARTESIAN_POINT('Ctrl Pts',(4.03624049699994,5.2,-1.19436146800001));
#349081=CARTESIAN_POINT('Ctrl Pts',(4.03624049699994,2.2,-1.19436146800001));
#349082=CARTESIAN_POINT('Ctrl Pts',(4.03497329899994,12.2,-1.19347857500001));
#349083=CARTESIAN_POINT('Ctrl Pts',(4.03497329899994,5.2,-1.19347857500001));
#349084=CARTESIAN_POINT('Ctrl Pts',(4.03497329899994,2.2,-1.19347857500001));
#349085=CARTESIAN_POINT('Ctrl Pts',(4.03370889999994,12.2,-1.19259981700001));
#349086=CARTESIAN_POINT('Ctrl Pts',(4.03370889999994,5.2,-1.19259981700001));
#349087=CARTESIAN_POINT('Ctrl Pts',(4.03370889999994,2.2,-1.19259981700001));
#349088=CARTESIAN_POINT('Ctrl Pts',(4.03244731199994,12.2,-1.19172518900001));
#349089=CARTESIAN_POINT('Ctrl Pts',(4.03244731199994,5.2,-1.19172518900001));
#349090=CARTESIAN_POINT('Ctrl Pts',(4.03244731199994,2.2,-1.19172518900001));
#349091=CARTESIAN_POINT('Ctrl Pts',(4.03118854799995,12.2,-1.19085468800002));
#349092=CARTESIAN_POINT('Ctrl Pts',(4.03118854799995,5.2,-1.19085468800002));
#349093=CARTESIAN_POINT('Ctrl Pts',(4.03118854799995,2.2,-1.19085468800002));
#349094=CARTESIAN_POINT('Ctrl Pts',(4.02993262099994,12.2,-1.18998831000001));
#349095=CARTESIAN_POINT('Ctrl Pts',(4.02993262099994,5.2,-1.18998831000001));
#349096=CARTESIAN_POINT('Ctrl Pts',(4.02993262099994,2.2,-1.18998831000001));
#349097=CARTESIAN_POINT('Ctrl Pts',(4.02867954299994,12.2,-1.18912605400002));
#349098=CARTESIAN_POINT('Ctrl Pts',(4.02867954299994,5.2,-1.18912605400002));
#349099=CARTESIAN_POINT('Ctrl Pts',(4.02867954299994,2.2,-1.18912605400002));
#349100=CARTESIAN_POINT('Ctrl Pts',(4.02742932799994,12.2,-1.18826791300001));
#349101=CARTESIAN_POINT('Ctrl Pts',(4.02742932799994,5.2,-1.18826791300001));
#349102=CARTESIAN_POINT('Ctrl Pts',(4.02742932799994,2.2,-1.18826791300001));
#349103=CARTESIAN_POINT('Ctrl Pts',(4.02618198699995,12.2,-1.18741388700002));
#349104=CARTESIAN_POINT('Ctrl Pts',(4.02618198699995,5.2,-1.18741388700002));
#349105=CARTESIAN_POINT('Ctrl Pts',(4.02618198699995,2.2,-1.18741388700002));
#349106=CARTESIAN_POINT('Ctrl Pts',(4.02493753399995,12.2,-1.18656397000001));
#349107=CARTESIAN_POINT('Ctrl Pts',(4.02493753399995,5.2,-1.18656397000001));
#349108=CARTESIAN_POINT('Ctrl Pts',(4.02493753399995,2.2,-1.18656397000001));
#349109=CARTESIAN_POINT('Ctrl Pts',(4.02369598199994,12.2,-1.18571816200001));
#349110=CARTESIAN_POINT('Ctrl Pts',(4.02369598199994,5.2,-1.18571816200001));
#349111=CARTESIAN_POINT('Ctrl Pts',(4.02369598199994,2.2,-1.18571816200001));
#349112=CARTESIAN_POINT('Ctrl Pts',(4.02245734399994,12.2,-1.18487645500001));
#349113=CARTESIAN_POINT('Ctrl Pts',(4.02245734399994,5.2,-1.18487645500001));
#349114=CARTESIAN_POINT('Ctrl Pts',(4.02245734399994,2.2,-1.18487645500001));
#349115=CARTESIAN_POINT('Ctrl Pts',(4.02122163199994,12.2,-1.18403884800002));
#349116=CARTESIAN_POINT('Ctrl Pts',(4.02122163199994,5.2,-1.18403884800002));
#349117=CARTESIAN_POINT('Ctrl Pts',(4.02122163199994,2.2,-1.18403884800002));
#349118=CARTESIAN_POINT('Ctrl Pts',(4.01998885999994,12.2,-1.18320533800001));
#349119=CARTESIAN_POINT('Ctrl Pts',(4.01998885999994,5.2,-1.18320533800001));
#349120=CARTESIAN_POINT('Ctrl Pts',(4.01998885999994,2.2,-1.18320533800001));
#349121=CARTESIAN_POINT('Ctrl Pts',(4.01875903999994,12.2,-1.18237591900002));
#349122=CARTESIAN_POINT('Ctrl Pts',(4.01875903999994,5.2,-1.18237591900002));
#349123=CARTESIAN_POINT('Ctrl Pts',(4.01875903999994,2.2,-1.18237591900002));
#349124=CARTESIAN_POINT('Ctrl Pts',(4.01753218399994,12.2,-1.18155058800001));
#349125=CARTESIAN_POINT('Ctrl Pts',(4.01753218399994,5.2,-1.18155058800001));
#349126=CARTESIAN_POINT('Ctrl Pts',(4.01753218399994,2.2,-1.18155058800001));
#349127=CARTESIAN_POINT('Ctrl Pts',(4.01630830799994,12.2,-1.18072934400002));
#349128=CARTESIAN_POINT('Ctrl Pts',(4.01630830799994,5.2,-1.18072934400002));
#349129=CARTESIAN_POINT('Ctrl Pts',(4.01630830799994,2.2,-1.18072934400002));
#349130=CARTESIAN_POINT('Ctrl Pts',(4.01508742299994,12.2,-1.17991218100002));
#349131=CARTESIAN_POINT('Ctrl Pts',(4.01508742299994,5.2,-1.17991218100002));
#349132=CARTESIAN_POINT('Ctrl Pts',(4.01508742299994,2.2,-1.17991218100002));
#349133=CARTESIAN_POINT('Ctrl Pts',(4.01386954199995,12.2,-1.17909909600002));
#349134=CARTESIAN_POINT('Ctrl Pts',(4.01386954199995,5.2,-1.17909909600002));
#349135=CARTESIAN_POINT('Ctrl Pts',(4.01386954199995,2.2,-1.17909909600002));
#349136=CARTESIAN_POINT('Ctrl Pts',(4.01265467899994,12.2,-1.17829008400001));
#349137=CARTESIAN_POINT('Ctrl Pts',(4.01265467899994,5.2,-1.17829008400001));
#349138=CARTESIAN_POINT('Ctrl Pts',(4.01265467899994,2.2,-1.17829008400001));
#349139=CARTESIAN_POINT('Ctrl Pts',(4.01144284499994,12.2,-1.17748514300001));
#349140=CARTESIAN_POINT('Ctrl Pts',(4.01144284499994,5.2,-1.17748514300001));
#349141=CARTESIAN_POINT('Ctrl Pts',(4.01144284499994,2.2,-1.17748514300001));
#349142=CARTESIAN_POINT('Ctrl Pts',(4.01023405599994,12.2,-1.17668426800002));
#349143=CARTESIAN_POINT('Ctrl Pts',(4.01023405599994,5.2,-1.17668426800002));
#349144=CARTESIAN_POINT('Ctrl Pts',(4.01023405599994,2.2,-1.17668426800002));
#349145=CARTESIAN_POINT('Ctrl Pts',(4.00902832299994,12.2,-1.17588745700001));
#349146=CARTESIAN_POINT('Ctrl Pts',(4.00902832299994,5.2,-1.17588745700001));
#349147=CARTESIAN_POINT('Ctrl Pts',(4.00902832299994,2.2,-1.17588745700001));
#349148=CARTESIAN_POINT('Ctrl Pts',(4.00782565899994,12.2,-1.17509470400002));
#349149=CARTESIAN_POINT('Ctrl Pts',(4.00782565899994,5.2,-1.17509470400002));
#349150=CARTESIAN_POINT('Ctrl Pts',(4.00782565899994,2.2,-1.17509470400002));
#349151=CARTESIAN_POINT('Ctrl Pts',(4.00662607899995,12.2,-1.17430600600001));
#349152=CARTESIAN_POINT('Ctrl Pts',(4.00662607899995,5.2,-1.17430600600001));
#349153=CARTESIAN_POINT('Ctrl Pts',(4.00662607899995,2.2,-1.17430600600001));
#349154=CARTESIAN_POINT('Ctrl Pts',(4.00542959399994,12.2,-1.17352136000001));
#349155=CARTESIAN_POINT('Ctrl Pts',(4.00542959399994,5.2,-1.17352136000001));
#349156=CARTESIAN_POINT('Ctrl Pts',(4.00542959399994,2.2,-1.17352136000001));
#349157=CARTESIAN_POINT('Ctrl Pts',(4.00423621899994,12.2,-1.17274076200002));
#349158=CARTESIAN_POINT('Ctrl Pts',(4.00423621899994,5.2,-1.17274076200002));
#349159=CARTESIAN_POINT('Ctrl Pts',(4.00423621899994,2.2,-1.17274076200002));
#349160=CARTESIAN_POINT('Ctrl Pts',(4.00304596699994,12.2,-1.17196420600001));
#349161=CARTESIAN_POINT('Ctrl Pts',(4.00304596699994,5.2,-1.17196420600001));
#349162=CARTESIAN_POINT('Ctrl Pts',(4.00304596699994,2.2,-1.17196420600001));
#349163=CARTESIAN_POINT('Ctrl Pts',(4.00185884899994,12.2,-1.17119169100001));
#349164=CARTESIAN_POINT('Ctrl Pts',(4.00185884899994,5.2,-1.17119169100001));
#349165=CARTESIAN_POINT('Ctrl Pts',(4.00185884899994,2.2,-1.17119169100001));
#349166=CARTESIAN_POINT('Ctrl Pts',(4.00067488099995,12.2,-1.17042321100001));
#349167=CARTESIAN_POINT('Ctrl Pts',(4.00067488099995,5.2,-1.17042321100001));
#349168=CARTESIAN_POINT('Ctrl Pts',(4.00067488099995,2.2,-1.17042321100001));
#349169=CARTESIAN_POINT('Ctrl Pts',(3.99949407599994,12.2,-1.16965876200001));
#349170=CARTESIAN_POINT('Ctrl Pts',(3.99949407599994,5.2,-1.16965876200001));
#349171=CARTESIAN_POINT('Ctrl Pts',(3.99949407599994,2.2,-1.16965876200001));
#349172=CARTESIAN_POINT('Ctrl Pts',(3.99831644599994,12.2,-1.16889834000002));
#349173=CARTESIAN_POINT('Ctrl Pts',(3.99831644599994,5.2,-1.16889834000002));
#349174=CARTESIAN_POINT('Ctrl Pts',(3.99831644599994,2.2,-1.16889834000002));
#349175=CARTESIAN_POINT('Ctrl Pts',(3.99714200399994,12.2,-1.16814194300002));
#349176=CARTESIAN_POINT('Ctrl Pts',(3.99714200399994,5.2,-1.16814194300002));
#349177=CARTESIAN_POINT('Ctrl Pts',(3.99714200399994,2.2,-1.16814194300002));
#349178=CARTESIAN_POINT('Ctrl Pts',(3.99597076499994,12.2,-1.16738956500001));
#349179=CARTESIAN_POINT('Ctrl Pts',(3.99597076499994,5.2,-1.16738956500001));
#349180=CARTESIAN_POINT('Ctrl Pts',(3.99597076499994,2.2,-1.16738956500001));
#349181=CARTESIAN_POINT('Ctrl Pts',(3.99480274199994,12.2,-1.16664120200001));
#349182=CARTESIAN_POINT('Ctrl Pts',(3.99480274199994,5.2,-1.16664120200001));
#349183=CARTESIAN_POINT('Ctrl Pts',(3.99480274199994,2.2,-1.16664120200001));
#349184=CARTESIAN_POINT('Ctrl Pts',(3.99363794799994,12.2,-1.16589685100001));
#349185=CARTESIAN_POINT('Ctrl Pts',(3.99363794799994,5.2,-1.16589685100001));
#349186=CARTESIAN_POINT('Ctrl Pts',(3.99363794799994,2.2,-1.16589685100001));
#349187=CARTESIAN_POINT('Ctrl Pts',(3.99247639599994,12.2,-1.16515650600002));
#349188=CARTESIAN_POINT('Ctrl Pts',(3.99247639599994,5.2,-1.16515650600002));
#349189=CARTESIAN_POINT('Ctrl Pts',(3.99247639599994,2.2,-1.16515650600002));
#349190=CARTESIAN_POINT('Ctrl Pts',(3.99131809999994,12.2,-1.16442016400002));
#349191=CARTESIAN_POINT('Ctrl Pts',(3.99131809999994,5.2,-1.16442016400002));
#349192=CARTESIAN_POINT('Ctrl Pts',(3.99131809999994,2.2,-1.16442016400002));
#349193=CARTESIAN_POINT('Ctrl Pts',(3.99016307399994,12.2,-1.16368782100002));
#349194=CARTESIAN_POINT('Ctrl Pts',(3.99016307399994,5.2,-1.16368782100002));
#349195=CARTESIAN_POINT('Ctrl Pts',(3.99016307399994,2.2,-1.16368782100002));
#349196=CARTESIAN_POINT('Ctrl Pts',(3.98901132899994,12.2,-1.16295947300001));
#349197=CARTESIAN_POINT('Ctrl Pts',(3.98901132899994,5.2,-1.16295947300001));
#349198=CARTESIAN_POINT('Ctrl Pts',(3.98901132899994,2.2,-1.16295947300001));
#349199=CARTESIAN_POINT('Ctrl Pts',(3.98786288299994,12.2,-1.16223511500001));
#349200=CARTESIAN_POINT('Ctrl Pts',(3.98786288299994,5.2,-1.16223511500001));
#349201=CARTESIAN_POINT('Ctrl Pts',(3.98786288299994,2.2,-1.16223511500001));
#349202=CARTESIAN_POINT('Ctrl Pts',(3.98671774499994,12.2,-1.16151474200001));
#349203=CARTESIAN_POINT('Ctrl Pts',(3.98671774499994,5.2,-1.16151474200001));
#349204=CARTESIAN_POINT('Ctrl Pts',(3.98671774499994,2.2,-1.16151474200001));
#349205=CARTESIAN_POINT('Ctrl Pts',(3.98557593099994,12.2,-1.16079835100001));
#349206=CARTESIAN_POINT('Ctrl Pts',(3.98557593099994,5.2,-1.16079835100001));
#349207=CARTESIAN_POINT('Ctrl Pts',(3.98557593099994,2.2,-1.16079835100001));
#349208=CARTESIAN_POINT('Ctrl Pts',(3.98443745399994,12.2,-1.16008593800002));
#349209=CARTESIAN_POINT('Ctrl Pts',(3.98443745399994,5.2,-1.16008593800002));
#349210=CARTESIAN_POINT('Ctrl Pts',(3.98443745399994,2.2,-1.16008593800002));
#349211=CARTESIAN_POINT('Ctrl Pts',(3.98330232899994,12.2,-1.15937749700001));
#349212=CARTESIAN_POINT('Ctrl Pts',(3.98330232899994,5.2,-1.15937749700001));
#349213=CARTESIAN_POINT('Ctrl Pts',(3.98330232899994,2.2,-1.15937749700001));
#349214=CARTESIAN_POINT('Ctrl Pts',(3.98217056699994,12.2,-1.15867302500002));
#349215=CARTESIAN_POINT('Ctrl Pts',(3.98217056699994,5.2,-1.15867302500002));
#349216=CARTESIAN_POINT('Ctrl Pts',(3.98217056699994,2.2,-1.15867302500002));
#349217=CARTESIAN_POINT('Ctrl Pts',(3.98104218299994,12.2,-1.15797251600001));
#349218=CARTESIAN_POINT('Ctrl Pts',(3.98104218299994,5.2,-1.15797251600001));
#349219=CARTESIAN_POINT('Ctrl Pts',(3.98104218299994,2.2,-1.15797251600001));
#349220=CARTESIAN_POINT('Ctrl Pts',(3.97991719099994,12.2,-1.15727596800001));
#349221=CARTESIAN_POINT('Ctrl Pts',(3.97991719099994,5.2,-1.15727596800001));
#349222=CARTESIAN_POINT('Ctrl Pts',(3.97991719099994,2.2,-1.15727596800001));
#349223=CARTESIAN_POINT('Ctrl Pts',(3.97879560399994,12.2,-1.15658337500002));
#349224=CARTESIAN_POINT('Ctrl Pts',(3.97879560399994,5.2,-1.15658337500002));
#349225=CARTESIAN_POINT('Ctrl Pts',(3.97879560399994,2.2,-1.15658337500002));
#349226=CARTESIAN_POINT('Ctrl Pts',(3.97767743699994,12.2,-1.15589473300002));
#349227=CARTESIAN_POINT('Ctrl Pts',(3.97767743699994,5.2,-1.15589473300002));
#349228=CARTESIAN_POINT('Ctrl Pts',(3.97767743699994,2.2,-1.15589473300002));
#349229=CARTESIAN_POINT('Ctrl Pts',(3.97656270199994,12.2,-1.15521003600001));
#349230=CARTESIAN_POINT('Ctrl Pts',(3.97656270199994,5.2,-1.15521003600001));
#349231=CARTESIAN_POINT('Ctrl Pts',(3.97656270199994,2.2,-1.15521003600001));
#349232=CARTESIAN_POINT('Ctrl Pts',(3.97545141399994,12.2,-1.15452928100002));
#349233=CARTESIAN_POINT('Ctrl Pts',(3.97545141399994,5.2,-1.15452928100002));
#349234=CARTESIAN_POINT('Ctrl Pts',(3.97545141399994,2.2,-1.15452928100002));
#349235=CARTESIAN_POINT('Ctrl Pts',(3.97434358599994,12.2,-1.15385246300002));
#349236=CARTESIAN_POINT('Ctrl Pts',(3.97434358599994,5.2,-1.15385246300002));
#349237=CARTESIAN_POINT('Ctrl Pts',(3.97434358599994,2.2,-1.15385246300002));
#349238=CARTESIAN_POINT('Ctrl Pts',(3.97323923299994,12.2,-1.15317957800002));
#349239=CARTESIAN_POINT('Ctrl Pts',(3.97323923299994,5.2,-1.15317957800002));
#349240=CARTESIAN_POINT('Ctrl Pts',(3.97323923299994,2.2,-1.15317957800002));
#349241=CARTESIAN_POINT('Ctrl Pts',(3.97213836699994,12.2,-1.15251062000001));
#349242=CARTESIAN_POINT('Ctrl Pts',(3.97213836699994,5.2,-1.15251062000001));
#349243=CARTESIAN_POINT('Ctrl Pts',(3.97213836699994,2.2,-1.15251062000001));
#349244=CARTESIAN_POINT('Ctrl Pts',(3.97104100499994,12.2,-1.15184558400002));
#349245=CARTESIAN_POINT('Ctrl Pts',(3.97104100499994,5.2,-1.15184558400002));
#349246=CARTESIAN_POINT('Ctrl Pts',(3.97104100499994,2.2,-1.15184558400002));
#349247=CARTESIAN_POINT('Ctrl Pts',(3.96994715599994,12.2,-1.15118446800002));
#349248=CARTESIAN_POINT('Ctrl Pts',(3.96994715599994,5.2,-1.15118446800002));
#349249=CARTESIAN_POINT('Ctrl Pts',(3.96994715599994,2.2,-1.15118446800002));
#349250=CARTESIAN_POINT('Ctrl Pts',(3.96885683999994,12.2,-1.15052726600001));
#349251=CARTESIAN_POINT('Ctrl Pts',(3.96885683999994,5.2,-1.15052726600001));
#349252=CARTESIAN_POINT('Ctrl Pts',(3.96885683999994,2.2,-1.15052726600001));
#349253=CARTESIAN_POINT('Ctrl Pts',(3.96777006599994,12.2,-1.14987397200002));
#349254=CARTESIAN_POINT('Ctrl Pts',(3.96777006599994,5.2,-1.14987397200002));
#349255=CARTESIAN_POINT('Ctrl Pts',(3.96777006599994,2.2,-1.14987397200002));
#349256=CARTESIAN_POINT('Ctrl Pts',(3.96668684899994,12.2,-1.14922458200001));
#349257=CARTESIAN_POINT('Ctrl Pts',(3.96668684899994,5.2,-1.14922458200001));
#349258=CARTESIAN_POINT('Ctrl Pts',(3.96668684899994,2.2,-1.14922458200001));
#349259=CARTESIAN_POINT('Ctrl Pts',(3.96560720599994,12.2,-1.14857909000001));
#349260=CARTESIAN_POINT('Ctrl Pts',(3.96560720599994,5.2,-1.14857909000001));
#349261=CARTESIAN_POINT('Ctrl Pts',(3.96560720599994,2.2,-1.14857909000001));
#349262=CARTESIAN_POINT('Ctrl Pts',(3.96453114699994,12.2,-1.14793749400001));
#349263=CARTESIAN_POINT('Ctrl Pts',(3.96453114699994,5.2,-1.14793749400001));
#349264=CARTESIAN_POINT('Ctrl Pts',(3.96453114699994,2.2,-1.14793749400001));
#349265=CARTESIAN_POINT('Ctrl Pts',(3.96345868799994,12.2,-1.14729978700002));
#349266=CARTESIAN_POINT('Ctrl Pts',(3.96345868799994,5.2,-1.14729978700002));
#349267=CARTESIAN_POINT('Ctrl Pts',(3.96345868799994,2.2,-1.14729978700002));
#349268=CARTESIAN_POINT('Ctrl Pts',(3.96238984399994,12.2,-1.14666596600001));
#349269=CARTESIAN_POINT('Ctrl Pts',(3.96238984399994,5.2,-1.14666596600001));
#349270=CARTESIAN_POINT('Ctrl Pts',(3.96238984399994,2.2,-1.14666596600001));
#349271=CARTESIAN_POINT('Ctrl Pts',(3.96132462599994,12.2,-1.14603602300001));
#349272=CARTESIAN_POINT('Ctrl Pts',(3.96132462599994,5.2,-1.14603602300001));
#349273=CARTESIAN_POINT('Ctrl Pts',(3.96132462599994,2.2,-1.14603602300001));
#349274=CARTESIAN_POINT('Ctrl Pts',(3.96026305099995,12.2,-1.14540995500001));
#349275=CARTESIAN_POINT('Ctrl Pts',(3.96026305099995,5.2,-1.14540995500001));
#349276=CARTESIAN_POINT('Ctrl Pts',(3.96026305099995,2.2,-1.14540995500001));
#349277=CARTESIAN_POINT('Ctrl Pts',(3.95920513399994,12.2,-1.14478775700002));
#349278=CARTESIAN_POINT('Ctrl Pts',(3.95920513399994,5.2,-1.14478775700002));
#349279=CARTESIAN_POINT('Ctrl Pts',(3.95920513399994,2.2,-1.14478775700002));
#349280=CARTESIAN_POINT('Ctrl Pts',(3.95815088599994,12.2,-1.14416942400001));
#349281=CARTESIAN_POINT('Ctrl Pts',(3.95815088599994,5.2,-1.14416942400001));
#349282=CARTESIAN_POINT('Ctrl Pts',(3.95815088599994,2.2,-1.14416942400001));
#349283=CARTESIAN_POINT('Ctrl Pts',(3.95710032199994,12.2,-1.14355494900002));
#349284=CARTESIAN_POINT('Ctrl Pts',(3.95710032199994,5.2,-1.14355494900002));
#349285=CARTESIAN_POINT('Ctrl Pts',(3.95710032199994,2.2,-1.14355494900002));
#349286=CARTESIAN_POINT('Ctrl Pts',(3.95605345899994,12.2,-1.14294433000001));
#349287=CARTESIAN_POINT('Ctrl Pts',(3.95605345899994,5.2,-1.14294433000001));
#349288=CARTESIAN_POINT('Ctrl Pts',(3.95605345899994,2.2,-1.14294433000001));
#349289=CARTESIAN_POINT('Ctrl Pts',(3.95501030799994,12.2,-1.14233756100001));
#349290=CARTESIAN_POINT('Ctrl Pts',(3.95501030799994,5.2,-1.14233756100001));
#349291=CARTESIAN_POINT('Ctrl Pts',(3.95501030799994,2.2,-1.14233756100001));
#349292=CARTESIAN_POINT('Ctrl Pts',(3.95397088399994,12.2,-1.14173463500002));
#349293=CARTESIAN_POINT('Ctrl Pts',(3.95397088399994,5.2,-1.14173463500002));
#349294=CARTESIAN_POINT('Ctrl Pts',(3.95397088399994,2.2,-1.14173463500002));
#349295=CARTESIAN_POINT('Ctrl Pts',(3.95293520099994,12.2,-1.14113554900001));
#349296=CARTESIAN_POINT('Ctrl Pts',(3.95293520099994,5.2,-1.14113554900001));
#349297=CARTESIAN_POINT('Ctrl Pts',(3.95293520099994,2.2,-1.14113554900001));
#349298=CARTESIAN_POINT('Ctrl Pts',(3.95190327599994,12.2,-1.14054029600001));
#349299=CARTESIAN_POINT('Ctrl Pts',(3.95190327599994,5.2,-1.14054029600001));
#349300=CARTESIAN_POINT('Ctrl Pts',(3.95190327599994,2.2,-1.14054029600001));
#349301=CARTESIAN_POINT('Ctrl Pts',(3.95087511999995,12.2,-1.13994887300001));
#349302=CARTESIAN_POINT('Ctrl Pts',(3.95087511999995,5.2,-1.13994887300001));
#349303=CARTESIAN_POINT('Ctrl Pts',(3.95087511999995,2.2,-1.13994887300001));
#349304=CARTESIAN_POINT('Ctrl Pts',(3.94985074899994,12.2,-1.13936127100001));
#349305=CARTESIAN_POINT('Ctrl Pts',(3.94985074899994,5.2,-1.13936127100001));
#349306=CARTESIAN_POINT('Ctrl Pts',(3.94985074899994,2.2,-1.13936127100001));
#349307=CARTESIAN_POINT('Ctrl Pts',(3.94883017799994,12.2,-1.13877749000002));
#349308=CARTESIAN_POINT('Ctrl Pts',(3.94883017799994,5.2,-1.13877749000002));
#349309=CARTESIAN_POINT('Ctrl Pts',(3.94883017799994,2.2,-1.13877749000002));
#349310=CARTESIAN_POINT('Ctrl Pts',(3.94781342099995,12.2,-1.13819752000001));
#349311=CARTESIAN_POINT('Ctrl Pts',(3.94781342099995,5.2,-1.13819752000001));
#349312=CARTESIAN_POINT('Ctrl Pts',(3.94781342099995,2.2,-1.13819752000001));
#349313=CARTESIAN_POINT('Ctrl Pts',(3.94680049099994,12.2,-1.13762135800001));
#349314=CARTESIAN_POINT('Ctrl Pts',(3.94680049099994,5.2,-1.13762135800001));
#349315=CARTESIAN_POINT('Ctrl Pts',(3.94680049099994,2.2,-1.13762135800001));
#349316=CARTESIAN_POINT('Ctrl Pts',(3.94579140499994,12.2,-1.13704899800001));
#349317=CARTESIAN_POINT('Ctrl Pts',(3.94579140499994,5.2,-1.13704899800001));
#349318=CARTESIAN_POINT('Ctrl Pts',(3.94579140499994,2.2,-1.13704899800001));
#349319=CARTESIAN_POINT('Ctrl Pts',(3.94478617499994,12.2,-1.13648043400001));
#349320=CARTESIAN_POINT('Ctrl Pts',(3.94478617499994,5.2,-1.13648043400001));
#349321=CARTESIAN_POINT('Ctrl Pts',(3.94478617499994,2.2,-1.13648043400001));
#349322=CARTESIAN_POINT('Ctrl Pts',(3.94378481699994,12.2,-1.13591566200002));
#349323=CARTESIAN_POINT('Ctrl Pts',(3.94378481699994,5.2,-1.13591566200002));
#349324=CARTESIAN_POINT('Ctrl Pts',(3.94378481699994,2.2,-1.13591566200002));
#349325=CARTESIAN_POINT('Ctrl Pts',(3.94278734499994,12.2,-1.13535467600002));
#349326=CARTESIAN_POINT('Ctrl Pts',(3.94278734499994,5.2,-1.13535467600002));
#349327=CARTESIAN_POINT('Ctrl Pts',(3.94278734499994,2.2,-1.13535467600002));
#349328=CARTESIAN_POINT('Ctrl Pts',(3.94179377499994,12.2,-1.13479746900001));
#349329=CARTESIAN_POINT('Ctrl Pts',(3.94179377499994,5.2,-1.13479746900001));
#349330=CARTESIAN_POINT('Ctrl Pts',(3.94179377499994,2.2,-1.13479746900001));
#349331=CARTESIAN_POINT('Ctrl Pts',(3.94080411899994,12.2,-1.13424403700002));
#349332=CARTESIAN_POINT('Ctrl Pts',(3.94080411899994,5.2,-1.13424403700002));
#349333=CARTESIAN_POINT('Ctrl Pts',(3.94080411899994,2.2,-1.13424403700002));
#349334=CARTESIAN_POINT('Ctrl Pts',(3.93981839399994,12.2,-1.13369437400001));
#349335=CARTESIAN_POINT('Ctrl Pts',(3.93981839399994,5.2,-1.13369437400001));
#349336=CARTESIAN_POINT('Ctrl Pts',(3.93981839399994,2.2,-1.13369437400001));
#349337=CARTESIAN_POINT('Ctrl Pts',(3.93883661399994,12.2,-1.13314847400002));
#349338=CARTESIAN_POINT('Ctrl Pts',(3.93883661399994,5.2,-1.13314847400002));
#349339=CARTESIAN_POINT('Ctrl Pts',(3.93883661399994,2.2,-1.13314847400002));
#349340=CARTESIAN_POINT('Ctrl Pts',(3.93785879399994,12.2,-1.13260633200001));
#349341=CARTESIAN_POINT('Ctrl Pts',(3.93785879399994,5.2,-1.13260633200001));
#349342=CARTESIAN_POINT('Ctrl Pts',(3.93785879399994,2.2,-1.13260633200001));
#349343=CARTESIAN_POINT('Ctrl Pts',(3.93688494699994,12.2,-1.13206794200002));
#349344=CARTESIAN_POINT('Ctrl Pts',(3.93688494699994,5.2,-1.13206794200002));
#349345=CARTESIAN_POINT('Ctrl Pts',(3.93688494699994,2.2,-1.13206794200002));
#349346=CARTESIAN_POINT('Ctrl Pts',(3.93591508999994,12.2,-1.13153329900001));
#349347=CARTESIAN_POINT('Ctrl Pts',(3.93591508999994,5.2,-1.13153329900001));
#349348=CARTESIAN_POINT('Ctrl Pts',(3.93591508999994,2.2,-1.13153329900001));
#349349=CARTESIAN_POINT('Ctrl Pts',(3.93494923699994,12.2,-1.13100239600001));
#349350=CARTESIAN_POINT('Ctrl Pts',(3.93494923699994,5.2,-1.13100239600001));
#349351=CARTESIAN_POINT('Ctrl Pts',(3.93494923699994,2.2,-1.13100239600001));
#349352=CARTESIAN_POINT('Ctrl Pts',(3.93398740299994,12.2,-1.13047522900001));
#349353=CARTESIAN_POINT('Ctrl Pts',(3.93398740299994,5.2,-1.13047522900001));
#349354=CARTESIAN_POINT('Ctrl Pts',(3.93398740299994,2.2,-1.13047522900001));
#349355=CARTESIAN_POINT('Ctrl Pts',(3.93302960199994,12.2,-1.12995179000002));
#349356=CARTESIAN_POINT('Ctrl Pts',(3.93302960199994,5.2,-1.12995179000002));
#349357=CARTESIAN_POINT('Ctrl Pts',(3.93302960199994,2.2,-1.12995179000002));
#349358=CARTESIAN_POINT('Ctrl Pts',(3.93207584999994,12.2,-1.12943207300002));
#349359=CARTESIAN_POINT('Ctrl Pts',(3.93207584999994,5.2,-1.12943207300002));
#349360=CARTESIAN_POINT('Ctrl Pts',(3.93207584999994,2.2,-1.12943207300002));
#349361=CARTESIAN_POINT('Ctrl Pts',(3.93112616099994,12.2,-1.12891607400002));
#349362=CARTESIAN_POINT('Ctrl Pts',(3.93112616099994,5.2,-1.12891607400002));
#349363=CARTESIAN_POINT('Ctrl Pts',(3.93112616099994,2.2,-1.12891607400002));
#349364=CARTESIAN_POINT('Ctrl Pts',(3.93018054999994,12.2,-1.12840378800001));
#349365=CARTESIAN_POINT('Ctrl Pts',(3.93018054999994,5.2,-1.12840378800001));
#349366=CARTESIAN_POINT('Ctrl Pts',(3.93018054999994,2.2,-1.12840378800001));
#349367=CARTESIAN_POINT('Ctrl Pts',(3.92923903199994,12.2,-1.12789520600002));
#349368=CARTESIAN_POINT('Ctrl Pts',(3.92923903199994,5.2,-1.12789520600002));
#349369=CARTESIAN_POINT('Ctrl Pts',(3.92923903199994,2.2,-1.12789520600002));
#349370=CARTESIAN_POINT('Ctrl Pts',(3.92830162399994,12.2,-1.12739032400002));
#349371=CARTESIAN_POINT('Ctrl Pts',(3.92830162399994,5.2,-1.12739032400002));
#349372=CARTESIAN_POINT('Ctrl Pts',(3.92830162399994,2.2,-1.12739032400002));
#349373=CARTESIAN_POINT('Ctrl Pts',(3.92736833799994,12.2,-1.12688913500001));
#349374=CARTESIAN_POINT('Ctrl Pts',(3.92736833799994,5.2,-1.12688913500001));
#349375=CARTESIAN_POINT('Ctrl Pts',(3.92736833799994,2.2,-1.12688913500001));
#349376=CARTESIAN_POINT('Ctrl Pts',(3.92643918999994,12.2,-1.12639163300001));
#349377=CARTESIAN_POINT('Ctrl Pts',(3.92643918999994,5.2,-1.12639163300001));
#349378=CARTESIAN_POINT('Ctrl Pts',(3.92643918999994,2.2,-1.12639163300001));
#349379=CARTESIAN_POINT('Ctrl Pts',(3.92551419599994,12.2,-1.12589781300001));
#349380=CARTESIAN_POINT('Ctrl Pts',(3.92551419599994,5.2,-1.12589781300001));
#349381=CARTESIAN_POINT('Ctrl Pts',(3.92551419599994,2.2,-1.12589781300001));
#349382=CARTESIAN_POINT('Ctrl Pts',(3.92459337099994,12.2,-1.12540766800001));
#349383=CARTESIAN_POINT('Ctrl Pts',(3.92459337099994,5.2,-1.12540766800001));
#349384=CARTESIAN_POINT('Ctrl Pts',(3.92459337099994,2.2,-1.12540766800001));
#349385=CARTESIAN_POINT('Ctrl Pts',(3.92367672899994,12.2,-1.12492119200001));
#349386=CARTESIAN_POINT('Ctrl Pts',(3.92367672899994,5.2,-1.12492119200001));
#349387=CARTESIAN_POINT('Ctrl Pts',(3.92367672899994,2.2,-1.12492119200001));
#349388=CARTESIAN_POINT('Ctrl Pts',(3.92276428599994,12.2,-1.12443837900001));
#349389=CARTESIAN_POINT('Ctrl Pts',(3.92276428599994,5.2,-1.12443837900001));
#349390=CARTESIAN_POINT('Ctrl Pts',(3.92276428599994,2.2,-1.12443837900001));
#349391=CARTESIAN_POINT('Ctrl Pts',(3.92185605799994,12.2,-1.12395922300002));
#349392=CARTESIAN_POINT('Ctrl Pts',(3.92185605799994,5.2,-1.12395922300002));
#349393=CARTESIAN_POINT('Ctrl Pts',(3.92185605799994,2.2,-1.12395922300002));
#349394=CARTESIAN_POINT('Ctrl Pts',(3.92095205899994,12.2,-1.12348371700001));
#349395=CARTESIAN_POINT('Ctrl Pts',(3.92095205899994,5.2,-1.12348371700001));
#349396=CARTESIAN_POINT('Ctrl Pts',(3.92095205899994,2.2,-1.12348371700001));
#349397=CARTESIAN_POINT('Ctrl Pts',(3.92005230299994,12.2,-1.12301185500002));
#349398=CARTESIAN_POINT('Ctrl Pts',(3.92005230299994,5.2,-1.12301185500002));
#349399=CARTESIAN_POINT('Ctrl Pts',(3.92005230299994,2.2,-1.12301185500002));
#349400=CARTESIAN_POINT('Ctrl Pts',(3.91915680899994,12.2,-1.12254363000002));
#349401=CARTESIAN_POINT('Ctrl Pts',(3.91915680899994,5.2,-1.12254363000002));
#349402=CARTESIAN_POINT('Ctrl Pts',(3.91915680899994,2.2,-1.12254363000002));
#349403=CARTESIAN_POINT('Ctrl Pts',(3.91826558899994,12.2,-1.12207903800002));
#349404=CARTESIAN_POINT('Ctrl Pts',(3.91826558899994,5.2,-1.12207903800002));
#349405=CARTESIAN_POINT('Ctrl Pts',(3.91826558899994,2.2,-1.12207903800002));
#349406=CARTESIAN_POINT('Ctrl Pts',(3.91737865999994,12.2,-1.12161807000001));
#349407=CARTESIAN_POINT('Ctrl Pts',(3.91737865999994,5.2,-1.12161807000001));
#349408=CARTESIAN_POINT('Ctrl Pts',(3.91737865999994,2.2,-1.12161807000001));
#349409=CARTESIAN_POINT('Ctrl Pts',(3.91649603699994,12.2,-1.12116072100001));
#349410=CARTESIAN_POINT('Ctrl Pts',(3.91649603699994,5.2,-1.12116072100001));
#349411=CARTESIAN_POINT('Ctrl Pts',(3.91649603699994,2.2,-1.12116072100001));
#349412=CARTESIAN_POINT('Ctrl Pts',(3.91561773599994,12.2,-1.12070698400002));
#349413=CARTESIAN_POINT('Ctrl Pts',(3.91561773599994,5.2,-1.12070698400002));
#349414=CARTESIAN_POINT('Ctrl Pts',(3.91561773599994,2.2,-1.12070698400002));
#349415=CARTESIAN_POINT('Ctrl Pts',(3.91474376999994,12.2,-1.12025685300001));
#349416=CARTESIAN_POINT('Ctrl Pts',(3.91474376999994,5.2,-1.12025685300001));
#349417=CARTESIAN_POINT('Ctrl Pts',(3.91474376999994,2.2,-1.12025685300001));
#349418=CARTESIAN_POINT('Ctrl Pts',(3.91387415799994,12.2,-1.11981032100001));
#349419=CARTESIAN_POINT('Ctrl Pts',(3.91387415799994,5.2,-1.11981032100001));
#349420=CARTESIAN_POINT('Ctrl Pts',(3.91387415799994,2.2,-1.11981032100001));
#349421=CARTESIAN_POINT('Ctrl Pts',(3.91300891299994,12.2,-1.11936738000002));
#349422=CARTESIAN_POINT('Ctrl Pts',(3.91300891299994,5.2,-1.11936738000002));
#349423=CARTESIAN_POINT('Ctrl Pts',(3.91300891299994,2.2,-1.11936738000002));
#349424=CARTESIAN_POINT('Ctrl Pts',(3.91214805199994,12.2,-1.11892802700002));
#349425=CARTESIAN_POINT('Ctrl Pts',(3.91214805199994,5.2,-1.11892802700002));
#349426=CARTESIAN_POINT('Ctrl Pts',(3.91214805199994,2.2,-1.11892802700002));
#349427=CARTESIAN_POINT('Ctrl Pts',(3.91129158899994,12.2,-1.11849225200002));
#349428=CARTESIAN_POINT('Ctrl Pts',(3.91129158899994,5.2,-1.11849225200002));
#349429=CARTESIAN_POINT('Ctrl Pts',(3.91129158899994,2.2,-1.11849225200002));
#349430=CARTESIAN_POINT('Ctrl Pts',(3.91043954099994,12.2,-1.11806005100001));
#349431=CARTESIAN_POINT('Ctrl Pts',(3.91043954099994,5.2,-1.11806005100001));
#349432=CARTESIAN_POINT('Ctrl Pts',(3.91043954099994,2.2,-1.11806005100001));
#349433=CARTESIAN_POINT('Ctrl Pts',(3.90959192299994,12.2,-1.11763141400001));
#349434=CARTESIAN_POINT('Ctrl Pts',(3.90959192299994,5.2,-1.11763141400001));
#349435=CARTESIAN_POINT('Ctrl Pts',(3.90959192299994,2.2,-1.11763141400001));
#349436=CARTESIAN_POINT('Ctrl Pts',(3.90874875099994,12.2,-1.11720633700001));
#349437=CARTESIAN_POINT('Ctrl Pts',(3.90874875099994,5.2,-1.11720633700001));
#349438=CARTESIAN_POINT('Ctrl Pts',(3.90874875099994,2.2,-1.11720633700001));
#349439=CARTESIAN_POINT('Ctrl Pts',(3.90791004099994,12.2,-1.11678481200002));
#349440=CARTESIAN_POINT('Ctrl Pts',(3.90791004099994,5.2,-1.11678481200002));
#349441=CARTESIAN_POINT('Ctrl Pts',(3.90791004099994,2.2,-1.11678481200002));
#349442=CARTESIAN_POINT('Ctrl Pts',(3.90707580699994,12.2,-1.11636683300001));
#349443=CARTESIAN_POINT('Ctrl Pts',(3.90707580699994,5.2,-1.11636683300001));
#349444=CARTESIAN_POINT('Ctrl Pts',(3.90707580699994,2.2,-1.11636683300001));
#349445=CARTESIAN_POINT('Ctrl Pts',(3.90624606799994,12.2,-1.11595239200001));
#349446=CARTESIAN_POINT('Ctrl Pts',(3.90624606799994,5.2,-1.11595239200001));
#349447=CARTESIAN_POINT('Ctrl Pts',(3.90624606799994,2.2,-1.11595239200001));
#349448=CARTESIAN_POINT('Ctrl Pts',(3.90542083599994,12.2,-1.11554148300002));
#349449=CARTESIAN_POINT('Ctrl Pts',(3.90542083599994,5.2,-1.11554148300002));
#349450=CARTESIAN_POINT('Ctrl Pts',(3.90542083599994,2.2,-1.11554148300002));
#349451=CARTESIAN_POINT('Ctrl Pts',(3.90460012899994,12.2,-1.11513409800001));
#349452=CARTESIAN_POINT('Ctrl Pts',(3.90460012899994,5.2,-1.11513409800001));
#349453=CARTESIAN_POINT('Ctrl Pts',(3.90460012899994,2.2,-1.11513409800001));
#349454=CARTESIAN_POINT('Ctrl Pts',(3.90378396299994,12.2,-1.11473023200002));
#349455=CARTESIAN_POINT('Ctrl Pts',(3.90378396299994,5.2,-1.11473023200002));
#349456=CARTESIAN_POINT('Ctrl Pts',(3.90378396299994,2.2,-1.11473023200002));
#349457=CARTESIAN_POINT('Ctrl Pts',(3.90297235299994,12.2,-1.11432987500002));
#349458=CARTESIAN_POINT('Ctrl Pts',(3.90297235299994,5.2,-1.11432987500002));
#349459=CARTESIAN_POINT('Ctrl Pts',(3.90297235299994,2.2,-1.11432987500002));
#349460=CARTESIAN_POINT('Ctrl Pts',(3.90216531599994,12.2,-1.11393302300002));
#349461=CARTESIAN_POINT('Ctrl Pts',(3.90216531599994,5.2,-1.11393302300002));
#349462=CARTESIAN_POINT('Ctrl Pts',(3.90216531599994,2.2,-1.11393302300002));
#349463=CARTESIAN_POINT('Ctrl Pts',(3.90136286599994,12.2,-1.11353966700001));
#349464=CARTESIAN_POINT('Ctrl Pts',(3.90136286599994,5.2,-1.11353966700001));
#349465=CARTESIAN_POINT('Ctrl Pts',(3.90136286599994,2.2,-1.11353966700001));
#349466=CARTESIAN_POINT('Ctrl Pts',(3.90056502099994,12.2,-1.11314980100001));
#349467=CARTESIAN_POINT('Ctrl Pts',(3.90056502099994,5.2,-1.11314980100001));
#349468=CARTESIAN_POINT('Ctrl Pts',(3.90056502099994,2.2,-1.11314980100001));
#349469=CARTESIAN_POINT('Ctrl Pts',(3.89977179699994,12.2,-1.11276341700002));
#349470=CARTESIAN_POINT('Ctrl Pts',(3.89977179699994,5.2,-1.11276341700002));
#349471=CARTESIAN_POINT('Ctrl Pts',(3.89977179699994,2.2,-1.11276341700002));
#349472=CARTESIAN_POINT('Ctrl Pts',(3.89898320899994,12.2,-1.11238050800001));
#349473=CARTESIAN_POINT('Ctrl Pts',(3.89898320899994,5.2,-1.11238050800001));
#349474=CARTESIAN_POINT('Ctrl Pts',(3.89898320899994,2.2,-1.11238050800001));
#349475=CARTESIAN_POINT('Ctrl Pts',(3.89819927199994,12.2,-1.11200106700001));
#349476=CARTESIAN_POINT('Ctrl Pts',(3.89819927199994,5.2,-1.11200106700001));
#349477=CARTESIAN_POINT('Ctrl Pts',(3.89819927199994,2.2,-1.11200106700001));
#349478=CARTESIAN_POINT('Ctrl Pts',(3.89742000499994,12.2,-1.11162508500001));
#349479=CARTESIAN_POINT('Ctrl Pts',(3.89742000499994,5.2,-1.11162508500001));
#349480=CARTESIAN_POINT('Ctrl Pts',(3.89742000499994,2.2,-1.11162508500001));
#349481=CARTESIAN_POINT('Ctrl Pts',(3.89664542199994,12.2,-1.11125255800001));
#349482=CARTESIAN_POINT('Ctrl Pts',(3.89664542199994,5.2,-1.11125255800001));
#349483=CARTESIAN_POINT('Ctrl Pts',(3.89664542199994,2.2,-1.11125255800001));
#349484=CARTESIAN_POINT('Ctrl Pts',(3.89587553999994,12.2,-1.11088347600001));
#349485=CARTESIAN_POINT('Ctrl Pts',(3.89587553999994,5.2,-1.11088347600001));
#349486=CARTESIAN_POINT('Ctrl Pts',(3.89587553999994,2.2,-1.11088347600001));
#349487=CARTESIAN_POINT('Ctrl Pts',(3.89511037599994,12.2,-1.11051783300002));
#349488=CARTESIAN_POINT('Ctrl Pts',(3.89511037599994,5.2,-1.11051783300002));
#349489=CARTESIAN_POINT('Ctrl Pts',(3.89511037599994,2.2,-1.11051783300002));
#349490=CARTESIAN_POINT('Ctrl Pts',(3.89434994499994,12.2,-1.11015562000001));
#349491=CARTESIAN_POINT('Ctrl Pts',(3.89434994499994,5.2,-1.11015562000001));
#349492=CARTESIAN_POINT('Ctrl Pts',(3.89434994499994,2.2,-1.11015562000001));
#349493=CARTESIAN_POINT('Ctrl Pts',(3.89359426299994,12.2,-1.10979683100001));
#349494=CARTESIAN_POINT('Ctrl Pts',(3.89359426299994,5.2,-1.10979683100001));
#349495=CARTESIAN_POINT('Ctrl Pts',(3.89359426299994,2.2,-1.10979683100001));
#349496=CARTESIAN_POINT('Ctrl Pts',(3.89284334799994,12.2,-1.10944145700001));
#349497=CARTESIAN_POINT('Ctrl Pts',(3.89284334799994,5.2,-1.10944145700001));
#349498=CARTESIAN_POINT('Ctrl Pts',(3.89284334799994,2.2,-1.10944145700001));
#349499=CARTESIAN_POINT('Ctrl Pts',(3.89209721499994,12.2,-1.10908949200001));
#349500=CARTESIAN_POINT('Ctrl Pts',(3.89209721499994,5.2,-1.10908949200001));
#349501=CARTESIAN_POINT('Ctrl Pts',(3.89209721499994,2.2,-1.10908949200001));
#349502=CARTESIAN_POINT('Ctrl Pts',(3.89135587999994,12.2,-1.10874092700001));
#349503=CARTESIAN_POINT('Ctrl Pts',(3.89135587999994,5.2,-1.10874092700001));
#349504=CARTESIAN_POINT('Ctrl Pts',(3.89135587999994,2.2,-1.10874092700001));
#349505=CARTESIAN_POINT('Ctrl Pts',(3.89061936199994,12.2,-1.10839575600002));
#349506=CARTESIAN_POINT('Ctrl Pts',(3.89061936199994,5.2,-1.10839575600002));
#349507=CARTESIAN_POINT('Ctrl Pts',(3.89061936199994,2.2,-1.10839575600002));
#349508=CARTESIAN_POINT('Ctrl Pts',(3.88988767399994,12.2,-1.10805397000002));
#349509=CARTESIAN_POINT('Ctrl Pts',(3.88988767399994,5.2,-1.10805397000002));
#349510=CARTESIAN_POINT('Ctrl Pts',(3.88988767399994,2.2,-1.10805397000002));
#349511=CARTESIAN_POINT('Ctrl Pts',(3.88916083499994,12.2,-1.10771556200001));
#349512=CARTESIAN_POINT('Ctrl Pts',(3.88916083499994,5.2,-1.10771556200001));
#349513=CARTESIAN_POINT('Ctrl Pts',(3.88916083499994,2.2,-1.10771556200001));
#349514=CARTESIAN_POINT('Ctrl Pts',(3.88843886099994,12.2,-1.10738052300002));
#349515=CARTESIAN_POINT('Ctrl Pts',(3.88843886099994,5.2,-1.10738052300002));
#349516=CARTESIAN_POINT('Ctrl Pts',(3.88843886099994,2.2,-1.10738052300002));
#349517=CARTESIAN_POINT('Ctrl Pts',(3.88772176899994,12.2,-1.10704884600001));
#349518=CARTESIAN_POINT('Ctrl Pts',(3.88772176899994,5.2,-1.10704884600001));
#349519=CARTESIAN_POINT('Ctrl Pts',(3.88772176899994,2.2,-1.10704884600001));
#349520=CARTESIAN_POINT('Ctrl Pts',(3.88700957299994,12.2,-1.10672052300002));
#349521=CARTESIAN_POINT('Ctrl Pts',(3.88700957299994,5.2,-1.10672052300002));
#349522=CARTESIAN_POINT('Ctrl Pts',(3.88700957299994,2.2,-1.10672052300002));
#349523=CARTESIAN_POINT('Ctrl Pts',(3.88630229399994,12.2,-1.10639554700001));
#349524=CARTESIAN_POINT('Ctrl Pts',(3.88630229399994,5.2,-1.10639554700001));
#349525=CARTESIAN_POINT('Ctrl Pts',(3.88630229399994,2.2,-1.10639554700001));
#349526=CARTESIAN_POINT('Ctrl Pts',(3.88559994499994,12.2,-1.10607390800002));
#349527=CARTESIAN_POINT('Ctrl Pts',(3.88559994499994,5.2,-1.10607390800002));
#349528=CARTESIAN_POINT('Ctrl Pts',(3.88559994499994,2.2,-1.10607390800002));
#349529=CARTESIAN_POINT('Ctrl Pts',(3.88490254399994,12.2,-1.10575560000001));
#349530=CARTESIAN_POINT('Ctrl Pts',(3.88490254399994,5.2,-1.10575560000001));
#349531=CARTESIAN_POINT('Ctrl Pts',(3.88490254399994,2.2,-1.10575560000001));
#349532=CARTESIAN_POINT('Ctrl Pts',(3.88421010699994,12.2,-1.10544061400002));
#349533=CARTESIAN_POINT('Ctrl Pts',(3.88421010699994,5.2,-1.10544061400002));
#349534=CARTESIAN_POINT('Ctrl Pts',(3.88421010699994,2.2,-1.10544061400002));
#349535=CARTESIAN_POINT('Ctrl Pts',(3.88352265299994,12.2,-1.10512894300001));
#349536=CARTESIAN_POINT('Ctrl Pts',(3.88352265299994,5.2,-1.10512894300001));
#349537=CARTESIAN_POINT('Ctrl Pts',(3.88352265299994,2.2,-1.10512894300001));
#349538=CARTESIAN_POINT('Ctrl Pts',(3.88284019699995,12.2,-1.10482057600001));
#349539=CARTESIAN_POINT('Ctrl Pts',(3.88284019699995,5.2,-1.10482057600001));
#349540=CARTESIAN_POINT('Ctrl Pts',(3.88284019699995,2.2,-1.10482057600001));
#349541=CARTESIAN_POINT('Ctrl Pts',(3.88216275599994,12.2,-1.10451550900001));
#349542=CARTESIAN_POINT('Ctrl Pts',(3.88216275599994,5.2,-1.10451550900001));
#349543=CARTESIAN_POINT('Ctrl Pts',(3.88216275599994,2.2,-1.10451550900001));
#349544=CARTESIAN_POINT('Ctrl Pts',(3.88149034799994,12.2,-1.10421373100001));
#349545=CARTESIAN_POINT('Ctrl Pts',(3.88149034799994,5.2,-1.10421373100001));
#349546=CARTESIAN_POINT('Ctrl Pts',(3.88149034799994,2.2,-1.10421373100001));
#349547=CARTESIAN_POINT('Ctrl Pts',(3.88082298799994,12.2,-1.10391523400001));
#349548=CARTESIAN_POINT('Ctrl Pts',(3.88082298799994,5.2,-1.10391523400001));
#349549=CARTESIAN_POINT('Ctrl Pts',(3.88082298799994,2.2,-1.10391523400001));
#349550=CARTESIAN_POINT('Ctrl Pts',(3.88016069499994,12.2,-1.10362001000002));
#349551=CARTESIAN_POINT('Ctrl Pts',(3.88016069499994,5.2,-1.10362001000002));
#349552=CARTESIAN_POINT('Ctrl Pts',(3.88016069499994,2.2,-1.10362001000002));
#349553=CARTESIAN_POINT('Ctrl Pts',(3.87950348599994,12.2,-1.10332805000001));
#349554=CARTESIAN_POINT('Ctrl Pts',(3.87950348599994,5.2,-1.10332805000001));
#349555=CARTESIAN_POINT('Ctrl Pts',(3.87950348599994,2.2,-1.10332805000001));
#349556=CARTESIAN_POINT('Ctrl Pts',(3.87885137499994,12.2,-1.10303934700001));
#349557=CARTESIAN_POINT('Ctrl Pts',(3.87885137499994,5.2,-1.10303934700001));
#349558=CARTESIAN_POINT('Ctrl Pts',(3.87885137499994,2.2,-1.10303934700001));
#349559=CARTESIAN_POINT('Ctrl Pts',(3.87820438299994,12.2,-1.10275389300002));
#349560=CARTESIAN_POINT('Ctrl Pts',(3.87820438299994,5.2,-1.10275389300002));
#349561=CARTESIAN_POINT('Ctrl Pts',(3.87820438299994,2.2,-1.10275389300002));
#349562=CARTESIAN_POINT('Ctrl Pts',(3.87756252599994,12.2,-1.10247167700001));
#349563=CARTESIAN_POINT('Ctrl Pts',(3.87756252599994,5.2,-1.10247167700001));
#349564=CARTESIAN_POINT('Ctrl Pts',(3.87756252599994,2.2,-1.10247167700001));
#349565=CARTESIAN_POINT('Ctrl Pts',(3.87692581899994,12.2,-1.10219269300002));
#349566=CARTESIAN_POINT('Ctrl Pts',(3.87692581899994,5.2,-1.10219269300002));
#349567=CARTESIAN_POINT('Ctrl Pts',(3.87692581899994,2.2,-1.10219269300002));
#349568=CARTESIAN_POINT('Ctrl Pts',(3.87629428199994,12.2,-1.10191693100001));
#349569=CARTESIAN_POINT('Ctrl Pts',(3.87629428199994,5.2,-1.10191693100001));
#349570=CARTESIAN_POINT('Ctrl Pts',(3.87629428199994,2.2,-1.10191693100001));
#349571=CARTESIAN_POINT('Ctrl Pts',(3.87566793099994,12.2,-1.10164438200002));
#349572=CARTESIAN_POINT('Ctrl Pts',(3.87566793099994,5.2,-1.10164438200002));
#349573=CARTESIAN_POINT('Ctrl Pts',(3.87566793099994,2.2,-1.10164438200002));
#349574=CARTESIAN_POINT('Ctrl Pts',(3.87504678299994,12.2,-1.10137503800001));
#349575=CARTESIAN_POINT('Ctrl Pts',(3.87504678299994,5.2,-1.10137503800001));
#349576=CARTESIAN_POINT('Ctrl Pts',(3.87504678299994,2.2,-1.10137503800001));
#349577=CARTESIAN_POINT('Ctrl Pts',(3.87443085699994,12.2,-1.10110889100001));
#349578=CARTESIAN_POINT('Ctrl Pts',(3.87443085699994,5.2,-1.10110889100001));
#349579=CARTESIAN_POINT('Ctrl Pts',(3.87443085699994,2.2,-1.10110889100001));
#349580=CARTESIAN_POINT('Ctrl Pts',(3.87382016699994,12.2,-1.10084593200002));
#349581=CARTESIAN_POINT('Ctrl Pts',(3.87382016699994,5.2,-1.10084593200002));
#349582=CARTESIAN_POINT('Ctrl Pts',(3.87382016699994,2.2,-1.10084593200002));
#349583=CARTESIAN_POINT('Ctrl Pts',(3.87321473399994,12.2,-1.10058615200002));
#349584=CARTESIAN_POINT('Ctrl Pts',(3.87321473399994,5.2,-1.10058615200002));
#349585=CARTESIAN_POINT('Ctrl Pts',(3.87321473399994,2.2,-1.10058615200002));
#349586=CARTESIAN_POINT('Ctrl Pts',(3.87261457399994,12.2,-1.10032954000001));
#349587=CARTESIAN_POINT('Ctrl Pts',(3.87261457399994,5.2,-1.10032954000001));
#349588=CARTESIAN_POINT('Ctrl Pts',(3.87261457399994,2.2,-1.10032954000001));
#349589=CARTESIAN_POINT('Ctrl Pts',(3.87201970499994,12.2,-1.10007609000002));
#349590=CARTESIAN_POINT('Ctrl Pts',(3.87201970499994,5.2,-1.10007609000002));
#349591=CARTESIAN_POINT('Ctrl Pts',(3.87201970499994,2.2,-1.10007609000002));
#349592=CARTESIAN_POINT('Ctrl Pts',(3.87143014299994,12.2,-1.09982579300001));
#349593=CARTESIAN_POINT('Ctrl Pts',(3.87143014299994,5.2,-1.09982579300001));
#349594=CARTESIAN_POINT('Ctrl Pts',(3.87143014299994,2.2,-1.09982579300001));
#349595=CARTESIAN_POINT('Ctrl Pts',(3.87084590699994,12.2,-1.09957863800001));
#349596=CARTESIAN_POINT('Ctrl Pts',(3.87084590699994,5.2,-1.09957863800001));
#349597=CARTESIAN_POINT('Ctrl Pts',(3.87084590699994,2.2,-1.09957863800001));
#349598=CARTESIAN_POINT('Ctrl Pts',(3.87026701399994,12.2,-1.09933461800001));
#349599=CARTESIAN_POINT('Ctrl Pts',(3.87026701399994,5.2,-1.09933461800001));
#349600=CARTESIAN_POINT('Ctrl Pts',(3.87026701399994,2.2,-1.09933461800001));
#349601=CARTESIAN_POINT('Ctrl Pts',(3.86969348299994,12.2,-1.09909372300002));
#349602=CARTESIAN_POINT('Ctrl Pts',(3.86969348299994,5.2,-1.09909372300002));
#349603=CARTESIAN_POINT('Ctrl Pts',(3.86969348299994,2.2,-1.09909372300002));
#349604=CARTESIAN_POINT('Ctrl Pts',(3.86912532999994,12.2,-1.09885594400001));
#349605=CARTESIAN_POINT('Ctrl Pts',(3.86912532999994,5.2,-1.09885594400001));
#349606=CARTESIAN_POINT('Ctrl Pts',(3.86912532999994,2.2,-1.09885594400001));
#349607=CARTESIAN_POINT('Ctrl Pts',(3.86856257199994,12.2,-1.09862127100001));
#349608=CARTESIAN_POINT('Ctrl Pts',(3.86856257199994,5.2,-1.09862127100001));
#349609=CARTESIAN_POINT('Ctrl Pts',(3.86856257199994,2.2,-1.09862127100001));
#349610=CARTESIAN_POINT('Ctrl Pts',(3.86800522999994,12.2,-1.09838969500001));
#349611=CARTESIAN_POINT('Ctrl Pts',(3.86800522999994,5.2,-1.09838969500001));
#349612=CARTESIAN_POINT('Ctrl Pts',(3.86800522999994,2.2,-1.09838969500001));
#349613=CARTESIAN_POINT('Ctrl Pts',(3.86745331999994,12.2,-1.09816120800001));
#349614=CARTESIAN_POINT('Ctrl Pts',(3.86745331999994,5.2,-1.09816120800001));
#349615=CARTESIAN_POINT('Ctrl Pts',(3.86745331999994,2.2,-1.09816120800001));
#349616=CARTESIAN_POINT('Ctrl Pts',(3.86690685899994,12.2,-1.09793580000002));
#349617=CARTESIAN_POINT('Ctrl Pts',(3.86690685899994,5.2,-1.09793580000002));
#349618=CARTESIAN_POINT('Ctrl Pts',(3.86690685899994,2.2,-1.09793580000002));
#349619=CARTESIAN_POINT('Ctrl Pts',(3.86636586599994,12.2,-1.09771346200001));
#349620=CARTESIAN_POINT('Ctrl Pts',(3.86636586599994,5.2,-1.09771346200001));
#349621=CARTESIAN_POINT('Ctrl Pts',(3.86636586599994,2.2,-1.09771346200001));
#349622=CARTESIAN_POINT('Ctrl Pts',(3.86583035899994,12.2,-1.09749418300002));
#349623=CARTESIAN_POINT('Ctrl Pts',(3.86583035899994,5.2,-1.09749418300002));
#349624=CARTESIAN_POINT('Ctrl Pts',(3.86583035899994,2.2,-1.09749418300002));
#349625=CARTESIAN_POINT('Ctrl Pts',(3.86530035599994,12.2,-1.09727795600001));
#349626=CARTESIAN_POINT('Ctrl Pts',(3.86530035599994,5.2,-1.09727795600001));
#349627=CARTESIAN_POINT('Ctrl Pts',(3.86530035599994,2.2,-1.09727795600001));
#349628=CARTESIAN_POINT('Ctrl Pts',(3.86477587299995,12.2,-1.09706476800001));
#349629=CARTESIAN_POINT('Ctrl Pts',(3.86477587299995,5.2,-1.09706476800001));
#349630=CARTESIAN_POINT('Ctrl Pts',(3.86477587299995,2.2,-1.09706476800001));
#349631=CARTESIAN_POINT('Ctrl Pts',(3.86425693199994,12.2,-1.09685461300002));
#349632=CARTESIAN_POINT('Ctrl Pts',(3.86425693199994,5.2,-1.09685461300002));
#349633=CARTESIAN_POINT('Ctrl Pts',(3.86425693199994,2.2,-1.09685461300002));
#349634=CARTESIAN_POINT('Ctrl Pts',(3.86374354899994,12.2,-1.09664748000001));
#349635=CARTESIAN_POINT('Ctrl Pts',(3.86374354899994,5.2,-1.09664748000001));
#349636=CARTESIAN_POINT('Ctrl Pts',(3.86374354899994,2.2,-1.09664748000001));
#349637=CARTESIAN_POINT('Ctrl Pts',(3.86323573999994,12.2,-1.09644335800001));
#349638=CARTESIAN_POINT('Ctrl Pts',(3.86323573999994,5.2,-1.09644335800001));
#349639=CARTESIAN_POINT('Ctrl Pts',(3.86323573999994,2.2,-1.09644335800001));
#349640=CARTESIAN_POINT('Ctrl Pts',(3.86273352699994,12.2,-1.09624223900001));
#349641=CARTESIAN_POINT('Ctrl Pts',(3.86273352699994,5.2,-1.09624223900001));
#349642=CARTESIAN_POINT('Ctrl Pts',(3.86273352699994,2.2,-1.09624223900001));
#349643=CARTESIAN_POINT('Ctrl Pts',(3.86223692699994,12.2,-1.09604411300001));
#349644=CARTESIAN_POINT('Ctrl Pts',(3.86223692699994,5.2,-1.09604411300001));
#349645=CARTESIAN_POINT('Ctrl Pts',(3.86223692699994,2.2,-1.09604411300001));
#349646=CARTESIAN_POINT('Ctrl Pts',(3.86174595699994,12.2,-1.09584897000001));
#349647=CARTESIAN_POINT('Ctrl Pts',(3.86174595699994,5.2,-1.09584897000001));
#349648=CARTESIAN_POINT('Ctrl Pts',(3.86174595699994,2.2,-1.09584897000001));
#349649=CARTESIAN_POINT('Ctrl Pts',(3.86126063599994,12.2,-1.09565680000001));
#349650=CARTESIAN_POINT('Ctrl Pts',(3.86126063599994,5.2,-1.09565680000001));
#349651=CARTESIAN_POINT('Ctrl Pts',(3.86126063599994,2.2,-1.09565680000001));
#349652=CARTESIAN_POINT('Ctrl Pts',(3.86078098399994,12.2,-1.09546759400001));
#349653=CARTESIAN_POINT('Ctrl Pts',(3.86078098399994,5.2,-1.09546759400001));
#349654=CARTESIAN_POINT('Ctrl Pts',(3.86078098399994,2.2,-1.09546759400001));
#349655=CARTESIAN_POINT('Ctrl Pts',(3.86030701699994,12.2,-1.09528133900001));
#349656=CARTESIAN_POINT('Ctrl Pts',(3.86030701699994,5.2,-1.09528133900001));
#349657=CARTESIAN_POINT('Ctrl Pts',(3.86030701699994,2.2,-1.09528133900001));
#349658=CARTESIAN_POINT('Ctrl Pts',(3.85983875499994,12.2,-1.09509802800002));
#349659=CARTESIAN_POINT('Ctrl Pts',(3.85983875499994,5.2,-1.09509802800002));
#349660=CARTESIAN_POINT('Ctrl Pts',(3.85983875499994,2.2,-1.09509802800002));
#349661=CARTESIAN_POINT('Ctrl Pts',(3.85937621599994,12.2,-1.09491765000001));
#349662=CARTESIAN_POINT('Ctrl Pts',(3.85937621599994,5.2,-1.09491765000001));
#349663=CARTESIAN_POINT('Ctrl Pts',(3.85937621599994,2.2,-1.09491765000001));
#349664=CARTESIAN_POINT('Ctrl Pts',(3.85891941899994,12.2,-1.09474019500002));
#349665=CARTESIAN_POINT('Ctrl Pts',(3.85891941899994,5.2,-1.09474019500002));
#349666=CARTESIAN_POINT('Ctrl Pts',(3.85891941899994,2.2,-1.09474019500002));
#349667=CARTESIAN_POINT('Ctrl Pts',(3.85846838299994,12.2,-1.09456565200002));
#349668=CARTESIAN_POINT('Ctrl Pts',(3.85846838299994,5.2,-1.09456565200002));
#349669=CARTESIAN_POINT('Ctrl Pts',(3.85846838299994,2.2,-1.09456565200002));
#349670=CARTESIAN_POINT('Ctrl Pts',(3.85802312499994,12.2,-1.09439401100001));
#349671=CARTESIAN_POINT('Ctrl Pts',(3.85802312499994,5.2,-1.09439401100001));
#349672=CARTESIAN_POINT('Ctrl Pts',(3.85802312499994,2.2,-1.09439401100001));
#349673=CARTESIAN_POINT('Ctrl Pts',(3.85758366499994,12.2,-1.09422526300001));
#349674=CARTESIAN_POINT('Ctrl Pts',(3.85758366499994,5.2,-1.09422526300001));
#349675=CARTESIAN_POINT('Ctrl Pts',(3.85758366499994,2.2,-1.09422526300001));
#349676=CARTESIAN_POINT('Ctrl Pts',(3.85715002099994,12.2,-1.09405939600002));
#349677=CARTESIAN_POINT('Ctrl Pts',(3.85715002099994,5.2,-1.09405939600002));
#349678=CARTESIAN_POINT('Ctrl Pts',(3.85715002099994,2.2,-1.09405939600002));
#349679=CARTESIAN_POINT('Ctrl Pts',(3.85672221399994,12.2,-1.09389640100002));
#349680=CARTESIAN_POINT('Ctrl Pts',(3.85672221399994,5.2,-1.09389640100002));
#349681=CARTESIAN_POINT('Ctrl Pts',(3.85672221399994,2.2,-1.09389640100002));
#349682=CARTESIAN_POINT('Ctrl Pts',(3.85630025899994,12.2,-1.09373626600001));
#349683=CARTESIAN_POINT('Ctrl Pts',(3.85630025899994,5.2,-1.09373626600001));
#349684=CARTESIAN_POINT('Ctrl Pts',(3.85630025899994,2.2,-1.09373626600001));
#349685=CARTESIAN_POINT('Ctrl Pts',(3.85588417899994,12.2,-1.09357898100002));
#349686=CARTESIAN_POINT('Ctrl Pts',(3.85588417899994,5.2,-1.09357898100002));
#349687=CARTESIAN_POINT('Ctrl Pts',(3.85588417899994,2.2,-1.09357898100002));
#349688=CARTESIAN_POINT('Ctrl Pts',(3.85547399099994,12.2,-1.09342453700001));
#349689=CARTESIAN_POINT('Ctrl Pts',(3.85547399099994,5.2,-1.09342453700001));
#349690=CARTESIAN_POINT('Ctrl Pts',(3.85547399099994,2.2,-1.09342453700001));
#349691=CARTESIAN_POINT('Ctrl Pts',(3.85506971299994,12.2,-1.09327292100001));
#349692=CARTESIAN_POINT('Ctrl Pts',(3.85506971299994,5.2,-1.09327292100001));
#349693=CARTESIAN_POINT('Ctrl Pts',(3.85506971299994,2.2,-1.09327292100001));
#349694=CARTESIAN_POINT('Ctrl Pts',(3.85467136599994,12.2,-1.09312412300001));
#349695=CARTESIAN_POINT('Ctrl Pts',(3.85467136599994,5.2,-1.09312412300001));
#349696=CARTESIAN_POINT('Ctrl Pts',(3.85467136599994,2.2,-1.09312412300001));
#349697=CARTESIAN_POINT('Ctrl Pts',(3.85427896699994,12.2,-1.09297813400001));
#349698=CARTESIAN_POINT('Ctrl Pts',(3.85427896699994,5.2,-1.09297813400001));
#349699=CARTESIAN_POINT('Ctrl Pts',(3.85427896699994,2.2,-1.09297813400001));
#349700=CARTESIAN_POINT('Ctrl Pts',(3.85389253799994,12.2,-1.09283494100001));
#349701=CARTESIAN_POINT('Ctrl Pts',(3.85389253799994,5.2,-1.09283494100001));
#349702=CARTESIAN_POINT('Ctrl Pts',(3.85389253799994,2.2,-1.09283494100001));
#349703=CARTESIAN_POINT('Ctrl Pts',(3.85351209599994,12.2,-1.09269453300001));
#349704=CARTESIAN_POINT('Ctrl Pts',(3.85351209599994,5.2,-1.09269453300001));
#349705=CARTESIAN_POINT('Ctrl Pts',(3.85351209599994,2.2,-1.09269453300001));
#349706=CARTESIAN_POINT('Ctrl Pts',(3.85313766099994,12.2,-1.09255690100001));
#349707=CARTESIAN_POINT('Ctrl Pts',(3.85313766099994,5.2,-1.09255690100001));
#349708=CARTESIAN_POINT('Ctrl Pts',(3.85313766099994,2.2,-1.09255690100001));
#349709=CARTESIAN_POINT('Ctrl Pts',(3.85276925099994,12.2,-1.09242203300001));
#349710=CARTESIAN_POINT('Ctrl Pts',(3.85276925099994,5.2,-1.09242203300001));
#349711=CARTESIAN_POINT('Ctrl Pts',(3.85276925099994,2.2,-1.09242203300001));
#349712=CARTESIAN_POINT('Ctrl Pts',(3.85240688799994,12.2,-1.09228991700002));
#349713=CARTESIAN_POINT('Ctrl Pts',(3.85240688799994,5.2,-1.09228991700002));
#349714=CARTESIAN_POINT('Ctrl Pts',(3.85240688799994,2.2,-1.09228991700002));
#349715=CARTESIAN_POINT('Ctrl Pts',(3.85205058899994,12.2,-1.09216054400001));
#349716=CARTESIAN_POINT('Ctrl Pts',(3.85205058899994,5.2,-1.09216054400001));
#349717=CARTESIAN_POINT('Ctrl Pts',(3.85205058899994,2.2,-1.09216054400001));
#349718=CARTESIAN_POINT('Ctrl Pts',(3.85170037499994,12.2,-1.09203390100001));
#349719=CARTESIAN_POINT('Ctrl Pts',(3.85170037499994,5.2,-1.09203390100001));
#349720=CARTESIAN_POINT('Ctrl Pts',(3.85170037499994,2.2,-1.09203390100001));
#349721=CARTESIAN_POINT('Ctrl Pts',(3.85135626499994,12.2,-1.09190997700002));
#349722=CARTESIAN_POINT('Ctrl Pts',(3.85135626499994,5.2,-1.09190997700002));
#349723=CARTESIAN_POINT('Ctrl Pts',(3.85135626499994,2.2,-1.09190997700002));
#349724=CARTESIAN_POINT('Ctrl Pts',(3.85101827699994,12.2,-1.09178876200001));
#349725=CARTESIAN_POINT('Ctrl Pts',(3.85101827699994,5.2,-1.09178876200001));
#349726=CARTESIAN_POINT('Ctrl Pts',(3.85101827699994,2.2,-1.09178876200001));
#349727=CARTESIAN_POINT('Ctrl Pts',(3.85068643399994,12.2,-1.09167024400001));
#349728=CARTESIAN_POINT('Ctrl Pts',(3.85068643399994,5.2,-1.09167024400001));
#349729=CARTESIAN_POINT('Ctrl Pts',(3.85068643399994,2.2,-1.09167024400001));
#349730=CARTESIAN_POINT('Ctrl Pts',(3.85036075299994,12.2,-1.09155441100001));
#349731=CARTESIAN_POINT('Ctrl Pts',(3.85036075299994,5.2,-1.09155441100001));
#349732=CARTESIAN_POINT('Ctrl Pts',(3.85036075299994,2.2,-1.09155441100001));
#349733=CARTESIAN_POINT('Ctrl Pts',(3.85004125399994,12.2,-1.09144125200002));
#349734=CARTESIAN_POINT('Ctrl Pts',(3.85004125399994,5.2,-1.09144125200002));
#349735=CARTESIAN_POINT('Ctrl Pts',(3.85004125399994,2.2,-1.09144125200002));
#349736=CARTESIAN_POINT('Ctrl Pts',(3.84972795699994,12.2,-1.09133075600001));
#349737=CARTESIAN_POINT('Ctrl Pts',(3.84972795699994,5.2,-1.09133075600001));
#349738=CARTESIAN_POINT('Ctrl Pts',(3.84972795699994,2.2,-1.09133075600001));
#349739=CARTESIAN_POINT('Ctrl Pts',(3.84942088299994,12.2,-1.09122291000002));
#349740=CARTESIAN_POINT('Ctrl Pts',(3.84942088299994,5.2,-1.09122291000002));
#349741=CARTESIAN_POINT('Ctrl Pts',(3.84942088299994,2.2,-1.09122291000002));
#349742=CARTESIAN_POINT('Ctrl Pts',(3.84912005099994,12.2,-1.09111770400002));
#349743=CARTESIAN_POINT('Ctrl Pts',(3.84912005099994,5.2,-1.09111770400002));
#349744=CARTESIAN_POINT('Ctrl Pts',(3.84912005099994,2.2,-1.09111770400002));
#349745=CARTESIAN_POINT('Ctrl Pts',(3.84882547999994,12.2,-1.09101512600001));
#349746=CARTESIAN_POINT('Ctrl Pts',(3.84882547999994,5.2,-1.09101512600001));
#349747=CARTESIAN_POINT('Ctrl Pts',(3.84882547999994,2.2,-1.09101512600001));
#349748=CARTESIAN_POINT('Ctrl Pts',(3.84853719099994,12.2,-1.09091516300001));
#349749=CARTESIAN_POINT('Ctrl Pts',(3.84853719099994,5.2,-1.09091516300001));
#349750=CARTESIAN_POINT('Ctrl Pts',(3.84853719099994,2.2,-1.09091516300001));
#349751=CARTESIAN_POINT('Ctrl Pts',(3.84825520499994,12.2,-1.09081780400002));
#349752=CARTESIAN_POINT('Ctrl Pts',(3.84825520499994,5.2,-1.09081780400002));
#349753=CARTESIAN_POINT('Ctrl Pts',(3.84825520499994,2.2,-1.09081780400002));
#349754=CARTESIAN_POINT('Ctrl Pts',(3.84797953999994,12.2,-1.09072303800001));
#349755=CARTESIAN_POINT('Ctrl Pts',(3.84797953999994,5.2,-1.09072303800001));
#349756=CARTESIAN_POINT('Ctrl Pts',(3.84797953999994,2.2,-1.09072303800001));
#349757=CARTESIAN_POINT('Ctrl Pts',(3.84771021599994,12.2,-1.09063085100002));
#349758=CARTESIAN_POINT('Ctrl Pts',(3.84771021599994,5.2,-1.09063085100002));
#349759=CARTESIAN_POINT('Ctrl Pts',(3.84771021599994,2.2,-1.09063085100002));
#349760=CARTESIAN_POINT('Ctrl Pts',(3.84744725699994,12.2,-1.09054123300002));
#349761=CARTESIAN_POINT('Ctrl Pts',(3.84744725699994,5.2,-1.09054123300002));
#349762=CARTESIAN_POINT('Ctrl Pts',(3.84744725699994,2.2,-1.09054123300002));
#349763=CARTESIAN_POINT('Ctrl Pts',(3.84719067799994,12.2,-1.09045417100001));
#349764=CARTESIAN_POINT('Ctrl Pts',(3.84719067799994,5.2,-1.09045417100001));
#349765=CARTESIAN_POINT('Ctrl Pts',(3.84719067799994,2.2,-1.09045417100001));
#349766=CARTESIAN_POINT('Ctrl Pts',(3.84694050299994,12.2,-1.09036965200001));
#349767=CARTESIAN_POINT('Ctrl Pts',(3.84694050299994,5.2,-1.09036965200001));
#349768=CARTESIAN_POINT('Ctrl Pts',(3.84694050299994,2.2,-1.09036965200001));
#349769=CARTESIAN_POINT('Ctrl Pts',(3.84669675099994,12.2,-1.09028766600002));
#349770=CARTESIAN_POINT('Ctrl Pts',(3.84669675099994,5.2,-1.09028766600002));
#349771=CARTESIAN_POINT('Ctrl Pts',(3.84669675099994,2.2,-1.09028766600002));
#349772=CARTESIAN_POINT('Ctrl Pts',(3.84645944399994,12.2,-1.09020819900001));
#349773=CARTESIAN_POINT('Ctrl Pts',(3.84645944399994,5.2,-1.09020819900001));
#349774=CARTESIAN_POINT('Ctrl Pts',(3.84645944399994,2.2,-1.09020819900001));
#349775=CARTESIAN_POINT('Ctrl Pts',(3.84622859999994,12.2,-1.09013123800001));
#349776=CARTESIAN_POINT('Ctrl Pts',(3.84622859999994,5.2,-1.09013123800001));
#349777=CARTESIAN_POINT('Ctrl Pts',(3.84622859999994,2.2,-1.09013123800001));
#349778=CARTESIAN_POINT('Ctrl Pts',(3.84600424099994,12.2,-1.09005677300001));
#349779=CARTESIAN_POINT('Ctrl Pts',(3.84600424099994,5.2,-1.09005677300001));
#349780=CARTESIAN_POINT('Ctrl Pts',(3.84600424099994,2.2,-1.09005677300001));
#349781=CARTESIAN_POINT('Ctrl Pts',(3.84578638699994,12.2,-1.08998479000002));
#349782=CARTESIAN_POINT('Ctrl Pts',(3.84578638699994,5.2,-1.08998479000002));
#349783=CARTESIAN_POINT('Ctrl Pts',(3.84578638699994,2.2,-1.08998479000002));
#349784=CARTESIAN_POINT('Ctrl Pts',(3.84557505899994,12.2,-1.08991527600002));
#349785=CARTESIAN_POINT('Ctrl Pts',(3.84557505899994,5.2,-1.08991527600002));
#349786=CARTESIAN_POINT('Ctrl Pts',(3.84557505899994,2.2,-1.08991527600002));
#349787=CARTESIAN_POINT('Ctrl Pts',(3.84537027799994,12.2,-1.08984822000001));
#349788=CARTESIAN_POINT('Ctrl Pts',(3.84537027799994,5.2,-1.08984822000001));
#349789=CARTESIAN_POINT('Ctrl Pts',(3.84537027799994,2.2,-1.08984822000001));
#349790=CARTESIAN_POINT('Ctrl Pts',(3.84517206499994,12.2,-1.08978360800001));
#349791=CARTESIAN_POINT('Ctrl Pts',(3.84517206499994,5.2,-1.08978360800001));
#349792=CARTESIAN_POINT('Ctrl Pts',(3.84517206499994,2.2,-1.08978360800001));
#349793=CARTESIAN_POINT('Ctrl Pts',(3.84498043899994,12.2,-1.08972142800001));
#349794=CARTESIAN_POINT('Ctrl Pts',(3.84498043899994,5.2,-1.08972142800001));
#349795=CARTESIAN_POINT('Ctrl Pts',(3.84498043899994,2.2,-1.08972142800001));
#349796=CARTESIAN_POINT('Ctrl Pts',(3.84479542399994,12.2,-1.08966166700001));
#349797=CARTESIAN_POINT('Ctrl Pts',(3.84479542399994,5.2,-1.08966166700001));
#349798=CARTESIAN_POINT('Ctrl Pts',(3.84479542399994,2.2,-1.08966166700001));
#349799=CARTESIAN_POINT('Ctrl Pts',(3.84461703899994,12.2,-1.08960431100002));
#349800=CARTESIAN_POINT('Ctrl Pts',(3.84461703899994,5.2,-1.08960431100002));
#349801=CARTESIAN_POINT('Ctrl Pts',(3.84461703899994,2.2,-1.08960431100002));
#349802=CARTESIAN_POINT('Ctrl Pts',(3.84444530599994,12.2,-1.08954934800002));
#349803=CARTESIAN_POINT('Ctrl Pts',(3.84444530599994,5.2,-1.08954934800002));
#349804=CARTESIAN_POINT('Ctrl Pts',(3.84444530599994,2.2,-1.08954934800002));
#349805=CARTESIAN_POINT('Ctrl Pts',(3.84428024399994,12.2,-1.08949676500002));
#349806=CARTESIAN_POINT('Ctrl Pts',(3.84428024399994,5.2,-1.08949676500002));
#349807=CARTESIAN_POINT('Ctrl Pts',(3.84428024399994,2.2,-1.08949676500002));
#349808=CARTESIAN_POINT('Ctrl Pts',(3.84412187499994,12.2,-1.08944655000002));
#349809=CARTESIAN_POINT('Ctrl Pts',(3.84412187499994,5.2,-1.08944655000002));
#349810=CARTESIAN_POINT('Ctrl Pts',(3.84412187499994,2.2,-1.08944655000002));
#349811=CARTESIAN_POINT('Ctrl Pts',(3.84397021999995,12.2,-1.08939869000002));
#349812=CARTESIAN_POINT('Ctrl Pts',(3.84397021999995,5.2,-1.08939869000002));
#349813=CARTESIAN_POINT('Ctrl Pts',(3.84397021999995,2.2,-1.08939869000002));
#349814=CARTESIAN_POINT('Ctrl Pts',(3.84382529999994,12.2,-1.08935317000002));
#349815=CARTESIAN_POINT('Ctrl Pts',(3.84382529999994,5.2,-1.08935317000002));
#349816=CARTESIAN_POINT('Ctrl Pts',(3.84382529999994,2.2,-1.08935317000002));
#349817=CARTESIAN_POINT('Ctrl Pts',(3.84368713799994,12.2,-1.08930997700002));
#349818=CARTESIAN_POINT('Ctrl Pts',(3.84368713799994,5.2,-1.08930997700002));
#349819=CARTESIAN_POINT('Ctrl Pts',(3.84368713799994,2.2,-1.08930997700002));
#349820=CARTESIAN_POINT('Ctrl Pts',(3.84355575699994,12.2,-1.08926909700001));
#349821=CARTESIAN_POINT('Ctrl Pts',(3.84355575699994,5.2,-1.08926909700001));
#349822=CARTESIAN_POINT('Ctrl Pts',(3.84355575699994,2.2,-1.08926909700001));
#349823=CARTESIAN_POINT('Ctrl Pts',(3.84343117799994,12.2,-1.08923051600001));
#349824=CARTESIAN_POINT('Ctrl Pts',(3.84343117799994,5.2,-1.08923051600001));
#349825=CARTESIAN_POINT('Ctrl Pts',(3.84343117799994,2.2,-1.08923051600001));
#349826=CARTESIAN_POINT('Ctrl Pts',(3.84331342199994,12.2,-1.08919422100001));
#349827=CARTESIAN_POINT('Ctrl Pts',(3.84331342199994,5.2,-1.08919422100001));
#349828=CARTESIAN_POINT('Ctrl Pts',(3.84331342199994,2.2,-1.08919422100001));
#349829=CARTESIAN_POINT('Ctrl Pts',(3.84320250899994,12.2,-1.08916020000001));
#349830=CARTESIAN_POINT('Ctrl Pts',(3.84320250899994,5.2,-1.08916020000001));
#349831=CARTESIAN_POINT('Ctrl Pts',(3.84320250899994,2.2,-1.08916020000001));
#349832=CARTESIAN_POINT('Ctrl Pts',(3.84309845699994,12.2,-1.08912844000002));
#349833=CARTESIAN_POINT('Ctrl Pts',(3.84309845699994,5.2,-1.08912844000002));
#349834=CARTESIAN_POINT('Ctrl Pts',(3.84309845699994,2.2,-1.08912844000002));
#349835=CARTESIAN_POINT('Ctrl Pts',(3.84300128699994,12.2,-1.08909893100002));
#349836=CARTESIAN_POINT('Ctrl Pts',(3.84300128699994,5.2,-1.08909893100002));
#349837=CARTESIAN_POINT('Ctrl Pts',(3.84300128699994,2.2,-1.08909893100002));
#349838=CARTESIAN_POINT('Ctrl Pts',(3.84291102199994,12.2,-1.08907165500002));
#349839=CARTESIAN_POINT('Ctrl Pts',(3.84291102199994,5.2,-1.08907165500002));
#349840=CARTESIAN_POINT('Ctrl Pts',(3.84291102199994,2.2,-1.08907165500002));
#349841=CARTESIAN_POINT('Ctrl Pts',(3.84282768499994,12.2,-1.08904659800002));
#349842=CARTESIAN_POINT('Ctrl Pts',(3.84282768499994,5.2,-1.08904659800002));
#349843=CARTESIAN_POINT('Ctrl Pts',(3.84282768499994,2.2,-1.08904659800002));
#349844=CARTESIAN_POINT('Ctrl Pts',(3.84275130599994,12.2,-1.08902374300001));
#349845=CARTESIAN_POINT('Ctrl Pts',(3.84275130599994,5.2,-1.08902374300001));
#349846=CARTESIAN_POINT('Ctrl Pts',(3.84275130599994,2.2,-1.08902374300001));
#349847=CARTESIAN_POINT('Ctrl Pts',(3.84268191099994,12.2,-1.08900307200001));
#349848=CARTESIAN_POINT('Ctrl Pts',(3.84268191099994,5.2,-1.08900307200001));
#349849=CARTESIAN_POINT('Ctrl Pts',(3.84268191099994,2.2,-1.08900307200001));
#349850=CARTESIAN_POINT('Ctrl Pts',(3.84261952399994,12.2,-1.08898456900001));
#349851=CARTESIAN_POINT('Ctrl Pts',(3.84261952399994,5.2,-1.08898456900001));
#349852=CARTESIAN_POINT('Ctrl Pts',(3.84261952399994,2.2,-1.08898456900001));
#349853=CARTESIAN_POINT('Ctrl Pts',(3.84256416399994,12.2,-1.08896822300002));
#349854=CARTESIAN_POINT('Ctrl Pts',(3.84256416399994,5.2,-1.08896822300002));
#349855=CARTESIAN_POINT('Ctrl Pts',(3.84256416399994,2.2,-1.08896822300002));
#349856=CARTESIAN_POINT('Ctrl Pts',(3.84251066686886,12.2,-1.0889525084115));
#349857=CARTESIAN_POINT('Ctrl Pts',(3.84251066686886,5.2,-1.0889525084115));
#349858=CARTESIAN_POINT('Ctrl Pts',(3.84251066686886,2.2,-1.0889525084115));
#349859=CARTESIAN_POINT('Ctrl Pts',(3.84247407877687,12.2,-1.08894183751314));
#349860=CARTESIAN_POINT('Ctrl Pts',(3.84247407877687,5.2,-1.08894183751314));
#349861=CARTESIAN_POINT('Ctrl Pts',(3.84247407877687,2.2,-1.08894183751314));
#349862=CARTESIAN_POINT('Ctrl Pts',(3.84244995866238,12.2,-1.08893486249907));
#349863=CARTESIAN_POINT('Ctrl Pts',(3.84244995866238,5.2,-1.08893486249907));
#349864=CARTESIAN_POINT('Ctrl Pts',(3.84244995866238,2.2,-1.08893486249907));
#349865=CARTESIAN_POINT('Ctrl Pts',(3.84243492681053,12.2,-1.0889305491042));
#349866=CARTESIAN_POINT('Ctrl Pts',(3.84243492681053,5.2,-1.0889305491042));
#349867=CARTESIAN_POINT('Ctrl Pts',(3.84243492681053,2.2,-1.0889305491042));
#349868=CARTESIAN_POINT('Ctrl Pts',(3.84242564299994,12.2,-1.08892788300002));
#349869=CARTESIAN_POINT('Ctrl Pts',(3.84242564299994,5.2,-1.08892788300002));
#349870=CARTESIAN_POINT('Ctrl Pts',(3.84242564299994,2.2,-1.08892788300002));
#349871=CARTESIAN_POINT('',(4.46529931499995,12.2,-1.61975369200002));
#349872=CARTESIAN_POINT('Origin',(-5.66300478732629E-14,15.2,-1.77635683940025E-14));
#349873=CARTESIAN_POINT('',(4.33922903699994,12.2,-1.93225033600001));
#349874=CARTESIAN_POINT('Ctrl Pts',(3.52236173899994,12.2,-1.88224066100001));
#349875=CARTESIAN_POINT('Ctrl Pts',(3.52236173899994,5.2,-1.88224066100001));
#349876=CARTESIAN_POINT('Ctrl Pts',(3.52236173899994,2.2,-1.88224066100001));
#349877=CARTESIAN_POINT('Ctrl Pts',(3.52236778764287,12.2,-1.88224386181091));
#349878=CARTESIAN_POINT('Ctrl Pts',(3.52236778764287,5.2,-1.88224386181091));
#349879=CARTESIAN_POINT('Ctrl Pts',(3.52236778764287,2.2,-1.88224386181091));
#349880=CARTESIAN_POINT('Ctrl Pts',(3.52237948178093,12.2,-1.88225005510073));
#349881=CARTESIAN_POINT('Ctrl Pts',(3.52237948178093,5.2,-1.88225005510073));
#349882=CARTESIAN_POINT('Ctrl Pts',(3.52237948178093,2.2,-1.88225005510073));
#349883=CARTESIAN_POINT('Ctrl Pts',(3.52239682951887,12.2,-1.88225923963477));
#349884=CARTESIAN_POINT('Ctrl Pts',(3.52239682951887,5.2,-1.88225923963477));
#349885=CARTESIAN_POINT('Ctrl Pts',(3.52239682951887,2.2,-1.88225923963477));
#349886=CARTESIAN_POINT('Ctrl Pts',(3.52241983802047,12.2,-1.88227141541148));
#349887=CARTESIAN_POINT('Ctrl Pts',(3.52241983802047,5.2,-1.88227141541148));
#349888=CARTESIAN_POINT('Ctrl Pts',(3.52241983802047,2.2,-1.88227141541148));
#349889=CARTESIAN_POINT('Ctrl Pts',(3.52245994599994,12.2,-1.88229242900002));
#349890=CARTESIAN_POINT('Ctrl Pts',(3.52245994599994,5.2,-1.88229242900002));
#349891=CARTESIAN_POINT('Ctrl Pts',(3.52245994599994,2.2,-1.88229242900002));
#349892=CARTESIAN_POINT('Ctrl Pts',(3.52250459199994,12.2,-1.88231573900001));
#349893=CARTESIAN_POINT('Ctrl Pts',(3.52250459199994,5.2,-1.88231573900001));
#349894=CARTESIAN_POINT('Ctrl Pts',(3.52250459199994,2.2,-1.88231573900001));
#349895=CARTESIAN_POINT('Ctrl Pts',(3.52255579699994,12.2,-1.88234238500002));
#349896=CARTESIAN_POINT('Ctrl Pts',(3.52255579699994,5.2,-1.88234238500002));
#349897=CARTESIAN_POINT('Ctrl Pts',(3.52255579699994,2.2,-1.88234238500002));
#349898=CARTESIAN_POINT('Ctrl Pts',(3.52261355799994,12.2,-1.88237235300001));
#349899=CARTESIAN_POINT('Ctrl Pts',(3.52261355799994,5.2,-1.88237235300001));
#349900=CARTESIAN_POINT('Ctrl Pts',(3.52261355799994,2.2,-1.88237235300001));
#349901=CARTESIAN_POINT('Ctrl Pts',(3.52267787099994,12.2,-1.88240562300001));
#349902=CARTESIAN_POINT('Ctrl Pts',(3.52267787099994,5.2,-1.88240562300001));
#349903=CARTESIAN_POINT('Ctrl Pts',(3.52267787099994,2.2,-1.88240562300001));
#349904=CARTESIAN_POINT('Ctrl Pts',(3.52274872699994,12.2,-1.88244216800001));
#349905=CARTESIAN_POINT('Ctrl Pts',(3.52274872699994,5.2,-1.88244216800001));
#349906=CARTESIAN_POINT('Ctrl Pts',(3.52274872699994,2.2,-1.88244216800001));
#349907=CARTESIAN_POINT('Ctrl Pts',(3.52282612199994,12.2,-1.88248195500002));
#349908=CARTESIAN_POINT('Ctrl Pts',(3.52282612199994,5.2,-1.88248195500002));
#349909=CARTESIAN_POINT('Ctrl Pts',(3.52282612199994,2.2,-1.88248195500002));
#349910=CARTESIAN_POINT('Ctrl Pts',(3.52291004499994,12.2,-1.88252495200001));
#349911=CARTESIAN_POINT('Ctrl Pts',(3.52291004499994,5.2,-1.88252495200001));
#349912=CARTESIAN_POINT('Ctrl Pts',(3.52291004499994,2.2,-1.88252495200001));
#349913=CARTESIAN_POINT('Ctrl Pts',(3.52300048899994,12.2,-1.88257113000001));
#349914=CARTESIAN_POINT('Ctrl Pts',(3.52300048899994,5.2,-1.88257113000001));
#349915=CARTESIAN_POINT('Ctrl Pts',(3.52300048899994,2.2,-1.88257113000001));
#349916=CARTESIAN_POINT('Ctrl Pts',(3.52309744999994,12.2,-1.88262046600002));
#349917=CARTESIAN_POINT('Ctrl Pts',(3.52309744999994,5.2,-1.88262046600002));
#349918=CARTESIAN_POINT('Ctrl Pts',(3.52309744999994,2.2,-1.88262046600002));
#349919=CARTESIAN_POINT('Ctrl Pts',(3.52320092099994,12.2,-1.88267293300001));
#349920=CARTESIAN_POINT('Ctrl Pts',(3.52320092099994,5.2,-1.88267293300001));
#349921=CARTESIAN_POINT('Ctrl Pts',(3.52320092099994,2.2,-1.88267293300001));
#349922=CARTESIAN_POINT('Ctrl Pts',(3.52331089799994,12.2,-1.88272851300002));
#349923=CARTESIAN_POINT('Ctrl Pts',(3.52331089799994,5.2,-1.88272851300002));
#349924=CARTESIAN_POINT('Ctrl Pts',(3.52331089799994,2.2,-1.88272851300002));
#349925=CARTESIAN_POINT('Ctrl Pts',(3.52342737399994,12.2,-1.88278718000001));
#349926=CARTESIAN_POINT('Ctrl Pts',(3.52342737399994,5.2,-1.88278718000001));
#349927=CARTESIAN_POINT('Ctrl Pts',(3.52342737399994,2.2,-1.88278718000001));
#349928=CARTESIAN_POINT('Ctrl Pts',(3.52355034299995,12.2,-1.88284891300002));
#349929=CARTESIAN_POINT('Ctrl Pts',(3.52355034299995,5.2,-1.88284891300002));
#349930=CARTESIAN_POINT('Ctrl Pts',(3.52355034299995,2.2,-1.88284891300002));
#349931=CARTESIAN_POINT('Ctrl Pts',(3.52367979899994,12.2,-1.88291368400002));
#349932=CARTESIAN_POINT('Ctrl Pts',(3.52367979899994,5.2,-1.88291368400002));
#349933=CARTESIAN_POINT('Ctrl Pts',(3.52367979899994,2.2,-1.88291368400002));
#349934=CARTESIAN_POINT('Ctrl Pts',(3.52381573499994,12.2,-1.88298147000001));
#349935=CARTESIAN_POINT('Ctrl Pts',(3.52381573499994,5.2,-1.88298147000001));
#349936=CARTESIAN_POINT('Ctrl Pts',(3.52381573499994,2.2,-1.88298147000001));
#349937=CARTESIAN_POINT('Ctrl Pts',(3.52395814699995,12.2,-1.88305224500001));
#349938=CARTESIAN_POINT('Ctrl Pts',(3.52395814699995,5.2,-1.88305224500001));
#349939=CARTESIAN_POINT('Ctrl Pts',(3.52395814699995,2.2,-1.88305224500001));
#349940=CARTESIAN_POINT('Ctrl Pts',(3.52410702599994,12.2,-1.88312598300001));
#349941=CARTESIAN_POINT('Ctrl Pts',(3.52410702599994,5.2,-1.88312598300001));
#349942=CARTESIAN_POINT('Ctrl Pts',(3.52410702599994,2.2,-1.88312598300001));
#349943=CARTESIAN_POINT('Ctrl Pts',(3.52426236699994,12.2,-1.88320266000002));
#349944=CARTESIAN_POINT('Ctrl Pts',(3.52426236699994,5.2,-1.88320266000002));
#349945=CARTESIAN_POINT('Ctrl Pts',(3.52426236699994,2.2,-1.88320266000002));
#349946=CARTESIAN_POINT('Ctrl Pts',(3.52442416399994,12.2,-1.88328225300001));
#349947=CARTESIAN_POINT('Ctrl Pts',(3.52442416399994,5.2,-1.88328225300001));
#349948=CARTESIAN_POINT('Ctrl Pts',(3.52442416399994,2.2,-1.88328225300001));
#349949=CARTESIAN_POINT('Ctrl Pts',(3.52459241099994,12.2,-1.88336473900002));
#349950=CARTESIAN_POINT('Ctrl Pts',(3.52459241099994,5.2,-1.88336473900002));
#349951=CARTESIAN_POINT('Ctrl Pts',(3.52459241099994,2.2,-1.88336473900002));
#349952=CARTESIAN_POINT('Ctrl Pts',(3.52476710199995,12.2,-1.88345009300001));
#349953=CARTESIAN_POINT('Ctrl Pts',(3.52476710199995,5.2,-1.88345009300001));
#349954=CARTESIAN_POINT('Ctrl Pts',(3.52476710199995,2.2,-1.88345009300001));
#349955=CARTESIAN_POINT('Ctrl Pts',(3.52494822899994,12.2,-1.88353829200001));
#349956=CARTESIAN_POINT('Ctrl Pts',(3.52494822899994,5.2,-1.88353829200001));
#349957=CARTESIAN_POINT('Ctrl Pts',(3.52494822899994,2.2,-1.88353829200001));
#349958=CARTESIAN_POINT('Ctrl Pts',(3.52513578899994,12.2,-1.88362931300002));
#349959=CARTESIAN_POINT('Ctrl Pts',(3.52513578899994,5.2,-1.88362931300002));
#349960=CARTESIAN_POINT('Ctrl Pts',(3.52513578899994,2.2,-1.88362931300002));
#349961=CARTESIAN_POINT('Ctrl Pts',(3.52532977399994,12.2,-1.88372313000002));
#349962=CARTESIAN_POINT('Ctrl Pts',(3.52532977399994,5.2,-1.88372313000002));
#349963=CARTESIAN_POINT('Ctrl Pts',(3.52532977399994,2.2,-1.88372313000002));
#349964=CARTESIAN_POINT('Ctrl Pts',(3.52553017799994,12.2,-1.88381972200002));
#349965=CARTESIAN_POINT('Ctrl Pts',(3.52553017799994,5.2,-1.88381972200002));
#349966=CARTESIAN_POINT('Ctrl Pts',(3.52553017799994,2.2,-1.88381972200002));
#349967=CARTESIAN_POINT('Ctrl Pts',(3.52573699499994,12.2,-1.88391906300001));
#349968=CARTESIAN_POINT('Ctrl Pts',(3.52573699499994,5.2,-1.88391906300001));
#349969=CARTESIAN_POINT('Ctrl Pts',(3.52573699499994,2.2,-1.88391906300001));
#349970=CARTESIAN_POINT('Ctrl Pts',(3.52595021799994,12.2,-1.88402113000001));
#349971=CARTESIAN_POINT('Ctrl Pts',(3.52595021799994,5.2,-1.88402113000001));
#349972=CARTESIAN_POINT('Ctrl Pts',(3.52595021799994,2.2,-1.88402113000001));
#349973=CARTESIAN_POINT('Ctrl Pts',(3.52616984199994,12.2,-1.88412590200001));
#349974=CARTESIAN_POINT('Ctrl Pts',(3.52616984199994,5.2,-1.88412590200001));
#349975=CARTESIAN_POINT('Ctrl Pts',(3.52616984199994,2.2,-1.88412590200001));
#349976=CARTESIAN_POINT('Ctrl Pts',(3.52639585899994,12.2,-1.88423335500001));
#349977=CARTESIAN_POINT('Ctrl Pts',(3.52639585899994,5.2,-1.88423335500001));
#349978=CARTESIAN_POINT('Ctrl Pts',(3.52639585899994,2.2,-1.88423335500001));
#349979=CARTESIAN_POINT('Ctrl Pts',(3.52662826599994,12.2,-1.88434346400001));
#349980=CARTESIAN_POINT('Ctrl Pts',(3.52662826599994,5.2,-1.88434346400001));
#349981=CARTESIAN_POINT('Ctrl Pts',(3.52662826599994,2.2,-1.88434346400001));
#349982=CARTESIAN_POINT('Ctrl Pts',(3.52686705399994,12.2,-1.88445620700001));
#349983=CARTESIAN_POINT('Ctrl Pts',(3.52686705399994,5.2,-1.88445620700001));
#349984=CARTESIAN_POINT('Ctrl Pts',(3.52686705399994,2.2,-1.88445620700001));
#349985=CARTESIAN_POINT('Ctrl Pts',(3.52711221799995,12.2,-1.88457156200001));
#349986=CARTESIAN_POINT('Ctrl Pts',(3.52711221799995,5.2,-1.88457156200001));
#349987=CARTESIAN_POINT('Ctrl Pts',(3.52711221799995,2.2,-1.88457156200001));
#349988=CARTESIAN_POINT('Ctrl Pts',(3.52736375099994,12.2,-1.88468950600001));
#349989=CARTESIAN_POINT('Ctrl Pts',(3.52736375099994,5.2,-1.88468950600001));
#349990=CARTESIAN_POINT('Ctrl Pts',(3.52736375099994,2.2,-1.88468950600001));
#349991=CARTESIAN_POINT('Ctrl Pts',(3.52762164799994,12.2,-1.88481001500001));
#349992=CARTESIAN_POINT('Ctrl Pts',(3.52762164799994,5.2,-1.88481001500001));
#349993=CARTESIAN_POINT('Ctrl Pts',(3.52762164799994,2.2,-1.88481001500001));
#349994=CARTESIAN_POINT('Ctrl Pts',(3.52788590099994,12.2,-1.88493306700002));
#349995=CARTESIAN_POINT('Ctrl Pts',(3.52788590099994,5.2,-1.88493306700002));
#349996=CARTESIAN_POINT('Ctrl Pts',(3.52788590099994,2.2,-1.88493306700002));
#349997=CARTESIAN_POINT('Ctrl Pts',(3.52815650599994,12.2,-1.88505864000001));
#349998=CARTESIAN_POINT('Ctrl Pts',(3.52815650599994,5.2,-1.88505864000001));
#349999=CARTESIAN_POINT('Ctrl Pts',(3.52815650599994,2.2,-1.88505864000001));
#350000=CARTESIAN_POINT('Ctrl Pts',(3.52843345499994,12.2,-1.88518671200002));
#350001=CARTESIAN_POINT('Ctrl Pts',(3.52843345499994,5.2,-1.88518671200002));
#350002=CARTESIAN_POINT('Ctrl Pts',(3.52843345499994,2.2,-1.88518671200002));
#350003=CARTESIAN_POINT('Ctrl Pts',(3.52871674199994,12.2,-1.88531725700001));
#350004=CARTESIAN_POINT('Ctrl Pts',(3.52871674199994,5.2,-1.88531725700001));
#350005=CARTESIAN_POINT('Ctrl Pts',(3.52871674199994,2.2,-1.88531725700001));
#350006=CARTESIAN_POINT('Ctrl Pts',(3.52900636199994,12.2,-1.88545025700002));
#350007=CARTESIAN_POINT('Ctrl Pts',(3.52900636199994,5.2,-1.88545025700002));
#350008=CARTESIAN_POINT('Ctrl Pts',(3.52900636199994,2.2,-1.88545025700002));
#350009=CARTESIAN_POINT('Ctrl Pts',(3.52930230799994,12.2,-1.88558568800001));
#350010=CARTESIAN_POINT('Ctrl Pts',(3.52930230799994,5.2,-1.88558568800001));
#350011=CARTESIAN_POINT('Ctrl Pts',(3.52930230799994,2.2,-1.88558568800001));
#350012=CARTESIAN_POINT('Ctrl Pts',(3.52960457399994,12.2,-1.88572352700001));
#350013=CARTESIAN_POINT('Ctrl Pts',(3.52960457399994,5.2,-1.88572352700001));
#350014=CARTESIAN_POINT('Ctrl Pts',(3.52960457399994,2.2,-1.88572352700001));
#350015=CARTESIAN_POINT('Ctrl Pts',(3.52991315199994,12.2,-1.88586375300002));
#350016=CARTESIAN_POINT('Ctrl Pts',(3.52991315199994,5.2,-1.88586375300002));
#350017=CARTESIAN_POINT('Ctrl Pts',(3.52991315199994,2.2,-1.88586375300002));
#350018=CARTESIAN_POINT('Ctrl Pts',(3.53022803899994,12.2,-1.88600634300002));
#350019=CARTESIAN_POINT('Ctrl Pts',(3.53022803899994,5.2,-1.88600634300002));
#350020=CARTESIAN_POINT('Ctrl Pts',(3.53022803899994,2.2,-1.88600634300002));
#350021=CARTESIAN_POINT('Ctrl Pts',(3.53054922599994,12.2,-1.88615127700002));
#350022=CARTESIAN_POINT('Ctrl Pts',(3.53054922599994,5.2,-1.88615127700002));
#350023=CARTESIAN_POINT('Ctrl Pts',(3.53054922599994,2.2,-1.88615127700002));
#350024=CARTESIAN_POINT('Ctrl Pts',(3.53087670799995,12.2,-1.88629853200001));
#350025=CARTESIAN_POINT('Ctrl Pts',(3.53087670799995,5.2,-1.88629853200001));
#350026=CARTESIAN_POINT('Ctrl Pts',(3.53087670799995,2.2,-1.88629853200001));
#350027=CARTESIAN_POINT('Ctrl Pts',(3.53121047799994,12.2,-1.88644808500001));
#350028=CARTESIAN_POINT('Ctrl Pts',(3.53121047799994,5.2,-1.88644808500001));
#350029=CARTESIAN_POINT('Ctrl Pts',(3.53121047799994,2.2,-1.88644808500001));
#350030=CARTESIAN_POINT('Ctrl Pts',(3.53155053099994,12.2,-1.88659991600002));
#350031=CARTESIAN_POINT('Ctrl Pts',(3.53155053099994,5.2,-1.88659991600002));
#350032=CARTESIAN_POINT('Ctrl Pts',(3.53155053099994,2.2,-1.88659991600002));
#350033=CARTESIAN_POINT('Ctrl Pts',(3.53189685999994,12.2,-1.88675400300002));
#350034=CARTESIAN_POINT('Ctrl Pts',(3.53189685999994,5.2,-1.88675400300002));
#350035=CARTESIAN_POINT('Ctrl Pts',(3.53189685999994,2.2,-1.88675400300002));
#350036=CARTESIAN_POINT('Ctrl Pts',(3.53224945799994,12.2,-1.88691032400001));
#350037=CARTESIAN_POINT('Ctrl Pts',(3.53224945799994,5.2,-1.88691032400001));
#350038=CARTESIAN_POINT('Ctrl Pts',(3.53224945799994,2.2,-1.88691032400001));
#350039=CARTESIAN_POINT('Ctrl Pts',(3.53260831999994,12.2,-1.88706885800002));
#350040=CARTESIAN_POINT('Ctrl Pts',(3.53260831999994,5.2,-1.88706885800002));
#350041=CARTESIAN_POINT('Ctrl Pts',(3.53260831999994,2.2,-1.88706885800002));
#350042=CARTESIAN_POINT('Ctrl Pts',(3.53297343799994,12.2,-1.88722958300001));
#350043=CARTESIAN_POINT('Ctrl Pts',(3.53297343799994,5.2,-1.88722958300001));
#350044=CARTESIAN_POINT('Ctrl Pts',(3.53297343799994,2.2,-1.88722958300001));
#350045=CARTESIAN_POINT('Ctrl Pts',(3.53334480699994,12.2,-1.88739247900001));
#350046=CARTESIAN_POINT('Ctrl Pts',(3.53334480699994,5.2,-1.88739247900001));
#350047=CARTESIAN_POINT('Ctrl Pts',(3.53334480699994,2.2,-1.88739247900001));
#350048=CARTESIAN_POINT('Ctrl Pts',(3.53372242199994,12.2,-1.88755752400001));
#350049=CARTESIAN_POINT('Ctrl Pts',(3.53372242199994,5.2,-1.88755752400001));
#350050=CARTESIAN_POINT('Ctrl Pts',(3.53372242199994,2.2,-1.88755752400001));
#350051=CARTESIAN_POINT('Ctrl Pts',(3.53410627399994,12.2,-1.88772469600002));
#350052=CARTESIAN_POINT('Ctrl Pts',(3.53410627399994,5.2,-1.88772469600002));
#350053=CARTESIAN_POINT('Ctrl Pts',(3.53410627399994,2.2,-1.88772469600002));
#350054=CARTESIAN_POINT('Ctrl Pts',(3.53449635899994,12.2,-1.88789397500001));
#350055=CARTESIAN_POINT('Ctrl Pts',(3.53449635899994,5.2,-1.88789397500001));
#350056=CARTESIAN_POINT('Ctrl Pts',(3.53449635899994,2.2,-1.88789397500001));
#350057=CARTESIAN_POINT('Ctrl Pts',(3.53489266999994,12.2,-1.88806533900001));
#350058=CARTESIAN_POINT('Ctrl Pts',(3.53489266999994,5.2,-1.88806533900001));
#350059=CARTESIAN_POINT('Ctrl Pts',(3.53489266999994,2.2,-1.88806533900001));
#350060=CARTESIAN_POINT('Ctrl Pts',(3.53529519999995,12.2,-1.88823876900001));
#350061=CARTESIAN_POINT('Ctrl Pts',(3.53529519999995,5.2,-1.88823876900001));
#350062=CARTESIAN_POINT('Ctrl Pts',(3.53529519999995,2.2,-1.88823876900001));
#350063=CARTESIAN_POINT('Ctrl Pts',(3.53570394199994,12.2,-1.88841424200001));
#350064=CARTESIAN_POINT('Ctrl Pts',(3.53570394199994,5.2,-1.88841424200001));
#350065=CARTESIAN_POINT('Ctrl Pts',(3.53570394199994,2.2,-1.88841424200001));
#350066=CARTESIAN_POINT('Ctrl Pts',(3.53611889099994,12.2,-1.88859173900001));
#350067=CARTESIAN_POINT('Ctrl Pts',(3.53611889099994,5.2,-1.88859173900001));
#350068=CARTESIAN_POINT('Ctrl Pts',(3.53611889099994,2.2,-1.88859173900001));
#350069=CARTESIAN_POINT('Ctrl Pts',(3.53654004199994,12.2,-1.88877123800001));
#350070=CARTESIAN_POINT('Ctrl Pts',(3.53654004199994,5.2,-1.88877123800001));
#350071=CARTESIAN_POINT('Ctrl Pts',(3.53654004199994,2.2,-1.88877123800001));
#350072=CARTESIAN_POINT('Ctrl Pts',(3.53696738599994,12.2,-1.88895271800002));
#350073=CARTESIAN_POINT('Ctrl Pts',(3.53696738599994,5.2,-1.88895271800002));
#350074=CARTESIAN_POINT('Ctrl Pts',(3.53696738599994,2.2,-1.88895271800002));
#350075=CARTESIAN_POINT('Ctrl Pts',(3.53740091799994,12.2,-1.88913616000002));
#350076=CARTESIAN_POINT('Ctrl Pts',(3.53740091799994,5.2,-1.88913616000002));
#350077=CARTESIAN_POINT('Ctrl Pts',(3.53740091799994,2.2,-1.88913616000002));
#350078=CARTESIAN_POINT('Ctrl Pts',(3.53784063199994,12.2,-1.88932154300002));
#350079=CARTESIAN_POINT('Ctrl Pts',(3.53784063199994,5.2,-1.88932154300002));
#350080=CARTESIAN_POINT('Ctrl Pts',(3.53784063199994,2.2,-1.88932154300002));
#350081=CARTESIAN_POINT('Ctrl Pts',(3.53828651899994,12.2,-1.88950884700001));
#350082=CARTESIAN_POINT('Ctrl Pts',(3.53828651899994,5.2,-1.88950884700001));
#350083=CARTESIAN_POINT('Ctrl Pts',(3.53828651899994,2.2,-1.88950884700001));
#350084=CARTESIAN_POINT('Ctrl Pts',(3.53873857699994,12.2,-1.88969805000001));
#350085=CARTESIAN_POINT('Ctrl Pts',(3.53873857699994,5.2,-1.88969805000001));
#350086=CARTESIAN_POINT('Ctrl Pts',(3.53873857699994,2.2,-1.88969805000001));
#350087=CARTESIAN_POINT('Ctrl Pts',(3.53919679799994,12.2,-1.88988913300001));
#350088=CARTESIAN_POINT('Ctrl Pts',(3.53919679799994,5.2,-1.88988913300001));
#350089=CARTESIAN_POINT('Ctrl Pts',(3.53919679799994,2.2,-1.88988913300001));
#350090=CARTESIAN_POINT('Ctrl Pts',(3.53966117399994,12.2,-1.89008207500001));
#350091=CARTESIAN_POINT('Ctrl Pts',(3.53966117399994,5.2,-1.89008207500001));
#350092=CARTESIAN_POINT('Ctrl Pts',(3.53966117399994,2.2,-1.89008207500001));
#350093=CARTESIAN_POINT('Ctrl Pts',(3.54013169999994,12.2,-1.89027685700002));
#350094=CARTESIAN_POINT('Ctrl Pts',(3.54013169999994,5.2,-1.89027685700002));
#350095=CARTESIAN_POINT('Ctrl Pts',(3.54013169999994,2.2,-1.89027685700002));
#350096=CARTESIAN_POINT('Ctrl Pts',(3.54060836999994,12.2,-1.89047345800001));
#350097=CARTESIAN_POINT('Ctrl Pts',(3.54060836999994,5.2,-1.89047345800001));
#350098=CARTESIAN_POINT('Ctrl Pts',(3.54060836999994,2.2,-1.89047345800001));
#350099=CARTESIAN_POINT('Ctrl Pts',(3.54109117699994,12.2,-1.89067186000001));
#350100=CARTESIAN_POINT('Ctrl Pts',(3.54109117699994,5.2,-1.89067186000001));
#350101=CARTESIAN_POINT('Ctrl Pts',(3.54109117699994,2.2,-1.89067186000001));
#350102=CARTESIAN_POINT('Ctrl Pts',(3.54158011499994,12.2,-1.89087203900002));
#350103=CARTESIAN_POINT('Ctrl Pts',(3.54158011499994,5.2,-1.89087203900002));
#350104=CARTESIAN_POINT('Ctrl Pts',(3.54158011499994,2.2,-1.89087203900002));
#350105=CARTESIAN_POINT('Ctrl Pts',(3.54207517599994,12.2,-1.89107397900001));
#350106=CARTESIAN_POINT('Ctrl Pts',(3.54207517599994,5.2,-1.89107397900001));
#350107=CARTESIAN_POINT('Ctrl Pts',(3.54207517599994,2.2,-1.89107397900001));
#350108=CARTESIAN_POINT('Ctrl Pts',(3.54257635599994,12.2,-1.89127765800002));
#350109=CARTESIAN_POINT('Ctrl Pts',(3.54257635599994,5.2,-1.89127765800002));
#350110=CARTESIAN_POINT('Ctrl Pts',(3.54257635599994,2.2,-1.89127765800002));
#350111=CARTESIAN_POINT('Ctrl Pts',(3.54308364899994,12.2,-1.89148305800002));
#350112=CARTESIAN_POINT('Ctrl Pts',(3.54308364899994,5.2,-1.89148305800002));
#350113=CARTESIAN_POINT('Ctrl Pts',(3.54308364899994,2.2,-1.89148305800002));
#350114=CARTESIAN_POINT('Ctrl Pts',(3.54359704599994,12.2,-1.89169015800001));
#350115=CARTESIAN_POINT('Ctrl Pts',(3.54359704599994,5.2,-1.89169015800001));
#350116=CARTESIAN_POINT('Ctrl Pts',(3.54359704599994,2.2,-1.89169015800001));
#350117=CARTESIAN_POINT('Ctrl Pts',(3.54411654299994,12.2,-1.89189893900001));
#350118=CARTESIAN_POINT('Ctrl Pts',(3.54411654299994,5.2,-1.89189893900001));
#350119=CARTESIAN_POINT('Ctrl Pts',(3.54411654299994,2.2,-1.89189893900001));
#350120=CARTESIAN_POINT('Ctrl Pts',(3.54464213099994,12.2,-1.89210938200001));
#350121=CARTESIAN_POINT('Ctrl Pts',(3.54464213099994,5.2,-1.89210938200001));
#350122=CARTESIAN_POINT('Ctrl Pts',(3.54464213099994,2.2,-1.89210938200001));
#350123=CARTESIAN_POINT('Ctrl Pts',(3.54517380599995,12.2,-1.89232146600002));
#350124=CARTESIAN_POINT('Ctrl Pts',(3.54517380599995,5.2,-1.89232146600002));
#350125=CARTESIAN_POINT('Ctrl Pts',(3.54517380599995,2.2,-1.89232146600002));
#350126=CARTESIAN_POINT('Ctrl Pts',(3.54571156199994,12.2,-1.89253517200001));
#350127=CARTESIAN_POINT('Ctrl Pts',(3.54571156199994,5.2,-1.89253517200001));
#350128=CARTESIAN_POINT('Ctrl Pts',(3.54571156199994,2.2,-1.89253517200001));
#350129=CARTESIAN_POINT('Ctrl Pts',(3.54625538999994,12.2,-1.89275048300001));
#350130=CARTESIAN_POINT('Ctrl Pts',(3.54625538999994,5.2,-1.89275048300001));
#350131=CARTESIAN_POINT('Ctrl Pts',(3.54625538999994,2.2,-1.89275048300001));
#350132=CARTESIAN_POINT('Ctrl Pts',(3.54680528599994,12.2,-1.89296737700001));
#350133=CARTESIAN_POINT('Ctrl Pts',(3.54680528599994,5.2,-1.89296737700001));
#350134=CARTESIAN_POINT('Ctrl Pts',(3.54680528599994,2.2,-1.89296737700001));
#350135=CARTESIAN_POINT('Ctrl Pts',(3.54736124099994,12.2,-1.89318583500001));
#350136=CARTESIAN_POINT('Ctrl Pts',(3.54736124099994,5.2,-1.89318583500001));
#350137=CARTESIAN_POINT('Ctrl Pts',(3.54736124099994,2.2,-1.89318583500001));
#350138=CARTESIAN_POINT('Ctrl Pts',(3.54792325099994,12.2,-1.89340584000002));
#350139=CARTESIAN_POINT('Ctrl Pts',(3.54792325099994,5.2,-1.89340584000002));
#350140=CARTESIAN_POINT('Ctrl Pts',(3.54792325099994,2.2,-1.89340584000002));
#350141=CARTESIAN_POINT('Ctrl Pts',(3.54849131099995,12.2,-1.89362737100002));
#350142=CARTESIAN_POINT('Ctrl Pts',(3.54849131099995,5.2,-1.89362737100002));
#350143=CARTESIAN_POINT('Ctrl Pts',(3.54849131099995,2.2,-1.89362737100002));
#350144=CARTESIAN_POINT('Ctrl Pts',(3.54906540999994,12.2,-1.89385041000001));
#350145=CARTESIAN_POINT('Ctrl Pts',(3.54906540999994,5.2,-1.89385041000001));
#350146=CARTESIAN_POINT('Ctrl Pts',(3.54906540999994,2.2,-1.89385041000001));
#350147=CARTESIAN_POINT('Ctrl Pts',(3.54964554499994,12.2,-1.89407493700001));
#350148=CARTESIAN_POINT('Ctrl Pts',(3.54964554499994,5.2,-1.89407493700001));
#350149=CARTESIAN_POINT('Ctrl Pts',(3.54964554499994,2.2,-1.89407493700001));
#350150=CARTESIAN_POINT('Ctrl Pts',(3.55023170899994,12.2,-1.89430093400001));
#350151=CARTESIAN_POINT('Ctrl Pts',(3.55023170899994,5.2,-1.89430093400001));
#350152=CARTESIAN_POINT('Ctrl Pts',(3.55023170899994,2.2,-1.89430093400001));
#350153=CARTESIAN_POINT('Ctrl Pts',(3.55082389399994,12.2,-1.89452838300001));
#350154=CARTESIAN_POINT('Ctrl Pts',(3.55082389399994,5.2,-1.89452838300001));
#350155=CARTESIAN_POINT('Ctrl Pts',(3.55082389399994,2.2,-1.89452838300001));
#350156=CARTESIAN_POINT('Ctrl Pts',(3.55142209599994,12.2,-1.89475726400001));
#350157=CARTESIAN_POINT('Ctrl Pts',(3.55142209599994,5.2,-1.89475726400001));
#350158=CARTESIAN_POINT('Ctrl Pts',(3.55142209599994,2.2,-1.89475726400001));
#350159=CARTESIAN_POINT('Ctrl Pts',(3.55202630799994,12.2,-1.89498755800001));
#350160=CARTESIAN_POINT('Ctrl Pts',(3.55202630799994,5.2,-1.89498755800001));
#350161=CARTESIAN_POINT('Ctrl Pts',(3.55202630799994,2.2,-1.89498755800001));
#350162=CARTESIAN_POINT('Ctrl Pts',(3.55263652199994,12.2,-1.89521924800002));
#350163=CARTESIAN_POINT('Ctrl Pts',(3.55263652199994,5.2,-1.89521924800002));
#350164=CARTESIAN_POINT('Ctrl Pts',(3.55263652199994,2.2,-1.89521924800002));
#350165=CARTESIAN_POINT('Ctrl Pts',(3.55325273199994,12.2,-1.89545231400002));
#350166=CARTESIAN_POINT('Ctrl Pts',(3.55325273199994,5.2,-1.89545231400002));
#350167=CARTESIAN_POINT('Ctrl Pts',(3.55325273199994,2.2,-1.89545231400002));
#350168=CARTESIAN_POINT('Ctrl Pts',(3.55387493299994,12.2,-1.89568673900002));
#350169=CARTESIAN_POINT('Ctrl Pts',(3.55387493299994,5.2,-1.89568673900002));
#350170=CARTESIAN_POINT('Ctrl Pts',(3.55387493299994,2.2,-1.89568673900002));
#350171=CARTESIAN_POINT('Ctrl Pts',(3.55450311699994,12.2,-1.89592250200001));
#350172=CARTESIAN_POINT('Ctrl Pts',(3.55450311699994,5.2,-1.89592250200001));
#350173=CARTESIAN_POINT('Ctrl Pts',(3.55450311699994,2.2,-1.89592250200001));
#350174=CARTESIAN_POINT('Ctrl Pts',(3.55513727899994,12.2,-1.89615958700001));
#350175=CARTESIAN_POINT('Ctrl Pts',(3.55513727899994,5.2,-1.89615958700001));
#350176=CARTESIAN_POINT('Ctrl Pts',(3.55513727899994,2.2,-1.89615958700001));
#350177=CARTESIAN_POINT('Ctrl Pts',(3.55577741199994,12.2,-1.89639797500002));
#350178=CARTESIAN_POINT('Ctrl Pts',(3.55577741199994,5.2,-1.89639797500002));
#350179=CARTESIAN_POINT('Ctrl Pts',(3.55577741199994,2.2,-1.89639797500002));
#350180=CARTESIAN_POINT('Ctrl Pts',(3.55642350799994,12.2,-1.89663764800001));
#350181=CARTESIAN_POINT('Ctrl Pts',(3.55642350799994,5.2,-1.89663764800001));
#350182=CARTESIAN_POINT('Ctrl Pts',(3.55642350799994,2.2,-1.89663764800001));
#350183=CARTESIAN_POINT('Ctrl Pts',(3.55707556299994,12.2,-1.89687858700001));
#350184=CARTESIAN_POINT('Ctrl Pts',(3.55707556299994,5.2,-1.89687858700001));
#350185=CARTESIAN_POINT('Ctrl Pts',(3.55707556299994,2.2,-1.89687858700001));
#350186=CARTESIAN_POINT('Ctrl Pts',(3.55773356999994,12.2,-1.89712077500001));
#350187=CARTESIAN_POINT('Ctrl Pts',(3.55773356999994,5.2,-1.89712077500001));
#350188=CARTESIAN_POINT('Ctrl Pts',(3.55773356999994,2.2,-1.89712077500001));
#350189=CARTESIAN_POINT('Ctrl Pts',(3.55839752099994,12.2,-1.89736419200001));
#350190=CARTESIAN_POINT('Ctrl Pts',(3.55839752099994,5.2,-1.89736419200001));
#350191=CARTESIAN_POINT('Ctrl Pts',(3.55839752099994,2.2,-1.89736419200001));
#350192=CARTESIAN_POINT('Ctrl Pts',(3.55906741099994,12.2,-1.89760882400002));
#350193=CARTESIAN_POINT('Ctrl Pts',(3.55906741099994,5.2,-1.89760882400002));
#350194=CARTESIAN_POINT('Ctrl Pts',(3.55906741099994,2.2,-1.89760882400002));
#350195=CARTESIAN_POINT('Ctrl Pts',(3.55974323299994,12.2,-1.89785464800002));
#350196=CARTESIAN_POINT('Ctrl Pts',(3.55974323299994,5.2,-1.89785464800002));
#350197=CARTESIAN_POINT('Ctrl Pts',(3.55974323299994,2.2,-1.89785464800002));
#350198=CARTESIAN_POINT('Ctrl Pts',(3.56042498099994,12.2,-1.89810164900001));
#350199=CARTESIAN_POINT('Ctrl Pts',(3.56042498099994,5.2,-1.89810164900001));
#350200=CARTESIAN_POINT('Ctrl Pts',(3.56042498099994,2.2,-1.89810164900001));
#350201=CARTESIAN_POINT('Ctrl Pts',(3.56111264699994,12.2,-1.89834981000002));
#350202=CARTESIAN_POINT('Ctrl Pts',(3.56111264699994,5.2,-1.89834981000002));
#350203=CARTESIAN_POINT('Ctrl Pts',(3.56111264699994,2.2,-1.89834981000002));
#350204=CARTESIAN_POINT('Ctrl Pts',(3.56180622499994,12.2,-1.89859911000001));
#350205=CARTESIAN_POINT('Ctrl Pts',(3.56180622499994,5.2,-1.89859911000001));
#350206=CARTESIAN_POINT('Ctrl Pts',(3.56180622499994,2.2,-1.89859911000001));
#350207=CARTESIAN_POINT('Ctrl Pts',(3.56250571199995,12.2,-1.89884953500002));
#350208=CARTESIAN_POINT('Ctrl Pts',(3.56250571199995,5.2,-1.89884953500002));
#350209=CARTESIAN_POINT('Ctrl Pts',(3.56250571199995,2.2,-1.89884953500002));
#350210=CARTESIAN_POINT('Ctrl Pts',(3.56321109699994,12.2,-1.89910106400001));
#350211=CARTESIAN_POINT('Ctrl Pts',(3.56321109699994,5.2,-1.89910106400001));
#350212=CARTESIAN_POINT('Ctrl Pts',(3.56321109699994,2.2,-1.89910106400001));
#350213=CARTESIAN_POINT('Ctrl Pts',(3.56392237499994,12.2,-1.89935368300001));
#350214=CARTESIAN_POINT('Ctrl Pts',(3.56392237499994,5.2,-1.89935368300001));
#350215=CARTESIAN_POINT('Ctrl Pts',(3.56392237499994,2.2,-1.89935368300001));
#350216=CARTESIAN_POINT('Ctrl Pts',(3.56463954099994,12.2,-1.89960737100002));
#350217=CARTESIAN_POINT('Ctrl Pts',(3.56463954099994,5.2,-1.89960737100002));
#350218=CARTESIAN_POINT('Ctrl Pts',(3.56463954099994,2.2,-1.89960737100002));
#350219=CARTESIAN_POINT('Ctrl Pts',(3.56536258599994,12.2,-1.89986211300001));
#350220=CARTESIAN_POINT('Ctrl Pts',(3.56536258599994,5.2,-1.89986211300001));
#350221=CARTESIAN_POINT('Ctrl Pts',(3.56536258599994,2.2,-1.89986211300001));
#350222=CARTESIAN_POINT('Ctrl Pts',(3.56609150599994,12.2,-1.90011789000001));
#350223=CARTESIAN_POINT('Ctrl Pts',(3.56609150599994,5.2,-1.90011789000001));
#350224=CARTESIAN_POINT('Ctrl Pts',(3.56609150599994,2.2,-1.90011789000001));
#350225=CARTESIAN_POINT('Ctrl Pts',(3.56682629199994,12.2,-1.90037468600002));
#350226=CARTESIAN_POINT('Ctrl Pts',(3.56682629199994,5.2,-1.90037468600002));
#350227=CARTESIAN_POINT('Ctrl Pts',(3.56682629199994,2.2,-1.90037468600002));
#350228=CARTESIAN_POINT('Ctrl Pts',(3.56756693899994,12.2,-1.90063248200001));
#350229=CARTESIAN_POINT('Ctrl Pts',(3.56756693899994,5.2,-1.90063248200001));
#350230=CARTESIAN_POINT('Ctrl Pts',(3.56756693899994,2.2,-1.90063248200001));
#350231=CARTESIAN_POINT('Ctrl Pts',(3.56831343999994,12.2,-1.90089126100002));
#350232=CARTESIAN_POINT('Ctrl Pts',(3.56831343999994,5.2,-1.90089126100002));
#350233=CARTESIAN_POINT('Ctrl Pts',(3.56831343999994,2.2,-1.90089126100002));
#350234=CARTESIAN_POINT('Ctrl Pts',(3.56906578999994,12.2,-1.90115100800002));
#350235=CARTESIAN_POINT('Ctrl Pts',(3.56906578999994,5.2,-1.90115100800002));
#350236=CARTESIAN_POINT('Ctrl Pts',(3.56906578999994,2.2,-1.90115100800002));
#350237=CARTESIAN_POINT('Ctrl Pts',(3.56982398099994,12.2,-1.90141170400001));
#350238=CARTESIAN_POINT('Ctrl Pts',(3.56982398099994,5.2,-1.90141170400001));
#350239=CARTESIAN_POINT('Ctrl Pts',(3.56982398099994,2.2,-1.90141170400001));
#350240=CARTESIAN_POINT('Ctrl Pts',(3.57058800599994,12.2,-1.90167333200002));
#350241=CARTESIAN_POINT('Ctrl Pts',(3.57058800599994,5.2,-1.90167333200002));
#350242=CARTESIAN_POINT('Ctrl Pts',(3.57058800599994,2.2,-1.90167333200002));
#350243=CARTESIAN_POINT('Ctrl Pts',(3.57135785899994,12.2,-1.90193587500001));
#350244=CARTESIAN_POINT('Ctrl Pts',(3.57135785899994,5.2,-1.90193587500001));
#350245=CARTESIAN_POINT('Ctrl Pts',(3.57135785899994,2.2,-1.90193587500001));
#350246=CARTESIAN_POINT('Ctrl Pts',(3.57213353499994,12.2,-1.90219931700002));
#350247=CARTESIAN_POINT('Ctrl Pts',(3.57213353499994,5.2,-1.90219931700002));
#350248=CARTESIAN_POINT('Ctrl Pts',(3.57213353499994,2.2,-1.90219931700002));
#350249=CARTESIAN_POINT('Ctrl Pts',(3.57291502499994,12.2,-1.90246364000001));
#350250=CARTESIAN_POINT('Ctrl Pts',(3.57291502499994,5.2,-1.90246364000001));
#350251=CARTESIAN_POINT('Ctrl Pts',(3.57291502499994,2.2,-1.90246364000001));
#350252=CARTESIAN_POINT('Ctrl Pts',(3.57370232399994,12.2,-1.90272882600001));
#350253=CARTESIAN_POINT('Ctrl Pts',(3.57370232399994,5.2,-1.90272882600001));
#350254=CARTESIAN_POINT('Ctrl Pts',(3.57370232399994,2.2,-1.90272882600001));
#350255=CARTESIAN_POINT('Ctrl Pts',(3.57449542499995,12.2,-1.90299486200002));
#350256=CARTESIAN_POINT('Ctrl Pts',(3.57449542499995,5.2,-1.90299486200002));
#350257=CARTESIAN_POINT('Ctrl Pts',(3.57449542499995,2.2,-1.90299486200002));
#350258=CARTESIAN_POINT('Ctrl Pts',(3.57529432199994,12.2,-1.90326172800001));
#350259=CARTESIAN_POINT('Ctrl Pts',(3.57529432199994,5.2,-1.90326172800001));
#350260=CARTESIAN_POINT('Ctrl Pts',(3.57529432199994,2.2,-1.90326172800001));
#350261=CARTESIAN_POINT('Ctrl Pts',(3.57609900899994,12.2,-1.90352940700001));
#350262=CARTESIAN_POINT('Ctrl Pts',(3.57609900899994,5.2,-1.90352940700001));
#350263=CARTESIAN_POINT('Ctrl Pts',(3.57609900899994,2.2,-1.90352940700001));
#350264=CARTESIAN_POINT('Ctrl Pts',(3.57690947699994,12.2,-1.90379788500001));
#350265=CARTESIAN_POINT('Ctrl Pts',(3.57690947699994,5.2,-1.90379788500001));
#350266=CARTESIAN_POINT('Ctrl Pts',(3.57690947699994,2.2,-1.90379788500001));
#350267=CARTESIAN_POINT('Ctrl Pts',(3.57772572199994,12.2,-1.90406714400002));
#350268=CARTESIAN_POINT('Ctrl Pts',(3.57772572199994,5.2,-1.90406714400002));
#350269=CARTESIAN_POINT('Ctrl Pts',(3.57772572199994,2.2,-1.90406714400002));
#350270=CARTESIAN_POINT('Ctrl Pts',(3.57854773599994,12.2,-1.90433716600001));
#350271=CARTESIAN_POINT('Ctrl Pts',(3.57854773599994,5.2,-1.90433716600001));
#350272=CARTESIAN_POINT('Ctrl Pts',(3.57854773599994,2.2,-1.90433716600001));
#350273=CARTESIAN_POINT('Ctrl Pts',(3.57937551199994,12.2,-1.90460793700002));
#350274=CARTESIAN_POINT('Ctrl Pts',(3.57937551199994,5.2,-1.90460793700002));
#350275=CARTESIAN_POINT('Ctrl Pts',(3.57937551199994,2.2,-1.90460793700002));
#350276=CARTESIAN_POINT('Ctrl Pts',(3.58020904499994,12.2,-1.90487943900001));
#350277=CARTESIAN_POINT('Ctrl Pts',(3.58020904499994,5.2,-1.90487943900001));
#350278=CARTESIAN_POINT('Ctrl Pts',(3.58020904499994,2.2,-1.90487943900001));
#350279=CARTESIAN_POINT('Ctrl Pts',(3.58104832799994,12.2,-1.90515165700001));
#350280=CARTESIAN_POINT('Ctrl Pts',(3.58104832799994,5.2,-1.90515165700001));
#350281=CARTESIAN_POINT('Ctrl Pts',(3.58104832799994,2.2,-1.90515165700001));
#350282=CARTESIAN_POINT('Ctrl Pts',(3.58189335499994,12.2,-1.90542457200001));
#350283=CARTESIAN_POINT('Ctrl Pts',(3.58189335499994,5.2,-1.90542457200001));
#350284=CARTESIAN_POINT('Ctrl Pts',(3.58189335499994,2.2,-1.90542457200001));
#350285=CARTESIAN_POINT('Ctrl Pts',(3.58274411699994,12.2,-1.90569817000001));
#350286=CARTESIAN_POINT('Ctrl Pts',(3.58274411699994,5.2,-1.90569817000001));
#350287=CARTESIAN_POINT('Ctrl Pts',(3.58274411699994,2.2,-1.90569817000001));
#350288=CARTESIAN_POINT('Ctrl Pts',(3.58360060999994,12.2,-1.90597243600001));
#350289=CARTESIAN_POINT('Ctrl Pts',(3.58360060999994,5.2,-1.90597243600001));
#350290=CARTESIAN_POINT('Ctrl Pts',(3.58360060999994,2.2,-1.90597243600001));
#350291=CARTESIAN_POINT('Ctrl Pts',(3.58446282799994,12.2,-1.90624734900001));
#350292=CARTESIAN_POINT('Ctrl Pts',(3.58446282799994,5.2,-1.90624734900001));
#350293=CARTESIAN_POINT('Ctrl Pts',(3.58446282799994,2.2,-1.90624734900001));
#350294=CARTESIAN_POINT('Ctrl Pts',(3.58533076099994,12.2,-1.90652289800001));
#350295=CARTESIAN_POINT('Ctrl Pts',(3.58533076099994,5.2,-1.90652289800001));
#350296=CARTESIAN_POINT('Ctrl Pts',(3.58533076099994,2.2,-1.90652289800001));
#350297=CARTESIAN_POINT('Ctrl Pts',(3.58620440499994,12.2,-1.90679906400002));
#350298=CARTESIAN_POINT('Ctrl Pts',(3.58620440499994,5.2,-1.90679906400002));
#350299=CARTESIAN_POINT('Ctrl Pts',(3.58620440499994,2.2,-1.90679906400002));
#350300=CARTESIAN_POINT('Ctrl Pts',(3.58708375299994,12.2,-1.90707583300001));
#350301=CARTESIAN_POINT('Ctrl Pts',(3.58708375299994,5.2,-1.90707583300001));
#350302=CARTESIAN_POINT('Ctrl Pts',(3.58708375299994,2.2,-1.90707583300001));
#350303=CARTESIAN_POINT('Ctrl Pts',(3.58796879799994,12.2,-1.90735318600002));
#350304=CARTESIAN_POINT('Ctrl Pts',(3.58796879799994,5.2,-1.90735318600002));
#350305=CARTESIAN_POINT('Ctrl Pts',(3.58796879799994,2.2,-1.90735318600002));
#350306=CARTESIAN_POINT('Ctrl Pts',(3.58885953399994,12.2,-1.90763110900001));
#350307=CARTESIAN_POINT('Ctrl Pts',(3.58885953399994,5.2,-1.90763110900001));
#350308=CARTESIAN_POINT('Ctrl Pts',(3.58885953399994,2.2,-1.90763110900001));
#350309=CARTESIAN_POINT('Ctrl Pts',(3.58975595399994,12.2,-1.90790958700001));
#350310=CARTESIAN_POINT('Ctrl Pts',(3.58975595399994,5.2,-1.90790958700001));
#350311=CARTESIAN_POINT('Ctrl Pts',(3.58975595399994,2.2,-1.90790958700001));
#350312=CARTESIAN_POINT('Ctrl Pts',(3.59065805099994,12.2,-1.90818860300002));
#350313=CARTESIAN_POINT('Ctrl Pts',(3.59065805099994,5.2,-1.90818860300002));
#350314=CARTESIAN_POINT('Ctrl Pts',(3.59065805099994,2.2,-1.90818860300002));
#350315=CARTESIAN_POINT('Ctrl Pts',(3.59156581999994,12.2,-1.90846814100002));
#350316=CARTESIAN_POINT('Ctrl Pts',(3.59156581999994,5.2,-1.90846814100002));
#350317=CARTESIAN_POINT('Ctrl Pts',(3.59156581999994,2.2,-1.90846814100002));
#350318=CARTESIAN_POINT('Ctrl Pts',(3.59247925199994,12.2,-1.90874818500001));
#350319=CARTESIAN_POINT('Ctrl Pts',(3.59247925199994,5.2,-1.90874818500001));
#350320=CARTESIAN_POINT('Ctrl Pts',(3.59247925199994,2.2,-1.90874818500001));
#350321=CARTESIAN_POINT('Ctrl Pts',(3.59339834299994,12.2,-1.90902872000001));
#350322=CARTESIAN_POINT('Ctrl Pts',(3.59339834299994,5.2,-1.90902872000001));
#350323=CARTESIAN_POINT('Ctrl Pts',(3.59339834299994,2.2,-1.90902872000001));
#350324=CARTESIAN_POINT('Ctrl Pts',(3.59432308499994,12.2,-1.90930973100001));
#350325=CARTESIAN_POINT('Ctrl Pts',(3.59432308499994,5.2,-1.90930973100001));
#350326=CARTESIAN_POINT('Ctrl Pts',(3.59432308499994,2.2,-1.90930973100001));
#350327=CARTESIAN_POINT('Ctrl Pts',(3.59525347199994,12.2,-1.90959120200001));
#350328=CARTESIAN_POINT('Ctrl Pts',(3.59525347199994,5.2,-1.90959120200001));
#350329=CARTESIAN_POINT('Ctrl Pts',(3.59525347199994,2.2,-1.90959120200001));
#350330=CARTESIAN_POINT('Ctrl Pts',(3.59618949499994,12.2,-1.90987311600002));
#350331=CARTESIAN_POINT('Ctrl Pts',(3.59618949499994,5.2,-1.90987311600002));
#350332=CARTESIAN_POINT('Ctrl Pts',(3.59618949499994,2.2,-1.90987311600002));
#350333=CARTESIAN_POINT('Ctrl Pts',(3.59713115099995,12.2,-1.91015545800001));
#350334=CARTESIAN_POINT('Ctrl Pts',(3.59713115099995,5.2,-1.91015545800001));
#350335=CARTESIAN_POINT('Ctrl Pts',(3.59713115099995,2.2,-1.91015545800001));
#350336=CARTESIAN_POINT('Ctrl Pts',(3.59807843099994,12.2,-1.91043821500001));
#350337=CARTESIAN_POINT('Ctrl Pts',(3.59807843099994,5.2,-1.91043821500001));
#350338=CARTESIAN_POINT('Ctrl Pts',(3.59807843099994,2.2,-1.91043821500001));
#350339=CARTESIAN_POINT('Ctrl Pts',(3.59903132999994,12.2,-1.91072136800001));
#350340=CARTESIAN_POINT('Ctrl Pts',(3.59903132999994,5.2,-1.91072136800001));
#350341=CARTESIAN_POINT('Ctrl Pts',(3.59903132999994,2.2,-1.91072136800001));
#350342=CARTESIAN_POINT('Ctrl Pts',(3.59998983999994,12.2,-1.91100490500002));
#350343=CARTESIAN_POINT('Ctrl Pts',(3.59998983999994,5.2,-1.91100490500002));
#350344=CARTESIAN_POINT('Ctrl Pts',(3.59998983999994,2.2,-1.91100490500002));
#350345=CARTESIAN_POINT('Ctrl Pts',(3.60095395499994,12.2,-1.91128880900001));
#350346=CARTESIAN_POINT('Ctrl Pts',(3.60095395499994,5.2,-1.91128880900001));
#350347=CARTESIAN_POINT('Ctrl Pts',(3.60095395499994,2.2,-1.91128880900001));
#350348=CARTESIAN_POINT('Ctrl Pts',(3.60192366899994,12.2,-1.91157306400001));
#350349=CARTESIAN_POINT('Ctrl Pts',(3.60192366899994,5.2,-1.91157306400001));
#350350=CARTESIAN_POINT('Ctrl Pts',(3.60192366899994,2.2,-1.91157306400001));
#350351=CARTESIAN_POINT('Ctrl Pts',(3.60289897299995,12.2,-1.91185765600002));
#350352=CARTESIAN_POINT('Ctrl Pts',(3.60289897299995,5.2,-1.91185765600002));
#350353=CARTESIAN_POINT('Ctrl Pts',(3.60289897299995,2.2,-1.91185765600002));
#350354=CARTESIAN_POINT('Ctrl Pts',(3.60387986299994,12.2,-1.91214256900002));
#350355=CARTESIAN_POINT('Ctrl Pts',(3.60387986299994,5.2,-1.91214256900002));
#350356=CARTESIAN_POINT('Ctrl Pts',(3.60387986299994,2.2,-1.91214256900002));
#350357=CARTESIAN_POINT('Ctrl Pts',(3.60486633099994,12.2,-1.91242778900001));
#350358=CARTESIAN_POINT('Ctrl Pts',(3.60486633099994,5.2,-1.91242778900001));
#350359=CARTESIAN_POINT('Ctrl Pts',(3.60486633099994,2.2,-1.91242778900001));
#350360=CARTESIAN_POINT('Ctrl Pts',(3.60585837199995,12.2,-1.91271330000002));
#350361=CARTESIAN_POINT('Ctrl Pts',(3.60585837199995,5.2,-1.91271330000002));
#350362=CARTESIAN_POINT('Ctrl Pts',(3.60585837199995,2.2,-1.91271330000002));
#350363=CARTESIAN_POINT('Ctrl Pts',(3.60685597699994,12.2,-1.91299908700001));
#350364=CARTESIAN_POINT('Ctrl Pts',(3.60685597699994,5.2,-1.91299908700001));
#350365=CARTESIAN_POINT('Ctrl Pts',(3.60685597699994,2.2,-1.91299908700001));
#350366=CARTESIAN_POINT('Ctrl Pts',(3.60785914099994,12.2,-1.91328513500002));
#350367=CARTESIAN_POINT('Ctrl Pts',(3.60785914099994,5.2,-1.91328513500002));
#350368=CARTESIAN_POINT('Ctrl Pts',(3.60785914099994,2.2,-1.91328513500002));
#350369=CARTESIAN_POINT('Ctrl Pts',(3.60886785599994,12.2,-1.91357143000001));
#350370=CARTESIAN_POINT('Ctrl Pts',(3.60886785599994,5.2,-1.91357143000001));
#350371=CARTESIAN_POINT('Ctrl Pts',(3.60886785599994,2.2,-1.91357143000001));
#350372=CARTESIAN_POINT('Ctrl Pts',(3.60988211699994,12.2,-1.91385795700001));
#350373=CARTESIAN_POINT('Ctrl Pts',(3.60988211699994,5.2,-1.91385795700001));
#350374=CARTESIAN_POINT('Ctrl Pts',(3.60988211699994,2.2,-1.91385795700001));
#350375=CARTESIAN_POINT('Ctrl Pts',(3.61090191699994,12.2,-1.91414470000002));
#350376=CARTESIAN_POINT('Ctrl Pts',(3.61090191699994,5.2,-1.91414470000002));
#350377=CARTESIAN_POINT('Ctrl Pts',(3.61090191699994,2.2,-1.91414470000002));
#350378=CARTESIAN_POINT('Ctrl Pts',(3.61192724899994,12.2,-1.91443164400001));
#350379=CARTESIAN_POINT('Ctrl Pts',(3.61192724899994,5.2,-1.91443164400001));
#350380=CARTESIAN_POINT('Ctrl Pts',(3.61192724899994,2.2,-1.91443164400001));
#350381=CARTESIAN_POINT('Ctrl Pts',(3.61295810599994,12.2,-1.91471877600002));
#350382=CARTESIAN_POINT('Ctrl Pts',(3.61295810599994,5.2,-1.91471877600002));
#350383=CARTESIAN_POINT('Ctrl Pts',(3.61295810599994,2.2,-1.91471877600002));
#350384=CARTESIAN_POINT('Ctrl Pts',(3.61399448099994,12.2,-1.91500608000001));
#350385=CARTESIAN_POINT('Ctrl Pts',(3.61399448099994,5.2,-1.91500608000001));
#350386=CARTESIAN_POINT('Ctrl Pts',(3.61399448099994,2.2,-1.91500608000001));
#350387=CARTESIAN_POINT('Ctrl Pts',(3.61503636899994,12.2,-1.91529354200001));
#350388=CARTESIAN_POINT('Ctrl Pts',(3.61503636899994,5.2,-1.91529354200001));
#350389=CARTESIAN_POINT('Ctrl Pts',(3.61503636899994,2.2,-1.91529354200001));
#350390=CARTESIAN_POINT('Ctrl Pts',(3.61608376199994,12.2,-1.91558114600001));
#350391=CARTESIAN_POINT('Ctrl Pts',(3.61608376199994,5.2,-1.91558114600001));
#350392=CARTESIAN_POINT('Ctrl Pts',(3.61608376199994,2.2,-1.91558114600001));
#350393=CARTESIAN_POINT('Ctrl Pts',(3.61713665199995,12.2,-1.91586887900002));
#350394=CARTESIAN_POINT('Ctrl Pts',(3.61713665199995,5.2,-1.91586887900002));
#350395=CARTESIAN_POINT('Ctrl Pts',(3.61713665199995,2.2,-1.91586887900002));
#350396=CARTESIAN_POINT('Ctrl Pts',(3.61819503599994,12.2,-1.91615672600001));
#350397=CARTESIAN_POINT('Ctrl Pts',(3.61819503599994,5.2,-1.91615672600001));
#350398=CARTESIAN_POINT('Ctrl Pts',(3.61819503599994,2.2,-1.91615672600001));
#350399=CARTESIAN_POINT('Ctrl Pts',(3.61925890499994,12.2,-1.91644467300002));
#350400=CARTESIAN_POINT('Ctrl Pts',(3.61925890499994,5.2,-1.91644467300002));
#350401=CARTESIAN_POINT('Ctrl Pts',(3.61925890499994,2.2,-1.91644467300002));
#350402=CARTESIAN_POINT('Ctrl Pts',(3.62032825299994,12.2,-1.91673270400001));
#350403=CARTESIAN_POINT('Ctrl Pts',(3.62032825299994,5.2,-1.91673270400001));
#350404=CARTESIAN_POINT('Ctrl Pts',(3.62032825299994,2.2,-1.91673270400001));
#350405=CARTESIAN_POINT('Ctrl Pts',(3.62140307199994,12.2,-1.91702080600002));
#350406=CARTESIAN_POINT('Ctrl Pts',(3.62140307199994,5.2,-1.91702080600002));
#350407=CARTESIAN_POINT('Ctrl Pts',(3.62140307199994,2.2,-1.91702080600002));
#350408=CARTESIAN_POINT('Ctrl Pts',(3.62248335699995,12.2,-1.91730896300002));
#350409=CARTESIAN_POINT('Ctrl Pts',(3.62248335699995,5.2,-1.91730896300002));
#350410=CARTESIAN_POINT('Ctrl Pts',(3.62248335699995,2.2,-1.91730896300002));
#350411=CARTESIAN_POINT('Ctrl Pts',(3.62356910199995,12.2,-1.91759716300002));
#350412=CARTESIAN_POINT('Ctrl Pts',(3.62356910199995,5.2,-1.91759716300002));
#350413=CARTESIAN_POINT('Ctrl Pts',(3.62356910199995,2.2,-1.91759716300002));
#350414=CARTESIAN_POINT('Ctrl Pts',(3.62466029599994,12.2,-1.91788539100001));
#350415=CARTESIAN_POINT('Ctrl Pts',(3.62466029599994,5.2,-1.91788539100001));
#350416=CARTESIAN_POINT('Ctrl Pts',(3.62466029599994,2.2,-1.91788539100001));
#350417=CARTESIAN_POINT('Ctrl Pts',(3.62575693799994,12.2,-1.91817363200002));
#350418=CARTESIAN_POINT('Ctrl Pts',(3.62575693799994,5.2,-1.91817363200002));
#350419=CARTESIAN_POINT('Ctrl Pts',(3.62575693799994,2.2,-1.91817363200002));
#350420=CARTESIAN_POINT('Ctrl Pts',(3.62685901799995,12.2,-1.91846187200001));
#350421=CARTESIAN_POINT('Ctrl Pts',(3.62685901799995,5.2,-1.91846187200001));
#350422=CARTESIAN_POINT('Ctrl Pts',(3.62685901799995,2.2,-1.91846187200001));
#350423=CARTESIAN_POINT('Ctrl Pts',(3.62796652899994,12.2,-1.91875009700002));
#350424=CARTESIAN_POINT('Ctrl Pts',(3.62796652899994,5.2,-1.91875009700002));
#350425=CARTESIAN_POINT('Ctrl Pts',(3.62796652899994,2.2,-1.91875009700002));
#350426=CARTESIAN_POINT('Ctrl Pts',(3.62907946699994,12.2,-1.91903829300001));
#350427=CARTESIAN_POINT('Ctrl Pts',(3.62907946699994,5.2,-1.91903829300001));
#350428=CARTESIAN_POINT('Ctrl Pts',(3.62907946699994,2.2,-1.91903829300001));
#350429=CARTESIAN_POINT('Ctrl Pts',(3.63019782199994,12.2,-1.91932644600001));
#350430=CARTESIAN_POINT('Ctrl Pts',(3.63019782199994,5.2,-1.91932644600001));
#350431=CARTESIAN_POINT('Ctrl Pts',(3.63019782199994,2.2,-1.91932644600001));
#350432=CARTESIAN_POINT('Ctrl Pts',(3.63132158899994,12.2,-1.91961454100001));
#350433=CARTESIAN_POINT('Ctrl Pts',(3.63132158899994,5.2,-1.91961454100001));
#350434=CARTESIAN_POINT('Ctrl Pts',(3.63132158899994,2.2,-1.91961454100001));
#350435=CARTESIAN_POINT('Ctrl Pts',(3.63245076099994,12.2,-1.91990256600001));
#350436=CARTESIAN_POINT('Ctrl Pts',(3.63245076099994,5.2,-1.91990256600001));
#350437=CARTESIAN_POINT('Ctrl Pts',(3.63245076099994,2.2,-1.91990256600001));
#350438=CARTESIAN_POINT('Ctrl Pts',(3.63358533199994,12.2,-1.92019050500001));
#350439=CARTESIAN_POINT('Ctrl Pts',(3.63358533199994,5.2,-1.92019050500001));
#350440=CARTESIAN_POINT('Ctrl Pts',(3.63358533199994,2.2,-1.92019050500001));
#350441=CARTESIAN_POINT('Ctrl Pts',(3.63472529599994,12.2,-1.92047834600002));
#350442=CARTESIAN_POINT('Ctrl Pts',(3.63472529599994,5.2,-1.92047834600002));
#350443=CARTESIAN_POINT('Ctrl Pts',(3.63472529599994,2.2,-1.92047834600002));
#350444=CARTESIAN_POINT('Ctrl Pts',(3.63587064399994,12.2,-1.92076607300002));
#350445=CARTESIAN_POINT('Ctrl Pts',(3.63587064399994,5.2,-1.92076607300002));
#350446=CARTESIAN_POINT('Ctrl Pts',(3.63587064399994,2.2,-1.92076607300002));
#350447=CARTESIAN_POINT('Ctrl Pts',(3.63702136999994,12.2,-1.92105367400002));
#350448=CARTESIAN_POINT('Ctrl Pts',(3.63702136999994,5.2,-1.92105367400002));
#350449=CARTESIAN_POINT('Ctrl Pts',(3.63702136999994,2.2,-1.92105367400002));
#350450=CARTESIAN_POINT('Ctrl Pts',(3.63817746799994,12.2,-1.92134113500002));
#350451=CARTESIAN_POINT('Ctrl Pts',(3.63817746799994,5.2,-1.92134113500002));
#350452=CARTESIAN_POINT('Ctrl Pts',(3.63817746799994,2.2,-1.92134113500002));
#350453=CARTESIAN_POINT('Ctrl Pts',(3.63933893199994,12.2,-1.92162844100002));
#350454=CARTESIAN_POINT('Ctrl Pts',(3.63933893199994,5.2,-1.92162844100002));
#350455=CARTESIAN_POINT('Ctrl Pts',(3.63933893199994,2.2,-1.92162844100002));
#350456=CARTESIAN_POINT('Ctrl Pts',(3.64050575399994,12.2,-1.92191557900002));
#350457=CARTESIAN_POINT('Ctrl Pts',(3.64050575399994,5.2,-1.92191557900002));
#350458=CARTESIAN_POINT('Ctrl Pts',(3.64050575399994,2.2,-1.92191557900002));
#350459=CARTESIAN_POINT('Ctrl Pts',(3.64167792599994,12.2,-1.92220253500002));
#350460=CARTESIAN_POINT('Ctrl Pts',(3.64167792599994,5.2,-1.92220253500002));
#350461=CARTESIAN_POINT('Ctrl Pts',(3.64167792599994,2.2,-1.92220253500002));
#350462=CARTESIAN_POINT('Ctrl Pts',(3.64285544499994,12.2,-1.92248929700002));
#350463=CARTESIAN_POINT('Ctrl Pts',(3.64285544499994,5.2,-1.92248929700002));
#350464=CARTESIAN_POINT('Ctrl Pts',(3.64285544499994,2.2,-1.92248929700002));
#350465=CARTESIAN_POINT('Ctrl Pts',(3.64403829999994,12.2,-1.92277585000001));
#350466=CARTESIAN_POINT('Ctrl Pts',(3.64403829999994,5.2,-1.92277585000001));
#350467=CARTESIAN_POINT('Ctrl Pts',(3.64403829999994,2.2,-1.92277585000001));
#350468=CARTESIAN_POINT('Ctrl Pts',(3.64522648799994,12.2,-1.92306218100001));
#350469=CARTESIAN_POINT('Ctrl Pts',(3.64522648799994,5.2,-1.92306218100001));
#350470=CARTESIAN_POINT('Ctrl Pts',(3.64522648799994,2.2,-1.92306218100001));
#350471=CARTESIAN_POINT('Ctrl Pts',(3.64641999999994,12.2,-1.92334827500002));
#350472=CARTESIAN_POINT('Ctrl Pts',(3.64641999999994,5.2,-1.92334827500002));
#350473=CARTESIAN_POINT('Ctrl Pts',(3.64641999999994,2.2,-1.92334827500002));
#350474=CARTESIAN_POINT('Ctrl Pts',(3.64761883099994,12.2,-1.92363412100002));
#350475=CARTESIAN_POINT('Ctrl Pts',(3.64761883099994,5.2,-1.92363412100002));
#350476=CARTESIAN_POINT('Ctrl Pts',(3.64761883099994,2.2,-1.92363412100002));
#350477=CARTESIAN_POINT('Ctrl Pts',(3.64882297099994,12.2,-1.92391970400001));
#350478=CARTESIAN_POINT('Ctrl Pts',(3.64882297099994,5.2,-1.92391970400001));
#350479=CARTESIAN_POINT('Ctrl Pts',(3.64882297099994,2.2,-1.92391970400001));
#350480=CARTESIAN_POINT('Ctrl Pts',(3.65003241699994,12.2,-1.92420501000001));
#350481=CARTESIAN_POINT('Ctrl Pts',(3.65003241699994,5.2,-1.92420501000001));
#350482=CARTESIAN_POINT('Ctrl Pts',(3.65003241699994,2.2,-1.92420501000001));
#350483=CARTESIAN_POINT('Ctrl Pts',(3.65124716099994,12.2,-1.92449002800001));
#350484=CARTESIAN_POINT('Ctrl Pts',(3.65124716099994,5.2,-1.92449002800001));
#350485=CARTESIAN_POINT('Ctrl Pts',(3.65124716099994,2.2,-1.92449002800001));
#350486=CARTESIAN_POINT('Ctrl Pts',(3.65246719699994,12.2,-1.92477474300001));
#350487=CARTESIAN_POINT('Ctrl Pts',(3.65246719699994,5.2,-1.92477474300001));
#350488=CARTESIAN_POINT('Ctrl Pts',(3.65246719699994,2.2,-1.92477474300001));
#350489=CARTESIAN_POINT('Ctrl Pts',(3.65369251599994,12.2,-1.92505914200002));
#350490=CARTESIAN_POINT('Ctrl Pts',(3.65369251599994,5.2,-1.92505914200002));
#350491=CARTESIAN_POINT('Ctrl Pts',(3.65369251599994,2.2,-1.92505914200002));
#350492=CARTESIAN_POINT('Ctrl Pts',(3.65492311299994,12.2,-1.92534321200001));
#350493=CARTESIAN_POINT('Ctrl Pts',(3.65492311299994,5.2,-1.92534321200001));
#350494=CARTESIAN_POINT('Ctrl Pts',(3.65492311299994,2.2,-1.92534321200001));
#350495=CARTESIAN_POINT('Ctrl Pts',(3.65615898099994,12.2,-1.92562693900001));
#350496=CARTESIAN_POINT('Ctrl Pts',(3.65615898099994,5.2,-1.92562693900001));
#350497=CARTESIAN_POINT('Ctrl Pts',(3.65615898099994,2.2,-1.92562693900001));
#350498=CARTESIAN_POINT('Ctrl Pts',(3.65740011199994,12.2,-1.92591031100001));
#350499=CARTESIAN_POINT('Ctrl Pts',(3.65740011199994,5.2,-1.92591031100001));
#350500=CARTESIAN_POINT('Ctrl Pts',(3.65740011199994,2.2,-1.92591031100001));
#350501=CARTESIAN_POINT('Ctrl Pts',(3.65864650099994,12.2,-1.92619331400001));
#350502=CARTESIAN_POINT('Ctrl Pts',(3.65864650099994,5.2,-1.92619331400001));
#350503=CARTESIAN_POINT('Ctrl Pts',(3.65864650099994,2.2,-1.92619331400001));
#350504=CARTESIAN_POINT('Ctrl Pts',(3.65989814199994,12.2,-1.92647593600002));
#350505=CARTESIAN_POINT('Ctrl Pts',(3.65989814199994,5.2,-1.92647593600002));
#350506=CARTESIAN_POINT('Ctrl Pts',(3.65989814199994,2.2,-1.92647593600002));
#350507=CARTESIAN_POINT('Ctrl Pts',(3.66115502599994,12.2,-1.92675816300001));
#350508=CARTESIAN_POINT('Ctrl Pts',(3.66115502599994,5.2,-1.92675816300001));
#350509=CARTESIAN_POINT('Ctrl Pts',(3.66115502599994,2.2,-1.92675816300001));
#350510=CARTESIAN_POINT('Ctrl Pts',(3.66241714699994,12.2,-1.92703998200002));
#350511=CARTESIAN_POINT('Ctrl Pts',(3.66241714699994,5.2,-1.92703998200002));
#350512=CARTESIAN_POINT('Ctrl Pts',(3.66241714699994,2.2,-1.92703998200002));
#350513=CARTESIAN_POINT('Ctrl Pts',(3.66368449699995,12.2,-1.92732138100002));
#350514=CARTESIAN_POINT('Ctrl Pts',(3.66368449699995,5.2,-1.92732138100002));
#350515=CARTESIAN_POINT('Ctrl Pts',(3.66368449699995,2.2,-1.92732138100002));
#350516=CARTESIAN_POINT('Ctrl Pts',(3.66495707299994,12.2,-1.92760234600001));
#350517=CARTESIAN_POINT('Ctrl Pts',(3.66495707299994,5.2,-1.92760234600001));
#350518=CARTESIAN_POINT('Ctrl Pts',(3.66495707299994,2.2,-1.92760234600001));
#350519=CARTESIAN_POINT('Ctrl Pts',(3.66623486499994,12.2,-1.92788286500001));
#350520=CARTESIAN_POINT('Ctrl Pts',(3.66623486499994,5.2,-1.92788286500001));
#350521=CARTESIAN_POINT('Ctrl Pts',(3.66623486499994,2.2,-1.92788286500001));
#350522=CARTESIAN_POINT('Ctrl Pts',(3.66751786599994,12.2,-1.92816292400002));
#350523=CARTESIAN_POINT('Ctrl Pts',(3.66751786599994,5.2,-1.92816292400002));
#350524=CARTESIAN_POINT('Ctrl Pts',(3.66751786599994,2.2,-1.92816292400002));
#350525=CARTESIAN_POINT('Ctrl Pts',(3.66880607199994,12.2,-1.92844251200002));
#350526=CARTESIAN_POINT('Ctrl Pts',(3.66880607199994,5.2,-1.92844251200002));
#350527=CARTESIAN_POINT('Ctrl Pts',(3.66880607199994,2.2,-1.92844251200002));
#350528=CARTESIAN_POINT('Ctrl Pts',(3.67009947399994,12.2,-1.92872161400001));
#350529=CARTESIAN_POINT('Ctrl Pts',(3.67009947399994,5.2,-1.92872161400001));
#350530=CARTESIAN_POINT('Ctrl Pts',(3.67009947399994,2.2,-1.92872161400001));
#350531=CARTESIAN_POINT('Ctrl Pts',(3.67139806599994,12.2,-1.92900021900002));
#350532=CARTESIAN_POINT('Ctrl Pts',(3.67139806599994,5.2,-1.92900021900002));
#350533=CARTESIAN_POINT('Ctrl Pts',(3.67139806599994,2.2,-1.92900021900002));
#350534=CARTESIAN_POINT('Ctrl Pts',(3.67270184099994,12.2,-1.92927831300001));
#350535=CARTESIAN_POINT('Ctrl Pts',(3.67270184099994,5.2,-1.92927831300001));
#350536=CARTESIAN_POINT('Ctrl Pts',(3.67270184099994,2.2,-1.92927831300001));
#350537=CARTESIAN_POINT('Ctrl Pts',(3.67401079199994,12.2,-1.92955588400002));
#350538=CARTESIAN_POINT('Ctrl Pts',(3.67401079199994,5.2,-1.92955588400002));
#350539=CARTESIAN_POINT('Ctrl Pts',(3.67401079199994,2.2,-1.92955588400002));
#350540=CARTESIAN_POINT('Ctrl Pts',(3.67532491199994,12.2,-1.92983292100001));
#350541=CARTESIAN_POINT('Ctrl Pts',(3.67532491199994,5.2,-1.92983292100001));
#350542=CARTESIAN_POINT('Ctrl Pts',(3.67532491199994,2.2,-1.92983292100001));
#350543=CARTESIAN_POINT('Ctrl Pts',(3.67664419599994,12.2,-1.93010940900002));
#350544=CARTESIAN_POINT('Ctrl Pts',(3.67664419599994,5.2,-1.93010940900002));
#350545=CARTESIAN_POINT('Ctrl Pts',(3.67664419599994,2.2,-1.93010940900002));
#350546=CARTESIAN_POINT('Ctrl Pts',(3.67796863599994,12.2,-1.93038533600001));
#350547=CARTESIAN_POINT('Ctrl Pts',(3.67796863599994,5.2,-1.93038533600001));
#350548=CARTESIAN_POINT('Ctrl Pts',(3.67796863599994,2.2,-1.93038533600001));
#350549=CARTESIAN_POINT('Ctrl Pts',(3.67929822499994,12.2,-1.93066069000002));
#350550=CARTESIAN_POINT('Ctrl Pts',(3.67929822499994,5.2,-1.93066069000002));
#350551=CARTESIAN_POINT('Ctrl Pts',(3.67929822499994,2.2,-1.93066069000002));
#350552=CARTESIAN_POINT('Ctrl Pts',(3.68063295599994,12.2,-1.93093545700001));
#350553=CARTESIAN_POINT('Ctrl Pts',(3.68063295599994,5.2,-1.93093545700001));
#350554=CARTESIAN_POINT('Ctrl Pts',(3.68063295599994,2.2,-1.93093545700001));
#350555=CARTESIAN_POINT('Ctrl Pts',(3.68197282299994,12.2,-1.93120962700001));
#350556=CARTESIAN_POINT('Ctrl Pts',(3.68197282299994,5.2,-1.93120962700001));
#350557=CARTESIAN_POINT('Ctrl Pts',(3.68197282299994,2.2,-1.93120962700001));
#350558=CARTESIAN_POINT('Ctrl Pts',(3.68331781899994,12.2,-1.93148318700001));
#350559=CARTESIAN_POINT('Ctrl Pts',(3.68331781899994,5.2,-1.93148318700001));
#350560=CARTESIAN_POINT('Ctrl Pts',(3.68331781899994,2.2,-1.93148318700001));
#350561=CARTESIAN_POINT('Ctrl Pts',(3.68466793599994,12.2,-1.93175612300001));
#350562=CARTESIAN_POINT('Ctrl Pts',(3.68466793599994,5.2,-1.93175612300001));
#350563=CARTESIAN_POINT('Ctrl Pts',(3.68466793599994,2.2,-1.93175612300001));
#350564=CARTESIAN_POINT('Ctrl Pts',(3.68602316999994,12.2,-1.93202842500002));
#350565=CARTESIAN_POINT('Ctrl Pts',(3.68602316999994,5.2,-1.93202842500002));
#350566=CARTESIAN_POINT('Ctrl Pts',(3.68602316999994,2.2,-1.93202842500002));
#350567=CARTESIAN_POINT('Ctrl Pts',(3.68738351099994,12.2,-1.93230007800001));
#350568=CARTESIAN_POINT('Ctrl Pts',(3.68738351099994,5.2,-1.93230007800001));
#350569=CARTESIAN_POINT('Ctrl Pts',(3.68738351099994,2.2,-1.93230007800001));
#350570=CARTESIAN_POINT('Ctrl Pts',(3.68874895499994,12.2,-1.93257107200001));
#350571=CARTESIAN_POINT('Ctrl Pts',(3.68874895499994,5.2,-1.93257107200001));
#350572=CARTESIAN_POINT('Ctrl Pts',(3.68874895499994,2.2,-1.93257107200001));
#350573=CARTESIAN_POINT('Ctrl Pts',(3.69011949399995,12.2,-1.93284139300001));
#350574=CARTESIAN_POINT('Ctrl Pts',(3.69011949399995,5.2,-1.93284139300001));
#350575=CARTESIAN_POINT('Ctrl Pts',(3.69011949399995,2.2,-1.93284139300001));
#350576=CARTESIAN_POINT('Ctrl Pts',(3.69149512099994,12.2,-1.93311103000001));
#350577=CARTESIAN_POINT('Ctrl Pts',(3.69149512099994,5.2,-1.93311103000001));
#350578=CARTESIAN_POINT('Ctrl Pts',(3.69149512099994,2.2,-1.93311103000001));
#350579=CARTESIAN_POINT('Ctrl Pts',(3.69287582899994,12.2,-1.93337997100001));
#350580=CARTESIAN_POINT('Ctrl Pts',(3.69287582899994,5.2,-1.93337997100001));
#350581=CARTESIAN_POINT('Ctrl Pts',(3.69287582899994,2.2,-1.93337997100001));
#350582=CARTESIAN_POINT('Ctrl Pts',(3.69426161099994,12.2,-1.93364820300001));
#350583=CARTESIAN_POINT('Ctrl Pts',(3.69426161099994,5.2,-1.93364820300001));
#350584=CARTESIAN_POINT('Ctrl Pts',(3.69426161099994,2.2,-1.93364820300001));
#350585=CARTESIAN_POINT('Ctrl Pts',(3.69565246199994,12.2,-1.93391571500001));
#350586=CARTESIAN_POINT('Ctrl Pts',(3.69565246199994,5.2,-1.93391571500001));
#350587=CARTESIAN_POINT('Ctrl Pts',(3.69565246199994,2.2,-1.93391571500001));
#350588=CARTESIAN_POINT('Ctrl Pts',(3.69704837299994,12.2,-1.93418249400001));
#350589=CARTESIAN_POINT('Ctrl Pts',(3.69704837299994,5.2,-1.93418249400001));
#350590=CARTESIAN_POINT('Ctrl Pts',(3.69704837299994,2.2,-1.93418249400001));
#350591=CARTESIAN_POINT('Ctrl Pts',(3.69844933899994,12.2,-1.93444852900001));
#350592=CARTESIAN_POINT('Ctrl Pts',(3.69844933899994,5.2,-1.93444852900001));
#350593=CARTESIAN_POINT('Ctrl Pts',(3.69844933899994,2.2,-1.93444852900001));
#350594=CARTESIAN_POINT('Ctrl Pts',(3.69985535199994,12.2,-1.93471380500001));
#350595=CARTESIAN_POINT('Ctrl Pts',(3.69985535199994,5.2,-1.93471380500001));
#350596=CARTESIAN_POINT('Ctrl Pts',(3.69985535199994,2.2,-1.93471380500001));
#350597=CARTESIAN_POINT('Ctrl Pts',(3.70126640599994,12.2,-1.93497831400002));
#350598=CARTESIAN_POINT('Ctrl Pts',(3.70126640599994,5.2,-1.93497831400002));
#350599=CARTESIAN_POINT('Ctrl Pts',(3.70126640599994,2.2,-1.93497831400002));
#350600=CARTESIAN_POINT('Ctrl Pts',(3.70268249299994,12.2,-1.93524204200001));
#350601=CARTESIAN_POINT('Ctrl Pts',(3.70268249299994,5.2,-1.93524204200001));
#350602=CARTESIAN_POINT('Ctrl Pts',(3.70268249299994,2.2,-1.93524204200001));
#350603=CARTESIAN_POINT('Ctrl Pts',(3.70410360799994,12.2,-1.93550497700001));
#350604=CARTESIAN_POINT('Ctrl Pts',(3.70410360799994,5.2,-1.93550497700001));
#350605=CARTESIAN_POINT('Ctrl Pts',(3.70410360799994,2.2,-1.93550497700001));
#350606=CARTESIAN_POINT('Ctrl Pts',(3.70552974199994,12.2,-1.93576710800002));
#350607=CARTESIAN_POINT('Ctrl Pts',(3.70552974199994,5.2,-1.93576710800002));
#350608=CARTESIAN_POINT('Ctrl Pts',(3.70552974199994,2.2,-1.93576710800002));
#350609=CARTESIAN_POINT('Ctrl Pts',(3.70696088999994,12.2,-1.93602842300002));
#350610=CARTESIAN_POINT('Ctrl Pts',(3.70696088999994,5.2,-1.93602842300002));
#350611=CARTESIAN_POINT('Ctrl Pts',(3.70696088999994,2.2,-1.93602842300002));
#350612=CARTESIAN_POINT('Ctrl Pts',(3.70839704399994,12.2,-1.93628891000001));
#350613=CARTESIAN_POINT('Ctrl Pts',(3.70839704399994,5.2,-1.93628891000001));
#350614=CARTESIAN_POINT('Ctrl Pts',(3.70839704399994,2.2,-1.93628891000001));
#350615=CARTESIAN_POINT('Ctrl Pts',(3.70983819799994,12.2,-1.93654855800002));
#350616=CARTESIAN_POINT('Ctrl Pts',(3.70983819799994,5.2,-1.93654855800002));
#350617=CARTESIAN_POINT('Ctrl Pts',(3.70983819799994,2.2,-1.93654855800002));
#350618=CARTESIAN_POINT('Ctrl Pts',(3.71128434599994,12.2,-1.93680735200001));
#350619=CARTESIAN_POINT('Ctrl Pts',(3.71128434599994,5.2,-1.93680735200001));
#350620=CARTESIAN_POINT('Ctrl Pts',(3.71128434599994,2.2,-1.93680735200001));
#350621=CARTESIAN_POINT('Ctrl Pts',(3.71273547899994,12.2,-1.93706528500002));
#350622=CARTESIAN_POINT('Ctrl Pts',(3.71273547899994,5.2,-1.93706528500002));
#350623=CARTESIAN_POINT('Ctrl Pts',(3.71273547899994,2.2,-1.93706528500002));
#350624=CARTESIAN_POINT('Ctrl Pts',(3.71419159099994,12.2,-1.93732234200001));
#350625=CARTESIAN_POINT('Ctrl Pts',(3.71419159099994,5.2,-1.93732234200001));
#350626=CARTESIAN_POINT('Ctrl Pts',(3.71419159099994,2.2,-1.93732234200001));
#350627=CARTESIAN_POINT('Ctrl Pts',(3.71565267599994,12.2,-1.93757851400001));
#350628=CARTESIAN_POINT('Ctrl Pts',(3.71565267599994,5.2,-1.93757851400001));
#350629=CARTESIAN_POINT('Ctrl Pts',(3.71565267599994,2.2,-1.93757851400001));
#350630=CARTESIAN_POINT('Ctrl Pts',(3.71711872599994,12.2,-1.93783378700001));
#350631=CARTESIAN_POINT('Ctrl Pts',(3.71711872599994,5.2,-1.93783378700001));
#350632=CARTESIAN_POINT('Ctrl Pts',(3.71711872599994,2.2,-1.93783378700001));
#350633=CARTESIAN_POINT('Ctrl Pts',(3.71858973499994,12.2,-1.93808815000001));
#350634=CARTESIAN_POINT('Ctrl Pts',(3.71858973499994,5.2,-1.93808815000001));
#350635=CARTESIAN_POINT('Ctrl Pts',(3.71858973499994,2.2,-1.93808815000001));
#350636=CARTESIAN_POINT('Ctrl Pts',(3.72006569699994,12.2,-1.93834159200001));
#350637=CARTESIAN_POINT('Ctrl Pts',(3.72006569699994,5.2,-1.93834159200001));
#350638=CARTESIAN_POINT('Ctrl Pts',(3.72006569699994,2.2,-1.93834159200001));
#350639=CARTESIAN_POINT('Ctrl Pts',(3.72154660299994,12.2,-1.93859410200002));
#350640=CARTESIAN_POINT('Ctrl Pts',(3.72154660299994,5.2,-1.93859410200002));
#350641=CARTESIAN_POINT('Ctrl Pts',(3.72154660299994,2.2,-1.93859410200002));
#350642=CARTESIAN_POINT('Ctrl Pts',(3.72303244799994,12.2,-1.93884566800001));
#350643=CARTESIAN_POINT('Ctrl Pts',(3.72303244799994,5.2,-1.93884566800001));
#350644=CARTESIAN_POINT('Ctrl Pts',(3.72303244799994,2.2,-1.93884566800001));
#350645=CARTESIAN_POINT('Ctrl Pts',(3.72452322399994,12.2,-1.93909627800001));
#350646=CARTESIAN_POINT('Ctrl Pts',(3.72452322399994,5.2,-1.93909627800001));
#350647=CARTESIAN_POINT('Ctrl Pts',(3.72452322399994,2.2,-1.93909627800001));
#350648=CARTESIAN_POINT('Ctrl Pts',(3.72601892499994,12.2,-1.93934592100002));
#350649=CARTESIAN_POINT('Ctrl Pts',(3.72601892499994,5.2,-1.93934592100002));
#350650=CARTESIAN_POINT('Ctrl Pts',(3.72601892499994,2.2,-1.93934592100002));
#350651=CARTESIAN_POINT('Ctrl Pts',(3.72751954399994,12.2,-1.93959458600002));
#350652=CARTESIAN_POINT('Ctrl Pts',(3.72751954399994,5.2,-1.93959458600002));
#350653=CARTESIAN_POINT('Ctrl Pts',(3.72751954399994,2.2,-1.93959458600002));
#350654=CARTESIAN_POINT('Ctrl Pts',(3.72902507299994,12.2,-1.93984226100001));
#350655=CARTESIAN_POINT('Ctrl Pts',(3.72902507299994,5.2,-1.93984226100001));
#350656=CARTESIAN_POINT('Ctrl Pts',(3.72902507299994,2.2,-1.93984226100001));
#350657=CARTESIAN_POINT('Ctrl Pts',(3.73053550699994,12.2,-1.94008893500001));
#350658=CARTESIAN_POINT('Ctrl Pts',(3.73053550699994,5.2,-1.94008893500001));
#350659=CARTESIAN_POINT('Ctrl Pts',(3.73053550699994,2.2,-1.94008893500001));
#350660=CARTESIAN_POINT('Ctrl Pts',(3.73205083799994,12.2,-1.94033459700002));
#350661=CARTESIAN_POINT('Ctrl Pts',(3.73205083799994,5.2,-1.94033459700002));
#350662=CARTESIAN_POINT('Ctrl Pts',(3.73205083799994,2.2,-1.94033459700002));
#350663=CARTESIAN_POINT('Ctrl Pts',(3.73357105999994,12.2,-1.94057923600001));
#350664=CARTESIAN_POINT('Ctrl Pts',(3.73357105999994,5.2,-1.94057923600001));
#350665=CARTESIAN_POINT('Ctrl Pts',(3.73357105999994,2.2,-1.94057923600001));
#350666=CARTESIAN_POINT('Ctrl Pts',(3.73509616599994,12.2,-1.94082284000002));
#350667=CARTESIAN_POINT('Ctrl Pts',(3.73509616599994,5.2,-1.94082284000002));
#350668=CARTESIAN_POINT('Ctrl Pts',(3.73509616599994,2.2,-1.94082284000002));
#350669=CARTESIAN_POINT('Ctrl Pts',(3.73662614799994,12.2,-1.94106539800002));
#350670=CARTESIAN_POINT('Ctrl Pts',(3.73662614799994,5.2,-1.94106539800002));
#350671=CARTESIAN_POINT('Ctrl Pts',(3.73662614799994,2.2,-1.94106539800002));
#350672=CARTESIAN_POINT('Ctrl Pts',(3.73816099999994,12.2,-1.94130689900001));
#350673=CARTESIAN_POINT('Ctrl Pts',(3.73816099999994,5.2,-1.94130689900001));
#350674=CARTESIAN_POINT('Ctrl Pts',(3.73816099999994,2.2,-1.94130689900001));
#350675=CARTESIAN_POINT('Ctrl Pts',(3.73970071499994,12.2,-1.94154733200001));
#350676=CARTESIAN_POINT('Ctrl Pts',(3.73970071499994,5.2,-1.94154733200001));
#350677=CARTESIAN_POINT('Ctrl Pts',(3.73970071499994,2.2,-1.94154733200001));
#350678=CARTESIAN_POINT('Ctrl Pts',(3.74124528699994,12.2,-1.94178668600001));
#350679=CARTESIAN_POINT('Ctrl Pts',(3.74124528699994,5.2,-1.94178668600001));
#350680=CARTESIAN_POINT('Ctrl Pts',(3.74124528699994,2.2,-1.94178668600001));
#350681=CARTESIAN_POINT('Ctrl Pts',(3.74279470799994,12.2,-1.94202495000001));
#350682=CARTESIAN_POINT('Ctrl Pts',(3.74279470799994,5.2,-1.94202495000001));
#350683=CARTESIAN_POINT('Ctrl Pts',(3.74279470799994,2.2,-1.94202495000001));
#350684=CARTESIAN_POINT('Ctrl Pts',(3.74434896999994,12.2,-1.94226211300002));
#350685=CARTESIAN_POINT('Ctrl Pts',(3.74434896999994,5.2,-1.94226211300002));
#350686=CARTESIAN_POINT('Ctrl Pts',(3.74434896999994,2.2,-1.94226211300002));
#350687=CARTESIAN_POINT('Ctrl Pts',(3.74590806999994,12.2,-1.94249816300001));
#350688=CARTESIAN_POINT('Ctrl Pts',(3.74590806999994,5.2,-1.94249816300001));
#350689=CARTESIAN_POINT('Ctrl Pts',(3.74590806999994,2.2,-1.94249816300001));
#350690=CARTESIAN_POINT('Ctrl Pts',(3.74747199799994,12.2,-1.94273309000002));
#350691=CARTESIAN_POINT('Ctrl Pts',(3.74747199799994,5.2,-1.94273309000002));
#350692=CARTESIAN_POINT('Ctrl Pts',(3.74747199799994,2.2,-1.94273309000002));
#350693=CARTESIAN_POINT('Ctrl Pts',(3.74904074799994,12.2,-1.94296688300001));
#350694=CARTESIAN_POINT('Ctrl Pts',(3.74904074799994,5.2,-1.94296688300001));
#350695=CARTESIAN_POINT('Ctrl Pts',(3.74904074799994,2.2,-1.94296688300001));
#350696=CARTESIAN_POINT('Ctrl Pts',(3.75061431399994,12.2,-1.94319953000001));
#350697=CARTESIAN_POINT('Ctrl Pts',(3.75061431399994,5.2,-1.94319953000001));
#350698=CARTESIAN_POINT('Ctrl Pts',(3.75061431399994,2.2,-1.94319953000001));
#350699=CARTESIAN_POINT('Ctrl Pts',(3.75219268599994,12.2,-1.94343102300001));
#350700=CARTESIAN_POINT('Ctrl Pts',(3.75219268599994,5.2,-1.94343102300001));
#350701=CARTESIAN_POINT('Ctrl Pts',(3.75219268599994,2.2,-1.94343102300001));
#350702=CARTESIAN_POINT('Ctrl Pts',(3.75377586099995,12.2,-1.94366134800001));
#350703=CARTESIAN_POINT('Ctrl Pts',(3.75377586099995,5.2,-1.94366134800001));
#350704=CARTESIAN_POINT('Ctrl Pts',(3.75377586099995,2.2,-1.94366134800001));
#350705=CARTESIAN_POINT('Ctrl Pts',(3.75536383099994,12.2,-1.94389049600002));
#350706=CARTESIAN_POINT('Ctrl Pts',(3.75536383099994,5.2,-1.94389049600002));
#350707=CARTESIAN_POINT('Ctrl Pts',(3.75536383099994,2.2,-1.94389049600002));
#350708=CARTESIAN_POINT('Ctrl Pts',(3.75695658799994,12.2,-1.94411845500001));
#350709=CARTESIAN_POINT('Ctrl Pts',(3.75695658799994,5.2,-1.94411845500001));
#350710=CARTESIAN_POINT('Ctrl Pts',(3.75695658799994,2.2,-1.94411845500001));
#350711=CARTESIAN_POINT('Ctrl Pts',(3.75855412599994,12.2,-1.94434521600002));
#350712=CARTESIAN_POINT('Ctrl Pts',(3.75855412599994,5.2,-1.94434521600002));
#350713=CARTESIAN_POINT('Ctrl Pts',(3.75855412599994,2.2,-1.94434521600002));
#350714=CARTESIAN_POINT('Ctrl Pts',(3.76015643799994,12.2,-1.94457076600001));
#350715=CARTESIAN_POINT('Ctrl Pts',(3.76015643799994,5.2,-1.94457076600001));
#350716=CARTESIAN_POINT('Ctrl Pts',(3.76015643799994,2.2,-1.94457076600001));
#350717=CARTESIAN_POINT('Ctrl Pts',(3.76176351799994,12.2,-1.94479509600002));
#350718=CARTESIAN_POINT('Ctrl Pts',(3.76176351799994,5.2,-1.94479509600002));
#350719=CARTESIAN_POINT('Ctrl Pts',(3.76176351799994,2.2,-1.94479509600002));
#350720=CARTESIAN_POINT('Ctrl Pts',(3.76337535699994,12.2,-1.94501819400001));
#350721=CARTESIAN_POINT('Ctrl Pts',(3.76337535699994,5.2,-1.94501819400001));
#350722=CARTESIAN_POINT('Ctrl Pts',(3.76337535699994,2.2,-1.94501819400001));
#350723=CARTESIAN_POINT('Ctrl Pts',(3.76499194999994,12.2,-1.94524005200002));
#350724=CARTESIAN_POINT('Ctrl Pts',(3.76499194999994,5.2,-1.94524005200002));
#350725=CARTESIAN_POINT('Ctrl Pts',(3.76499194999994,2.2,-1.94524005200002));
#350726=CARTESIAN_POINT('Ctrl Pts',(3.76661328999994,12.2,-1.94546065700001));
#350727=CARTESIAN_POINT('Ctrl Pts',(3.76661328999994,5.2,-1.94546065700001));
#350728=CARTESIAN_POINT('Ctrl Pts',(3.76661328999994,2.2,-1.94546065700001));
#350729=CARTESIAN_POINT('Ctrl Pts',(3.76823936799994,12.2,-1.94567999800002));
#350730=CARTESIAN_POINT('Ctrl Pts',(3.76823936799994,5.2,-1.94567999800002));
#350731=CARTESIAN_POINT('Ctrl Pts',(3.76823936799994,2.2,-1.94567999800002));
#350732=CARTESIAN_POINT('Ctrl Pts',(3.76987017999994,12.2,-1.94589806700002));
#350733=CARTESIAN_POINT('Ctrl Pts',(3.76987017999994,5.2,-1.94589806700002));
#350734=CARTESIAN_POINT('Ctrl Pts',(3.76987017999994,2.2,-1.94589806700002));
#350735=CARTESIAN_POINT('Ctrl Pts',(3.77150571799994,12.2,-1.94611485100001));
#350736=CARTESIAN_POINT('Ctrl Pts',(3.77150571799994,5.2,-1.94611485100001));
#350737=CARTESIAN_POINT('Ctrl Pts',(3.77150571799994,2.2,-1.94611485100001));
#350738=CARTESIAN_POINT('Ctrl Pts',(3.77314597499994,12.2,-1.94633034000002));
#350739=CARTESIAN_POINT('Ctrl Pts',(3.77314597499994,5.2,-1.94633034000002));
#350740=CARTESIAN_POINT('Ctrl Pts',(3.77314597499994,2.2,-1.94633034000002));
#350741=CARTESIAN_POINT('Ctrl Pts',(3.77479094399995,12.2,-1.94654452600002));
#350742=CARTESIAN_POINT('Ctrl Pts',(3.77479094399995,5.2,-1.94654452600002));
#350743=CARTESIAN_POINT('Ctrl Pts',(3.77479094399995,2.2,-1.94654452600002));
#350744=CARTESIAN_POINT('Ctrl Pts',(3.77644061799994,12.2,-1.94675739500001));
#350745=CARTESIAN_POINT('Ctrl Pts',(3.77644061799994,5.2,-1.94675739500001));
#350746=CARTESIAN_POINT('Ctrl Pts',(3.77644061799994,2.2,-1.94675739500001));
#350747=CARTESIAN_POINT('Ctrl Pts',(3.77809499099994,12.2,-1.94696893800002));
#350748=CARTESIAN_POINT('Ctrl Pts',(3.77809499099994,5.2,-1.94696893800002));
#350749=CARTESIAN_POINT('Ctrl Pts',(3.77809499099994,2.2,-1.94696893800002));
#350750=CARTESIAN_POINT('Ctrl Pts',(3.77975405499994,12.2,-1.94717914600002));
#350751=CARTESIAN_POINT('Ctrl Pts',(3.77975405499994,5.2,-1.94717914600002));
#350752=CARTESIAN_POINT('Ctrl Pts',(3.77975405499994,2.2,-1.94717914600002));
#350753=CARTESIAN_POINT('Ctrl Pts',(3.78141780399994,12.2,-1.94738800700001));
#350754=CARTESIAN_POINT('Ctrl Pts',(3.78141780399994,5.2,-1.94738800700001));
#350755=CARTESIAN_POINT('Ctrl Pts',(3.78141780399994,2.2,-1.94738800700001));
#350756=CARTESIAN_POINT('Ctrl Pts',(3.78308623099994,12.2,-1.94759551100002));
#350757=CARTESIAN_POINT('Ctrl Pts',(3.78308623099994,5.2,-1.94759551100002));
#350758=CARTESIAN_POINT('Ctrl Pts',(3.78308623099994,2.2,-1.94759551100002));
#350759=CARTESIAN_POINT('Ctrl Pts',(3.78475932799994,12.2,-1.94780164800001));
#350760=CARTESIAN_POINT('Ctrl Pts',(3.78475932799994,5.2,-1.94780164800001));
#350761=CARTESIAN_POINT('Ctrl Pts',(3.78475932799994,2.2,-1.94780164800001));
#350762=CARTESIAN_POINT('Ctrl Pts',(3.78643708899994,12.2,-1.94800640900001));
#350763=CARTESIAN_POINT('Ctrl Pts',(3.78643708899994,5.2,-1.94800640900001));
#350764=CARTESIAN_POINT('Ctrl Pts',(3.78643708899994,2.2,-1.94800640900001));
#350765=CARTESIAN_POINT('Ctrl Pts',(3.78811950799994,12.2,-1.94820978100001));
#350766=CARTESIAN_POINT('Ctrl Pts',(3.78811950799994,5.2,-1.94820978100001));
#350767=CARTESIAN_POINT('Ctrl Pts',(3.78811950799994,2.2,-1.94820978100001));
#350768=CARTESIAN_POINT('Ctrl Pts',(3.78980657699994,12.2,-1.94841175400001));
#350769=CARTESIAN_POINT('Ctrl Pts',(3.78980657699994,5.2,-1.94841175400001));
#350770=CARTESIAN_POINT('Ctrl Pts',(3.78980657699994,2.2,-1.94841175400001));
#350771=CARTESIAN_POINT('Ctrl Pts',(3.79149828999994,12.2,-1.94861232100001));
#350772=CARTESIAN_POINT('Ctrl Pts',(3.79149828999994,5.2,-1.94861232100001));
#350773=CARTESIAN_POINT('Ctrl Pts',(3.79149828999994,2.2,-1.94861232100001));
#350774=CARTESIAN_POINT('Ctrl Pts',(3.79319463899995,12.2,-1.94881147000002));
#350775=CARTESIAN_POINT('Ctrl Pts',(3.79319463899995,5.2,-1.94881147000002));
#350776=CARTESIAN_POINT('Ctrl Pts',(3.79319463899995,2.2,-1.94881147000002));
#350777=CARTESIAN_POINT('Ctrl Pts',(3.79489561699994,12.2,-1.94900919000002));
#350778=CARTESIAN_POINT('Ctrl Pts',(3.79489561699994,5.2,-1.94900919000002));
#350779=CARTESIAN_POINT('Ctrl Pts',(3.79489561699994,2.2,-1.94900919000002));
#350780=CARTESIAN_POINT('Ctrl Pts',(3.79660121799994,12.2,-1.94920547100002));
#350781=CARTESIAN_POINT('Ctrl Pts',(3.79660121799994,5.2,-1.94920547100002));
#350782=CARTESIAN_POINT('Ctrl Pts',(3.79660121799994,2.2,-1.94920547100002));
#350783=CARTESIAN_POINT('Ctrl Pts',(3.79831143499994,12.2,-1.94940030600002));
#350784=CARTESIAN_POINT('Ctrl Pts',(3.79831143499994,5.2,-1.94940030600002));
#350785=CARTESIAN_POINT('Ctrl Pts',(3.79831143499994,2.2,-1.94940030600002));
#350786=CARTESIAN_POINT('Ctrl Pts',(3.80002626099994,12.2,-1.94959368100001));
#350787=CARTESIAN_POINT('Ctrl Pts',(3.80002626099994,5.2,-1.94959368100001));
#350788=CARTESIAN_POINT('Ctrl Pts',(3.80002626099994,2.2,-1.94959368100001));
#350789=CARTESIAN_POINT('Ctrl Pts',(3.80174568899994,12.2,-1.94978558700001));
#350790=CARTESIAN_POINT('Ctrl Pts',(3.80174568899994,5.2,-1.94978558700001));
#350791=CARTESIAN_POINT('Ctrl Pts',(3.80174568899994,2.2,-1.94978558700001));
#350792=CARTESIAN_POINT('Ctrl Pts',(3.80346971199994,12.2,-1.94997601600001));
#350793=CARTESIAN_POINT('Ctrl Pts',(3.80346971199994,5.2,-1.94997601600001));
#350794=CARTESIAN_POINT('Ctrl Pts',(3.80346971199994,2.2,-1.94997601600001));
#350795=CARTESIAN_POINT('Ctrl Pts',(3.80519832299994,12.2,-1.95016495500001));
#350796=CARTESIAN_POINT('Ctrl Pts',(3.80519832299994,5.2,-1.95016495500001));
#350797=CARTESIAN_POINT('Ctrl Pts',(3.80519832299994,2.2,-1.95016495500001));
#350798=CARTESIAN_POINT('Ctrl Pts',(3.80693151599994,12.2,-1.95035239700001));
#350799=CARTESIAN_POINT('Ctrl Pts',(3.80693151599994,5.2,-1.95035239700001));
#350800=CARTESIAN_POINT('Ctrl Pts',(3.80693151599994,2.2,-1.95035239700001));
#350801=CARTESIAN_POINT('Ctrl Pts',(3.80866928199994,12.2,-1.95053833200001));
#350802=CARTESIAN_POINT('Ctrl Pts',(3.80866928199994,5.2,-1.95053833200001));
#350803=CARTESIAN_POINT('Ctrl Pts',(3.80866928199994,2.2,-1.95053833200001));
#350804=CARTESIAN_POINT('Ctrl Pts',(3.81041161799994,12.2,-1.95072274600002));
#350805=CARTESIAN_POINT('Ctrl Pts',(3.81041161799994,5.2,-1.95072274600002));
#350806=CARTESIAN_POINT('Ctrl Pts',(3.81041161799994,2.2,-1.95072274600002));
#350807=CARTESIAN_POINT('Ctrl Pts',(3.81215851299994,12.2,-1.95090563500001));
#350808=CARTESIAN_POINT('Ctrl Pts',(3.81215851299994,5.2,-1.95090563500001));
#350809=CARTESIAN_POINT('Ctrl Pts',(3.81215851299994,2.2,-1.95090563500001));
#350810=CARTESIAN_POINT('Ctrl Pts',(3.81390996099995,12.2,-1.95108698500002));
#350811=CARTESIAN_POINT('Ctrl Pts',(3.81390996099995,5.2,-1.95108698500002));
#350812=CARTESIAN_POINT('Ctrl Pts',(3.81390996099995,2.2,-1.95108698500002));
#350813=CARTESIAN_POINT('Ctrl Pts',(3.81566595699994,12.2,-1.95126678800001));
#350814=CARTESIAN_POINT('Ctrl Pts',(3.81566595699994,5.2,-1.95126678800001));
#350815=CARTESIAN_POINT('Ctrl Pts',(3.81566595699994,2.2,-1.95126678800001));
#350816=CARTESIAN_POINT('Ctrl Pts',(3.81742649299994,12.2,-1.95144503300002));
#350817=CARTESIAN_POINT('Ctrl Pts',(3.81742649299994,5.2,-1.95144503300002));
#350818=CARTESIAN_POINT('Ctrl Pts',(3.81742649299994,2.2,-1.95144503300002));
#350819=CARTESIAN_POINT('Ctrl Pts',(3.81919156199995,12.2,-1.95162171200002));
#350820=CARTESIAN_POINT('Ctrl Pts',(3.81919156199995,5.2,-1.95162171200002));
#350821=CARTESIAN_POINT('Ctrl Pts',(3.81919156199995,2.2,-1.95162171200002));
#350822=CARTESIAN_POINT('Ctrl Pts',(3.82096115699994,12.2,-1.95179681300001));
#350823=CARTESIAN_POINT('Ctrl Pts',(3.82096115699994,5.2,-1.95179681300001));
#350824=CARTESIAN_POINT('Ctrl Pts',(3.82096115699994,2.2,-1.95179681300001));
#350825=CARTESIAN_POINT('Ctrl Pts',(3.82273527099994,12.2,-1.95197032900001));
#350826=CARTESIAN_POINT('Ctrl Pts',(3.82273527099994,5.2,-1.95197032900001));
#350827=CARTESIAN_POINT('Ctrl Pts',(3.82273527099994,2.2,-1.95197032900001));
#350828=CARTESIAN_POINT('Ctrl Pts',(3.82451389799995,12.2,-1.95214224900001));
#350829=CARTESIAN_POINT('Ctrl Pts',(3.82451389799995,5.2,-1.95214224900001));
#350830=CARTESIAN_POINT('Ctrl Pts',(3.82451389799995,2.2,-1.95214224900001));
#350831=CARTESIAN_POINT('Ctrl Pts',(3.82629703099994,12.2,-1.95231256300001));
#350832=CARTESIAN_POINT('Ctrl Pts',(3.82629703099994,5.2,-1.95231256300001));
#350833=CARTESIAN_POINT('Ctrl Pts',(3.82629703099994,2.2,-1.95231256300001));
#350834=CARTESIAN_POINT('Ctrl Pts',(3.82808465999994,12.2,-1.95248126200001));
#350835=CARTESIAN_POINT('Ctrl Pts',(3.82808465999994,5.2,-1.95248126200001));
#350836=CARTESIAN_POINT('Ctrl Pts',(3.82808465999994,2.2,-1.95248126200001));
#350837=CARTESIAN_POINT('Ctrl Pts',(3.82987678299994,12.2,-1.95264833600001));
#350838=CARTESIAN_POINT('Ctrl Pts',(3.82987678299994,5.2,-1.95264833600001));
#350839=CARTESIAN_POINT('Ctrl Pts',(3.82987678299994,2.2,-1.95264833600001));
#350840=CARTESIAN_POINT('Ctrl Pts',(3.83167338899994,12.2,-1.95281377600002));
#350841=CARTESIAN_POINT('Ctrl Pts',(3.83167338899994,5.2,-1.95281377600002));
#350842=CARTESIAN_POINT('Ctrl Pts',(3.83167338899994,2.2,-1.95281377600002));
#350843=CARTESIAN_POINT('Ctrl Pts',(3.83347447499994,12.2,-1.95297757100001));
#350844=CARTESIAN_POINT('Ctrl Pts',(3.83347447499994,5.2,-1.95297757100001));
#350845=CARTESIAN_POINT('Ctrl Pts',(3.83347447499994,2.2,-1.95297757100001));
#350846=CARTESIAN_POINT('Ctrl Pts',(3.83528002999994,12.2,-1.95313971300001));
#350847=CARTESIAN_POINT('Ctrl Pts',(3.83528002999994,5.2,-1.95313971300001));
#350848=CARTESIAN_POINT('Ctrl Pts',(3.83528002999994,2.2,-1.95313971300001));
#350849=CARTESIAN_POINT('Ctrl Pts',(3.83709004999994,12.2,-1.95330019300001));
#350850=CARTESIAN_POINT('Ctrl Pts',(3.83709004999994,5.2,-1.95330019300001));
#350851=CARTESIAN_POINT('Ctrl Pts',(3.83709004999994,2.2,-1.95330019300001));
#350852=CARTESIAN_POINT('Ctrl Pts',(3.83890452599994,12.2,-1.95345900100001));
#350853=CARTESIAN_POINT('Ctrl Pts',(3.83890452599994,5.2,-1.95345900100001));
#350854=CARTESIAN_POINT('Ctrl Pts',(3.83890452599994,2.2,-1.95345900100001));
#350855=CARTESIAN_POINT('Ctrl Pts',(3.84072345299994,12.2,-1.95361612600002));
#350856=CARTESIAN_POINT('Ctrl Pts',(3.84072345299994,5.2,-1.95361612600002));
#350857=CARTESIAN_POINT('Ctrl Pts',(3.84072345299994,2.2,-1.95361612600002));
#350858=CARTESIAN_POINT('Ctrl Pts',(3.84254682399995,12.2,-1.95377156100002));
#350859=CARTESIAN_POINT('Ctrl Pts',(3.84254682399995,5.2,-1.95377156100002));
#350860=CARTESIAN_POINT('Ctrl Pts',(3.84254682399995,2.2,-1.95377156100002));
#350861=CARTESIAN_POINT('Ctrl Pts',(3.84437462999994,12.2,-1.95392529400001));
#350862=CARTESIAN_POINT('Ctrl Pts',(3.84437462999994,5.2,-1.95392529400001));
#350863=CARTESIAN_POINT('Ctrl Pts',(3.84437462999994,2.2,-1.95392529400001));
#350864=CARTESIAN_POINT('Ctrl Pts',(3.84620686599995,12.2,-1.95407731900001));
#350865=CARTESIAN_POINT('Ctrl Pts',(3.84620686599995,5.2,-1.95407731900001));
#350866=CARTESIAN_POINT('Ctrl Pts',(3.84620686599995,2.2,-1.95407731900001));
#350867=CARTESIAN_POINT('Ctrl Pts',(3.84804352399994,12.2,-1.95422762400002));
#350868=CARTESIAN_POINT('Ctrl Pts',(3.84804352399994,5.2,-1.95422762400002));
#350869=CARTESIAN_POINT('Ctrl Pts',(3.84804352399994,2.2,-1.95422762400002));
#350870=CARTESIAN_POINT('Ctrl Pts',(3.84988459799994,12.2,-1.95437620100002));
#350871=CARTESIAN_POINT('Ctrl Pts',(3.84988459799994,5.2,-1.95437620100002));
#350872=CARTESIAN_POINT('Ctrl Pts',(3.84988459799994,2.2,-1.95437620100002));
#350873=CARTESIAN_POINT('Ctrl Pts',(3.85173007999994,12.2,-1.95452304000002));
#350874=CARTESIAN_POINT('Ctrl Pts',(3.85173007999994,5.2,-1.95452304000002));
#350875=CARTESIAN_POINT('Ctrl Pts',(3.85173007999994,2.2,-1.95452304000002));
#350876=CARTESIAN_POINT('Ctrl Pts',(3.85357996499994,12.2,-1.95466813200001));
#350877=CARTESIAN_POINT('Ctrl Pts',(3.85357996499994,5.2,-1.95466813200001));
#350878=CARTESIAN_POINT('Ctrl Pts',(3.85357996499994,2.2,-1.95466813200001));
#350879=CARTESIAN_POINT('Ctrl Pts',(3.85543424399994,12.2,-1.95481146900002));
#350880=CARTESIAN_POINT('Ctrl Pts',(3.85543424399994,5.2,-1.95481146900002));
#350881=CARTESIAN_POINT('Ctrl Pts',(3.85543424399994,2.2,-1.95481146900002));
#350882=CARTESIAN_POINT('Ctrl Pts',(3.85729291099994,12.2,-1.95495303900001));
#350883=CARTESIAN_POINT('Ctrl Pts',(3.85729291099994,5.2,-1.95495303900001));
#350884=CARTESIAN_POINT('Ctrl Pts',(3.85729291099994,2.2,-1.95495303900001));
#350885=CARTESIAN_POINT('Ctrl Pts',(3.85915595899994,12.2,-1.95509283500002));
#350886=CARTESIAN_POINT('Ctrl Pts',(3.85915595899994,5.2,-1.95509283500002));
#350887=CARTESIAN_POINT('Ctrl Pts',(3.85915595899994,2.2,-1.95509283500002));
#350888=CARTESIAN_POINT('Ctrl Pts',(3.86102338099994,12.2,-1.95523084800001));
#350889=CARTESIAN_POINT('Ctrl Pts',(3.86102338099994,5.2,-1.95523084800001));
#350890=CARTESIAN_POINT('Ctrl Pts',(3.86102338099994,2.2,-1.95523084800001));
#350891=CARTESIAN_POINT('Ctrl Pts',(3.86289516999994,12.2,-1.95536706700001));
#350892=CARTESIAN_POINT('Ctrl Pts',(3.86289516999994,5.2,-1.95536706700001));
#350893=CARTESIAN_POINT('Ctrl Pts',(3.86289516999994,2.2,-1.95536706700001));
#350894=CARTESIAN_POINT('Ctrl Pts',(3.86477131999994,12.2,-1.95550148500002));
#350895=CARTESIAN_POINT('Ctrl Pts',(3.86477131999994,5.2,-1.95550148500002));
#350896=CARTESIAN_POINT('Ctrl Pts',(3.86477131999994,2.2,-1.95550148500002));
#350897=CARTESIAN_POINT('Ctrl Pts',(3.86665182199994,12.2,-1.95563409200001));
#350898=CARTESIAN_POINT('Ctrl Pts',(3.86665182199994,5.2,-1.95563409200001));
#350899=CARTESIAN_POINT('Ctrl Pts',(3.86665182199994,2.2,-1.95563409200001));
#350900=CARTESIAN_POINT('Ctrl Pts',(3.86853667099994,12.2,-1.95576487900002));
#350901=CARTESIAN_POINT('Ctrl Pts',(3.86853667099994,5.2,-1.95576487900002));
#350902=CARTESIAN_POINT('Ctrl Pts',(3.86853667099994,2.2,-1.95576487900002));
#350903=CARTESIAN_POINT('Ctrl Pts',(3.87042586099994,12.2,-1.95589383700002));
#350904=CARTESIAN_POINT('Ctrl Pts',(3.87042586099994,5.2,-1.95589383700002));
#350905=CARTESIAN_POINT('Ctrl Pts',(3.87042586099994,2.2,-1.95589383700002));
#350906=CARTESIAN_POINT('Ctrl Pts',(3.87231938099994,12.2,-1.95602095700002));
#350907=CARTESIAN_POINT('Ctrl Pts',(3.87231938099994,5.2,-1.95602095700002));
#350908=CARTESIAN_POINT('Ctrl Pts',(3.87231938099994,2.2,-1.95602095700002));
#350909=CARTESIAN_POINT('Ctrl Pts',(3.87421722899994,12.2,-1.95614623000001));
#350910=CARTESIAN_POINT('Ctrl Pts',(3.87421722899994,5.2,-1.95614623000001));
#350911=CARTESIAN_POINT('Ctrl Pts',(3.87421722899994,2.2,-1.95614623000001));
#350912=CARTESIAN_POINT('Ctrl Pts',(3.87611939399994,12.2,-1.95626964900002));
#350913=CARTESIAN_POINT('Ctrl Pts',(3.87611939399994,5.2,-1.95626964900002));
#350914=CARTESIAN_POINT('Ctrl Pts',(3.87611939399994,2.2,-1.95626964900002));
#350915=CARTESIAN_POINT('Ctrl Pts',(3.87802587099995,12.2,-1.95639120100001));
#350916=CARTESIAN_POINT('Ctrl Pts',(3.87802587099995,5.2,-1.95639120100001));
#350917=CARTESIAN_POINT('Ctrl Pts',(3.87802587099995,2.2,-1.95639120100001));
#350918=CARTESIAN_POINT('Ctrl Pts',(3.87993665399994,12.2,-1.95651088000002));
#350919=CARTESIAN_POINT('Ctrl Pts',(3.87993665399994,5.2,-1.95651088000002));
#350920=CARTESIAN_POINT('Ctrl Pts',(3.87993665399994,2.2,-1.95651088000002));
#350921=CARTESIAN_POINT('Ctrl Pts',(3.88185173299994,12.2,-1.95662867600001));
#350922=CARTESIAN_POINT('Ctrl Pts',(3.88185173299994,5.2,-1.95662867600001));
#350923=CARTESIAN_POINT('Ctrl Pts',(3.88185173299994,2.2,-1.95662867600001));
#350924=CARTESIAN_POINT('Ctrl Pts',(3.88377110399994,12.2,-1.95674458100001));
#350925=CARTESIAN_POINT('Ctrl Pts',(3.88377110399994,5.2,-1.95674458100001));
#350926=CARTESIAN_POINT('Ctrl Pts',(3.88377110399994,2.2,-1.95674458100001));
#350927=CARTESIAN_POINT('Ctrl Pts',(3.88569475899994,12.2,-1.95685858600001));
#350928=CARTESIAN_POINT('Ctrl Pts',(3.88569475899994,5.2,-1.95685858600001));
#350929=CARTESIAN_POINT('Ctrl Pts',(3.88569475899994,2.2,-1.95685858600001));
#350930=CARTESIAN_POINT('Ctrl Pts',(3.88762269099994,12.2,-1.95697068200001));
#350931=CARTESIAN_POINT('Ctrl Pts',(3.88762269099994,5.2,-1.95697068200001));
#350932=CARTESIAN_POINT('Ctrl Pts',(3.88762269099994,2.2,-1.95697068200001));
#350933=CARTESIAN_POINT('Ctrl Pts',(3.88955489299994,12.2,-1.95708085900002));
#350934=CARTESIAN_POINT('Ctrl Pts',(3.88955489299994,5.2,-1.95708085900002));
#350935=CARTESIAN_POINT('Ctrl Pts',(3.88955489299994,2.2,-1.95708085900002));
#350936=CARTESIAN_POINT('Ctrl Pts',(3.89149135899994,12.2,-1.95718911000001));
#350937=CARTESIAN_POINT('Ctrl Pts',(3.89149135899994,5.2,-1.95718911000001));
#350938=CARTESIAN_POINT('Ctrl Pts',(3.89149135899994,2.2,-1.95718911000001));
#350939=CARTESIAN_POINT('Ctrl Pts',(3.89343207999994,12.2,-1.95729542700001));
#350940=CARTESIAN_POINT('Ctrl Pts',(3.89343207999994,5.2,-1.95729542700001));
#350941=CARTESIAN_POINT('Ctrl Pts',(3.89343207999994,2.2,-1.95729542700001));
#350942=CARTESIAN_POINT('Ctrl Pts',(3.89537705199994,12.2,-1.95739979900001));
#350943=CARTESIAN_POINT('Ctrl Pts',(3.89537705199994,5.2,-1.95739979900001));
#350944=CARTESIAN_POINT('Ctrl Pts',(3.89537705199994,2.2,-1.95739979900001));
#350945=CARTESIAN_POINT('Ctrl Pts',(3.89732626499994,12.2,-1.95750221800001));
#350946=CARTESIAN_POINT('Ctrl Pts',(3.89732626499994,5.2,-1.95750221800001));
#350947=CARTESIAN_POINT('Ctrl Pts',(3.89732626499994,2.2,-1.95750221800001));
#350948=CARTESIAN_POINT('Ctrl Pts',(3.89927971499994,12.2,-1.95760267600001));
#350949=CARTESIAN_POINT('Ctrl Pts',(3.89927971499994,5.2,-1.95760267600001));
#350950=CARTESIAN_POINT('Ctrl Pts',(3.89927971499994,2.2,-1.95760267600001));
#350951=CARTESIAN_POINT('Ctrl Pts',(3.90123739199994,12.2,-1.95770116400002));
#350952=CARTESIAN_POINT('Ctrl Pts',(3.90123739199994,5.2,-1.95770116400002));
#350953=CARTESIAN_POINT('Ctrl Pts',(3.90123739199994,2.2,-1.95770116400002));
#350954=CARTESIAN_POINT('Ctrl Pts',(3.90319929199994,12.2,-1.95779767400001));
#350955=CARTESIAN_POINT('Ctrl Pts',(3.90319929199994,5.2,-1.95779767400001));
#350956=CARTESIAN_POINT('Ctrl Pts',(3.90319929199994,2.2,-1.95779767400001));
#350957=CARTESIAN_POINT('Ctrl Pts',(3.90516540699994,12.2,-1.95789219700002));
#350958=CARTESIAN_POINT('Ctrl Pts',(3.90516540699994,5.2,-1.95789219700002));
#350959=CARTESIAN_POINT('Ctrl Pts',(3.90516540699994,2.2,-1.95789219700002));
#350960=CARTESIAN_POINT('Ctrl Pts',(3.90713572899994,12.2,-1.95798472300002));
#350961=CARTESIAN_POINT('Ctrl Pts',(3.90713572899994,5.2,-1.95798472300002));
#350962=CARTESIAN_POINT('Ctrl Pts',(3.90713572899994,2.2,-1.95798472300002));
#350963=CARTESIAN_POINT('Ctrl Pts',(3.90911025099994,12.2,-1.95807524500001));
#350964=CARTESIAN_POINT('Ctrl Pts',(3.90911025099994,5.2,-1.95807524500001));
#350965=CARTESIAN_POINT('Ctrl Pts',(3.90911025099994,2.2,-1.95807524500001));
#350966=CARTESIAN_POINT('Ctrl Pts',(3.91108896799994,12.2,-1.95816375500002));
#350967=CARTESIAN_POINT('Ctrl Pts',(3.91108896799994,5.2,-1.95816375500002));
#350968=CARTESIAN_POINT('Ctrl Pts',(3.91108896799994,2.2,-1.95816375500002));
#350969=CARTESIAN_POINT('Ctrl Pts',(3.91307187099994,12.2,-1.95825024400001));
#350970=CARTESIAN_POINT('Ctrl Pts',(3.91307187099994,5.2,-1.95825024400001));
#350971=CARTESIAN_POINT('Ctrl Pts',(3.91307187099994,2.2,-1.95825024400001));
#350972=CARTESIAN_POINT('Ctrl Pts',(3.91505895599995,12.2,-1.95833470300002));
#350973=CARTESIAN_POINT('Ctrl Pts',(3.91505895599995,5.2,-1.95833470300002));
#350974=CARTESIAN_POINT('Ctrl Pts',(3.91505895599995,2.2,-1.95833470300002));
#350975=CARTESIAN_POINT('Ctrl Pts',(3.91705021199994,12.2,-1.95841712400001));
#350976=CARTESIAN_POINT('Ctrl Pts',(3.91705021199994,5.2,-1.95841712400001));
#350977=CARTESIAN_POINT('Ctrl Pts',(3.91705021199994,2.2,-1.95841712400001));
#350978=CARTESIAN_POINT('Ctrl Pts',(3.91904563499994,12.2,-1.95849749800002));
#350979=CARTESIAN_POINT('Ctrl Pts',(3.91904563499994,5.2,-1.95849749800002));
#350980=CARTESIAN_POINT('Ctrl Pts',(3.91904563499994,2.2,-1.95849749800002));
#350981=CARTESIAN_POINT('Ctrl Pts',(3.92104521699994,12.2,-1.95857581700002));
#350982=CARTESIAN_POINT('Ctrl Pts',(3.92104521699994,5.2,-1.95857581700002));
#350983=CARTESIAN_POINT('Ctrl Pts',(3.92104521699994,2.2,-1.95857581700002));
#350984=CARTESIAN_POINT('Ctrl Pts',(3.92304895199994,12.2,-1.95865207300002));
#350985=CARTESIAN_POINT('Ctrl Pts',(3.92304895199994,5.2,-1.95865207300002));
#350986=CARTESIAN_POINT('Ctrl Pts',(3.92304895199994,2.2,-1.95865207300002));
#350987=CARTESIAN_POINT('Ctrl Pts',(3.92505683199994,12.2,-1.95872625700002));
#350988=CARTESIAN_POINT('Ctrl Pts',(3.92505683199994,5.2,-1.95872625700002));
#350989=CARTESIAN_POINT('Ctrl Pts',(3.92505683199994,2.2,-1.95872625700002));
#350990=CARTESIAN_POINT('Ctrl Pts',(3.92706884999994,12.2,-1.95879836000001));
#350991=CARTESIAN_POINT('Ctrl Pts',(3.92706884999994,5.2,-1.95879836000001));
#350992=CARTESIAN_POINT('Ctrl Pts',(3.92706884999994,2.2,-1.95879836000001));
#350993=CARTESIAN_POINT('Ctrl Pts',(3.92908500099994,12.2,-1.95886837500002));
#350994=CARTESIAN_POINT('Ctrl Pts',(3.92908500099994,5.2,-1.95886837500002));
#350995=CARTESIAN_POINT('Ctrl Pts',(3.92908500099994,2.2,-1.95886837500002));
#350996=CARTESIAN_POINT('Ctrl Pts',(3.93110527499994,12.2,-1.95893629500001));
#350997=CARTESIAN_POINT('Ctrl Pts',(3.93110527499994,5.2,-1.95893629500001));
#350998=CARTESIAN_POINT('Ctrl Pts',(3.93110527499994,2.2,-1.95893629500001));
#350999=CARTESIAN_POINT('Ctrl Pts',(3.93312966599995,12.2,-1.95900210900001));
#351000=CARTESIAN_POINT('Ctrl Pts',(3.93312966599995,5.2,-1.95900210900001));
#351001=CARTESIAN_POINT('Ctrl Pts',(3.93312966599995,2.2,-1.95900210900001));
#351002=CARTESIAN_POINT('Ctrl Pts',(3.93515816899995,12.2,-1.95906581000001));
#351003=CARTESIAN_POINT('Ctrl Pts',(3.93515816899995,5.2,-1.95906581000001));
#351004=CARTESIAN_POINT('Ctrl Pts',(3.93515816899995,2.2,-1.95906581000001));
#351005=CARTESIAN_POINT('Ctrl Pts',(3.93719077599994,12.2,-1.95912739000002));
#351006=CARTESIAN_POINT('Ctrl Pts',(3.93719077599994,5.2,-1.95912739000002));
#351007=CARTESIAN_POINT('Ctrl Pts',(3.93719077599994,2.2,-1.95912739000002));
#351008=CARTESIAN_POINT('Ctrl Pts',(3.93922747899994,12.2,-1.95918683900001));
#351009=CARTESIAN_POINT('Ctrl Pts',(3.93922747899994,5.2,-1.95918683900001));
#351010=CARTESIAN_POINT('Ctrl Pts',(3.93922747899994,2.2,-1.95918683900001));
#351011=CARTESIAN_POINT('Ctrl Pts',(3.94126827199994,12.2,-1.95924415200002));
#351012=CARTESIAN_POINT('Ctrl Pts',(3.94126827199994,5.2,-1.95924415200002));
#351013=CARTESIAN_POINT('Ctrl Pts',(3.94126827199994,2.2,-1.95924415200002));
#351014=CARTESIAN_POINT('Ctrl Pts',(3.94331314799994,12.2,-1.95929931800002));
#351015=CARTESIAN_POINT('Ctrl Pts',(3.94331314799994,5.2,-1.95929931800002));
#351016=CARTESIAN_POINT('Ctrl Pts',(3.94331314799994,2.2,-1.95929931800002));
#351017=CARTESIAN_POINT('Ctrl Pts',(3.94536209899994,12.2,-1.95935233100001));
#351018=CARTESIAN_POINT('Ctrl Pts',(3.94536209899994,5.2,-1.95935233100001));
#351019=CARTESIAN_POINT('Ctrl Pts',(3.94536209899994,2.2,-1.95935233100001));
#351020=CARTESIAN_POINT('Ctrl Pts',(3.94741511999994,12.2,-1.95940318100002));
#351021=CARTESIAN_POINT('Ctrl Pts',(3.94741511999994,5.2,-1.95940318100002));
#351022=CARTESIAN_POINT('Ctrl Pts',(3.94741511999994,2.2,-1.95940318100002));
#351023=CARTESIAN_POINT('Ctrl Pts',(3.94947220299994,12.2,-1.95945186100001));
#351024=CARTESIAN_POINT('Ctrl Pts',(3.94947220299994,5.2,-1.95945186100001));
#351025=CARTESIAN_POINT('Ctrl Pts',(3.94947220299994,2.2,-1.95945186100001));
#351026=CARTESIAN_POINT('Ctrl Pts',(3.95153334099994,12.2,-1.95949836300001));
#351027=CARTESIAN_POINT('Ctrl Pts',(3.95153334099994,5.2,-1.95949836300001));
#351028=CARTESIAN_POINT('Ctrl Pts',(3.95153334099994,2.2,-1.95949836300001));
#351029=CARTESIAN_POINT('Ctrl Pts',(3.95359852699994,12.2,-1.95954267800001));
#351030=CARTESIAN_POINT('Ctrl Pts',(3.95359852699994,5.2,-1.95954267800001));
#351031=CARTESIAN_POINT('Ctrl Pts',(3.95359852699994,2.2,-1.95954267800001));
#351032=CARTESIAN_POINT('Ctrl Pts',(3.95566775399994,12.2,-1.95958480000002));
#351033=CARTESIAN_POINT('Ctrl Pts',(3.95566775399994,5.2,-1.95958480000002));
#351034=CARTESIAN_POINT('Ctrl Pts',(3.95566775399994,2.2,-1.95958480000002));
#351035=CARTESIAN_POINT('Ctrl Pts',(3.95774101599994,12.2,-1.95962471800001));
#351036=CARTESIAN_POINT('Ctrl Pts',(3.95774101599994,5.2,-1.95962471800001));
#351037=CARTESIAN_POINT('Ctrl Pts',(3.95774101599994,2.2,-1.95962471800001));
#351038=CARTESIAN_POINT('Ctrl Pts',(3.95981830499994,12.2,-1.95966242600001));
#351039=CARTESIAN_POINT('Ctrl Pts',(3.95981830499994,5.2,-1.95966242600001));
#351040=CARTESIAN_POINT('Ctrl Pts',(3.95981830499994,2.2,-1.95966242600001));
#351041=CARTESIAN_POINT('Ctrl Pts',(3.96189961499994,12.2,-1.95969791700001));
#351042=CARTESIAN_POINT('Ctrl Pts',(3.96189961499994,5.2,-1.95969791700001));
#351043=CARTESIAN_POINT('Ctrl Pts',(3.96189961499994,2.2,-1.95969791700001));
#351044=CARTESIAN_POINT('Ctrl Pts',(3.96398493799994,12.2,-1.95973118100001));
#351045=CARTESIAN_POINT('Ctrl Pts',(3.96398493799994,5.2,-1.95973118100001));
#351046=CARTESIAN_POINT('Ctrl Pts',(3.96398493799994,2.2,-1.95973118100001));
#351047=CARTESIAN_POINT('Ctrl Pts',(3.96607426699994,12.2,-1.95976221100001));
#351048=CARTESIAN_POINT('Ctrl Pts',(3.96607426699994,5.2,-1.95976221100001));
#351049=CARTESIAN_POINT('Ctrl Pts',(3.96607426699994,2.2,-1.95976221100001));
#351050=CARTESIAN_POINT('Ctrl Pts',(3.96816759599994,12.2,-1.95979099800001));
#351051=CARTESIAN_POINT('Ctrl Pts',(3.96816759599994,5.2,-1.95979099800001));
#351052=CARTESIAN_POINT('Ctrl Pts',(3.96816759599994,2.2,-1.95979099800001));
#351053=CARTESIAN_POINT('Ctrl Pts',(3.97026491799994,12.2,-1.95981753700002));
#351054=CARTESIAN_POINT('Ctrl Pts',(3.97026491799994,5.2,-1.95981753700002));
#351055=CARTESIAN_POINT('Ctrl Pts',(3.97026491799994,2.2,-1.95981753700002));
#351056=CARTESIAN_POINT('Ctrl Pts',(3.97236622599995,12.2,-1.95984181700001));
#351057=CARTESIAN_POINT('Ctrl Pts',(3.97236622599995,5.2,-1.95984181700001));
#351058=CARTESIAN_POINT('Ctrl Pts',(3.97236622599995,2.2,-1.95984181700001));
#351059=CARTESIAN_POINT('Ctrl Pts',(3.97447151099994,12.2,-1.95986383200002));
#351060=CARTESIAN_POINT('Ctrl Pts',(3.97447151099994,5.2,-1.95986383200002));
#351061=CARTESIAN_POINT('Ctrl Pts',(3.97447151099994,2.2,-1.95986383200002));
#351062=CARTESIAN_POINT('Ctrl Pts',(3.97658076899994,12.2,-1.95988357400001));
#351063=CARTESIAN_POINT('Ctrl Pts',(3.97658076899994,5.2,-1.95988357400001));
#351064=CARTESIAN_POINT('Ctrl Pts',(3.97658076899994,2.2,-1.95988357400001));
#351065=CARTESIAN_POINT('Ctrl Pts',(3.97869399199994,12.2,-1.95990103400002));
#351066=CARTESIAN_POINT('Ctrl Pts',(3.97869399199994,5.2,-1.95990103400002));
#351067=CARTESIAN_POINT('Ctrl Pts',(3.97869399199994,2.2,-1.95990103400002));
#351068=CARTESIAN_POINT('Ctrl Pts',(3.98081117199994,12.2,-1.95991620600001));
#351069=CARTESIAN_POINT('Ctrl Pts',(3.98081117199994,5.2,-1.95991620600001));
#351070=CARTESIAN_POINT('Ctrl Pts',(3.98081117199994,2.2,-1.95991620600001));
#351071=CARTESIAN_POINT('Ctrl Pts',(3.98293230399994,12.2,-1.95992908000001));
#351072=CARTESIAN_POINT('Ctrl Pts',(3.98293230399994,5.2,-1.95992908000001));
#351073=CARTESIAN_POINT('Ctrl Pts',(3.98293230399994,2.2,-1.95992908000001));
#351074=CARTESIAN_POINT('Ctrl Pts',(3.98505737899994,12.2,-1.95993965100001));
#351075=CARTESIAN_POINT('Ctrl Pts',(3.98505737899994,5.2,-1.95993965100001));
#351076=CARTESIAN_POINT('Ctrl Pts',(3.98505737899994,2.2,-1.95993965100001));
#351077=CARTESIAN_POINT('Ctrl Pts',(3.98718639199994,12.2,-1.95994791000001));
#351078=CARTESIAN_POINT('Ctrl Pts',(3.98718639199994,5.2,-1.95994791000001));
#351079=CARTESIAN_POINT('Ctrl Pts',(3.98718639199994,2.2,-1.95994791000001));
#351080=CARTESIAN_POINT('Ctrl Pts',(3.98931933399994,12.2,-1.95995384900002));
#351081=CARTESIAN_POINT('Ctrl Pts',(3.98931933399994,5.2,-1.95995384900002));
#351082=CARTESIAN_POINT('Ctrl Pts',(3.98931933399994,2.2,-1.95995384900002));
#351083=CARTESIAN_POINT('Ctrl Pts',(3.99145619999994,12.2,-1.95995746100001));
#351084=CARTESIAN_POINT('Ctrl Pts',(3.99145619999994,5.2,-1.95995746100001));
#351085=CARTESIAN_POINT('Ctrl Pts',(3.99145619999994,2.2,-1.95995746100001));
#351086=CARTESIAN_POINT('Ctrl Pts',(3.99359698299994,12.2,-1.95995873700001));
#351087=CARTESIAN_POINT('Ctrl Pts',(3.99359698299994,5.2,-1.95995873700001));
#351088=CARTESIAN_POINT('Ctrl Pts',(3.99359698299994,2.2,-1.95995873700001));
#351089=CARTESIAN_POINT('Ctrl Pts',(3.99574167399994,12.2,-1.95995767100001));
#351090=CARTESIAN_POINT('Ctrl Pts',(3.99574167399994,5.2,-1.95995767100001));
#351091=CARTESIAN_POINT('Ctrl Pts',(3.99574167399994,2.2,-1.95995767100001));
#351092=CARTESIAN_POINT('Ctrl Pts',(3.99789026699994,12.2,-1.95995425500001));
#351093=CARTESIAN_POINT('Ctrl Pts',(3.99789026699994,5.2,-1.95995425500001));
#351094=CARTESIAN_POINT('Ctrl Pts',(3.99789026699994,2.2,-1.95995425500001));
#351095=CARTESIAN_POINT('Ctrl Pts',(4.00004275699995,12.2,-1.95994848100002));
#351096=CARTESIAN_POINT('Ctrl Pts',(4.00004275699995,5.2,-1.95994848100002));
#351097=CARTESIAN_POINT('Ctrl Pts',(4.00004275699995,2.2,-1.95994848100002));
#351098=CARTESIAN_POINT('Ctrl Pts',(4.00219913399994,12.2,-1.95994034100002));
#351099=CARTESIAN_POINT('Ctrl Pts',(4.00219913399994,5.2,-1.95994034100002));
#351100=CARTESIAN_POINT('Ctrl Pts',(4.00219913399994,2.2,-1.95994034100002));
#351101=CARTESIAN_POINT('Ctrl Pts',(4.00435939399994,12.2,-1.95992982900002));
#351102=CARTESIAN_POINT('Ctrl Pts',(4.00435939399994,5.2,-1.95992982900002));
#351103=CARTESIAN_POINT('Ctrl Pts',(4.00435939399994,2.2,-1.95992982900002));
#351104=CARTESIAN_POINT('Ctrl Pts',(4.00652352699994,12.2,-1.95991693600002));
#351105=CARTESIAN_POINT('Ctrl Pts',(4.00652352699994,5.2,-1.95991693600002));
#351106=CARTESIAN_POINT('Ctrl Pts',(4.00652352699994,2.2,-1.95991693600002));
#351107=CARTESIAN_POINT('Ctrl Pts',(4.00869152799994,12.2,-1.95990165600001));
#351108=CARTESIAN_POINT('Ctrl Pts',(4.00869152799994,5.2,-1.95990165600001));
#351109=CARTESIAN_POINT('Ctrl Pts',(4.00869152799994,2.2,-1.95990165600001));
#351110=CARTESIAN_POINT('Ctrl Pts',(4.01086338899994,12.2,-1.95988398100001));
#351111=CARTESIAN_POINT('Ctrl Pts',(4.01086338899994,5.2,-1.95988398100001));
#351112=CARTESIAN_POINT('Ctrl Pts',(4.01086338899994,2.2,-1.95988398100001));
#351113=CARTESIAN_POINT('Ctrl Pts',(4.01303910599994,12.2,-1.95986390200002));
#351114=CARTESIAN_POINT('Ctrl Pts',(4.01303910599994,5.2,-1.95986390200002));
#351115=CARTESIAN_POINT('Ctrl Pts',(4.01303910599994,2.2,-1.95986390200002));
#351116=CARTESIAN_POINT('Ctrl Pts',(4.01521866799994,12.2,-1.95984141300002));
#351117=CARTESIAN_POINT('Ctrl Pts',(4.01521866799994,5.2,-1.95984141300002));
#351118=CARTESIAN_POINT('Ctrl Pts',(4.01521866799994,2.2,-1.95984141300002));
#351119=CARTESIAN_POINT('Ctrl Pts',(4.01740206999994,12.2,-1.95981650700002));
#351120=CARTESIAN_POINT('Ctrl Pts',(4.01740206999994,5.2,-1.95981650700002));
#351121=CARTESIAN_POINT('Ctrl Pts',(4.01740206999994,2.2,-1.95981650700002));
#351122=CARTESIAN_POINT('Ctrl Pts',(4.01958930399995,12.2,-1.95978917600002));
#351123=CARTESIAN_POINT('Ctrl Pts',(4.01958930399995,5.2,-1.95978917600002));
#351124=CARTESIAN_POINT('Ctrl Pts',(4.01958930399995,2.2,-1.95978917600002));
#351125=CARTESIAN_POINT('Ctrl Pts',(4.02178036499994,12.2,-1.95975941200001));
#351126=CARTESIAN_POINT('Ctrl Pts',(4.02178036499994,5.2,-1.95975941200001));
#351127=CARTESIAN_POINT('Ctrl Pts',(4.02178036499994,2.2,-1.95975941200001));
#351128=CARTESIAN_POINT('Ctrl Pts',(4.02397524499994,12.2,-1.95972720900001));
#351129=CARTESIAN_POINT('Ctrl Pts',(4.02397524499994,5.2,-1.95972720900001));
#351130=CARTESIAN_POINT('Ctrl Pts',(4.02397524499994,2.2,-1.95972720900001));
#351131=CARTESIAN_POINT('Ctrl Pts',(4.02617393699995,12.2,-1.95969255800001));
#351132=CARTESIAN_POINT('Ctrl Pts',(4.02617393699995,5.2,-1.95969255800001));
#351133=CARTESIAN_POINT('Ctrl Pts',(4.02617393699995,2.2,-1.95969255800001));
#351134=CARTESIAN_POINT('Ctrl Pts',(4.02837643299994,12.2,-1.95965545400002));
#351135=CARTESIAN_POINT('Ctrl Pts',(4.02837643299994,5.2,-1.95965545400002));
#351136=CARTESIAN_POINT('Ctrl Pts',(4.02837643299994,2.2,-1.95965545400002));
#351137=CARTESIAN_POINT('Ctrl Pts',(4.03058272899994,12.2,-1.95961588700001));
#351138=CARTESIAN_POINT('Ctrl Pts',(4.03058272899994,5.2,-1.95961588700001));
#351139=CARTESIAN_POINT('Ctrl Pts',(4.03058272899994,2.2,-1.95961588700001));
#351140=CARTESIAN_POINT('Ctrl Pts',(4.03279281399994,12.2,-1.95957385300002));
#351141=CARTESIAN_POINT('Ctrl Pts',(4.03279281399994,5.2,-1.95957385300002));
#351142=CARTESIAN_POINT('Ctrl Pts',(4.03279281399994,2.2,-1.95957385300002));
#351143=CARTESIAN_POINT('Ctrl Pts',(4.03500668499994,12.2,-1.95952934100001));
#351144=CARTESIAN_POINT('Ctrl Pts',(4.03500668499994,5.2,-1.95952934100001));
#351145=CARTESIAN_POINT('Ctrl Pts',(4.03500668499994,2.2,-1.95952934100001));
#351146=CARTESIAN_POINT('Ctrl Pts',(4.03722433299994,12.2,-1.95948234700001));
#351147=CARTESIAN_POINT('Ctrl Pts',(4.03722433299994,5.2,-1.95948234700001));
#351148=CARTESIAN_POINT('Ctrl Pts',(4.03722433299994,2.2,-1.95948234700001));
#351149=CARTESIAN_POINT('Ctrl Pts',(4.03944575099994,12.2,-1.95943286200002));
#351150=CARTESIAN_POINT('Ctrl Pts',(4.03944575099994,5.2,-1.95943286200002));
#351151=CARTESIAN_POINT('Ctrl Pts',(4.03944575099994,2.2,-1.95943286200002));
#351152=CARTESIAN_POINT('Ctrl Pts',(4.04167093199994,12.2,-1.95938087800001));
#351153=CARTESIAN_POINT('Ctrl Pts',(4.04167093199994,5.2,-1.95938087800001));
#351154=CARTESIAN_POINT('Ctrl Pts',(4.04167093199994,2.2,-1.95938087800001));
#351155=CARTESIAN_POINT('Ctrl Pts',(4.04389986999994,12.2,-1.95932639000001));
#351156=CARTESIAN_POINT('Ctrl Pts',(4.04389986999994,5.2,-1.95932639000001));
#351157=CARTESIAN_POINT('Ctrl Pts',(4.04389986999994,2.2,-1.95932639000001));
#351158=CARTESIAN_POINT('Ctrl Pts',(4.04613255699994,12.2,-1.95926939100001));
#351159=CARTESIAN_POINT('Ctrl Pts',(4.04613255699994,5.2,-1.95926939100001));
#351160=CARTESIAN_POINT('Ctrl Pts',(4.04613255699994,2.2,-1.95926939100001));
#351161=CARTESIAN_POINT('Ctrl Pts',(4.04836898699994,12.2,-1.95920987100001));
#351162=CARTESIAN_POINT('Ctrl Pts',(4.04836898699994,5.2,-1.95920987100001));
#351163=CARTESIAN_POINT('Ctrl Pts',(4.04836898699994,2.2,-1.95920987100001));
#351164=CARTESIAN_POINT('Ctrl Pts',(4.05060915299994,12.2,-1.95914782500001));
#351165=CARTESIAN_POINT('Ctrl Pts',(4.05060915299994,5.2,-1.95914782500001));
#351166=CARTESIAN_POINT('Ctrl Pts',(4.05060915299994,2.2,-1.95914782500001));
#351167=CARTESIAN_POINT('Ctrl Pts',(4.05285304699994,12.2,-1.95908324700001));
#351168=CARTESIAN_POINT('Ctrl Pts',(4.05285304699994,5.2,-1.95908324700001));
#351169=CARTESIAN_POINT('Ctrl Pts',(4.05285304699994,2.2,-1.95908324700001));
#351170=CARTESIAN_POINT('Ctrl Pts',(4.05510066299995,12.2,-1.95901612800002));
#351171=CARTESIAN_POINT('Ctrl Pts',(4.05510066299995,5.2,-1.95901612800002));
#351172=CARTESIAN_POINT('Ctrl Pts',(4.05510066299995,2.2,-1.95901612800002));
#351173=CARTESIAN_POINT('Ctrl Pts',(4.05735199399994,12.2,-1.95894646100002));
#351174=CARTESIAN_POINT('Ctrl Pts',(4.05735199399994,5.2,-1.95894646100002));
#351175=CARTESIAN_POINT('Ctrl Pts',(4.05735199399994,2.2,-1.95894646100002));
#351176=CARTESIAN_POINT('Ctrl Pts',(4.05960703199994,12.2,-1.95887423900002));
#351177=CARTESIAN_POINT('Ctrl Pts',(4.05960703199994,5.2,-1.95887423900002));
#351178=CARTESIAN_POINT('Ctrl Pts',(4.05960703199994,2.2,-1.95887423900002));
#351179=CARTESIAN_POINT('Ctrl Pts',(4.06186577099994,12.2,-1.95879945700002));
#351180=CARTESIAN_POINT('Ctrl Pts',(4.06186577099994,5.2,-1.95879945700002));
#351181=CARTESIAN_POINT('Ctrl Pts',(4.06186577099994,2.2,-1.95879945700002));
#351182=CARTESIAN_POINT('Ctrl Pts',(4.06412820499995,12.2,-1.95872210500001));
#351183=CARTESIAN_POINT('Ctrl Pts',(4.06412820499995,5.2,-1.95872210500001));
#351184=CARTESIAN_POINT('Ctrl Pts',(4.06412820499995,2.2,-1.95872210500001));
#351185=CARTESIAN_POINT('Ctrl Pts',(4.06639432499994,12.2,-1.95864217800001));
#351186=CARTESIAN_POINT('Ctrl Pts',(4.06639432499994,5.2,-1.95864217800001));
#351187=CARTESIAN_POINT('Ctrl Pts',(4.06639432499994,2.2,-1.95864217800001));
#351188=CARTESIAN_POINT('Ctrl Pts',(4.06866412499994,12.2,-1.95855966900002));
#351189=CARTESIAN_POINT('Ctrl Pts',(4.06866412499994,5.2,-1.95855966900002));
#351190=CARTESIAN_POINT('Ctrl Pts',(4.06866412499994,2.2,-1.95855966900002));
#351191=CARTESIAN_POINT('Ctrl Pts',(4.07093759899994,12.2,-1.95847457000002));
#351192=CARTESIAN_POINT('Ctrl Pts',(4.07093759899994,5.2,-1.95847457000002));
#351193=CARTESIAN_POINT('Ctrl Pts',(4.07093759899994,2.2,-1.95847457000002));
#351194=CARTESIAN_POINT('Ctrl Pts',(4.07321473899994,12.2,-1.95838687600002));
#351195=CARTESIAN_POINT('Ctrl Pts',(4.07321473899994,5.2,-1.95838687600002));
#351196=CARTESIAN_POINT('Ctrl Pts',(4.07321473899994,2.2,-1.95838687600002));
#351197=CARTESIAN_POINT('Ctrl Pts',(4.07549553699995,12.2,-1.95829657700001));
#351198=CARTESIAN_POINT('Ctrl Pts',(4.07549553699995,5.2,-1.95829657700001));
#351199=CARTESIAN_POINT('Ctrl Pts',(4.07549553699995,2.2,-1.95829657700001));
#351200=CARTESIAN_POINT('Ctrl Pts',(4.07777998799994,12.2,-1.95820366900001));
#351201=CARTESIAN_POINT('Ctrl Pts',(4.07777998799994,5.2,-1.95820366900001));
#351202=CARTESIAN_POINT('Ctrl Pts',(4.07777998799994,2.2,-1.95820366900001));
#351203=CARTESIAN_POINT('Ctrl Pts',(4.08006808399994,12.2,-1.95810814400001));
#351204=CARTESIAN_POINT('Ctrl Pts',(4.08006808399994,5.2,-1.95810814400001));
#351205=CARTESIAN_POINT('Ctrl Pts',(4.08006808399994,2.2,-1.95810814400001));
#351206=CARTESIAN_POINT('Ctrl Pts',(4.08235981899994,12.2,-1.95800999500001));
#351207=CARTESIAN_POINT('Ctrl Pts',(4.08235981899994,5.2,-1.95800999500001));
#351208=CARTESIAN_POINT('Ctrl Pts',(4.08235981899994,2.2,-1.95800999500001));
#351209=CARTESIAN_POINT('Ctrl Pts',(4.08465518599994,12.2,-1.95790921500001));
#351210=CARTESIAN_POINT('Ctrl Pts',(4.08465518599994,5.2,-1.95790921500001));
#351211=CARTESIAN_POINT('Ctrl Pts',(4.08465518599994,2.2,-1.95790921500001));
#351212=CARTESIAN_POINT('Ctrl Pts',(4.08695417599994,12.2,-1.95780579800001));
#351213=CARTESIAN_POINT('Ctrl Pts',(4.08695417599994,5.2,-1.95780579800001));
#351214=CARTESIAN_POINT('Ctrl Pts',(4.08695417599994,2.2,-1.95780579800001));
#351215=CARTESIAN_POINT('Ctrl Pts',(4.08925678399994,12.2,-1.95769973800001));
#351216=CARTESIAN_POINT('Ctrl Pts',(4.08925678399994,5.2,-1.95769973800001));
#351217=CARTESIAN_POINT('Ctrl Pts',(4.08925678399994,2.2,-1.95769973800001));
#351218=CARTESIAN_POINT('Ctrl Pts',(4.09156300299994,12.2,-1.95759102500002));
#351219=CARTESIAN_POINT('Ctrl Pts',(4.09156300299994,5.2,-1.95759102500002));
#351220=CARTESIAN_POINT('Ctrl Pts',(4.09156300299994,2.2,-1.95759102500002));
#351221=CARTESIAN_POINT('Ctrl Pts',(4.09387282499994,12.2,-1.95747965600002));
#351222=CARTESIAN_POINT('Ctrl Pts',(4.09387282499994,5.2,-1.95747965600002));
#351223=CARTESIAN_POINT('Ctrl Pts',(4.09387282499994,2.2,-1.95747965600002));
#351224=CARTESIAN_POINT('Ctrl Pts',(4.09618624499995,12.2,-1.95736562200001));
#351225=CARTESIAN_POINT('Ctrl Pts',(4.09618624499995,5.2,-1.95736562200001));
#351226=CARTESIAN_POINT('Ctrl Pts',(4.09618624499995,2.2,-1.95736562200001));
#351227=CARTESIAN_POINT('Ctrl Pts',(4.09850325399994,12.2,-1.95724891700001));
#351228=CARTESIAN_POINT('Ctrl Pts',(4.09850325399994,5.2,-1.95724891700001));
#351229=CARTESIAN_POINT('Ctrl Pts',(4.09850325399994,2.2,-1.95724891700001));
#351230=CARTESIAN_POINT('Ctrl Pts',(4.10082384499994,12.2,-1.95712953400001));
#351231=CARTESIAN_POINT('Ctrl Pts',(4.10082384499994,5.2,-1.95712953400001));
#351232=CARTESIAN_POINT('Ctrl Pts',(4.10082384499994,2.2,-1.95712953400001));
#351233=CARTESIAN_POINT('Ctrl Pts',(4.10314801299995,12.2,-1.95700746600001));
#351234=CARTESIAN_POINT('Ctrl Pts',(4.10314801299995,5.2,-1.95700746600001));
#351235=CARTESIAN_POINT('Ctrl Pts',(4.10314801299995,2.2,-1.95700746600001));
#351236=CARTESIAN_POINT('Ctrl Pts',(4.10547574999994,12.2,-1.95688270800002));
#351237=CARTESIAN_POINT('Ctrl Pts',(4.10547574999994,5.2,-1.95688270800002));
#351238=CARTESIAN_POINT('Ctrl Pts',(4.10547574999994,2.2,-1.95688270800002));
#351239=CARTESIAN_POINT('Ctrl Pts',(4.10780704799994,12.2,-1.95675525200001));
#351240=CARTESIAN_POINT('Ctrl Pts',(4.10780704799994,5.2,-1.95675525200001));
#351241=CARTESIAN_POINT('Ctrl Pts',(4.10780704799994,2.2,-1.95675525200001));
#351242=CARTESIAN_POINT('Ctrl Pts',(4.11014190199994,12.2,-1.95662509100002));
#351243=CARTESIAN_POINT('Ctrl Pts',(4.11014190199994,5.2,-1.95662509100002));
#351244=CARTESIAN_POINT('Ctrl Pts',(4.11014190199994,2.2,-1.95662509100002));
#351245=CARTESIAN_POINT('Ctrl Pts',(4.11248030499994,12.2,-1.95649222000001));
#351246=CARTESIAN_POINT('Ctrl Pts',(4.11248030499994,5.2,-1.95649222000001));
#351247=CARTESIAN_POINT('Ctrl Pts',(4.11248030499994,2.2,-1.95649222000001));
#351248=CARTESIAN_POINT('Ctrl Pts',(4.11482224699994,12.2,-1.95635663100001));
#351249=CARTESIAN_POINT('Ctrl Pts',(4.11482224699994,5.2,-1.95635663100001));
#351250=CARTESIAN_POINT('Ctrl Pts',(4.11482224699994,2.2,-1.95635663100001));
#351251=CARTESIAN_POINT('Ctrl Pts',(4.11716772399994,12.2,-1.95621831700001));
#351252=CARTESIAN_POINT('Ctrl Pts',(4.11716772399994,5.2,-1.95621831700001));
#351253=CARTESIAN_POINT('Ctrl Pts',(4.11716772399994,2.2,-1.95621831700001));
#351254=CARTESIAN_POINT('Ctrl Pts',(4.11951672899994,12.2,-1.95607727400001));
#351255=CARTESIAN_POINT('Ctrl Pts',(4.11951672899994,5.2,-1.95607727400001));
#351256=CARTESIAN_POINT('Ctrl Pts',(4.11951672899994,2.2,-1.95607727400001));
#351257=CARTESIAN_POINT('Ctrl Pts',(4.12186925499994,12.2,-1.95593349300001));
#351258=CARTESIAN_POINT('Ctrl Pts',(4.12186925499994,5.2,-1.95593349300001));
#351259=CARTESIAN_POINT('Ctrl Pts',(4.12186925499994,2.2,-1.95593349300001));
#351260=CARTESIAN_POINT('Ctrl Pts',(4.12422529299994,12.2,-1.95578696800002));
#351261=CARTESIAN_POINT('Ctrl Pts',(4.12422529299994,5.2,-1.95578696800002));
#351262=CARTESIAN_POINT('Ctrl Pts',(4.12422529299994,2.2,-1.95578696800002));
#351263=CARTESIAN_POINT('Ctrl Pts',(4.12658483799994,12.2,-1.95563769400001));
#351264=CARTESIAN_POINT('Ctrl Pts',(4.12658483799994,5.2,-1.95563769400001));
#351265=CARTESIAN_POINT('Ctrl Pts',(4.12658483799994,2.2,-1.95563769400001));
#351266=CARTESIAN_POINT('Ctrl Pts',(4.12894788199995,12.2,-1.95548566200001));
#351267=CARTESIAN_POINT('Ctrl Pts',(4.12894788199995,5.2,-1.95548566200001));
#351268=CARTESIAN_POINT('Ctrl Pts',(4.12894788199995,2.2,-1.95548566200001));
#351269=CARTESIAN_POINT('Ctrl Pts',(4.13131441899994,12.2,-1.95533086900001));
#351270=CARTESIAN_POINT('Ctrl Pts',(4.13131441899994,5.2,-1.95533086900001));
#351271=CARTESIAN_POINT('Ctrl Pts',(4.13131441899994,2.2,-1.95533086900001));
#351272=CARTESIAN_POINT('Ctrl Pts',(4.13368444199994,12.2,-1.95517330500001));
#351273=CARTESIAN_POINT('Ctrl Pts',(4.13368444199994,5.2,-1.95517330500001));
#351274=CARTESIAN_POINT('Ctrl Pts',(4.13368444199994,2.2,-1.95517330500001));
#351275=CARTESIAN_POINT('Ctrl Pts',(4.13605794499994,12.2,-1.95501296600002));
#351276=CARTESIAN_POINT('Ctrl Pts',(4.13605794499994,5.2,-1.95501296600002));
#351277=CARTESIAN_POINT('Ctrl Pts',(4.13605794499994,2.2,-1.95501296600002));
#351278=CARTESIAN_POINT('Ctrl Pts',(4.13843491799994,12.2,-1.95484984400002));
#351279=CARTESIAN_POINT('Ctrl Pts',(4.13843491799994,5.2,-1.95484984400002));
#351280=CARTESIAN_POINT('Ctrl Pts',(4.13843491799994,2.2,-1.95484984400002));
#351281=CARTESIAN_POINT('Ctrl Pts',(4.14081535599994,12.2,-1.95468393300001));
#351282=CARTESIAN_POINT('Ctrl Pts',(4.14081535599994,5.2,-1.95468393300001));
#351283=CARTESIAN_POINT('Ctrl Pts',(4.14081535599994,2.2,-1.95468393300001));
#351284=CARTESIAN_POINT('Ctrl Pts',(4.14319925299994,12.2,-1.95451522700001));
#351285=CARTESIAN_POINT('Ctrl Pts',(4.14319925299994,5.2,-1.95451522700001));
#351286=CARTESIAN_POINT('Ctrl Pts',(4.14319925299994,2.2,-1.95451522700001));
#351287=CARTESIAN_POINT('Ctrl Pts',(4.14558659999994,12.2,-1.95434372100001));
#351288=CARTESIAN_POINT('Ctrl Pts',(4.14558659999994,5.2,-1.95434372100001));
#351289=CARTESIAN_POINT('Ctrl Pts',(4.14558659999994,2.2,-1.95434372100001));
#351290=CARTESIAN_POINT('Ctrl Pts',(4.14797739099994,12.2,-1.95416940600001));
#351291=CARTESIAN_POINT('Ctrl Pts',(4.14797739099994,5.2,-1.95416940600001));
#351292=CARTESIAN_POINT('Ctrl Pts',(4.14797739099994,2.2,-1.95416940600001));
#351293=CARTESIAN_POINT('Ctrl Pts',(4.15037161999994,12.2,-1.95399227800001));
#351294=CARTESIAN_POINT('Ctrl Pts',(4.15037161999994,5.2,-1.95399227800001));
#351295=CARTESIAN_POINT('Ctrl Pts',(4.15037161999994,2.2,-1.95399227800001));
#351296=CARTESIAN_POINT('Ctrl Pts',(4.15276927899995,12.2,-1.95381233000001));
#351297=CARTESIAN_POINT('Ctrl Pts',(4.15276927899995,5.2,-1.95381233000001));
#351298=CARTESIAN_POINT('Ctrl Pts',(4.15276927899995,2.2,-1.95381233000001));
#351299=CARTESIAN_POINT('Ctrl Pts',(4.15517036099994,12.2,-1.95362955500002));
#351300=CARTESIAN_POINT('Ctrl Pts',(4.15517036099994,5.2,-1.95362955500002));
#351301=CARTESIAN_POINT('Ctrl Pts',(4.15517036099994,2.2,-1.95362955500002));
#351302=CARTESIAN_POINT('Ctrl Pts',(4.15757485899994,12.2,-1.95344394600002));
#351303=CARTESIAN_POINT('Ctrl Pts',(4.15757485899994,5.2,-1.95344394600002));
#351304=CARTESIAN_POINT('Ctrl Pts',(4.15757485899994,2.2,-1.95344394600002));
#351305=CARTESIAN_POINT('Ctrl Pts',(4.15998276699994,12.2,-1.95325549900002));
#351306=CARTESIAN_POINT('Ctrl Pts',(4.15998276699994,5.2,-1.95325549900002));
#351307=CARTESIAN_POINT('Ctrl Pts',(4.15998276699994,2.2,-1.95325549900002));
#351308=CARTESIAN_POINT('Ctrl Pts',(4.16239407799995,12.2,-1.95306420700001));
#351309=CARTESIAN_POINT('Ctrl Pts',(4.16239407799995,5.2,-1.95306420700001));
#351310=CARTESIAN_POINT('Ctrl Pts',(4.16239407799995,2.2,-1.95306420700001));
#351311=CARTESIAN_POINT('Ctrl Pts',(4.16480878399994,12.2,-1.95287006400001));
#351312=CARTESIAN_POINT('Ctrl Pts',(4.16480878399994,5.2,-1.95287006400001));
#351313=CARTESIAN_POINT('Ctrl Pts',(4.16480878399994,2.2,-1.95287006400001));
#351314=CARTESIAN_POINT('Ctrl Pts',(4.16722687799994,12.2,-1.95267306200002));
#351315=CARTESIAN_POINT('Ctrl Pts',(4.16722687799994,5.2,-1.95267306200002));
#351316=CARTESIAN_POINT('Ctrl Pts',(4.16722687799994,2.2,-1.95267306200002));
#351317=CARTESIAN_POINT('Ctrl Pts',(4.16964835399994,12.2,-1.95247319700002));
#351318=CARTESIAN_POINT('Ctrl Pts',(4.16964835399994,5.2,-1.95247319700002));
#351319=CARTESIAN_POINT('Ctrl Pts',(4.16964835399994,2.2,-1.95247319700002));
#351320=CARTESIAN_POINT('Ctrl Pts',(4.17207320499995,12.2,-1.95227046200001));
#351321=CARTESIAN_POINT('Ctrl Pts',(4.17207320499995,5.2,-1.95227046200001));
#351322=CARTESIAN_POINT('Ctrl Pts',(4.17207320499995,2.2,-1.95227046200001));
#351323=CARTESIAN_POINT('Ctrl Pts',(4.17450142499994,12.2,-1.95206485100002));
#351324=CARTESIAN_POINT('Ctrl Pts',(4.17450142499994,5.2,-1.95206485100002));
#351325=CARTESIAN_POINT('Ctrl Pts',(4.17450142499994,2.2,-1.95206485100002));
#351326=CARTESIAN_POINT('Ctrl Pts',(4.17693300399994,12.2,-1.95185635800001));
#351327=CARTESIAN_POINT('Ctrl Pts',(4.17693300399994,5.2,-1.95185635800001));
#351328=CARTESIAN_POINT('Ctrl Pts',(4.17693300399994,2.2,-1.95185635800001));
#351329=CARTESIAN_POINT('Ctrl Pts',(4.17936793799994,12.2,-1.95164497700001));
#351330=CARTESIAN_POINT('Ctrl Pts',(4.17936793799994,5.2,-1.95164497700001));
#351331=CARTESIAN_POINT('Ctrl Pts',(4.17936793799994,2.2,-1.95164497700001));
#351332=CARTESIAN_POINT('Ctrl Pts',(4.18180621899995,12.2,-1.95143070000002));
#351333=CARTESIAN_POINT('Ctrl Pts',(4.18180621899995,5.2,-1.95143070000002));
#351334=CARTESIAN_POINT('Ctrl Pts',(4.18180621899995,2.2,-1.95143070000002));
#351335=CARTESIAN_POINT('Ctrl Pts',(4.18424783999995,12.2,-1.95121352400002));
#351336=CARTESIAN_POINT('Ctrl Pts',(4.18424783999995,5.2,-1.95121352400002));
#351337=CARTESIAN_POINT('Ctrl Pts',(4.18424783999995,2.2,-1.95121352400002));
#351338=CARTESIAN_POINT('Ctrl Pts',(4.18669279499994,12.2,-1.95099344200001));
#351339=CARTESIAN_POINT('Ctrl Pts',(4.18669279499994,5.2,-1.95099344200001));
#351340=CARTESIAN_POINT('Ctrl Pts',(4.18669279499994,2.2,-1.95099344200001));
#351341=CARTESIAN_POINT('Ctrl Pts',(4.18914107499995,12.2,-1.95077044700001));
#351342=CARTESIAN_POINT('Ctrl Pts',(4.18914107499995,5.2,-1.95077044700001));
#351343=CARTESIAN_POINT('Ctrl Pts',(4.18914107499995,2.2,-1.95077044700001));
#351344=CARTESIAN_POINT('Ctrl Pts',(4.19159267499994,12.2,-1.95054453300001));
#351345=CARTESIAN_POINT('Ctrl Pts',(4.19159267499994,5.2,-1.95054453300001));
#351346=CARTESIAN_POINT('Ctrl Pts',(4.19159267499994,2.2,-1.95054453300001));
#351347=CARTESIAN_POINT('Ctrl Pts',(4.19404758699994,12.2,-1.95031569600001));
#351348=CARTESIAN_POINT('Ctrl Pts',(4.19404758699994,5.2,-1.95031569600001));
#351349=CARTESIAN_POINT('Ctrl Pts',(4.19404758699994,2.2,-1.95031569600001));
#351350=CARTESIAN_POINT('Ctrl Pts',(4.19650580499995,12.2,-1.95008392700001));
#351351=CARTESIAN_POINT('Ctrl Pts',(4.19650580499995,5.2,-1.95008392700001));
#351352=CARTESIAN_POINT('Ctrl Pts',(4.19650580499995,2.2,-1.95008392700001));
#351353=CARTESIAN_POINT('Ctrl Pts',(4.19896732099994,12.2,-1.94984922200002));
#351354=CARTESIAN_POINT('Ctrl Pts',(4.19896732099994,5.2,-1.94984922200002));
#351355=CARTESIAN_POINT('Ctrl Pts',(4.19896732099994,2.2,-1.94984922200002));
#351356=CARTESIAN_POINT('Ctrl Pts',(4.20143212999994,12.2,-1.94961157500002));
#351357=CARTESIAN_POINT('Ctrl Pts',(4.20143212999994,5.2,-1.94961157500002));
#351358=CARTESIAN_POINT('Ctrl Pts',(4.20143212999994,2.2,-1.94961157500002));
#351359=CARTESIAN_POINT('Ctrl Pts',(4.20390022299994,12.2,-1.94937098000001));
#351360=CARTESIAN_POINT('Ctrl Pts',(4.20390022299994,5.2,-1.94937098000001));
#351361=CARTESIAN_POINT('Ctrl Pts',(4.20390022299994,2.2,-1.94937098000001));
#351362=CARTESIAN_POINT('Ctrl Pts',(4.20637159399995,12.2,-1.94912743000001));
#351363=CARTESIAN_POINT('Ctrl Pts',(4.20637159399995,5.2,-1.94912743000001));
#351364=CARTESIAN_POINT('Ctrl Pts',(4.20637159399995,2.2,-1.94912743000001));
#351365=CARTESIAN_POINT('Ctrl Pts',(4.20884623499994,12.2,-1.94888092100001));
#351366=CARTESIAN_POINT('Ctrl Pts',(4.20884623499994,5.2,-1.94888092100001));
#351367=CARTESIAN_POINT('Ctrl Pts',(4.20884623499994,2.2,-1.94888092100001));
#351368=CARTESIAN_POINT('Ctrl Pts',(4.21132414099994,12.2,-1.94863144500002));
#351369=CARTESIAN_POINT('Ctrl Pts',(4.21132414099994,5.2,-1.94863144500002));
#351370=CARTESIAN_POINT('Ctrl Pts',(4.21132414099994,2.2,-1.94863144500002));
#351371=CARTESIAN_POINT('Ctrl Pts',(4.21380530299994,12.2,-1.94837899800001));
#351372=CARTESIAN_POINT('Ctrl Pts',(4.21380530299994,5.2,-1.94837899800001));
#351373=CARTESIAN_POINT('Ctrl Pts',(4.21380530299994,2.2,-1.94837899800001));
#351374=CARTESIAN_POINT('Ctrl Pts',(4.21628971599994,12.2,-1.94812357300002));
#351375=CARTESIAN_POINT('Ctrl Pts',(4.21628971599994,5.2,-1.94812357300002));
#351376=CARTESIAN_POINT('Ctrl Pts',(4.21628971599994,2.2,-1.94812357300002));
#351377=CARTESIAN_POINT('Ctrl Pts',(4.21877737199994,12.2,-1.94786516400002));
#351378=CARTESIAN_POINT('Ctrl Pts',(4.21877737199994,5.2,-1.94786516400002));
#351379=CARTESIAN_POINT('Ctrl Pts',(4.21877737199994,2.2,-1.94786516400002));
#351380=CARTESIAN_POINT('Ctrl Pts',(4.22126826399994,12.2,-1.94760376700001));
#351381=CARTESIAN_POINT('Ctrl Pts',(4.22126826399994,5.2,-1.94760376700001));
#351382=CARTESIAN_POINT('Ctrl Pts',(4.22126826399994,2.2,-1.94760376700001));
#351383=CARTESIAN_POINT('Ctrl Pts',(4.22376238699994,12.2,-1.94733937400001));
#351384=CARTESIAN_POINT('Ctrl Pts',(4.22376238699994,5.2,-1.94733937400001));
#351385=CARTESIAN_POINT('Ctrl Pts',(4.22376238699994,2.2,-1.94733937400001));
#351386=CARTESIAN_POINT('Ctrl Pts',(4.22625973099994,12.2,-1.94707198100001));
#351387=CARTESIAN_POINT('Ctrl Pts',(4.22625973099994,5.2,-1.94707198100001));
#351388=CARTESIAN_POINT('Ctrl Pts',(4.22625973099994,2.2,-1.94707198100001));
#351389=CARTESIAN_POINT('Ctrl Pts',(4.22876029099994,12.2,-1.94680158100001));
#351390=CARTESIAN_POINT('Ctrl Pts',(4.22876029099994,5.2,-1.94680158100001));
#351391=CARTESIAN_POINT('Ctrl Pts',(4.22876029099994,2.2,-1.94680158100001));
#351392=CARTESIAN_POINT('Ctrl Pts',(4.23126405899994,12.2,-1.94652816800001));
#351393=CARTESIAN_POINT('Ctrl Pts',(4.23126405899994,5.2,-1.94652816800001));
#351394=CARTESIAN_POINT('Ctrl Pts',(4.23126405899994,2.2,-1.94652816800001));
#351395=CARTESIAN_POINT('Ctrl Pts',(4.23377102899994,12.2,-1.94625173800001));
#351396=CARTESIAN_POINT('Ctrl Pts',(4.23377102899994,5.2,-1.94625173800001));
#351397=CARTESIAN_POINT('Ctrl Pts',(4.23377102899994,2.2,-1.94625173800001));
#351398=CARTESIAN_POINT('Ctrl Pts',(4.23628119499995,12.2,-1.94597228400001));
#351399=CARTESIAN_POINT('Ctrl Pts',(4.23628119499995,5.2,-1.94597228400001));
#351400=CARTESIAN_POINT('Ctrl Pts',(4.23628119499995,2.2,-1.94597228400001));
#351401=CARTESIAN_POINT('Ctrl Pts',(4.23879454799994,12.2,-1.94568980000001));
#351402=CARTESIAN_POINT('Ctrl Pts',(4.23879454799994,5.2,-1.94568980000001));
#351403=CARTESIAN_POINT('Ctrl Pts',(4.23879454799994,2.2,-1.94568980000001));
#351404=CARTESIAN_POINT('Ctrl Pts',(4.24131108199994,12.2,-1.94540428100002));
#351405=CARTESIAN_POINT('Ctrl Pts',(4.24131108199994,5.2,-1.94540428100002));
#351406=CARTESIAN_POINT('Ctrl Pts',(4.24131108199994,2.2,-1.94540428100002));
#351407=CARTESIAN_POINT('Ctrl Pts',(4.24383078999994,12.2,-1.94511572200001));
#351408=CARTESIAN_POINT('Ctrl Pts',(4.24383078999994,5.2,-1.94511572200001));
#351409=CARTESIAN_POINT('Ctrl Pts',(4.24383078999994,2.2,-1.94511572200001));
#351410=CARTESIAN_POINT('Ctrl Pts',(4.24635366599994,12.2,-1.94482411700001));
#351411=CARTESIAN_POINT('Ctrl Pts',(4.24635366599994,5.2,-1.94482411700001));
#351412=CARTESIAN_POINT('Ctrl Pts',(4.24635366599994,2.2,-1.94482411700001));
#351413=CARTESIAN_POINT('Ctrl Pts',(4.24887970099994,12.2,-1.94452945900002));
#351414=CARTESIAN_POINT('Ctrl Pts',(4.24887970099994,5.2,-1.94452945900002));
#351415=CARTESIAN_POINT('Ctrl Pts',(4.24887970099994,2.2,-1.94452945900002));
#351416=CARTESIAN_POINT('Ctrl Pts',(4.25140889099994,12.2,-1.94423174300002));
#351417=CARTESIAN_POINT('Ctrl Pts',(4.25140889099994,5.2,-1.94423174300002));
#351418=CARTESIAN_POINT('Ctrl Pts',(4.25140889099994,2.2,-1.94423174300002));
#351419=CARTESIAN_POINT('Ctrl Pts',(4.25394122599995,12.2,-1.94393096500002));
#351420=CARTESIAN_POINT('Ctrl Pts',(4.25394122599995,5.2,-1.94393096500002));
#351421=CARTESIAN_POINT('Ctrl Pts',(4.25394122599995,2.2,-1.94393096500002));
#351422=CARTESIAN_POINT('Ctrl Pts',(4.25647670199994,12.2,-1.94362711800002));
#351423=CARTESIAN_POINT('Ctrl Pts',(4.25647670199994,5.2,-1.94362711800002));
#351424=CARTESIAN_POINT('Ctrl Pts',(4.25647670199994,2.2,-1.94362711800002));
#351425=CARTESIAN_POINT('Ctrl Pts',(4.25901530899994,12.2,-1.94332019600001));
#351426=CARTESIAN_POINT('Ctrl Pts',(4.25901530899994,5.2,-1.94332019600001));
#351427=CARTESIAN_POINT('Ctrl Pts',(4.25901530899994,2.2,-1.94332019600001));
#351428=CARTESIAN_POINT('Ctrl Pts',(4.26155704199994,12.2,-1.94301019400001));
#351429=CARTESIAN_POINT('Ctrl Pts',(4.26155704199994,5.2,-1.94301019400001));
#351430=CARTESIAN_POINT('Ctrl Pts',(4.26155704199994,2.2,-1.94301019400001));
#351431=CARTESIAN_POINT('Ctrl Pts',(4.26410189499994,12.2,-1.94269710600001));
#351432=CARTESIAN_POINT('Ctrl Pts',(4.26410189499994,5.2,-1.94269710600001));
#351433=CARTESIAN_POINT('Ctrl Pts',(4.26410189499994,2.2,-1.94269710600001));
#351434=CARTESIAN_POINT('Ctrl Pts',(4.26664985899994,12.2,-1.94238092900001));
#351435=CARTESIAN_POINT('Ctrl Pts',(4.26664985899994,5.2,-1.94238092900001));
#351436=CARTESIAN_POINT('Ctrl Pts',(4.26664985899994,2.2,-1.94238092900001));
#351437=CARTESIAN_POINT('Ctrl Pts',(4.26920092799994,12.2,-1.94206165400002));
#351438=CARTESIAN_POINT('Ctrl Pts',(4.26920092799994,5.2,-1.94206165400002));
#351439=CARTESIAN_POINT('Ctrl Pts',(4.26920092799994,2.2,-1.94206165400002));
#351440=CARTESIAN_POINT('Ctrl Pts',(4.27175509499994,12.2,-1.94173927700001));
#351441=CARTESIAN_POINT('Ctrl Pts',(4.27175509499994,5.2,-1.94173927700001));
#351442=CARTESIAN_POINT('Ctrl Pts',(4.27175509499994,2.2,-1.94173927700001));
#351443=CARTESIAN_POINT('Ctrl Pts',(4.27431235399994,12.2,-1.94141379400001));
#351444=CARTESIAN_POINT('Ctrl Pts',(4.27431235399994,5.2,-1.94141379400001));
#351445=CARTESIAN_POINT('Ctrl Pts',(4.27431235399994,2.2,-1.94141379400001));
#351446=CARTESIAN_POINT('Ctrl Pts',(4.27687269699994,12.2,-1.94108519700002));
#351447=CARTESIAN_POINT('Ctrl Pts',(4.27687269699994,5.2,-1.94108519700002));
#351448=CARTESIAN_POINT('Ctrl Pts',(4.27687269699994,2.2,-1.94108519700002));
#351449=CARTESIAN_POINT('Ctrl Pts',(4.27943611799994,12.2,-1.94075348200001));
#351450=CARTESIAN_POINT('Ctrl Pts',(4.27943611799994,5.2,-1.94075348200001));
#351451=CARTESIAN_POINT('Ctrl Pts',(4.27943611799994,2.2,-1.94075348200001));
#351452=CARTESIAN_POINT('Ctrl Pts',(4.28200260999995,12.2,-1.94041864400001));
#351453=CARTESIAN_POINT('Ctrl Pts',(4.28200260999995,5.2,-1.94041864400001));
#351454=CARTESIAN_POINT('Ctrl Pts',(4.28200260999995,2.2,-1.94041864400001));
#351455=CARTESIAN_POINT('Ctrl Pts',(4.28457216599995,12.2,-1.94008067700001));
#351456=CARTESIAN_POINT('Ctrl Pts',(4.28457216599995,5.2,-1.94008067700001));
#351457=CARTESIAN_POINT('Ctrl Pts',(4.28457216599995,2.2,-1.94008067700001));
#351458=CARTESIAN_POINT('Ctrl Pts',(4.28714477699994,12.2,-1.93973957500001));
#351459=CARTESIAN_POINT('Ctrl Pts',(4.28714477699994,5.2,-1.93973957500001));
#351460=CARTESIAN_POINT('Ctrl Pts',(4.28714477699994,2.2,-1.93973957500001));
#351461=CARTESIAN_POINT('Ctrl Pts',(4.28972043899994,12.2,-1.93939533400002));
#351462=CARTESIAN_POINT('Ctrl Pts',(4.28972043899994,5.2,-1.93939533400002));
#351463=CARTESIAN_POINT('Ctrl Pts',(4.28972043899994,2.2,-1.93939533400002));
#351464=CARTESIAN_POINT('Ctrl Pts',(4.29229914299994,12.2,-1.93904794600002));
#351465=CARTESIAN_POINT('Ctrl Pts',(4.29229914299994,5.2,-1.93904794600002));
#351466=CARTESIAN_POINT('Ctrl Pts',(4.29229914299994,2.2,-1.93904794600002));
#351467=CARTESIAN_POINT('Ctrl Pts',(4.29488088199994,12.2,-1.93869740900002));
#351468=CARTESIAN_POINT('Ctrl Pts',(4.29488088199994,5.2,-1.93869740900002));
#351469=CARTESIAN_POINT('Ctrl Pts',(4.29488088199994,2.2,-1.93869740900002));
#351470=CARTESIAN_POINT('Ctrl Pts',(4.29746564899994,12.2,-1.93834371400001));
#351471=CARTESIAN_POINT('Ctrl Pts',(4.29746564899994,5.2,-1.93834371400001));
#351472=CARTESIAN_POINT('Ctrl Pts',(4.29746564899994,2.2,-1.93834371400001));
#351473=CARTESIAN_POINT('Ctrl Pts',(4.30005343899994,12.2,-1.93798685700001));
#351474=CARTESIAN_POINT('Ctrl Pts',(4.30005343899994,5.2,-1.93798685700001));
#351475=CARTESIAN_POINT('Ctrl Pts',(4.30005343899994,2.2,-1.93798685700001));
#351476=CARTESIAN_POINT('Ctrl Pts',(4.30264424499994,12.2,-1.93762683600001));
#351477=CARTESIAN_POINT('Ctrl Pts',(4.30264424499994,5.2,-1.93762683600001));
#351478=CARTESIAN_POINT('Ctrl Pts',(4.30264424499994,2.2,-1.93762683600001));
#351479=CARTESIAN_POINT('Ctrl Pts',(4.30523806099994,12.2,-1.93726364300002));
#351480=CARTESIAN_POINT('Ctrl Pts',(4.30523806099994,5.2,-1.93726364300002));
#351481=CARTESIAN_POINT('Ctrl Pts',(4.30523806099994,2.2,-1.93726364300002));
#351482=CARTESIAN_POINT('Ctrl Pts',(4.30783487999994,12.2,-1.93689727500002));
#351483=CARTESIAN_POINT('Ctrl Pts',(4.30783487999994,5.2,-1.93689727500002));
#351484=CARTESIAN_POINT('Ctrl Pts',(4.30783487999994,2.2,-1.93689727500002));
#351485=CARTESIAN_POINT('Ctrl Pts',(4.31043469599994,12.2,-1.93652772600001));
#351486=CARTESIAN_POINT('Ctrl Pts',(4.31043469599994,5.2,-1.93652772600001));
#351487=CARTESIAN_POINT('Ctrl Pts',(4.31043469599994,2.2,-1.93652772600001));
#351488=CARTESIAN_POINT('Ctrl Pts',(4.31303749999994,12.2,-1.93615499100002));
#351489=CARTESIAN_POINT('Ctrl Pts',(4.31303749999994,5.2,-1.93615499100002));
#351490=CARTESIAN_POINT('Ctrl Pts',(4.31303749999994,2.2,-1.93615499100002));
#351491=CARTESIAN_POINT('Ctrl Pts',(4.31564328599995,12.2,-1.93577906200002));
#351492=CARTESIAN_POINT('Ctrl Pts',(4.31564328599995,5.2,-1.93577906200002));
#351493=CARTESIAN_POINT('Ctrl Pts',(4.31564328599995,2.2,-1.93577906200002));
#351494=CARTESIAN_POINT('Ctrl Pts',(4.31825204199995,12.2,-1.93539993400002));
#351495=CARTESIAN_POINT('Ctrl Pts',(4.31825204199995,5.2,-1.93539993400002));
#351496=CARTESIAN_POINT('Ctrl Pts',(4.31825204199995,2.2,-1.93539993400002));
#351497=CARTESIAN_POINT('Ctrl Pts',(4.32086376199995,12.2,-1.93501760000002));
#351498=CARTESIAN_POINT('Ctrl Pts',(4.32086376199995,5.2,-1.93501760000002));
#351499=CARTESIAN_POINT('Ctrl Pts',(4.32086376199995,2.2,-1.93501760000002));
#351500=CARTESIAN_POINT('Ctrl Pts',(4.32347843899994,12.2,-1.93463205400001));
#351501=CARTESIAN_POINT('Ctrl Pts',(4.32347843899994,5.2,-1.93463205400001));
#351502=CARTESIAN_POINT('Ctrl Pts',(4.32347843899994,2.2,-1.93463205400001));
#351503=CARTESIAN_POINT('Ctrl Pts',(4.32609606399994,12.2,-1.93424329200001));
#351504=CARTESIAN_POINT('Ctrl Pts',(4.32609606399994,5.2,-1.93424329200001));
#351505=CARTESIAN_POINT('Ctrl Pts',(4.32609606399994,2.2,-1.93424329200001));
#351506=CARTESIAN_POINT('Ctrl Pts',(4.32871663299994,12.2,-1.93385130900001));
#351507=CARTESIAN_POINT('Ctrl Pts',(4.32871663299994,5.2,-1.93385130900001));
#351508=CARTESIAN_POINT('Ctrl Pts',(4.32871663299994,2.2,-1.93385130900001));
#351509=CARTESIAN_POINT('Ctrl Pts',(4.33134014299995,12.2,-1.93345610400002));
#351510=CARTESIAN_POINT('Ctrl Pts',(4.33134014299995,5.2,-1.93345610400002));
#351511=CARTESIAN_POINT('Ctrl Pts',(4.33134014299995,2.2,-1.93345610400002));
#351512=CARTESIAN_POINT('Ctrl Pts',(4.33396659199994,12.2,-1.93305767500001));
#351513=CARTESIAN_POINT('Ctrl Pts',(4.33396659199994,5.2,-1.93305767500001));
#351514=CARTESIAN_POINT('Ctrl Pts',(4.33396659199994,2.2,-1.93305767500001));
#351515=CARTESIAN_POINT('Ctrl Pts',(4.33607010199994,12.2,-1.93273635200002));
#351516=CARTESIAN_POINT('Ctrl Pts',(4.33607010199994,5.2,-1.93273635200002));
#351517=CARTESIAN_POINT('Ctrl Pts',(4.33607010199994,2.2,-1.93273635200002));
#351518=CARTESIAN_POINT('Ctrl Pts',(4.33764905499994,12.2,-1.93249390800001));
#351519=CARTESIAN_POINT('Ctrl Pts',(4.33764905499994,5.2,-1.93249390800001));
#351520=CARTESIAN_POINT('Ctrl Pts',(4.33764905499994,2.2,-1.93249390800001));
#351521=CARTESIAN_POINT('Ctrl Pts',(4.33870227899994,12.2,-1.93233163400001));
#351522=CARTESIAN_POINT('Ctrl Pts',(4.33870227899994,5.2,-1.93233163400001));
#351523=CARTESIAN_POINT('Ctrl Pts',(4.33870227899994,2.2,-1.93233163400001));
#351524=CARTESIAN_POINT('Ctrl Pts',(4.33922903699994,12.2,-1.93225033600001));
#351525=CARTESIAN_POINT('Ctrl Pts',(4.33922903699994,5.2,-1.93225033600001));
#351526=CARTESIAN_POINT('Ctrl Pts',(4.33922903699994,2.2,-1.93225033600001));
#351527=CARTESIAN_POINT('Origin',(-5.66300478732629E-14,15.2,-1.77635683940025E-14));
#351528=CARTESIAN_POINT('',(2.89509244999994,2.2,-2.18152806500001));
#351529=CARTESIAN_POINT('Origin',(3.18954822099994,15.2,-2.40340820900002));
#351530=CARTESIAN_POINT('',(3.18958920499994,12.2,-2.40343909200002));
#351531=CARTESIAN_POINT('Ctrl Pts',(3.57864508499994,12.2,-3.12342750100001));
#351532=CARTESIAN_POINT('Ctrl Pts',(3.57864508499994,5.2,-3.12342750100001));
#351533=CARTESIAN_POINT('Ctrl Pts',(3.57864508499994,2.2,-3.12342750100001));
#351534=CARTESIAN_POINT('Ctrl Pts',(3.57849719899995,12.2,-3.12291543200002));
#351535=CARTESIAN_POINT('Ctrl Pts',(3.57849719899995,5.2,-3.12291543200002));
#351536=CARTESIAN_POINT('Ctrl Pts',(3.57849719899995,2.2,-3.12291543200002));
#351537=CARTESIAN_POINT('Ctrl Pts',(3.57820125899994,12.2,-3.12189169800002));
#351538=CARTESIAN_POINT('Ctrl Pts',(3.57820125899994,5.2,-3.12189169800002));
#351539=CARTESIAN_POINT('Ctrl Pts',(3.57820125899994,2.2,-3.12189169800002));
#351540=CARTESIAN_POINT('Ctrl Pts',(3.57775684299994,12.2,-3.12035730300002));
#351541=CARTESIAN_POINT('Ctrl Pts',(3.57775684299994,5.2,-3.12035730300002));
#351542=CARTESIAN_POINT('Ctrl Pts',(3.57775684299994,2.2,-3.12035730300002));
#351543=CARTESIAN_POINT('Ctrl Pts',(3.57716327299994,12.2,-3.11831385700001));
#351544=CARTESIAN_POINT('Ctrl Pts',(3.57716327299994,5.2,-3.11831385700001));
#351545=CARTESIAN_POINT('Ctrl Pts',(3.57716327299994,2.2,-3.11831385700001));
#351546=CARTESIAN_POINT('Ctrl Pts',(3.57641962299994,12.2,-3.11576357000002));
#351547=CARTESIAN_POINT('Ctrl Pts',(3.57641962299994,5.2,-3.11576357000002));
#351548=CARTESIAN_POINT('Ctrl Pts',(3.57641962299994,2.2,-3.11576357000002));
#351549=CARTESIAN_POINT('Ctrl Pts',(3.57567428399994,12.2,-3.11321730600001));
#351550=CARTESIAN_POINT('Ctrl Pts',(3.57567428399994,5.2,-3.11321730600001));
#351551=CARTESIAN_POINT('Ctrl Pts',(3.57567428399994,2.2,-3.11321730600001));
#351552=CARTESIAN_POINT('Ctrl Pts',(3.57492725899994,12.2,-3.11067506500001));
#351553=CARTESIAN_POINT('Ctrl Pts',(3.57492725899994,5.2,-3.11067506500001));
#351554=CARTESIAN_POINT('Ctrl Pts',(3.57492725899994,2.2,-3.11067506500001));
#351555=CARTESIAN_POINT('Ctrl Pts',(3.57417855099994,12.2,-3.10813685000001));
#351556=CARTESIAN_POINT('Ctrl Pts',(3.57417855099994,5.2,-3.10813685000001));
#351557=CARTESIAN_POINT('Ctrl Pts',(3.57417855099994,2.2,-3.10813685000001));
#351558=CARTESIAN_POINT('Ctrl Pts',(3.57342816699994,12.2,-3.10560266400001));
#351559=CARTESIAN_POINT('Ctrl Pts',(3.57342816699994,5.2,-3.10560266400001));
#351560=CARTESIAN_POINT('Ctrl Pts',(3.57342816699994,2.2,-3.10560266400001));
#351561=CARTESIAN_POINT('Ctrl Pts',(3.57267611199994,12.2,-3.10307251000001));
#351562=CARTESIAN_POINT('Ctrl Pts',(3.57267611199994,5.2,-3.10307251000001));
#351563=CARTESIAN_POINT('Ctrl Pts',(3.57267611199994,2.2,-3.10307251000001));
#351564=CARTESIAN_POINT('Ctrl Pts',(3.57192239599994,12.2,-3.10054639500001));
#351565=CARTESIAN_POINT('Ctrl Pts',(3.57192239599994,5.2,-3.10054639500001));
#351566=CARTESIAN_POINT('Ctrl Pts',(3.57192239599994,2.2,-3.10054639500001));
#351567=CARTESIAN_POINT('Ctrl Pts',(3.57116702699994,12.2,-3.09802432100001));
#351568=CARTESIAN_POINT('Ctrl Pts',(3.57116702699994,5.2,-3.09802432100001));
#351569=CARTESIAN_POINT('Ctrl Pts',(3.57116702699994,2.2,-3.09802432100001));
#351570=CARTESIAN_POINT('Ctrl Pts',(3.57041001599994,12.2,-3.09550629400002));
#351571=CARTESIAN_POINT('Ctrl Pts',(3.57041001599994,5.2,-3.09550629400002));
#351572=CARTESIAN_POINT('Ctrl Pts',(3.57041001599994,2.2,-3.09550629400002));
#351573=CARTESIAN_POINT('Ctrl Pts',(3.56965137099994,12.2,-3.09299232000001));
#351574=CARTESIAN_POINT('Ctrl Pts',(3.56965137099994,5.2,-3.09299232000001));
#351575=CARTESIAN_POINT('Ctrl Pts',(3.56965137099994,2.2,-3.09299232000001));
#351576=CARTESIAN_POINT('Ctrl Pts',(3.56889110299994,12.2,-3.09048240200001));
#351577=CARTESIAN_POINT('Ctrl Pts',(3.56889110299994,5.2,-3.09048240200001));
#351578=CARTESIAN_POINT('Ctrl Pts',(3.56889110299994,2.2,-3.09048240200001));
#351579=CARTESIAN_POINT('Ctrl Pts',(3.56812921699994,12.2,-3.08797654500002));
#351580=CARTESIAN_POINT('Ctrl Pts',(3.56812921699994,5.2,-3.08797654500002));
#351581=CARTESIAN_POINT('Ctrl Pts',(3.56812921699994,2.2,-3.08797654500002));
#351582=CARTESIAN_POINT('Ctrl Pts',(3.56736572099994,12.2,-3.08547475200001));
#351583=CARTESIAN_POINT('Ctrl Pts',(3.56736572099994,5.2,-3.08547475200001));
#351584=CARTESIAN_POINT('Ctrl Pts',(3.56736572099994,2.2,-3.08547475200001));
#351585=CARTESIAN_POINT('Ctrl Pts',(3.56660062199994,12.2,-3.08297702800001));
#351586=CARTESIAN_POINT('Ctrl Pts',(3.56660062199994,5.2,-3.08297702800001));
#351587=CARTESIAN_POINT('Ctrl Pts',(3.56660062199994,2.2,-3.08297702800001));
#351588=CARTESIAN_POINT('Ctrl Pts',(3.56583392699994,12.2,-3.08048337600002));
#351589=CARTESIAN_POINT('Ctrl Pts',(3.56583392699994,5.2,-3.08048337600002));
#351590=CARTESIAN_POINT('Ctrl Pts',(3.56583392699994,2.2,-3.08048337600002));
#351591=CARTESIAN_POINT('Ctrl Pts',(3.56506564299994,12.2,-3.07799380000001));
#351592=CARTESIAN_POINT('Ctrl Pts',(3.56506564299994,5.2,-3.07799380000001));
#351593=CARTESIAN_POINT('Ctrl Pts',(3.56506564299994,2.2,-3.07799380000001));
#351594=CARTESIAN_POINT('Ctrl Pts',(3.56429577799994,12.2,-3.07550830200002));
#351595=CARTESIAN_POINT('Ctrl Pts',(3.56429577799994,5.2,-3.07550830200002));
#351596=CARTESIAN_POINT('Ctrl Pts',(3.56429577799994,2.2,-3.07550830200002));
#351597=CARTESIAN_POINT('Ctrl Pts',(3.56352433899994,12.2,-3.07302688700001));
#351598=CARTESIAN_POINT('Ctrl Pts',(3.56352433899994,5.2,-3.07302688700001));
#351599=CARTESIAN_POINT('Ctrl Pts',(3.56352433899994,2.2,-3.07302688700001));
#351600=CARTESIAN_POINT('Ctrl Pts',(3.56275133299994,12.2,-3.07054956100002));
#351601=CARTESIAN_POINT('Ctrl Pts',(3.56275133299994,5.2,-3.07054956100002));
#351602=CARTESIAN_POINT('Ctrl Pts',(3.56275133299994,2.2,-3.07054956100002));
#351603=CARTESIAN_POINT('Ctrl Pts',(3.56197677199994,12.2,-3.06807632600002));
#351604=CARTESIAN_POINT('Ctrl Pts',(3.56197677199994,5.2,-3.06807632600002));
#351605=CARTESIAN_POINT('Ctrl Pts',(3.56197677199994,2.2,-3.06807632600002));
#351606=CARTESIAN_POINT('Ctrl Pts',(3.56120065999994,12.2,-3.06560718700001));
#351607=CARTESIAN_POINT('Ctrl Pts',(3.56120065999994,5.2,-3.06560718700001));
#351608=CARTESIAN_POINT('Ctrl Pts',(3.56120065999994,2.2,-3.06560718700001));
#351609=CARTESIAN_POINT('Ctrl Pts',(3.56042300699994,12.2,-3.06314214800001));
#351610=CARTESIAN_POINT('Ctrl Pts',(3.56042300699994,5.2,-3.06314214800001));
#351611=CARTESIAN_POINT('Ctrl Pts',(3.56042300699994,2.2,-3.06314214800001));
#351612=CARTESIAN_POINT('Ctrl Pts',(3.55964381999994,12.2,-3.06068121400001));
#351613=CARTESIAN_POINT('Ctrl Pts',(3.55964381999994,5.2,-3.06068121400001));
#351614=CARTESIAN_POINT('Ctrl Pts',(3.55964381999994,2.2,-3.06068121400001));
#351615=CARTESIAN_POINT('Ctrl Pts',(3.55886310799994,12.2,-3.05822438600002));
#351616=CARTESIAN_POINT('Ctrl Pts',(3.55886310799994,5.2,-3.05822438600002));
#351617=CARTESIAN_POINT('Ctrl Pts',(3.55886310799994,2.2,-3.05822438600002));
#351618=CARTESIAN_POINT('Ctrl Pts',(3.55808087699994,12.2,-3.05577167100001));
#351619=CARTESIAN_POINT('Ctrl Pts',(3.55808087699994,5.2,-3.05577167100001));
#351620=CARTESIAN_POINT('Ctrl Pts',(3.55808087699994,2.2,-3.05577167100001));
#351621=CARTESIAN_POINT('Ctrl Pts',(3.55729713599994,12.2,-3.05332307200001));
#351622=CARTESIAN_POINT('Ctrl Pts',(3.55729713599994,5.2,-3.05332307200001));
#351623=CARTESIAN_POINT('Ctrl Pts',(3.55729713599994,2.2,-3.05332307200001));
#351624=CARTESIAN_POINT('Ctrl Pts',(3.55651189199994,12.2,-3.05087859200002));
#351625=CARTESIAN_POINT('Ctrl Pts',(3.55651189199994,5.2,-3.05087859200002));
#351626=CARTESIAN_POINT('Ctrl Pts',(3.55651189199994,2.2,-3.05087859200002));
#351627=CARTESIAN_POINT('Ctrl Pts',(3.55572515299994,12.2,-3.04843823600002));
#351628=CARTESIAN_POINT('Ctrl Pts',(3.55572515299994,5.2,-3.04843823600002));
#351629=CARTESIAN_POINT('Ctrl Pts',(3.55572515299994,2.2,-3.04843823600002));
#351630=CARTESIAN_POINT('Ctrl Pts',(3.55493692799994,12.2,-3.04600200600001));
#351631=CARTESIAN_POINT('Ctrl Pts',(3.55493692799994,5.2,-3.04600200600001));
#351632=CARTESIAN_POINT('Ctrl Pts',(3.55493692799994,2.2,-3.04600200600001));
#351633=CARTESIAN_POINT('Ctrl Pts',(3.55414722399995,12.2,-3.04356990900001));
#351634=CARTESIAN_POINT('Ctrl Pts',(3.55414722399995,5.2,-3.04356990900001));
#351635=CARTESIAN_POINT('Ctrl Pts',(3.55414722399995,2.2,-3.04356990900001));
#351636=CARTESIAN_POINT('Ctrl Pts',(3.55335604899994,12.2,-3.04114194700002));
#351637=CARTESIAN_POINT('Ctrl Pts',(3.55335604899994,5.2,-3.04114194700002));
#351638=CARTESIAN_POINT('Ctrl Pts',(3.55335604899994,2.2,-3.04114194700002));
#351639=CARTESIAN_POINT('Ctrl Pts',(3.55256340999994,12.2,-3.03871812400001));
#351640=CARTESIAN_POINT('Ctrl Pts',(3.55256340999994,5.2,-3.03871812400001));
#351641=CARTESIAN_POINT('Ctrl Pts',(3.55256340999994,2.2,-3.03871812400001));
#351642=CARTESIAN_POINT('Ctrl Pts',(3.55176931699994,12.2,-3.03629844500001));
#351643=CARTESIAN_POINT('Ctrl Pts',(3.55176931699994,5.2,-3.03629844500001));
#351644=CARTESIAN_POINT('Ctrl Pts',(3.55176931699994,2.2,-3.03629844500001));
#351645=CARTESIAN_POINT('Ctrl Pts',(3.55097377799994,12.2,-3.03388291200001));
#351646=CARTESIAN_POINT('Ctrl Pts',(3.55097377799994,5.2,-3.03388291200001));
#351647=CARTESIAN_POINT('Ctrl Pts',(3.55097377799994,2.2,-3.03388291200001));
#351648=CARTESIAN_POINT('Ctrl Pts',(3.55017679899994,12.2,-3.03147153100001));
#351649=CARTESIAN_POINT('Ctrl Pts',(3.55017679899994,5.2,-3.03147153100001));
#351650=CARTESIAN_POINT('Ctrl Pts',(3.55017679899994,2.2,-3.03147153100001));
#351651=CARTESIAN_POINT('Ctrl Pts',(3.54937838799994,12.2,-3.02906430500002));
#351652=CARTESIAN_POINT('Ctrl Pts',(3.54937838799994,5.2,-3.02906430500002));
#351653=CARTESIAN_POINT('Ctrl Pts',(3.54937838799994,2.2,-3.02906430500002));
#351654=CARTESIAN_POINT('Ctrl Pts',(3.54857855599994,12.2,-3.02666123800002));
#351655=CARTESIAN_POINT('Ctrl Pts',(3.54857855599994,5.2,-3.02666123800002));
#351656=CARTESIAN_POINT('Ctrl Pts',(3.54857855599994,2.2,-3.02666123800002));
#351657=CARTESIAN_POINT('Ctrl Pts',(3.54777730799994,12.2,-3.02426233300002));
#351658=CARTESIAN_POINT('Ctrl Pts',(3.54777730799994,5.2,-3.02426233300002));
#351659=CARTESIAN_POINT('Ctrl Pts',(3.54777730799994,2.2,-3.02426233300002));
#351660=CARTESIAN_POINT('Ctrl Pts',(3.54697465399994,12.2,-3.02186759600001));
#351661=CARTESIAN_POINT('Ctrl Pts',(3.54697465399994,5.2,-3.02186759600001));
#351662=CARTESIAN_POINT('Ctrl Pts',(3.54697465399994,2.2,-3.02186759600001));
#351663=CARTESIAN_POINT('Ctrl Pts',(3.54617059999994,12.2,-3.01947702900002));
#351664=CARTESIAN_POINT('Ctrl Pts',(3.54617059999994,5.2,-3.01947702900002));
#351665=CARTESIAN_POINT('Ctrl Pts',(3.54617059999994,2.2,-3.01947702900002));
#351666=CARTESIAN_POINT('Ctrl Pts',(3.54536515599994,12.2,-3.01709063600001));
#351667=CARTESIAN_POINT('Ctrl Pts',(3.54536515599994,5.2,-3.01709063600001));
#351668=CARTESIAN_POINT('Ctrl Pts',(3.54536515599994,2.2,-3.01709063600001));
#351669=CARTESIAN_POINT('Ctrl Pts',(3.54455832799994,12.2,-3.01470842100001));
#351670=CARTESIAN_POINT('Ctrl Pts',(3.54455832799994,5.2,-3.01470842100001));
#351671=CARTESIAN_POINT('Ctrl Pts',(3.54455832799994,2.2,-3.01470842100001));
#351672=CARTESIAN_POINT('Ctrl Pts',(3.54375012699994,12.2,-3.01233038900001));
#351673=CARTESIAN_POINT('Ctrl Pts',(3.54375012699994,5.2,-3.01233038900001));
#351674=CARTESIAN_POINT('Ctrl Pts',(3.54375012699994,2.2,-3.01233038900001));
#351675=CARTESIAN_POINT('Ctrl Pts',(3.54294055999994,12.2,-3.00995654200001));
#351676=CARTESIAN_POINT('Ctrl Pts',(3.54294055999994,5.2,-3.00995654200001));
#351677=CARTESIAN_POINT('Ctrl Pts',(3.54294055999994,2.2,-3.00995654200001));
#351678=CARTESIAN_POINT('Ctrl Pts',(3.54212963399994,12.2,-3.00758688500002));
#351679=CARTESIAN_POINT('Ctrl Pts',(3.54212963399994,5.2,-3.00758688500002));
#351680=CARTESIAN_POINT('Ctrl Pts',(3.54212963399994,2.2,-3.00758688500002));
#351681=CARTESIAN_POINT('Ctrl Pts',(3.54131735699994,12.2,-3.00522142200002));
#351682=CARTESIAN_POINT('Ctrl Pts',(3.54131735699994,5.2,-3.00522142200002));
#351683=CARTESIAN_POINT('Ctrl Pts',(3.54131735699994,2.2,-3.00522142200002));
#351684=CARTESIAN_POINT('Ctrl Pts',(3.54050373999994,12.2,-3.00286015700001));
#351685=CARTESIAN_POINT('Ctrl Pts',(3.54050373999994,5.2,-3.00286015700001));
#351686=CARTESIAN_POINT('Ctrl Pts',(3.54050373999994,2.2,-3.00286015700001));
#351687=CARTESIAN_POINT('Ctrl Pts',(3.53968878799995,12.2,-3.00050309300001));
#351688=CARTESIAN_POINT('Ctrl Pts',(3.53968878799995,5.2,-3.00050309300001));
#351689=CARTESIAN_POINT('Ctrl Pts',(3.53968878799995,2.2,-3.00050309300001));
#351690=CARTESIAN_POINT('Ctrl Pts',(3.53887251099994,12.2,-2.99815023300001));
#351691=CARTESIAN_POINT('Ctrl Pts',(3.53887251099994,5.2,-2.99815023300001));
#351692=CARTESIAN_POINT('Ctrl Pts',(3.53887251099994,2.2,-2.99815023300001));
#351693=CARTESIAN_POINT('Ctrl Pts',(3.53805491599994,12.2,-2.99580158300001));
#351694=CARTESIAN_POINT('Ctrl Pts',(3.53805491599994,5.2,-2.99580158300001));
#351695=CARTESIAN_POINT('Ctrl Pts',(3.53805491599994,2.2,-2.99580158300001));
#351696=CARTESIAN_POINT('Ctrl Pts',(3.53723601399994,12.2,-2.99345714500001));
#351697=CARTESIAN_POINT('Ctrl Pts',(3.53723601399994,5.2,-2.99345714500001));
#351698=CARTESIAN_POINT('Ctrl Pts',(3.53723601399994,2.2,-2.99345714500001));
#351699=CARTESIAN_POINT('Ctrl Pts',(3.53641580999994,12.2,-2.99111692500002));
#351700=CARTESIAN_POINT('Ctrl Pts',(3.53641580999994,5.2,-2.99111692500002));
#351701=CARTESIAN_POINT('Ctrl Pts',(3.53641580999994,2.2,-2.99111692500002));
#351702=CARTESIAN_POINT('Ctrl Pts',(3.53559431299994,12.2,-2.98878092400002));
#351703=CARTESIAN_POINT('Ctrl Pts',(3.53559431299994,5.2,-2.98878092400002));
#351704=CARTESIAN_POINT('Ctrl Pts',(3.53559431299994,2.2,-2.98878092400002));
#351705=CARTESIAN_POINT('Ctrl Pts',(3.53477153199994,12.2,-2.98644914800001));
#351706=CARTESIAN_POINT('Ctrl Pts',(3.53477153199994,5.2,-2.98644914800001));
#351707=CARTESIAN_POINT('Ctrl Pts',(3.53477153199994,2.2,-2.98644914800001));
#351708=CARTESIAN_POINT('Ctrl Pts',(3.53394747499994,12.2,-2.98412160000002));
#351709=CARTESIAN_POINT('Ctrl Pts',(3.53394747499994,5.2,-2.98412160000002));
#351710=CARTESIAN_POINT('Ctrl Pts',(3.53394747499994,2.2,-2.98412160000002));
#351711=CARTESIAN_POINT('Ctrl Pts',(3.53312214999994,12.2,-2.98179828200002));
#351712=CARTESIAN_POINT('Ctrl Pts',(3.53312214999994,5.2,-2.98179828200002));
#351713=CARTESIAN_POINT('Ctrl Pts',(3.53312214999994,2.2,-2.98179828200002));
#351714=CARTESIAN_POINT('Ctrl Pts',(3.53229556699994,12.2,-2.97947920200002));
#351715=CARTESIAN_POINT('Ctrl Pts',(3.53229556699994,5.2,-2.97947920200002));
#351716=CARTESIAN_POINT('Ctrl Pts',(3.53229556699994,2.2,-2.97947920200002));
#351717=CARTESIAN_POINT('Ctrl Pts',(3.53146773199994,12.2,-2.97716435900002));
#351718=CARTESIAN_POINT('Ctrl Pts',(3.53146773199994,5.2,-2.97716435900002));
#351719=CARTESIAN_POINT('Ctrl Pts',(3.53146773199994,2.2,-2.97716435900002));
#351720=CARTESIAN_POINT('Ctrl Pts',(3.53063865499994,12.2,-2.97485375900001));
#351721=CARTESIAN_POINT('Ctrl Pts',(3.53063865499994,5.2,-2.97485375900001));
#351722=CARTESIAN_POINT('Ctrl Pts',(3.53063865499994,2.2,-2.97485375900001));
#351723=CARTESIAN_POINT('Ctrl Pts',(3.52980834499994,12.2,-2.97254740700001));
#351724=CARTESIAN_POINT('Ctrl Pts',(3.52980834499994,5.2,-2.97254740700001));
#351725=CARTESIAN_POINT('Ctrl Pts',(3.52980834499994,2.2,-2.97254740700001));
#351726=CARTESIAN_POINT('Ctrl Pts',(3.52897680699995,12.2,-2.97024530500002));
#351727=CARTESIAN_POINT('Ctrl Pts',(3.52897680699995,5.2,-2.97024530500002));
#351728=CARTESIAN_POINT('Ctrl Pts',(3.52897680699995,2.2,-2.97024530500002));
#351729=CARTESIAN_POINT('Ctrl Pts',(3.52814405299994,12.2,-2.96794745700002));
#351730=CARTESIAN_POINT('Ctrl Pts',(3.52814405299994,5.2,-2.96794745700002));
#351731=CARTESIAN_POINT('Ctrl Pts',(3.52814405299994,2.2,-2.96794745700002));
#351732=CARTESIAN_POINT('Ctrl Pts',(3.52731008999994,12.2,-2.96565386600002));
#351733=CARTESIAN_POINT('Ctrl Pts',(3.52731008999994,5.2,-2.96565386600002));
#351734=CARTESIAN_POINT('Ctrl Pts',(3.52731008999994,2.2,-2.96565386600002));
#351735=CARTESIAN_POINT('Ctrl Pts',(3.52647492599994,12.2,-2.96336453900001));
#351736=CARTESIAN_POINT('Ctrl Pts',(3.52647492599994,5.2,-2.96336453900001));
#351737=CARTESIAN_POINT('Ctrl Pts',(3.52647492599994,2.2,-2.96336453900001));
#351738=CARTESIAN_POINT('Ctrl Pts',(3.52563856999994,12.2,-2.96107947500001));
#351739=CARTESIAN_POINT('Ctrl Pts',(3.52563856999994,5.2,-2.96107947500001));
#351740=CARTESIAN_POINT('Ctrl Pts',(3.52563856999994,2.2,-2.96107947500001));
#351741=CARTESIAN_POINT('Ctrl Pts',(3.52480103099994,12.2,-2.95879868200001));
#351742=CARTESIAN_POINT('Ctrl Pts',(3.52480103099994,5.2,-2.95879868200001));
#351743=CARTESIAN_POINT('Ctrl Pts',(3.52480103099994,2.2,-2.95879868200001));
#351744=CARTESIAN_POINT('Ctrl Pts',(3.52396231599994,12.2,-2.95652216000001));
#351745=CARTESIAN_POINT('Ctrl Pts',(3.52396231599994,5.2,-2.95652216000001));
#351746=CARTESIAN_POINT('Ctrl Pts',(3.52396231599994,2.2,-2.95652216000001));
#351747=CARTESIAN_POINT('Ctrl Pts',(3.52312243499994,12.2,-2.95424991500001));
#351748=CARTESIAN_POINT('Ctrl Pts',(3.52312243499994,5.2,-2.95424991500001));
#351749=CARTESIAN_POINT('Ctrl Pts',(3.52312243499994,2.2,-2.95424991500001));
#351750=CARTESIAN_POINT('Ctrl Pts',(3.52228139599994,12.2,-2.95198195100001));
#351751=CARTESIAN_POINT('Ctrl Pts',(3.52228139599994,5.2,-2.95198195100001));
#351752=CARTESIAN_POINT('Ctrl Pts',(3.52228139599994,2.2,-2.95198195100001));
#351753=CARTESIAN_POINT('Ctrl Pts',(3.52143920699994,12.2,-2.94971827000001));
#351754=CARTESIAN_POINT('Ctrl Pts',(3.52143920699994,5.2,-2.94971827000001));
#351755=CARTESIAN_POINT('Ctrl Pts',(3.52143920699994,2.2,-2.94971827000001));
#351756=CARTESIAN_POINT('Ctrl Pts',(3.52059587799994,12.2,-2.94745887700001));
#351757=CARTESIAN_POINT('Ctrl Pts',(3.52059587799994,5.2,-2.94745887700001));
#351758=CARTESIAN_POINT('Ctrl Pts',(3.52059587799994,2.2,-2.94745887700001));
#351759=CARTESIAN_POINT('Ctrl Pts',(3.51975141499994,12.2,-2.94520377500001));
#351760=CARTESIAN_POINT('Ctrl Pts',(3.51975141499994,5.2,-2.94520377500001));
#351761=CARTESIAN_POINT('Ctrl Pts',(3.51975141499994,2.2,-2.94520377500001));
#351762=CARTESIAN_POINT('Ctrl Pts',(3.51890582999994,12.2,-2.94295296700001));
#351763=CARTESIAN_POINT('Ctrl Pts',(3.51890582999994,5.2,-2.94295296700001));
#351764=CARTESIAN_POINT('Ctrl Pts',(3.51890582999994,2.2,-2.94295296700001));
#351765=CARTESIAN_POINT('Ctrl Pts',(3.51805912899994,12.2,-2.94070645800002));
#351766=CARTESIAN_POINT('Ctrl Pts',(3.51805912899994,5.2,-2.94070645800002));
#351767=CARTESIAN_POINT('Ctrl Pts',(3.51805912899994,2.2,-2.94070645800002));
#351768=CARTESIAN_POINT('Ctrl Pts',(3.51721132199994,12.2,-2.93846425100002));
#351769=CARTESIAN_POINT('Ctrl Pts',(3.51721132199994,5.2,-2.93846425100002));
#351770=CARTESIAN_POINT('Ctrl Pts',(3.51721132199994,2.2,-2.93846425100002));
#351771=CARTESIAN_POINT('Ctrl Pts',(3.51636241699994,12.2,-2.93622635000002));
#351772=CARTESIAN_POINT('Ctrl Pts',(3.51636241699994,5.2,-2.93622635000002));
#351773=CARTESIAN_POINT('Ctrl Pts',(3.51636241699994,2.2,-2.93622635000002));
#351774=CARTESIAN_POINT('Ctrl Pts',(3.51551242199994,12.2,-2.93399275800001));
#351775=CARTESIAN_POINT('Ctrl Pts',(3.51551242199994,5.2,-2.93399275800001));
#351776=CARTESIAN_POINT('Ctrl Pts',(3.51551242199994,2.2,-2.93399275800001));
#351777=CARTESIAN_POINT('Ctrl Pts',(3.51466134699994,12.2,-2.93176347900001));
#351778=CARTESIAN_POINT('Ctrl Pts',(3.51466134699994,5.2,-2.93176347900001));
#351779=CARTESIAN_POINT('Ctrl Pts',(3.51466134699994,2.2,-2.93176347900001));
#351780=CARTESIAN_POINT('Ctrl Pts',(3.51380919999994,12.2,-2.92953851700001));
#351781=CARTESIAN_POINT('Ctrl Pts',(3.51380919999994,5.2,-2.92953851700001));
#351782=CARTESIAN_POINT('Ctrl Pts',(3.51380919999994,2.2,-2.92953851700001));
#351783=CARTESIAN_POINT('Ctrl Pts',(3.51295598899994,12.2,-2.92731787500002));
#351784=CARTESIAN_POINT('Ctrl Pts',(3.51295598899994,5.2,-2.92731787500002));
#351785=CARTESIAN_POINT('Ctrl Pts',(3.51295598899994,2.2,-2.92731787500002));
#351786=CARTESIAN_POINT('Ctrl Pts',(3.51210172499994,12.2,-2.92510155600001));
#351787=CARTESIAN_POINT('Ctrl Pts',(3.51210172499994,5.2,-2.92510155600001));
#351788=CARTESIAN_POINT('Ctrl Pts',(3.51210172499994,2.2,-2.92510155600001));
#351789=CARTESIAN_POINT('Ctrl Pts',(3.51124641399994,12.2,-2.92288956500002));
#351790=CARTESIAN_POINT('Ctrl Pts',(3.51124641399994,5.2,-2.92288956500002));
#351791=CARTESIAN_POINT('Ctrl Pts',(3.51124641399994,2.2,-2.92288956500002));
#351792=CARTESIAN_POINT('Ctrl Pts',(3.51039006699994,12.2,-2.92068190600002));
#351793=CARTESIAN_POINT('Ctrl Pts',(3.51039006699994,5.2,-2.92068190600002));
#351794=CARTESIAN_POINT('Ctrl Pts',(3.51039006699994,2.2,-2.92068190600002));
#351795=CARTESIAN_POINT('Ctrl Pts',(3.50953269099994,12.2,-2.91847858000001));
#351796=CARTESIAN_POINT('Ctrl Pts',(3.50953269099994,5.2,-2.91847858000001));
#351797=CARTESIAN_POINT('Ctrl Pts',(3.50953269099994,2.2,-2.91847858000001));
#351798=CARTESIAN_POINT('Ctrl Pts',(3.50867429599994,12.2,-2.91627959300001));
#351799=CARTESIAN_POINT('Ctrl Pts',(3.50867429599994,5.2,-2.91627959300001));
#351800=CARTESIAN_POINT('Ctrl Pts',(3.50867429599994,2.2,-2.91627959300001));
#351801=CARTESIAN_POINT('Ctrl Pts',(3.50781488999994,12.2,-2.91408494800002));
#351802=CARTESIAN_POINT('Ctrl Pts',(3.50781488999994,5.2,-2.91408494800002));
#351803=CARTESIAN_POINT('Ctrl Pts',(3.50781488999994,2.2,-2.91408494800002));
#351804=CARTESIAN_POINT('Ctrl Pts',(3.50695448299994,12.2,-2.91189464800001));
#351805=CARTESIAN_POINT('Ctrl Pts',(3.50695448299994,5.2,-2.91189464800001));
#351806=CARTESIAN_POINT('Ctrl Pts',(3.50695448299994,2.2,-2.91189464800001));
#351807=CARTESIAN_POINT('Ctrl Pts',(3.50609308099994,12.2,-2.90970869600002));
#351808=CARTESIAN_POINT('Ctrl Pts',(3.50609308099994,5.2,-2.90970869600002));
#351809=CARTESIAN_POINT('Ctrl Pts',(3.50609308099994,2.2,-2.90970869600002));
#351810=CARTESIAN_POINT('Ctrl Pts',(3.50523069599994,12.2,-2.90752709800001));
#351811=CARTESIAN_POINT('Ctrl Pts',(3.50523069599994,5.2,-2.90752709800001));
#351812=CARTESIAN_POINT('Ctrl Pts',(3.50523069599994,2.2,-2.90752709800001));
#351813=CARTESIAN_POINT('Ctrl Pts',(3.50436733599994,12.2,-2.90534985400001));
#351814=CARTESIAN_POINT('Ctrl Pts',(3.50436733599994,5.2,-2.90534985400001));
#351815=CARTESIAN_POINT('Ctrl Pts',(3.50436733599994,2.2,-2.90534985400001));
#351816=CARTESIAN_POINT('Ctrl Pts',(3.50350300999994,12.2,-2.90317697000001));
#351817=CARTESIAN_POINT('Ctrl Pts',(3.50350300999994,5.2,-2.90317697000001));
#351818=CARTESIAN_POINT('Ctrl Pts',(3.50350300999994,2.2,-2.90317697000001));
#351819=CARTESIAN_POINT('Ctrl Pts',(3.50263772599994,12.2,-2.90100844900001));
#351820=CARTESIAN_POINT('Ctrl Pts',(3.50263772599994,5.2,-2.90100844900001));
#351821=CARTESIAN_POINT('Ctrl Pts',(3.50263772599994,2.2,-2.90100844900001));
#351822=CARTESIAN_POINT('Ctrl Pts',(3.50177149399994,12.2,-2.89884429600002));
#351823=CARTESIAN_POINT('Ctrl Pts',(3.50177149399994,5.2,-2.89884429600002));
#351824=CARTESIAN_POINT('Ctrl Pts',(3.50177149399994,2.2,-2.89884429600002));
#351825=CARTESIAN_POINT('Ctrl Pts',(3.50090432099994,12.2,-2.89668451100002));
#351826=CARTESIAN_POINT('Ctrl Pts',(3.50090432099994,5.2,-2.89668451100002));
#351827=CARTESIAN_POINT('Ctrl Pts',(3.50090432099994,2.2,-2.89668451100002));
#351828=CARTESIAN_POINT('Ctrl Pts',(3.50003621799994,12.2,-2.89452910100001));
#351829=CARTESIAN_POINT('Ctrl Pts',(3.50003621799994,5.2,-2.89452910100001));
#351830=CARTESIAN_POINT('Ctrl Pts',(3.50003621799994,2.2,-2.89452910100001));
#351831=CARTESIAN_POINT('Ctrl Pts',(3.49916719399994,12.2,-2.89237806600001));
#351832=CARTESIAN_POINT('Ctrl Pts',(3.49916719399994,5.2,-2.89237806600001));
#351833=CARTESIAN_POINT('Ctrl Pts',(3.49916719399994,2.2,-2.89237806600001));
#351834=CARTESIAN_POINT('Ctrl Pts',(3.49829725599994,12.2,-2.89023141200001));
#351835=CARTESIAN_POINT('Ctrl Pts',(3.49829725599994,5.2,-2.89023141200001));
#351836=CARTESIAN_POINT('Ctrl Pts',(3.49829725599994,2.2,-2.89023141200001));
#351837=CARTESIAN_POINT('Ctrl Pts',(3.49742641599994,12.2,-2.88808914300001));
#351838=CARTESIAN_POINT('Ctrl Pts',(3.49742641599994,5.2,-2.88808914300001));
#351839=CARTESIAN_POINT('Ctrl Pts',(3.49742641599994,2.2,-2.88808914300001));
#351840=CARTESIAN_POINT('Ctrl Pts',(3.49655467999994,12.2,-2.88595126100001));
#351841=CARTESIAN_POINT('Ctrl Pts',(3.49655467999994,5.2,-2.88595126100001));
#351842=CARTESIAN_POINT('Ctrl Pts',(3.49655467999994,2.2,-2.88595126100001));
#351843=CARTESIAN_POINT('Ctrl Pts',(3.49568205799994,12.2,-2.88381777000001));
#351844=CARTESIAN_POINT('Ctrl Pts',(3.49568205799994,5.2,-2.88381777000001));
#351845=CARTESIAN_POINT('Ctrl Pts',(3.49568205799994,2.2,-2.88381777000001));
#351846=CARTESIAN_POINT('Ctrl Pts',(3.49480855999994,12.2,-2.88168867300001));
#351847=CARTESIAN_POINT('Ctrl Pts',(3.49480855999994,5.2,-2.88168867300001));
#351848=CARTESIAN_POINT('Ctrl Pts',(3.49480855999994,2.2,-2.88168867300001));
#351849=CARTESIAN_POINT('Ctrl Pts',(3.49393419499994,12.2,-2.87956397300002));
#351850=CARTESIAN_POINT('Ctrl Pts',(3.49393419499994,5.2,-2.87956397300002));
#351851=CARTESIAN_POINT('Ctrl Pts',(3.49393419499994,2.2,-2.87956397300002));
#351852=CARTESIAN_POINT('Ctrl Pts',(3.49305897099994,12.2,-2.87744367500002));
#351853=CARTESIAN_POINT('Ctrl Pts',(3.49305897099994,5.2,-2.87744367500002));
#351854=CARTESIAN_POINT('Ctrl Pts',(3.49305897099994,2.2,-2.87744367500002));
#351855=CARTESIAN_POINT('Ctrl Pts',(3.49218289699994,12.2,-2.87532778100001));
#351856=CARTESIAN_POINT('Ctrl Pts',(3.49218289699994,5.2,-2.87532778100001));
#351857=CARTESIAN_POINT('Ctrl Pts',(3.49218289699994,2.2,-2.87532778100001));
#351858=CARTESIAN_POINT('Ctrl Pts',(3.49130598399995,12.2,-2.87321629600001));
#351859=CARTESIAN_POINT('Ctrl Pts',(3.49130598399995,5.2,-2.87321629600001));
#351860=CARTESIAN_POINT('Ctrl Pts',(3.49130598399995,2.2,-2.87321629600001));
#351861=CARTESIAN_POINT('Ctrl Pts',(3.49042823899994,12.2,-2.87110922200001));
#351862=CARTESIAN_POINT('Ctrl Pts',(3.49042823899994,5.2,-2.87110922200001));
#351863=CARTESIAN_POINT('Ctrl Pts',(3.49042823899994,2.2,-2.87110922200001));
#351864=CARTESIAN_POINT('Ctrl Pts',(3.48954967299994,12.2,-2.86900656300002));
#351865=CARTESIAN_POINT('Ctrl Pts',(3.48954967299994,5.2,-2.86900656300002));
#351866=CARTESIAN_POINT('Ctrl Pts',(3.48954967299994,2.2,-2.86900656300002));
#351867=CARTESIAN_POINT('Ctrl Pts',(3.48867029399994,12.2,-2.86690832200001));
#351868=CARTESIAN_POINT('Ctrl Pts',(3.48867029399994,5.2,-2.86690832200001));
#351869=CARTESIAN_POINT('Ctrl Pts',(3.48867029399994,2.2,-2.86690832200001));
#351870=CARTESIAN_POINT('Ctrl Pts',(3.48779011099994,12.2,-2.86481450300001));
#351871=CARTESIAN_POINT('Ctrl Pts',(3.48779011099994,5.2,-2.86481450300001));
#351872=CARTESIAN_POINT('Ctrl Pts',(3.48779011099994,2.2,-2.86481450300001));
#351873=CARTESIAN_POINT('Ctrl Pts',(3.48690913399994,12.2,-2.86272510700002));
#351874=CARTESIAN_POINT('Ctrl Pts',(3.48690913399994,5.2,-2.86272510700002));
#351875=CARTESIAN_POINT('Ctrl Pts',(3.48690913399994,2.2,-2.86272510700002));
#351876=CARTESIAN_POINT('Ctrl Pts',(3.48602737199994,12.2,-2.86064014200001));
#351877=CARTESIAN_POINT('Ctrl Pts',(3.48602737199994,5.2,-2.86064014200001));
#351878=CARTESIAN_POINT('Ctrl Pts',(3.48602737199994,2.2,-2.86064014200001));
#351879=CARTESIAN_POINT('Ctrl Pts',(3.48514483399994,12.2,-2.85855960700002));
#351880=CARTESIAN_POINT('Ctrl Pts',(3.48514483399994,5.2,-2.85855960700002));
#351881=CARTESIAN_POINT('Ctrl Pts',(3.48514483399994,2.2,-2.85855960700002));
#351882=CARTESIAN_POINT('Ctrl Pts',(3.48426152799994,12.2,-2.85648350800002));
#351883=CARTESIAN_POINT('Ctrl Pts',(3.48426152799994,5.2,-2.85648350800002));
#351884=CARTESIAN_POINT('Ctrl Pts',(3.48426152799994,2.2,-2.85648350800002));
#351885=CARTESIAN_POINT('Ctrl Pts',(3.48337746699994,12.2,-2.85441184800002));
#351886=CARTESIAN_POINT('Ctrl Pts',(3.48337746699994,5.2,-2.85441184800002));
#351887=CARTESIAN_POINT('Ctrl Pts',(3.48337746699994,2.2,-2.85441184800002));
#351888=CARTESIAN_POINT('Ctrl Pts',(3.48249265699994,12.2,-2.85234462900001));
#351889=CARTESIAN_POINT('Ctrl Pts',(3.48249265699994,5.2,-2.85234462900001));
#351890=CARTESIAN_POINT('Ctrl Pts',(3.48249265699994,2.2,-2.85234462900001));
#351891=CARTESIAN_POINT('Ctrl Pts',(3.48160710799994,12.2,-2.85028185600002));
#351892=CARTESIAN_POINT('Ctrl Pts',(3.48160710799994,5.2,-2.85028185600002));
#351893=CARTESIAN_POINT('Ctrl Pts',(3.48160710799994,2.2,-2.85028185600002));
#351894=CARTESIAN_POINT('Ctrl Pts',(3.48072082999995,12.2,-2.84822353100001));
#351895=CARTESIAN_POINT('Ctrl Pts',(3.48072082999995,5.2,-2.84822353100001));
#351896=CARTESIAN_POINT('Ctrl Pts',(3.48072082999995,2.2,-2.84822353100001));
#351897=CARTESIAN_POINT('Ctrl Pts',(3.47983383199994,12.2,-2.84616965800002));
#351898=CARTESIAN_POINT('Ctrl Pts',(3.47983383199994,5.2,-2.84616965800002));
#351899=CARTESIAN_POINT('Ctrl Pts',(3.47983383199994,2.2,-2.84616965800002));
#351900=CARTESIAN_POINT('Ctrl Pts',(3.47894612299994,12.2,-2.84412023900002));
#351901=CARTESIAN_POINT('Ctrl Pts',(3.47894612299994,5.2,-2.84412023900002));
#351902=CARTESIAN_POINT('Ctrl Pts',(3.47894612299994,2.2,-2.84412023900002));
#351903=CARTESIAN_POINT('Ctrl Pts',(3.47805771399994,12.2,-2.84207527900001));
#351904=CARTESIAN_POINT('Ctrl Pts',(3.47805771399994,5.2,-2.84207527900001));
#351905=CARTESIAN_POINT('Ctrl Pts',(3.47805771399994,2.2,-2.84207527900001));
#351906=CARTESIAN_POINT('Ctrl Pts',(3.47716861199994,12.2,-2.84003478100002));
#351907=CARTESIAN_POINT('Ctrl Pts',(3.47716861199994,5.2,-2.84003478100002));
#351908=CARTESIAN_POINT('Ctrl Pts',(3.47716861199994,2.2,-2.84003478100002));
#351909=CARTESIAN_POINT('Ctrl Pts',(3.47627882699994,12.2,-2.83799874900001));
#351910=CARTESIAN_POINT('Ctrl Pts',(3.47627882699994,5.2,-2.83799874900001));
#351911=CARTESIAN_POINT('Ctrl Pts',(3.47627882699994,2.2,-2.83799874900001));
#351912=CARTESIAN_POINT('Ctrl Pts',(3.47538836999994,12.2,-2.83596718400001));
#351913=CARTESIAN_POINT('Ctrl Pts',(3.47538836999994,5.2,-2.83596718400001));
#351914=CARTESIAN_POINT('Ctrl Pts',(3.47538836999994,2.2,-2.83596718400001));
#351915=CARTESIAN_POINT('Ctrl Pts',(3.47449724999994,12.2,-2.83394009000002));
#351916=CARTESIAN_POINT('Ctrl Pts',(3.47449724999994,5.2,-2.83394009000002));
#351917=CARTESIAN_POINT('Ctrl Pts',(3.47449724999994,2.2,-2.83394009000002));
#351918=CARTESIAN_POINT('Ctrl Pts',(3.47360547499994,12.2,-2.83191747100001));
#351919=CARTESIAN_POINT('Ctrl Pts',(3.47360547499994,5.2,-2.83191747100001));
#351920=CARTESIAN_POINT('Ctrl Pts',(3.47360547499994,2.2,-2.83191747100001));
#351921=CARTESIAN_POINT('Ctrl Pts',(3.47271305499994,12.2,-2.82989933100001));
#351922=CARTESIAN_POINT('Ctrl Pts',(3.47271305499994,5.2,-2.82989933100001));
#351923=CARTESIAN_POINT('Ctrl Pts',(3.47271305499994,2.2,-2.82989933100001));
#351924=CARTESIAN_POINT('Ctrl Pts',(3.47182000099994,12.2,-2.82788567200001));
#351925=CARTESIAN_POINT('Ctrl Pts',(3.47182000099994,5.2,-2.82788567200001));
#351926=CARTESIAN_POINT('Ctrl Pts',(3.47182000099994,2.2,-2.82788567200001));
#351927=CARTESIAN_POINT('Ctrl Pts',(3.47092632099995,12.2,-2.82587649700002));
#351928=CARTESIAN_POINT('Ctrl Pts',(3.47092632099995,5.2,-2.82587649700002));
#351929=CARTESIAN_POINT('Ctrl Pts',(3.47092632099995,2.2,-2.82587649700002));
#351930=CARTESIAN_POINT('Ctrl Pts',(3.47003202499995,12.2,-2.82387181000002));
#351931=CARTESIAN_POINT('Ctrl Pts',(3.47003202499995,5.2,-2.82387181000002));
#351932=CARTESIAN_POINT('Ctrl Pts',(3.47003202499995,2.2,-2.82387181000002));
#351933=CARTESIAN_POINT('Ctrl Pts',(3.46913712299994,12.2,-2.82187161500001));
#351934=CARTESIAN_POINT('Ctrl Pts',(3.46913712299994,5.2,-2.82187161500001));
#351935=CARTESIAN_POINT('Ctrl Pts',(3.46913712299994,2.2,-2.82187161500001));
#351936=CARTESIAN_POINT('Ctrl Pts',(3.46824162499995,12.2,-2.81987591300001));
#351937=CARTESIAN_POINT('Ctrl Pts',(3.46824162499995,5.2,-2.81987591300001));
#351938=CARTESIAN_POINT('Ctrl Pts',(3.46824162499995,2.2,-2.81987591300001));
#351939=CARTESIAN_POINT('Ctrl Pts',(3.46734553799994,12.2,-2.81788470800001));
#351940=CARTESIAN_POINT('Ctrl Pts',(3.46734553799994,5.2,-2.81788470800001));
#351941=CARTESIAN_POINT('Ctrl Pts',(3.46734553799994,2.2,-2.81788470800001));
#351942=CARTESIAN_POINT('Ctrl Pts',(3.46644887499994,12.2,-2.81589800400001));
#351943=CARTESIAN_POINT('Ctrl Pts',(3.46644887499994,5.2,-2.81589800400001));
#351944=CARTESIAN_POINT('Ctrl Pts',(3.46644887499994,2.2,-2.81589800400001));
#351945=CARTESIAN_POINT('Ctrl Pts',(3.46555164299994,12.2,-2.81391580500001));
#351946=CARTESIAN_POINT('Ctrl Pts',(3.46555164299994,5.2,-2.81391580500001));
#351947=CARTESIAN_POINT('Ctrl Pts',(3.46555164299994,2.2,-2.81391580500001));
#351948=CARTESIAN_POINT('Ctrl Pts',(3.46465385299994,12.2,-2.81193811200001));
#351949=CARTESIAN_POINT('Ctrl Pts',(3.46465385299994,5.2,-2.81193811200001));
#351950=CARTESIAN_POINT('Ctrl Pts',(3.46465385299994,2.2,-2.81193811200001));
#351951=CARTESIAN_POINT('Ctrl Pts',(3.46375551499994,12.2,-2.80996492900002));
#351952=CARTESIAN_POINT('Ctrl Pts',(3.46375551499994,5.2,-2.80996492900002));
#351953=CARTESIAN_POINT('Ctrl Pts',(3.46375551499994,2.2,-2.80996492900002));
#351954=CARTESIAN_POINT('Ctrl Pts',(3.46285663699994,12.2,-2.80799625900002));
#351955=CARTESIAN_POINT('Ctrl Pts',(3.46285663699994,5.2,-2.80799625900002));
#351956=CARTESIAN_POINT('Ctrl Pts',(3.46285663699994,2.2,-2.80799625900002));
#351957=CARTESIAN_POINT('Ctrl Pts',(3.46195723099994,12.2,-2.80603210700002));
#351958=CARTESIAN_POINT('Ctrl Pts',(3.46195723099994,5.2,-2.80603210700002));
#351959=CARTESIAN_POINT('Ctrl Pts',(3.46195723099994,2.2,-2.80603210700002));
#351960=CARTESIAN_POINT('Ctrl Pts',(3.46105730499994,12.2,-2.80407247300001));
#351961=CARTESIAN_POINT('Ctrl Pts',(3.46105730499994,5.2,-2.80407247300001));
#351962=CARTESIAN_POINT('Ctrl Pts',(3.46105730499994,2.2,-2.80407247300001));
#351963=CARTESIAN_POINT('Ctrl Pts',(3.46015686899994,12.2,-2.80211736300001));
#351964=CARTESIAN_POINT('Ctrl Pts',(3.46015686899994,5.2,-2.80211736300001));
#351965=CARTESIAN_POINT('Ctrl Pts',(3.46015686899994,2.2,-2.80211736300001));
#351966=CARTESIAN_POINT('Ctrl Pts',(3.45925593399994,12.2,-2.80016677700001));
#351967=CARTESIAN_POINT('Ctrl Pts',(3.45925593399994,5.2,-2.80016677700001));
#351968=CARTESIAN_POINT('Ctrl Pts',(3.45925593399994,2.2,-2.80016677700001));
#351969=CARTESIAN_POINT('Ctrl Pts',(3.45835450899994,12.2,-2.79822072100002));
#351970=CARTESIAN_POINT('Ctrl Pts',(3.45835450899994,5.2,-2.79822072100002));
#351971=CARTESIAN_POINT('Ctrl Pts',(3.45835450899994,2.2,-2.79822072100002));
#351972=CARTESIAN_POINT('Ctrl Pts',(3.45745260299994,12.2,-2.79627919700001));
#351973=CARTESIAN_POINT('Ctrl Pts',(3.45745260299994,5.2,-2.79627919700001));
#351974=CARTESIAN_POINT('Ctrl Pts',(3.45745260299994,2.2,-2.79627919700001));
#351975=CARTESIAN_POINT('Ctrl Pts',(3.45655022599994,12.2,-2.79434220800002));
#351976=CARTESIAN_POINT('Ctrl Pts',(3.45655022599994,5.2,-2.79434220800002));
#351977=CARTESIAN_POINT('Ctrl Pts',(3.45655022599994,2.2,-2.79434220800002));
#351978=CARTESIAN_POINT('Ctrl Pts',(3.45564738899995,12.2,-2.79240975700001));
#351979=CARTESIAN_POINT('Ctrl Pts',(3.45564738899995,5.2,-2.79240975700001));
#351980=CARTESIAN_POINT('Ctrl Pts',(3.45564738899995,2.2,-2.79240975700001));
#351981=CARTESIAN_POINT('Ctrl Pts',(3.45474410099994,12.2,-2.79048184900001));
#351982=CARTESIAN_POINT('Ctrl Pts',(3.45474410099994,5.2,-2.79048184900001));
#351983=CARTESIAN_POINT('Ctrl Pts',(3.45474410099994,2.2,-2.79048184900001));
#351984=CARTESIAN_POINT('Ctrl Pts',(3.45384037299994,12.2,-2.78855848300001));
#351985=CARTESIAN_POINT('Ctrl Pts',(3.45384037299994,5.2,-2.78855848300001));
#351986=CARTESIAN_POINT('Ctrl Pts',(3.45384037299994,2.2,-2.78855848300001));
#351987=CARTESIAN_POINT('Ctrl Pts',(3.45293621399994,12.2,-2.78663966600002));
#351988=CARTESIAN_POINT('Ctrl Pts',(3.45293621399994,5.2,-2.78663966600002));
#351989=CARTESIAN_POINT('Ctrl Pts',(3.45293621399994,2.2,-2.78663966600002));
#351990=CARTESIAN_POINT('Ctrl Pts',(3.45203163299994,12.2,-2.78472539900001));
#351991=CARTESIAN_POINT('Ctrl Pts',(3.45203163299994,5.2,-2.78472539900001));
#351992=CARTESIAN_POINT('Ctrl Pts',(3.45203163299994,2.2,-2.78472539900001));
#351993=CARTESIAN_POINT('Ctrl Pts',(3.45112664199994,12.2,-2.78281568600002));
#351994=CARTESIAN_POINT('Ctrl Pts',(3.45112664199994,5.2,-2.78281568600002));
#351995=CARTESIAN_POINT('Ctrl Pts',(3.45112664199994,2.2,-2.78281568600002));
#351996=CARTESIAN_POINT('Ctrl Pts',(3.45022124899995,12.2,-2.78091052900002));
#351997=CARTESIAN_POINT('Ctrl Pts',(3.45022124899995,5.2,-2.78091052900002));
#351998=CARTESIAN_POINT('Ctrl Pts',(3.45022124899995,2.2,-2.78091052900002));
#351999=CARTESIAN_POINT('Ctrl Pts',(3.44931546499994,12.2,-2.77900993200001));
#352000=CARTESIAN_POINT('Ctrl Pts',(3.44931546499994,5.2,-2.77900993200001));
#352001=CARTESIAN_POINT('Ctrl Pts',(3.44931546499994,2.2,-2.77900993200001));
#352002=CARTESIAN_POINT('Ctrl Pts',(3.44840929999994,12.2,-2.77711389800002));
#352003=CARTESIAN_POINT('Ctrl Pts',(3.44840929999994,5.2,-2.77711389800002));
#352004=CARTESIAN_POINT('Ctrl Pts',(3.44840929999994,2.2,-2.77711389800002));
#352005=CARTESIAN_POINT('Ctrl Pts',(3.44750276299994,12.2,-2.77522242900002));
#352006=CARTESIAN_POINT('Ctrl Pts',(3.44750276299994,5.2,-2.77522242900002));
#352007=CARTESIAN_POINT('Ctrl Pts',(3.44750276299994,2.2,-2.77522242900002));
#352008=CARTESIAN_POINT('Ctrl Pts',(3.44659586599994,12.2,-2.77333552900001));
#352009=CARTESIAN_POINT('Ctrl Pts',(3.44659586599994,5.2,-2.77333552900001));
#352010=CARTESIAN_POINT('Ctrl Pts',(3.44659586599994,2.2,-2.77333552900001));
#352011=CARTESIAN_POINT('Ctrl Pts',(3.44568861799994,12.2,-2.77145320000002));
#352012=CARTESIAN_POINT('Ctrl Pts',(3.44568861799994,5.2,-2.77145320000002));
#352013=CARTESIAN_POINT('Ctrl Pts',(3.44568861799994,2.2,-2.77145320000002));
#352014=CARTESIAN_POINT('Ctrl Pts',(3.44478102899994,12.2,-2.76957544600001));
#352015=CARTESIAN_POINT('Ctrl Pts',(3.44478102899994,5.2,-2.76957544600001));
#352016=CARTESIAN_POINT('Ctrl Pts',(3.44478102899994,2.2,-2.76957544600001));
#352017=CARTESIAN_POINT('Ctrl Pts',(3.44387310799994,12.2,-2.76770227000001));
#352018=CARTESIAN_POINT('Ctrl Pts',(3.44387310799994,5.2,-2.76770227000001));
#352019=CARTESIAN_POINT('Ctrl Pts',(3.44387310799994,2.2,-2.76770227000001));
#352020=CARTESIAN_POINT('Ctrl Pts',(3.44296486699994,12.2,-2.76583367300002));
#352021=CARTESIAN_POINT('Ctrl Pts',(3.44296486699994,5.2,-2.76583367300002));
#352022=CARTESIAN_POINT('Ctrl Pts',(3.44296486699994,2.2,-2.76583367300002));
#352023=CARTESIAN_POINT('Ctrl Pts',(3.44205631599994,12.2,-2.76396966100001));
#352024=CARTESIAN_POINT('Ctrl Pts',(3.44205631599994,5.2,-2.76396966100001));
#352025=CARTESIAN_POINT('Ctrl Pts',(3.44205631599994,2.2,-2.76396966100001));
#352026=CARTESIAN_POINT('Ctrl Pts',(3.44114746399995,12.2,-2.76211023600001));
#352027=CARTESIAN_POINT('Ctrl Pts',(3.44114746399995,5.2,-2.76211023600001));
#352028=CARTESIAN_POINT('Ctrl Pts',(3.44114746399995,2.2,-2.76211023600001));
#352029=CARTESIAN_POINT('Ctrl Pts',(3.44023832099994,12.2,-2.76025539900001));
#352030=CARTESIAN_POINT('Ctrl Pts',(3.44023832099994,5.2,-2.76025539900001));
#352031=CARTESIAN_POINT('Ctrl Pts',(3.44023832099994,2.2,-2.76025539900001));
#352032=CARTESIAN_POINT('Ctrl Pts',(3.43932889999994,12.2,-2.75840515500001));
#352033=CARTESIAN_POINT('Ctrl Pts',(3.43932889999994,5.2,-2.75840515500001));
#352034=CARTESIAN_POINT('Ctrl Pts',(3.43932889999994,2.2,-2.75840515500001));
#352035=CARTESIAN_POINT('Ctrl Pts',(3.43841920699994,12.2,-2.75655950600001));
#352036=CARTESIAN_POINT('Ctrl Pts',(3.43841920699994,5.2,-2.75655950600001));
#352037=CARTESIAN_POINT('Ctrl Pts',(3.43841920699994,2.2,-2.75655950600001));
#352038=CARTESIAN_POINT('Ctrl Pts',(3.43750925599994,12.2,-2.75471845600002));
#352039=CARTESIAN_POINT('Ctrl Pts',(3.43750925599994,5.2,-2.75471845600002));
#352040=CARTESIAN_POINT('Ctrl Pts',(3.43750925599994,2.2,-2.75471845600002));
#352041=CARTESIAN_POINT('Ctrl Pts',(3.43659905399994,12.2,-2.75288200500002));
#352042=CARTESIAN_POINT('Ctrl Pts',(3.43659905399994,5.2,-2.75288200500002));
#352043=CARTESIAN_POINT('Ctrl Pts',(3.43659905399994,2.2,-2.75288200500002));
#352044=CARTESIAN_POINT('Ctrl Pts',(3.43568861399994,12.2,-2.75105016000001));
#352045=CARTESIAN_POINT('Ctrl Pts',(3.43568861399994,5.2,-2.75105016000001));
#352046=CARTESIAN_POINT('Ctrl Pts',(3.43568861399994,2.2,-2.75105016000001));
#352047=CARTESIAN_POINT('Ctrl Pts',(3.43477794499994,12.2,-2.74922292100001));
#352048=CARTESIAN_POINT('Ctrl Pts',(3.43477794499994,5.2,-2.74922292100001));
#352049=CARTESIAN_POINT('Ctrl Pts',(3.43477794499994,2.2,-2.74922292100001));
#352050=CARTESIAN_POINT('Ctrl Pts',(3.43386705799994,12.2,-2.74740029100002));
#352051=CARTESIAN_POINT('Ctrl Pts',(3.43386705799994,5.2,-2.74740029100002));
#352052=CARTESIAN_POINT('Ctrl Pts',(3.43386705799994,2.2,-2.74740029100002));
#352053=CARTESIAN_POINT('Ctrl Pts',(3.43295596299994,12.2,-2.74558227400002));
#352054=CARTESIAN_POINT('Ctrl Pts',(3.43295596299994,5.2,-2.74558227400002));
#352055=CARTESIAN_POINT('Ctrl Pts',(3.43295596299994,2.2,-2.74558227400002));
#352056=CARTESIAN_POINT('Ctrl Pts',(3.43204466899994,12.2,-2.74376887300001));
#352057=CARTESIAN_POINT('Ctrl Pts',(3.43204466899994,5.2,-2.74376887300001));
#352058=CARTESIAN_POINT('Ctrl Pts',(3.43204466899994,2.2,-2.74376887300001));
#352059=CARTESIAN_POINT('Ctrl Pts',(3.43113318899994,12.2,-2.74196008900002));
#352060=CARTESIAN_POINT('Ctrl Pts',(3.43113318899994,5.2,-2.74196008900002));
#352061=CARTESIAN_POINT('Ctrl Pts',(3.43113318899994,2.2,-2.74196008900002));
#352062=CARTESIAN_POINT('Ctrl Pts',(3.43022152999994,12.2,-2.74015592700001));
#352063=CARTESIAN_POINT('Ctrl Pts',(3.43022152999994,5.2,-2.74015592700001));
#352064=CARTESIAN_POINT('Ctrl Pts',(3.43022152999994,2.2,-2.74015592700001));
#352065=CARTESIAN_POINT('Ctrl Pts',(3.42930970599994,12.2,-2.73835638800001));
#352066=CARTESIAN_POINT('Ctrl Pts',(3.42930970599994,5.2,-2.73835638800001));
#352067=CARTESIAN_POINT('Ctrl Pts',(3.42930970599994,2.2,-2.73835638800001));
#352068=CARTESIAN_POINT('Ctrl Pts',(3.42839772599994,12.2,-2.73656147700001));
#352069=CARTESIAN_POINT('Ctrl Pts',(3.42839772599994,5.2,-2.73656147700001));
#352070=CARTESIAN_POINT('Ctrl Pts',(3.42839772599994,2.2,-2.73656147700001));
#352071=CARTESIAN_POINT('Ctrl Pts',(3.42748559899994,12.2,-2.73477119400001));
#352072=CARTESIAN_POINT('Ctrl Pts',(3.42748559899994,5.2,-2.73477119400001));
#352073=CARTESIAN_POINT('Ctrl Pts',(3.42748559899994,2.2,-2.73477119400001));
#352074=CARTESIAN_POINT('Ctrl Pts',(3.42657333799994,12.2,-2.73298554400002));
#352075=CARTESIAN_POINT('Ctrl Pts',(3.42657333799994,5.2,-2.73298554400002));
#352076=CARTESIAN_POINT('Ctrl Pts',(3.42657333799994,2.2,-2.73298554400002));
#352077=CARTESIAN_POINT('Ctrl Pts',(3.42566095199994,12.2,-2.73120452900002));
#352078=CARTESIAN_POINT('Ctrl Pts',(3.42566095199994,5.2,-2.73120452900002));
#352079=CARTESIAN_POINT('Ctrl Pts',(3.42566095199994,2.2,-2.73120452900002));
#352080=CARTESIAN_POINT('Ctrl Pts',(3.42474845199995,12.2,-2.72942815200001));
#352081=CARTESIAN_POINT('Ctrl Pts',(3.42474845199995,5.2,-2.72942815200001));
#352082=CARTESIAN_POINT('Ctrl Pts',(3.42474845199995,2.2,-2.72942815200001));
#352083=CARTESIAN_POINT('Ctrl Pts',(3.42383584799994,12.2,-2.72765641500001));
#352084=CARTESIAN_POINT('Ctrl Pts',(3.42383584799994,5.2,-2.72765641500001));
#352085=CARTESIAN_POINT('Ctrl Pts',(3.42383584799994,2.2,-2.72765641500001));
#352086=CARTESIAN_POINT('Ctrl Pts',(3.42292315099994,12.2,-2.72588932200001));
#352087=CARTESIAN_POINT('Ctrl Pts',(3.42292315099994,5.2,-2.72588932200001));
#352088=CARTESIAN_POINT('Ctrl Pts',(3.42292315099994,2.2,-2.72588932200001));
#352089=CARTESIAN_POINT('Ctrl Pts',(3.42201037099994,12.2,-2.72412687400001));
#352090=CARTESIAN_POINT('Ctrl Pts',(3.42201037099994,5.2,-2.72412687400001));
#352091=CARTESIAN_POINT('Ctrl Pts',(3.42201037099994,2.2,-2.72412687400001));
#352092=CARTESIAN_POINT('Ctrl Pts',(3.42109751999994,12.2,-2.72236907600002));
#352093=CARTESIAN_POINT('Ctrl Pts',(3.42109751999994,5.2,-2.72236907600002));
#352094=CARTESIAN_POINT('Ctrl Pts',(3.42109751999994,2.2,-2.72236907600002));
#352095=CARTESIAN_POINT('Ctrl Pts',(3.42018460699994,12.2,-2.72061592900001));
#352096=CARTESIAN_POINT('Ctrl Pts',(3.42018460699994,5.2,-2.72061592900001));
#352097=CARTESIAN_POINT('Ctrl Pts',(3.42018460699994,2.2,-2.72061592900001));
#352098=CARTESIAN_POINT('Ctrl Pts',(3.41927164399995,12.2,-2.71886743500001));
#352099=CARTESIAN_POINT('Ctrl Pts',(3.41927164399995,5.2,-2.71886743500001));
#352100=CARTESIAN_POINT('Ctrl Pts',(3.41927164399995,2.2,-2.71886743500001));
#352101=CARTESIAN_POINT('Ctrl Pts',(3.41835863999994,12.2,-2.71712360000001));
#352102=CARTESIAN_POINT('Ctrl Pts',(3.41835863999994,5.2,-2.71712360000001));
#352103=CARTESIAN_POINT('Ctrl Pts',(3.41835863999994,2.2,-2.71712360000001));
#352104=CARTESIAN_POINT('Ctrl Pts',(3.41744560799994,12.2,-2.71538442300002));
#352105=CARTESIAN_POINT('Ctrl Pts',(3.41744560799994,5.2,-2.71538442300002));
#352106=CARTESIAN_POINT('Ctrl Pts',(3.41744560799994,2.2,-2.71538442300002));
#352107=CARTESIAN_POINT('Ctrl Pts',(3.41653255599994,12.2,-2.71364990900001));
#352108=CARTESIAN_POINT('Ctrl Pts',(3.41653255599994,5.2,-2.71364990900001));
#352109=CARTESIAN_POINT('Ctrl Pts',(3.41653255599994,2.2,-2.71364990900001));
#352110=CARTESIAN_POINT('Ctrl Pts',(3.41561949699994,12.2,-2.71192005900001));
#352111=CARTESIAN_POINT('Ctrl Pts',(3.41561949699994,5.2,-2.71192005900001));
#352112=CARTESIAN_POINT('Ctrl Pts',(3.41561949699994,2.2,-2.71192005900001));
#352113=CARTESIAN_POINT('Ctrl Pts',(3.41470643999994,12.2,-2.71019487800002));
#352114=CARTESIAN_POINT('Ctrl Pts',(3.41470643999994,5.2,-2.71019487800002));
#352115=CARTESIAN_POINT('Ctrl Pts',(3.41470643999994,2.2,-2.71019487800002));
#352116=CARTESIAN_POINT('Ctrl Pts',(3.41379339799994,12.2,-2.70847436600001));
#352117=CARTESIAN_POINT('Ctrl Pts',(3.41379339799994,5.2,-2.70847436600001));
#352118=CARTESIAN_POINT('Ctrl Pts',(3.41379339799994,2.2,-2.70847436600001));
#352119=CARTESIAN_POINT('Ctrl Pts',(3.41288037899994,12.2,-2.70675852800002));
#352120=CARTESIAN_POINT('Ctrl Pts',(3.41288037899994,5.2,-2.70675852800002));
#352121=CARTESIAN_POINT('Ctrl Pts',(3.41288037899994,2.2,-2.70675852800002));
#352122=CARTESIAN_POINT('Ctrl Pts',(3.41196739599994,12.2,-2.70504736500001));
#352123=CARTESIAN_POINT('Ctrl Pts',(3.41196739599994,5.2,-2.70504736500001));
#352124=CARTESIAN_POINT('Ctrl Pts',(3.41196739599994,2.2,-2.70504736500001));
#352125=CARTESIAN_POINT('Ctrl Pts',(3.41105445899994,12.2,-2.70334088000002));
#352126=CARTESIAN_POINT('Ctrl Pts',(3.41105445899994,5.2,-2.70334088000002));
#352127=CARTESIAN_POINT('Ctrl Pts',(3.41105445899994,2.2,-2.70334088000002));
#352128=CARTESIAN_POINT('Ctrl Pts',(3.41014157899994,12.2,-2.70163907500002));
#352129=CARTESIAN_POINT('Ctrl Pts',(3.41014157899994,5.2,-2.70163907500002));
#352130=CARTESIAN_POINT('Ctrl Pts',(3.41014157899994,2.2,-2.70163907500002));
#352131=CARTESIAN_POINT('Ctrl Pts',(3.40922876599994,12.2,-2.69994195500002));
#352132=CARTESIAN_POINT('Ctrl Pts',(3.40922876599994,5.2,-2.69994195500002));
#352133=CARTESIAN_POINT('Ctrl Pts',(3.40922876599994,2.2,-2.69994195500002));
#352134=CARTESIAN_POINT('Ctrl Pts',(3.40831603299995,12.2,-2.69824951900001));
#352135=CARTESIAN_POINT('Ctrl Pts',(3.40831603299995,5.2,-2.69824951900001));
#352136=CARTESIAN_POINT('Ctrl Pts',(3.40831603299995,2.2,-2.69824951900001));
#352137=CARTESIAN_POINT('Ctrl Pts',(3.40740338899994,12.2,-2.69656177300002));
#352138=CARTESIAN_POINT('Ctrl Pts',(3.40740338899994,5.2,-2.69656177300002));
#352139=CARTESIAN_POINT('Ctrl Pts',(3.40740338899994,2.2,-2.69656177300002));
#352140=CARTESIAN_POINT('Ctrl Pts',(3.40649084599994,12.2,-2.69487871800001));
#352141=CARTESIAN_POINT('Ctrl Pts',(3.40649084599994,5.2,-2.69487871800001));
#352142=CARTESIAN_POINT('Ctrl Pts',(3.40649084599994,2.2,-2.69487871800001));
#352143=CARTESIAN_POINT('Ctrl Pts',(3.40557841399994,12.2,-2.69320035500002));
#352144=CARTESIAN_POINT('Ctrl Pts',(3.40557841399994,5.2,-2.69320035500002));
#352145=CARTESIAN_POINT('Ctrl Pts',(3.40557841399994,2.2,-2.69320035500002));
#352146=CARTESIAN_POINT('Ctrl Pts',(3.40466610499994,12.2,-2.69152669000002));
#352147=CARTESIAN_POINT('Ctrl Pts',(3.40466610499994,5.2,-2.69152669000002));
#352148=CARTESIAN_POINT('Ctrl Pts',(3.40466610499994,2.2,-2.69152669000002));
#352149=CARTESIAN_POINT('Ctrl Pts',(3.40375392899994,12.2,-2.68985772300002));
#352150=CARTESIAN_POINT('Ctrl Pts',(3.40375392899994,5.2,-2.68985772300002));
#352151=CARTESIAN_POINT('Ctrl Pts',(3.40375392899994,2.2,-2.68985772300002));
#352152=CARTESIAN_POINT('Ctrl Pts',(3.40284189799994,12.2,-2.68819345700001));
#352153=CARTESIAN_POINT('Ctrl Pts',(3.40284189799994,5.2,-2.68819345700001));
#352154=CARTESIAN_POINT('Ctrl Pts',(3.40284189799994,2.2,-2.68819345700001));
#352155=CARTESIAN_POINT('Ctrl Pts',(3.40193002199995,12.2,-2.68653389500002));
#352156=CARTESIAN_POINT('Ctrl Pts',(3.40193002199995,5.2,-2.68653389500002));
#352157=CARTESIAN_POINT('Ctrl Pts',(3.40193002199995,2.2,-2.68653389500002));
#352158=CARTESIAN_POINT('Ctrl Pts',(3.40101831299994,12.2,-2.68487903900001));
#352159=CARTESIAN_POINT('Ctrl Pts',(3.40101831299994,5.2,-2.68487903900001));
#352160=CARTESIAN_POINT('Ctrl Pts',(3.40101831299994,2.2,-2.68487903900001));
#352161=CARTESIAN_POINT('Ctrl Pts',(3.40010678199994,12.2,-2.68322889200002));
#352162=CARTESIAN_POINT('Ctrl Pts',(3.40010678199994,5.2,-2.68322889200002));
#352163=CARTESIAN_POINT('Ctrl Pts',(3.40010678199994,2.2,-2.68322889200002));
#352164=CARTESIAN_POINT('Ctrl Pts',(3.39919543899994,12.2,-2.68158345600002));
#352165=CARTESIAN_POINT('Ctrl Pts',(3.39919543899994,5.2,-2.68158345600002));
#352166=CARTESIAN_POINT('Ctrl Pts',(3.39919543899994,2.2,-2.68158345600002));
#352167=CARTESIAN_POINT('Ctrl Pts',(3.39828429699994,12.2,-2.67994273300001));
#352168=CARTESIAN_POINT('Ctrl Pts',(3.39828429699994,5.2,-2.67994273300001));
#352169=CARTESIAN_POINT('Ctrl Pts',(3.39828429699994,2.2,-2.67994273300001));
#352170=CARTESIAN_POINT('Ctrl Pts',(3.39737336599994,12.2,-2.67830672600001));
#352171=CARTESIAN_POINT('Ctrl Pts',(3.39737336599994,5.2,-2.67830672600001));
#352172=CARTESIAN_POINT('Ctrl Pts',(3.39737336599994,2.2,-2.67830672600001));
#352173=CARTESIAN_POINT('Ctrl Pts',(3.39646265699994,12.2,-2.67667543800002));
#352174=CARTESIAN_POINT('Ctrl Pts',(3.39646265699994,5.2,-2.67667543800002));
#352175=CARTESIAN_POINT('Ctrl Pts',(3.39646265699994,2.2,-2.67667543800002));
#352176=CARTESIAN_POINT('Ctrl Pts',(3.39555218099994,12.2,-2.67504887100001));
#352177=CARTESIAN_POINT('Ctrl Pts',(3.39555218099994,5.2,-2.67504887100001));
#352178=CARTESIAN_POINT('Ctrl Pts',(3.39555218099994,2.2,-2.67504887100001));
#352179=CARTESIAN_POINT('Ctrl Pts',(3.39464195099994,12.2,-2.67342702700001));
#352180=CARTESIAN_POINT('Ctrl Pts',(3.39464195099994,5.2,-2.67342702700001));
#352181=CARTESIAN_POINT('Ctrl Pts',(3.39464195099994,2.2,-2.67342702700001));
#352182=CARTESIAN_POINT('Ctrl Pts',(3.39373197699994,12.2,-2.67180991000001));
#352183=CARTESIAN_POINT('Ctrl Pts',(3.39373197699994,5.2,-2.67180991000001));
#352184=CARTESIAN_POINT('Ctrl Pts',(3.39373197699994,2.2,-2.67180991000001));
#352185=CARTESIAN_POINT('Ctrl Pts',(3.39282226999994,12.2,-2.67019752000001));
#352186=CARTESIAN_POINT('Ctrl Pts',(3.39282226999994,5.2,-2.67019752000001));
#352187=CARTESIAN_POINT('Ctrl Pts',(3.39282226999994,2.2,-2.67019752000001));
#352188=CARTESIAN_POINT('Ctrl Pts',(3.39191284199994,12.2,-2.66858986100001));
#352189=CARTESIAN_POINT('Ctrl Pts',(3.39191284199994,5.2,-2.66858986100001));
#352190=CARTESIAN_POINT('Ctrl Pts',(3.39191284199994,2.2,-2.66858986100001));
#352191=CARTESIAN_POINT('Ctrl Pts',(3.39100370299994,12.2,-2.66698693500001));
#352192=CARTESIAN_POINT('Ctrl Pts',(3.39100370299994,5.2,-2.66698693500001));
#352193=CARTESIAN_POINT('Ctrl Pts',(3.39100370299994,2.2,-2.66698693500001));
#352194=CARTESIAN_POINT('Ctrl Pts',(3.39009486499994,12.2,-2.66538874400001));
#352195=CARTESIAN_POINT('Ctrl Pts',(3.39009486499994,5.2,-2.66538874400001));
#352196=CARTESIAN_POINT('Ctrl Pts',(3.39009486499994,2.2,-2.66538874400001));
#352197=CARTESIAN_POINT('Ctrl Pts',(3.38918633999994,12.2,-2.66379529100002));
#352198=CARTESIAN_POINT('Ctrl Pts',(3.38918633999994,5.2,-2.66379529100002));
#352199=CARTESIAN_POINT('Ctrl Pts',(3.38918633999994,2.2,-2.66379529100002));
#352200=CARTESIAN_POINT('Ctrl Pts',(3.38827813999994,12.2,-2.66220657700002));
#352201=CARTESIAN_POINT('Ctrl Pts',(3.38827813999994,5.2,-2.66220657700002));
#352202=CARTESIAN_POINT('Ctrl Pts',(3.38827813999994,2.2,-2.66220657700002));
#352203=CARTESIAN_POINT('Ctrl Pts',(3.38737027399994,12.2,-2.66062260600001));
#352204=CARTESIAN_POINT('Ctrl Pts',(3.38737027399994,5.2,-2.66062260600001));
#352205=CARTESIAN_POINT('Ctrl Pts',(3.38737027399994,2.2,-2.66062260600001));
#352206=CARTESIAN_POINT('Ctrl Pts',(3.38646275499995,12.2,-2.65904338000002));
#352207=CARTESIAN_POINT('Ctrl Pts',(3.38646275499995,5.2,-2.65904338000002));
#352208=CARTESIAN_POINT('Ctrl Pts',(3.38646275499995,2.2,-2.65904338000002));
#352209=CARTESIAN_POINT('Ctrl Pts',(3.38555559599994,12.2,-2.65746890100001));
#352210=CARTESIAN_POINT('Ctrl Pts',(3.38555559599994,5.2,-2.65746890100001));
#352211=CARTESIAN_POINT('Ctrl Pts',(3.38555559599994,2.2,-2.65746890100001));
#352212=CARTESIAN_POINT('Ctrl Pts',(3.38464880499994,12.2,-2.65589917200002));
#352213=CARTESIAN_POINT('Ctrl Pts',(3.38464880499994,5.2,-2.65589917200002));
#352214=CARTESIAN_POINT('Ctrl Pts',(3.38464880499994,2.2,-2.65589917200002));
#352215=CARTESIAN_POINT('Ctrl Pts',(3.38374239599994,12.2,-2.65433419300001));
#352216=CARTESIAN_POINT('Ctrl Pts',(3.38374239599994,5.2,-2.65433419300001));
#352217=CARTESIAN_POINT('Ctrl Pts',(3.38374239599994,2.2,-2.65433419300001));
#352218=CARTESIAN_POINT('Ctrl Pts',(3.38283637899994,12.2,-2.65277396800002));
#352219=CARTESIAN_POINT('Ctrl Pts',(3.38283637899994,5.2,-2.65277396800002));
#352220=CARTESIAN_POINT('Ctrl Pts',(3.38283637899994,2.2,-2.65277396800002));
#352221=CARTESIAN_POINT('Ctrl Pts',(3.38193076699994,12.2,-2.65121849900002));
#352222=CARTESIAN_POINT('Ctrl Pts',(3.38193076699994,5.2,-2.65121849900002));
#352223=CARTESIAN_POINT('Ctrl Pts',(3.38193076699994,2.2,-2.65121849900002));
#352224=CARTESIAN_POINT('Ctrl Pts',(3.38102557099994,12.2,-2.64966778900002));
#352225=CARTESIAN_POINT('Ctrl Pts',(3.38102557099994,5.2,-2.64966778900002));
#352226=CARTESIAN_POINT('Ctrl Pts',(3.38102557099994,2.2,-2.64966778900002));
#352227=CARTESIAN_POINT('Ctrl Pts',(3.38012080199994,12.2,-2.64812183900001));
#352228=CARTESIAN_POINT('Ctrl Pts',(3.38012080199994,5.2,-2.64812183900001));
#352229=CARTESIAN_POINT('Ctrl Pts',(3.38012080199994,2.2,-2.64812183900001));
#352230=CARTESIAN_POINT('Ctrl Pts',(3.37921647399994,12.2,-2.64658065300001));
#352231=CARTESIAN_POINT('Ctrl Pts',(3.37921647399994,5.2,-2.64658065300001));
#352232=CARTESIAN_POINT('Ctrl Pts',(3.37921647399994,2.2,-2.64658065300001));
#352233=CARTESIAN_POINT('Ctrl Pts',(3.37831259399994,12.2,-2.64504423000002));
#352234=CARTESIAN_POINT('Ctrl Pts',(3.37831259399994,5.2,-2.64504423000002));
#352235=CARTESIAN_POINT('Ctrl Pts',(3.37831259399994,2.2,-2.64504423000002));
#352236=CARTESIAN_POINT('Ctrl Pts',(3.37740917799994,12.2,-2.64351257600001));
#352237=CARTESIAN_POINT('Ctrl Pts',(3.37740917799994,5.2,-2.64351257600001));
#352238=CARTESIAN_POINT('Ctrl Pts',(3.37740917799994,2.2,-2.64351257600001));
#352239=CARTESIAN_POINT('Ctrl Pts',(3.37650623599994,12.2,-2.64198569100001));
#352240=CARTESIAN_POINT('Ctrl Pts',(3.37650623599994,5.2,-2.64198569100001));
#352241=CARTESIAN_POINT('Ctrl Pts',(3.37650623599994,2.2,-2.64198569100001));
#352242=CARTESIAN_POINT('Ctrl Pts',(3.37560377899994,12.2,-2.64046357700002));
#352243=CARTESIAN_POINT('Ctrl Pts',(3.37560377899994,5.2,-2.64046357700002));
#352244=CARTESIAN_POINT('Ctrl Pts',(3.37560377899994,2.2,-2.64046357700002));
#352245=CARTESIAN_POINT('Ctrl Pts',(3.37470181999994,12.2,-2.63894623700001));
#352246=CARTESIAN_POINT('Ctrl Pts',(3.37470181999994,5.2,-2.63894623700001));
#352247=CARTESIAN_POINT('Ctrl Pts',(3.37470181999994,2.2,-2.63894623700001));
#352248=CARTESIAN_POINT('Ctrl Pts',(3.37380037099994,12.2,-2.63743367300001));
#352249=CARTESIAN_POINT('Ctrl Pts',(3.37380037099994,5.2,-2.63743367300001));
#352250=CARTESIAN_POINT('Ctrl Pts',(3.37380037099994,2.2,-2.63743367300001));
#352251=CARTESIAN_POINT('Ctrl Pts',(3.37289944199994,12.2,-2.63592588700002));
#352252=CARTESIAN_POINT('Ctrl Pts',(3.37289944199994,5.2,-2.63592588700002));
#352253=CARTESIAN_POINT('Ctrl Pts',(3.37289944199994,2.2,-2.63592588700002));
#352254=CARTESIAN_POINT('Ctrl Pts',(3.37199904699995,12.2,-2.63442288100002));
#352255=CARTESIAN_POINT('Ctrl Pts',(3.37199904699995,5.2,-2.63442288100002));
#352256=CARTESIAN_POINT('Ctrl Pts',(3.37199904699995,2.2,-2.63442288100002));
#352257=CARTESIAN_POINT('Ctrl Pts',(3.37109919599994,12.2,-2.63292465700002));
#352258=CARTESIAN_POINT('Ctrl Pts',(3.37109919599994,5.2,-2.63292465700002));
#352259=CARTESIAN_POINT('Ctrl Pts',(3.37109919599994,2.2,-2.63292465700002));
#352260=CARTESIAN_POINT('Ctrl Pts',(3.37019990199994,12.2,-2.63143121700002));
#352261=CARTESIAN_POINT('Ctrl Pts',(3.37019990199994,5.2,-2.63143121700002));
#352262=CARTESIAN_POINT('Ctrl Pts',(3.37019990199994,2.2,-2.63143121700002));
#352263=CARTESIAN_POINT('Ctrl Pts',(3.36930117599994,12.2,-2.62994256500001));
#352264=CARTESIAN_POINT('Ctrl Pts',(3.36930117599994,5.2,-2.62994256500001));
#352265=CARTESIAN_POINT('Ctrl Pts',(3.36930117599994,2.2,-2.62994256500001));
#352266=CARTESIAN_POINT('Ctrl Pts',(3.36840302999994,12.2,-2.62845870100001));
#352267=CARTESIAN_POINT('Ctrl Pts',(3.36840302999994,5.2,-2.62845870100001));
#352268=CARTESIAN_POINT('Ctrl Pts',(3.36840302999994,2.2,-2.62845870100001));
#352269=CARTESIAN_POINT('Ctrl Pts',(3.36750547699994,12.2,-2.62697962700001));
#352270=CARTESIAN_POINT('Ctrl Pts',(3.36750547699994,5.2,-2.62697962700001));
#352271=CARTESIAN_POINT('Ctrl Pts',(3.36750547699994,2.2,-2.62697962700001));
#352272=CARTESIAN_POINT('Ctrl Pts',(3.36660852899994,12.2,-2.62550534600001));
#352273=CARTESIAN_POINT('Ctrl Pts',(3.36660852899994,5.2,-2.62550534600001));
#352274=CARTESIAN_POINT('Ctrl Pts',(3.36660852899994,2.2,-2.62550534600001));
#352275=CARTESIAN_POINT('Ctrl Pts',(3.36571219499994,12.2,-2.62403586000001));
#352276=CARTESIAN_POINT('Ctrl Pts',(3.36571219499994,5.2,-2.62403586000001));
#352277=CARTESIAN_POINT('Ctrl Pts',(3.36571219499994,2.2,-2.62403586000001));
#352278=CARTESIAN_POINT('Ctrl Pts',(3.36481649099994,12.2,-2.62257117000001));
#352279=CARTESIAN_POINT('Ctrl Pts',(3.36481649099994,5.2,-2.62257117000001));
#352280=CARTESIAN_POINT('Ctrl Pts',(3.36481649099994,2.2,-2.62257117000001));
#352281=CARTESIAN_POINT('Ctrl Pts',(3.36392142799995,12.2,-2.62111128000001));
#352282=CARTESIAN_POINT('Ctrl Pts',(3.36392142799995,5.2,-2.62111128000001));
#352283=CARTESIAN_POINT('Ctrl Pts',(3.36392142799995,2.2,-2.62111128000001));
#352284=CARTESIAN_POINT('Ctrl Pts',(3.36302701599994,12.2,-2.61965619000001));
#352285=CARTESIAN_POINT('Ctrl Pts',(3.36302701599994,5.2,-2.61965619000001));
#352286=CARTESIAN_POINT('Ctrl Pts',(3.36302701599994,2.2,-2.61965619000001));
#352287=CARTESIAN_POINT('Ctrl Pts',(3.36213326799994,12.2,-2.61820590300001));
#352288=CARTESIAN_POINT('Ctrl Pts',(3.36213326799994,5.2,-2.61820590300001));
#352289=CARTESIAN_POINT('Ctrl Pts',(3.36213326799994,2.2,-2.61820590300001));
#352290=CARTESIAN_POINT('Ctrl Pts',(3.36124019699994,12.2,-2.61676042000001));
#352291=CARTESIAN_POINT('Ctrl Pts',(3.36124019699994,5.2,-2.61676042000001));
#352292=CARTESIAN_POINT('Ctrl Pts',(3.36124019699994,2.2,-2.61676042000001));
#352293=CARTESIAN_POINT('Ctrl Pts',(3.36034781499994,12.2,-2.61531974400001));
#352294=CARTESIAN_POINT('Ctrl Pts',(3.36034781499994,5.2,-2.61531974400001));
#352295=CARTESIAN_POINT('Ctrl Pts',(3.36034781499994,2.2,-2.61531974400001));
#352296=CARTESIAN_POINT('Ctrl Pts',(3.35945613299995,12.2,-2.61388387700002));
#352297=CARTESIAN_POINT('Ctrl Pts',(3.35945613299995,5.2,-2.61388387700002));
#352298=CARTESIAN_POINT('Ctrl Pts',(3.35945613299995,2.2,-2.61388387700002));
#352299=CARTESIAN_POINT('Ctrl Pts',(3.35856516399994,12.2,-2.61245282100001));
#352300=CARTESIAN_POINT('Ctrl Pts',(3.35856516399994,5.2,-2.61245282100001));
#352301=CARTESIAN_POINT('Ctrl Pts',(3.35856516399994,2.2,-2.61245282100001));
#352302=CARTESIAN_POINT('Ctrl Pts',(3.35767492099994,12.2,-2.61102657700001));
#352303=CARTESIAN_POINT('Ctrl Pts',(3.35767492099994,5.2,-2.61102657700001));
#352304=CARTESIAN_POINT('Ctrl Pts',(3.35767492099994,2.2,-2.61102657700001));
#352305=CARTESIAN_POINT('Ctrl Pts',(3.35678541399994,12.2,-2.60960514700002));
#352306=CARTESIAN_POINT('Ctrl Pts',(3.35678541399994,5.2,-2.60960514700002));
#352307=CARTESIAN_POINT('Ctrl Pts',(3.35678541399994,2.2,-2.60960514700002));
#352308=CARTESIAN_POINT('Ctrl Pts',(3.35589665799994,12.2,-2.60818853300002));
#352309=CARTESIAN_POINT('Ctrl Pts',(3.35589665799994,5.2,-2.60818853300002));
#352310=CARTESIAN_POINT('Ctrl Pts',(3.35589665799994,2.2,-2.60818853300002));
#352311=CARTESIAN_POINT('Ctrl Pts',(3.35500866399994,12.2,-2.60677673900001));
#352312=CARTESIAN_POINT('Ctrl Pts',(3.35500866399994,5.2,-2.60677673900001));
#352313=CARTESIAN_POINT('Ctrl Pts',(3.35500866399994,2.2,-2.60677673900001));
#352314=CARTESIAN_POINT('Ctrl Pts',(3.35412144299994,12.2,-2.60536976400001));
#352315=CARTESIAN_POINT('Ctrl Pts',(3.35412144299994,5.2,-2.60536976400001));
#352316=CARTESIAN_POINT('Ctrl Pts',(3.35412144299994,2.2,-2.60536976400001));
#352317=CARTESIAN_POINT('Ctrl Pts',(3.35323500899994,12.2,-2.60396761000001));
#352318=CARTESIAN_POINT('Ctrl Pts',(3.35323500899994,5.2,-2.60396761000001));
#352319=CARTESIAN_POINT('Ctrl Pts',(3.35323500899994,2.2,-2.60396761000001));
#352320=CARTESIAN_POINT('Ctrl Pts',(3.35234937399994,12.2,-2.60257028200002));
#352321=CARTESIAN_POINT('Ctrl Pts',(3.35234937399994,5.2,-2.60257028200002));
#352322=CARTESIAN_POINT('Ctrl Pts',(3.35234937399994,2.2,-2.60257028200002));
#352323=CARTESIAN_POINT('Ctrl Pts',(3.35146454899995,12.2,-2.60117777900001));
#352324=CARTESIAN_POINT('Ctrl Pts',(3.35146454899995,5.2,-2.60117777900001));
#352325=CARTESIAN_POINT('Ctrl Pts',(3.35146454899995,2.2,-2.60117777900001));
#352326=CARTESIAN_POINT('Ctrl Pts',(3.35058054899994,12.2,-2.59979010200002));
#352327=CARTESIAN_POINT('Ctrl Pts',(3.35058054899994,5.2,-2.59979010200002));
#352328=CARTESIAN_POINT('Ctrl Pts',(3.35058054899994,2.2,-2.59979010200002));
#352329=CARTESIAN_POINT('Ctrl Pts',(3.34969738399994,12.2,-2.59840725600001));
#352330=CARTESIAN_POINT('Ctrl Pts',(3.34969738399994,5.2,-2.59840725600001));
#352331=CARTESIAN_POINT('Ctrl Pts',(3.34969738399994,2.2,-2.59840725600001));
#352332=CARTESIAN_POINT('Ctrl Pts',(3.34881506899994,12.2,-2.59702924100001));
#352333=CARTESIAN_POINT('Ctrl Pts',(3.34881506899994,5.2,-2.59702924100001));
#352334=CARTESIAN_POINT('Ctrl Pts',(3.34881506899994,2.2,-2.59702924100001));
#352335=CARTESIAN_POINT('Ctrl Pts',(3.34793361399994,12.2,-2.59565605800002));
#352336=CARTESIAN_POINT('Ctrl Pts',(3.34793361399994,5.2,-2.59565605800002));
#352337=CARTESIAN_POINT('Ctrl Pts',(3.34793361399994,2.2,-2.59565605800002));
#352338=CARTESIAN_POINT('Ctrl Pts',(3.34705303299994,12.2,-2.59428771000001));
#352339=CARTESIAN_POINT('Ctrl Pts',(3.34705303299994,5.2,-2.59428771000001));
#352340=CARTESIAN_POINT('Ctrl Pts',(3.34705303299994,2.2,-2.59428771000001));
#352341=CARTESIAN_POINT('Ctrl Pts',(3.34617333799994,12.2,-2.59292419800001));
#352342=CARTESIAN_POINT('Ctrl Pts',(3.34617333799994,5.2,-2.59292419800001));
#352343=CARTESIAN_POINT('Ctrl Pts',(3.34617333799994,2.2,-2.59292419800001));
#352344=CARTESIAN_POINT('Ctrl Pts',(3.34529454199994,12.2,-2.59156552500002));
#352345=CARTESIAN_POINT('Ctrl Pts',(3.34529454199994,5.2,-2.59156552500002));
#352346=CARTESIAN_POINT('Ctrl Pts',(3.34529454199994,2.2,-2.59156552500002));
#352347=CARTESIAN_POINT('Ctrl Pts',(3.34441665599994,12.2,-2.59021169100001));
#352348=CARTESIAN_POINT('Ctrl Pts',(3.34441665599994,5.2,-2.59021169100001));
#352349=CARTESIAN_POINT('Ctrl Pts',(3.34441665599994,2.2,-2.59021169100001));
#352350=CARTESIAN_POINT('Ctrl Pts',(3.34353969499994,12.2,-2.58886269900001));
#352351=CARTESIAN_POINT('Ctrl Pts',(3.34353969499994,5.2,-2.58886269900001));
#352352=CARTESIAN_POINT('Ctrl Pts',(3.34353969499994,2.2,-2.58886269900001));
#352353=CARTESIAN_POINT('Ctrl Pts',(3.34266366899994,12.2,-2.58751855100002));
#352354=CARTESIAN_POINT('Ctrl Pts',(3.34266366899994,5.2,-2.58751855100002));
#352355=CARTESIAN_POINT('Ctrl Pts',(3.34266366899994,2.2,-2.58751855100002));
#352356=CARTESIAN_POINT('Ctrl Pts',(3.34178859299994,12.2,-2.58617924600001));
#352357=CARTESIAN_POINT('Ctrl Pts',(3.34178859299994,5.2,-2.58617924600001));
#352358=CARTESIAN_POINT('Ctrl Pts',(3.34178859299994,2.2,-2.58617924600001));
#352359=CARTESIAN_POINT('Ctrl Pts',(3.34091447899994,12.2,-2.58484479000002));
#352360=CARTESIAN_POINT('Ctrl Pts',(3.34091447899994,5.2,-2.58484479000002));
#352361=CARTESIAN_POINT('Ctrl Pts',(3.34091447899994,2.2,-2.58484479000002));
#352362=CARTESIAN_POINT('Ctrl Pts',(3.34004133899994,12.2,-2.58351518100001));
#352363=CARTESIAN_POINT('Ctrl Pts',(3.34004133899994,5.2,-2.58351518100001));
#352364=CARTESIAN_POINT('Ctrl Pts',(3.34004133899994,2.2,-2.58351518100001));
#352365=CARTESIAN_POINT('Ctrl Pts',(3.33916918599994,12.2,-2.58219042200002));
#352366=CARTESIAN_POINT('Ctrl Pts',(3.33916918599994,5.2,-2.58219042200002));
#352367=CARTESIAN_POINT('Ctrl Pts',(3.33916918599994,2.2,-2.58219042200002));
#352368=CARTESIAN_POINT('Ctrl Pts',(3.33829803499994,12.2,-2.58087051500001));
#352369=CARTESIAN_POINT('Ctrl Pts',(3.33829803499994,5.2,-2.58087051500001));
#352370=CARTESIAN_POINT('Ctrl Pts',(3.33829803499994,2.2,-2.58087051500001));
#352371=CARTESIAN_POINT('Ctrl Pts',(3.33742789499994,12.2,-2.57955546100002));
#352372=CARTESIAN_POINT('Ctrl Pts',(3.33742789499994,5.2,-2.57955546100002));
#352373=CARTESIAN_POINT('Ctrl Pts',(3.33742789499994,2.2,-2.57955546100002));
#352374=CARTESIAN_POINT('Ctrl Pts',(3.33655878199994,12.2,-2.57824526200002));
#352375=CARTESIAN_POINT('Ctrl Pts',(3.33655878199994,5.2,-2.57824526200002));
#352376=CARTESIAN_POINT('Ctrl Pts',(3.33655878199994,2.2,-2.57824526200002));
#352377=CARTESIAN_POINT('Ctrl Pts',(3.33569070599995,12.2,-2.57693991900001));
#352378=CARTESIAN_POINT('Ctrl Pts',(3.33569070599995,5.2,-2.57693991900001));
#352379=CARTESIAN_POINT('Ctrl Pts',(3.33569070599995,2.2,-2.57693991900001));
#352380=CARTESIAN_POINT('Ctrl Pts',(3.33482368199994,12.2,-2.57563943400001));
#352381=CARTESIAN_POINT('Ctrl Pts',(3.33482368199994,5.2,-2.57563943400001));
#352382=CARTESIAN_POINT('Ctrl Pts',(3.33482368199994,2.2,-2.57563943400001));
#352383=CARTESIAN_POINT('Ctrl Pts',(3.33395772199995,12.2,-2.57434380900001));
#352384=CARTESIAN_POINT('Ctrl Pts',(3.33395772199995,5.2,-2.57434380900001));
#352385=CARTESIAN_POINT('Ctrl Pts',(3.33395772199995,2.2,-2.57434380900001));
#352386=CARTESIAN_POINT('Ctrl Pts',(3.33309283999994,12.2,-2.57305304400001));
#352387=CARTESIAN_POINT('Ctrl Pts',(3.33309283999994,5.2,-2.57305304400001));
#352388=CARTESIAN_POINT('Ctrl Pts',(3.33309283999994,2.2,-2.57305304400001));
#352389=CARTESIAN_POINT('Ctrl Pts',(3.33222904799995,12.2,-2.57176714300002));
#352390=CARTESIAN_POINT('Ctrl Pts',(3.33222904799995,5.2,-2.57176714300002));
#352391=CARTESIAN_POINT('Ctrl Pts',(3.33222904799995,2.2,-2.57176714300002));
#352392=CARTESIAN_POINT('Ctrl Pts',(3.33136635799994,12.2,-2.57048610500001));
#352393=CARTESIAN_POINT('Ctrl Pts',(3.33136635799994,5.2,-2.57048610500001));
#352394=CARTESIAN_POINT('Ctrl Pts',(3.33136635799994,2.2,-2.57048610500001));
#352395=CARTESIAN_POINT('Ctrl Pts',(3.33050478599994,12.2,-2.56920993400001));
#352396=CARTESIAN_POINT('Ctrl Pts',(3.33050478599994,5.2,-2.56920993400001));
#352397=CARTESIAN_POINT('Ctrl Pts',(3.33050478599994,2.2,-2.56920993400001));
#352398=CARTESIAN_POINT('Ctrl Pts',(3.32964434199994,12.2,-2.56793862900001));
#352399=CARTESIAN_POINT('Ctrl Pts',(3.32964434199994,5.2,-2.56793862900001));
#352400=CARTESIAN_POINT('Ctrl Pts',(3.32964434199994,2.2,-2.56793862900001));
#352401=CARTESIAN_POINT('Ctrl Pts',(3.32878504099994,12.2,-2.56667219300001));
#352402=CARTESIAN_POINT('Ctrl Pts',(3.32878504099994,5.2,-2.56667219300001));
#352403=CARTESIAN_POINT('Ctrl Pts',(3.32878504099994,2.2,-2.56667219300001));
#352404=CARTESIAN_POINT('Ctrl Pts',(3.32792689599994,12.2,-2.56541062700002));
#352405=CARTESIAN_POINT('Ctrl Pts',(3.32792689599994,5.2,-2.56541062700002));
#352406=CARTESIAN_POINT('Ctrl Pts',(3.32792689599994,2.2,-2.56541062700002));
#352407=CARTESIAN_POINT('Ctrl Pts',(3.32706991799995,12.2,-2.56415393300002));
#352408=CARTESIAN_POINT('Ctrl Pts',(3.32706991799995,5.2,-2.56415393300002));
#352409=CARTESIAN_POINT('Ctrl Pts',(3.32706991799995,2.2,-2.56415393300002));
#352410=CARTESIAN_POINT('Ctrl Pts',(3.32621412299994,12.2,-2.56290211100001));
#352411=CARTESIAN_POINT('Ctrl Pts',(3.32621412299994,5.2,-2.56290211100001));
#352412=CARTESIAN_POINT('Ctrl Pts',(3.32621412299994,2.2,-2.56290211100001));
#352413=CARTESIAN_POINT('Ctrl Pts',(3.32535952199994,12.2,-2.56165516400001));
#352414=CARTESIAN_POINT('Ctrl Pts',(3.32535952199994,5.2,-2.56165516400001));
#352415=CARTESIAN_POINT('Ctrl Pts',(3.32535952199994,2.2,-2.56165516400001));
#352416=CARTESIAN_POINT('Ctrl Pts',(3.32450612999994,12.2,-2.56041309300001));
#352417=CARTESIAN_POINT('Ctrl Pts',(3.32450612999994,5.2,-2.56041309300001));
#352418=CARTESIAN_POINT('Ctrl Pts',(3.32450612999994,2.2,-2.56041309300001));
#352419=CARTESIAN_POINT('Ctrl Pts',(3.32365395799994,12.2,-2.55917589900001));
#352420=CARTESIAN_POINT('Ctrl Pts',(3.32365395799994,5.2,-2.55917589900001));
#352421=CARTESIAN_POINT('Ctrl Pts',(3.32365395799994,2.2,-2.55917589900001));
#352422=CARTESIAN_POINT('Ctrl Pts',(3.32280302199994,12.2,-2.55794358200002));
#352423=CARTESIAN_POINT('Ctrl Pts',(3.32280302199994,5.2,-2.55794358200002));
#352424=CARTESIAN_POINT('Ctrl Pts',(3.32280302199994,2.2,-2.55794358200002));
#352425=CARTESIAN_POINT('Ctrl Pts',(3.32195333399994,12.2,-2.55671614800002));
#352426=CARTESIAN_POINT('Ctrl Pts',(3.32195333399994,5.2,-2.55671614800002));
#352427=CARTESIAN_POINT('Ctrl Pts',(3.32195333399994,2.2,-2.55671614800002));
#352428=CARTESIAN_POINT('Ctrl Pts',(3.32110490699994,12.2,-2.55549359300002));
#352429=CARTESIAN_POINT('Ctrl Pts',(3.32110490699994,5.2,-2.55549359300002));
#352430=CARTESIAN_POINT('Ctrl Pts',(3.32110490699994,2.2,-2.55549359300002));
#352431=CARTESIAN_POINT('Ctrl Pts',(3.32025775399994,12.2,-2.55427592000002));
#352432=CARTESIAN_POINT('Ctrl Pts',(3.32025775399994,5.2,-2.55427592000002));
#352433=CARTESIAN_POINT('Ctrl Pts',(3.32025775399994,2.2,-2.55427592000002));
#352434=CARTESIAN_POINT('Ctrl Pts',(3.31941188999994,12.2,-2.55306313200002));
#352435=CARTESIAN_POINT('Ctrl Pts',(3.31941188999994,5.2,-2.55306313200002));
#352436=CARTESIAN_POINT('Ctrl Pts',(3.31941188999994,2.2,-2.55306313200002));
#352437=CARTESIAN_POINT('Ctrl Pts',(3.31856732599995,12.2,-2.55185522900002));
#352438=CARTESIAN_POINT('Ctrl Pts',(3.31856732599995,5.2,-2.55185522900002));
#352439=CARTESIAN_POINT('Ctrl Pts',(3.31856732599995,2.2,-2.55185522900002));
#352440=CARTESIAN_POINT('Ctrl Pts',(3.31772407899994,12.2,-2.55065221300002));
#352441=CARTESIAN_POINT('Ctrl Pts',(3.31772407899994,5.2,-2.55065221300002));
#352442=CARTESIAN_POINT('Ctrl Pts',(3.31772407899994,2.2,-2.55065221300002));
#352443=CARTESIAN_POINT('Ctrl Pts',(3.31688215899994,12.2,-2.54945408300001));
#352444=CARTESIAN_POINT('Ctrl Pts',(3.31688215899994,5.2,-2.54945408300001));
#352445=CARTESIAN_POINT('Ctrl Pts',(3.31688215899994,2.2,-2.54945408300001));
#352446=CARTESIAN_POINT('Ctrl Pts',(3.31604158099994,12.2,-2.54826084400001));
#352447=CARTESIAN_POINT('Ctrl Pts',(3.31604158099994,5.2,-2.54826084400001));
#352448=CARTESIAN_POINT('Ctrl Pts',(3.31604158099994,2.2,-2.54826084400001));
#352449=CARTESIAN_POINT('Ctrl Pts',(3.31520235799994,12.2,-2.54707249400001));
#352450=CARTESIAN_POINT('Ctrl Pts',(3.31520235799994,5.2,-2.54707249400001));
#352451=CARTESIAN_POINT('Ctrl Pts',(3.31520235799994,2.2,-2.54707249400001));
#352452=CARTESIAN_POINT('Ctrl Pts',(3.31436450499994,12.2,-2.54588903500002));
#352453=CARTESIAN_POINT('Ctrl Pts',(3.31436450499994,5.2,-2.54588903500002));
#352454=CARTESIAN_POINT('Ctrl Pts',(3.31436450499994,2.2,-2.54588903500002));
#352455=CARTESIAN_POINT('Ctrl Pts',(3.31352803299994,12.2,-2.54471047000001));
#352456=CARTESIAN_POINT('Ctrl Pts',(3.31352803299994,5.2,-2.54471047000001));
#352457=CARTESIAN_POINT('Ctrl Pts',(3.31352803299994,2.2,-2.54471047000001));
#352458=CARTESIAN_POINT('Ctrl Pts',(3.31269295899994,12.2,-2.54353679800001));
#352459=CARTESIAN_POINT('Ctrl Pts',(3.31269295899994,5.2,-2.54353679800001));
#352460=CARTESIAN_POINT('Ctrl Pts',(3.31269295899994,2.2,-2.54353679800001));
#352461=CARTESIAN_POINT('Ctrl Pts',(3.31185929299994,12.2,-2.54236802100001));
#352462=CARTESIAN_POINT('Ctrl Pts',(3.31185929299994,5.2,-2.54236802100001));
#352463=CARTESIAN_POINT('Ctrl Pts',(3.31185929299994,2.2,-2.54236802100001));
#352464=CARTESIAN_POINT('Ctrl Pts',(3.31102705199994,12.2,-2.54120414000001));
#352465=CARTESIAN_POINT('Ctrl Pts',(3.31102705199994,5.2,-2.54120414000001));
#352466=CARTESIAN_POINT('Ctrl Pts',(3.31102705199994,2.2,-2.54120414000001));
#352467=CARTESIAN_POINT('Ctrl Pts',(3.31019624799994,12.2,-2.54004515600001));
#352468=CARTESIAN_POINT('Ctrl Pts',(3.31019624799994,5.2,-2.54004515600001));
#352469=CARTESIAN_POINT('Ctrl Pts',(3.31019624799994,2.2,-2.54004515600001));
#352470=CARTESIAN_POINT('Ctrl Pts',(3.30936689399994,12.2,-2.53889107200001));
#352471=CARTESIAN_POINT('Ctrl Pts',(3.30936689399994,5.2,-2.53889107200001));
#352472=CARTESIAN_POINT('Ctrl Pts',(3.30936689399994,2.2,-2.53889107200001));
#352473=CARTESIAN_POINT('Ctrl Pts',(3.30853900499994,12.2,-2.53774188600001));
#352474=CARTESIAN_POINT('Ctrl Pts',(3.30853900499994,5.2,-2.53774188600001));
#352475=CARTESIAN_POINT('Ctrl Pts',(3.30853900499994,2.2,-2.53774188600001));
#352476=CARTESIAN_POINT('Ctrl Pts',(3.30771259499994,12.2,-2.53659760000001));
#352477=CARTESIAN_POINT('Ctrl Pts',(3.30771259499994,5.2,-2.53659760000001));
#352478=CARTESIAN_POINT('Ctrl Pts',(3.30771259499994,2.2,-2.53659760000001));
#352479=CARTESIAN_POINT('Ctrl Pts',(3.30688767699994,12.2,-2.53545821700001));
#352480=CARTESIAN_POINT('Ctrl Pts',(3.30688767699994,5.2,-2.53545821700001));
#352481=CARTESIAN_POINT('Ctrl Pts',(3.30688767699994,2.2,-2.53545821700001));
#352482=CARTESIAN_POINT('Ctrl Pts',(3.30606426599994,12.2,-2.53432373600001));
#352483=CARTESIAN_POINT('Ctrl Pts',(3.30606426599994,5.2,-2.53432373600001));
#352484=CARTESIAN_POINT('Ctrl Pts',(3.30606426599994,2.2,-2.53432373600001));
#352485=CARTESIAN_POINT('Ctrl Pts',(3.30524237399994,12.2,-2.53319416000001));
#352486=CARTESIAN_POINT('Ctrl Pts',(3.30524237399994,5.2,-2.53319416000001));
#352487=CARTESIAN_POINT('Ctrl Pts',(3.30524237399994,2.2,-2.53319416000001));
#352488=CARTESIAN_POINT('Ctrl Pts',(3.30442201699995,12.2,-2.53206948800001));
#352489=CARTESIAN_POINT('Ctrl Pts',(3.30442201699995,5.2,-2.53206948800001));
#352490=CARTESIAN_POINT('Ctrl Pts',(3.30442201699995,2.2,-2.53206948800001));
#352491=CARTESIAN_POINT('Ctrl Pts',(3.30360320699994,12.2,-2.53094972100001));
#352492=CARTESIAN_POINT('Ctrl Pts',(3.30360320699994,5.2,-2.53094972100001));
#352493=CARTESIAN_POINT('Ctrl Pts',(3.30360320699994,2.2,-2.53094972100001));
#352494=CARTESIAN_POINT('Ctrl Pts',(3.30278595899994,12.2,-2.52983486200002));
#352495=CARTESIAN_POINT('Ctrl Pts',(3.30278595899994,5.2,-2.52983486200002));
#352496=CARTESIAN_POINT('Ctrl Pts',(3.30278595899994,2.2,-2.52983486200002));
#352497=CARTESIAN_POINT('Ctrl Pts',(3.30197028899994,12.2,-2.52872491000002));
#352498=CARTESIAN_POINT('Ctrl Pts',(3.30197028899994,5.2,-2.52872491000002));
#352499=CARTESIAN_POINT('Ctrl Pts',(3.30197028899994,2.2,-2.52872491000002));
#352500=CARTESIAN_POINT('Ctrl Pts',(3.30115620599994,12.2,-2.52761986800001));
#352501=CARTESIAN_POINT('Ctrl Pts',(3.30115620599994,5.2,-2.52761986800001));
#352502=CARTESIAN_POINT('Ctrl Pts',(3.30115620599994,2.2,-2.52761986800001));
#352503=CARTESIAN_POINT('Ctrl Pts',(3.30034372899994,12.2,-2.52651973400001));
#352504=CARTESIAN_POINT('Ctrl Pts',(3.30034372899994,5.2,-2.52651973400001));
#352505=CARTESIAN_POINT('Ctrl Pts',(3.30034372899994,2.2,-2.52651973400001));
#352506=CARTESIAN_POINT('Ctrl Pts',(3.29953286999995,12.2,-2.52542451100001));
#352507=CARTESIAN_POINT('Ctrl Pts',(3.29953286999995,5.2,-2.52542451100001));
#352508=CARTESIAN_POINT('Ctrl Pts',(3.29953286999995,2.2,-2.52542451100001));
#352509=CARTESIAN_POINT('Ctrl Pts',(3.29872364399994,12.2,-2.52433420000001));
#352510=CARTESIAN_POINT('Ctrl Pts',(3.29872364399994,5.2,-2.52433420000001));
#352511=CARTESIAN_POINT('Ctrl Pts',(3.29872364399994,2.2,-2.52433420000001));
#352512=CARTESIAN_POINT('Ctrl Pts',(3.29791606299994,12.2,-2.52324880100002));
#352513=CARTESIAN_POINT('Ctrl Pts',(3.29791606299994,5.2,-2.52324880100002));
#352514=CARTESIAN_POINT('Ctrl Pts',(3.29791606299994,2.2,-2.52324880100002));
#352515=CARTESIAN_POINT('Ctrl Pts',(3.29711014399994,12.2,-2.52216831700002));
#352516=CARTESIAN_POINT('Ctrl Pts',(3.29711014399994,5.2,-2.52216831700002));
#352517=CARTESIAN_POINT('Ctrl Pts',(3.29711014399994,2.2,-2.52216831700002));
#352518=CARTESIAN_POINT('Ctrl Pts',(3.29630589899994,12.2,-2.52109274600001));
#352519=CARTESIAN_POINT('Ctrl Pts',(3.29630589899994,5.2,-2.52109274600001));
#352520=CARTESIAN_POINT('Ctrl Pts',(3.29630589899994,2.2,-2.52109274600001));
#352521=CARTESIAN_POINT('Ctrl Pts',(3.29550334399995,12.2,-2.52002208900001));
#352522=CARTESIAN_POINT('Ctrl Pts',(3.29550334399995,5.2,-2.52002208900001));
#352523=CARTESIAN_POINT('Ctrl Pts',(3.29550334399995,2.2,-2.52002208900001));
#352524=CARTESIAN_POINT('Ctrl Pts',(3.29470249199994,12.2,-2.51895634900002));
#352525=CARTESIAN_POINT('Ctrl Pts',(3.29470249199994,5.2,-2.51895634900002));
#352526=CARTESIAN_POINT('Ctrl Pts',(3.29470249199994,2.2,-2.51895634900002));
#352527=CARTESIAN_POINT('Ctrl Pts',(3.29390335899994,12.2,-2.51789552600002));
#352528=CARTESIAN_POINT('Ctrl Pts',(3.29390335899994,5.2,-2.51789552600002));
#352529=CARTESIAN_POINT('Ctrl Pts',(3.29390335899994,2.2,-2.51789552600002));
#352530=CARTESIAN_POINT('Ctrl Pts',(3.29310595699994,12.2,-2.51683961900001));
#352531=CARTESIAN_POINT('Ctrl Pts',(3.29310595699994,5.2,-2.51683961900001));
#352532=CARTESIAN_POINT('Ctrl Pts',(3.29310595699994,2.2,-2.51683961900001));
#352533=CARTESIAN_POINT('Ctrl Pts',(3.29231030199994,12.2,-2.51578863100002));
#352534=CARTESIAN_POINT('Ctrl Pts',(3.29231030199994,5.2,-2.51578863100002));
#352535=CARTESIAN_POINT('Ctrl Pts',(3.29231030199994,2.2,-2.51578863100002));
#352536=CARTESIAN_POINT('Ctrl Pts',(3.29151640799994,12.2,-2.51474256300002));
#352537=CARTESIAN_POINT('Ctrl Pts',(3.29151640799994,5.2,-2.51474256300002));
#352538=CARTESIAN_POINT('Ctrl Pts',(3.29151640799994,2.2,-2.51474256300002));
#352539=CARTESIAN_POINT('Ctrl Pts',(3.29072428899994,12.2,-2.51370141400002));
#352540=CARTESIAN_POINT('Ctrl Pts',(3.29072428899994,5.2,-2.51370141400002));
#352541=CARTESIAN_POINT('Ctrl Pts',(3.29072428899994,2.2,-2.51370141400002));
#352542=CARTESIAN_POINT('Ctrl Pts',(3.28993396199994,12.2,-2.51266518600001));
#352543=CARTESIAN_POINT('Ctrl Pts',(3.28993396199994,5.2,-2.51266518600001));
#352544=CARTESIAN_POINT('Ctrl Pts',(3.28993396199994,2.2,-2.51266518600001));
#352545=CARTESIAN_POINT('Ctrl Pts',(3.28914543799995,12.2,-2.51163387800001));
#352546=CARTESIAN_POINT('Ctrl Pts',(3.28914543799995,5.2,-2.51163387800001));
#352547=CARTESIAN_POINT('Ctrl Pts',(3.28914543799995,2.2,-2.51163387800001));
#352548=CARTESIAN_POINT('Ctrl Pts',(3.28835873299994,12.2,-2.51060749200001));
#352549=CARTESIAN_POINT('Ctrl Pts',(3.28835873299994,5.2,-2.51060749200001));
#352550=CARTESIAN_POINT('Ctrl Pts',(3.28835873299994,2.2,-2.51060749200001));
#352551=CARTESIAN_POINT('Ctrl Pts',(3.28757386299994,12.2,-2.50958602900001));
#352552=CARTESIAN_POINT('Ctrl Pts',(3.28757386299994,5.2,-2.50958602900001));
#352553=CARTESIAN_POINT('Ctrl Pts',(3.28757386299994,2.2,-2.50958602900001));
#352554=CARTESIAN_POINT('Ctrl Pts',(3.28679083999994,12.2,-2.50856948900001));
#352555=CARTESIAN_POINT('Ctrl Pts',(3.28679083999994,5.2,-2.50856948900001));
#352556=CARTESIAN_POINT('Ctrl Pts',(3.28679083999994,2.2,-2.50856948900001));
#352557=CARTESIAN_POINT('Ctrl Pts',(3.28600967999995,12.2,-2.50755787300001));
#352558=CARTESIAN_POINT('Ctrl Pts',(3.28600967999995,5.2,-2.50755787300001));
#352559=CARTESIAN_POINT('Ctrl Pts',(3.28600967999995,2.2,-2.50755787300001));
#352560=CARTESIAN_POINT('Ctrl Pts',(3.28523039899994,12.2,-2.50655118100001));
#352561=CARTESIAN_POINT('Ctrl Pts',(3.28523039899994,5.2,-2.50655118100001));
#352562=CARTESIAN_POINT('Ctrl Pts',(3.28523039899994,2.2,-2.50655118100001));
#352563=CARTESIAN_POINT('Ctrl Pts',(3.28445300899994,12.2,-2.50554941500001));
#352564=CARTESIAN_POINT('Ctrl Pts',(3.28445300899994,5.2,-2.50554941500001));
#352565=CARTESIAN_POINT('Ctrl Pts',(3.28445300899994,2.2,-2.50554941500001));
#352566=CARTESIAN_POINT('Ctrl Pts',(3.28367752699994,12.2,-2.50455257400001));
#352567=CARTESIAN_POINT('Ctrl Pts',(3.28367752699994,5.2,-2.50455257400001));
#352568=CARTESIAN_POINT('Ctrl Pts',(3.28367752699994,2.2,-2.50455257400001));
#352569=CARTESIAN_POINT('Ctrl Pts',(3.28290396699995,12.2,-2.50356065900001));
#352570=CARTESIAN_POINT('Ctrl Pts',(3.28290396699995,5.2,-2.50356065900001));
#352571=CARTESIAN_POINT('Ctrl Pts',(3.28290396699995,2.2,-2.50356065900001));
#352572=CARTESIAN_POINT('Ctrl Pts',(3.28213234399994,12.2,-2.50257367100001));
#352573=CARTESIAN_POINT('Ctrl Pts',(3.28213234399994,5.2,-2.50257367100001));
#352574=CARTESIAN_POINT('Ctrl Pts',(3.28213234399994,2.2,-2.50257367100001));
#352575=CARTESIAN_POINT('Ctrl Pts',(3.28136267199994,12.2,-2.50159161100001));
#352576=CARTESIAN_POINT('Ctrl Pts',(3.28136267199994,5.2,-2.50159161100001));
#352577=CARTESIAN_POINT('Ctrl Pts',(3.28136267199994,2.2,-2.50159161100001));
#352578=CARTESIAN_POINT('Ctrl Pts',(3.28059496699994,12.2,-2.50061447800002));
#352579=CARTESIAN_POINT('Ctrl Pts',(3.28059496699994,5.2,-2.50061447800002));
#352580=CARTESIAN_POINT('Ctrl Pts',(3.28059496699994,2.2,-2.50061447800002));
#352581=CARTESIAN_POINT('Ctrl Pts',(3.27982924299994,12.2,-2.49964227300001));
#352582=CARTESIAN_POINT('Ctrl Pts',(3.27982924299994,5.2,-2.49964227300001));
#352583=CARTESIAN_POINT('Ctrl Pts',(3.27982924299994,2.2,-2.49964227300001));
#352584=CARTESIAN_POINT('Ctrl Pts',(3.27906551599995,12.2,-2.49867499700001));
#352585=CARTESIAN_POINT('Ctrl Pts',(3.27906551599995,5.2,-2.49867499700001));
#352586=CARTESIAN_POINT('Ctrl Pts',(3.27906551599995,2.2,-2.49867499700001));
#352587=CARTESIAN_POINT('Ctrl Pts',(3.27830380099994,12.2,-2.49771265100001));
#352588=CARTESIAN_POINT('Ctrl Pts',(3.27830380099994,5.2,-2.49771265100001));
#352589=CARTESIAN_POINT('Ctrl Pts',(3.27830380099994,2.2,-2.49771265100001));
#352590=CARTESIAN_POINT('Ctrl Pts',(3.27754411199995,12.2,-2.49675523400001));
#352591=CARTESIAN_POINT('Ctrl Pts',(3.27754411199995,5.2,-2.49675523400001));
#352592=CARTESIAN_POINT('Ctrl Pts',(3.27754411199995,2.2,-2.49675523400001));
#352593=CARTESIAN_POINT('Ctrl Pts',(3.27678646399994,12.2,-2.49580274700001));
#352594=CARTESIAN_POINT('Ctrl Pts',(3.27678646399994,5.2,-2.49580274700001));
#352595=CARTESIAN_POINT('Ctrl Pts',(3.27678646399994,2.2,-2.49580274700001));
#352596=CARTESIAN_POINT('Ctrl Pts',(3.27603087399994,12.2,-2.49485519100002));
#352597=CARTESIAN_POINT('Ctrl Pts',(3.27603087399994,5.2,-2.49485519100002));
#352598=CARTESIAN_POINT('Ctrl Pts',(3.27603087399994,2.2,-2.49485519100002));
#352599=CARTESIAN_POINT('Ctrl Pts',(3.27527735399994,12.2,-2.49391256500001));
#352600=CARTESIAN_POINT('Ctrl Pts',(3.27527735399994,5.2,-2.49391256500001));
#352601=CARTESIAN_POINT('Ctrl Pts',(3.27527735399994,2.2,-2.49391256500001));
#352602=CARTESIAN_POINT('Ctrl Pts',(3.27452592299994,12.2,-2.49297487000002));
#352603=CARTESIAN_POINT('Ctrl Pts',(3.27452592299994,5.2,-2.49297487000002));
#352604=CARTESIAN_POINT('Ctrl Pts',(3.27452592299994,2.2,-2.49297487000002));
#352605=CARTESIAN_POINT('Ctrl Pts',(3.27377659299994,12.2,-2.49204210700002));
#352606=CARTESIAN_POINT('Ctrl Pts',(3.27377659299994,5.2,-2.49204210700002));
#352607=CARTESIAN_POINT('Ctrl Pts',(3.27377659299994,2.2,-2.49204210700002));
#352608=CARTESIAN_POINT('Ctrl Pts',(3.27302938099994,12.2,-2.49111427700001));
#352609=CARTESIAN_POINT('Ctrl Pts',(3.27302938099994,5.2,-2.49111427700001));
#352610=CARTESIAN_POINT('Ctrl Pts',(3.27302938099994,2.2,-2.49111427700001));
#352611=CARTESIAN_POINT('Ctrl Pts',(3.27228430099994,12.2,-2.49019137800001));
#352612=CARTESIAN_POINT('Ctrl Pts',(3.27228430099994,5.2,-2.49019137800001));
#352613=CARTESIAN_POINT('Ctrl Pts',(3.27228430099994,2.2,-2.49019137800001));
#352614=CARTESIAN_POINT('Ctrl Pts',(3.27154136999994,12.2,-2.48927341100002));
#352615=CARTESIAN_POINT('Ctrl Pts',(3.27154136999994,5.2,-2.48927341100002));
#352616=CARTESIAN_POINT('Ctrl Pts',(3.27154136999994,2.2,-2.48927341100002));
#352617=CARTESIAN_POINT('Ctrl Pts',(3.27080060199994,12.2,-2.48836037800002));
#352618=CARTESIAN_POINT('Ctrl Pts',(3.27080060199994,5.2,-2.48836037800002));
#352619=CARTESIAN_POINT('Ctrl Pts',(3.27080060199994,2.2,-2.48836037800002));
#352620=CARTESIAN_POINT('Ctrl Pts',(3.27006201299994,12.2,-2.48745227700002));
#352621=CARTESIAN_POINT('Ctrl Pts',(3.27006201299994,5.2,-2.48745227700002));
#352622=CARTESIAN_POINT('Ctrl Pts',(3.27006201299994,2.2,-2.48745227700002));
#352623=CARTESIAN_POINT('Ctrl Pts',(3.26932561799994,12.2,-2.48654910900001));
#352624=CARTESIAN_POINT('Ctrl Pts',(3.26932561799994,5.2,-2.48654910900001));
#352625=CARTESIAN_POINT('Ctrl Pts',(3.26932561799994,2.2,-2.48654910900001));
#352626=CARTESIAN_POINT('Ctrl Pts',(3.26859143299994,12.2,-2.48565087500001));
#352627=CARTESIAN_POINT('Ctrl Pts',(3.26859143299994,5.2,-2.48565087500001));
#352628=CARTESIAN_POINT('Ctrl Pts',(3.26859143299994,2.2,-2.48565087500001));
#352629=CARTESIAN_POINT('Ctrl Pts',(3.26785947299994,12.2,-2.48475757400001));
#352630=CARTESIAN_POINT('Ctrl Pts',(3.26785947299994,5.2,-2.48475757400001));
#352631=CARTESIAN_POINT('Ctrl Pts',(3.26785947299994,2.2,-2.48475757400001));
#352632=CARTESIAN_POINT('Ctrl Pts',(3.26712975399994,12.2,-2.48386920800002));
#352633=CARTESIAN_POINT('Ctrl Pts',(3.26712975399994,5.2,-2.48386920800002));
#352634=CARTESIAN_POINT('Ctrl Pts',(3.26712975399994,2.2,-2.48386920800002));
#352635=CARTESIAN_POINT('Ctrl Pts',(3.26640229099994,12.2,-2.48298577500002));
#352636=CARTESIAN_POINT('Ctrl Pts',(3.26640229099994,5.2,-2.48298577500002));
#352637=CARTESIAN_POINT('Ctrl Pts',(3.26640229099994,2.2,-2.48298577500002));
#352638=CARTESIAN_POINT('Ctrl Pts',(3.26567710099994,12.2,-2.48210727600001));
#352639=CARTESIAN_POINT('Ctrl Pts',(3.26567710099994,5.2,-2.48210727600001));
#352640=CARTESIAN_POINT('Ctrl Pts',(3.26567710099994,2.2,-2.48210727600001));
#352641=CARTESIAN_POINT('Ctrl Pts',(3.26495419599994,12.2,-2.48123371200001));
#352642=CARTESIAN_POINT('Ctrl Pts',(3.26495419599994,5.2,-2.48123371200001));
#352643=CARTESIAN_POINT('Ctrl Pts',(3.26495419599994,2.2,-2.48123371200001));
#352644=CARTESIAN_POINT('Ctrl Pts',(3.26423359699994,12.2,-2.48036508100002));
#352645=CARTESIAN_POINT('Ctrl Pts',(3.26423359699994,5.2,-2.48036508100002));
#352646=CARTESIAN_POINT('Ctrl Pts',(3.26423359699994,2.2,-2.48036508100002));
#352647=CARTESIAN_POINT('Ctrl Pts',(3.26351531599995,12.2,-2.47950138600002));
#352648=CARTESIAN_POINT('Ctrl Pts',(3.26351531599995,5.2,-2.47950138600002));
#352649=CARTESIAN_POINT('Ctrl Pts',(3.26351531599995,2.2,-2.47950138600002));
#352650=CARTESIAN_POINT('Ctrl Pts',(3.26279936899994,12.2,-2.47864262300002));
#352651=CARTESIAN_POINT('Ctrl Pts',(3.26279936899994,5.2,-2.47864262300002));
#352652=CARTESIAN_POINT('Ctrl Pts',(3.26279936899994,2.2,-2.47864262300002));
#352653=CARTESIAN_POINT('Ctrl Pts',(3.26208577399994,12.2,-2.47778879600002));
#352654=CARTESIAN_POINT('Ctrl Pts',(3.26208577399994,5.2,-2.47778879600002));
#352655=CARTESIAN_POINT('Ctrl Pts',(3.26208577399994,2.2,-2.47778879600002));
#352656=CARTESIAN_POINT('Ctrl Pts',(3.26137454399994,12.2,-2.47693990400002));
#352657=CARTESIAN_POINT('Ctrl Pts',(3.26137454399994,5.2,-2.47693990400002));
#352658=CARTESIAN_POINT('Ctrl Pts',(3.26137454399994,2.2,-2.47693990400002));
#352659=CARTESIAN_POINT('Ctrl Pts',(3.26066569699994,12.2,-2.47609594400001));
#352660=CARTESIAN_POINT('Ctrl Pts',(3.26066569699994,5.2,-2.47609594400001));
#352661=CARTESIAN_POINT('Ctrl Pts',(3.26066569699994,2.2,-2.47609594400001));
#352662=CARTESIAN_POINT('Ctrl Pts',(3.25995924799994,12.2,-2.47525692100002));
#352663=CARTESIAN_POINT('Ctrl Pts',(3.25995924799994,5.2,-2.47525692100002));
#352664=CARTESIAN_POINT('Ctrl Pts',(3.25995924799994,2.2,-2.47525692100002));
#352665=CARTESIAN_POINT('Ctrl Pts',(3.25925521399994,12.2,-2.47442283100002));
#352666=CARTESIAN_POINT('Ctrl Pts',(3.25925521399994,5.2,-2.47442283100002));
#352667=CARTESIAN_POINT('Ctrl Pts',(3.25925521399994,2.2,-2.47442283100002));
#352668=CARTESIAN_POINT('Ctrl Pts',(3.25855360899994,12.2,-2.47359367500001));
#352669=CARTESIAN_POINT('Ctrl Pts',(3.25855360899994,5.2,-2.47359367500001));
#352670=CARTESIAN_POINT('Ctrl Pts',(3.25855360899994,2.2,-2.47359367500001));
#352671=CARTESIAN_POINT('Ctrl Pts',(3.25785445099994,12.2,-2.47276945400001));
#352672=CARTESIAN_POINT('Ctrl Pts',(3.25785445099994,5.2,-2.47276945400001));
#352673=CARTESIAN_POINT('Ctrl Pts',(3.25785445099994,2.2,-2.47276945400001));
#352674=CARTESIAN_POINT('Ctrl Pts',(3.25715775499994,12.2,-2.47195016500001));
#352675=CARTESIAN_POINT('Ctrl Pts',(3.25715775499994,5.2,-2.47195016500001));
#352676=CARTESIAN_POINT('Ctrl Pts',(3.25715775499994,2.2,-2.47195016500001));
#352677=CARTESIAN_POINT('Ctrl Pts',(3.25646353699995,12.2,-2.47113581200002));
#352678=CARTESIAN_POINT('Ctrl Pts',(3.25646353699995,5.2,-2.47113581200002));
#352679=CARTESIAN_POINT('Ctrl Pts',(3.25646353699995,2.2,-2.47113581200002));
#352680=CARTESIAN_POINT('Ctrl Pts',(3.25577181299994,12.2,-2.47032639200001));
#352681=CARTESIAN_POINT('Ctrl Pts',(3.25577181299994,5.2,-2.47032639200001));
#352682=CARTESIAN_POINT('Ctrl Pts',(3.25577181299994,2.2,-2.47032639200001));
#352683=CARTESIAN_POINT('Ctrl Pts',(3.25508260099994,12.2,-2.46952190600001));
#352684=CARTESIAN_POINT('Ctrl Pts',(3.25508260099994,5.2,-2.46952190600001));
#352685=CARTESIAN_POINT('Ctrl Pts',(3.25508260099994,2.2,-2.46952190600001));
#352686=CARTESIAN_POINT('Ctrl Pts',(3.25439591399994,12.2,-2.46872235300001));
#352687=CARTESIAN_POINT('Ctrl Pts',(3.25439591399994,5.2,-2.46872235300001));
#352688=CARTESIAN_POINT('Ctrl Pts',(3.25439591399994,2.2,-2.46872235300001));
#352689=CARTESIAN_POINT('Ctrl Pts',(3.25371177099994,12.2,-2.46792773300001));
#352690=CARTESIAN_POINT('Ctrl Pts',(3.25371177099994,5.2,-2.46792773300001));
#352691=CARTESIAN_POINT('Ctrl Pts',(3.25371177099994,2.2,-2.46792773300001));
#352692=CARTESIAN_POINT('Ctrl Pts',(3.25303018899994,12.2,-2.46713804600001));
#352693=CARTESIAN_POINT('Ctrl Pts',(3.25303018899994,5.2,-2.46713804600001));
#352694=CARTESIAN_POINT('Ctrl Pts',(3.25303018899994,2.2,-2.46713804600001));
#352695=CARTESIAN_POINT('Ctrl Pts',(3.25235118099994,12.2,-2.46635329200001));
#352696=CARTESIAN_POINT('Ctrl Pts',(3.25235118099994,5.2,-2.46635329200001));
#352697=CARTESIAN_POINT('Ctrl Pts',(3.25235118099994,2.2,-2.46635329200001));
#352698=CARTESIAN_POINT('Ctrl Pts',(3.25167476499994,12.2,-2.46557346900001));
#352699=CARTESIAN_POINT('Ctrl Pts',(3.25167476499994,5.2,-2.46557346900001));
#352700=CARTESIAN_POINT('Ctrl Pts',(3.25167476499994,2.2,-2.46557346900001));
#352701=CARTESIAN_POINT('Ctrl Pts',(3.25100095899994,12.2,-2.46479857900002));
#352702=CARTESIAN_POINT('Ctrl Pts',(3.25100095899994,5.2,-2.46479857900002));
#352703=CARTESIAN_POINT('Ctrl Pts',(3.25100095899994,2.2,-2.46479857900002));
#352704=CARTESIAN_POINT('Ctrl Pts',(3.25032977699995,12.2,-2.46402862100001));
#352705=CARTESIAN_POINT('Ctrl Pts',(3.25032977699995,5.2,-2.46402862100001));
#352706=CARTESIAN_POINT('Ctrl Pts',(3.25032977699995,2.2,-2.46402862100001));
#352707=CARTESIAN_POINT('Ctrl Pts',(3.24966123699994,12.2,-2.46326359400001));
#352708=CARTESIAN_POINT('Ctrl Pts',(3.24966123699994,5.2,-2.46326359400001));
#352709=CARTESIAN_POINT('Ctrl Pts',(3.24966123699994,2.2,-2.46326359400001));
#352710=CARTESIAN_POINT('Ctrl Pts',(3.24899535499994,12.2,-2.46250349800002));
#352711=CARTESIAN_POINT('Ctrl Pts',(3.24899535499994,5.2,-2.46250349800002));
#352712=CARTESIAN_POINT('Ctrl Pts',(3.24899535499994,2.2,-2.46250349800002));
#352713=CARTESIAN_POINT('Ctrl Pts',(3.24833214799995,12.2,-2.46174833200001));
#352714=CARTESIAN_POINT('Ctrl Pts',(3.24833214799995,5.2,-2.46174833200001));
#352715=CARTESIAN_POINT('Ctrl Pts',(3.24833214799995,2.2,-2.46174833200001));
#352716=CARTESIAN_POINT('Ctrl Pts',(3.24767163199994,12.2,-2.46099809700001));
#352717=CARTESIAN_POINT('Ctrl Pts',(3.24767163199994,5.2,-2.46099809700001));
#352718=CARTESIAN_POINT('Ctrl Pts',(3.24767163199994,2.2,-2.46099809700001));
#352719=CARTESIAN_POINT('Ctrl Pts',(3.24701382399994,12.2,-2.46025279100001));
#352720=CARTESIAN_POINT('Ctrl Pts',(3.24701382399994,5.2,-2.46025279100001));
#352721=CARTESIAN_POINT('Ctrl Pts',(3.24701382399994,2.2,-2.46025279100001));
#352722=CARTESIAN_POINT('Ctrl Pts',(3.24635874099994,12.2,-2.45951241500002));
#352723=CARTESIAN_POINT('Ctrl Pts',(3.24635874099994,5.2,-2.45951241500002));
#352724=CARTESIAN_POINT('Ctrl Pts',(3.24635874099994,2.2,-2.45951241500002));
#352725=CARTESIAN_POINT('Ctrl Pts',(3.24570639899994,12.2,-2.45877696800001));
#352726=CARTESIAN_POINT('Ctrl Pts',(3.24570639899994,5.2,-2.45877696800001));
#352727=CARTESIAN_POINT('Ctrl Pts',(3.24570639899994,2.2,-2.45877696800001));
#352728=CARTESIAN_POINT('Ctrl Pts',(3.24505681599994,12.2,-2.45804644900002));
#352729=CARTESIAN_POINT('Ctrl Pts',(3.24505681599994,5.2,-2.45804644900002));
#352730=CARTESIAN_POINT('Ctrl Pts',(3.24505681599994,2.2,-2.45804644900002));
#352731=CARTESIAN_POINT('Ctrl Pts',(3.24441000699994,12.2,-2.45732085700002));
#352732=CARTESIAN_POINT('Ctrl Pts',(3.24441000699994,5.2,-2.45732085700002));
#352733=CARTESIAN_POINT('Ctrl Pts',(3.24441000699994,2.2,-2.45732085700002));
#352734=CARTESIAN_POINT('Ctrl Pts',(3.24376599099995,12.2,-2.45660019300002));
#352735=CARTESIAN_POINT('Ctrl Pts',(3.24376599099995,5.2,-2.45660019300002));
#352736=CARTESIAN_POINT('Ctrl Pts',(3.24376599099995,2.2,-2.45660019300002));
#352737=CARTESIAN_POINT('Ctrl Pts',(3.24312478299994,12.2,-2.45588445400001));
#352738=CARTESIAN_POINT('Ctrl Pts',(3.24312478299994,5.2,-2.45588445400001));
#352739=CARTESIAN_POINT('Ctrl Pts',(3.24312478299994,2.2,-2.45588445400001));
#352740=CARTESIAN_POINT('Ctrl Pts',(3.24248640099994,12.2,-2.45517364300001));
#352741=CARTESIAN_POINT('Ctrl Pts',(3.24248640099994,5.2,-2.45517364300001));
#352742=CARTESIAN_POINT('Ctrl Pts',(3.24248640099994,2.2,-2.45517364300001));
#352743=CARTESIAN_POINT('Ctrl Pts',(3.24185086299994,12.2,-2.45446775600001));
#352744=CARTESIAN_POINT('Ctrl Pts',(3.24185086299994,5.2,-2.45446775600001));
#352745=CARTESIAN_POINT('Ctrl Pts',(3.24185086299994,2.2,-2.45446775600001));
#352746=CARTESIAN_POINT('Ctrl Pts',(3.24121818399994,12.2,-2.45376679500001));
#352747=CARTESIAN_POINT('Ctrl Pts',(3.24121818399994,5.2,-2.45376679500001));
#352748=CARTESIAN_POINT('Ctrl Pts',(3.24121818399994,2.2,-2.45376679500001));
#352749=CARTESIAN_POINT('Ctrl Pts',(3.24058838199994,12.2,-2.45307075800001));
#352750=CARTESIAN_POINT('Ctrl Pts',(3.24058838199994,5.2,-2.45307075800001));
#352751=CARTESIAN_POINT('Ctrl Pts',(3.24058838199994,2.2,-2.45307075800001));
#352752=CARTESIAN_POINT('Ctrl Pts',(3.23996147399995,12.2,-2.45237964400001));
#352753=CARTESIAN_POINT('Ctrl Pts',(3.23996147399995,5.2,-2.45237964400001));
#352754=CARTESIAN_POINT('Ctrl Pts',(3.23996147399995,2.2,-2.45237964400001));
#352755=CARTESIAN_POINT('Ctrl Pts',(3.23933747799994,12.2,-2.45169345300001));
#352756=CARTESIAN_POINT('Ctrl Pts',(3.23933747799994,5.2,-2.45169345300001));
#352757=CARTESIAN_POINT('Ctrl Pts',(3.23933747799994,2.2,-2.45169345300001));
#352758=CARTESIAN_POINT('Ctrl Pts',(3.23871640999994,12.2,-2.45101218300002));
#352759=CARTESIAN_POINT('Ctrl Pts',(3.23871640999994,5.2,-2.45101218300002));
#352760=CARTESIAN_POINT('Ctrl Pts',(3.23871640999994,2.2,-2.45101218300002));
#352761=CARTESIAN_POINT('Ctrl Pts',(3.23809828799994,12.2,-2.45033583500001));
#352762=CARTESIAN_POINT('Ctrl Pts',(3.23809828799994,5.2,-2.45033583500001));
#352763=CARTESIAN_POINT('Ctrl Pts',(3.23809828799994,2.2,-2.45033583500001));
#352764=CARTESIAN_POINT('Ctrl Pts',(3.23748312899995,12.2,-2.44966440700002));
#352765=CARTESIAN_POINT('Ctrl Pts',(3.23748312899995,5.2,-2.44966440700002));
#352766=CARTESIAN_POINT('Ctrl Pts',(3.23748312899995,2.2,-2.44966440700002));
#352767=CARTESIAN_POINT('Ctrl Pts',(3.23687094999995,12.2,-2.44899789900002));
#352768=CARTESIAN_POINT('Ctrl Pts',(3.23687094999995,5.2,-2.44899789900002));
#352769=CARTESIAN_POINT('Ctrl Pts',(3.23687094999995,2.2,-2.44899789900002));
#352770=CARTESIAN_POINT('Ctrl Pts',(3.23626176999994,12.2,-2.44833630900001));
#352771=CARTESIAN_POINT('Ctrl Pts',(3.23626176999994,5.2,-2.44833630900001));
#352772=CARTESIAN_POINT('Ctrl Pts',(3.23626176999994,2.2,-2.44833630900001));
#352773=CARTESIAN_POINT('Ctrl Pts',(3.23565560499994,12.2,-2.44767963800001));
#352774=CARTESIAN_POINT('Ctrl Pts',(3.23565560499994,5.2,-2.44767963800001));
#352775=CARTESIAN_POINT('Ctrl Pts',(3.23565560499994,2.2,-2.44767963800001));
#352776=CARTESIAN_POINT('Ctrl Pts',(3.23505247299994,12.2,-2.44702788400001));
#352777=CARTESIAN_POINT('Ctrl Pts',(3.23505247299994,5.2,-2.44702788400001));
#352778=CARTESIAN_POINT('Ctrl Pts',(3.23505247299994,2.2,-2.44702788400001));
#352779=CARTESIAN_POINT('Ctrl Pts',(3.23445239099994,12.2,-2.44638104600002));
#352780=CARTESIAN_POINT('Ctrl Pts',(3.23445239099994,5.2,-2.44638104600002));
#352781=CARTESIAN_POINT('Ctrl Pts',(3.23445239099994,2.2,-2.44638104600002));
#352782=CARTESIAN_POINT('Ctrl Pts',(3.23385537699994,12.2,-2.44573912300002));
#352783=CARTESIAN_POINT('Ctrl Pts',(3.23385537699994,5.2,-2.44573912300002));
#352784=CARTESIAN_POINT('Ctrl Pts',(3.23385537699994,2.2,-2.44573912300002));
#352785=CARTESIAN_POINT('Ctrl Pts',(3.23326144799994,12.2,-2.44510211400002));
#352786=CARTESIAN_POINT('Ctrl Pts',(3.23326144799994,5.2,-2.44510211400002));
#352787=CARTESIAN_POINT('Ctrl Pts',(3.23326144799994,2.2,-2.44510211400002));
#352788=CARTESIAN_POINT('Ctrl Pts',(3.23267062299994,12.2,-2.44447001800001));
#352789=CARTESIAN_POINT('Ctrl Pts',(3.23267062299994,5.2,-2.44447001800001));
#352790=CARTESIAN_POINT('Ctrl Pts',(3.23267062299994,2.2,-2.44447001800001));
#352791=CARTESIAN_POINT('Ctrl Pts',(3.23208291799994,12.2,-2.44384283500001));
#352792=CARTESIAN_POINT('Ctrl Pts',(3.23208291799994,5.2,-2.44384283500001));
#352793=CARTESIAN_POINT('Ctrl Pts',(3.23208291799994,2.2,-2.44384283500001));
#352794=CARTESIAN_POINT('Ctrl Pts',(3.23149835299994,12.2,-2.44322056300001));
#352795=CARTESIAN_POINT('Ctrl Pts',(3.23149835299994,5.2,-2.44322056300001));
#352796=CARTESIAN_POINT('Ctrl Pts',(3.23149835299994,2.2,-2.44322056300001));
#352797=CARTESIAN_POINT('Ctrl Pts',(3.23091694299994,12.2,-2.44260320100001));
#352798=CARTESIAN_POINT('Ctrl Pts',(3.23091694299994,5.2,-2.44260320100001));
#352799=CARTESIAN_POINT('Ctrl Pts',(3.23091694299994,2.2,-2.44260320100001));
#352800=CARTESIAN_POINT('Ctrl Pts',(3.23033870899994,12.2,-2.44199074800001));
#352801=CARTESIAN_POINT('Ctrl Pts',(3.23033870899994,5.2,-2.44199074800001));
#352802=CARTESIAN_POINT('Ctrl Pts',(3.23033870899994,2.2,-2.44199074800001));
#352803=CARTESIAN_POINT('Ctrl Pts',(3.22976366699995,12.2,-2.44138320400001));
#352804=CARTESIAN_POINT('Ctrl Pts',(3.22976366699995,5.2,-2.44138320400001));
#352805=CARTESIAN_POINT('Ctrl Pts',(3.22976366699995,2.2,-2.44138320400001));
#352806=CARTESIAN_POINT('Ctrl Pts',(3.22919183499994,12.2,-2.44078056700001));
#352807=CARTESIAN_POINT('Ctrl Pts',(3.22919183499994,5.2,-2.44078056700001));
#352808=CARTESIAN_POINT('Ctrl Pts',(3.22919183499994,2.2,-2.44078056700001));
#352809=CARTESIAN_POINT('Ctrl Pts',(3.22862323099995,12.2,-2.44018283400001));
#352810=CARTESIAN_POINT('Ctrl Pts',(3.22862323099995,5.2,-2.44018283400001));
#352811=CARTESIAN_POINT('Ctrl Pts',(3.22862323099995,2.2,-2.44018283400001));
#352812=CARTESIAN_POINT('Ctrl Pts',(3.22805787299994,12.2,-2.43959000700002));
#352813=CARTESIAN_POINT('Ctrl Pts',(3.22805787299994,5.2,-2.43959000700002));
#352814=CARTESIAN_POINT('Ctrl Pts',(3.22805787299994,2.2,-2.43959000700002));
#352815=CARTESIAN_POINT('Ctrl Pts',(3.22749577999994,12.2,-2.43900208300001));
#352816=CARTESIAN_POINT('Ctrl Pts',(3.22749577999994,5.2,-2.43900208300001));
#352817=CARTESIAN_POINT('Ctrl Pts',(3.22749577999994,2.2,-2.43900208300001));
#352818=CARTESIAN_POINT('Ctrl Pts',(3.22693696999994,12.2,-2.43841906100001));
#352819=CARTESIAN_POINT('Ctrl Pts',(3.22693696999994,5.2,-2.43841906100001));
#352820=CARTESIAN_POINT('Ctrl Pts',(3.22693696999994,2.2,-2.43841906100001));
#352821=CARTESIAN_POINT('Ctrl Pts',(3.22638145999994,12.2,-2.43784093900001));
#352822=CARTESIAN_POINT('Ctrl Pts',(3.22638145999994,5.2,-2.43784093900001));
#352823=CARTESIAN_POINT('Ctrl Pts',(3.22638145999994,2.2,-2.43784093900001));
#352824=CARTESIAN_POINT('Ctrl Pts',(3.22582926899994,12.2,-2.43726771800001));
#352825=CARTESIAN_POINT('Ctrl Pts',(3.22582926899994,5.2,-2.43726771800001));
#352826=CARTESIAN_POINT('Ctrl Pts',(3.22582926899994,2.2,-2.43726771800001));
#352827=CARTESIAN_POINT('Ctrl Pts',(3.22528041499994,12.2,-2.43669939500001));
#352828=CARTESIAN_POINT('Ctrl Pts',(3.22528041499994,5.2,-2.43669939500001));
#352829=CARTESIAN_POINT('Ctrl Pts',(3.22528041499994,2.2,-2.43669939500001));
#352830=CARTESIAN_POINT('Ctrl Pts',(3.22473491699995,12.2,-2.43613596900001));
#352831=CARTESIAN_POINT('Ctrl Pts',(3.22473491699995,5.2,-2.43613596900001));
#352832=CARTESIAN_POINT('Ctrl Pts',(3.22473491699995,2.2,-2.43613596900001));
#352833=CARTESIAN_POINT('Ctrl Pts',(3.22419279299994,12.2,-2.43557743800002));
#352834=CARTESIAN_POINT('Ctrl Pts',(3.22419279299994,5.2,-2.43557743800002));
#352835=CARTESIAN_POINT('Ctrl Pts',(3.22419279299994,2.2,-2.43557743800002));
#352836=CARTESIAN_POINT('Ctrl Pts',(3.22365406099994,12.2,-2.43502380100002));
#352837=CARTESIAN_POINT('Ctrl Pts',(3.22365406099994,5.2,-2.43502380100002));
#352838=CARTESIAN_POINT('Ctrl Pts',(3.22365406099994,2.2,-2.43502380100002));
#352839=CARTESIAN_POINT('Ctrl Pts',(3.22311873999995,12.2,-2.43447505800002));
#352840=CARTESIAN_POINT('Ctrl Pts',(3.22311873999995,5.2,-2.43447505800002));
#352841=CARTESIAN_POINT('Ctrl Pts',(3.22311873999995,2.2,-2.43447505800002));
#352842=CARTESIAN_POINT('Ctrl Pts',(3.22258684899994,12.2,-2.43393120500001));
#352843=CARTESIAN_POINT('Ctrl Pts',(3.22258684899994,5.2,-2.43393120500001));
#352844=CARTESIAN_POINT('Ctrl Pts',(3.22258684899994,2.2,-2.43393120500001));
#352845=CARTESIAN_POINT('Ctrl Pts',(3.22205840599994,12.2,-2.43339224300001));
#352846=CARTESIAN_POINT('Ctrl Pts',(3.22205840599994,5.2,-2.43339224300001));
#352847=CARTESIAN_POINT('Ctrl Pts',(3.22205840599994,2.2,-2.43339224300001));
#352848=CARTESIAN_POINT('Ctrl Pts',(3.22153342899994,12.2,-2.43285816900002));
#352849=CARTESIAN_POINT('Ctrl Pts',(3.22153342899994,5.2,-2.43285816900002));
#352850=CARTESIAN_POINT('Ctrl Pts',(3.22153342899994,2.2,-2.43285816900002));
#352851=CARTESIAN_POINT('Ctrl Pts',(3.22101193699994,12.2,-2.43232898100001));
#352852=CARTESIAN_POINT('Ctrl Pts',(3.22101193699994,5.2,-2.43232898100001));
#352853=CARTESIAN_POINT('Ctrl Pts',(3.22101193699994,2.2,-2.43232898100001));
#352854=CARTESIAN_POINT('Ctrl Pts',(3.22049394999994,12.2,-2.43180467900002));
#352855=CARTESIAN_POINT('Ctrl Pts',(3.22049394999994,5.2,-2.43180467900002));
#352856=CARTESIAN_POINT('Ctrl Pts',(3.22049394999994,2.2,-2.43180467900002));
#352857=CARTESIAN_POINT('Ctrl Pts',(3.21997948499994,12.2,-2.43128526200001));
#352858=CARTESIAN_POINT('Ctrl Pts',(3.21997948499994,5.2,-2.43128526200001));
#352859=CARTESIAN_POINT('Ctrl Pts',(3.21997948499994,2.2,-2.43128526200001));
#352860=CARTESIAN_POINT('Ctrl Pts',(3.21946856199995,12.2,-2.43077072500002));
#352861=CARTESIAN_POINT('Ctrl Pts',(3.21946856199995,5.2,-2.43077072500002));
#352862=CARTESIAN_POINT('Ctrl Pts',(3.21946856199995,2.2,-2.43077072500002));
#352863=CARTESIAN_POINT('Ctrl Pts',(3.21896119999994,12.2,-2.43026107000002));
#352864=CARTESIAN_POINT('Ctrl Pts',(3.21896119999994,5.2,-2.43026107000002));
#352865=CARTESIAN_POINT('Ctrl Pts',(3.21896119999994,2.2,-2.43026107000002));
#352866=CARTESIAN_POINT('Ctrl Pts',(3.21845741799994,12.2,-2.42975629300001));
#352867=CARTESIAN_POINT('Ctrl Pts',(3.21845741799994,5.2,-2.42975629300001));
#352868=CARTESIAN_POINT('Ctrl Pts',(3.21845741799994,2.2,-2.42975629300001));
#352869=CARTESIAN_POINT('Ctrl Pts',(3.21795723299994,12.2,-2.42925639400001));
#352870=CARTESIAN_POINT('Ctrl Pts',(3.21795723299994,5.2,-2.42925639400001));
#352871=CARTESIAN_POINT('Ctrl Pts',(3.21795723299994,2.2,-2.42925639400001));
#352872=CARTESIAN_POINT('Ctrl Pts',(3.21746066699995,12.2,-2.42876137000001));
#352873=CARTESIAN_POINT('Ctrl Pts',(3.21746066699995,5.2,-2.42876137000001));
#352874=CARTESIAN_POINT('Ctrl Pts',(3.21746066699995,2.2,-2.42876137000001));
#352875=CARTESIAN_POINT('Ctrl Pts',(3.21696773699994,12.2,-2.42827122000001));
#352876=CARTESIAN_POINT('Ctrl Pts',(3.21696773699994,5.2,-2.42827122000001));
#352877=CARTESIAN_POINT('Ctrl Pts',(3.21696773699994,2.2,-2.42827122000001));
#352878=CARTESIAN_POINT('Ctrl Pts',(3.21647846299994,12.2,-2.42778594200002));
#352879=CARTESIAN_POINT('Ctrl Pts',(3.21647846299994,5.2,-2.42778594200002));
#352880=CARTESIAN_POINT('Ctrl Pts',(3.21647846299994,2.2,-2.42778594200002));
#352881=CARTESIAN_POINT('Ctrl Pts',(3.21599286399994,12.2,-2.42730553400001));
#352882=CARTESIAN_POINT('Ctrl Pts',(3.21599286399994,5.2,-2.42730553400001));
#352883=CARTESIAN_POINT('Ctrl Pts',(3.21599286399994,2.2,-2.42730553400001));
#352884=CARTESIAN_POINT('Ctrl Pts',(3.21551095899994,12.2,-2.42682999400001));
#352885=CARTESIAN_POINT('Ctrl Pts',(3.21551095899994,5.2,-2.42682999400001));
#352886=CARTESIAN_POINT('Ctrl Pts',(3.21551095899994,2.2,-2.42682999400001));
#352887=CARTESIAN_POINT('Ctrl Pts',(3.21503276799994,12.2,-2.42635932000002));
#352888=CARTESIAN_POINT('Ctrl Pts',(3.21503276799994,5.2,-2.42635932000002));
#352889=CARTESIAN_POINT('Ctrl Pts',(3.21503276799994,2.2,-2.42635932000002));
#352890=CARTESIAN_POINT('Ctrl Pts',(3.21455830899994,12.2,-2.42589351200001));
#352891=CARTESIAN_POINT('Ctrl Pts',(3.21455830899994,5.2,-2.42589351200001));
#352892=CARTESIAN_POINT('Ctrl Pts',(3.21455830899994,2.2,-2.42589351200001));
#352893=CARTESIAN_POINT('Ctrl Pts',(3.21408760299994,12.2,-2.42543256700001));
#352894=CARTESIAN_POINT('Ctrl Pts',(3.21408760299994,5.2,-2.42543256700001));
#352895=CARTESIAN_POINT('Ctrl Pts',(3.21408760299994,2.2,-2.42543256700001));
#352896=CARTESIAN_POINT('Ctrl Pts',(3.21362066899994,12.2,-2.42497648100001));
#352897=CARTESIAN_POINT('Ctrl Pts',(3.21362066899994,5.2,-2.42497648100001));
#352898=CARTESIAN_POINT('Ctrl Pts',(3.21362066899994,2.2,-2.42497648100001));
#352899=CARTESIAN_POINT('Ctrl Pts',(3.21315752599994,12.2,-2.42452525400001));
#352900=CARTESIAN_POINT('Ctrl Pts',(3.21315752599994,5.2,-2.42452525400001));
#352901=CARTESIAN_POINT('Ctrl Pts',(3.21315752599994,2.2,-2.42452525400001));
#352902=CARTESIAN_POINT('Ctrl Pts',(3.21269819499994,12.2,-2.42407888400002));
#352903=CARTESIAN_POINT('Ctrl Pts',(3.21269819499994,5.2,-2.42407888400002));
#352904=CARTESIAN_POINT('Ctrl Pts',(3.21269819499994,2.2,-2.42407888400002));
#352905=CARTESIAN_POINT('Ctrl Pts',(3.21224269299994,12.2,-2.42363736900002));
#352906=CARTESIAN_POINT('Ctrl Pts',(3.21224269299994,5.2,-2.42363736900002));
#352907=CARTESIAN_POINT('Ctrl Pts',(3.21224269299994,2.2,-2.42363736900002));
#352908=CARTESIAN_POINT('Ctrl Pts',(3.21179104199994,12.2,-2.42320070700002));
#352909=CARTESIAN_POINT('Ctrl Pts',(3.21179104199994,5.2,-2.42320070700002));
#352910=CARTESIAN_POINT('Ctrl Pts',(3.21179104199994,2.2,-2.42320070700002));
#352911=CARTESIAN_POINT('Ctrl Pts',(3.21134326099994,12.2,-2.42276889600001));
#352912=CARTESIAN_POINT('Ctrl Pts',(3.21134326099994,5.2,-2.42276889600001));
#352913=CARTESIAN_POINT('Ctrl Pts',(3.21134326099994,2.2,-2.42276889600001));
#352914=CARTESIAN_POINT('Ctrl Pts',(3.21089936999994,12.2,-2.42234193200002));
#352915=CARTESIAN_POINT('Ctrl Pts',(3.21089936999994,5.2,-2.42234193200002));
#352916=CARTESIAN_POINT('Ctrl Pts',(3.21089936999994,2.2,-2.42234193200002));
#352917=CARTESIAN_POINT('Ctrl Pts',(3.21045938799994,12.2,-2.42191981500001));
#352918=CARTESIAN_POINT('Ctrl Pts',(3.21045938799994,5.2,-2.42191981500001));
#352919=CARTESIAN_POINT('Ctrl Pts',(3.21045938799994,2.2,-2.42191981500001));
#352920=CARTESIAN_POINT('Ctrl Pts',(3.21002333599994,12.2,-2.42150254300002));
#352921=CARTESIAN_POINT('Ctrl Pts',(3.21002333599994,5.2,-2.42150254300002));
#352922=CARTESIAN_POINT('Ctrl Pts',(3.21002333599994,2.2,-2.42150254300002));
#352923=CARTESIAN_POINT('Ctrl Pts',(3.20959123499994,12.2,-2.42109011200002));
#352924=CARTESIAN_POINT('Ctrl Pts',(3.20959123499994,5.2,-2.42109011200002));
#352925=CARTESIAN_POINT('Ctrl Pts',(3.20959123499994,2.2,-2.42109011200002));
#352926=CARTESIAN_POINT('Ctrl Pts',(3.20916310199994,12.2,-2.42068252000001));
#352927=CARTESIAN_POINT('Ctrl Pts',(3.20916310199994,5.2,-2.42068252000001));
#352928=CARTESIAN_POINT('Ctrl Pts',(3.20916310199994,2.2,-2.42068252000001));
#352929=CARTESIAN_POINT('Ctrl Pts',(3.20873895899994,12.2,-2.42027976700002));
#352930=CARTESIAN_POINT('Ctrl Pts',(3.20873895899994,5.2,-2.42027976700002));
#352931=CARTESIAN_POINT('Ctrl Pts',(3.20873895899994,2.2,-2.42027976700002));
#352932=CARTESIAN_POINT('Ctrl Pts',(3.20831882599995,12.2,-2.41988184800002));
#352933=CARTESIAN_POINT('Ctrl Pts',(3.20831882599995,5.2,-2.41988184800002));
#352934=CARTESIAN_POINT('Ctrl Pts',(3.20831882599995,2.2,-2.41988184800002));
#352935=CARTESIAN_POINT('Ctrl Pts',(3.20790272299994,12.2,-2.41948876200002));
#352936=CARTESIAN_POINT('Ctrl Pts',(3.20790272299994,5.2,-2.41948876200002));
#352937=CARTESIAN_POINT('Ctrl Pts',(3.20790272299994,2.2,-2.41948876200002));
#352938=CARTESIAN_POINT('Ctrl Pts',(3.20749066999995,12.2,-2.41910050600001));
#352939=CARTESIAN_POINT('Ctrl Pts',(3.20749066999995,5.2,-2.41910050600001));
#352940=CARTESIAN_POINT('Ctrl Pts',(3.20749066999995,2.2,-2.41910050600001));
#352941=CARTESIAN_POINT('Ctrl Pts',(3.20708268799994,12.2,-2.41871707900001));
#352942=CARTESIAN_POINT('Ctrl Pts',(3.20708268799994,5.2,-2.41871707900001));
#352943=CARTESIAN_POINT('Ctrl Pts',(3.20708268799994,2.2,-2.41871707900001));
#352944=CARTESIAN_POINT('Ctrl Pts',(3.20667879699994,12.2,-2.41833847700001));
#352945=CARTESIAN_POINT('Ctrl Pts',(3.20667879699994,5.2,-2.41833847700001));
#352946=CARTESIAN_POINT('Ctrl Pts',(3.20667879699994,2.2,-2.41833847700001));
#352947=CARTESIAN_POINT('Ctrl Pts',(3.20627901799994,12.2,-2.41796469800001));
#352948=CARTESIAN_POINT('Ctrl Pts',(3.20627901799994,5.2,-2.41796469800001));
#352949=CARTESIAN_POINT('Ctrl Pts',(3.20627901799994,2.2,-2.41796469800001));
#352950=CARTESIAN_POINT('Ctrl Pts',(3.20588337099994,12.2,-2.41759574100001));
#352951=CARTESIAN_POINT('Ctrl Pts',(3.20588337099994,5.2,-2.41759574100001));
#352952=CARTESIAN_POINT('Ctrl Pts',(3.20588337099994,2.2,-2.41759574100001));
#352953=CARTESIAN_POINT('Ctrl Pts',(3.20549187599994,12.2,-2.41723160100001));
#352954=CARTESIAN_POINT('Ctrl Pts',(3.20549187599994,5.2,-2.41723160100001));
#352955=CARTESIAN_POINT('Ctrl Pts',(3.20549187599994,2.2,-2.41723160100001));
#352956=CARTESIAN_POINT('Ctrl Pts',(3.20510455399994,12.2,-2.41687227600002));
#352957=CARTESIAN_POINT('Ctrl Pts',(3.20510455399994,5.2,-2.41687227600002));
#352958=CARTESIAN_POINT('Ctrl Pts',(3.20510455399994,2.2,-2.41687227600002));
#352959=CARTESIAN_POINT('Ctrl Pts',(3.20472142599994,12.2,-2.41651776500001));
#352960=CARTESIAN_POINT('Ctrl Pts',(3.20472142599994,5.2,-2.41651776500001));
#352961=CARTESIAN_POINT('Ctrl Pts',(3.20472142599994,2.2,-2.41651776500001));
#352962=CARTESIAN_POINT('Ctrl Pts',(3.20434251199994,12.2,-2.41616806400001));
#352963=CARTESIAN_POINT('Ctrl Pts',(3.20434251199994,5.2,-2.41616806400001));
#352964=CARTESIAN_POINT('Ctrl Pts',(3.20434251199994,2.2,-2.41616806400001));
#352965=CARTESIAN_POINT('Ctrl Pts',(3.20396783399994,12.2,-2.41582317100002));
#352966=CARTESIAN_POINT('Ctrl Pts',(3.20396783399994,5.2,-2.41582317100002));
#352967=CARTESIAN_POINT('Ctrl Pts',(3.20396783399994,2.2,-2.41582317100002));
#352968=CARTESIAN_POINT('Ctrl Pts',(3.20359741299994,12.2,-2.41548308200001));
#352969=CARTESIAN_POINT('Ctrl Pts',(3.20359741299994,5.2,-2.41548308200001));
#352970=CARTESIAN_POINT('Ctrl Pts',(3.20359741299994,2.2,-2.41548308200001));
#352971=CARTESIAN_POINT('Ctrl Pts',(3.20323126799994,12.2,-2.41514779700001));
#352972=CARTESIAN_POINT('Ctrl Pts',(3.20323126799994,5.2,-2.41514779700001));
#352973=CARTESIAN_POINT('Ctrl Pts',(3.20323126799994,2.2,-2.41514779700001));
#352974=CARTESIAN_POINT('Ctrl Pts',(3.20286942299994,12.2,-2.41481731100002));
#352975=CARTESIAN_POINT('Ctrl Pts',(3.20286942299994,5.2,-2.41481731100002));
#352976=CARTESIAN_POINT('Ctrl Pts',(3.20286942299994,2.2,-2.41481731100002));
#352977=CARTESIAN_POINT('Ctrl Pts',(3.20251189499994,12.2,-2.41449162100002));
#352978=CARTESIAN_POINT('Ctrl Pts',(3.20251189499994,5.2,-2.41449162100002));
#352979=CARTESIAN_POINT('Ctrl Pts',(3.20251189499994,2.2,-2.41449162100002));
#352980=CARTESIAN_POINT('Ctrl Pts',(3.20215870799994,12.2,-2.41417072600001));
#352981=CARTESIAN_POINT('Ctrl Pts',(3.20215870799994,5.2,-2.41417072600001));
#352982=CARTESIAN_POINT('Ctrl Pts',(3.20215870799994,2.2,-2.41417072600001));
#352983=CARTESIAN_POINT('Ctrl Pts',(3.20180988299994,12.2,-2.41385462100002));
#352984=CARTESIAN_POINT('Ctrl Pts',(3.20180988299994,5.2,-2.41385462100002));
#352985=CARTESIAN_POINT('Ctrl Pts',(3.20180988299994,2.2,-2.41385462100002));
#352986=CARTESIAN_POINT('Ctrl Pts',(3.20146543999994,12.2,-2.41354330500001));
#352987=CARTESIAN_POINT('Ctrl Pts',(3.20146543999994,5.2,-2.41354330500001));
#352988=CARTESIAN_POINT('Ctrl Pts',(3.20146543999994,2.2,-2.41354330500001));
#352989=CARTESIAN_POINT('Ctrl Pts',(3.20112540199994,12.2,-2.41323677400001));
#352990=CARTESIAN_POINT('Ctrl Pts',(3.20112540199994,5.2,-2.41323677400001));
#352991=CARTESIAN_POINT('Ctrl Pts',(3.20112540199994,2.2,-2.41323677400001));
#352992=CARTESIAN_POINT('Ctrl Pts',(3.20078978999994,12.2,-2.41293502500001));
#352993=CARTESIAN_POINT('Ctrl Pts',(3.20078978999994,5.2,-2.41293502500001));
#352994=CARTESIAN_POINT('Ctrl Pts',(3.20078978999994,2.2,-2.41293502500001));
#352995=CARTESIAN_POINT('Ctrl Pts',(3.20045862399994,12.2,-2.41263805700001));
#352996=CARTESIAN_POINT('Ctrl Pts',(3.20045862399994,5.2,-2.41263805700001));
#352997=CARTESIAN_POINT('Ctrl Pts',(3.20045862399994,2.2,-2.41263805700001));
#352998=CARTESIAN_POINT('Ctrl Pts',(3.20013192599995,12.2,-2.41234586400001));
#352999=CARTESIAN_POINT('Ctrl Pts',(3.20013192599995,5.2,-2.41234586400001));
#353000=CARTESIAN_POINT('Ctrl Pts',(3.20013192599995,2.2,-2.41234586400001));
#353001=CARTESIAN_POINT('Ctrl Pts',(3.19980971799994,12.2,-2.41205844500001));
#353002=CARTESIAN_POINT('Ctrl Pts',(3.19980971799994,5.2,-2.41205844500001));
#353003=CARTESIAN_POINT('Ctrl Pts',(3.19980971799994,2.2,-2.41205844500001));
#353004=CARTESIAN_POINT('Ctrl Pts',(3.19949202199994,12.2,-2.41177579500001));
#353005=CARTESIAN_POINT('Ctrl Pts',(3.19949202199994,5.2,-2.41177579500001));
#353006=CARTESIAN_POINT('Ctrl Pts',(3.19949202199994,2.2,-2.41177579500001));
#353007=CARTESIAN_POINT('Ctrl Pts',(3.19917885999994,12.2,-2.41149791400002));
#353008=CARTESIAN_POINT('Ctrl Pts',(3.19917885999994,5.2,-2.41149791400002));
#353009=CARTESIAN_POINT('Ctrl Pts',(3.19917885999994,2.2,-2.41149791400002));
#353010=CARTESIAN_POINT('Ctrl Pts',(3.19887025199994,12.2,-2.41122479400001));
#353011=CARTESIAN_POINT('Ctrl Pts',(3.19887025199994,5.2,-2.41122479400001));
#353012=CARTESIAN_POINT('Ctrl Pts',(3.19887025199994,2.2,-2.41122479400001));
#353013=CARTESIAN_POINT('Ctrl Pts',(3.19856622099994,12.2,-2.41095643700001));
#353014=CARTESIAN_POINT('Ctrl Pts',(3.19856622099994,5.2,-2.41095643700001));
#353015=CARTESIAN_POINT('Ctrl Pts',(3.19856622099994,2.2,-2.41095643700001));
#353016=CARTESIAN_POINT('Ctrl Pts',(3.19826678899994,12.2,-2.41069283800002));
#353017=CARTESIAN_POINT('Ctrl Pts',(3.19826678899994,5.2,-2.41069283800002));
#353018=CARTESIAN_POINT('Ctrl Pts',(3.19826678899994,2.2,-2.41069283800002));
#353019=CARTESIAN_POINT('Ctrl Pts',(3.19797197799994,12.2,-2.41043399200001));
#353020=CARTESIAN_POINT('Ctrl Pts',(3.19797197799994,5.2,-2.41043399200001));
#353021=CARTESIAN_POINT('Ctrl Pts',(3.19797197799994,2.2,-2.41043399200001));
#353022=CARTESIAN_POINT('Ctrl Pts',(3.19768180899994,12.2,-2.41017989700001));
#353023=CARTESIAN_POINT('Ctrl Pts',(3.19768180899994,5.2,-2.41017989700001));
#353024=CARTESIAN_POINT('Ctrl Pts',(3.19768180899994,2.2,-2.41017989700001));
#353025=CARTESIAN_POINT('Ctrl Pts',(3.19739630699994,12.2,-2.40993055000001));
#353026=CARTESIAN_POINT('Ctrl Pts',(3.19739630699994,5.2,-2.40993055000001));
#353027=CARTESIAN_POINT('Ctrl Pts',(3.19739630699994,2.2,-2.40993055000001));
#353028=CARTESIAN_POINT('Ctrl Pts',(3.19711548999994,12.2,-2.40968594700002));
#353029=CARTESIAN_POINT('Ctrl Pts',(3.19711548999994,5.2,-2.40968594700002));
#353030=CARTESIAN_POINT('Ctrl Pts',(3.19711548999994,2.2,-2.40968594700002));
#353031=CARTESIAN_POINT('Ctrl Pts',(3.19683938199995,12.2,-2.40944608600001));
#353032=CARTESIAN_POINT('Ctrl Pts',(3.19683938199995,5.2,-2.40944608600001));
#353033=CARTESIAN_POINT('Ctrl Pts',(3.19683938199995,2.2,-2.40944608600001));
#353034=CARTESIAN_POINT('Ctrl Pts',(3.19656800699994,12.2,-2.40921096100001));
#353035=CARTESIAN_POINT('Ctrl Pts',(3.19656800699994,5.2,-2.40921096100001));
#353036=CARTESIAN_POINT('Ctrl Pts',(3.19656800699994,2.2,-2.40921096100001));
#353037=CARTESIAN_POINT('Ctrl Pts',(3.19630138499994,12.2,-2.40898056900001));
#353038=CARTESIAN_POINT('Ctrl Pts',(3.19630138499994,5.2,-2.40898056900001));
#353039=CARTESIAN_POINT('Ctrl Pts',(3.19630138499994,2.2,-2.40898056900001));
#353040=CARTESIAN_POINT('Ctrl Pts',(3.19603954099994,12.2,-2.40875490900001));
#353041=CARTESIAN_POINT('Ctrl Pts',(3.19603954099994,5.2,-2.40875490900001));
#353042=CARTESIAN_POINT('Ctrl Pts',(3.19603954099994,2.2,-2.40875490900001));
#353043=CARTESIAN_POINT('Ctrl Pts',(3.19578249499994,12.2,-2.40853397500001));
#353044=CARTESIAN_POINT('Ctrl Pts',(3.19578249499994,5.2,-2.40853397500001));
#353045=CARTESIAN_POINT('Ctrl Pts',(3.19578249499994,2.2,-2.40853397500001));
#353046=CARTESIAN_POINT('Ctrl Pts',(3.19553027099994,12.2,-2.40831776500002));
#353047=CARTESIAN_POINT('Ctrl Pts',(3.19553027099994,5.2,-2.40831776500002));
#353048=CARTESIAN_POINT('Ctrl Pts',(3.19553027099994,2.2,-2.40831776500002));
#353049=CARTESIAN_POINT('Ctrl Pts',(3.19528289099994,12.2,-2.40810627400001));
#353050=CARTESIAN_POINT('Ctrl Pts',(3.19528289099994,5.2,-2.40810627400001));
#353051=CARTESIAN_POINT('Ctrl Pts',(3.19528289099994,2.2,-2.40810627400001));
#353052=CARTESIAN_POINT('Ctrl Pts',(3.19504037699994,12.2,-2.40789949900002));
#353053=CARTESIAN_POINT('Ctrl Pts',(3.19504037699994,5.2,-2.40789949900002));
#353054=CARTESIAN_POINT('Ctrl Pts',(3.19504037699994,2.2,-2.40789949900002));
#353055=CARTESIAN_POINT('Ctrl Pts',(3.19480275399994,12.2,-2.40769743600001));
#353056=CARTESIAN_POINT('Ctrl Pts',(3.19480275399994,5.2,-2.40769743600001));
#353057=CARTESIAN_POINT('Ctrl Pts',(3.19480275399994,2.2,-2.40769743600001));
#353058=CARTESIAN_POINT('Ctrl Pts',(3.19457004399994,12.2,-2.40750008200001));
#353059=CARTESIAN_POINT('Ctrl Pts',(3.19457004399994,5.2,-2.40750008200001));
#353060=CARTESIAN_POINT('Ctrl Pts',(3.19457004399994,2.2,-2.40750008200001));
#353061=CARTESIAN_POINT('Ctrl Pts',(3.19434226799994,12.2,-2.40730743200002));
#353062=CARTESIAN_POINT('Ctrl Pts',(3.19434226799994,5.2,-2.40730743200002));
#353063=CARTESIAN_POINT('Ctrl Pts',(3.19434226799994,2.2,-2.40730743200002));
#353064=CARTESIAN_POINT('Ctrl Pts',(3.19411945299994,12.2,-2.40711948300001));
#353065=CARTESIAN_POINT('Ctrl Pts',(3.19411945299994,5.2,-2.40711948300001));
#353066=CARTESIAN_POINT('Ctrl Pts',(3.19411945299994,2.2,-2.40711948300001));
#353067=CARTESIAN_POINT('Ctrl Pts',(3.19390161799994,12.2,-2.40693623100002));
#353068=CARTESIAN_POINT('Ctrl Pts',(3.19390161799994,5.2,-2.40693623100002));
#353069=CARTESIAN_POINT('Ctrl Pts',(3.19390161799994,2.2,-2.40693623100002));
#353070=CARTESIAN_POINT('Ctrl Pts',(3.19368878899994,12.2,-2.40675767200001));
#353071=CARTESIAN_POINT('Ctrl Pts',(3.19368878899994,5.2,-2.40675767200001));
#353072=CARTESIAN_POINT('Ctrl Pts',(3.19368878899994,2.2,-2.40675767200001));
#353073=CARTESIAN_POINT('Ctrl Pts',(3.19348098699994,12.2,-2.40658380300002));
#353074=CARTESIAN_POINT('Ctrl Pts',(3.19348098699994,5.2,-2.40658380300002));
#353075=CARTESIAN_POINT('Ctrl Pts',(3.19348098699994,2.2,-2.40658380300002));
#353076=CARTESIAN_POINT('Ctrl Pts',(3.19327823699994,12.2,-2.40641461800001));
#353077=CARTESIAN_POINT('Ctrl Pts',(3.19327823699994,5.2,-2.40641461800001));
#353078=CARTESIAN_POINT('Ctrl Pts',(3.19327823699994,2.2,-2.40641461800001));
#353079=CARTESIAN_POINT('Ctrl Pts',(3.19308056199994,12.2,-2.40625011400001));
#353080=CARTESIAN_POINT('Ctrl Pts',(3.19308056199994,5.2,-2.40625011400001));
#353081=CARTESIAN_POINT('Ctrl Pts',(3.19308056199994,2.2,-2.40625011400001));
#353082=CARTESIAN_POINT('Ctrl Pts',(3.19288798699994,12.2,-2.40609028800002));
#353083=CARTESIAN_POINT('Ctrl Pts',(3.19288798699994,5.2,-2.40609028800002));
#353084=CARTESIAN_POINT('Ctrl Pts',(3.19288798699994,2.2,-2.40609028800002));
#353085=CARTESIAN_POINT('Ctrl Pts',(3.19270053199994,12.2,-2.40593513400002));
#353086=CARTESIAN_POINT('Ctrl Pts',(3.19270053199994,5.2,-2.40593513400002));
#353087=CARTESIAN_POINT('Ctrl Pts',(3.19270053199994,2.2,-2.40593513400002));
#353088=CARTESIAN_POINT('Ctrl Pts',(3.19251822399994,12.2,-2.40578464900001));
#353089=CARTESIAN_POINT('Ctrl Pts',(3.19251822399994,5.2,-2.40578464900001));
#353090=CARTESIAN_POINT('Ctrl Pts',(3.19251822399994,2.2,-2.40578464900001));
#353091=CARTESIAN_POINT('Ctrl Pts',(3.19234108499994,12.2,-2.40563882900001));
#353092=CARTESIAN_POINT('Ctrl Pts',(3.19234108499994,5.2,-2.40563882900001));
#353093=CARTESIAN_POINT('Ctrl Pts',(3.19234108499994,2.2,-2.40563882900001));
#353094=CARTESIAN_POINT('Ctrl Pts',(3.19216913799994,12.2,-2.40549766900001));
#353095=CARTESIAN_POINT('Ctrl Pts',(3.19216913799994,5.2,-2.40549766900001));
#353096=CARTESIAN_POINT('Ctrl Pts',(3.19216913799994,2.2,-2.40549766900001));
#353097=CARTESIAN_POINT('Ctrl Pts',(3.19200240899994,12.2,-2.40536116600001));
#353098=CARTESIAN_POINT('Ctrl Pts',(3.19200240899994,5.2,-2.40536116600001));
#353099=CARTESIAN_POINT('Ctrl Pts',(3.19200240899994,2.2,-2.40536116600001));
#353100=CARTESIAN_POINT('Ctrl Pts',(3.19184092099994,12.2,-2.40522931500001));
#353101=CARTESIAN_POINT('Ctrl Pts',(3.19184092099994,5.2,-2.40522931500001));
#353102=CARTESIAN_POINT('Ctrl Pts',(3.19184092099994,2.2,-2.40522931500001));
#353103=CARTESIAN_POINT('Ctrl Pts',(3.19168469799994,12.2,-2.40510211000001));
#353104=CARTESIAN_POINT('Ctrl Pts',(3.19168469799994,5.2,-2.40510211000001));
#353105=CARTESIAN_POINT('Ctrl Pts',(3.19168469799994,2.2,-2.40510211000001));
#353106=CARTESIAN_POINT('Ctrl Pts',(3.19153376499994,12.2,-2.40497954800002));
#353107=CARTESIAN_POINT('Ctrl Pts',(3.19153376499994,5.2,-2.40497954800002));
#353108=CARTESIAN_POINT('Ctrl Pts',(3.19153376499994,2.2,-2.40497954800002));
#353109=CARTESIAN_POINT('Ctrl Pts',(3.19138814499994,12.2,-2.40486162600002));
#353110=CARTESIAN_POINT('Ctrl Pts',(3.19138814499994,5.2,-2.40486162600002));
#353111=CARTESIAN_POINT('Ctrl Pts',(3.19138814499994,2.2,-2.40486162600002));
#353112=CARTESIAN_POINT('Ctrl Pts',(3.19124786299994,12.2,-2.40474833800001));
#353113=CARTESIAN_POINT('Ctrl Pts',(3.19124786299994,5.2,-2.40474833800001));
#353114=CARTESIAN_POINT('Ctrl Pts',(3.19124786299994,2.2,-2.40474833800001));
#353115=CARTESIAN_POINT('Ctrl Pts',(3.19111294299995,12.2,-2.40463967800002));
#353116=CARTESIAN_POINT('Ctrl Pts',(3.19111294299995,5.2,-2.40463967800002));
#353117=CARTESIAN_POINT('Ctrl Pts',(3.19111294299995,2.2,-2.40463967800002));
#353118=CARTESIAN_POINT('Ctrl Pts',(3.19098340799994,12.2,-2.40453564500001));
#353119=CARTESIAN_POINT('Ctrl Pts',(3.19098340799994,5.2,-2.40453564500001));
#353120=CARTESIAN_POINT('Ctrl Pts',(3.19098340799994,2.2,-2.40453564500001));
#353121=CARTESIAN_POINT('Ctrl Pts',(3.19085928299994,12.2,-2.40443623200001));
#353122=CARTESIAN_POINT('Ctrl Pts',(3.19085928299994,5.2,-2.40443623200001));
#353123=CARTESIAN_POINT('Ctrl Pts',(3.19085928299994,2.2,-2.40443623200001));
#353124=CARTESIAN_POINT('Ctrl Pts',(3.19074059299994,12.2,-2.40434143500002));
#353125=CARTESIAN_POINT('Ctrl Pts',(3.19074059299994,5.2,-2.40434143500002));
#353126=CARTESIAN_POINT('Ctrl Pts',(3.19074059299994,2.2,-2.40434143500002));
#353127=CARTESIAN_POINT('Ctrl Pts',(3.19062736399994,12.2,-2.40425124900002));
#353128=CARTESIAN_POINT('Ctrl Pts',(3.19062736399994,5.2,-2.40425124900002));
#353129=CARTESIAN_POINT('Ctrl Pts',(3.19062736399994,2.2,-2.40425124900002));
#353130=CARTESIAN_POINT('Ctrl Pts',(3.19051962099994,12.2,-2.40416566900001));
#353131=CARTESIAN_POINT('Ctrl Pts',(3.19051962099994,5.2,-2.40416566900001));
#353132=CARTESIAN_POINT('Ctrl Pts',(3.19051962099994,2.2,-2.40416566900001));
#353133=CARTESIAN_POINT('Ctrl Pts',(3.19041739199994,12.2,-2.40408469100001));
#353134=CARTESIAN_POINT('Ctrl Pts',(3.19041739199994,5.2,-2.40408469100001));
#353135=CARTESIAN_POINT('Ctrl Pts',(3.19041739199994,2.2,-2.40408469100001));
#353136=CARTESIAN_POINT('Ctrl Pts',(3.19032069899994,12.2,-2.40400830800001));
#353137=CARTESIAN_POINT('Ctrl Pts',(3.19032069899994,5.2,-2.40400830800001));
#353138=CARTESIAN_POINT('Ctrl Pts',(3.19032069899994,2.2,-2.40400830800001));
#353139=CARTESIAN_POINT('Ctrl Pts',(3.19022956499994,12.2,-2.40393651800002));
#353140=CARTESIAN_POINT('Ctrl Pts',(3.19022956499994,5.2,-2.40393651800002));
#353141=CARTESIAN_POINT('Ctrl Pts',(3.19022956499994,2.2,-2.40393651800002));
#353142=CARTESIAN_POINT('Ctrl Pts',(3.19014401299994,12.2,-2.40386931500002));
#353143=CARTESIAN_POINT('Ctrl Pts',(3.19014401299994,5.2,-2.40386931500002));
#353144=CARTESIAN_POINT('Ctrl Pts',(3.19014401299994,2.2,-2.40386931500002));
#353145=CARTESIAN_POINT('Ctrl Pts',(3.19006406599994,12.2,-2.40380669500002));
#353146=CARTESIAN_POINT('Ctrl Pts',(3.19006406599994,5.2,-2.40380669500002));
#353147=CARTESIAN_POINT('Ctrl Pts',(3.19006406599994,2.2,-2.40380669500002));
#353148=CARTESIAN_POINT('Ctrl Pts',(3.18998974899994,12.2,-2.40374865400002));
#353149=CARTESIAN_POINT('Ctrl Pts',(3.18998974899994,5.2,-2.40374865400002));
#353150=CARTESIAN_POINT('Ctrl Pts',(3.18998974899994,2.2,-2.40374865400002));
#353151=CARTESIAN_POINT('Ctrl Pts',(3.18992109099994,12.2,-2.40369518600001));
#353152=CARTESIAN_POINT('Ctrl Pts',(3.18992109099994,5.2,-2.40369518600001));
#353153=CARTESIAN_POINT('Ctrl Pts',(3.18992109099994,2.2,-2.40369518600001));
#353154=CARTESIAN_POINT('Ctrl Pts',(3.18985812499994,12.2,-2.40364628200001));
#353155=CARTESIAN_POINT('Ctrl Pts',(3.18985812499994,5.2,-2.40364628200001));
#353156=CARTESIAN_POINT('Ctrl Pts',(3.18985812499994,2.2,-2.40364628200001));
#353157=CARTESIAN_POINT('Ctrl Pts',(3.18980088399994,12.2,-2.40360193900001));
#353158=CARTESIAN_POINT('Ctrl Pts',(3.18980088399994,5.2,-2.40360193900001));
#353159=CARTESIAN_POINT('Ctrl Pts',(3.18980088399994,2.2,-2.40360193900001));
#353160=CARTESIAN_POINT('Ctrl Pts',(3.18974939399994,12.2,-2.40356214900002));
#353161=CARTESIAN_POINT('Ctrl Pts',(3.18974939399994,5.2,-2.40356214900002));
#353162=CARTESIAN_POINT('Ctrl Pts',(3.18974939399994,2.2,-2.40356214900002));
#353163=CARTESIAN_POINT('Ctrl Pts',(3.18970367699994,12.2,-2.40352690800002));
#353164=CARTESIAN_POINT('Ctrl Pts',(3.18970367699994,5.2,-2.40352690800002));
#353165=CARTESIAN_POINT('Ctrl Pts',(3.18970367699994,2.2,-2.40352690800002));
#353166=CARTESIAN_POINT('Ctrl Pts',(3.18965947128237,12.2,-2.40349292812735));
#353167=CARTESIAN_POINT('Ctrl Pts',(3.18965947128237,5.2,-2.40349292812735));
#353168=CARTESIAN_POINT('Ctrl Pts',(3.18965947128237,2.2,-2.40349292812735));
#353169=CARTESIAN_POINT('Ctrl Pts',(3.18962920612091,12.2,-2.40346976281444));
#353170=CARTESIAN_POINT('Ctrl Pts',(3.18962920612091,5.2,-2.40346976281444));
#353171=CARTESIAN_POINT('Ctrl Pts',(3.18962920612091,2.2,-2.40346976281444));
#353172=CARTESIAN_POINT('Ctrl Pts',(3.18960923616151,12.2,-2.40345454411699));
#353173=CARTESIAN_POINT('Ctrl Pts',(3.18960923616151,5.2,-2.40345454411699));
#353174=CARTESIAN_POINT('Ctrl Pts',(3.18960923616151,2.2,-2.40345454411699));
#353175=CARTESIAN_POINT('Ctrl Pts',(3.18959677471721,12.2,-2.40344508870311));
#353176=CARTESIAN_POINT('Ctrl Pts',(3.18959677471721,5.2,-2.40344508870311));
#353177=CARTESIAN_POINT('Ctrl Pts',(3.18959677471721,2.2,-2.40344508870311));
#353178=CARTESIAN_POINT('Ctrl Pts',(3.18958908299994,12.2,-2.40343925200001));
#353179=CARTESIAN_POINT('Ctrl Pts',(3.18958908299994,5.2,-2.40343925200001));
#353180=CARTESIAN_POINT('Ctrl Pts',(3.18958908299994,2.2,-2.40343925200001));
#353181=CARTESIAN_POINT('',(3.57864508499994,12.2,-3.12342750100001));
#353182=CARTESIAN_POINT('Origin',(-5.66300478732629E-14,15.2,-1.77635683940025E-14));
#353183=CARTESIAN_POINT('',(3.34820124399994,12.2,-3.36928010500001));
#353184=CARTESIAN_POINT('Ctrl Pts',(2.60456075099994,12.2,-3.02756096900001));
#353185=CARTESIAN_POINT('Ctrl Pts',(2.60456075099994,5.2,-3.02756096900001));
#353186=CARTESIAN_POINT('Ctrl Pts',(2.60456075099994,2.2,-3.02756096900001));
#353187=CARTESIAN_POINT('Ctrl Pts',(2.60456523372611,12.2,-3.02756613868415));
#353188=CARTESIAN_POINT('Ctrl Pts',(2.60456523372611,5.2,-3.02756613868415));
#353189=CARTESIAN_POINT('Ctrl Pts',(2.60456523372611,2.2,-3.02756613868415));
#353190=CARTESIAN_POINT('Ctrl Pts',(2.60457390279746,12.2,-3.02757613848311));
#353191=CARTESIAN_POINT('Ctrl Pts',(2.60457390279746,5.2,-3.02757613848311));
#353192=CARTESIAN_POINT('Ctrl Pts',(2.60457390279746,2.2,-3.02757613848311));
#353193=CARTESIAN_POINT('Ctrl Pts',(2.60458675887381,12.2,-3.02759096800462));
#353194=CARTESIAN_POINT('Ctrl Pts',(2.60458675887381,5.2,-3.02759096800462));
#353195=CARTESIAN_POINT('Ctrl Pts',(2.60458675887381,2.2,-3.02759096800462));
#353196=CARTESIAN_POINT('Ctrl Pts',(2.60460382305029,12.2,-3.0276106272463));
#353197=CARTESIAN_POINT('Ctrl Pts',(2.60460382305029,5.19999999999999,-3.0276106272463));
#353198=CARTESIAN_POINT('Ctrl Pts',(2.60460382305029,2.2,-3.0276106272463));
#353199=CARTESIAN_POINT('Ctrl Pts',(2.60463362599994,12.2,-3.02764471800002));
#353200=CARTESIAN_POINT('Ctrl Pts',(2.60463362599994,5.2,-3.02764471800002));
#353201=CARTESIAN_POINT('Ctrl Pts',(2.60463362599994,2.2,-3.02764471800002));
#353202=CARTESIAN_POINT('Ctrl Pts',(2.60466683599994,12.2,-3.02768258200001));
#353203=CARTESIAN_POINT('Ctrl Pts',(2.60466683599994,5.2,-3.02768258200001));
#353204=CARTESIAN_POINT('Ctrl Pts',(2.60466683599994,2.2,-3.02768258200001));
#353205=CARTESIAN_POINT('Ctrl Pts',(2.60470495699994,12.2,-3.02772592500002));
#353206=CARTESIAN_POINT('Ctrl Pts',(2.60470495699994,5.2,-3.02772592500002));
#353207=CARTESIAN_POINT('Ctrl Pts',(2.60470495699994,2.2,-3.02772592500002));
#353208=CARTESIAN_POINT('Ctrl Pts',(2.60474799299995,12.2,-3.02777473600001));
#353209=CARTESIAN_POINT('Ctrl Pts',(2.60474799299995,5.2,-3.02777473600001));
#353210=CARTESIAN_POINT('Ctrl Pts',(2.60474799299995,2.2,-3.02777473600001));
#353211=CARTESIAN_POINT('Ctrl Pts',(2.60479594299994,12.2,-3.02782899200002));
#353212=CARTESIAN_POINT('Ctrl Pts',(2.60479594299994,5.2,-3.02782899200002));
#353213=CARTESIAN_POINT('Ctrl Pts',(2.60479594299994,2.2,-3.02782899200002));
#353214=CARTESIAN_POINT('Ctrl Pts',(2.60484881399994,12.2,-3.02788866500002));
#353215=CARTESIAN_POINT('Ctrl Pts',(2.60484881399994,5.2,-3.02788866500002));
#353216=CARTESIAN_POINT('Ctrl Pts',(2.60484881399994,2.2,-3.02788866500002));
#353217=CARTESIAN_POINT('Ctrl Pts',(2.60490660899994,12.2,-3.02795372300002));
#353218=CARTESIAN_POINT('Ctrl Pts',(2.60490660899994,5.2,-3.02795372300002));
#353219=CARTESIAN_POINT('Ctrl Pts',(2.60490660899994,2.2,-3.02795372300002));
#353220=CARTESIAN_POINT('Ctrl Pts',(2.60496933299994,12.2,-3.02802413400002));
#353221=CARTESIAN_POINT('Ctrl Pts',(2.60496933299994,5.2,-3.02802413400002));
#353222=CARTESIAN_POINT('Ctrl Pts',(2.60496933299994,2.2,-3.02802413400002));
#353223=CARTESIAN_POINT('Ctrl Pts',(2.60503698899994,12.2,-3.02809986600002));
#353224=CARTESIAN_POINT('Ctrl Pts',(2.60503698899994,5.2,-3.02809986600002));
#353225=CARTESIAN_POINT('Ctrl Pts',(2.60503698899994,2.2,-3.02809986600002));
#353226=CARTESIAN_POINT('Ctrl Pts',(2.60510957999994,12.2,-3.02818089600001));
#353227=CARTESIAN_POINT('Ctrl Pts',(2.60510957999994,5.2,-3.02818089600001));
#353228=CARTESIAN_POINT('Ctrl Pts',(2.60510957999994,2.2,-3.02818089600001));
#353229=CARTESIAN_POINT('Ctrl Pts',(2.60518711099994,12.2,-3.02826719900001));
#353230=CARTESIAN_POINT('Ctrl Pts',(2.60518711099994,5.2,-3.02826719900001));
#353231=CARTESIAN_POINT('Ctrl Pts',(2.60518711099994,2.2,-3.02826719900001));
#353232=CARTESIAN_POINT('Ctrl Pts',(2.60526958299995,12.2,-3.02835875300001));
#353233=CARTESIAN_POINT('Ctrl Pts',(2.60526958299995,5.2,-3.02835875300001));
#353234=CARTESIAN_POINT('Ctrl Pts',(2.60526958299995,2.2,-3.02835875300001));
#353235=CARTESIAN_POINT('Ctrl Pts',(2.60535699999994,12.2,-3.02845553400001));
#353236=CARTESIAN_POINT('Ctrl Pts',(2.60535699999994,5.2,-3.02845553400001));
#353237=CARTESIAN_POINT('Ctrl Pts',(2.60535699999994,2.2,-3.02845553400001));
#353238=CARTESIAN_POINT('Ctrl Pts',(2.60544936499994,12.2,-3.02855752000001));
#353239=CARTESIAN_POINT('Ctrl Pts',(2.60544936499994,5.2,-3.02855752000001));
#353240=CARTESIAN_POINT('Ctrl Pts',(2.60544936499994,2.2,-3.02855752000001));
#353241=CARTESIAN_POINT('Ctrl Pts',(2.60554668099994,12.2,-3.02866468300001));
#353242=CARTESIAN_POINT('Ctrl Pts',(2.60554668099994,5.2,-3.02866468300001));
#353243=CARTESIAN_POINT('Ctrl Pts',(2.60554668099994,2.2,-3.02866468300001));
#353244=CARTESIAN_POINT('Ctrl Pts',(2.60564895099994,12.2,-3.02877699800002));
#353245=CARTESIAN_POINT('Ctrl Pts',(2.60564895099994,5.2,-3.02877699800002));
#353246=CARTESIAN_POINT('Ctrl Pts',(2.60564895099994,2.2,-3.02877699800002));
#353247=CARTESIAN_POINT('Ctrl Pts',(2.60575617899995,12.2,-3.02889443700002));
#353248=CARTESIAN_POINT('Ctrl Pts',(2.60575617899995,5.2,-3.02889443700002));
#353249=CARTESIAN_POINT('Ctrl Pts',(2.60575617899995,2.2,-3.02889443700002));
#353250=CARTESIAN_POINT('Ctrl Pts',(2.60586836799995,12.2,-3.02901697700001));
#353251=CARTESIAN_POINT('Ctrl Pts',(2.60586836799995,5.2,-3.02901697700001));
#353252=CARTESIAN_POINT('Ctrl Pts',(2.60586836799995,2.2,-3.02901697700001));
#353253=CARTESIAN_POINT('Ctrl Pts',(2.60598551899994,12.2,-3.02914459200001));
#353254=CARTESIAN_POINT('Ctrl Pts',(2.60598551899994,5.2,-3.02914459200001));
#353255=CARTESIAN_POINT('Ctrl Pts',(2.60598551899994,2.2,-3.02914459200001));
#353256=CARTESIAN_POINT('Ctrl Pts',(2.60610763899995,12.2,-3.02927725900001));
#353257=CARTESIAN_POINT('Ctrl Pts',(2.60610763899995,5.2,-3.02927725900001));
#353258=CARTESIAN_POINT('Ctrl Pts',(2.60610763899995,2.2,-3.02927725900001));
#353259=CARTESIAN_POINT('Ctrl Pts',(2.60623472699994,12.2,-3.02941495200002));
#353260=CARTESIAN_POINT('Ctrl Pts',(2.60623472699994,5.2,-3.02941495200002));
#353261=CARTESIAN_POINT('Ctrl Pts',(2.60623472699994,2.2,-3.02941495200002));
#353262=CARTESIAN_POINT('Ctrl Pts',(2.60636678699994,12.2,-3.02955764800001));
#353263=CARTESIAN_POINT('Ctrl Pts',(2.60636678699994,5.2,-3.02955764800001));
#353264=CARTESIAN_POINT('Ctrl Pts',(2.60636678699994,2.2,-3.02955764800001));
#353265=CARTESIAN_POINT('Ctrl Pts',(2.60650382299994,12.2,-3.02970532200002));
#353266=CARTESIAN_POINT('Ctrl Pts',(2.60650382299994,5.2,-3.02970532200002));
#353267=CARTESIAN_POINT('Ctrl Pts',(2.60650382299994,2.2,-3.02970532200002));
#353268=CARTESIAN_POINT('Ctrl Pts',(2.60664583599994,12.2,-3.02985795000001));
#353269=CARTESIAN_POINT('Ctrl Pts',(2.60664583599994,5.2,-3.02985795000001));
#353270=CARTESIAN_POINT('Ctrl Pts',(2.60664583599994,2.2,-3.02985795000001));
#353271=CARTESIAN_POINT('Ctrl Pts',(2.60679283099994,12.2,-3.03001550900001));
#353272=CARTESIAN_POINT('Ctrl Pts',(2.60679283099994,5.2,-3.03001550900001));
#353273=CARTESIAN_POINT('Ctrl Pts',(2.60679283099994,2.2,-3.03001550900001));
#353274=CARTESIAN_POINT('Ctrl Pts',(2.60694480999994,12.2,-3.03017797100001));
#353275=CARTESIAN_POINT('Ctrl Pts',(2.60694480999994,5.2,-3.03017797100001));
#353276=CARTESIAN_POINT('Ctrl Pts',(2.60694480999994,2.2,-3.03017797100001));
#353277=CARTESIAN_POINT('Ctrl Pts',(2.60710177399994,12.2,-3.03034531500002));
#353278=CARTESIAN_POINT('Ctrl Pts',(2.60710177399994,5.2,-3.03034531500002));
#353279=CARTESIAN_POINT('Ctrl Pts',(2.60710177399994,2.2,-3.03034531500002));
#353280=CARTESIAN_POINT('Ctrl Pts',(2.60726372699994,12.2,-3.03051751600002));
#353281=CARTESIAN_POINT('Ctrl Pts',(2.60726372699994,5.2,-3.03051751600002));
#353282=CARTESIAN_POINT('Ctrl Pts',(2.60726372699994,2.2,-3.03051751600002));
#353283=CARTESIAN_POINT('Ctrl Pts',(2.60743067299994,12.2,-3.03069454900001));
#353284=CARTESIAN_POINT('Ctrl Pts',(2.60743067299994,5.2,-3.03069454900001));
#353285=CARTESIAN_POINT('Ctrl Pts',(2.60743067299994,2.2,-3.03069454900001));
#353286=CARTESIAN_POINT('Ctrl Pts',(2.60760261299994,12.2,-3.03087639200001));
#353287=CARTESIAN_POINT('Ctrl Pts',(2.60760261299994,5.2,-3.03087639200001));
#353288=CARTESIAN_POINT('Ctrl Pts',(2.60760261299994,2.2,-3.03087639200001));
#353289=CARTESIAN_POINT('Ctrl Pts',(2.60777954899994,12.2,-3.03106302100002));
#353290=CARTESIAN_POINT('Ctrl Pts',(2.60777954899994,5.2,-3.03106302100002));
#353291=CARTESIAN_POINT('Ctrl Pts',(2.60777954899994,2.2,-3.03106302100002));
#353292=CARTESIAN_POINT('Ctrl Pts',(2.60796148499994,12.2,-3.03125441200002));
#353293=CARTESIAN_POINT('Ctrl Pts',(2.60796148499994,5.2,-3.03125441200002));
#353294=CARTESIAN_POINT('Ctrl Pts',(2.60796148499994,2.2,-3.03125441200002));
#353295=CARTESIAN_POINT('Ctrl Pts',(2.60814842099995,12.2,-3.03145054100002));
#353296=CARTESIAN_POINT('Ctrl Pts',(2.60814842099995,5.2,-3.03145054100002));
#353297=CARTESIAN_POINT('Ctrl Pts',(2.60814842099995,2.2,-3.03145054100002));
#353298=CARTESIAN_POINT('Ctrl Pts',(2.60834036299994,12.2,-3.03165138400002));
#353299=CARTESIAN_POINT('Ctrl Pts',(2.60834036299994,5.2,-3.03165138400002));
#353300=CARTESIAN_POINT('Ctrl Pts',(2.60834036299994,2.2,-3.03165138400002));
#353301=CARTESIAN_POINT('Ctrl Pts',(2.60853731199994,12.2,-3.03185691800001));
#353302=CARTESIAN_POINT('Ctrl Pts',(2.60853731199994,5.2,-3.03185691800001));
#353303=CARTESIAN_POINT('Ctrl Pts',(2.60853731199994,2.2,-3.03185691800001));
#353304=CARTESIAN_POINT('Ctrl Pts',(2.60873926899994,12.2,-3.03206712000001));
#353305=CARTESIAN_POINT('Ctrl Pts',(2.60873926899994,5.2,-3.03206712000001));
#353306=CARTESIAN_POINT('Ctrl Pts',(2.60873926899994,2.2,-3.03206712000001));
#353307=CARTESIAN_POINT('Ctrl Pts',(2.60894623799994,12.2,-3.03228196800001));
#353308=CARTESIAN_POINT('Ctrl Pts',(2.60894623799994,5.2,-3.03228196800001));
#353309=CARTESIAN_POINT('Ctrl Pts',(2.60894623799994,2.2,-3.03228196800001));
#353310=CARTESIAN_POINT('Ctrl Pts',(2.60915822099994,12.2,-3.03250143600001));
#353311=CARTESIAN_POINT('Ctrl Pts',(2.60915822099994,5.2,-3.03250143600001));
#353312=CARTESIAN_POINT('Ctrl Pts',(2.60915822099994,2.2,-3.03250143600001));
#353313=CARTESIAN_POINT('Ctrl Pts',(2.60937522099994,12.2,-3.03272550100001));
#353314=CARTESIAN_POINT('Ctrl Pts',(2.60937522099994,5.2,-3.03272550100001));
#353315=CARTESIAN_POINT('Ctrl Pts',(2.60937522099994,2.2,-3.03272550100001));
#353316=CARTESIAN_POINT('Ctrl Pts',(2.60959723799994,12.2,-3.03295414300001));
#353317=CARTESIAN_POINT('Ctrl Pts',(2.60959723799994,5.2,-3.03295414300001));
#353318=CARTESIAN_POINT('Ctrl Pts',(2.60959723799994,2.2,-3.03295414300001));
#353319=CARTESIAN_POINT('Ctrl Pts',(2.60982427499994,12.2,-3.03318733600001));
#353320=CARTESIAN_POINT('Ctrl Pts',(2.60982427499994,5.2,-3.03318733600001));
#353321=CARTESIAN_POINT('Ctrl Pts',(2.60982427499994,2.2,-3.03318733600001));
#353322=CARTESIAN_POINT('Ctrl Pts',(2.61005633599994,12.2,-3.03342505900002));
#353323=CARTESIAN_POINT('Ctrl Pts',(2.61005633599994,5.2,-3.03342505900002));
#353324=CARTESIAN_POINT('Ctrl Pts',(2.61005633599994,2.2,-3.03342505900002));
#353325=CARTESIAN_POINT('Ctrl Pts',(2.61029342199994,12.2,-3.03366728700002));
#353326=CARTESIAN_POINT('Ctrl Pts',(2.61029342199994,5.2,-3.03366728700002));
#353327=CARTESIAN_POINT('Ctrl Pts',(2.61029342199994,2.2,-3.03366728700002));
#353328=CARTESIAN_POINT('Ctrl Pts',(2.61053553499994,12.2,-3.03391399900002));
#353329=CARTESIAN_POINT('Ctrl Pts',(2.61053553499994,5.2,-3.03391399900002));
#353330=CARTESIAN_POINT('Ctrl Pts',(2.61053553499994,2.2,-3.03391399900002));
#353331=CARTESIAN_POINT('Ctrl Pts',(2.61078267799994,12.2,-3.03416517100001));
#353332=CARTESIAN_POINT('Ctrl Pts',(2.61078267799994,5.2,-3.03416517100001));
#353333=CARTESIAN_POINT('Ctrl Pts',(2.61078267799994,2.2,-3.03416517100001));
#353334=CARTESIAN_POINT('Ctrl Pts',(2.61103485099994,12.2,-3.03442078200002));
#353335=CARTESIAN_POINT('Ctrl Pts',(2.61103485099994,5.2,-3.03442078200002));
#353336=CARTESIAN_POINT('Ctrl Pts',(2.61103485099994,2.2,-3.03442078200002));
#353337=CARTESIAN_POINT('Ctrl Pts',(2.61129205699994,12.2,-3.03468080800001));
#353338=CARTESIAN_POINT('Ctrl Pts',(2.61129205699994,5.2,-3.03468080800001));
#353339=CARTESIAN_POINT('Ctrl Pts',(2.61129205699994,2.2,-3.03468080800001));
#353340=CARTESIAN_POINT('Ctrl Pts',(2.61155429899994,12.2,-3.03494522800001));
#353341=CARTESIAN_POINT('Ctrl Pts',(2.61155429899994,5.2,-3.03494522800001));
#353342=CARTESIAN_POINT('Ctrl Pts',(2.61155429899994,2.2,-3.03494522800001));
#353343=CARTESIAN_POINT('Ctrl Pts',(2.61182157899994,12.2,-3.03521401800001));
#353344=CARTESIAN_POINT('Ctrl Pts',(2.61182157899994,5.2,-3.03521401800001));
#353345=CARTESIAN_POINT('Ctrl Pts',(2.61182157899994,2.2,-3.03521401800001));
#353346=CARTESIAN_POINT('Ctrl Pts',(2.61209389699995,12.2,-3.03548715600002));
#353347=CARTESIAN_POINT('Ctrl Pts',(2.61209389699995,5.2,-3.03548715600002));
#353348=CARTESIAN_POINT('Ctrl Pts',(2.61209389699995,2.2,-3.03548715600002));
#353349=CARTESIAN_POINT('Ctrl Pts',(2.61237125599994,12.2,-3.03576462000001));
#353350=CARTESIAN_POINT('Ctrl Pts',(2.61237125599994,5.2,-3.03576462000001));
#353351=CARTESIAN_POINT('Ctrl Pts',(2.61237125599994,2.2,-3.03576462000001));
#353352=CARTESIAN_POINT('Ctrl Pts',(2.61265365899995,12.2,-3.03604638900001));
#353353=CARTESIAN_POINT('Ctrl Pts',(2.61265365899995,5.2,-3.03604638900001));
#353354=CARTESIAN_POINT('Ctrl Pts',(2.61265365899995,2.2,-3.03604638900001));
#353355=CARTESIAN_POINT('Ctrl Pts',(2.61294110599994,12.2,-3.03633243900002));
#353356=CARTESIAN_POINT('Ctrl Pts',(2.61294110599994,5.2,-3.03633243900002));
#353357=CARTESIAN_POINT('Ctrl Pts',(2.61294110599994,2.2,-3.03633243900002));
#353358=CARTESIAN_POINT('Ctrl Pts',(2.61323359999994,12.2,-3.03662274800002));
#353359=CARTESIAN_POINT('Ctrl Pts',(2.61323359999994,5.2,-3.03662274800002));
#353360=CARTESIAN_POINT('Ctrl Pts',(2.61323359999994,2.2,-3.03662274800002));
#353361=CARTESIAN_POINT('Ctrl Pts',(2.61353114199995,12.2,-3.03691729500001));
#353362=CARTESIAN_POINT('Ctrl Pts',(2.61353114199995,5.2,-3.03691729500001));
#353363=CARTESIAN_POINT('Ctrl Pts',(2.61353114199995,2.2,-3.03691729500001));
#353364=CARTESIAN_POINT('Ctrl Pts',(2.61383373399994,12.2,-3.03721605800002));
#353365=CARTESIAN_POINT('Ctrl Pts',(2.61383373399994,5.2,-3.03721605800002));
#353366=CARTESIAN_POINT('Ctrl Pts',(2.61383373399994,2.2,-3.03721605800002));
#353367=CARTESIAN_POINT('Ctrl Pts',(2.61414137899994,12.2,-3.03751901400001));
#353368=CARTESIAN_POINT('Ctrl Pts',(2.61414137899994,5.2,-3.03751901400001));
#353369=CARTESIAN_POINT('Ctrl Pts',(2.61414137899994,2.2,-3.03751901400001));
#353370=CARTESIAN_POINT('Ctrl Pts',(2.61445407699994,12.2,-3.03782614300002));
#353371=CARTESIAN_POINT('Ctrl Pts',(2.61445407699994,5.2,-3.03782614300002));
#353372=CARTESIAN_POINT('Ctrl Pts',(2.61445407699994,2.2,-3.03782614300002));
#353373=CARTESIAN_POINT('Ctrl Pts',(2.61477182999994,12.2,-3.03813742200001));
#353374=CARTESIAN_POINT('Ctrl Pts',(2.61477182999994,5.2,-3.03813742200001));
#353375=CARTESIAN_POINT('Ctrl Pts',(2.61477182999994,2.2,-3.03813742200001));
#353376=CARTESIAN_POINT('Ctrl Pts',(2.61509463899994,12.2,-3.03845282900001));
#353377=CARTESIAN_POINT('Ctrl Pts',(2.61509463899994,5.2,-3.03845282900001));
#353378=CARTESIAN_POINT('Ctrl Pts',(2.61509463899994,2.2,-3.03845282900001));
#353379=CARTESIAN_POINT('Ctrl Pts',(2.61542250699994,12.2,-3.03877234400002));
#353380=CARTESIAN_POINT('Ctrl Pts',(2.61542250699994,5.2,-3.03877234400002));
#353381=CARTESIAN_POINT('Ctrl Pts',(2.61542250699994,2.2,-3.03877234400002));
#353382=CARTESIAN_POINT('Ctrl Pts',(2.61575543499994,12.2,-3.03909594400002));
#353383=CARTESIAN_POINT('Ctrl Pts',(2.61575543499994,5.2,-3.03909594400002));
#353384=CARTESIAN_POINT('Ctrl Pts',(2.61575543499994,2.2,-3.03909594400002));
#353385=CARTESIAN_POINT('Ctrl Pts',(2.61609342599994,12.2,-3.03942360900002));
#353386=CARTESIAN_POINT('Ctrl Pts',(2.61609342599994,5.2,-3.03942360900002));
#353387=CARTESIAN_POINT('Ctrl Pts',(2.61609342599994,2.2,-3.03942360900002));
#353388=CARTESIAN_POINT('Ctrl Pts',(2.61643647899994,12.2,-3.03975531600001));
#353389=CARTESIAN_POINT('Ctrl Pts',(2.61643647899994,5.2,-3.03975531600001));
#353390=CARTESIAN_POINT('Ctrl Pts',(2.61643647899994,2.2,-3.03975531600001));
#353391=CARTESIAN_POINT('Ctrl Pts',(2.61678459599994,12.2,-3.04009104500001));
#353392=CARTESIAN_POINT('Ctrl Pts',(2.61678459599994,5.2,-3.04009104500001));
#353393=CARTESIAN_POINT('Ctrl Pts',(2.61678459599994,2.2,-3.04009104500001));
#353394=CARTESIAN_POINT('Ctrl Pts',(2.61713777799994,12.2,-3.04043077300001));
#353395=CARTESIAN_POINT('Ctrl Pts',(2.61713777799994,5.2,-3.04043077300001));
#353396=CARTESIAN_POINT('Ctrl Pts',(2.61713777799994,2.2,-3.04043077300001));
#353397=CARTESIAN_POINT('Ctrl Pts',(2.61749602899994,12.2,-3.04077448100001));
#353398=CARTESIAN_POINT('Ctrl Pts',(2.61749602899994,5.2,-3.04077448100001));
#353399=CARTESIAN_POINT('Ctrl Pts',(2.61749602899994,2.2,-3.04077448100001));
#353400=CARTESIAN_POINT('Ctrl Pts',(2.61785934799994,12.2,-3.04112214700002));
#353401=CARTESIAN_POINT('Ctrl Pts',(2.61785934799994,5.2,-3.04112214700002));
#353402=CARTESIAN_POINT('Ctrl Pts',(2.61785934799994,2.2,-3.04112214700002));
#353403=CARTESIAN_POINT('Ctrl Pts',(2.61822773799994,12.2,-3.04147374900001));
#353404=CARTESIAN_POINT('Ctrl Pts',(2.61822773799994,5.2,-3.04147374900001));
#353405=CARTESIAN_POINT('Ctrl Pts',(2.61822773799994,2.2,-3.04147374900001));
#353406=CARTESIAN_POINT('Ctrl Pts',(2.61860119799994,12.2,-3.04182926700001));
#353407=CARTESIAN_POINT('Ctrl Pts',(2.61860119799994,5.2,-3.04182926700001));
#353408=CARTESIAN_POINT('Ctrl Pts',(2.61860119799994,2.2,-3.04182926700001));
#353409=CARTESIAN_POINT('Ctrl Pts',(2.61897973099994,12.2,-3.04218868100001));
#353410=CARTESIAN_POINT('Ctrl Pts',(2.61897973099994,5.2,-3.04218868100001));
#353411=CARTESIAN_POINT('Ctrl Pts',(2.61897973099994,2.2,-3.04218868100001));
#353412=CARTESIAN_POINT('Ctrl Pts',(2.61936333899994,12.2,-3.04255196700002));
#353413=CARTESIAN_POINT('Ctrl Pts',(2.61936333899994,5.2,-3.04255196700002));
#353414=CARTESIAN_POINT('Ctrl Pts',(2.61936333899994,2.2,-3.04255196700002));
#353415=CARTESIAN_POINT('Ctrl Pts',(2.61975202199995,12.2,-3.04291910800002));
#353416=CARTESIAN_POINT('Ctrl Pts',(2.61975202199995,5.2,-3.04291910800002));
#353417=CARTESIAN_POINT('Ctrl Pts',(2.61975202199995,2.2,-3.04291910800002));
#353418=CARTESIAN_POINT('Ctrl Pts',(2.62014577999994,12.2,-3.04329008000002));
#353419=CARTESIAN_POINT('Ctrl Pts',(2.62014577999994,5.2,-3.04329008000002));
#353420=CARTESIAN_POINT('Ctrl Pts',(2.62014577999994,2.2,-3.04329008000002));
#353421=CARTESIAN_POINT('Ctrl Pts',(2.62054461699994,12.2,-3.04366486500002));
#353422=CARTESIAN_POINT('Ctrl Pts',(2.62054461699994,5.2,-3.04366486500002));
#353423=CARTESIAN_POINT('Ctrl Pts',(2.62054461699994,2.2,-3.04366486500002));
#353424=CARTESIAN_POINT('Ctrl Pts',(2.62094853299994,12.2,-3.04404344100002));
#353425=CARTESIAN_POINT('Ctrl Pts',(2.62094853299994,5.2,-3.04404344100002));
#353426=CARTESIAN_POINT('Ctrl Pts',(2.62094853299994,2.2,-3.04404344100002));
#353427=CARTESIAN_POINT('Ctrl Pts',(2.62135752799994,12.2,-3.04442578600002));
#353428=CARTESIAN_POINT('Ctrl Pts',(2.62135752799994,5.2,-3.04442578600002));
#353429=CARTESIAN_POINT('Ctrl Pts',(2.62135752799994,2.2,-3.04442578600002));
#353430=CARTESIAN_POINT('Ctrl Pts',(2.62177160499995,12.2,-3.04481188200001));
#353431=CARTESIAN_POINT('Ctrl Pts',(2.62177160499995,5.2,-3.04481188200001));
#353432=CARTESIAN_POINT('Ctrl Pts',(2.62177160499995,2.2,-3.04481188200001));
#353433=CARTESIAN_POINT('Ctrl Pts',(2.62219076399994,12.2,-3.04520170900001));
#353434=CARTESIAN_POINT('Ctrl Pts',(2.62219076399994,5.2,-3.04520170900001));
#353435=CARTESIAN_POINT('Ctrl Pts',(2.62219076399994,2.2,-3.04520170900001));
#353436=CARTESIAN_POINT('Ctrl Pts',(2.62261500499994,12.2,-3.04559524400001));
#353437=CARTESIAN_POINT('Ctrl Pts',(2.62261500499994,5.2,-3.04559524400001));
#353438=CARTESIAN_POINT('Ctrl Pts',(2.62261500499994,2.2,-3.04559524400001));
#353439=CARTESIAN_POINT('Ctrl Pts',(2.62304433199994,12.2,-3.04599246800001));
#353440=CARTESIAN_POINT('Ctrl Pts',(2.62304433199994,5.2,-3.04599246800001));
#353441=CARTESIAN_POINT('Ctrl Pts',(2.62304433199994,2.2,-3.04599246800001));
#353442=CARTESIAN_POINT('Ctrl Pts',(2.62347874199994,12.2,-3.04639336100001));
#353443=CARTESIAN_POINT('Ctrl Pts',(2.62347874199994,5.2,-3.04639336100001));
#353444=CARTESIAN_POINT('Ctrl Pts',(2.62347874199994,2.2,-3.04639336100001));
#353445=CARTESIAN_POINT('Ctrl Pts',(2.62391823999995,12.2,-3.04679790300002));
#353446=CARTESIAN_POINT('Ctrl Pts',(2.62391823999995,5.2,-3.04679790300002));
#353447=CARTESIAN_POINT('Ctrl Pts',(2.62391823999995,2.2,-3.04679790300002));
#353448=CARTESIAN_POINT('Ctrl Pts',(2.62436282399995,12.2,-3.04720607100001));
#353449=CARTESIAN_POINT('Ctrl Pts',(2.62436282399995,5.2,-3.04720607100001));
#353450=CARTESIAN_POINT('Ctrl Pts',(2.62436282399995,2.2,-3.04720607100001));
#353451=CARTESIAN_POINT('Ctrl Pts',(2.62481249599994,12.2,-3.04761785000002));
#353452=CARTESIAN_POINT('Ctrl Pts',(2.62481249599994,5.2,-3.04761785000002));
#353453=CARTESIAN_POINT('Ctrl Pts',(2.62481249599994,2.2,-3.04761785000002));
#353454=CARTESIAN_POINT('Ctrl Pts',(2.62526725699994,12.2,-3.04803321600001));
#353455=CARTESIAN_POINT('Ctrl Pts',(2.62526725699994,5.2,-3.04803321600001));
#353456=CARTESIAN_POINT('Ctrl Pts',(2.62526725699994,2.2,-3.04803321600001));
#353457=CARTESIAN_POINT('Ctrl Pts',(2.62572710899994,12.2,-3.04845215000002));
#353458=CARTESIAN_POINT('Ctrl Pts',(2.62572710899994,5.2,-3.04845215000002));
#353459=CARTESIAN_POINT('Ctrl Pts',(2.62572710899994,2.2,-3.04845215000002));
#353460=CARTESIAN_POINT('Ctrl Pts',(2.62619204999994,12.2,-3.04887463400001));
#353461=CARTESIAN_POINT('Ctrl Pts',(2.62619204999994,5.2,-3.04887463400001));
#353462=CARTESIAN_POINT('Ctrl Pts',(2.62619204999994,2.2,-3.04887463400001));
#353463=CARTESIAN_POINT('Ctrl Pts',(2.62666208299994,12.2,-3.04930064600001));
#353464=CARTESIAN_POINT('Ctrl Pts',(2.62666208299994,5.2,-3.04930064600001));
#353465=CARTESIAN_POINT('Ctrl Pts',(2.62666208299994,2.2,-3.04930064600001));
#353466=CARTESIAN_POINT('Ctrl Pts',(2.62713720799994,12.2,-3.04973016600002));
#353467=CARTESIAN_POINT('Ctrl Pts',(2.62713720799994,5.2,-3.04973016600002));
#353468=CARTESIAN_POINT('Ctrl Pts',(2.62713720799994,2.2,-3.04973016600002));
#353469=CARTESIAN_POINT('Ctrl Pts',(2.62761742699994,12.2,-3.05016317500002));
#353470=CARTESIAN_POINT('Ctrl Pts',(2.62761742699994,5.2,-3.05016317500002));
#353471=CARTESIAN_POINT('Ctrl Pts',(2.62761742699994,2.2,-3.05016317500002));
#353472=CARTESIAN_POINT('Ctrl Pts',(2.62810273799994,12.2,-3.05059965400002));
#353473=CARTESIAN_POINT('Ctrl Pts',(2.62810273799994,5.2,-3.05059965400002));
#353474=CARTESIAN_POINT('Ctrl Pts',(2.62810273799994,2.2,-3.05059965400002));
#353475=CARTESIAN_POINT('Ctrl Pts',(2.62859314499994,12.2,-3.05103958300001));
#353476=CARTESIAN_POINT('Ctrl Pts',(2.62859314499994,5.2,-3.05103958300001));
#353477=CARTESIAN_POINT('Ctrl Pts',(2.62859314499994,2.2,-3.05103958300001));
#353478=CARTESIAN_POINT('Ctrl Pts',(2.62908864599994,12.2,-3.05148294100002));
#353479=CARTESIAN_POINT('Ctrl Pts',(2.62908864599994,5.2,-3.05148294100002));
#353480=CARTESIAN_POINT('Ctrl Pts',(2.62908864599994,2.2,-3.05148294100002));
#353481=CARTESIAN_POINT('Ctrl Pts',(2.62958924299994,12.2,-3.05192971100002));
#353482=CARTESIAN_POINT('Ctrl Pts',(2.62958924299994,5.2,-3.05192971100002));
#353483=CARTESIAN_POINT('Ctrl Pts',(2.62958924299994,2.2,-3.05192971100002));
#353484=CARTESIAN_POINT('Ctrl Pts',(2.63009493599994,12.2,-3.05237987200002));
#353485=CARTESIAN_POINT('Ctrl Pts',(2.63009493599994,5.2,-3.05237987200002));
#353486=CARTESIAN_POINT('Ctrl Pts',(2.63009493599994,2.2,-3.05237987200002));
#353487=CARTESIAN_POINT('Ctrl Pts',(2.63060572599994,12.2,-3.05283340500001));
#353488=CARTESIAN_POINT('Ctrl Pts',(2.63060572599994,5.2,-3.05283340500001));
#353489=CARTESIAN_POINT('Ctrl Pts',(2.63060572599994,2.2,-3.05283340500001));
#353490=CARTESIAN_POINT('Ctrl Pts',(2.63112161299994,12.2,-3.05329029000001));
#353491=CARTESIAN_POINT('Ctrl Pts',(2.63112161299994,5.2,-3.05329029000001));
#353492=CARTESIAN_POINT('Ctrl Pts',(2.63112161299994,2.2,-3.05329029000001));
#353493=CARTESIAN_POINT('Ctrl Pts',(2.63164259999995,12.2,-3.05375050800002));
#353494=CARTESIAN_POINT('Ctrl Pts',(2.63164259999995,5.2,-3.05375050800002));
#353495=CARTESIAN_POINT('Ctrl Pts',(2.63164259999995,2.2,-3.05375050800002));
#353496=CARTESIAN_POINT('Ctrl Pts',(2.63216868399994,12.2,-3.05421404000001));
#353497=CARTESIAN_POINT('Ctrl Pts',(2.63216868399994,5.2,-3.05421404000001));
#353498=CARTESIAN_POINT('Ctrl Pts',(2.63216868399994,2.2,-3.05421404000001));
#353499=CARTESIAN_POINT('Ctrl Pts',(2.63269986699994,12.2,-3.05468086800001));
#353500=CARTESIAN_POINT('Ctrl Pts',(2.63269986699994,5.2,-3.05468086800001));
#353501=CARTESIAN_POINT('Ctrl Pts',(2.63269986699994,2.2,-3.05468086800001));
#353502=CARTESIAN_POINT('Ctrl Pts',(2.63323614999994,12.2,-3.05515097100002));
#353503=CARTESIAN_POINT('Ctrl Pts',(2.63323614999994,5.2,-3.05515097100002));
#353504=CARTESIAN_POINT('Ctrl Pts',(2.63323614999994,2.2,-3.05515097100002));
#353505=CARTESIAN_POINT('Ctrl Pts',(2.63377753299994,12.2,-3.05562433100001));
#353506=CARTESIAN_POINT('Ctrl Pts',(2.63377753299994,5.2,-3.05562433100001));
#353507=CARTESIAN_POINT('Ctrl Pts',(2.63377753299994,2.2,-3.05562433100001));
#353508=CARTESIAN_POINT('Ctrl Pts',(2.63432401599994,12.2,-3.05610092900002));
#353509=CARTESIAN_POINT('Ctrl Pts',(2.63432401599994,5.2,-3.05610092900002));
#353510=CARTESIAN_POINT('Ctrl Pts',(2.63432401599994,2.2,-3.05610092900002));
#353511=CARTESIAN_POINT('Ctrl Pts',(2.63487559999994,12.2,-3.05658074500001));
#353512=CARTESIAN_POINT('Ctrl Pts',(2.63487559999994,5.2,-3.05658074500001));
#353513=CARTESIAN_POINT('Ctrl Pts',(2.63487559999994,2.2,-3.05658074500001));
#353514=CARTESIAN_POINT('Ctrl Pts',(2.63543228599994,12.2,-3.05706376100002));
#353515=CARTESIAN_POINT('Ctrl Pts',(2.63543228599994,5.2,-3.05706376100002));
#353516=CARTESIAN_POINT('Ctrl Pts',(2.63543228599994,2.2,-3.05706376100002));
#353517=CARTESIAN_POINT('Ctrl Pts',(2.63599407299994,12.2,-3.05754995900001));
#353518=CARTESIAN_POINT('Ctrl Pts',(2.63599407299994,5.2,-3.05754995900001));
#353519=CARTESIAN_POINT('Ctrl Pts',(2.63599407299994,2.2,-3.05754995900001));
#353520=CARTESIAN_POINT('Ctrl Pts',(2.63656096199994,12.2,-3.05803931700002));
#353521=CARTESIAN_POINT('Ctrl Pts',(2.63656096199994,5.2,-3.05803931700002));
#353522=CARTESIAN_POINT('Ctrl Pts',(2.63656096199994,2.2,-3.05803931700002));
#353523=CARTESIAN_POINT('Ctrl Pts',(2.63713295299994,12.2,-3.05853182000002));
#353524=CARTESIAN_POINT('Ctrl Pts',(2.63713295299994,5.2,-3.05853182000002));
#353525=CARTESIAN_POINT('Ctrl Pts',(2.63713295299994,2.2,-3.05853182000002));
#353526=CARTESIAN_POINT('Ctrl Pts',(2.63771004699994,12.2,-3.05902744800001));
#353527=CARTESIAN_POINT('Ctrl Pts',(2.63771004699994,5.2,-3.05902744800001));
#353528=CARTESIAN_POINT('Ctrl Pts',(2.63771004699994,2.2,-3.05902744800001));
#353529=CARTESIAN_POINT('Ctrl Pts',(2.63829224399994,12.2,-3.05952618200001));
#353530=CARTESIAN_POINT('Ctrl Pts',(2.63829224399994,5.2,-3.05952618200001));
#353531=CARTESIAN_POINT('Ctrl Pts',(2.63829224399994,2.2,-3.05952618200001));
#353532=CARTESIAN_POINT('Ctrl Pts',(2.63887954299994,12.2,-3.06002800200002));
#353533=CARTESIAN_POINT('Ctrl Pts',(2.63887954299994,5.2,-3.06002800200002));
#353534=CARTESIAN_POINT('Ctrl Pts',(2.63887954299994,2.2,-3.06002800200002));
#353535=CARTESIAN_POINT('Ctrl Pts',(2.63947194599994,12.2,-3.06053289200001));
#353536=CARTESIAN_POINT('Ctrl Pts',(2.63947194599994,5.2,-3.06053289200001));
#353537=CARTESIAN_POINT('Ctrl Pts',(2.63947194599994,2.2,-3.06053289200001));
#353538=CARTESIAN_POINT('Ctrl Pts',(2.64006945299994,12.2,-3.06104083300001));
#353539=CARTESIAN_POINT('Ctrl Pts',(2.64006945299994,5.2,-3.06104083300001));
#353540=CARTESIAN_POINT('Ctrl Pts',(2.64006945299994,2.2,-3.06104083300001));
#353541=CARTESIAN_POINT('Ctrl Pts',(2.64067206299994,12.2,-3.06155180600001));
#353542=CARTESIAN_POINT('Ctrl Pts',(2.64067206299994,5.2,-3.06155180600001));
#353543=CARTESIAN_POINT('Ctrl Pts',(2.64067206299994,2.2,-3.06155180600001));
#353544=CARTESIAN_POINT('Ctrl Pts',(2.64127977599995,12.2,-3.06206579200001));
#353545=CARTESIAN_POINT('Ctrl Pts',(2.64127977599995,5.2,-3.06206579200001));
#353546=CARTESIAN_POINT('Ctrl Pts',(2.64127977599995,2.2,-3.06206579200001));
#353547=CARTESIAN_POINT('Ctrl Pts',(2.64189259399994,12.2,-3.06258277400001));
#353548=CARTESIAN_POINT('Ctrl Pts',(2.64189259399994,5.2,-3.06258277400001));
#353549=CARTESIAN_POINT('Ctrl Pts',(2.64189259399994,2.2,-3.06258277400001));
#353550=CARTESIAN_POINT('Ctrl Pts',(2.64251051499994,12.2,-3.06310273200001));
#353551=CARTESIAN_POINT('Ctrl Pts',(2.64251051499994,5.2,-3.06310273200001));
#353552=CARTESIAN_POINT('Ctrl Pts',(2.64251051499994,2.2,-3.06310273200001));
#353553=CARTESIAN_POINT('Ctrl Pts',(2.64313353999994,12.2,-3.06362564900001));
#353554=CARTESIAN_POINT('Ctrl Pts',(2.64313353999994,5.2,-3.06362564900001));
#353555=CARTESIAN_POINT('Ctrl Pts',(2.64313353999994,2.2,-3.06362564900001));
#353556=CARTESIAN_POINT('Ctrl Pts',(2.64376166999994,12.2,-3.06415150700001));
#353557=CARTESIAN_POINT('Ctrl Pts',(2.64376166999994,5.2,-3.06415150700001));
#353558=CARTESIAN_POINT('Ctrl Pts',(2.64376166999994,2.2,-3.06415150700001));
#353559=CARTESIAN_POINT('Ctrl Pts',(2.64439490399994,12.2,-3.06468028800001));
#353560=CARTESIAN_POINT('Ctrl Pts',(2.64439490399994,5.2,-3.06468028800001));
#353561=CARTESIAN_POINT('Ctrl Pts',(2.64439490399994,2.2,-3.06468028800001));
#353562=CARTESIAN_POINT('Ctrl Pts',(2.64503324199994,12.2,-3.06521197300002));
#353563=CARTESIAN_POINT('Ctrl Pts',(2.64503324199994,5.2,-3.06521197300002));
#353564=CARTESIAN_POINT('Ctrl Pts',(2.64503324199994,2.2,-3.06521197300002));
#353565=CARTESIAN_POINT('Ctrl Pts',(2.64567668399994,12.2,-3.06574654400002));
#353566=CARTESIAN_POINT('Ctrl Pts',(2.64567668399994,5.2,-3.06574654400002));
#353567=CARTESIAN_POINT('Ctrl Pts',(2.64567668399994,2.2,-3.06574654400002));
#353568=CARTESIAN_POINT('Ctrl Pts',(2.64632522999994,12.2,-3.06628398400001));
#353569=CARTESIAN_POINT('Ctrl Pts',(2.64632522999994,5.2,-3.06628398400001));
#353570=CARTESIAN_POINT('Ctrl Pts',(2.64632522999994,2.2,-3.06628398400001));
#353571=CARTESIAN_POINT('Ctrl Pts',(2.64697887999994,12.2,-3.06682427500002));
#353572=CARTESIAN_POINT('Ctrl Pts',(2.64697887999994,5.2,-3.06682427500002));
#353573=CARTESIAN_POINT('Ctrl Pts',(2.64697887999994,2.2,-3.06682427500002));
#353574=CARTESIAN_POINT('Ctrl Pts',(2.64763763499994,12.2,-3.06736739700002));
#353575=CARTESIAN_POINT('Ctrl Pts',(2.64763763499994,5.2,-3.06736739700002));
#353576=CARTESIAN_POINT('Ctrl Pts',(2.64763763499994,2.2,-3.06736739700002));
#353577=CARTESIAN_POINT('Ctrl Pts',(2.64830149199994,12.2,-3.06791333600001));
#353578=CARTESIAN_POINT('Ctrl Pts',(2.64830149199994,5.2,-3.06791333600001));
#353579=CARTESIAN_POINT('Ctrl Pts',(2.64830149199994,2.2,-3.06791333600001));
#353580=CARTESIAN_POINT('Ctrl Pts',(2.64897045499994,12.2,-3.06846207000001));
#353581=CARTESIAN_POINT('Ctrl Pts',(2.64897045499994,5.2,-3.06846207000001));
#353582=CARTESIAN_POINT('Ctrl Pts',(2.64897045499994,2.2,-3.06846207000001));
#353583=CARTESIAN_POINT('Ctrl Pts',(2.64964451899994,12.2,-3.06901358300002));
#353584=CARTESIAN_POINT('Ctrl Pts',(2.64964451899994,5.2,-3.06901358300002));
#353585=CARTESIAN_POINT('Ctrl Pts',(2.64964451899994,2.2,-3.06901358300002));
#353586=CARTESIAN_POINT('Ctrl Pts',(2.65032368799994,12.2,-3.06956785900002));
#353587=CARTESIAN_POINT('Ctrl Pts',(2.65032368799994,5.2,-3.06956785900002));
#353588=CARTESIAN_POINT('Ctrl Pts',(2.65032368799994,2.2,-3.06956785900002));
#353589=CARTESIAN_POINT('Ctrl Pts',(2.65100795999994,12.2,-3.07012487700002));
#353590=CARTESIAN_POINT('Ctrl Pts',(2.65100795999994,5.2,-3.07012487700002));
#353591=CARTESIAN_POINT('Ctrl Pts',(2.65100795999994,2.2,-3.07012487700002));
#353592=CARTESIAN_POINT('Ctrl Pts',(2.65169733399994,12.2,-3.07068462200002));
#353593=CARTESIAN_POINT('Ctrl Pts',(2.65169733399994,5.2,-3.07068462200002));
#353594=CARTESIAN_POINT('Ctrl Pts',(2.65169733399994,2.2,-3.07068462200002));
#353595=CARTESIAN_POINT('Ctrl Pts',(2.65239181199994,12.2,-3.07124707700002));
#353596=CARTESIAN_POINT('Ctrl Pts',(2.65239181199994,5.2,-3.07124707700002));
#353597=CARTESIAN_POINT('Ctrl Pts',(2.65239181199994,2.2,-3.07124707700002));
#353598=CARTESIAN_POINT('Ctrl Pts',(2.65309139299994,12.2,-3.07181222200001));
#353599=CARTESIAN_POINT('Ctrl Pts',(2.65309139299994,5.2,-3.07181222200001));
#353600=CARTESIAN_POINT('Ctrl Pts',(2.65309139299994,2.2,-3.07181222200001));
#353601=CARTESIAN_POINT('Ctrl Pts',(2.65379607499994,12.2,-3.07238004000002));
#353602=CARTESIAN_POINT('Ctrl Pts',(2.65379607499994,5.2,-3.07238004000002));
#353603=CARTESIAN_POINT('Ctrl Pts',(2.65379607499994,2.2,-3.07238004000002));
#353604=CARTESIAN_POINT('Ctrl Pts',(2.65450585899994,12.2,-3.07295051500001));
#353605=CARTESIAN_POINT('Ctrl Pts',(2.65450585899994,5.2,-3.07295051500001));
#353606=CARTESIAN_POINT('Ctrl Pts',(2.65450585899994,2.2,-3.07295051500001));
#353607=CARTESIAN_POINT('Ctrl Pts',(2.65522074599994,12.2,-3.07352363000001));
#353608=CARTESIAN_POINT('Ctrl Pts',(2.65522074599994,5.2,-3.07352363000001));
#353609=CARTESIAN_POINT('Ctrl Pts',(2.65522074599994,2.2,-3.07352363000001));
#353610=CARTESIAN_POINT('Ctrl Pts',(2.65594073299994,12.2,-3.07409936400001));
#353611=CARTESIAN_POINT('Ctrl Pts',(2.65594073299994,5.2,-3.07409936400001));
#353612=CARTESIAN_POINT('Ctrl Pts',(2.65594073299994,2.2,-3.07409936400001));
#353613=CARTESIAN_POINT('Ctrl Pts',(2.65666582099994,12.2,-3.07467770500002));
#353614=CARTESIAN_POINT('Ctrl Pts',(2.65666582099994,5.2,-3.07467770500002));
#353615=CARTESIAN_POINT('Ctrl Pts',(2.65666582099994,2.2,-3.07467770500002));
#353616=CARTESIAN_POINT('Ctrl Pts',(2.65739600999995,12.2,-3.07525863200001));
#353617=CARTESIAN_POINT('Ctrl Pts',(2.65739600999995,5.2,-3.07525863200001));
#353618=CARTESIAN_POINT('Ctrl Pts',(2.65739600999995,2.2,-3.07525863200001));
#353619=CARTESIAN_POINT('Ctrl Pts',(2.65813129899994,12.2,-3.07584212800001));
#353620=CARTESIAN_POINT('Ctrl Pts',(2.65813129899994,5.2,-3.07584212800001));
#353621=CARTESIAN_POINT('Ctrl Pts',(2.65813129899994,2.2,-3.07584212800001));
#353622=CARTESIAN_POINT('Ctrl Pts',(2.65887168799994,12.2,-3.07642817700001));
#353623=CARTESIAN_POINT('Ctrl Pts',(2.65887168799994,5.2,-3.07642817700001));
#353624=CARTESIAN_POINT('Ctrl Pts',(2.65887168799994,2.2,-3.07642817700001));
#353625=CARTESIAN_POINT('Ctrl Pts',(2.65961717599994,12.2,-3.07701676300002));
#353626=CARTESIAN_POINT('Ctrl Pts',(2.65961717599994,5.2,-3.07701676300002));
#353627=CARTESIAN_POINT('Ctrl Pts',(2.65961717599994,2.2,-3.07701676300002));
#353628=CARTESIAN_POINT('Ctrl Pts',(2.66036776299994,12.2,-3.07760786700001));
#353629=CARTESIAN_POINT('Ctrl Pts',(2.66036776299994,5.2,-3.07760786700001));
#353630=CARTESIAN_POINT('Ctrl Pts',(2.66036776299994,2.2,-3.07760786700001));
#353631=CARTESIAN_POINT('Ctrl Pts',(2.66112344799994,12.2,-3.07820147200002));
#353632=CARTESIAN_POINT('Ctrl Pts',(2.66112344799994,5.2,-3.07820147200002));
#353633=CARTESIAN_POINT('Ctrl Pts',(2.66112344799994,2.2,-3.07820147200002));
#353634=CARTESIAN_POINT('Ctrl Pts',(2.66188423199994,12.2,-3.07879756100002));
#353635=CARTESIAN_POINT('Ctrl Pts',(2.66188423199994,5.2,-3.07879756100002));
#353636=CARTESIAN_POINT('Ctrl Pts',(2.66188423199994,2.2,-3.07879756100002));
#353637=CARTESIAN_POINT('Ctrl Pts',(2.66265011199994,12.2,-3.07939611900002));
#353638=CARTESIAN_POINT('Ctrl Pts',(2.66265011199994,5.2,-3.07939611900002));
#353639=CARTESIAN_POINT('Ctrl Pts',(2.66265011199994,2.2,-3.07939611900002));
#353640=CARTESIAN_POINT('Ctrl Pts',(2.66342108999994,12.2,-3.07999712700001));
#353641=CARTESIAN_POINT('Ctrl Pts',(2.66342108999994,5.2,-3.07999712700001));
#353642=CARTESIAN_POINT('Ctrl Pts',(2.66342108999994,2.2,-3.07999712700001));
#353643=CARTESIAN_POINT('Ctrl Pts',(2.66419716399994,12.2,-3.08060056900001));
#353644=CARTESIAN_POINT('Ctrl Pts',(2.66419716399994,5.2,-3.08060056900001));
#353645=CARTESIAN_POINT('Ctrl Pts',(2.66419716399994,2.2,-3.08060056900001));
#353646=CARTESIAN_POINT('Ctrl Pts',(2.66497833299994,12.2,-3.08120642900001));
#353647=CARTESIAN_POINT('Ctrl Pts',(2.66497833299994,5.2,-3.08120642900001));
#353648=CARTESIAN_POINT('Ctrl Pts',(2.66497833299994,2.2,-3.08120642900001));
#353649=CARTESIAN_POINT('Ctrl Pts',(2.66576459699994,12.2,-3.08181468900001));
#353650=CARTESIAN_POINT('Ctrl Pts',(2.66576459699994,5.2,-3.08181468900001));
#353651=CARTESIAN_POINT('Ctrl Pts',(2.66576459699994,2.2,-3.08181468900001));
#353652=CARTESIAN_POINT('Ctrl Pts',(2.66655595599994,12.2,-3.08242533300001));
#353653=CARTESIAN_POINT('Ctrl Pts',(2.66655595599994,5.2,-3.08242533300001));
#353654=CARTESIAN_POINT('Ctrl Pts',(2.66655595599994,2.2,-3.08242533300001));
#353655=CARTESIAN_POINT('Ctrl Pts',(2.66735240899994,12.2,-3.08303834300002));
#353656=CARTESIAN_POINT('Ctrl Pts',(2.66735240899994,5.2,-3.08303834300002));
#353657=CARTESIAN_POINT('Ctrl Pts',(2.66735240899994,2.2,-3.08303834300002));
#353658=CARTESIAN_POINT('Ctrl Pts',(2.66815395399994,12.2,-3.08365370400002));
#353659=CARTESIAN_POINT('Ctrl Pts',(2.66815395399994,5.2,-3.08365370400002));
#353660=CARTESIAN_POINT('Ctrl Pts',(2.66815395399994,2.2,-3.08365370400002));
#353661=CARTESIAN_POINT('Ctrl Pts',(2.66896059199994,12.2,-3.08427139900001));
#353662=CARTESIAN_POINT('Ctrl Pts',(2.66896059199994,5.2,-3.08427139900001));
#353663=CARTESIAN_POINT('Ctrl Pts',(2.66896059199994,2.2,-3.08427139900001));
#353664=CARTESIAN_POINT('Ctrl Pts',(2.66977232299995,12.2,-3.08489141100001));
#353665=CARTESIAN_POINT('Ctrl Pts',(2.66977232299995,5.2,-3.08489141100001));
#353666=CARTESIAN_POINT('Ctrl Pts',(2.66977232299995,2.2,-3.08489141100001));
#353667=CARTESIAN_POINT('Ctrl Pts',(2.67058914399994,12.2,-3.08551372400002));
#353668=CARTESIAN_POINT('Ctrl Pts',(2.67058914399994,5.2,-3.08551372400002));
#353669=CARTESIAN_POINT('Ctrl Pts',(2.67058914399994,2.2,-3.08551372400002));
#353670=CARTESIAN_POINT('Ctrl Pts',(2.67141105599995,12.2,-3.08613832200002));
#353671=CARTESIAN_POINT('Ctrl Pts',(2.67141105599995,5.2,-3.08613832200002));
#353672=CARTESIAN_POINT('Ctrl Pts',(2.67141105599995,2.2,-3.08613832200002));
#353673=CARTESIAN_POINT('Ctrl Pts',(2.67223805599994,12.2,-3.08676518600001));
#353674=CARTESIAN_POINT('Ctrl Pts',(2.67223805599994,5.2,-3.08676518600001));
#353675=CARTESIAN_POINT('Ctrl Pts',(2.67223805599994,2.2,-3.08676518600001));
#353676=CARTESIAN_POINT('Ctrl Pts',(2.67307014599994,12.2,-3.08739430300002));
#353677=CARTESIAN_POINT('Ctrl Pts',(2.67307014599994,5.2,-3.08739430300002));
#353678=CARTESIAN_POINT('Ctrl Pts',(2.67307014599994,2.2,-3.08739430300002));
#353679=CARTESIAN_POINT('Ctrl Pts',(2.67390732399994,12.2,-3.08802565600002));
#353680=CARTESIAN_POINT('Ctrl Pts',(2.67390732399994,5.2,-3.08802565600002));
#353681=CARTESIAN_POINT('Ctrl Pts',(2.67390732399994,2.2,-3.08802565600002));
#353682=CARTESIAN_POINT('Ctrl Pts',(2.67474958899995,12.2,-3.08865922700001));
#353683=CARTESIAN_POINT('Ctrl Pts',(2.67474958899995,5.2,-3.08865922700001));
#353684=CARTESIAN_POINT('Ctrl Pts',(2.67474958899995,2.2,-3.08865922700001));
#353685=CARTESIAN_POINT('Ctrl Pts',(2.67559693999994,12.2,-3.08929500100001));
#353686=CARTESIAN_POINT('Ctrl Pts',(2.67559693999994,5.2,-3.08929500100001));
#353687=CARTESIAN_POINT('Ctrl Pts',(2.67559693999994,2.2,-3.08929500100001));
#353688=CARTESIAN_POINT('Ctrl Pts',(2.67644937699994,12.2,-3.08993296100001));
#353689=CARTESIAN_POINT('Ctrl Pts',(2.67644937699994,5.2,-3.08993296100001));
#353690=CARTESIAN_POINT('Ctrl Pts',(2.67644937699994,2.2,-3.08993296100001));
#353691=CARTESIAN_POINT('Ctrl Pts',(2.67730689799994,12.2,-3.09057309200002));
#353692=CARTESIAN_POINT('Ctrl Pts',(2.67730689799994,5.2,-3.09057309200002));
#353693=CARTESIAN_POINT('Ctrl Pts',(2.67730689799994,2.2,-3.09057309200002));
#353694=CARTESIAN_POINT('Ctrl Pts',(2.67816950399994,12.2,-3.09121537600001));
#353695=CARTESIAN_POINT('Ctrl Pts',(2.67816950399994,5.2,-3.09121537600001));
#353696=CARTESIAN_POINT('Ctrl Pts',(2.67816950399994,2.2,-3.09121537600001));
#353697=CARTESIAN_POINT('Ctrl Pts',(2.67903719199994,12.2,-3.09185980000001));
#353698=CARTESIAN_POINT('Ctrl Pts',(2.67903719199994,5.2,-3.09185980000001));
#353699=CARTESIAN_POINT('Ctrl Pts',(2.67903719199994,2.2,-3.09185980000001));
#353700=CARTESIAN_POINT('Ctrl Pts',(2.67990996199994,12.2,-3.09250634500001));
#353701=CARTESIAN_POINT('Ctrl Pts',(2.67990996199994,5.2,-3.09250634500001));
#353702=CARTESIAN_POINT('Ctrl Pts',(2.67990996199994,2.2,-3.09250634500001));
#353703=CARTESIAN_POINT('Ctrl Pts',(2.68078781199995,12.2,-3.09315499600002));
#353704=CARTESIAN_POINT('Ctrl Pts',(2.68078781199995,5.2,-3.09315499600002));
#353705=CARTESIAN_POINT('Ctrl Pts',(2.68078781199995,2.2,-3.09315499600002));
#353706=CARTESIAN_POINT('Ctrl Pts',(2.68167074299994,12.2,-3.09380573700002));
#353707=CARTESIAN_POINT('Ctrl Pts',(2.68167074299994,5.2,-3.09380573700002));
#353708=CARTESIAN_POINT('Ctrl Pts',(2.68167074299994,2.2,-3.09380573700002));
#353709=CARTESIAN_POINT('Ctrl Pts',(2.68255875399994,12.2,-3.09445855300002));
#353710=CARTESIAN_POINT('Ctrl Pts',(2.68255875399994,5.2,-3.09445855300002));
#353711=CARTESIAN_POINT('Ctrl Pts',(2.68255875399994,2.2,-3.09445855300002));
#353712=CARTESIAN_POINT('Ctrl Pts',(2.68345184199994,12.2,-3.09511342700001));
#353713=CARTESIAN_POINT('Ctrl Pts',(2.68345184199994,5.2,-3.09511342700001));
#353714=CARTESIAN_POINT('Ctrl Pts',(2.68345184199994,2.2,-3.09511342700001));
#353715=CARTESIAN_POINT('Ctrl Pts',(2.68435000699994,12.2,-3.09577034500002));
#353716=CARTESIAN_POINT('Ctrl Pts',(2.68435000699994,5.2,-3.09577034500002));
#353717=CARTESIAN_POINT('Ctrl Pts',(2.68435000699994,2.2,-3.09577034500002));
#353718=CARTESIAN_POINT('Ctrl Pts',(2.68525324699994,12.2,-3.09642928700002));
#353719=CARTESIAN_POINT('Ctrl Pts',(2.68525324699994,5.2,-3.09642928700002));
#353720=CARTESIAN_POINT('Ctrl Pts',(2.68525324699994,2.2,-3.09642928700002));
#353721=CARTESIAN_POINT('Ctrl Pts',(2.68616156399994,12.2,-3.09709024200002));
#353722=CARTESIAN_POINT('Ctrl Pts',(2.68616156399994,5.2,-3.09709024200002));
#353723=CARTESIAN_POINT('Ctrl Pts',(2.68616156399994,2.2,-3.09709024200002));
#353724=CARTESIAN_POINT('Ctrl Pts',(2.68707495399994,12.2,-3.09775319100002));
#353725=CARTESIAN_POINT('Ctrl Pts',(2.68707495399994,5.2,-3.09775319100002));
#353726=CARTESIAN_POINT('Ctrl Pts',(2.68707495399994,2.2,-3.09775319100002));
#353727=CARTESIAN_POINT('Ctrl Pts',(2.68799341599995,12.2,-3.09841812100002));
#353728=CARTESIAN_POINT('Ctrl Pts',(2.68799341599995,5.2,-3.09841812100002));
#353729=CARTESIAN_POINT('Ctrl Pts',(2.68799341599995,2.2,-3.09841812100002));
#353730=CARTESIAN_POINT('Ctrl Pts',(2.68891695099994,12.2,-3.09908501400002));
#353731=CARTESIAN_POINT('Ctrl Pts',(2.68891695099994,5.2,-3.09908501400002));
#353732=CARTESIAN_POINT('Ctrl Pts',(2.68891695099994,2.2,-3.09908501400002));
#353733=CARTESIAN_POINT('Ctrl Pts',(2.68984555499994,12.2,-3.09975385400001));
#353734=CARTESIAN_POINT('Ctrl Pts',(2.68984555499994,5.2,-3.09975385400001));
#353735=CARTESIAN_POINT('Ctrl Pts',(2.68984555499994,2.2,-3.09975385400001));
#353736=CARTESIAN_POINT('Ctrl Pts',(2.69077922999994,12.2,-3.10042462800002));
#353737=CARTESIAN_POINT('Ctrl Pts',(2.69077922999994,5.2,-3.10042462800002));
#353738=CARTESIAN_POINT('Ctrl Pts',(2.69077922999994,2.2,-3.10042462800002));
#353739=CARTESIAN_POINT('Ctrl Pts',(2.69171797199995,12.2,-3.10109732000001));
#353740=CARTESIAN_POINT('Ctrl Pts',(2.69171797199995,5.2,-3.10109732000001));
#353741=CARTESIAN_POINT('Ctrl Pts',(2.69171797199995,2.2,-3.10109732000001));
#353742=CARTESIAN_POINT('Ctrl Pts',(2.69266178199994,12.2,-3.10177191300001));
#353743=CARTESIAN_POINT('Ctrl Pts',(2.69266178199994,5.2,-3.10177191300001));
#353744=CARTESIAN_POINT('Ctrl Pts',(2.69266178199994,2.2,-3.10177191300001));
#353745=CARTESIAN_POINT('Ctrl Pts',(2.69361065799994,12.2,-3.10244839200001));
#353746=CARTESIAN_POINT('Ctrl Pts',(2.69361065799994,5.2,-3.10244839200001));
#353747=CARTESIAN_POINT('Ctrl Pts',(2.69361065799994,2.2,-3.10244839200001));
#353748=CARTESIAN_POINT('Ctrl Pts',(2.69456459899994,12.2,-3.10312674100001));
#353749=CARTESIAN_POINT('Ctrl Pts',(2.69456459899994,5.2,-3.10312674100001));
#353750=CARTESIAN_POINT('Ctrl Pts',(2.69456459899994,2.2,-3.10312674100001));
#353751=CARTESIAN_POINT('Ctrl Pts',(2.69552360299994,12.2,-3.10380694600001));
#353752=CARTESIAN_POINT('Ctrl Pts',(2.69552360299994,5.2,-3.10380694600001));
#353753=CARTESIAN_POINT('Ctrl Pts',(2.69552360299994,2.2,-3.10380694600001));
#353754=CARTESIAN_POINT('Ctrl Pts',(2.69648766799994,12.2,-3.10448899200002));
#353755=CARTESIAN_POINT('Ctrl Pts',(2.69648766799994,5.2,-3.10448899200002));
#353756=CARTESIAN_POINT('Ctrl Pts',(2.69648766799994,2.2,-3.10448899200002));
#353757=CARTESIAN_POINT('Ctrl Pts',(2.69745679499994,12.2,-3.10517286200001));
#353758=CARTESIAN_POINT('Ctrl Pts',(2.69745679499994,5.2,-3.10517286200001));
#353759=CARTESIAN_POINT('Ctrl Pts',(2.69745679499994,2.2,-3.10517286200001));
#353760=CARTESIAN_POINT('Ctrl Pts',(2.69843098199994,12.2,-3.10585854200002));
#353761=CARTESIAN_POINT('Ctrl Pts',(2.69843098199994,5.2,-3.10585854200002));
#353762=CARTESIAN_POINT('Ctrl Pts',(2.69843098199994,2.2,-3.10585854200002));
#353763=CARTESIAN_POINT('Ctrl Pts',(2.69941022799994,12.2,-3.10654601500001));
#353764=CARTESIAN_POINT('Ctrl Pts',(2.69941022799994,5.2,-3.10654601500001));
#353765=CARTESIAN_POINT('Ctrl Pts',(2.69941022799994,2.2,-3.10654601500001));
#353766=CARTESIAN_POINT('Ctrl Pts',(2.70039452999994,12.2,-3.10723526900002));
#353767=CARTESIAN_POINT('Ctrl Pts',(2.70039452999994,5.2,-3.10723526900002));
#353768=CARTESIAN_POINT('Ctrl Pts',(2.70039452999994,2.2,-3.10723526900002));
#353769=CARTESIAN_POINT('Ctrl Pts',(2.70138388799994,12.2,-3.10792628600002));
#353770=CARTESIAN_POINT('Ctrl Pts',(2.70138388799994,5.2,-3.10792628600002));
#353771=CARTESIAN_POINT('Ctrl Pts',(2.70138388799994,2.2,-3.10792628600002));
#353772=CARTESIAN_POINT('Ctrl Pts',(2.70237829999994,12.2,-3.10861905100001));
#353773=CARTESIAN_POINT('Ctrl Pts',(2.70237829999994,5.2,-3.10861905100001));
#353774=CARTESIAN_POINT('Ctrl Pts',(2.70237829999994,2.2,-3.10861905100001));
#353775=CARTESIAN_POINT('Ctrl Pts',(2.70337776599994,12.2,-3.10931355100001));
#353776=CARTESIAN_POINT('Ctrl Pts',(2.70337776599994,5.2,-3.10931355100001));
#353777=CARTESIAN_POINT('Ctrl Pts',(2.70337776599994,2.2,-3.10931355100001));
#353778=CARTESIAN_POINT('Ctrl Pts',(2.70438228399994,12.2,-3.11000976900001));
#353779=CARTESIAN_POINT('Ctrl Pts',(2.70438228399994,5.2,-3.11000976900001));
#353780=CARTESIAN_POINT('Ctrl Pts',(2.70438228399994,2.2,-3.11000976900001));
#353781=CARTESIAN_POINT('Ctrl Pts',(2.70539185199994,12.2,-3.11070769100001));
#353782=CARTESIAN_POINT('Ctrl Pts',(2.70539185199994,5.2,-3.11070769100001));
#353783=CARTESIAN_POINT('Ctrl Pts',(2.70539185199994,2.2,-3.11070769100001));
#353784=CARTESIAN_POINT('Ctrl Pts',(2.70640646799994,12.2,-3.11140730100002));
#353785=CARTESIAN_POINT('Ctrl Pts',(2.70640646799994,5.2,-3.11140730100002));
#353786=CARTESIAN_POINT('Ctrl Pts',(2.70640646799994,2.2,-3.11140730100002));
#353787=CARTESIAN_POINT('Ctrl Pts',(2.70742613199995,12.2,-3.11210858600001));
#353788=CARTESIAN_POINT('Ctrl Pts',(2.70742613199995,5.2,-3.11210858600001));
#353789=CARTESIAN_POINT('Ctrl Pts',(2.70742613199995,2.2,-3.11210858600001));
#353790=CARTESIAN_POINT('Ctrl Pts',(2.70845084199994,12.2,-3.11281152900001));
#353791=CARTESIAN_POINT('Ctrl Pts',(2.70845084199994,5.2,-3.11281152900001));
#353792=CARTESIAN_POINT('Ctrl Pts',(2.70845084199994,2.2,-3.11281152900001));
#353793=CARTESIAN_POINT('Ctrl Pts',(2.70948059699994,12.2,-3.11351611600001));
#353794=CARTESIAN_POINT('Ctrl Pts',(2.70948059699994,5.2,-3.11351611600001));
#353795=CARTESIAN_POINT('Ctrl Pts',(2.70948059699994,2.2,-3.11351611600001));
#353796=CARTESIAN_POINT('Ctrl Pts',(2.71051539499994,12.2,-3.11422233200001));
#353797=CARTESIAN_POINT('Ctrl Pts',(2.71051539499994,5.2,-3.11422233200001));
#353798=CARTESIAN_POINT('Ctrl Pts',(2.71051539499994,2.2,-3.11422233200001));
#353799=CARTESIAN_POINT('Ctrl Pts',(2.71155523399994,12.2,-3.11493016200002));
#353800=CARTESIAN_POINT('Ctrl Pts',(2.71155523399994,5.2,-3.11493016200002));
#353801=CARTESIAN_POINT('Ctrl Pts',(2.71155523399994,2.2,-3.11493016200002));
#353802=CARTESIAN_POINT('Ctrl Pts',(2.71260011399994,12.2,-3.11563959200001));
#353803=CARTESIAN_POINT('Ctrl Pts',(2.71260011399994,5.2,-3.11563959200001));
#353804=CARTESIAN_POINT('Ctrl Pts',(2.71260011399994,2.2,-3.11563959200001));
#353805=CARTESIAN_POINT('Ctrl Pts',(2.71365003199994,12.2,-3.11635060700001));
#353806=CARTESIAN_POINT('Ctrl Pts',(2.71365003199994,5.2,-3.11635060700001));
#353807=CARTESIAN_POINT('Ctrl Pts',(2.71365003199994,2.2,-3.11635060700001));
#353808=CARTESIAN_POINT('Ctrl Pts',(2.71470498699995,12.2,-3.11706319200002));
#353809=CARTESIAN_POINT('Ctrl Pts',(2.71470498699995,5.2,-3.11706319200002));
#353810=CARTESIAN_POINT('Ctrl Pts',(2.71470498699995,2.2,-3.11706319200002));
#353811=CARTESIAN_POINT('Ctrl Pts',(2.71576497699995,12.2,-3.11777733300001));
#353812=CARTESIAN_POINT('Ctrl Pts',(2.71576497699995,5.2,-3.11777733300001));
#353813=CARTESIAN_POINT('Ctrl Pts',(2.71576497699995,2.2,-3.11777733300001));
#353814=CARTESIAN_POINT('Ctrl Pts',(2.71683000299995,12.2,-3.11849301300001));
#353815=CARTESIAN_POINT('Ctrl Pts',(2.71683000299995,5.2,-3.11849301300001));
#353816=CARTESIAN_POINT('Ctrl Pts',(2.71683000299995,2.2,-3.11849301300001));
#353817=CARTESIAN_POINT('Ctrl Pts',(2.71790005899994,12.2,-3.11921022100002));
#353818=CARTESIAN_POINT('Ctrl Pts',(2.71790005899994,5.2,-3.11921022100002));
#353819=CARTESIAN_POINT('Ctrl Pts',(2.71790005899994,2.2,-3.11921022100002));
#353820=CARTESIAN_POINT('Ctrl Pts',(2.71897514799994,12.2,-3.11992894100001));
#353821=CARTESIAN_POINT('Ctrl Pts',(2.71897514799994,5.2,-3.11992894100001));
#353822=CARTESIAN_POINT('Ctrl Pts',(2.71897514799994,2.2,-3.11992894100001));
#353823=CARTESIAN_POINT('Ctrl Pts',(2.72005526399994,12.2,-3.12064915700001));
#353824=CARTESIAN_POINT('Ctrl Pts',(2.72005526399994,5.2,-3.12064915700001));
#353825=CARTESIAN_POINT('Ctrl Pts',(2.72005526399994,2.2,-3.12064915700001));
#353826=CARTESIAN_POINT('Ctrl Pts',(2.72114040899994,12.2,-3.12137085700002));
#353827=CARTESIAN_POINT('Ctrl Pts',(2.72114040899994,5.2,-3.12137085700002));
#353828=CARTESIAN_POINT('Ctrl Pts',(2.72114040899994,2.2,-3.12137085700002));
#353829=CARTESIAN_POINT('Ctrl Pts',(2.72223057899994,12.2,-3.12209402400002));
#353830=CARTESIAN_POINT('Ctrl Pts',(2.72223057899994,5.2,-3.12209402400002));
#353831=CARTESIAN_POINT('Ctrl Pts',(2.72223057899994,2.2,-3.12209402400002));
#353832=CARTESIAN_POINT('Ctrl Pts',(2.72332577399995,12.2,-3.12281864500001));
#353833=CARTESIAN_POINT('Ctrl Pts',(2.72332577399995,5.2,-3.12281864500001));
#353834=CARTESIAN_POINT('Ctrl Pts',(2.72332577399995,2.2,-3.12281864500001));
#353835=CARTESIAN_POINT('Ctrl Pts',(2.72442599199994,12.2,-3.12354470700001));
#353836=CARTESIAN_POINT('Ctrl Pts',(2.72442599199994,5.2,-3.12354470700001));
#353837=CARTESIAN_POINT('Ctrl Pts',(2.72442599199994,2.2,-3.12354470700001));
#353838=CARTESIAN_POINT('Ctrl Pts',(2.72553122899994,12.2,-3.12427219300002));
#353839=CARTESIAN_POINT('Ctrl Pts',(2.72553122899994,5.2,-3.12427219300002));
#353840=CARTESIAN_POINT('Ctrl Pts',(2.72553122899994,2.2,-3.12427219300002));
#353841=CARTESIAN_POINT('Ctrl Pts',(2.72664148599994,12.2,-3.12500108900001));
#353842=CARTESIAN_POINT('Ctrl Pts',(2.72664148599994,5.2,-3.12500108900001));
#353843=CARTESIAN_POINT('Ctrl Pts',(2.72664148599994,2.2,-3.12500108900001));
#353844=CARTESIAN_POINT('Ctrl Pts',(2.72775676099994,12.2,-3.12573138200001));
#353845=CARTESIAN_POINT('Ctrl Pts',(2.72775676099994,5.2,-3.12573138200001));
#353846=CARTESIAN_POINT('Ctrl Pts',(2.72775676099994,2.2,-3.12573138200001));
#353847=CARTESIAN_POINT('Ctrl Pts',(2.72887705099994,12.2,-3.12646305800001));
#353848=CARTESIAN_POINT('Ctrl Pts',(2.72887705099994,5.2,-3.12646305800001));
#353849=CARTESIAN_POINT('Ctrl Pts',(2.72887705099994,2.2,-3.12646305800001));
#353850=CARTESIAN_POINT('Ctrl Pts',(2.73000235499994,12.2,-3.12719610100002));
#353851=CARTESIAN_POINT('Ctrl Pts',(2.73000235499994,5.2,-3.12719610100002));
#353852=CARTESIAN_POINT('Ctrl Pts',(2.73000235499994,2.2,-3.12719610100002));
#353853=CARTESIAN_POINT('Ctrl Pts',(2.73113267199995,12.2,-3.12793049800002));
#353854=CARTESIAN_POINT('Ctrl Pts',(2.73113267199995,5.2,-3.12793049800002));
#353855=CARTESIAN_POINT('Ctrl Pts',(2.73113267199995,2.2,-3.12793049800002));
#353856=CARTESIAN_POINT('Ctrl Pts',(2.73226799899994,12.2,-3.12866623600002));
#353857=CARTESIAN_POINT('Ctrl Pts',(2.73226799899994,5.2,-3.12866623600002));
#353858=CARTESIAN_POINT('Ctrl Pts',(2.73226799899994,2.2,-3.12866623600002));
#353859=CARTESIAN_POINT('Ctrl Pts',(2.73340833399994,12.2,-3.12940329900002));
#353860=CARTESIAN_POINT('Ctrl Pts',(2.73340833399994,5.2,-3.12940329900002));
#353861=CARTESIAN_POINT('Ctrl Pts',(2.73340833399994,2.2,-3.12940329900002));
#353862=CARTESIAN_POINT('Ctrl Pts',(2.73455367599994,12.2,-3.13014167200001));
#353863=CARTESIAN_POINT('Ctrl Pts',(2.73455367599994,5.2,-3.13014167200001));
#353864=CARTESIAN_POINT('Ctrl Pts',(2.73455367599994,2.2,-3.13014167200001));
#353865=CARTESIAN_POINT('Ctrl Pts',(2.73570402299995,12.2,-3.13088134400001));
#353866=CARTESIAN_POINT('Ctrl Pts',(2.73570402299995,5.2,-3.13088134400001));
#353867=CARTESIAN_POINT('Ctrl Pts',(2.73570402299995,2.2,-3.13088134400001));
#353868=CARTESIAN_POINT('Ctrl Pts',(2.73685937399994,12.2,-3.13162229900001));
#353869=CARTESIAN_POINT('Ctrl Pts',(2.73685937399994,5.2,-3.13162229900001));
#353870=CARTESIAN_POINT('Ctrl Pts',(2.73685937399994,2.2,-3.13162229900001));
#353871=CARTESIAN_POINT('Ctrl Pts',(2.73801972499994,12.2,-3.13236452400002));
#353872=CARTESIAN_POINT('Ctrl Pts',(2.73801972499994,5.2,-3.13236452400002));
#353873=CARTESIAN_POINT('Ctrl Pts',(2.73801972499994,2.2,-3.13236452400002));
#353874=CARTESIAN_POINT('Ctrl Pts',(2.73918507599994,12.2,-3.13310800400001));
#353875=CARTESIAN_POINT('Ctrl Pts',(2.73918507599994,5.2,-3.13310800400001));
#353876=CARTESIAN_POINT('Ctrl Pts',(2.73918507599994,2.2,-3.13310800400001));
#353877=CARTESIAN_POINT('Ctrl Pts',(2.74035542399994,12.2,-3.13385272500001));
#353878=CARTESIAN_POINT('Ctrl Pts',(2.74035542399994,5.2,-3.13385272500001));
#353879=CARTESIAN_POINT('Ctrl Pts',(2.74035542399994,2.2,-3.13385272500001));
#353880=CARTESIAN_POINT('Ctrl Pts',(2.74153076699994,12.2,-3.13459867400002));
#353881=CARTESIAN_POINT('Ctrl Pts',(2.74153076699994,5.2,-3.13459867400002));
#353882=CARTESIAN_POINT('Ctrl Pts',(2.74153076699994,2.2,-3.13459867400002));
#353883=CARTESIAN_POINT('Ctrl Pts',(2.74271110499994,12.2,-3.13534583800001));
#353884=CARTESIAN_POINT('Ctrl Pts',(2.74271110499994,5.2,-3.13534583800001));
#353885=CARTESIAN_POINT('Ctrl Pts',(2.74271110499994,2.2,-3.13534583800001));
#353886=CARTESIAN_POINT('Ctrl Pts',(2.74389643499994,12.2,-3.13609420100001));
#353887=CARTESIAN_POINT('Ctrl Pts',(2.74389643499994,5.2,-3.13609420100001));
#353888=CARTESIAN_POINT('Ctrl Pts',(2.74389643499994,2.2,-3.13609420100001));
#353889=CARTESIAN_POINT('Ctrl Pts',(2.74508675499994,12.2,-3.13684375000001));
#353890=CARTESIAN_POINT('Ctrl Pts',(2.74508675499994,5.2,-3.13684375000001));
#353891=CARTESIAN_POINT('Ctrl Pts',(2.74508675499994,2.2,-3.13684375000001));
#353892=CARTESIAN_POINT('Ctrl Pts',(2.74628206099994,12.2,-3.13759447100002));
#353893=CARTESIAN_POINT('Ctrl Pts',(2.74628206099994,5.2,-3.13759447100002));
#353894=CARTESIAN_POINT('Ctrl Pts',(2.74628206099994,2.2,-3.13759447100002));
#353895=CARTESIAN_POINT('Ctrl Pts',(2.74748235499994,12.2,-3.13834635100001));
#353896=CARTESIAN_POINT('Ctrl Pts',(2.74748235499994,5.2,-3.13834635100001));
#353897=CARTESIAN_POINT('Ctrl Pts',(2.74748235499994,2.2,-3.13834635100001));
#353898=CARTESIAN_POINT('Ctrl Pts',(2.74868763199994,12.2,-3.13909937600001));
#353899=CARTESIAN_POINT('Ctrl Pts',(2.74868763199994,5.2,-3.13909937600001));
#353900=CARTESIAN_POINT('Ctrl Pts',(2.74868763199994,2.2,-3.13909937600001));
#353901=CARTESIAN_POINT('Ctrl Pts',(2.74989788999994,12.2,-3.13985353400001));
#353902=CARTESIAN_POINT('Ctrl Pts',(2.74989788999994,5.2,-3.13985353400001));
#353903=CARTESIAN_POINT('Ctrl Pts',(2.74989788999994,2.2,-3.13985353400001));
#353904=CARTESIAN_POINT('Ctrl Pts',(2.75111312999994,12.2,-3.14060880700001));
#353905=CARTESIAN_POINT('Ctrl Pts',(2.75111312999994,5.2,-3.14060880700001));
#353906=CARTESIAN_POINT('Ctrl Pts',(2.75111312999994,2.2,-3.14060880700001));
#353907=CARTESIAN_POINT('Ctrl Pts',(2.75233334699994,12.2,-3.14136518500002));
#353908=CARTESIAN_POINT('Ctrl Pts',(2.75233334699994,5.2,-3.14136518500002));
#353909=CARTESIAN_POINT('Ctrl Pts',(2.75233334699994,2.2,-3.14136518500002));
#353910=CARTESIAN_POINT('Ctrl Pts',(2.75355853999995,12.2,-3.14212265500001));
#353911=CARTESIAN_POINT('Ctrl Pts',(2.75355853999995,5.2,-3.14212265500001));
#353912=CARTESIAN_POINT('Ctrl Pts',(2.75355853999995,2.2,-3.14212265500001));
#353913=CARTESIAN_POINT('Ctrl Pts',(2.75478870599994,12.2,-3.14288120000001));
#353914=CARTESIAN_POINT('Ctrl Pts',(2.75478870599994,5.2,-3.14288120000001));
#353915=CARTESIAN_POINT('Ctrl Pts',(2.75478870599994,2.2,-3.14288120000001));
#353916=CARTESIAN_POINT('Ctrl Pts',(2.75602384399994,12.2,-3.14364080900001));
#353917=CARTESIAN_POINT('Ctrl Pts',(2.75602384399994,5.2,-3.14364080900001));
#353918=CARTESIAN_POINT('Ctrl Pts',(2.75602384399994,2.2,-3.14364080900001));
#353919=CARTESIAN_POINT('Ctrl Pts',(2.75726395199994,12.2,-3.14440146800001));
#353920=CARTESIAN_POINT('Ctrl Pts',(2.75726395199994,5.2,-3.14440146800001));
#353921=CARTESIAN_POINT('Ctrl Pts',(2.75726395199994,2.2,-3.14440146800001));
#353922=CARTESIAN_POINT('Ctrl Pts',(2.75850902699994,12.2,-3.14516316300002));
#353923=CARTESIAN_POINT('Ctrl Pts',(2.75850902699994,5.2,-3.14516316300002));
#353924=CARTESIAN_POINT('Ctrl Pts',(2.75850902699994,2.2,-3.14516316300002));
#353925=CARTESIAN_POINT('Ctrl Pts',(2.75975906799995,12.2,-3.14592588300001));
#353926=CARTESIAN_POINT('Ctrl Pts',(2.75975906799995,5.2,-3.14592588300001));
#353927=CARTESIAN_POINT('Ctrl Pts',(2.75975906799995,2.2,-3.14592588300001));
#353928=CARTESIAN_POINT('Ctrl Pts',(2.76101407199994,12.2,-3.14668961000002));
#353929=CARTESIAN_POINT('Ctrl Pts',(2.76101407199994,5.2,-3.14668961000002));
#353930=CARTESIAN_POINT('Ctrl Pts',(2.76101407199994,2.2,-3.14668961000002));
#353931=CARTESIAN_POINT('Ctrl Pts',(2.76227403799994,12.2,-3.14745433500002));
#353932=CARTESIAN_POINT('Ctrl Pts',(2.76227403799994,5.2,-3.14745433500002));
#353933=CARTESIAN_POINT('Ctrl Pts',(2.76227403799994,2.2,-3.14745433500002));
#353934=CARTESIAN_POINT('Ctrl Pts',(2.76353896199995,12.2,-3.14822004300002));
#353935=CARTESIAN_POINT('Ctrl Pts',(2.76353896199995,5.2,-3.14822004300002));
#353936=CARTESIAN_POINT('Ctrl Pts',(2.76353896199995,2.2,-3.14822004300002));
#353937=CARTESIAN_POINT('Ctrl Pts',(2.76480884399994,12.2,-3.14898672000002));
#353938=CARTESIAN_POINT('Ctrl Pts',(2.76480884399994,5.2,-3.14898672000002));
#353939=CARTESIAN_POINT('Ctrl Pts',(2.76480884399994,2.2,-3.14898672000002));
#353940=CARTESIAN_POINT('Ctrl Pts',(2.76608367999994,12.2,-3.14975435300001));
#353941=CARTESIAN_POINT('Ctrl Pts',(2.76608367999994,5.2,-3.14975435300001));
#353942=CARTESIAN_POINT('Ctrl Pts',(2.76608367999994,2.2,-3.14975435300001));
#353943=CARTESIAN_POINT('Ctrl Pts',(2.76736346799995,12.2,-3.15052293000001));
#353944=CARTESIAN_POINT('Ctrl Pts',(2.76736346799995,5.2,-3.15052293000001));
#353945=CARTESIAN_POINT('Ctrl Pts',(2.76736346799995,2.2,-3.15052293000001));
#353946=CARTESIAN_POINT('Ctrl Pts',(2.76864820699994,12.2,-3.15129243700001));
#353947=CARTESIAN_POINT('Ctrl Pts',(2.76864820699994,5.2,-3.15129243700001));
#353948=CARTESIAN_POINT('Ctrl Pts',(2.76864820699994,2.2,-3.15129243700001));
#353949=CARTESIAN_POINT('Ctrl Pts',(2.76993789399994,12.2,-3.15206286000001));
#353950=CARTESIAN_POINT('Ctrl Pts',(2.76993789399994,5.2,-3.15206286000001));
#353951=CARTESIAN_POINT('Ctrl Pts',(2.76993789399994,2.2,-3.15206286000001));
#353952=CARTESIAN_POINT('Ctrl Pts',(2.77123252699994,12.2,-3.15283418700002));
#353953=CARTESIAN_POINT('Ctrl Pts',(2.77123252699994,5.2,-3.15283418700002));
#353954=CARTESIAN_POINT('Ctrl Pts',(2.77123252699994,2.2,-3.15283418700002));
#353955=CARTESIAN_POINT('Ctrl Pts',(2.77253210399994,12.2,-3.15360640400002));
#353956=CARTESIAN_POINT('Ctrl Pts',(2.77253210399994,5.2,-3.15360640400002));
#353957=CARTESIAN_POINT('Ctrl Pts',(2.77253210399994,2.2,-3.15360640400002));
#353958=CARTESIAN_POINT('Ctrl Pts',(2.77383662199994,12.2,-3.15437949900002));
#353959=CARTESIAN_POINT('Ctrl Pts',(2.77383662199994,5.2,-3.15437949900002));
#353960=CARTESIAN_POINT('Ctrl Pts',(2.77383662199994,2.2,-3.15437949900002));
#353961=CARTESIAN_POINT('Ctrl Pts',(2.77514607899994,12.2,-3.15515345800002));
#353962=CARTESIAN_POINT('Ctrl Pts',(2.77514607899994,5.2,-3.15515345800002));
#353963=CARTESIAN_POINT('Ctrl Pts',(2.77514607899994,2.2,-3.15515345800002));
#353964=CARTESIAN_POINT('Ctrl Pts',(2.77646047299994,12.2,-3.15592826800001));
#353965=CARTESIAN_POINT('Ctrl Pts',(2.77646047299994,5.2,-3.15592826800001));
#353966=CARTESIAN_POINT('Ctrl Pts',(2.77646047299994,2.2,-3.15592826800001));
#353967=CARTESIAN_POINT('Ctrl Pts',(2.77777980199994,12.2,-3.15670391700001));
#353968=CARTESIAN_POINT('Ctrl Pts',(2.77777980199994,5.2,-3.15670391700001));
#353969=CARTESIAN_POINT('Ctrl Pts',(2.77777980199994,2.2,-3.15670391700001));
#353970=CARTESIAN_POINT('Ctrl Pts',(2.77910406199994,12.2,-3.15748039100002));
#353971=CARTESIAN_POINT('Ctrl Pts',(2.77910406199994,5.2,-3.15748039100002));
#353972=CARTESIAN_POINT('Ctrl Pts',(2.77910406199994,2.2,-3.15748039100002));
#353973=CARTESIAN_POINT('Ctrl Pts',(2.78043325399994,12.2,-3.15825767700002));
#353974=CARTESIAN_POINT('Ctrl Pts',(2.78043325399994,5.2,-3.15825767700002));
#353975=CARTESIAN_POINT('Ctrl Pts',(2.78043325399994,2.2,-3.15825767700002));
#353976=CARTESIAN_POINT('Ctrl Pts',(2.78176737199994,12.2,-3.15903576300002));
#353977=CARTESIAN_POINT('Ctrl Pts',(2.78176737199994,5.2,-3.15903576300002));
#353978=CARTESIAN_POINT('Ctrl Pts',(2.78176737199994,2.2,-3.15903576300002));
#353979=CARTESIAN_POINT('Ctrl Pts',(2.78310641599994,12.2,-3.15981463500002));
#353980=CARTESIAN_POINT('Ctrl Pts',(2.78310641599994,5.2,-3.15981463500002));
#353981=CARTESIAN_POINT('Ctrl Pts',(2.78310641599994,2.2,-3.15981463500002));
#353982=CARTESIAN_POINT('Ctrl Pts',(2.78445038299994,12.2,-3.16059428000001));
#353983=CARTESIAN_POINT('Ctrl Pts',(2.78445038299994,5.2,-3.16059428000001));
#353984=CARTESIAN_POINT('Ctrl Pts',(2.78445038299994,2.2,-3.16059428000001));
#353985=CARTESIAN_POINT('Ctrl Pts',(2.78579926999994,12.2,-3.16137468700001));
#353986=CARTESIAN_POINT('Ctrl Pts',(2.78579926999994,5.2,-3.16137468700001));
#353987=CARTESIAN_POINT('Ctrl Pts',(2.78579926999994,2.2,-3.16137468700001));
#353988=CARTESIAN_POINT('Ctrl Pts',(2.78715307499994,12.2,-3.16215584200001));
#353989=CARTESIAN_POINT('Ctrl Pts',(2.78715307499994,5.2,-3.16215584200001));
#353990=CARTESIAN_POINT('Ctrl Pts',(2.78715307499994,2.2,-3.16215584200001));
#353991=CARTESIAN_POINT('Ctrl Pts',(2.78851179699994,12.2,-3.16293773100002));
#353992=CARTESIAN_POINT('Ctrl Pts',(2.78851179699994,5.2,-3.16293773100002));
#353993=CARTESIAN_POINT('Ctrl Pts',(2.78851179699994,2.2,-3.16293773100002));
#353994=CARTESIAN_POINT('Ctrl Pts',(2.78987543099994,12.2,-3.16372034300001));
#353995=CARTESIAN_POINT('Ctrl Pts',(2.78987543099994,5.2,-3.16372034300001));
#353996=CARTESIAN_POINT('Ctrl Pts',(2.78987543099994,2.2,-3.16372034300001));
#353997=CARTESIAN_POINT('Ctrl Pts',(2.79124397599994,12.2,-3.16450366500002));
#353998=CARTESIAN_POINT('Ctrl Pts',(2.79124397599994,5.2,-3.16450366500002));
#353999=CARTESIAN_POINT('Ctrl Pts',(2.79124397599994,2.2,-3.16450366500002));
#354000=CARTESIAN_POINT('Ctrl Pts',(2.79261742999994,12.2,-3.16528768500001));
#354001=CARTESIAN_POINT('Ctrl Pts',(2.79261742999994,5.2,-3.16528768500001));
#354002=CARTESIAN_POINT('Ctrl Pts',(2.79261742999994,2.2,-3.16528768500001));
#354003=CARTESIAN_POINT('Ctrl Pts',(2.79399578999994,12.2,-3.16607238700001));
#354004=CARTESIAN_POINT('Ctrl Pts',(2.79399578999994,5.2,-3.16607238700001));
#354005=CARTESIAN_POINT('Ctrl Pts',(2.79399578999994,2.2,-3.16607238700001));
#354006=CARTESIAN_POINT('Ctrl Pts',(2.79537905499994,12.2,-3.16685776300002));
#354007=CARTESIAN_POINT('Ctrl Pts',(2.79537905499994,5.2,-3.16685776300002));
#354008=CARTESIAN_POINT('Ctrl Pts',(2.79537905499994,2.2,-3.16685776300002));
#354009=CARTESIAN_POINT('Ctrl Pts',(2.79676721799994,12.2,-3.16764379600002));
#354010=CARTESIAN_POINT('Ctrl Pts',(2.79676721799994,5.2,-3.16764379600002));
#354011=CARTESIAN_POINT('Ctrl Pts',(2.79676721799994,2.2,-3.16764379600002));
#354012=CARTESIAN_POINT('Ctrl Pts',(2.79816028199994,12.2,-3.16843047700001));
#354013=CARTESIAN_POINT('Ctrl Pts',(2.79816028199994,5.2,-3.16843047700001));
#354014=CARTESIAN_POINT('Ctrl Pts',(2.79816028199994,2.2,-3.16843047700001));
#354015=CARTESIAN_POINT('Ctrl Pts',(2.79955824199994,12.2,-3.16921779200001));
#354016=CARTESIAN_POINT('Ctrl Pts',(2.79955824199994,5.2,-3.16921779200001));
#354017=CARTESIAN_POINT('Ctrl Pts',(2.79955824199994,2.2,-3.16921779200001));
#354018=CARTESIAN_POINT('Ctrl Pts',(2.80096109499994,12.2,-3.17000572800001));
#354019=CARTESIAN_POINT('Ctrl Pts',(2.80096109499994,5.2,-3.17000572800001));
#354020=CARTESIAN_POINT('Ctrl Pts',(2.80096109499994,2.2,-3.17000572800001));
#354021=CARTESIAN_POINT('Ctrl Pts',(2.80236883999994,12.2,-3.17079427300001));
#354022=CARTESIAN_POINT('Ctrl Pts',(2.80236883999994,5.2,-3.17079427300001));
#354023=CARTESIAN_POINT('Ctrl Pts',(2.80236883999994,2.2,-3.17079427300001));
#354024=CARTESIAN_POINT('Ctrl Pts',(2.80378147399994,12.2,-3.17158341500001));
#354025=CARTESIAN_POINT('Ctrl Pts',(2.80378147399994,5.2,-3.17158341500001));
#354026=CARTESIAN_POINT('Ctrl Pts',(2.80378147399994,2.2,-3.17158341500001));
#354027=CARTESIAN_POINT('Ctrl Pts',(2.80519899199994,12.2,-3.17237314000002));
#354028=CARTESIAN_POINT('Ctrl Pts',(2.80519899199994,5.2,-3.17237314000002));
#354029=CARTESIAN_POINT('Ctrl Pts',(2.80519899199994,2.2,-3.17237314000002));
#354030=CARTESIAN_POINT('Ctrl Pts',(2.80662139499994,12.2,-3.17316343700002));
#354031=CARTESIAN_POINT('Ctrl Pts',(2.80662139499994,5.2,-3.17316343700002));
#354032=CARTESIAN_POINT('Ctrl Pts',(2.80662139499994,2.2,-3.17316343700002));
#354033=CARTESIAN_POINT('Ctrl Pts',(2.80804867999994,12.2,-3.17395429300001));
#354034=CARTESIAN_POINT('Ctrl Pts',(2.80804867999994,5.2,-3.17395429300001));
#354035=CARTESIAN_POINT('Ctrl Pts',(2.80804867999994,2.2,-3.17395429300001));
#354036=CARTESIAN_POINT('Ctrl Pts',(2.80948084099994,12.2,-3.17474569600002));
#354037=CARTESIAN_POINT('Ctrl Pts',(2.80948084099994,5.2,-3.17474569600002));
#354038=CARTESIAN_POINT('Ctrl Pts',(2.80948084099994,2.2,-3.17474569600002));
#354039=CARTESIAN_POINT('Ctrl Pts',(2.81091787999994,12.2,-3.17553763400001));
#354040=CARTESIAN_POINT('Ctrl Pts',(2.81091787999994,5.2,-3.17553763400001));
#354041=CARTESIAN_POINT('Ctrl Pts',(2.81091787999994,2.2,-3.17553763400001));
#354042=CARTESIAN_POINT('Ctrl Pts',(2.81235979099994,12.2,-3.17633009400001));
#354043=CARTESIAN_POINT('Ctrl Pts',(2.81235979099994,5.2,-3.17633009400001));
#354044=CARTESIAN_POINT('Ctrl Pts',(2.81235979099994,2.2,-3.17633009400001));
#354045=CARTESIAN_POINT('Ctrl Pts',(2.81380657399994,12.2,-3.17712306300002));
#354046=CARTESIAN_POINT('Ctrl Pts',(2.81380657399994,5.2,-3.17712306300002));
#354047=CARTESIAN_POINT('Ctrl Pts',(2.81380657399994,2.2,-3.17712306300002));
#354048=CARTESIAN_POINT('Ctrl Pts',(2.81525822399994,12.2,-3.17791653100001));
#354049=CARTESIAN_POINT('Ctrl Pts',(2.81525822399994,5.2,-3.17791653100001));
#354050=CARTESIAN_POINT('Ctrl Pts',(2.81525822399994,2.2,-3.17791653100001));
#354051=CARTESIAN_POINT('Ctrl Pts',(2.81671473899994,12.2,-3.17871048300002));
#354052=CARTESIAN_POINT('Ctrl Pts',(2.81671473899994,5.2,-3.17871048300002));
#354053=CARTESIAN_POINT('Ctrl Pts',(2.81671473899994,2.2,-3.17871048300002));
#354054=CARTESIAN_POINT('Ctrl Pts',(2.81817611699994,12.2,-3.17950490900001));
#354055=CARTESIAN_POINT('Ctrl Pts',(2.81817611699994,5.2,-3.17950490900001));
#354056=CARTESIAN_POINT('Ctrl Pts',(2.81817611699994,2.2,-3.17950490900001));
#354057=CARTESIAN_POINT('Ctrl Pts',(2.81964235599995,12.2,-3.18029979600002));
#354058=CARTESIAN_POINT('Ctrl Pts',(2.81964235599995,5.2,-3.18029979600002));
#354059=CARTESIAN_POINT('Ctrl Pts',(2.81964235599995,2.2,-3.18029979600002));
#354060=CARTESIAN_POINT('Ctrl Pts',(2.82111345099994,12.2,-3.18109513200001));
#354061=CARTESIAN_POINT('Ctrl Pts',(2.82111345099994,5.2,-3.18109513200001));
#354062=CARTESIAN_POINT('Ctrl Pts',(2.82111345099994,2.2,-3.18109513200001));
#354063=CARTESIAN_POINT('Ctrl Pts',(2.82258940099994,12.2,-3.18189090400002));
#354064=CARTESIAN_POINT('Ctrl Pts',(2.82258940099994,5.2,-3.18189090400002));
#354065=CARTESIAN_POINT('Ctrl Pts',(2.82258940099994,2.2,-3.18189090400002));
#354066=CARTESIAN_POINT('Ctrl Pts',(2.82407020299994,12.2,-3.18268710200002));
#354067=CARTESIAN_POINT('Ctrl Pts',(2.82407020299994,5.2,-3.18268710200002));
#354068=CARTESIAN_POINT('Ctrl Pts',(2.82407020299994,2.2,-3.18268710200002));
#354069=CARTESIAN_POINT('Ctrl Pts',(2.82555585599995,12.2,-3.18348371100001));
#354070=CARTESIAN_POINT('Ctrl Pts',(2.82555585599995,5.2,-3.18348371100001));
#354071=CARTESIAN_POINT('Ctrl Pts',(2.82555585599995,2.2,-3.18348371100001));
#354072=CARTESIAN_POINT('Ctrl Pts',(2.82704635399994,12.2,-3.18428072100001));
#354073=CARTESIAN_POINT('Ctrl Pts',(2.82704635399994,5.2,-3.18428072100001));
#354074=CARTESIAN_POINT('Ctrl Pts',(2.82704635399994,2.2,-3.18428072100001));
#354075=CARTESIAN_POINT('Ctrl Pts',(2.82854169599994,12.2,-3.18507812000002));
#354076=CARTESIAN_POINT('Ctrl Pts',(2.82854169599994,5.2,-3.18507812000002));
#354077=CARTESIAN_POINT('Ctrl Pts',(2.82854169599994,2.2,-3.18507812000002));
#354078=CARTESIAN_POINT('Ctrl Pts',(2.83004187899994,12.2,-3.18587589500002));
#354079=CARTESIAN_POINT('Ctrl Pts',(2.83004187899994,5.2,-3.18587589500002));
#354080=CARTESIAN_POINT('Ctrl Pts',(2.83004187899994,2.2,-3.18587589500002));
#354081=CARTESIAN_POINT('Ctrl Pts',(2.83154690099995,12.2,-3.18667403500001));
#354082=CARTESIAN_POINT('Ctrl Pts',(2.83154690099995,5.2,-3.18667403500001));
#354083=CARTESIAN_POINT('Ctrl Pts',(2.83154690099995,2.2,-3.18667403500001));
#354084=CARTESIAN_POINT('Ctrl Pts',(2.83305675899994,12.2,-3.18747252700001));
#354085=CARTESIAN_POINT('Ctrl Pts',(2.83305675899994,5.2,-3.18747252700001));
#354086=CARTESIAN_POINT('Ctrl Pts',(2.83305675899994,2.2,-3.18747252700001));
#354087=CARTESIAN_POINT('Ctrl Pts',(2.83457144899995,12.2,-3.18827136000001));
#354088=CARTESIAN_POINT('Ctrl Pts',(2.83457144899995,5.2,-3.18827136000001));
#354089=CARTESIAN_POINT('Ctrl Pts',(2.83457144899995,2.2,-3.18827136000001));
#354090=CARTESIAN_POINT('Ctrl Pts',(2.83609096999994,12.2,-3.18907052200001));
#354091=CARTESIAN_POINT('Ctrl Pts',(2.83609096999994,5.2,-3.18907052200001));
#354092=CARTESIAN_POINT('Ctrl Pts',(2.83609096999994,2.2,-3.18907052200001));
#354093=CARTESIAN_POINT('Ctrl Pts',(2.83761531699994,12.2,-3.18987000000002));
#354094=CARTESIAN_POINT('Ctrl Pts',(2.83761531699994,5.2,-3.18987000000002));
#354095=CARTESIAN_POINT('Ctrl Pts',(2.83761531699994,2.2,-3.18987000000002));
#354096=CARTESIAN_POINT('Ctrl Pts',(2.83914448999994,12.2,-3.19066978400001));
#354097=CARTESIAN_POINT('Ctrl Pts',(2.83914448999994,5.2,-3.19066978400001));
#354098=CARTESIAN_POINT('Ctrl Pts',(2.83914448999994,2.2,-3.19066978400001));
#354099=CARTESIAN_POINT('Ctrl Pts',(2.84067848399994,12.2,-3.19146986100002));
#354100=CARTESIAN_POINT('Ctrl Pts',(2.84067848399994,5.2,-3.19146986100002));
#354101=CARTESIAN_POINT('Ctrl Pts',(2.84067848399994,2.2,-3.19146986100002));
#354102=CARTESIAN_POINT('Ctrl Pts',(2.84221729699994,12.2,-3.19227021900002));
#354103=CARTESIAN_POINT('Ctrl Pts',(2.84221729699994,5.2,-3.19227021900002));
#354104=CARTESIAN_POINT('Ctrl Pts',(2.84221729699994,2.2,-3.19227021900002));
#354105=CARTESIAN_POINT('Ctrl Pts',(2.84376092599994,12.2,-3.19307084600001));
#354106=CARTESIAN_POINT('Ctrl Pts',(2.84376092599994,5.2,-3.19307084600001));
#354107=CARTESIAN_POINT('Ctrl Pts',(2.84376092599994,2.2,-3.19307084600001));
#354108=CARTESIAN_POINT('Ctrl Pts',(2.84530936799994,12.2,-3.19387173300001));
#354109=CARTESIAN_POINT('Ctrl Pts',(2.84530936799994,5.2,-3.19387173300001));
#354110=CARTESIAN_POINT('Ctrl Pts',(2.84530936799994,2.2,-3.19387173300001));
#354111=CARTESIAN_POINT('Ctrl Pts',(2.84686261999994,12.2,-3.19467286400001));
#354112=CARTESIAN_POINT('Ctrl Pts',(2.84686261999994,5.2,-3.19467286400001));
#354113=CARTESIAN_POINT('Ctrl Pts',(2.84686261999994,2.2,-3.19467286400001));
#354114=CARTESIAN_POINT('Ctrl Pts',(2.84842067999994,12.2,-3.19547423000001));
#354115=CARTESIAN_POINT('Ctrl Pts',(2.84842067999994,5.2,-3.19547423000001));
#354116=CARTESIAN_POINT('Ctrl Pts',(2.84842067999994,2.2,-3.19547423000001));
#354117=CARTESIAN_POINT('Ctrl Pts',(2.84998354499994,12.2,-3.19627582000001));
#354118=CARTESIAN_POINT('Ctrl Pts',(2.84998354499994,5.2,-3.19627582000001));
#354119=CARTESIAN_POINT('Ctrl Pts',(2.84998354499994,2.2,-3.19627582000001));
#354120=CARTESIAN_POINT('Ctrl Pts',(2.85155121099995,12.2,-3.19707762000002));
#354121=CARTESIAN_POINT('Ctrl Pts',(2.85155121099995,5.2,-3.19707762000002));
#354122=CARTESIAN_POINT('Ctrl Pts',(2.85155121099995,2.2,-3.19707762000002));
#354123=CARTESIAN_POINT('Ctrl Pts',(2.85312367599994,12.2,-3.19787962000001));
#354124=CARTESIAN_POINT('Ctrl Pts',(2.85312367599994,5.2,-3.19787962000001));
#354125=CARTESIAN_POINT('Ctrl Pts',(2.85312367599994,2.2,-3.19787962000001));
#354126=CARTESIAN_POINT('Ctrl Pts',(2.85470093699994,12.2,-3.19868180800002));
#354127=CARTESIAN_POINT('Ctrl Pts',(2.85470093699994,5.2,-3.19868180800002));
#354128=CARTESIAN_POINT('Ctrl Pts',(2.85470093699994,2.2,-3.19868180800002));
#354129=CARTESIAN_POINT('Ctrl Pts',(2.85628299099994,12.2,-3.19948417200001));
#354130=CARTESIAN_POINT('Ctrl Pts',(2.85628299099994,5.2,-3.19948417200001));
#354131=CARTESIAN_POINT('Ctrl Pts',(2.85628299099994,2.2,-3.19948417200001));
#354132=CARTESIAN_POINT('Ctrl Pts',(2.85786983499994,12.2,-3.20028670200001));
#354133=CARTESIAN_POINT('Ctrl Pts',(2.85786983499994,5.2,-3.20028670200001));
#354134=CARTESIAN_POINT('Ctrl Pts',(2.85786983499994,2.2,-3.20028670200001));
#354135=CARTESIAN_POINT('Ctrl Pts',(2.85946146699994,12.2,-3.20108938400002));
#354136=CARTESIAN_POINT('Ctrl Pts',(2.85946146699994,5.2,-3.20108938400002));
#354137=CARTESIAN_POINT('Ctrl Pts',(2.85946146699994,2.2,-3.20108938400002));
#354138=CARTESIAN_POINT('Ctrl Pts',(2.86105788299994,12.2,-3.20189220800001));
#354139=CARTESIAN_POINT('Ctrl Pts',(2.86105788299994,5.2,-3.20189220800001));
#354140=CARTESIAN_POINT('Ctrl Pts',(2.86105788299994,2.2,-3.20189220800001));
#354141=CARTESIAN_POINT('Ctrl Pts',(2.86265907899995,12.2,-3.20269516300002));
#354142=CARTESIAN_POINT('Ctrl Pts',(2.86265907899995,5.2,-3.20269516300002));
#354143=CARTESIAN_POINT('Ctrl Pts',(2.86265907899995,2.2,-3.20269516300002));
#354144=CARTESIAN_POINT('Ctrl Pts',(2.86426505399994,12.2,-3.20349823600001));
#354145=CARTESIAN_POINT('Ctrl Pts',(2.86426505399994,5.2,-3.20349823600001));
#354146=CARTESIAN_POINT('Ctrl Pts',(2.86426505399994,2.2,-3.20349823600001));
#354147=CARTESIAN_POINT('Ctrl Pts',(2.86587580399994,12.2,-3.20430141700002));
#354148=CARTESIAN_POINT('Ctrl Pts',(2.86587580399994,5.2,-3.20430141700002));
#354149=CARTESIAN_POINT('Ctrl Pts',(2.86587580399994,2.2,-3.20430141700002));
#354150=CARTESIAN_POINT('Ctrl Pts',(2.86749132599994,12.2,-3.20510469500002));
#354151=CARTESIAN_POINT('Ctrl Pts',(2.86749132599994,5.2,-3.20510469500002));
#354152=CARTESIAN_POINT('Ctrl Pts',(2.86749132599994,2.2,-3.20510469500002));
#354153=CARTESIAN_POINT('Ctrl Pts',(2.86911161699994,12.2,-3.20590805700002));
#354154=CARTESIAN_POINT('Ctrl Pts',(2.86911161699994,5.2,-3.20590805700002));
#354155=CARTESIAN_POINT('Ctrl Pts',(2.86911161699994,2.2,-3.20590805700002));
#354156=CARTESIAN_POINT('Ctrl Pts',(2.87073667499994,12.2,-3.20671149100002));
#354157=CARTESIAN_POINT('Ctrl Pts',(2.87073667499994,5.2,-3.20671149100002));
#354158=CARTESIAN_POINT('Ctrl Pts',(2.87073667499994,2.2,-3.20671149100002));
#354159=CARTESIAN_POINT('Ctrl Pts',(2.87236649699994,12.2,-3.20751498800002));
#354160=CARTESIAN_POINT('Ctrl Pts',(2.87236649699994,5.2,-3.20751498800002));
#354161=CARTESIAN_POINT('Ctrl Pts',(2.87236649699994,2.2,-3.20751498800002));
#354162=CARTESIAN_POINT('Ctrl Pts',(2.87400107799994,12.2,-3.20831853700001));
#354163=CARTESIAN_POINT('Ctrl Pts',(2.87400107799994,5.2,-3.20831853700001));
#354164=CARTESIAN_POINT('Ctrl Pts',(2.87400107799994,2.2,-3.20831853700001));
#354165=CARTESIAN_POINT('Ctrl Pts',(2.87564041599994,12.2,-3.20912212400001));
#354166=CARTESIAN_POINT('Ctrl Pts',(2.87564041599994,5.2,-3.20912212400001));
#354167=CARTESIAN_POINT('Ctrl Pts',(2.87564041599994,2.2,-3.20912212400001));
#354168=CARTESIAN_POINT('Ctrl Pts',(2.87728450899994,12.2,-3.20992574000002));
#354169=CARTESIAN_POINT('Ctrl Pts',(2.87728450899994,5.2,-3.20992574000002));
#354170=CARTESIAN_POINT('Ctrl Pts',(2.87728450899994,2.2,-3.20992574000002));
#354171=CARTESIAN_POINT('Ctrl Pts',(2.87893335299994,12.2,-3.21072937300002));
#354172=CARTESIAN_POINT('Ctrl Pts',(2.87893335299994,5.2,-3.21072937300002));
#354173=CARTESIAN_POINT('Ctrl Pts',(2.87893335299994,2.2,-3.21072937300002));
#354174=CARTESIAN_POINT('Ctrl Pts',(2.88058694399994,12.2,-3.21153301100002));
#354175=CARTESIAN_POINT('Ctrl Pts',(2.88058694399994,5.2,-3.21153301100002));
#354176=CARTESIAN_POINT('Ctrl Pts',(2.88058694399994,2.2,-3.21153301100002));
#354177=CARTESIAN_POINT('Ctrl Pts',(2.88224527999994,12.2,-3.21233664400001));
#354178=CARTESIAN_POINT('Ctrl Pts',(2.88224527999994,5.2,-3.21233664400001));
#354179=CARTESIAN_POINT('Ctrl Pts',(2.88224527999994,2.2,-3.21233664400001));
#354180=CARTESIAN_POINT('Ctrl Pts',(2.88390835799994,12.2,-3.21314026000001));
#354181=CARTESIAN_POINT('Ctrl Pts',(2.88390835799994,5.2,-3.21314026000001));
#354182=CARTESIAN_POINT('Ctrl Pts',(2.88390835799994,2.2,-3.21314026000001));
#354183=CARTESIAN_POINT('Ctrl Pts',(2.88557617499994,12.2,-3.21394384900001));
#354184=CARTESIAN_POINT('Ctrl Pts',(2.88557617499994,5.2,-3.21394384900001));
#354185=CARTESIAN_POINT('Ctrl Pts',(2.88557617499994,2.2,-3.21394384900001));
#354186=CARTESIAN_POINT('Ctrl Pts',(2.88724872799994,12.2,-3.21474739800002));
#354187=CARTESIAN_POINT('Ctrl Pts',(2.88724872799994,5.2,-3.21474739800002));
#354188=CARTESIAN_POINT('Ctrl Pts',(2.88724872799994,2.2,-3.21474739800002));
#354189=CARTESIAN_POINT('Ctrl Pts',(2.88892601299994,12.2,-3.21555089800002));
#354190=CARTESIAN_POINT('Ctrl Pts',(2.88892601299994,5.2,-3.21555089800002));
#354191=CARTESIAN_POINT('Ctrl Pts',(2.88892601299994,2.2,-3.21555089800002));
#354192=CARTESIAN_POINT('Ctrl Pts',(2.89060802699994,12.2,-3.21635433700001));
#354193=CARTESIAN_POINT('Ctrl Pts',(2.89060802699994,5.2,-3.21635433700001));
#354194=CARTESIAN_POINT('Ctrl Pts',(2.89060802699994,2.2,-3.21635433700001));
#354195=CARTESIAN_POINT('Ctrl Pts',(2.89229476699994,12.2,-3.21715770300001));
#354196=CARTESIAN_POINT('Ctrl Pts',(2.89229476699994,5.2,-3.21715770300001));
#354197=CARTESIAN_POINT('Ctrl Pts',(2.89229476699994,2.2,-3.21715770300001));
#354198=CARTESIAN_POINT('Ctrl Pts',(2.89398623099994,12.2,-3.21796098700001));
#354199=CARTESIAN_POINT('Ctrl Pts',(2.89398623099994,5.2,-3.21796098700001));
#354200=CARTESIAN_POINT('Ctrl Pts',(2.89398623099994,2.2,-3.21796098700001));
#354201=CARTESIAN_POINT('Ctrl Pts',(2.89568241399994,12.2,-3.21876417600001));
#354202=CARTESIAN_POINT('Ctrl Pts',(2.89568241399994,5.2,-3.21876417600001));
#354203=CARTESIAN_POINT('Ctrl Pts',(2.89568241399994,2.2,-3.21876417600001));
#354204=CARTESIAN_POINT('Ctrl Pts',(2.89738331399994,12.2,-3.21956726100002));
#354205=CARTESIAN_POINT('Ctrl Pts',(2.89738331399994,5.2,-3.21956726100002));
#354206=CARTESIAN_POINT('Ctrl Pts',(2.89738331399994,2.2,-3.21956726100002));
#354207=CARTESIAN_POINT('Ctrl Pts',(2.89908892699994,12.2,-3.22037022900002));
#354208=CARTESIAN_POINT('Ctrl Pts',(2.89908892699994,5.2,-3.22037022900002));
#354209=CARTESIAN_POINT('Ctrl Pts',(2.89908892699994,2.2,-3.22037022900002));
#354210=CARTESIAN_POINT('Ctrl Pts',(2.90079925099994,12.2,-3.22117307100001));
#354211=CARTESIAN_POINT('Ctrl Pts',(2.90079925099994,5.2,-3.22117307100001));
#354212=CARTESIAN_POINT('Ctrl Pts',(2.90079925099994,2.2,-3.22117307100001));
#354213=CARTESIAN_POINT('Ctrl Pts',(2.90251428199995,12.2,-3.22197577400001));
#354214=CARTESIAN_POINT('Ctrl Pts',(2.90251428199995,5.2,-3.22197577400001));
#354215=CARTESIAN_POINT('Ctrl Pts',(2.90251428199995,2.2,-3.22197577400001));
#354216=CARTESIAN_POINT('Ctrl Pts',(2.90423401699994,12.2,-3.22277832900001));
#354217=CARTESIAN_POINT('Ctrl Pts',(2.90423401699994,5.2,-3.22277832900001));
#354218=CARTESIAN_POINT('Ctrl Pts',(2.90423401699994,2.2,-3.22277832900001));
#354219=CARTESIAN_POINT('Ctrl Pts',(2.90595845199995,12.2,-3.22358072300001));
#354220=CARTESIAN_POINT('Ctrl Pts',(2.90595845199995,5.2,-3.22358072300001));
#354221=CARTESIAN_POINT('Ctrl Pts',(2.90595845199995,2.2,-3.22358072300001));
#354222=CARTESIAN_POINT('Ctrl Pts',(2.90768758499994,12.2,-3.22438294800001));
#354223=CARTESIAN_POINT('Ctrl Pts',(2.90768758499994,5.2,-3.22438294800001));
#354224=CARTESIAN_POINT('Ctrl Pts',(2.90768758499994,2.2,-3.22438294800001));
#354225=CARTESIAN_POINT('Ctrl Pts',(2.90942141199994,12.2,-3.22518499100001));
#354226=CARTESIAN_POINT('Ctrl Pts',(2.90942141199994,5.2,-3.22518499100001));
#354227=CARTESIAN_POINT('Ctrl Pts',(2.90942141199994,2.2,-3.22518499100001));
#354228=CARTESIAN_POINT('Ctrl Pts',(2.91115992999994,12.2,-3.22598684300001));
#354229=CARTESIAN_POINT('Ctrl Pts',(2.91115992999994,5.2,-3.22598684300001));
#354230=CARTESIAN_POINT('Ctrl Pts',(2.91115992999994,2.2,-3.22598684300001));
#354231=CARTESIAN_POINT('Ctrl Pts',(2.91290313599994,12.2,-3.22678849200001));
#354232=CARTESIAN_POINT('Ctrl Pts',(2.91290313599994,5.2,-3.22678849200001));
#354233=CARTESIAN_POINT('Ctrl Pts',(2.91290313599994,2.2,-3.22678849200001));
#354234=CARTESIAN_POINT('Ctrl Pts',(2.91465102699994,12.2,-3.22758992600002));
#354235=CARTESIAN_POINT('Ctrl Pts',(2.91465102699994,5.2,-3.22758992600002));
#354236=CARTESIAN_POINT('Ctrl Pts',(2.91465102699994,2.2,-3.22758992600002));
#354237=CARTESIAN_POINT('Ctrl Pts',(2.91640359899994,12.2,-3.22839113700002));
#354238=CARTESIAN_POINT('Ctrl Pts',(2.91640359899994,5.2,-3.22839113700002));
#354239=CARTESIAN_POINT('Ctrl Pts',(2.91640359899994,2.2,-3.22839113700002));
#354240=CARTESIAN_POINT('Ctrl Pts',(2.91816084799994,12.2,-3.22919211200002));
#354241=CARTESIAN_POINT('Ctrl Pts',(2.91816084799994,5.2,-3.22919211200002));
#354242=CARTESIAN_POINT('Ctrl Pts',(2.91816084799994,2.2,-3.22919211200002));
#354243=CARTESIAN_POINT('Ctrl Pts',(2.91992277299994,12.2,-3.22999284300002));
#354244=CARTESIAN_POINT('Ctrl Pts',(2.91992277299994,5.2,-3.22999284300002));
#354245=CARTESIAN_POINT('Ctrl Pts',(2.91992277299994,2.2,-3.22999284300002));
#354246=CARTESIAN_POINT('Ctrl Pts',(2.92168936799994,12.2,-3.23079331600002));
#354247=CARTESIAN_POINT('Ctrl Pts',(2.92168936799994,5.2,-3.23079331600002));
#354248=CARTESIAN_POINT('Ctrl Pts',(2.92168936799994,2.2,-3.23079331600002));
#354249=CARTESIAN_POINT('Ctrl Pts',(2.92346063199994,12.2,-3.23159352200001));
#354250=CARTESIAN_POINT('Ctrl Pts',(2.92346063199994,5.2,-3.23159352200001));
#354251=CARTESIAN_POINT('Ctrl Pts',(2.92346063199994,2.2,-3.23159352200001));
#354252=CARTESIAN_POINT('Ctrl Pts',(2.92523655999994,12.2,-3.23239345100002));
#354253=CARTESIAN_POINT('Ctrl Pts',(2.92523655999994,5.2,-3.23239345100002));
#354254=CARTESIAN_POINT('Ctrl Pts',(2.92523655999994,2.2,-3.23239345100002));
#354255=CARTESIAN_POINT('Ctrl Pts',(2.92701714899994,12.2,-3.23319309200001));
#354256=CARTESIAN_POINT('Ctrl Pts',(2.92701714899994,5.2,-3.23319309200001));
#354257=CARTESIAN_POINT('Ctrl Pts',(2.92701714899994,2.2,-3.23319309200001));
#354258=CARTESIAN_POINT('Ctrl Pts',(2.92880239599994,12.2,-3.23399243300001));
#354259=CARTESIAN_POINT('Ctrl Pts',(2.92880239599994,5.2,-3.23399243300001));
#354260=CARTESIAN_POINT('Ctrl Pts',(2.92880239599994,2.2,-3.23399243300001));
#354261=CARTESIAN_POINT('Ctrl Pts',(2.93059229899994,12.2,-3.23479146500001));
#354262=CARTESIAN_POINT('Ctrl Pts',(2.93059229899994,5.2,-3.23479146500001));
#354263=CARTESIAN_POINT('Ctrl Pts',(2.93059229899994,2.2,-3.23479146500001));
#354264=CARTESIAN_POINT('Ctrl Pts',(2.93238685199994,12.2,-3.23559017800001));
#354265=CARTESIAN_POINT('Ctrl Pts',(2.93238685199994,5.2,-3.23559017800001));
#354266=CARTESIAN_POINT('Ctrl Pts',(2.93238685199994,2.2,-3.23559017800001));
#354267=CARTESIAN_POINT('Ctrl Pts',(2.93418605299994,12.2,-3.23638855900001));
#354268=CARTESIAN_POINT('Ctrl Pts',(2.93418605299994,5.2,-3.23638855900001));
#354269=CARTESIAN_POINT('Ctrl Pts',(2.93418605299994,2.2,-3.23638855900001));
#354270=CARTESIAN_POINT('Ctrl Pts',(2.93598989899994,12.2,-3.23718660000001));
#354271=CARTESIAN_POINT('Ctrl Pts',(2.93598989899994,5.2,-3.23718660000001));
#354272=CARTESIAN_POINT('Ctrl Pts',(2.93598989899994,2.2,-3.23718660000001));
#354273=CARTESIAN_POINT('Ctrl Pts',(2.93779838599994,12.2,-3.23798429000002));
#354274=CARTESIAN_POINT('Ctrl Pts',(2.93779838599994,5.2,-3.23798429000002));
#354275=CARTESIAN_POINT('Ctrl Pts',(2.93779838599994,2.2,-3.23798429000002));
#354276=CARTESIAN_POINT('Ctrl Pts',(2.93961151099994,12.2,-3.23878161800002));
#354277=CARTESIAN_POINT('Ctrl Pts',(2.93961151099994,5.2,-3.23878161800002));
#354278=CARTESIAN_POINT('Ctrl Pts',(2.93961151099994,2.2,-3.23878161800002));
#354279=CARTESIAN_POINT('Ctrl Pts',(2.94142926999994,12.2,-3.23957857300002));
#354280=CARTESIAN_POINT('Ctrl Pts',(2.94142926999994,5.2,-3.23957857300002));
#354281=CARTESIAN_POINT('Ctrl Pts',(2.94142926999994,2.2,-3.23957857300002));
#354282=CARTESIAN_POINT('Ctrl Pts',(2.94325166099994,12.2,-3.24037514600001));
#354283=CARTESIAN_POINT('Ctrl Pts',(2.94325166099994,5.2,-3.24037514600001));
#354284=CARTESIAN_POINT('Ctrl Pts',(2.94325166099994,2.2,-3.24037514600001));
#354285=CARTESIAN_POINT('Ctrl Pts',(2.94507867899994,12.2,-3.24117132700001));
#354286=CARTESIAN_POINT('Ctrl Pts',(2.94507867899994,5.2,-3.24117132700001));
#354287=CARTESIAN_POINT('Ctrl Pts',(2.94507867899994,2.2,-3.24117132700001));
#354288=CARTESIAN_POINT('Ctrl Pts',(2.94691032199994,12.2,-3.24196710300001));
#354289=CARTESIAN_POINT('Ctrl Pts',(2.94691032199994,5.2,-3.24196710300001));
#354290=CARTESIAN_POINT('Ctrl Pts',(2.94691032199994,2.2,-3.24196710300001));
#354291=CARTESIAN_POINT('Ctrl Pts',(2.94874658399995,12.2,-3.24276246600002));
#354292=CARTESIAN_POINT('Ctrl Pts',(2.94874658399995,5.2,-3.24276246600002));
#354293=CARTESIAN_POINT('Ctrl Pts',(2.94874658399995,2.2,-3.24276246600002));
#354294=CARTESIAN_POINT('Ctrl Pts',(2.95058746399994,12.2,-3.24355740400001));
#354295=CARTESIAN_POINT('Ctrl Pts',(2.95058746399994,5.2,-3.24355740400001));
#354296=CARTESIAN_POINT('Ctrl Pts',(2.95058746399994,2.2,-3.24355740400001));
#354297=CARTESIAN_POINT('Ctrl Pts',(2.95243295799994,12.2,-3.24435190900001));
#354298=CARTESIAN_POINT('Ctrl Pts',(2.95243295799994,5.2,-3.24435190900001));
#354299=CARTESIAN_POINT('Ctrl Pts',(2.95243295799994,2.2,-3.24435190900001));
#354300=CARTESIAN_POINT('Ctrl Pts',(2.95428306199994,12.2,-3.24514596900002));
#354301=CARTESIAN_POINT('Ctrl Pts',(2.95428306199994,5.2,-3.24514596900002));
#354302=CARTESIAN_POINT('Ctrl Pts',(2.95428306199994,2.2,-3.24514596900002));
#354303=CARTESIAN_POINT('Ctrl Pts',(2.95613777399995,12.2,-3.24593957400001));
#354304=CARTESIAN_POINT('Ctrl Pts',(2.95613777399995,5.2,-3.24593957400001));
#354305=CARTESIAN_POINT('Ctrl Pts',(2.95613777399995,2.2,-3.24593957400001));
#354306=CARTESIAN_POINT('Ctrl Pts',(2.95799708799994,12.2,-3.24673271300002));
#354307=CARTESIAN_POINT('Ctrl Pts',(2.95799708799994,5.2,-3.24673271300002));
#354308=CARTESIAN_POINT('Ctrl Pts',(2.95799708799994,2.2,-3.24673271300002));
#354309=CARTESIAN_POINT('Ctrl Pts',(2.95986100299995,12.2,-3.24752537800002));
#354310=CARTESIAN_POINT('Ctrl Pts',(2.95986100299995,5.2,-3.24752537800002));
#354311=CARTESIAN_POINT('Ctrl Pts',(2.95986100299995,2.2,-3.24752537800002));
#354312=CARTESIAN_POINT('Ctrl Pts',(2.96172951299994,12.2,-3.24831755800002));
#354313=CARTESIAN_POINT('Ctrl Pts',(2.96172951299994,5.2,-3.24831755800002));
#354314=CARTESIAN_POINT('Ctrl Pts',(2.96172951299994,2.2,-3.24831755800002));
#354315=CARTESIAN_POINT('Ctrl Pts',(2.96360261799994,12.2,-3.24910924000001));
#354316=CARTESIAN_POINT('Ctrl Pts',(2.96360261799994,5.2,-3.24910924000001));
#354317=CARTESIAN_POINT('Ctrl Pts',(2.96360261799994,2.2,-3.24910924000001));
#354318=CARTESIAN_POINT('Ctrl Pts',(2.96548031099995,12.2,-3.24990041900001));
#354319=CARTESIAN_POINT('Ctrl Pts',(2.96548031099995,5.2,-3.24990041900001));
#354320=CARTESIAN_POINT('Ctrl Pts',(2.96548031099995,2.2,-3.24990041900001));
#354321=CARTESIAN_POINT('Ctrl Pts',(2.96736258999994,12.2,-3.25069108000001));
#354322=CARTESIAN_POINT('Ctrl Pts',(2.96736258999994,5.2,-3.25069108000001));
#354323=CARTESIAN_POINT('Ctrl Pts',(2.96736258999994,2.2,-3.25069108000001));
#354324=CARTESIAN_POINT('Ctrl Pts',(2.96924945199994,12.2,-3.25148121500002));
#354325=CARTESIAN_POINT('Ctrl Pts',(2.96924945199994,5.2,-3.25148121500002));
#354326=CARTESIAN_POINT('Ctrl Pts',(2.96924945199994,2.2,-3.25148121500002));
#354327=CARTESIAN_POINT('Ctrl Pts',(2.97114089099995,12.2,-3.25227081400001));
#354328=CARTESIAN_POINT('Ctrl Pts',(2.97114089099995,5.2,-3.25227081400001));
#354329=CARTESIAN_POINT('Ctrl Pts',(2.97114089099995,2.2,-3.25227081400001));
#354330=CARTESIAN_POINT('Ctrl Pts',(2.97303690699994,12.2,-3.25305986700001));
#354331=CARTESIAN_POINT('Ctrl Pts',(2.97303690699994,5.2,-3.25305986700001));
#354332=CARTESIAN_POINT('Ctrl Pts',(2.97303690699994,2.2,-3.25305986700001));
#354333=CARTESIAN_POINT('Ctrl Pts',(2.97493749499994,12.2,-3.25384836400001));
#354334=CARTESIAN_POINT('Ctrl Pts',(2.97493749499994,5.2,-3.25384836400001));
#354335=CARTESIAN_POINT('Ctrl Pts',(2.97493749499994,2.2,-3.25384836400001));
#354336=CARTESIAN_POINT('Ctrl Pts',(2.97684265099994,12.2,-3.25463629500002));
#354337=CARTESIAN_POINT('Ctrl Pts',(2.97684265099994,5.2,-3.25463629500002));
#354338=CARTESIAN_POINT('Ctrl Pts',(2.97684265099994,2.2,-3.25463629500002));
#354339=CARTESIAN_POINT('Ctrl Pts',(2.97875237099994,12.2,-3.25542364900001));
#354340=CARTESIAN_POINT('Ctrl Pts',(2.97875237099994,5.2,-3.25542364900001));
#354341=CARTESIAN_POINT('Ctrl Pts',(2.97875237099994,2.2,-3.25542364900001));
#354342=CARTESIAN_POINT('Ctrl Pts',(2.98066665199994,12.2,-3.25621041800002));
#354343=CARTESIAN_POINT('Ctrl Pts',(2.98066665199994,5.2,-3.25621041800002));
#354344=CARTESIAN_POINT('Ctrl Pts',(2.98066665199994,2.2,-3.25621041800002));
#354345=CARTESIAN_POINT('Ctrl Pts',(2.98258548999994,12.2,-3.25699658900001));
#354346=CARTESIAN_POINT('Ctrl Pts',(2.98258548999994,5.2,-3.25699658900001));
#354347=CARTESIAN_POINT('Ctrl Pts',(2.98258548999994,2.2,-3.25699658900001));
#354348=CARTESIAN_POINT('Ctrl Pts',(2.98450888299994,12.2,-3.25778215400002));
#354349=CARTESIAN_POINT('Ctrl Pts',(2.98450888299994,5.2,-3.25778215400002));
#354350=CARTESIAN_POINT('Ctrl Pts',(2.98450888299994,2.2,-3.25778215400002));
#354351=CARTESIAN_POINT('Ctrl Pts',(2.98643682599995,12.2,-3.25856710300001));
#354352=CARTESIAN_POINT('Ctrl Pts',(2.98643682599995,5.2,-3.25856710300001));
#354353=CARTESIAN_POINT('Ctrl Pts',(2.98643682599995,2.2,-3.25856710300001));
#354354=CARTESIAN_POINT('Ctrl Pts',(2.98836931499994,12.2,-3.25935142800001));
#354355=CARTESIAN_POINT('Ctrl Pts',(2.98836931499994,5.2,-3.25935142800001));
#354356=CARTESIAN_POINT('Ctrl Pts',(2.98836931499994,2.2,-3.25935142800001));
#354357=CARTESIAN_POINT('Ctrl Pts',(2.99030634799994,12.2,-3.26013511400001));
#354358=CARTESIAN_POINT('Ctrl Pts',(2.99030634799994,5.2,-3.26013511400001));
#354359=CARTESIAN_POINT('Ctrl Pts',(2.99030634799994,2.2,-3.26013511400001));
#354360=CARTESIAN_POINT('Ctrl Pts',(2.99224791899994,12.2,-3.26091815600002));
#354361=CARTESIAN_POINT('Ctrl Pts',(2.99224791899994,5.2,-3.26091815600002));
#354362=CARTESIAN_POINT('Ctrl Pts',(2.99224791899994,2.2,-3.26091815600002));
#354363=CARTESIAN_POINT('Ctrl Pts',(2.99419402599994,12.2,-3.26170054200002));
#354364=CARTESIAN_POINT('Ctrl Pts',(2.99419402599994,5.2,-3.26170054200002));
#354365=CARTESIAN_POINT('Ctrl Pts',(2.99419402599994,2.2,-3.26170054200002));
#354366=CARTESIAN_POINT('Ctrl Pts',(2.99614466599994,12.2,-3.26248226200001));
#354367=CARTESIAN_POINT('Ctrl Pts',(2.99614466599994,5.2,-3.26248226200001));
#354368=CARTESIAN_POINT('Ctrl Pts',(2.99614466599994,2.2,-3.26248226200001));
#354369=CARTESIAN_POINT('Ctrl Pts',(2.99809983499994,12.2,-3.26326330800002));
#354370=CARTESIAN_POINT('Ctrl Pts',(2.99809983499994,5.2,-3.26326330800002));
#354371=CARTESIAN_POINT('Ctrl Pts',(2.99809983499994,2.2,-3.26326330800002));
#354372=CARTESIAN_POINT('Ctrl Pts',(3.00005952799994,12.2,-3.26404366800002));
#354373=CARTESIAN_POINT('Ctrl Pts',(3.00005952799994,5.2,-3.26404366800002));
#354374=CARTESIAN_POINT('Ctrl Pts',(3.00005952799994,2.2,-3.26404366800002));
#354375=CARTESIAN_POINT('Ctrl Pts',(3.00202374199994,12.2,-3.26482333400001));
#354376=CARTESIAN_POINT('Ctrl Pts',(3.00202374199994,5.2,-3.26482333400001));
#354377=CARTESIAN_POINT('Ctrl Pts',(3.00202374199994,2.2,-3.26482333400001));
#354378=CARTESIAN_POINT('Ctrl Pts',(3.00399247299994,12.2,-3.26560229400001));
#354379=CARTESIAN_POINT('Ctrl Pts',(3.00399247299994,5.2,-3.26560229400001));
#354380=CARTESIAN_POINT('Ctrl Pts',(3.00399247299994,2.2,-3.26560229400001));
#354381=CARTESIAN_POINT('Ctrl Pts',(3.00596571799994,12.2,-3.26638054100002));
#354382=CARTESIAN_POINT('Ctrl Pts',(3.00596571799994,5.2,-3.26638054100002));
#354383=CARTESIAN_POINT('Ctrl Pts',(3.00596571799994,2.2,-3.26638054100002));
#354384=CARTESIAN_POINT('Ctrl Pts',(3.00794347399994,12.2,-3.26715806400002));
#354385=CARTESIAN_POINT('Ctrl Pts',(3.00794347399994,5.2,-3.26715806400002));
#354386=CARTESIAN_POINT('Ctrl Pts',(3.00794347399994,2.2,-3.26715806400002));
#354387=CARTESIAN_POINT('Ctrl Pts',(3.00992573499994,12.2,-3.26793485300001));
#354388=CARTESIAN_POINT('Ctrl Pts',(3.00992573499994,5.2,-3.26793485300001));
#354389=CARTESIAN_POINT('Ctrl Pts',(3.00992573499994,2.2,-3.26793485300001));
#354390=CARTESIAN_POINT('Ctrl Pts',(3.01191249899994,12.2,-3.26871089900001));
#354391=CARTESIAN_POINT('Ctrl Pts',(3.01191249899994,5.2,-3.26871089900001));
#354392=CARTESIAN_POINT('Ctrl Pts',(3.01191249899994,2.2,-3.26871089900001));
#354393=CARTESIAN_POINT('Ctrl Pts',(3.01390376299994,12.2,-3.26948619100001));
#354394=CARTESIAN_POINT('Ctrl Pts',(3.01390376299994,5.2,-3.26948619100001));
#354395=CARTESIAN_POINT('Ctrl Pts',(3.01390376299994,2.2,-3.26948619100001));
#354396=CARTESIAN_POINT('Ctrl Pts',(3.01589952199994,12.2,-3.27026072100002));
#354397=CARTESIAN_POINT('Ctrl Pts',(3.01589952199994,5.2,-3.27026072100002));
#354398=CARTESIAN_POINT('Ctrl Pts',(3.01589952199994,2.2,-3.27026072100002));
#354399=CARTESIAN_POINT('Ctrl Pts',(3.01789977199994,12.2,-3.27103447900001));
#354400=CARTESIAN_POINT('Ctrl Pts',(3.01789977199994,5.2,-3.27103447900001));
#354401=CARTESIAN_POINT('Ctrl Pts',(3.01789977199994,2.2,-3.27103447900001));
#354402=CARTESIAN_POINT('Ctrl Pts',(3.01990450999994,12.2,-3.27180745500002));
#354403=CARTESIAN_POINT('Ctrl Pts',(3.01990450999994,5.2,-3.27180745500002));
#354404=CARTESIAN_POINT('Ctrl Pts',(3.01990450999994,2.2,-3.27180745500002));
#354405=CARTESIAN_POINT('Ctrl Pts',(3.02191373299994,12.2,-3.27257964000002));
#354406=CARTESIAN_POINT('Ctrl Pts',(3.02191373299994,5.2,-3.27257964000002));
#354407=CARTESIAN_POINT('Ctrl Pts',(3.02191373299994,2.2,-3.27257964000002));
#354408=CARTESIAN_POINT('Ctrl Pts',(3.02392743499994,12.2,-3.27335102300002));
#354409=CARTESIAN_POINT('Ctrl Pts',(3.02392743499994,5.2,-3.27335102300002));
#354410=CARTESIAN_POINT('Ctrl Pts',(3.02392743499994,2.2,-3.27335102300002));
#354411=CARTESIAN_POINT('Ctrl Pts',(3.02594561299995,12.2,-3.27412159700001));
#354412=CARTESIAN_POINT('Ctrl Pts',(3.02594561299995,5.2,-3.27412159700001));
#354413=CARTESIAN_POINT('Ctrl Pts',(3.02594561299995,2.2,-3.27412159700001));
#354414=CARTESIAN_POINT('Ctrl Pts',(3.02796826499995,12.2,-3.27489135000001));
#354415=CARTESIAN_POINT('Ctrl Pts',(3.02796826499995,5.2,-3.27489135000001));
#354416=CARTESIAN_POINT('Ctrl Pts',(3.02796826499995,2.2,-3.27489135000001));
#354417=CARTESIAN_POINT('Ctrl Pts',(3.02999538599994,12.2,-3.27566027400001));
#354418=CARTESIAN_POINT('Ctrl Pts',(3.02999538599994,5.2,-3.27566027400001));
#354419=CARTESIAN_POINT('Ctrl Pts',(3.02999538599994,2.2,-3.27566027400001));
#354420=CARTESIAN_POINT('Ctrl Pts',(3.03202697199994,12.2,-3.27642835800001));
#354421=CARTESIAN_POINT('Ctrl Pts',(3.03202697199994,5.2,-3.27642835800001));
#354422=CARTESIAN_POINT('Ctrl Pts',(3.03202697199994,2.2,-3.27642835800001));
#354423=CARTESIAN_POINT('Ctrl Pts',(3.03406301999994,12.2,-3.27719559500002));
#354424=CARTESIAN_POINT('Ctrl Pts',(3.03406301999994,5.2,-3.27719559500002));
#354425=CARTESIAN_POINT('Ctrl Pts',(3.03406301999994,2.2,-3.27719559500002));
#354426=CARTESIAN_POINT('Ctrl Pts',(3.03610352499994,12.2,-3.27796197400001));
#354427=CARTESIAN_POINT('Ctrl Pts',(3.03610352499994,5.2,-3.27796197400001));
#354428=CARTESIAN_POINT('Ctrl Pts',(3.03610352499994,2.2,-3.27796197400001));
#354429=CARTESIAN_POINT('Ctrl Pts',(3.03814848399994,12.2,-3.27872748400001));
#354430=CARTESIAN_POINT('Ctrl Pts',(3.03814848399994,5.2,-3.27872748400001));
#354431=CARTESIAN_POINT('Ctrl Pts',(3.03814848399994,2.2,-3.27872748400001));
#354432=CARTESIAN_POINT('Ctrl Pts',(3.04019789299995,12.2,-3.27949211900001));
#354433=CARTESIAN_POINT('Ctrl Pts',(3.04019789299995,5.2,-3.27949211900001));
#354434=CARTESIAN_POINT('Ctrl Pts',(3.04019789299995,2.2,-3.27949211900001));
#354435=CARTESIAN_POINT('Ctrl Pts',(3.04225174799994,12.2,-3.28025586800001));
#354436=CARTESIAN_POINT('Ctrl Pts',(3.04225174799994,5.2,-3.28025586800001));
#354437=CARTESIAN_POINT('Ctrl Pts',(3.04225174799994,2.2,-3.28025586800001));
#354438=CARTESIAN_POINT('Ctrl Pts',(3.04431004599994,12.2,-3.28101872200001));
#354439=CARTESIAN_POINT('Ctrl Pts',(3.04431004599994,5.2,-3.28101872200001));
#354440=CARTESIAN_POINT('Ctrl Pts',(3.04431004599994,2.2,-3.28101872200001));
#354441=CARTESIAN_POINT('Ctrl Pts',(3.04637278199994,12.2,-3.28178067000001));
#354442=CARTESIAN_POINT('Ctrl Pts',(3.04637278199994,5.2,-3.28178067000001));
#354443=CARTESIAN_POINT('Ctrl Pts',(3.04637278199994,2.2,-3.28178067000001));
#354444=CARTESIAN_POINT('Ctrl Pts',(3.04843995199994,12.2,-3.28254170400001));
#354445=CARTESIAN_POINT('Ctrl Pts',(3.04843995199994,5.2,-3.28254170400001));
#354446=CARTESIAN_POINT('Ctrl Pts',(3.04843995199994,2.2,-3.28254170400001));
#354447=CARTESIAN_POINT('Ctrl Pts',(3.05051155499994,12.2,-3.28330181600001));
#354448=CARTESIAN_POINT('Ctrl Pts',(3.05051155499994,5.2,-3.28330181600001));
#354449=CARTESIAN_POINT('Ctrl Pts',(3.05051155499994,2.2,-3.28330181600001));
#354450=CARTESIAN_POINT('Ctrl Pts',(3.05258758299995,12.2,-3.28406099500001));
#354451=CARTESIAN_POINT('Ctrl Pts',(3.05258758299995,5.2,-3.28406099500001));
#354452=CARTESIAN_POINT('Ctrl Pts',(3.05258758299995,2.2,-3.28406099500001));
#354453=CARTESIAN_POINT('Ctrl Pts',(3.05466803499994,12.2,-3.28481923100002));
#354454=CARTESIAN_POINT('Ctrl Pts',(3.05466803499994,5.2,-3.28481923100002));
#354455=CARTESIAN_POINT('Ctrl Pts',(3.05466803499994,2.2,-3.28481923100002));
#354456=CARTESIAN_POINT('Ctrl Pts',(3.05675290699994,12.2,-3.28557651600001));
#354457=CARTESIAN_POINT('Ctrl Pts',(3.05675290699994,5.2,-3.28557651600001));
#354458=CARTESIAN_POINT('Ctrl Pts',(3.05675290699994,2.2,-3.28557651600001));
#354459=CARTESIAN_POINT('Ctrl Pts',(3.05884219399994,12.2,-3.28633284200002));
#354460=CARTESIAN_POINT('Ctrl Pts',(3.05884219399994,5.2,-3.28633284200002));
#354461=CARTESIAN_POINT('Ctrl Pts',(3.05884219399994,2.2,-3.28633284200002));
#354462=CARTESIAN_POINT('Ctrl Pts',(3.06093589199994,12.2,-3.28708819800001));
#354463=CARTESIAN_POINT('Ctrl Pts',(3.06093589199994,5.2,-3.28708819800001));
#354464=CARTESIAN_POINT('Ctrl Pts',(3.06093589199994,2.2,-3.28708819800001));
#354465=CARTESIAN_POINT('Ctrl Pts',(3.06303399699994,12.2,-3.28784257500002));
#354466=CARTESIAN_POINT('Ctrl Pts',(3.06303399699994,5.2,-3.28784257500002));
#354467=CARTESIAN_POINT('Ctrl Pts',(3.06303399699994,2.2,-3.28784257500002));
#354468=CARTESIAN_POINT('Ctrl Pts',(3.06513650699994,12.2,-3.28859596300001));
#354469=CARTESIAN_POINT('Ctrl Pts',(3.06513650699994,5.2,-3.28859596300001));
#354470=CARTESIAN_POINT('Ctrl Pts',(3.06513650699994,2.2,-3.28859596300001));
#354471=CARTESIAN_POINT('Ctrl Pts',(3.06724341699995,12.2,-3.28934835500001));
#354472=CARTESIAN_POINT('Ctrl Pts',(3.06724341699995,5.2,-3.28934835500001));
#354473=CARTESIAN_POINT('Ctrl Pts',(3.06724341699995,2.2,-3.28934835500001));
#354474=CARTESIAN_POINT('Ctrl Pts',(3.06935472199994,12.2,-3.29009974000002));
#354475=CARTESIAN_POINT('Ctrl Pts',(3.06935472199994,5.2,-3.29009974000002));
#354476=CARTESIAN_POINT('Ctrl Pts',(3.06935472199994,2.2,-3.29009974000002));
#354477=CARTESIAN_POINT('Ctrl Pts',(3.07147041999994,12.2,-3.29085011100001));
#354478=CARTESIAN_POINT('Ctrl Pts',(3.07147041999994,5.2,-3.29085011100001));
#354479=CARTESIAN_POINT('Ctrl Pts',(3.07147041999994,2.2,-3.29085011100001));
#354480=CARTESIAN_POINT('Ctrl Pts',(3.07359050599994,12.2,-3.29159945600002));
#354481=CARTESIAN_POINT('Ctrl Pts',(3.07359050599994,5.2,-3.29159945600002));
#354482=CARTESIAN_POINT('Ctrl Pts',(3.07359050599994,2.2,-3.29159945600002));
#354483=CARTESIAN_POINT('Ctrl Pts',(3.07571497499994,12.2,-3.29234776800002));
#354484=CARTESIAN_POINT('Ctrl Pts',(3.07571497499994,5.2,-3.29234776800002));
#354485=CARTESIAN_POINT('Ctrl Pts',(3.07571497499994,2.2,-3.29234776800002));
#354486=CARTESIAN_POINT('Ctrl Pts',(3.07784382499994,12.2,-3.29309503700001));
#354487=CARTESIAN_POINT('Ctrl Pts',(3.07784382499994,5.2,-3.29309503700001));
#354488=CARTESIAN_POINT('Ctrl Pts',(3.07784382499994,2.2,-3.29309503700001));
#354489=CARTESIAN_POINT('Ctrl Pts',(3.07997705199994,12.2,-3.29384125500002));
#354490=CARTESIAN_POINT('Ctrl Pts',(3.07997705199994,5.2,-3.29384125500002));
#354491=CARTESIAN_POINT('Ctrl Pts',(3.07997705199994,2.2,-3.29384125500002));
#354492=CARTESIAN_POINT('Ctrl Pts',(3.08211465099994,12.2,-3.29458641300001));
#354493=CARTESIAN_POINT('Ctrl Pts',(3.08211465099994,5.2,-3.29458641300001));
#354494=CARTESIAN_POINT('Ctrl Pts',(3.08211465099994,2.2,-3.29458641300001));
#354495=CARTESIAN_POINT('Ctrl Pts',(3.08425661699995,12.2,-3.29533050000002));
#354496=CARTESIAN_POINT('Ctrl Pts',(3.08425661699995,5.2,-3.29533050000002));
#354497=CARTESIAN_POINT('Ctrl Pts',(3.08425661699995,2.2,-3.29533050000002));
#354498=CARTESIAN_POINT('Ctrl Pts',(3.08640294899994,12.2,-3.29607351000002));
#354499=CARTESIAN_POINT('Ctrl Pts',(3.08640294899994,5.2,-3.29607351000002));
#354500=CARTESIAN_POINT('Ctrl Pts',(3.08640294899994,2.2,-3.29607351000002));
#354501=CARTESIAN_POINT('Ctrl Pts',(3.08855364099994,12.2,-3.29681543000001));
#354502=CARTESIAN_POINT('Ctrl Pts',(3.08855364099994,5.2,-3.29681543000001));
#354503=CARTESIAN_POINT('Ctrl Pts',(3.08855364099994,2.2,-3.29681543000001));
#354504=CARTESIAN_POINT('Ctrl Pts',(3.09070868999994,12.2,-3.29755625500002));
#354505=CARTESIAN_POINT('Ctrl Pts',(3.09070868999994,5.2,-3.29755625500002));
#354506=CARTESIAN_POINT('Ctrl Pts',(3.09070868999994,2.2,-3.29755625500002));
#354507=CARTESIAN_POINT('Ctrl Pts',(3.09286808999994,12.2,-3.29829597400002));
#354508=CARTESIAN_POINT('Ctrl Pts',(3.09286808999994,5.2,-3.29829597400002));
#354509=CARTESIAN_POINT('Ctrl Pts',(3.09286808999994,2.2,-3.29829597400002));
#354510=CARTESIAN_POINT('Ctrl Pts',(3.09503183999994,12.2,-3.29903457800001));
#354511=CARTESIAN_POINT('Ctrl Pts',(3.09503183999994,5.2,-3.29903457800001));
#354512=CARTESIAN_POINT('Ctrl Pts',(3.09503183999994,2.2,-3.29903457800001));
#354513=CARTESIAN_POINT('Ctrl Pts',(3.09719993399994,12.2,-3.29977205900001));
#354514=CARTESIAN_POINT('Ctrl Pts',(3.09719993399994,5.2,-3.29977205900001));
#354515=CARTESIAN_POINT('Ctrl Pts',(3.09719993399994,2.2,-3.29977205900001));
#354516=CARTESIAN_POINT('Ctrl Pts',(3.09937236799994,12.2,-3.30050840800002));
#354517=CARTESIAN_POINT('Ctrl Pts',(3.09937236799994,5.2,-3.30050840800002));
#354518=CARTESIAN_POINT('Ctrl Pts',(3.09937236799994,2.2,-3.30050840800002));
#354519=CARTESIAN_POINT('Ctrl Pts',(3.10154913999994,12.2,-3.30124361600001));
#354520=CARTESIAN_POINT('Ctrl Pts',(3.10154913999994,5.2,-3.30124361600001));
#354521=CARTESIAN_POINT('Ctrl Pts',(3.10154913999994,2.2,-3.30124361600001));
#354522=CARTESIAN_POINT('Ctrl Pts',(3.10373024299994,12.2,-3.30197767400001));
#354523=CARTESIAN_POINT('Ctrl Pts',(3.10373024299994,5.2,-3.30197767400001));
#354524=CARTESIAN_POINT('Ctrl Pts',(3.10373024299994,2.2,-3.30197767400001));
#354525=CARTESIAN_POINT('Ctrl Pts',(3.10591567499995,12.2,-3.30271057300001));
#354526=CARTESIAN_POINT('Ctrl Pts',(3.10591567499995,5.2,-3.30271057300001));
#354527=CARTESIAN_POINT('Ctrl Pts',(3.10591567499995,2.2,-3.30271057300001));
#354528=CARTESIAN_POINT('Ctrl Pts',(3.10810543099994,12.2,-3.30344230400001));
#354529=CARTESIAN_POINT('Ctrl Pts',(3.10810543099994,5.2,-3.30344230400001));
#354530=CARTESIAN_POINT('Ctrl Pts',(3.10810543099994,2.2,-3.30344230400001));
#354531=CARTESIAN_POINT('Ctrl Pts',(3.11029950799994,12.2,-3.30417286000001));
#354532=CARTESIAN_POINT('Ctrl Pts',(3.11029950799994,5.2,-3.30417286000001));
#354533=CARTESIAN_POINT('Ctrl Pts',(3.11029950799994,2.2,-3.30417286000001));
#354534=CARTESIAN_POINT('Ctrl Pts',(3.11249790099994,12.2,-3.30490222900002));
#354535=CARTESIAN_POINT('Ctrl Pts',(3.11249790099994,5.2,-3.30490222900002));
#354536=CARTESIAN_POINT('Ctrl Pts',(3.11249790099994,2.2,-3.30490222900002));
#354537=CARTESIAN_POINT('Ctrl Pts',(3.11470060599994,12.2,-3.30563040500001));
#354538=CARTESIAN_POINT('Ctrl Pts',(3.11470060599994,5.2,-3.30563040500001));
#354539=CARTESIAN_POINT('Ctrl Pts',(3.11470060599994,2.2,-3.30563040500001));
#354540=CARTESIAN_POINT('Ctrl Pts',(3.11690761999994,12.2,-3.30635737800002));
#354541=CARTESIAN_POINT('Ctrl Pts',(3.11690761999994,5.2,-3.30635737800002));
#354542=CARTESIAN_POINT('Ctrl Pts',(3.11690761999994,2.2,-3.30635737800002));
#354543=CARTESIAN_POINT('Ctrl Pts',(3.11911893699994,12.2,-3.30708314000002));
#354544=CARTESIAN_POINT('Ctrl Pts',(3.11911893699994,5.2,-3.30708314000002));
#354545=CARTESIAN_POINT('Ctrl Pts',(3.11911893699994,2.2,-3.30708314000002));
#354546=CARTESIAN_POINT('Ctrl Pts',(3.12133455499994,12.2,-3.30780768200002));
#354547=CARTESIAN_POINT('Ctrl Pts',(3.12133455499994,5.2,-3.30780768200002));
#354548=CARTESIAN_POINT('Ctrl Pts',(3.12133455499994,2.2,-3.30780768200002));
#354549=CARTESIAN_POINT('Ctrl Pts',(3.12355446899995,12.2,-3.30853099500001));
#354550=CARTESIAN_POINT('Ctrl Pts',(3.12355446899995,5.2,-3.30853099500001));
#354551=CARTESIAN_POINT('Ctrl Pts',(3.12355446899995,2.2,-3.30853099500001));
#354552=CARTESIAN_POINT('Ctrl Pts',(3.12577867499995,12.2,-3.30925307000001));
#354553=CARTESIAN_POINT('Ctrl Pts',(3.12577867499995,5.2,-3.30925307000001));
#354554=CARTESIAN_POINT('Ctrl Pts',(3.12577867499995,2.2,-3.30925307000001));
#354555=CARTESIAN_POINT('Ctrl Pts',(3.12800716799994,12.2,-3.30997389900002));
#354556=CARTESIAN_POINT('Ctrl Pts',(3.12800716799994,5.2,-3.30997389900002));
#354557=CARTESIAN_POINT('Ctrl Pts',(3.12800716799994,2.2,-3.30997389900002));
#354558=CARTESIAN_POINT('Ctrl Pts',(3.13023994599994,12.2,-3.31069347300001));
#354559=CARTESIAN_POINT('Ctrl Pts',(3.13023994599994,5.2,-3.31069347300001));
#354560=CARTESIAN_POINT('Ctrl Pts',(3.13023994599994,2.2,-3.31069347300001));
#354561=CARTESIAN_POINT('Ctrl Pts',(3.13247700299994,12.2,-3.31141178400001));
#354562=CARTESIAN_POINT('Ctrl Pts',(3.13247700299994,5.2,-3.31141178400001));
#354563=CARTESIAN_POINT('Ctrl Pts',(3.13247700299994,2.2,-3.31141178400001));
#354564=CARTESIAN_POINT('Ctrl Pts',(3.13471833499994,12.2,-3.31212882300001));
#354565=CARTESIAN_POINT('Ctrl Pts',(3.13471833499994,5.2,-3.31212882300001));
#354566=CARTESIAN_POINT('Ctrl Pts',(3.13471833499994,2.2,-3.31212882300001));
#354567=CARTESIAN_POINT('Ctrl Pts',(3.13696393899995,12.2,-3.31284458200001));
#354568=CARTESIAN_POINT('Ctrl Pts',(3.13696393899995,5.2,-3.31284458200001));
#354569=CARTESIAN_POINT('Ctrl Pts',(3.13696393899995,2.2,-3.31284458200001));
#354570=CARTESIAN_POINT('Ctrl Pts',(3.13921380999994,12.2,-3.31355905100001));
#354571=CARTESIAN_POINT('Ctrl Pts',(3.13921380999994,5.2,-3.31355905100001));
#354572=CARTESIAN_POINT('Ctrl Pts',(3.13921380999994,2.2,-3.31355905100001));
#354573=CARTESIAN_POINT('Ctrl Pts',(3.14146794399994,12.2,-3.31427222300002));
#354574=CARTESIAN_POINT('Ctrl Pts',(3.14146794399994,5.2,-3.31427222300002));
#354575=CARTESIAN_POINT('Ctrl Pts',(3.14146794399994,2.2,-3.31427222300002));
#354576=CARTESIAN_POINT('Ctrl Pts',(3.14372633799994,12.2,-3.31498408800002));
#354577=CARTESIAN_POINT('Ctrl Pts',(3.14372633799994,5.2,-3.31498408800002));
#354578=CARTESIAN_POINT('Ctrl Pts',(3.14372633799994,2.2,-3.31498408800002));
#354579=CARTESIAN_POINT('Ctrl Pts',(3.14598898599994,12.2,-3.31569463800002));
#354580=CARTESIAN_POINT('Ctrl Pts',(3.14598898599994,5.2,-3.31569463800002));
#354581=CARTESIAN_POINT('Ctrl Pts',(3.14598898599994,2.2,-3.31569463800002));
#354582=CARTESIAN_POINT('Ctrl Pts',(3.14825588499994,12.2,-3.31640386600002));
#354583=CARTESIAN_POINT('Ctrl Pts',(3.14825588499994,5.2,-3.31640386600002));
#354584=CARTESIAN_POINT('Ctrl Pts',(3.14825588499994,2.2,-3.31640386600002));
#354585=CARTESIAN_POINT('Ctrl Pts',(3.15052703099994,12.2,-3.31711176200002));
#354586=CARTESIAN_POINT('Ctrl Pts',(3.15052703099994,5.2,-3.31711176200002));
#354587=CARTESIAN_POINT('Ctrl Pts',(3.15052703099994,2.2,-3.31711176200002));
#354588=CARTESIAN_POINT('Ctrl Pts',(3.15280241899994,12.2,-3.31781831700001));
#354589=CARTESIAN_POINT('Ctrl Pts',(3.15280241899994,5.2,-3.31781831700001));
#354590=CARTESIAN_POINT('Ctrl Pts',(3.15280241899994,2.2,-3.31781831700001));
#354591=CARTESIAN_POINT('Ctrl Pts',(3.15508204599994,12.2,-3.31852352400002));
#354592=CARTESIAN_POINT('Ctrl Pts',(3.15508204599994,5.2,-3.31852352400002));
#354593=CARTESIAN_POINT('Ctrl Pts',(3.15508204599994,2.2,-3.31852352400002));
#354594=CARTESIAN_POINT('Ctrl Pts',(3.15736590599994,12.2,-3.31922737400001));
#354595=CARTESIAN_POINT('Ctrl Pts',(3.15736590599994,5.2,-3.31922737400001));
#354596=CARTESIAN_POINT('Ctrl Pts',(3.15736590599994,2.2,-3.31922737400001));
#354597=CARTESIAN_POINT('Ctrl Pts',(3.15965399599994,12.2,-3.31992985800001));
#354598=CARTESIAN_POINT('Ctrl Pts',(3.15965399599994,5.2,-3.31992985800001));
#354599=CARTESIAN_POINT('Ctrl Pts',(3.15965399599994,2.2,-3.31992985800001));
#354600=CARTESIAN_POINT('Ctrl Pts',(3.16194631299994,12.2,-3.32063096700002));
#354601=CARTESIAN_POINT('Ctrl Pts',(3.16194631299994,5.2,-3.32063096700002));
#354602=CARTESIAN_POINT('Ctrl Pts',(3.16194631299994,2.2,-3.32063096700002));
#354603=CARTESIAN_POINT('Ctrl Pts',(3.16424285099994,12.2,-3.32133069500001));
#354604=CARTESIAN_POINT('Ctrl Pts',(3.16424285099994,5.2,-3.32133069500001));
#354605=CARTESIAN_POINT('Ctrl Pts',(3.16424285099994,2.2,-3.32133069500001));
#354606=CARTESIAN_POINT('Ctrl Pts',(3.16654360599995,12.2,-3.32202903200002));
#354607=CARTESIAN_POINT('Ctrl Pts',(3.16654360599995,5.2,-3.32202903200002));
#354608=CARTESIAN_POINT('Ctrl Pts',(3.16654360599995,2.2,-3.32202903200002));
#354609=CARTESIAN_POINT('Ctrl Pts',(3.16884857399995,12.2,-3.32272597000001));
#354610=CARTESIAN_POINT('Ctrl Pts',(3.16884857399995,5.2,-3.32272597000001));
#354611=CARTESIAN_POINT('Ctrl Pts',(3.16884857399995,2.2,-3.32272597000001));
#354612=CARTESIAN_POINT('Ctrl Pts',(3.17115775199994,12.2,-3.32342150100001));
#354613=CARTESIAN_POINT('Ctrl Pts',(3.17115775199994,5.2,-3.32342150100001));
#354614=CARTESIAN_POINT('Ctrl Pts',(3.17115775199994,2.2,-3.32342150100001));
#354615=CARTESIAN_POINT('Ctrl Pts',(3.17347113499994,12.2,-3.32411561600002));
#354616=CARTESIAN_POINT('Ctrl Pts',(3.17347113499994,5.2,-3.32411561600002));
#354617=CARTESIAN_POINT('Ctrl Pts',(3.17347113499994,2.2,-3.32411561600002));
#354618=CARTESIAN_POINT('Ctrl Pts',(3.17578871699994,12.2,-3.32480830800002));
#354619=CARTESIAN_POINT('Ctrl Pts',(3.17578871699994,5.2,-3.32480830800002));
#354620=CARTESIAN_POINT('Ctrl Pts',(3.17578871699994,2.2,-3.32480830800002));
#354621=CARTESIAN_POINT('Ctrl Pts',(3.17811049599994,12.2,-3.32549956700001));
#354622=CARTESIAN_POINT('Ctrl Pts',(3.17811049599994,5.2,-3.32549956700001));
#354623=CARTESIAN_POINT('Ctrl Pts',(3.17811049599994,2.2,-3.32549956700001));
#354624=CARTESIAN_POINT('Ctrl Pts',(3.18043646699994,12.2,-3.32618938500001));
#354625=CARTESIAN_POINT('Ctrl Pts',(3.18043646699994,5.2,-3.32618938500001));
#354626=CARTESIAN_POINT('Ctrl Pts',(3.18043646699994,2.2,-3.32618938500001));
#354627=CARTESIAN_POINT('Ctrl Pts',(3.18276662599994,12.2,-3.32687775400001));
#354628=CARTESIAN_POINT('Ctrl Pts',(3.18276662599994,5.2,-3.32687775400001));
#354629=CARTESIAN_POINT('Ctrl Pts',(3.18276662599994,2.2,-3.32687775400001));
#354630=CARTESIAN_POINT('Ctrl Pts',(3.18510096799994,12.2,-3.32756466700001));
#354631=CARTESIAN_POINT('Ctrl Pts',(3.18510096799994,5.2,-3.32756466700001));
#354632=CARTESIAN_POINT('Ctrl Pts',(3.18510096799994,2.2,-3.32756466700001));
#354633=CARTESIAN_POINT('Ctrl Pts',(3.18743949099995,12.2,-3.32825011400002));
#354634=CARTESIAN_POINT('Ctrl Pts',(3.18743949099995,5.2,-3.32825011400002));
#354635=CARTESIAN_POINT('Ctrl Pts',(3.18743949099995,2.2,-3.32825011400002));
#354636=CARTESIAN_POINT('Ctrl Pts',(3.18978218799994,12.2,-3.32893408800001));
#354637=CARTESIAN_POINT('Ctrl Pts',(3.18978218799994,5.2,-3.32893408800001));
#354638=CARTESIAN_POINT('Ctrl Pts',(3.18978218799994,2.2,-3.32893408800001));
#354639=CARTESIAN_POINT('Ctrl Pts',(3.19212905499994,12.2,-3.32961658000002));
#354640=CARTESIAN_POINT('Ctrl Pts',(3.19212905499994,5.2,-3.32961658000002));
#354641=CARTESIAN_POINT('Ctrl Pts',(3.19212905499994,2.2,-3.32961658000002));
#354642=CARTESIAN_POINT('Ctrl Pts',(3.19448009099994,12.2,-3.33029758200002));
#354643=CARTESIAN_POINT('Ctrl Pts',(3.19448009099994,5.2,-3.33029758200002));
#354644=CARTESIAN_POINT('Ctrl Pts',(3.19448009099994,2.2,-3.33029758200002));
#354645=CARTESIAN_POINT('Ctrl Pts',(3.19683528699994,12.2,-3.33097708700001));
#354646=CARTESIAN_POINT('Ctrl Pts',(3.19683528699994,5.2,-3.33097708700001));
#354647=CARTESIAN_POINT('Ctrl Pts',(3.19683528699994,2.2,-3.33097708700001));
#354648=CARTESIAN_POINT('Ctrl Pts',(3.19919464199995,12.2,-3.33165508500001));
#354649=CARTESIAN_POINT('Ctrl Pts',(3.19919464199995,5.2,-3.33165508500001));
#354650=CARTESIAN_POINT('Ctrl Pts',(3.19919464199995,2.2,-3.33165508500001));
#354651=CARTESIAN_POINT('Ctrl Pts',(3.20155814999994,12.2,-3.33233157000001));
#354652=CARTESIAN_POINT('Ctrl Pts',(3.20155814999994,5.2,-3.33233157000001));
#354653=CARTESIAN_POINT('Ctrl Pts',(3.20155814999994,2.2,-3.33233157000001));
#354654=CARTESIAN_POINT('Ctrl Pts',(3.20392580899994,12.2,-3.33300653200002));
#354655=CARTESIAN_POINT('Ctrl Pts',(3.20392580899994,5.2,-3.33300653200002));
#354656=CARTESIAN_POINT('Ctrl Pts',(3.20392580899994,2.2,-3.33300653200002));
#354657=CARTESIAN_POINT('Ctrl Pts',(3.20629761299994,12.2,-3.33367996300002));
#354658=CARTESIAN_POINT('Ctrl Pts',(3.20629761299994,5.2,-3.33367996300002));
#354659=CARTESIAN_POINT('Ctrl Pts',(3.20629761299994,2.2,-3.33367996300002));
#354660=CARTESIAN_POINT('Ctrl Pts',(3.20867355699994,12.2,-3.33435185700001));
#354661=CARTESIAN_POINT('Ctrl Pts',(3.20867355699994,5.2,-3.33435185700001));
#354662=CARTESIAN_POINT('Ctrl Pts',(3.20867355699994,2.2,-3.33435185700001));
#354663=CARTESIAN_POINT('Ctrl Pts',(3.21105363699994,12.2,-3.33502220300002));
#354664=CARTESIAN_POINT('Ctrl Pts',(3.21105363699994,5.2,-3.33502220300002));
#354665=CARTESIAN_POINT('Ctrl Pts',(3.21105363699994,2.2,-3.33502220300002));
#354666=CARTESIAN_POINT('Ctrl Pts',(3.21343785099995,12.2,-3.33569099500002));
#354667=CARTESIAN_POINT('Ctrl Pts',(3.21343785099995,5.2,-3.33569099500002));
#354668=CARTESIAN_POINT('Ctrl Pts',(3.21343785099995,2.2,-3.33569099500002));
#354669=CARTESIAN_POINT('Ctrl Pts',(3.21582619199994,12.2,-3.33635822400002));
#354670=CARTESIAN_POINT('Ctrl Pts',(3.21582619199994,5.2,-3.33635822400002));
#354671=CARTESIAN_POINT('Ctrl Pts',(3.21582619199994,2.2,-3.33635822400002));
#354672=CARTESIAN_POINT('Ctrl Pts',(3.21821865699994,12.2,-3.33702388300001));
#354673=CARTESIAN_POINT('Ctrl Pts',(3.21821865699994,5.2,-3.33702388300001));
#354674=CARTESIAN_POINT('Ctrl Pts',(3.21821865699994,2.2,-3.33702388300001));
#354675=CARTESIAN_POINT('Ctrl Pts',(3.22061524099994,12.2,-3.33768796400001));
#354676=CARTESIAN_POINT('Ctrl Pts',(3.22061524099994,5.2,-3.33768796400001));
#354677=CARTESIAN_POINT('Ctrl Pts',(3.22061524099994,2.2,-3.33768796400001));
#354678=CARTESIAN_POINT('Ctrl Pts',(3.22301593999994,12.2,-3.33835045800001));
#354679=CARTESIAN_POINT('Ctrl Pts',(3.22301593999994,5.2,-3.33835045800001));
#354680=CARTESIAN_POINT('Ctrl Pts',(3.22301593999994,2.2,-3.33835045800001));
#354681=CARTESIAN_POINT('Ctrl Pts',(3.22542074999994,12.2,-3.33901135600001));
#354682=CARTESIAN_POINT('Ctrl Pts',(3.22542074999994,5.2,-3.33901135600001));
#354683=CARTESIAN_POINT('Ctrl Pts',(3.22542074999994,2.2,-3.33901135600001));
#354684=CARTESIAN_POINT('Ctrl Pts',(3.22782966599994,12.2,-3.33967065300001));
#354685=CARTESIAN_POINT('Ctrl Pts',(3.22782966599994,5.2,-3.33967065300001));
#354686=CARTESIAN_POINT('Ctrl Pts',(3.22782966599994,2.2,-3.33967065300001));
#354687=CARTESIAN_POINT('Ctrl Pts',(3.23024268399994,12.2,-3.34032834000002));
#354688=CARTESIAN_POINT('Ctrl Pts',(3.23024268399994,5.2,-3.34032834000002));
#354689=CARTESIAN_POINT('Ctrl Pts',(3.23024268399994,2.2,-3.34032834000002));
#354690=CARTESIAN_POINT('Ctrl Pts',(3.23265979899995,12.2,-3.34098440800001));
#354691=CARTESIAN_POINT('Ctrl Pts',(3.23265979899995,5.2,-3.34098440800001));
#354692=CARTESIAN_POINT('Ctrl Pts',(3.23265979899995,2.2,-3.34098440800001));
#354693=CARTESIAN_POINT('Ctrl Pts',(3.23508100799994,12.2,-3.34163885000001));
#354694=CARTESIAN_POINT('Ctrl Pts',(3.23508100799994,5.2,-3.34163885000001));
#354695=CARTESIAN_POINT('Ctrl Pts',(3.23508100799994,2.2,-3.34163885000001));
#354696=CARTESIAN_POINT('Ctrl Pts',(3.23750630699994,12.2,-3.34229165800001));
#354697=CARTESIAN_POINT('Ctrl Pts',(3.23750630699994,5.2,-3.34229165800001));
#354698=CARTESIAN_POINT('Ctrl Pts',(3.23750630699994,2.2,-3.34229165800001));
#354699=CARTESIAN_POINT('Ctrl Pts',(3.23993568899994,12.2,-3.34294282300001));
#354700=CARTESIAN_POINT('Ctrl Pts',(3.23993568899994,5.2,-3.34294282300001));
#354701=CARTESIAN_POINT('Ctrl Pts',(3.23993568899994,2.2,-3.34294282300001));
#354702=CARTESIAN_POINT('Ctrl Pts',(3.24236915199994,12.2,-3.34359234000001));
#354703=CARTESIAN_POINT('Ctrl Pts',(3.24236915199994,5.2,-3.34359234000001));
#354704=CARTESIAN_POINT('Ctrl Pts',(3.24236915199994,2.2,-3.34359234000001));
#354705=CARTESIAN_POINT('Ctrl Pts',(3.24480668999994,12.2,-3.34424019800001));
#354706=CARTESIAN_POINT('Ctrl Pts',(3.24480668999994,5.2,-3.34424019800001));
#354707=CARTESIAN_POINT('Ctrl Pts',(3.24480668999994,2.2,-3.34424019800001));
#354708=CARTESIAN_POINT('Ctrl Pts',(3.24724830099994,12.2,-3.34488639100002));
#354709=CARTESIAN_POINT('Ctrl Pts',(3.24724830099994,5.2,-3.34488639100002));
#354710=CARTESIAN_POINT('Ctrl Pts',(3.24724830099994,2.2,-3.34488639100002));
#354711=CARTESIAN_POINT('Ctrl Pts',(3.24969397699994,12.2,-3.34553091100001));
#354712=CARTESIAN_POINT('Ctrl Pts',(3.24969397699994,5.2,-3.34553091100001));
#354713=CARTESIAN_POINT('Ctrl Pts',(3.24969397699994,2.2,-3.34553091100001));
#354714=CARTESIAN_POINT('Ctrl Pts',(3.25214371599994,12.2,-3.34617375000001));
#354715=CARTESIAN_POINT('Ctrl Pts',(3.25214371599994,5.2,-3.34617375000001));
#354716=CARTESIAN_POINT('Ctrl Pts',(3.25214371599994,2.2,-3.34617375000001));
#354717=CARTESIAN_POINT('Ctrl Pts',(3.25459751399995,12.2,-3.34681490000001));
#354718=CARTESIAN_POINT('Ctrl Pts',(3.25459751399995,5.2,-3.34681490000001));
#354719=CARTESIAN_POINT('Ctrl Pts',(3.25459751399995,2.2,-3.34681490000001));
#354720=CARTESIAN_POINT('Ctrl Pts',(3.25705536499994,12.2,-3.34745435300002));
#354721=CARTESIAN_POINT('Ctrl Pts',(3.25705536499994,5.2,-3.34745435300002));
#354722=CARTESIAN_POINT('Ctrl Pts',(3.25705536499994,2.2,-3.34745435300002));
#354723=CARTESIAN_POINT('Ctrl Pts',(3.25951726499994,12.2,-3.34809210200001));
#354724=CARTESIAN_POINT('Ctrl Pts',(3.25951726499994,5.2,-3.34809210200001));
#354725=CARTESIAN_POINT('Ctrl Pts',(3.25951726499994,2.2,-3.34809210200001));
#354726=CARTESIAN_POINT('Ctrl Pts',(3.26198321199994,12.2,-3.34872814000001));
#354727=CARTESIAN_POINT('Ctrl Pts',(3.26198321199994,5.2,-3.34872814000001));
#354728=CARTESIAN_POINT('Ctrl Pts',(3.26198321199994,2.2,-3.34872814000001));
#354729=CARTESIAN_POINT('Ctrl Pts',(3.26445319799994,12.2,-3.34936245700002));
#354730=CARTESIAN_POINT('Ctrl Pts',(3.26445319799994,5.2,-3.34936245700002));
#354731=CARTESIAN_POINT('Ctrl Pts',(3.26445319799994,2.2,-3.34936245700002));
#354732=CARTESIAN_POINT('Ctrl Pts',(3.26692722099994,12.2,-3.34999504700002));
#354733=CARTESIAN_POINT('Ctrl Pts',(3.26692722099994,5.2,-3.34999504700002));
#354734=CARTESIAN_POINT('Ctrl Pts',(3.26692722099994,2.2,-3.34999504700002));
#354735=CARTESIAN_POINT('Ctrl Pts',(3.26940527499994,12.2,-3.35062590200002));
#354736=CARTESIAN_POINT('Ctrl Pts',(3.26940527499994,5.2,-3.35062590200002));
#354737=CARTESIAN_POINT('Ctrl Pts',(3.26940527499994,2.2,-3.35062590200002));
#354738=CARTESIAN_POINT('Ctrl Pts',(3.27188735699994,12.2,-3.35125501400002));
#354739=CARTESIAN_POINT('Ctrl Pts',(3.27188735699994,5.2,-3.35125501400002));
#354740=CARTESIAN_POINT('Ctrl Pts',(3.27188735699994,2.2,-3.35125501400002));
#354741=CARTESIAN_POINT('Ctrl Pts',(3.27437345999994,12.2,-3.35188237600001));
#354742=CARTESIAN_POINT('Ctrl Pts',(3.27437345999994,5.2,-3.35188237600001));
#354743=CARTESIAN_POINT('Ctrl Pts',(3.27437345999994,2.2,-3.35188237600001));
#354744=CARTESIAN_POINT('Ctrl Pts',(3.27686358299994,12.2,-3.35250797900001));
#354745=CARTESIAN_POINT('Ctrl Pts',(3.27686358299994,5.2,-3.35250797900001));
#354746=CARTESIAN_POINT('Ctrl Pts',(3.27686358299994,2.2,-3.35250797900001));
#354747=CARTESIAN_POINT('Ctrl Pts',(3.27935771899994,12.2,-3.35313181700001));
#354748=CARTESIAN_POINT('Ctrl Pts',(3.27935771899994,5.2,-3.35313181700001));
#354749=CARTESIAN_POINT('Ctrl Pts',(3.27935771899994,2.2,-3.35313181700001));
#354750=CARTESIAN_POINT('Ctrl Pts',(3.28185586499994,12.2,-3.35375388100001));
#354751=CARTESIAN_POINT('Ctrl Pts',(3.28185586499994,5.2,-3.35375388100001));
#354752=CARTESIAN_POINT('Ctrl Pts',(3.28185586499994,2.2,-3.35375388100001));
#354753=CARTESIAN_POINT('Ctrl Pts',(3.28435801599994,12.2,-3.35437416500001));
#354754=CARTESIAN_POINT('Ctrl Pts',(3.28435801599994,5.2,-3.35437416500001));
#354755=CARTESIAN_POINT('Ctrl Pts',(3.28435801599994,2.2,-3.35437416500001));
#354756=CARTESIAN_POINT('Ctrl Pts',(3.28686416799994,12.2,-3.35499266000001));
#354757=CARTESIAN_POINT('Ctrl Pts',(3.28686416799994,5.2,-3.35499266000001));
#354758=CARTESIAN_POINT('Ctrl Pts',(3.28686416799994,2.2,-3.35499266000001));
#354759=CARTESIAN_POINT('Ctrl Pts',(3.28937431499994,12.2,-3.35560936000002));
#354760=CARTESIAN_POINT('Ctrl Pts',(3.28937431499994,5.2,-3.35560936000002));
#354761=CARTESIAN_POINT('Ctrl Pts',(3.28937431499994,2.2,-3.35560936000002));
#354762=CARTESIAN_POINT('Ctrl Pts',(3.29188845499994,12.2,-3.35622425600001));
#354763=CARTESIAN_POINT('Ctrl Pts',(3.29188845499994,5.2,-3.35622425600001));
#354764=CARTESIAN_POINT('Ctrl Pts',(3.29188845499994,2.2,-3.35622425600001));
#354765=CARTESIAN_POINT('Ctrl Pts',(3.29440658299994,12.2,-3.35683734200002));
#354766=CARTESIAN_POINT('Ctrl Pts',(3.29440658299994,5.2,-3.35683734200002));
#354767=CARTESIAN_POINT('Ctrl Pts',(3.29440658299994,2.2,-3.35683734200002));
#354768=CARTESIAN_POINT('Ctrl Pts',(3.29692869199994,12.2,-3.35744860900002));
#354769=CARTESIAN_POINT('Ctrl Pts',(3.29692869199994,5.2,-3.35744860900002));
#354770=CARTESIAN_POINT('Ctrl Pts',(3.29692869199994,2.2,-3.35744860900002));
#354771=CARTESIAN_POINT('Ctrl Pts',(3.29945477899994,12.2,-3.35805805000001));
#354772=CARTESIAN_POINT('Ctrl Pts',(3.29945477899994,5.2,-3.35805805000001));
#354773=CARTESIAN_POINT('Ctrl Pts',(3.29945477899994,2.2,-3.35805805000001));
#354774=CARTESIAN_POINT('Ctrl Pts',(3.30198483999995,12.2,-3.35866565600002));
#354775=CARTESIAN_POINT('Ctrl Pts',(3.30198483999995,5.2,-3.35866565600002));
#354776=CARTESIAN_POINT('Ctrl Pts',(3.30198483999995,2.2,-3.35866565600002));
#354777=CARTESIAN_POINT('Ctrl Pts',(3.30451886899994,12.2,-3.35927142000001));
#354778=CARTESIAN_POINT('Ctrl Pts',(3.30451886899994,5.2,-3.35927142000001));
#354779=CARTESIAN_POINT('Ctrl Pts',(3.30451886899994,2.2,-3.35927142000001));
#354780=CARTESIAN_POINT('Ctrl Pts',(3.30705686199994,12.2,-3.35987533600001));
#354781=CARTESIAN_POINT('Ctrl Pts',(3.30705686199994,5.2,-3.35987533600001));
#354782=CARTESIAN_POINT('Ctrl Pts',(3.30705686199994,2.2,-3.35987533600001));
#354783=CARTESIAN_POINT('Ctrl Pts',(3.30959881599994,12.2,-3.36047739500001));
#354784=CARTESIAN_POINT('Ctrl Pts',(3.30959881599994,5.2,-3.36047739500001));
#354785=CARTESIAN_POINT('Ctrl Pts',(3.30959881599994,2.2,-3.36047739500001));
#354786=CARTESIAN_POINT('Ctrl Pts',(3.31214472499994,12.2,-3.36107759100001));
#354787=CARTESIAN_POINT('Ctrl Pts',(3.31214472499994,5.2,-3.36107759100001));
#354788=CARTESIAN_POINT('Ctrl Pts',(3.31214472499994,2.2,-3.36107759100001));
#354789=CARTESIAN_POINT('Ctrl Pts',(3.31469458699994,12.2,-3.36167591800002));
#354790=CARTESIAN_POINT('Ctrl Pts',(3.31469458699994,5.2,-3.36167591800002));
#354791=CARTESIAN_POINT('Ctrl Pts',(3.31469458699994,2.2,-3.36167591800002));
#354792=CARTESIAN_POINT('Ctrl Pts',(3.31724839599994,12.2,-3.36227237000001));
#354793=CARTESIAN_POINT('Ctrl Pts',(3.31724839599994,5.2,-3.36227237000001));
#354794=CARTESIAN_POINT('Ctrl Pts',(3.31724839599994,2.2,-3.36227237000001));
#354795=CARTESIAN_POINT('Ctrl Pts',(3.31980614799994,12.2,-3.36286693800002));
#354796=CARTESIAN_POINT('Ctrl Pts',(3.31980614799994,5.2,-3.36286693800002));
#354797=CARTESIAN_POINT('Ctrl Pts',(3.31980614799994,2.2,-3.36286693800002));
#354798=CARTESIAN_POINT('Ctrl Pts',(3.32236783799994,12.2,-3.36345961400002));
#354799=CARTESIAN_POINT('Ctrl Pts',(3.32236783799994,5.2,-3.36345961400002));
#354800=CARTESIAN_POINT('Ctrl Pts',(3.32236783799994,2.2,-3.36345961400002));
#354801=CARTESIAN_POINT('Ctrl Pts',(3.32493346199994,12.2,-3.36405038900002));
#354802=CARTESIAN_POINT('Ctrl Pts',(3.32493346199994,5.2,-3.36405038900002));
#354803=CARTESIAN_POINT('Ctrl Pts',(3.32493346199994,2.2,-3.36405038900002));
#354804=CARTESIAN_POINT('Ctrl Pts',(3.32750301199995,12.2,-3.36463925400002));
#354805=CARTESIAN_POINT('Ctrl Pts',(3.32750301199995,5.2,-3.36463925400002));
#354806=CARTESIAN_POINT('Ctrl Pts',(3.32750301199995,2.2,-3.36463925400002));
#354807=CARTESIAN_POINT('Ctrl Pts',(3.33007648399994,12.2,-3.36522620100002));
#354808=CARTESIAN_POINT('Ctrl Pts',(3.33007648399994,5.2,-3.36522620100002));
#354809=CARTESIAN_POINT('Ctrl Pts',(3.33007648399994,2.2,-3.36522620100002));
#354810=CARTESIAN_POINT('Ctrl Pts',(3.33265387199994,12.2,-3.36581122000001));
#354811=CARTESIAN_POINT('Ctrl Pts',(3.33265387199994,5.2,-3.36581122000001));
#354812=CARTESIAN_POINT('Ctrl Pts',(3.33265387199994,2.2,-3.36581122000001));
#354813=CARTESIAN_POINT('Ctrl Pts',(3.33523517199994,12.2,-3.36639430500002));
#354814=CARTESIAN_POINT('Ctrl Pts',(3.33523517199994,5.2,-3.36639430500002));
#354815=CARTESIAN_POINT('Ctrl Pts',(3.33523517199994,2.2,-3.36639430500002));
#354816=CARTESIAN_POINT('Ctrl Pts',(3.33782038099995,12.2,-3.36697545100002));
#354817=CARTESIAN_POINT('Ctrl Pts',(3.33782038099995,5.2,-3.36697545100002));
#354818=CARTESIAN_POINT('Ctrl Pts',(3.33782038099995,2.2,-3.36697545100002));
#354819=CARTESIAN_POINT('Ctrl Pts',(3.34040949499995,12.2,-3.36755465400001));
#354820=CARTESIAN_POINT('Ctrl Pts',(3.34040949499995,5.2,-3.36755465400001));
#354821=CARTESIAN_POINT('Ctrl Pts',(3.34040949499995,2.2,-3.36755465400001));
#354822=CARTESIAN_POINT('Ctrl Pts',(3.34300251499994,12.2,-3.36813191300001));
#354823=CARTESIAN_POINT('Ctrl Pts',(3.34300251499994,5.2,-3.36813191300001));
#354824=CARTESIAN_POINT('Ctrl Pts',(3.34300251499994,2.2,-3.36813191300001));
#354825=CARTESIAN_POINT('Ctrl Pts',(3.34508005499994,12.2,-3.36859216300001));
#354826=CARTESIAN_POINT('Ctrl Pts',(3.34508005499994,5.2,-3.36859216300001));
#354827=CARTESIAN_POINT('Ctrl Pts',(3.34508005499994,2.2,-3.36859216300001));
#354828=CARTESIAN_POINT('Ctrl Pts',(3.34663996599994,12.2,-3.36893647500002));
#354829=CARTESIAN_POINT('Ctrl Pts',(3.34663996599994,5.2,-3.36893647500002));
#354830=CARTESIAN_POINT('Ctrl Pts',(3.34663996599994,2.2,-3.36893647500002));
#354831=CARTESIAN_POINT('Ctrl Pts',(3.34768068699994,12.2,-3.36916562700001));
#354832=CARTESIAN_POINT('Ctrl Pts',(3.34768068699994,5.2,-3.36916562700001));
#354833=CARTESIAN_POINT('Ctrl Pts',(3.34768068699994,2.2,-3.36916562700001));
#354834=CARTESIAN_POINT('Ctrl Pts',(3.34820124399994,12.2,-3.36928010500001));
#354835=CARTESIAN_POINT('Ctrl Pts',(3.34820124399994,5.2,-3.36928010500001));
#354836=CARTESIAN_POINT('Ctrl Pts',(3.34820124399994,2.2,-3.36928010500001));
#354837=CARTESIAN_POINT('',(2.60456064899994,12.2,-3.02756105800002));
#354838=CARTESIAN_POINT('Origin',(-5.66300478732629E-14,15.2,-1.77635683940025E-14));
#354839=CARTESIAN_POINT('',(2.36409006999994,12.2,-2.74803623300001));
#354840=CARTESIAN_POINT('Origin',(-5.66300478732629E-14,15.2,-1.77635683940025E-14));
#354841=CARTESIAN_POINT('Origin',(-5.66300478732629E-14,15.2,-1.77635683940025E-14));
#354842=CARTESIAN_POINT('',(1.91153447899994,2.2,-3.08004235900002));
#354843=CARTESIAN_POINT('Origin',(-5.66300478732629E-14,15.2,-1.77635683940025E-14));
#354844=CARTESIAN_POINT('',(1.33499927399995,12.2,-3.76399243800002));
#354845=CARTESIAN_POINT('',(1.21174314999994,12.2,-3.41647530900001));
#354846=CARTESIAN_POINT('Origin',(2.10595395499994,15.2,-3.39330912400001));
#354847=CARTESIAN_POINT('',(2.10598101599994,12.2,-3.39335272700001));
#354848=CARTESIAN_POINT('Ctrl Pts',(2.20867500599994,12.2,-4.20526511900002));
#354849=CARTESIAN_POINT('Ctrl Pts',(2.20867500599994,5.2,-4.20526511900002));
#354850=CARTESIAN_POINT('Ctrl Pts',(2.20867500599994,2.2,-4.20526511900002));
#354851=CARTESIAN_POINT('Ctrl Pts',(2.20872208699994,12.2,-4.20473420700001));
#354852=CARTESIAN_POINT('Ctrl Pts',(2.20872208699994,5.2,-4.20473420700001));
#354853=CARTESIAN_POINT('Ctrl Pts',(2.20872208699994,2.2,-4.20473420700001));
#354854=CARTESIAN_POINT('Ctrl Pts',(2.20881594599994,12.2,-4.20367269700002));
#354855=CARTESIAN_POINT('Ctrl Pts',(2.20881594599994,5.2,-4.20367269700002));
#354856=CARTESIAN_POINT('Ctrl Pts',(2.20881594599994,2.2,-4.20367269700002));
#354857=CARTESIAN_POINT('Ctrl Pts',(2.20895582799994,12.2,-4.20208137500001));
#354858=CARTESIAN_POINT('Ctrl Pts',(2.20895582799994,5.2,-4.20208137500001));
#354859=CARTESIAN_POINT('Ctrl Pts',(2.20895582799994,2.2,-4.20208137500001));
#354860=CARTESIAN_POINT('Ctrl Pts',(2.20914051899994,12.2,-4.19996149500002));
#354861=CARTESIAN_POINT('Ctrl Pts',(2.20914051899994,5.2,-4.19996149500002));
#354862=CARTESIAN_POINT('Ctrl Pts',(2.20914051899994,2.2,-4.19996149500002));
#354863=CARTESIAN_POINT('Ctrl Pts',(2.20936835599994,12.2,-4.19731478600001));
#354864=CARTESIAN_POINT('Ctrl Pts',(2.20936835599994,5.2,-4.19731478600001));
#354865=CARTESIAN_POINT('Ctrl Pts',(2.20936835599994,2.2,-4.19731478600001));
#354866=CARTESIAN_POINT('Ctrl Pts',(2.20959316499994,12.2,-4.19467121700002));
#354867=CARTESIAN_POINT('Ctrl Pts',(2.20959316499994,5.2,-4.19467121700002));
#354868=CARTESIAN_POINT('Ctrl Pts',(2.20959316499994,2.2,-4.19467121700002));
#354869=CARTESIAN_POINT('Ctrl Pts',(2.20981494699994,12.2,-4.19203079200001));
#354870=CARTESIAN_POINT('Ctrl Pts',(2.20981494699994,5.2,-4.19203079200001));
#354871=CARTESIAN_POINT('Ctrl Pts',(2.20981494699994,2.2,-4.19203079200001));
#354872=CARTESIAN_POINT('Ctrl Pts',(2.21003370799994,12.2,-4.18939351300001));
#354873=CARTESIAN_POINT('Ctrl Pts',(2.21003370799994,5.2,-4.18939351300001));
#354874=CARTESIAN_POINT('Ctrl Pts',(2.21003370799994,2.2,-4.18939351300001));
#354875=CARTESIAN_POINT('Ctrl Pts',(2.21024944899994,12.2,-4.18675938500002));
#354876=CARTESIAN_POINT('Ctrl Pts',(2.21024944899994,5.2,-4.18675938500002));
#354877=CARTESIAN_POINT('Ctrl Pts',(2.21024944899994,2.2,-4.18675938500002));
#354878=CARTESIAN_POINT('Ctrl Pts',(2.21046217399994,12.2,-4.18412841400002));
#354879=CARTESIAN_POINT('Ctrl Pts',(2.21046217399994,5.2,-4.18412841400002));
#354880=CARTESIAN_POINT('Ctrl Pts',(2.21046217399994,2.2,-4.18412841400002));
#354881=CARTESIAN_POINT('Ctrl Pts',(2.21067189399994,12.2,-4.18150060600002));
#354882=CARTESIAN_POINT('Ctrl Pts',(2.21067189399994,5.2,-4.18150060600002));
#354883=CARTESIAN_POINT('Ctrl Pts',(2.21067189399994,2.2,-4.18150060600002));
#354884=CARTESIAN_POINT('Ctrl Pts',(2.21087861199994,12.2,-4.17887597200002));
#354885=CARTESIAN_POINT('Ctrl Pts',(2.21087861199994,5.2,-4.17887597200002));
#354886=CARTESIAN_POINT('Ctrl Pts',(2.21087861199994,2.2,-4.17887597200002));
#354887=CARTESIAN_POINT('Ctrl Pts',(2.21108233599994,12.2,-4.17625451800001));
#354888=CARTESIAN_POINT('Ctrl Pts',(2.21108233599994,5.2,-4.17625451800001));
#354889=CARTESIAN_POINT('Ctrl Pts',(2.21108233599994,2.2,-4.17625451800001));
#354890=CARTESIAN_POINT('Ctrl Pts',(2.21128307299994,12.2,-4.17363625300001));
#354891=CARTESIAN_POINT('Ctrl Pts',(2.21128307299994,5.2,-4.17363625300001));
#354892=CARTESIAN_POINT('Ctrl Pts',(2.21128307299994,2.2,-4.17363625300001));
#354893=CARTESIAN_POINT('Ctrl Pts',(2.21148083099994,12.2,-4.17102118400001));
#354894=CARTESIAN_POINT('Ctrl Pts',(2.21148083099994,5.2,-4.17102118400001));
#354895=CARTESIAN_POINT('Ctrl Pts',(2.21148083099994,2.2,-4.17102118400001));
#354896=CARTESIAN_POINT('Ctrl Pts',(2.21167561299994,12.2,-4.16840931700001));
#354897=CARTESIAN_POINT('Ctrl Pts',(2.21167561299994,5.2,-4.16840931700001));
#354898=CARTESIAN_POINT('Ctrl Pts',(2.21167561299994,2.2,-4.16840931700001));
#354899=CARTESIAN_POINT('Ctrl Pts',(2.21186742599994,12.2,-4.16580065900002));
#354900=CARTESIAN_POINT('Ctrl Pts',(2.21186742599994,5.2,-4.16580065900002));
#354901=CARTESIAN_POINT('Ctrl Pts',(2.21186742599994,2.2,-4.16580065900002));
#354902=CARTESIAN_POINT('Ctrl Pts',(2.21205627499994,12.2,-4.16319521500002));
#354903=CARTESIAN_POINT('Ctrl Pts',(2.21205627499994,5.2,-4.16319521500002));
#354904=CARTESIAN_POINT('Ctrl Pts',(2.21205627499994,2.2,-4.16319521500002));
#354905=CARTESIAN_POINT('Ctrl Pts',(2.21224216399994,12.2,-4.16059299100001));
#354906=CARTESIAN_POINT('Ctrl Pts',(2.21224216399994,5.2,-4.16059299100001));
#354907=CARTESIAN_POINT('Ctrl Pts',(2.21224216399994,2.2,-4.16059299100001));
#354908=CARTESIAN_POINT('Ctrl Pts',(2.21242509999994,12.2,-4.15799399300001));
#354909=CARTESIAN_POINT('Ctrl Pts',(2.21242509999994,5.2,-4.15799399300001));
#354910=CARTESIAN_POINT('Ctrl Pts',(2.21242509999994,2.2,-4.15799399300001));
#354911=CARTESIAN_POINT('Ctrl Pts',(2.21260508699994,12.2,-4.15539822800001));
#354912=CARTESIAN_POINT('Ctrl Pts',(2.21260508699994,5.2,-4.15539822800001));
#354913=CARTESIAN_POINT('Ctrl Pts',(2.21260508699994,2.2,-4.15539822800001));
#354914=CARTESIAN_POINT('Ctrl Pts',(2.21278213099994,12.2,-4.15280570200002));
#354915=CARTESIAN_POINT('Ctrl Pts',(2.21278213099994,5.2,-4.15280570200002));
#354916=CARTESIAN_POINT('Ctrl Pts',(2.21278213099994,2.2,-4.15280570200002));
#354917=CARTESIAN_POINT('Ctrl Pts',(2.21295623999994,12.2,-4.15021642300001));
#354918=CARTESIAN_POINT('Ctrl Pts',(2.21295623999994,5.2,-4.15021642300001));
#354919=CARTESIAN_POINT('Ctrl Pts',(2.21295623999994,2.2,-4.15021642300001));
#354920=CARTESIAN_POINT('Ctrl Pts',(2.21312741799994,12.2,-4.14763039500002));
#354921=CARTESIAN_POINT('Ctrl Pts',(2.21312741799994,5.2,-4.14763039500002));
#354922=CARTESIAN_POINT('Ctrl Pts',(2.21312741799994,2.2,-4.14763039500002));
#354923=CARTESIAN_POINT('Ctrl Pts',(2.21329566999994,12.2,-4.14504762800001));
#354924=CARTESIAN_POINT('Ctrl Pts',(2.21329566999994,5.2,-4.14504762800001));
#354925=CARTESIAN_POINT('Ctrl Pts',(2.21329566999994,2.2,-4.14504762800001));
#354926=CARTESIAN_POINT('Ctrl Pts',(2.21346100499995,12.2,-4.14246812800001));
#354927=CARTESIAN_POINT('Ctrl Pts',(2.21346100499995,5.2,-4.14246812800001));
#354928=CARTESIAN_POINT('Ctrl Pts',(2.21346100499995,2.2,-4.14246812800001));
#354929=CARTESIAN_POINT('Ctrl Pts',(2.21362342699994,12.2,-4.13989189900001));
#354930=CARTESIAN_POINT('Ctrl Pts',(2.21362342699994,5.2,-4.13989189900001));
#354931=CARTESIAN_POINT('Ctrl Pts',(2.21362342699994,2.2,-4.13989189900001));
#354932=CARTESIAN_POINT('Ctrl Pts',(2.21378294299994,12.2,-4.13731895000002));
#354933=CARTESIAN_POINT('Ctrl Pts',(2.21378294299994,5.2,-4.13731895000002));
#354934=CARTESIAN_POINT('Ctrl Pts',(2.21378294299994,2.2,-4.13731895000002));
#354935=CARTESIAN_POINT('Ctrl Pts',(2.21393955699994,12.2,-4.13474928700001));
#354936=CARTESIAN_POINT('Ctrl Pts',(2.21393955699994,5.2,-4.13474928700001));
#354937=CARTESIAN_POINT('Ctrl Pts',(2.21393955699994,2.2,-4.13474928700001));
#354938=CARTESIAN_POINT('Ctrl Pts',(2.21409327699994,12.2,-4.13218291600002));
#354939=CARTESIAN_POINT('Ctrl Pts',(2.21409327699994,5.2,-4.13218291600002));
#354940=CARTESIAN_POINT('Ctrl Pts',(2.21409327699994,2.2,-4.13218291600002));
#354941=CARTESIAN_POINT('Ctrl Pts',(2.21424410699994,12.2,-4.12961984400001));
#354942=CARTESIAN_POINT('Ctrl Pts',(2.21424410699994,5.2,-4.12961984400001));
#354943=CARTESIAN_POINT('Ctrl Pts',(2.21424410699994,2.2,-4.12961984400001));
#354944=CARTESIAN_POINT('Ctrl Pts',(2.21439205399994,12.2,-4.12706007600002));
#354945=CARTESIAN_POINT('Ctrl Pts',(2.21439205399994,5.2,-4.12706007600002));
#354946=CARTESIAN_POINT('Ctrl Pts',(2.21439205399994,2.2,-4.12706007600002));
#354947=CARTESIAN_POINT('Ctrl Pts',(2.21453712299994,12.2,-4.12450362100001));
#354948=CARTESIAN_POINT('Ctrl Pts',(2.21453712299994,5.2,-4.12450362100001));
#354949=CARTESIAN_POINT('Ctrl Pts',(2.21453712299994,2.2,-4.12450362100001));
#354950=CARTESIAN_POINT('Ctrl Pts',(2.21467932099995,12.2,-4.12195048400001));
#354951=CARTESIAN_POINT('Ctrl Pts',(2.21467932099995,5.2,-4.12195048400001));
#354952=CARTESIAN_POINT('Ctrl Pts',(2.21467932099995,2.2,-4.12195048400001));
#354953=CARTESIAN_POINT('Ctrl Pts',(2.21481865199994,12.2,-4.11940067100002));
#354954=CARTESIAN_POINT('Ctrl Pts',(2.21481865199994,5.2,-4.11940067100002));
#354955=CARTESIAN_POINT('Ctrl Pts',(2.21481865199994,2.2,-4.11940067100002));
#354956=CARTESIAN_POINT('Ctrl Pts',(2.21495512599994,12.2,-4.11685419000001));
#354957=CARTESIAN_POINT('Ctrl Pts',(2.21495512599994,5.2,-4.11685419000001));
#354958=CARTESIAN_POINT('Ctrl Pts',(2.21495512599994,2.2,-4.11685419000001));
#354959=CARTESIAN_POINT('Ctrl Pts',(2.21508874499994,12.2,-4.11431104600001));
#354960=CARTESIAN_POINT('Ctrl Pts',(2.21508874499994,5.2,-4.11431104600001));
#354961=CARTESIAN_POINT('Ctrl Pts',(2.21508874499994,2.2,-4.11431104600001));
#354962=CARTESIAN_POINT('Ctrl Pts',(2.21521951699994,12.2,-4.11177124700002));
#354963=CARTESIAN_POINT('Ctrl Pts',(2.21521951699994,5.2,-4.11177124700002));
#354964=CARTESIAN_POINT('Ctrl Pts',(2.21521951699994,2.2,-4.11177124700002));
#354965=CARTESIAN_POINT('Ctrl Pts',(2.21534744799994,12.2,-4.10923479900001));
#354966=CARTESIAN_POINT('Ctrl Pts',(2.21534744799994,5.2,-4.10923479900001));
#354967=CARTESIAN_POINT('Ctrl Pts',(2.21534744799994,2.2,-4.10923479900001));
#354968=CARTESIAN_POINT('Ctrl Pts',(2.21547254299994,12.2,-4.10670170900001));
#354969=CARTESIAN_POINT('Ctrl Pts',(2.21547254299994,5.2,-4.10670170900001));
#354970=CARTESIAN_POINT('Ctrl Pts',(2.21547254299994,2.2,-4.10670170900001));
#354971=CARTESIAN_POINT('Ctrl Pts',(2.21559480899994,12.2,-4.10417198300001));
#354972=CARTESIAN_POINT('Ctrl Pts',(2.21559480899994,5.2,-4.10417198300001));
#354973=CARTESIAN_POINT('Ctrl Pts',(2.21559480899994,2.2,-4.10417198300001));
#354974=CARTESIAN_POINT('Ctrl Pts',(2.21571425199994,12.2,-4.10164562700002));
#354975=CARTESIAN_POINT('Ctrl Pts',(2.21571425199994,5.2,-4.10164562700002));
#354976=CARTESIAN_POINT('Ctrl Pts',(2.21571425199994,2.2,-4.10164562700002));
#354977=CARTESIAN_POINT('Ctrl Pts',(2.21583087799994,12.2,-4.09912264800001));
#354978=CARTESIAN_POINT('Ctrl Pts',(2.21583087799994,5.2,-4.09912264800001));
#354979=CARTESIAN_POINT('Ctrl Pts',(2.21583087799994,2.2,-4.09912264800001));
#354980=CARTESIAN_POINT('Ctrl Pts',(2.21594469199994,12.2,-4.09660305300001));
#354981=CARTESIAN_POINT('Ctrl Pts',(2.21594469199994,5.2,-4.09660305300001));
#354982=CARTESIAN_POINT('Ctrl Pts',(2.21594469199994,2.2,-4.09660305300001));
#354983=CARTESIAN_POINT('Ctrl Pts',(2.21605570199995,12.2,-4.09408684800002));
#354984=CARTESIAN_POINT('Ctrl Pts',(2.21605570199995,5.2,-4.09408684800002));
#354985=CARTESIAN_POINT('Ctrl Pts',(2.21605570199995,2.2,-4.09408684800002));
#354986=CARTESIAN_POINT('Ctrl Pts',(2.21616391399994,12.2,-4.09157403900001));
#354987=CARTESIAN_POINT('Ctrl Pts',(2.21616391399994,5.2,-4.09157403900001));
#354988=CARTESIAN_POINT('Ctrl Pts',(2.21616391399994,2.2,-4.09157403900001));
#354989=CARTESIAN_POINT('Ctrl Pts',(2.21626933299994,12.2,-4.08906463400001));
#354990=CARTESIAN_POINT('Ctrl Pts',(2.21626933299994,5.2,-4.08906463400001));
#354991=CARTESIAN_POINT('Ctrl Pts',(2.21626933299994,2.2,-4.08906463400001));
#354992=CARTESIAN_POINT('Ctrl Pts',(2.21637196599994,12.2,-4.08655863900002));
#354993=CARTESIAN_POINT('Ctrl Pts',(2.21637196599994,5.2,-4.08655863900002));
#354994=CARTESIAN_POINT('Ctrl Pts',(2.21637196599994,2.2,-4.08655863900002));
#354995=CARTESIAN_POINT('Ctrl Pts',(2.21647181899994,12.2,-4.08405605900001));
#354996=CARTESIAN_POINT('Ctrl Pts',(2.21647181899994,5.2,-4.08405605900001));
#354997=CARTESIAN_POINT('Ctrl Pts',(2.21647181899994,2.2,-4.08405605900001));
#354998=CARTESIAN_POINT('Ctrl Pts',(2.21656889799994,12.2,-4.08155690200001));
#354999=CARTESIAN_POINT('Ctrl Pts',(2.21656889799994,5.2,-4.08155690200001));
#355000=CARTESIAN_POINT('Ctrl Pts',(2.21656889799994,2.2,-4.08155690200001));
#355001=CARTESIAN_POINT('Ctrl Pts',(2.21666320899994,12.2,-4.07906117500001));
#355002=CARTESIAN_POINT('Ctrl Pts',(2.21666320899994,5.2,-4.07906117500001));
#355003=CARTESIAN_POINT('Ctrl Pts',(2.21666320899994,2.2,-4.07906117500001));
#355004=CARTESIAN_POINT('Ctrl Pts',(2.21675475899994,12.2,-4.07656888400002));
#355005=CARTESIAN_POINT('Ctrl Pts',(2.21675475899994,5.2,-4.07656888400002));
#355006=CARTESIAN_POINT('Ctrl Pts',(2.21675475899994,2.2,-4.07656888400002));
#355007=CARTESIAN_POINT('Ctrl Pts',(2.21684355399994,12.2,-4.07408003500001));
#355008=CARTESIAN_POINT('Ctrl Pts',(2.21684355399994,5.2,-4.07408003500001));
#355009=CARTESIAN_POINT('Ctrl Pts',(2.21684355399994,2.2,-4.07408003500001));
#355010=CARTESIAN_POINT('Ctrl Pts',(2.21692959999995,12.2,-4.07159463400002));
#355011=CARTESIAN_POINT('Ctrl Pts',(2.21692959999995,5.2,-4.07159463400002));
#355012=CARTESIAN_POINT('Ctrl Pts',(2.21692959999995,2.2,-4.07159463400002));
#355013=CARTESIAN_POINT('Ctrl Pts',(2.21701290399994,12.2,-4.06911268900001));
#355014=CARTESIAN_POINT('Ctrl Pts',(2.21701290399994,5.2,-4.06911268900001));
#355015=CARTESIAN_POINT('Ctrl Pts',(2.21701290399994,2.2,-4.06911268900001));
#355016=CARTESIAN_POINT('Ctrl Pts',(2.21709347199994,12.2,-4.06663420700001));
#355017=CARTESIAN_POINT('Ctrl Pts',(2.21709347199994,5.2,-4.06663420700001));
#355018=CARTESIAN_POINT('Ctrl Pts',(2.21709347199994,2.2,-4.06663420700001));
#355019=CARTESIAN_POINT('Ctrl Pts',(2.21717130999994,12.2,-4.06415919200001));
#355020=CARTESIAN_POINT('Ctrl Pts',(2.21717130999994,5.2,-4.06415919200001));
#355021=CARTESIAN_POINT('Ctrl Pts',(2.21717130999994,2.2,-4.06415919200001));
#355022=CARTESIAN_POINT('Ctrl Pts',(2.21724642399994,12.2,-4.06168765200002));
#355023=CARTESIAN_POINT('Ctrl Pts',(2.21724642399994,5.2,-4.06168765200002));
#355024=CARTESIAN_POINT('Ctrl Pts',(2.21724642399994,2.2,-4.06168765200002));
#355025=CARTESIAN_POINT('Ctrl Pts',(2.21731882199994,12.2,-4.05921959500001));
#355026=CARTESIAN_POINT('Ctrl Pts',(2.21731882199994,5.2,-4.05921959500001));
#355027=CARTESIAN_POINT('Ctrl Pts',(2.21731882199994,2.2,-4.05921959500001));
#355028=CARTESIAN_POINT('Ctrl Pts',(2.21738850899994,12.2,-4.05675502500001));
#355029=CARTESIAN_POINT('Ctrl Pts',(2.21738850899994,5.2,-4.05675502500001));
#355030=CARTESIAN_POINT('Ctrl Pts',(2.21738850899994,2.2,-4.05675502500001));
#355031=CARTESIAN_POINT('Ctrl Pts',(2.21745549199994,12.2,-4.05429394900001));
#355032=CARTESIAN_POINT('Ctrl Pts',(2.21745549199994,5.2,-4.05429394900001));
#355033=CARTESIAN_POINT('Ctrl Pts',(2.21745549199994,2.2,-4.05429394900001));
#355034=CARTESIAN_POINT('Ctrl Pts',(2.21751977599994,12.2,-4.05183637500001));
#355035=CARTESIAN_POINT('Ctrl Pts',(2.21751977599994,5.2,-4.05183637500001));
#355036=CARTESIAN_POINT('Ctrl Pts',(2.21751977599994,2.2,-4.05183637500001));
#355037=CARTESIAN_POINT('Ctrl Pts',(2.21758136999994,12.2,-4.04938230800001));
#355038=CARTESIAN_POINT('Ctrl Pts',(2.21758136999994,5.2,-4.04938230800001));
#355039=CARTESIAN_POINT('Ctrl Pts',(2.21758136999994,2.2,-4.04938230800001));
#355040=CARTESIAN_POINT('Ctrl Pts',(2.21764027799995,12.2,-4.04693175500002));
#355041=CARTESIAN_POINT('Ctrl Pts',(2.21764027799995,5.2,-4.04693175500002));
#355042=CARTESIAN_POINT('Ctrl Pts',(2.21764027799995,2.2,-4.04693175500002));
#355043=CARTESIAN_POINT('Ctrl Pts',(2.21769650799994,12.2,-4.04448472300002));
#355044=CARTESIAN_POINT('Ctrl Pts',(2.21769650799994,5.2,-4.04448472300002));
#355045=CARTESIAN_POINT('Ctrl Pts',(2.21769650799994,2.2,-4.04448472300002));
#355046=CARTESIAN_POINT('Ctrl Pts',(2.21775006599994,12.2,-4.04204121900001));
#355047=CARTESIAN_POINT('Ctrl Pts',(2.21775006599994,5.2,-4.04204121900001));
#355048=CARTESIAN_POINT('Ctrl Pts',(2.21775006599994,2.2,-4.04204121900001));
#355049=CARTESIAN_POINT('Ctrl Pts',(2.21780095899994,12.2,-4.03960124700002));
#355050=CARTESIAN_POINT('Ctrl Pts',(2.21780095899994,5.2,-4.03960124700002));
#355051=CARTESIAN_POINT('Ctrl Pts',(2.21780095899994,2.2,-4.03960124700002));
#355052=CARTESIAN_POINT('Ctrl Pts',(2.21784919199994,12.2,-4.03716481500001));
#355053=CARTESIAN_POINT('Ctrl Pts',(2.21784919199994,5.2,-4.03716481500001));
#355054=CARTESIAN_POINT('Ctrl Pts',(2.21784919199994,2.2,-4.03716481500001));
#355055=CARTESIAN_POINT('Ctrl Pts',(2.21789477399994,12.2,-4.03473193200002));
#355056=CARTESIAN_POINT('Ctrl Pts',(2.21789477399994,5.2,-4.03473193200002));
#355057=CARTESIAN_POINT('Ctrl Pts',(2.21789477399994,2.2,-4.03473193200002));
#355058=CARTESIAN_POINT('Ctrl Pts',(2.21793770999994,12.2,-4.03230260000001));
#355059=CARTESIAN_POINT('Ctrl Pts',(2.21793770999994,5.2,-4.03230260000001));
#355060=CARTESIAN_POINT('Ctrl Pts',(2.21793770999994,2.2,-4.03230260000001));
#355061=CARTESIAN_POINT('Ctrl Pts',(2.21797800499994,12.2,-4.02987682900001));
#355062=CARTESIAN_POINT('Ctrl Pts',(2.21797800499994,5.2,-4.02987682900001));
#355063=CARTESIAN_POINT('Ctrl Pts',(2.21797800499994,2.2,-4.02987682900001));
#355064=CARTESIAN_POINT('Ctrl Pts',(2.21801566999994,12.2,-4.02745462400001));
#355065=CARTESIAN_POINT('Ctrl Pts',(2.21801566999994,5.2,-4.02745462400001));
#355066=CARTESIAN_POINT('Ctrl Pts',(2.21801566999994,2.2,-4.02745462400001));
#355067=CARTESIAN_POINT('Ctrl Pts',(2.21805070699994,12.2,-4.02503599200001));
#355068=CARTESIAN_POINT('Ctrl Pts',(2.21805070699994,5.2,-4.02503599200001));
#355069=CARTESIAN_POINT('Ctrl Pts',(2.21805070699994,2.2,-4.02503599200001));
#355070=CARTESIAN_POINT('Ctrl Pts',(2.21808312599994,12.2,-4.02262093800001));
#355071=CARTESIAN_POINT('Ctrl Pts',(2.21808312599994,5.2,-4.02262093800001));
#355072=CARTESIAN_POINT('Ctrl Pts',(2.21808312599994,2.2,-4.02262093800001));
#355073=CARTESIAN_POINT('Ctrl Pts',(2.21811293099994,12.2,-4.02020947100001));
#355074=CARTESIAN_POINT('Ctrl Pts',(2.21811293099994,5.2,-4.02020947100001));
#355075=CARTESIAN_POINT('Ctrl Pts',(2.21811293099994,2.2,-4.02020947100001));
#355076=CARTESIAN_POINT('Ctrl Pts',(2.21814013099995,12.2,-4.01780159600001));
#355077=CARTESIAN_POINT('Ctrl Pts',(2.21814013099995,5.2,-4.01780159600001));
#355078=CARTESIAN_POINT('Ctrl Pts',(2.21814013099995,2.2,-4.01780159600001));
#355079=CARTESIAN_POINT('Ctrl Pts',(2.21816473099994,12.2,-4.01539731900002));
#355080=CARTESIAN_POINT('Ctrl Pts',(2.21816473099994,5.2,-4.01539731900002));
#355081=CARTESIAN_POINT('Ctrl Pts',(2.21816473099994,2.2,-4.01539731900002));
#355082=CARTESIAN_POINT('Ctrl Pts',(2.21818673899994,12.2,-4.01299664900002));
#355083=CARTESIAN_POINT('Ctrl Pts',(2.21818673899994,5.2,-4.01299664900002));
#355084=CARTESIAN_POINT('Ctrl Pts',(2.21818673899994,2.2,-4.01299664900002));
#355085=CARTESIAN_POINT('Ctrl Pts',(2.21820616099994,12.2,-4.01059959000001));
#355086=CARTESIAN_POINT('Ctrl Pts',(2.21820616099994,5.2,-4.01059959000001));
#355087=CARTESIAN_POINT('Ctrl Pts',(2.21820616099994,2.2,-4.01059959000001));
#355088=CARTESIAN_POINT('Ctrl Pts',(2.21822300299995,12.2,-4.00820614800002));
#355089=CARTESIAN_POINT('Ctrl Pts',(2.21822300299995,5.2,-4.00820614800002));
#355090=CARTESIAN_POINT('Ctrl Pts',(2.21822300299995,2.2,-4.00820614800002));
#355091=CARTESIAN_POINT('Ctrl Pts',(2.21823727299994,12.2,-4.00581633300002));
#355092=CARTESIAN_POINT('Ctrl Pts',(2.21823727299994,5.2,-4.00581633300002));
#355093=CARTESIAN_POINT('Ctrl Pts',(2.21823727299994,2.2,-4.00581633300002));
#355094=CARTESIAN_POINT('Ctrl Pts',(2.21824897699994,12.2,-4.00343014800002));
#355095=CARTESIAN_POINT('Ctrl Pts',(2.21824897699994,5.2,-4.00343014800002));
#355096=CARTESIAN_POINT('Ctrl Pts',(2.21824897699994,2.2,-4.00343014800002));
#355097=CARTESIAN_POINT('Ctrl Pts',(2.21825812299994,12.2,-4.00104760200001));
#355098=CARTESIAN_POINT('Ctrl Pts',(2.21825812299994,5.2,-4.00104760200001));
#355099=CARTESIAN_POINT('Ctrl Pts',(2.21825812299994,2.2,-4.00104760200001));
#355100=CARTESIAN_POINT('Ctrl Pts',(2.21826471699994,12.2,-3.99866870000002));
#355101=CARTESIAN_POINT('Ctrl Pts',(2.21826471699994,5.2,-3.99866870000002));
#355102=CARTESIAN_POINT('Ctrl Pts',(2.21826471699994,2.2,-3.99866870000002));
#355103=CARTESIAN_POINT('Ctrl Pts',(2.21826876399994,12.2,-3.99629344800001));
#355104=CARTESIAN_POINT('Ctrl Pts',(2.21826876399994,5.2,-3.99629344800001));
#355105=CARTESIAN_POINT('Ctrl Pts',(2.21826876399994,2.2,-3.99629344800001));
#355106=CARTESIAN_POINT('Ctrl Pts',(2.21827027499994,12.2,-3.99392185500002));
#355107=CARTESIAN_POINT('Ctrl Pts',(2.21827027499994,5.2,-3.99392185500002));
#355108=CARTESIAN_POINT('Ctrl Pts',(2.21827027499994,2.2,-3.99392185500002));
#355109=CARTESIAN_POINT('Ctrl Pts',(2.21826925299994,12.2,-3.99155392500001));
#355110=CARTESIAN_POINT('Ctrl Pts',(2.21826925299994,5.2,-3.99155392500001));
#355111=CARTESIAN_POINT('Ctrl Pts',(2.21826925299994,2.2,-3.99155392500001));
#355112=CARTESIAN_POINT('Ctrl Pts',(2.21826570699994,12.2,-3.98918966500001));
#355113=CARTESIAN_POINT('Ctrl Pts',(2.21826570699994,5.2,-3.98918966500001));
#355114=CARTESIAN_POINT('Ctrl Pts',(2.21826570699994,2.2,-3.98918966500001));
#355115=CARTESIAN_POINT('Ctrl Pts',(2.21825964399994,12.2,-3.98682908300001));
#355116=CARTESIAN_POINT('Ctrl Pts',(2.21825964399994,5.2,-3.98682908300001));
#355117=CARTESIAN_POINT('Ctrl Pts',(2.21825964399994,2.2,-3.98682908300001));
#355118=CARTESIAN_POINT('Ctrl Pts',(2.21825106799994,12.2,-3.98447218300001));
#355119=CARTESIAN_POINT('Ctrl Pts',(2.21825106799994,5.2,-3.98447218300001));
#355120=CARTESIAN_POINT('Ctrl Pts',(2.21825106799994,2.2,-3.98447218300001));
#355121=CARTESIAN_POINT('Ctrl Pts',(2.21823998999994,12.2,-3.98211897400001));
#355122=CARTESIAN_POINT('Ctrl Pts',(2.21823998999994,5.2,-3.98211897400001));
#355123=CARTESIAN_POINT('Ctrl Pts',(2.21823998999994,2.2,-3.98211897400001));
#355124=CARTESIAN_POINT('Ctrl Pts',(2.21822641399994,12.2,-3.97976946200002));
#355125=CARTESIAN_POINT('Ctrl Pts',(2.21822641399994,5.2,-3.97976946200002));
#355126=CARTESIAN_POINT('Ctrl Pts',(2.21822641399994,2.2,-3.97976946200002));
#355127=CARTESIAN_POINT('Ctrl Pts',(2.21821034899994,12.2,-3.97742365200001));
#355128=CARTESIAN_POINT('Ctrl Pts',(2.21821034899994,5.2,-3.97742365200001));
#355129=CARTESIAN_POINT('Ctrl Pts',(2.21821034899994,2.2,-3.97742365200001));
#355130=CARTESIAN_POINT('Ctrl Pts',(2.21819180099994,12.2,-3.97508155100001));
#355131=CARTESIAN_POINT('Ctrl Pts',(2.21819180099994,5.2,-3.97508155100001));
#355132=CARTESIAN_POINT('Ctrl Pts',(2.21819180099994,2.2,-3.97508155100001));
#355133=CARTESIAN_POINT('Ctrl Pts',(2.21817077599994,12.2,-3.97274316600001));
#355134=CARTESIAN_POINT('Ctrl Pts',(2.21817077599994,5.2,-3.97274316600001));
#355135=CARTESIAN_POINT('Ctrl Pts',(2.21817077599994,2.2,-3.97274316600001));
#355136=CARTESIAN_POINT('Ctrl Pts',(2.21814728299994,12.2,-3.97040850500002));
#355137=CARTESIAN_POINT('Ctrl Pts',(2.21814728299994,5.2,-3.97040850500002));
#355138=CARTESIAN_POINT('Ctrl Pts',(2.21814728299994,2.2,-3.97040850500002));
#355139=CARTESIAN_POINT('Ctrl Pts',(2.21812132799994,12.2,-3.96807757200001));
#355140=CARTESIAN_POINT('Ctrl Pts',(2.21812132799994,5.2,-3.96807757200001));
#355141=CARTESIAN_POINT('Ctrl Pts',(2.21812132799994,2.2,-3.96807757200001));
#355142=CARTESIAN_POINT('Ctrl Pts',(2.21809291799994,12.2,-3.96575037400002));
#355143=CARTESIAN_POINT('Ctrl Pts',(2.21809291799994,5.2,-3.96575037400002));
#355144=CARTESIAN_POINT('Ctrl Pts',(2.21809291799994,2.2,-3.96575037400002));
#355145=CARTESIAN_POINT('Ctrl Pts',(2.21806205999994,12.2,-3.96342691800001));
#355146=CARTESIAN_POINT('Ctrl Pts',(2.21806205999994,5.2,-3.96342691800001));
#355147=CARTESIAN_POINT('Ctrl Pts',(2.21806205999994,2.2,-3.96342691800001));
#355148=CARTESIAN_POINT('Ctrl Pts',(2.21802876299994,12.2,-3.96110721100001));
#355149=CARTESIAN_POINT('Ctrl Pts',(2.21802876299994,5.2,-3.96110721100001));
#355150=CARTESIAN_POINT('Ctrl Pts',(2.21802876299994,2.2,-3.96110721100001));
#355151=CARTESIAN_POINT('Ctrl Pts',(2.21799303099994,12.2,-3.95879125900001));
#355152=CARTESIAN_POINT('Ctrl Pts',(2.21799303099994,5.2,-3.95879125900001));
#355153=CARTESIAN_POINT('Ctrl Pts',(2.21799303099994,2.2,-3.95879125900001));
#355154=CARTESIAN_POINT('Ctrl Pts',(2.21795487199994,12.2,-3.95647906800002));
#355155=CARTESIAN_POINT('Ctrl Pts',(2.21795487199994,5.2,-3.95647906800002));
#355156=CARTESIAN_POINT('Ctrl Pts',(2.21795487199994,2.2,-3.95647906800002));
#355157=CARTESIAN_POINT('Ctrl Pts',(2.21791429499994,12.2,-3.95417064500001));
#355158=CARTESIAN_POINT('Ctrl Pts',(2.21791429499994,5.2,-3.95417064500001));
#355159=CARTESIAN_POINT('Ctrl Pts',(2.21791429499994,2.2,-3.95417064500001));
#355160=CARTESIAN_POINT('Ctrl Pts',(2.21787130599994,12.2,-3.95186599600001));
#355161=CARTESIAN_POINT('Ctrl Pts',(2.21787130599994,5.2,-3.95186599600001));
#355162=CARTESIAN_POINT('Ctrl Pts',(2.21787130599994,2.2,-3.95186599600001));
#355163=CARTESIAN_POINT('Ctrl Pts',(2.21782591199994,12.2,-3.94956512800002));
#355164=CARTESIAN_POINT('Ctrl Pts',(2.21782591199994,5.2,-3.94956512800002));
#355165=CARTESIAN_POINT('Ctrl Pts',(2.21782591199994,2.2,-3.94956512800002));
#355166=CARTESIAN_POINT('Ctrl Pts',(2.21777812099994,12.2,-3.94726804800001));
#355167=CARTESIAN_POINT('Ctrl Pts',(2.21777812099994,5.2,-3.94726804800001));
#355168=CARTESIAN_POINT('Ctrl Pts',(2.21777812099994,2.2,-3.94726804800001));
#355169=CARTESIAN_POINT('Ctrl Pts',(2.21772793799994,12.2,-3.94497476100002));
#355170=CARTESIAN_POINT('Ctrl Pts',(2.21772793799994,5.2,-3.94497476100002));
#355171=CARTESIAN_POINT('Ctrl Pts',(2.21772793799994,2.2,-3.94497476100002));
#355172=CARTESIAN_POINT('Ctrl Pts',(2.21767537399994,12.2,-3.94268527500001));
#355173=CARTESIAN_POINT('Ctrl Pts',(2.21767537399994,5.2,-3.94268527500001));
#355174=CARTESIAN_POINT('Ctrl Pts',(2.21767537399994,2.2,-3.94268527500001));
#355175=CARTESIAN_POINT('Ctrl Pts',(2.21762043199994,12.2,-3.94039959600001));
#355176=CARTESIAN_POINT('Ctrl Pts',(2.21762043199994,5.2,-3.94039959600001));
#355177=CARTESIAN_POINT('Ctrl Pts',(2.21762043199994,2.2,-3.94039959600001));
#355178=CARTESIAN_POINT('Ctrl Pts',(2.21756312299994,12.2,-3.93811773000001));
#355179=CARTESIAN_POINT('Ctrl Pts',(2.21756312299994,5.2,-3.93811773000001));
#355180=CARTESIAN_POINT('Ctrl Pts',(2.21756312299994,2.2,-3.93811773000001));
#355181=CARTESIAN_POINT('Ctrl Pts',(2.21750345199994,12.2,-3.93583968300002));
#355182=CARTESIAN_POINT('Ctrl Pts',(2.21750345199994,5.2,-3.93583968300002));
#355183=CARTESIAN_POINT('Ctrl Pts',(2.21750345199994,2.2,-3.93583968300002));
#355184=CARTESIAN_POINT('Ctrl Pts',(2.21744142799994,12.2,-3.93356546400002));
#355185=CARTESIAN_POINT('Ctrl Pts',(2.21744142799994,5.2,-3.93356546400002));
#355186=CARTESIAN_POINT('Ctrl Pts',(2.21744142799994,2.2,-3.93356546400002));
#355187=CARTESIAN_POINT('Ctrl Pts',(2.21737705699994,12.2,-3.93129507700001));
#355188=CARTESIAN_POINT('Ctrl Pts',(2.21737705699994,5.2,-3.93129507700001));
#355189=CARTESIAN_POINT('Ctrl Pts',(2.21737705699994,2.2,-3.93129507700001));
#355190=CARTESIAN_POINT('Ctrl Pts',(2.21731034499994,12.2,-3.92902852900002));
#355191=CARTESIAN_POINT('Ctrl Pts',(2.21731034499994,5.2,-3.92902852900002));
#355192=CARTESIAN_POINT('Ctrl Pts',(2.21731034499994,2.2,-3.92902852900002));
#355193=CARTESIAN_POINT('Ctrl Pts',(2.21724130399994,12.2,-3.92676582700001));
#355194=CARTESIAN_POINT('Ctrl Pts',(2.21724130399994,5.2,-3.92676582700001));
#355195=CARTESIAN_POINT('Ctrl Pts',(2.21724130399994,2.2,-3.92676582700001));
#355196=CARTESIAN_POINT('Ctrl Pts',(2.21716993699994,12.2,-3.92450697700002));
#355197=CARTESIAN_POINT('Ctrl Pts',(2.21716993699994,5.2,-3.92450697700002));
#355198=CARTESIAN_POINT('Ctrl Pts',(2.21716993699994,2.2,-3.92450697700002));
#355199=CARTESIAN_POINT('Ctrl Pts',(2.21709625399995,12.2,-3.92225198600002));
#355200=CARTESIAN_POINT('Ctrl Pts',(2.21709625399995,5.2,-3.92225198600002));
#355201=CARTESIAN_POINT('Ctrl Pts',(2.21709625399995,2.2,-3.92225198600002));
#355202=CARTESIAN_POINT('Ctrl Pts',(2.21702025999994,12.2,-3.92000086000001));
#355203=CARTESIAN_POINT('Ctrl Pts',(2.21702025999994,5.2,-3.92000086000001));
#355204=CARTESIAN_POINT('Ctrl Pts',(2.21702025999994,2.2,-3.92000086000001));
#355205=CARTESIAN_POINT('Ctrl Pts',(2.21694196499994,12.2,-3.91775360500001));
#355206=CARTESIAN_POINT('Ctrl Pts',(2.21694196499994,5.2,-3.91775360500001));
#355207=CARTESIAN_POINT('Ctrl Pts',(2.21694196499994,2.2,-3.91775360500001));
#355208=CARTESIAN_POINT('Ctrl Pts',(2.21686137499994,12.2,-3.91551022900002));
#355209=CARTESIAN_POINT('Ctrl Pts',(2.21686137499994,5.2,-3.91551022900002));
#355210=CARTESIAN_POINT('Ctrl Pts',(2.21686137499994,2.2,-3.91551022900002));
#355211=CARTESIAN_POINT('Ctrl Pts',(2.21677849799994,12.2,-3.91327073800001));
#355212=CARTESIAN_POINT('Ctrl Pts',(2.21677849799994,5.2,-3.91327073800001));
#355213=CARTESIAN_POINT('Ctrl Pts',(2.21677849799994,2.2,-3.91327073800001));
#355214=CARTESIAN_POINT('Ctrl Pts',(2.21669334199994,12.2,-3.91103513700001));
#355215=CARTESIAN_POINT('Ctrl Pts',(2.21669334199994,5.2,-3.91103513700001));
#355216=CARTESIAN_POINT('Ctrl Pts',(2.21669334199994,2.2,-3.91103513700001));
#355217=CARTESIAN_POINT('Ctrl Pts',(2.21660591299994,12.2,-3.90880343400001));
#355218=CARTESIAN_POINT('Ctrl Pts',(2.21660591299994,5.2,-3.90880343400001));
#355219=CARTESIAN_POINT('Ctrl Pts',(2.21660591299994,2.2,-3.90880343400001));
#355220=CARTESIAN_POINT('Ctrl Pts',(2.21651622099994,12.2,-3.90657563500001));
#355221=CARTESIAN_POINT('Ctrl Pts',(2.21651622099994,5.2,-3.90657563500001));
#355222=CARTESIAN_POINT('Ctrl Pts',(2.21651622099994,2.2,-3.90657563500001));
#355223=CARTESIAN_POINT('Ctrl Pts',(2.21642427099995,12.2,-3.90435174700002));
#355224=CARTESIAN_POINT('Ctrl Pts',(2.21642427099995,5.2,-3.90435174700002));
#355225=CARTESIAN_POINT('Ctrl Pts',(2.21642427099995,2.2,-3.90435174700002));
#355226=CARTESIAN_POINT('Ctrl Pts',(2.21633007199994,12.2,-3.90213177500002));
#355227=CARTESIAN_POINT('Ctrl Pts',(2.21633007199994,5.2,-3.90213177500002));
#355228=CARTESIAN_POINT('Ctrl Pts',(2.21633007199994,2.2,-3.90213177500002));
#355229=CARTESIAN_POINT('Ctrl Pts',(2.21623363099994,12.2,-3.89991572700001));
#355230=CARTESIAN_POINT('Ctrl Pts',(2.21623363099994,5.2,-3.89991572700001));
#355231=CARTESIAN_POINT('Ctrl Pts',(2.21623363099994,2.2,-3.89991572700001));
#355232=CARTESIAN_POINT('Ctrl Pts',(2.21613495599994,12.2,-3.89770360900001));
#355233=CARTESIAN_POINT('Ctrl Pts',(2.21613495599994,5.2,-3.89770360900001));
#355234=CARTESIAN_POINT('Ctrl Pts',(2.21613495599994,2.2,-3.89770360900001));
#355235=CARTESIAN_POINT('Ctrl Pts',(2.21603405499994,12.2,-3.89549542700002));
#355236=CARTESIAN_POINT('Ctrl Pts',(2.21603405499994,5.2,-3.89549542700002));
#355237=CARTESIAN_POINT('Ctrl Pts',(2.21603405499994,2.2,-3.89549542700002));
#355238=CARTESIAN_POINT('Ctrl Pts',(2.21593093499994,12.2,-3.89329118800001));
#355239=CARTESIAN_POINT('Ctrl Pts',(2.21593093499994,5.2,-3.89329118800001));
#355240=CARTESIAN_POINT('Ctrl Pts',(2.21593093499994,2.2,-3.89329118800001));
#355241=CARTESIAN_POINT('Ctrl Pts',(2.21582560499994,12.2,-3.89109089900002));
#355242=CARTESIAN_POINT('Ctrl Pts',(2.21582560499994,5.2,-3.89109089900002));
#355243=CARTESIAN_POINT('Ctrl Pts',(2.21582560499994,2.2,-3.89109089900002));
#355244=CARTESIAN_POINT('Ctrl Pts',(2.21571806999994,12.2,-3.88889456500001));
#355245=CARTESIAN_POINT('Ctrl Pts',(2.21571806999994,5.2,-3.88889456500001));
#355246=CARTESIAN_POINT('Ctrl Pts',(2.21571806999994,2.2,-3.88889456500001));
#355247=CARTESIAN_POINT('Ctrl Pts',(2.21560834099995,12.2,-3.88670219300002));
#355248=CARTESIAN_POINT('Ctrl Pts',(2.21560834099995,5.2,-3.88670219300002));
#355249=CARTESIAN_POINT('Ctrl Pts',(2.21560834099995,2.2,-3.88670219300002));
#355250=CARTESIAN_POINT('Ctrl Pts',(2.21549642299994,12.2,-3.88451379100001));
#355251=CARTESIAN_POINT('Ctrl Pts',(2.21549642299994,5.2,-3.88451379100001));
#355252=CARTESIAN_POINT('Ctrl Pts',(2.21549642299994,2.2,-3.88451379100001));
#355253=CARTESIAN_POINT('Ctrl Pts',(2.21538232599995,12.2,-3.88232936200001));
#355254=CARTESIAN_POINT('Ctrl Pts',(2.21538232599995,5.2,-3.88232936200001));
#355255=CARTESIAN_POINT('Ctrl Pts',(2.21538232599995,2.2,-3.88232936200001));
#355256=CARTESIAN_POINT('Ctrl Pts',(2.21526605699994,12.2,-3.88014891600001));
#355257=CARTESIAN_POINT('Ctrl Pts',(2.21526605699994,5.2,-3.88014891600001));
#355258=CARTESIAN_POINT('Ctrl Pts',(2.21526605699994,2.2,-3.88014891600001));
#355259=CARTESIAN_POINT('Ctrl Pts',(2.21514762299994,12.2,-3.87797245700002));
#355260=CARTESIAN_POINT('Ctrl Pts',(2.21514762299994,5.2,-3.87797245700002));
#355261=CARTESIAN_POINT('Ctrl Pts',(2.21514762299994,2.2,-3.87797245700002));
#355262=CARTESIAN_POINT('Ctrl Pts',(2.21502703299994,12.2,-3.87579999400002));
#355263=CARTESIAN_POINT('Ctrl Pts',(2.21502703299994,5.2,-3.87579999400002));
#355264=CARTESIAN_POINT('Ctrl Pts',(2.21502703299994,2.2,-3.87579999400002));
#355265=CARTESIAN_POINT('Ctrl Pts',(2.21490429399994,12.2,-3.87363153100001));
#355266=CARTESIAN_POINT('Ctrl Pts',(2.21490429399994,5.2,-3.87363153100001));
#355267=CARTESIAN_POINT('Ctrl Pts',(2.21490429399994,2.2,-3.87363153100001));
#355268=CARTESIAN_POINT('Ctrl Pts',(2.21477941399994,12.2,-3.87146707600001));
#355269=CARTESIAN_POINT('Ctrl Pts',(2.21477941399994,5.2,-3.87146707600001));
#355270=CARTESIAN_POINT('Ctrl Pts',(2.21477941399994,2.2,-3.87146707600001));
#355271=CARTESIAN_POINT('Ctrl Pts',(2.21465240199994,12.2,-3.86930663400001));
#355272=CARTESIAN_POINT('Ctrl Pts',(2.21465240199994,5.2,-3.86930663400001));
#355273=CARTESIAN_POINT('Ctrl Pts',(2.21465240199994,2.2,-3.86930663400001));
#355274=CARTESIAN_POINT('Ctrl Pts',(2.21452326299994,12.2,-3.86715021300001));
#355275=CARTESIAN_POINT('Ctrl Pts',(2.21452326299994,5.2,-3.86715021300001));
#355276=CARTESIAN_POINT('Ctrl Pts',(2.21452326299994,2.2,-3.86715021300001));
#355277=CARTESIAN_POINT('Ctrl Pts',(2.21439200899994,12.2,-3.86499781800001));
#355278=CARTESIAN_POINT('Ctrl Pts',(2.21439200899994,5.2,-3.86499781800001));
#355279=CARTESIAN_POINT('Ctrl Pts',(2.21439200899994,2.2,-3.86499781800001));
#355280=CARTESIAN_POINT('Ctrl Pts',(2.21425864499994,12.2,-3.86284945600002));
#355281=CARTESIAN_POINT('Ctrl Pts',(2.21425864499994,5.2,-3.86284945600002));
#355282=CARTESIAN_POINT('Ctrl Pts',(2.21425864499994,2.2,-3.86284945600002));
#355283=CARTESIAN_POINT('Ctrl Pts',(2.21412318099994,12.2,-3.86070513500002));
#355284=CARTESIAN_POINT('Ctrl Pts',(2.21412318099994,5.2,-3.86070513500002));
#355285=CARTESIAN_POINT('Ctrl Pts',(2.21412318099994,2.2,-3.86070513500002));
#355286=CARTESIAN_POINT('Ctrl Pts',(2.21398562199994,12.2,-3.85856485900002));
#355287=CARTESIAN_POINT('Ctrl Pts',(2.21398562199994,5.2,-3.85856485900002));
#355288=CARTESIAN_POINT('Ctrl Pts',(2.21398562199994,2.2,-3.85856485900002));
#355289=CARTESIAN_POINT('Ctrl Pts',(2.21384597999994,12.2,-3.85642863600001));
#355290=CARTESIAN_POINT('Ctrl Pts',(2.21384597999994,5.2,-3.85642863600001));
#355291=CARTESIAN_POINT('Ctrl Pts',(2.21384597999994,2.2,-3.85642863600001));
#355292=CARTESIAN_POINT('Ctrl Pts',(2.21370425999994,12.2,-3.85429647200001));
#355293=CARTESIAN_POINT('Ctrl Pts',(2.21370425999994,5.2,-3.85429647200001));
#355294=CARTESIAN_POINT('Ctrl Pts',(2.21370425999994,2.2,-3.85429647200001));
#355295=CARTESIAN_POINT('Ctrl Pts',(2.21356047199994,12.2,-3.85216837300002));
#355296=CARTESIAN_POINT('Ctrl Pts',(2.21356047199994,5.2,-3.85216837300002));
#355297=CARTESIAN_POINT('Ctrl Pts',(2.21356047199994,2.2,-3.85216837300002));
#355298=CARTESIAN_POINT('Ctrl Pts',(2.21341462199994,12.2,-3.85004434600001));
#355299=CARTESIAN_POINT('Ctrl Pts',(2.21341462199994,5.2,-3.85004434600001));
#355300=CARTESIAN_POINT('Ctrl Pts',(2.21341462199994,2.2,-3.85004434600001));
#355301=CARTESIAN_POINT('Ctrl Pts',(2.21326671999994,12.2,-3.84792439700002));
#355302=CARTESIAN_POINT('Ctrl Pts',(2.21326671999994,5.2,-3.84792439700002));
#355303=CARTESIAN_POINT('Ctrl Pts',(2.21326671999994,2.2,-3.84792439700002));
#355304=CARTESIAN_POINT('Ctrl Pts',(2.21311677299994,12.2,-3.84580853300001));
#355305=CARTESIAN_POINT('Ctrl Pts',(2.21311677299994,5.2,-3.84580853300001));
#355306=CARTESIAN_POINT('Ctrl Pts',(2.21311677299994,2.2,-3.84580853300001));
#355307=CARTESIAN_POINT('Ctrl Pts',(2.21296478899994,12.2,-3.84369676000002));
#355308=CARTESIAN_POINT('Ctrl Pts',(2.21296478899994,5.2,-3.84369676000002));
#355309=CARTESIAN_POINT('Ctrl Pts',(2.21296478899994,2.2,-3.84369676000002));
#355310=CARTESIAN_POINT('Ctrl Pts',(2.21281077799994,12.2,-3.84158908500002));
#355311=CARTESIAN_POINT('Ctrl Pts',(2.21281077799994,5.2,-3.84158908500002));
#355312=CARTESIAN_POINT('Ctrl Pts',(2.21281077799994,2.2,-3.84158908500002));
#355313=CARTESIAN_POINT('Ctrl Pts',(2.21265474699994,12.2,-3.83948551400001));
#355314=CARTESIAN_POINT('Ctrl Pts',(2.21265474699994,5.2,-3.83948551400001));
#355315=CARTESIAN_POINT('Ctrl Pts',(2.21265474699994,2.2,-3.83948551400001));
#355316=CARTESIAN_POINT('Ctrl Pts',(2.21249670299994,12.2,-3.83738605300001));
#355317=CARTESIAN_POINT('Ctrl Pts',(2.21249670299994,5.2,-3.83738605300001));
#355318=CARTESIAN_POINT('Ctrl Pts',(2.21249670299994,2.2,-3.83738605300001));
#355319=CARTESIAN_POINT('Ctrl Pts',(2.21233665499994,12.2,-3.83529070900002));
#355320=CARTESIAN_POINT('Ctrl Pts',(2.21233665499994,5.2,-3.83529070900002));
#355321=CARTESIAN_POINT('Ctrl Pts',(2.21233665499994,2.2,-3.83529070900002));
#355322=CARTESIAN_POINT('Ctrl Pts',(2.21217461299994,12.2,-3.83319948700001));
#355323=CARTESIAN_POINT('Ctrl Pts',(2.21217461299994,5.2,-3.83319948700001));
#355324=CARTESIAN_POINT('Ctrl Pts',(2.21217461299994,2.2,-3.83319948700001));
#355325=CARTESIAN_POINT('Ctrl Pts',(2.21201058399994,12.2,-3.83111239700002));
#355326=CARTESIAN_POINT('Ctrl Pts',(2.21201058399994,5.2,-3.83111239700002));
#355327=CARTESIAN_POINT('Ctrl Pts',(2.21201058399994,2.2,-3.83111239700002));
#355328=CARTESIAN_POINT('Ctrl Pts',(2.21184457499994,12.2,-3.82902944200001));
#355329=CARTESIAN_POINT('Ctrl Pts',(2.21184457499994,5.2,-3.82902944200001));
#355330=CARTESIAN_POINT('Ctrl Pts',(2.21184457499994,2.2,-3.82902944200001));
#355331=CARTESIAN_POINT('Ctrl Pts',(2.21167659699994,12.2,-3.82695062900002));
#355332=CARTESIAN_POINT('Ctrl Pts',(2.21167659699994,5.2,-3.82695062900002));
#355333=CARTESIAN_POINT('Ctrl Pts',(2.21167659699994,2.2,-3.82695062900002));
#355334=CARTESIAN_POINT('Ctrl Pts',(2.21150665499994,12.2,-3.82487596600001));
#355335=CARTESIAN_POINT('Ctrl Pts',(2.21150665499994,5.2,-3.82487596600001));
#355336=CARTESIAN_POINT('Ctrl Pts',(2.21150665499994,2.2,-3.82487596600001));
#355337=CARTESIAN_POINT('Ctrl Pts',(2.21133475999994,12.2,-3.82280545700001));
#355338=CARTESIAN_POINT('Ctrl Pts',(2.21133475999994,5.2,-3.82280545700001));
#355339=CARTESIAN_POINT('Ctrl Pts',(2.21133475999994,2.2,-3.82280545700001));
#355340=CARTESIAN_POINT('Ctrl Pts',(2.21116091999995,12.2,-3.82073911100001));
#355341=CARTESIAN_POINT('Ctrl Pts',(2.21116091999995,5.2,-3.82073911100001));
#355342=CARTESIAN_POINT('Ctrl Pts',(2.21116091999995,2.2,-3.82073911100001));
#355343=CARTESIAN_POINT('Ctrl Pts',(2.21098514299995,12.2,-3.81867693300002));
#355344=CARTESIAN_POINT('Ctrl Pts',(2.21098514299995,5.2,-3.81867693300002));
#355345=CARTESIAN_POINT('Ctrl Pts',(2.21098514299995,2.2,-3.81867693300002));
#355346=CARTESIAN_POINT('Ctrl Pts',(2.21080743799994,12.2,-3.81661893000001));
#355347=CARTESIAN_POINT('Ctrl Pts',(2.21080743799994,5.2,-3.81661893000001));
#355348=CARTESIAN_POINT('Ctrl Pts',(2.21080743799994,2.2,-3.81661893000001));
#355349=CARTESIAN_POINT('Ctrl Pts',(2.21062781199994,12.2,-3.81456510700001));
#355350=CARTESIAN_POINT('Ctrl Pts',(2.21062781199994,5.2,-3.81456510700001));
#355351=CARTESIAN_POINT('Ctrl Pts',(2.21062781199994,2.2,-3.81456510700001));
#355352=CARTESIAN_POINT('Ctrl Pts',(2.21044627499994,12.2,-3.81251547200002));
#355353=CARTESIAN_POINT('Ctrl Pts',(2.21044627499994,5.2,-3.81251547200002));
#355354=CARTESIAN_POINT('Ctrl Pts',(2.21044627499994,2.2,-3.81251547200002));
#355355=CARTESIAN_POINT('Ctrl Pts',(2.21026283499994,12.2,-3.81047003000001));
#355356=CARTESIAN_POINT('Ctrl Pts',(2.21026283499994,5.2,-3.81047003000001));
#355357=CARTESIAN_POINT('Ctrl Pts',(2.21026283499994,2.2,-3.81047003000001));
#355358=CARTESIAN_POINT('Ctrl Pts',(2.21007749899994,12.2,-3.80842879000001));
#355359=CARTESIAN_POINT('Ctrl Pts',(2.21007749899994,5.2,-3.80842879000001));
#355360=CARTESIAN_POINT('Ctrl Pts',(2.21007749899994,2.2,-3.80842879000001));
#355361=CARTESIAN_POINT('Ctrl Pts',(2.20989027799994,12.2,-3.80639175500002));
#355362=CARTESIAN_POINT('Ctrl Pts',(2.20989027799994,5.2,-3.80639175500002));
#355363=CARTESIAN_POINT('Ctrl Pts',(2.20989027799994,2.2,-3.80639175500002));
#355364=CARTESIAN_POINT('Ctrl Pts',(2.20970117999994,12.2,-3.80435893400001));
#355365=CARTESIAN_POINT('Ctrl Pts',(2.20970117999994,5.2,-3.80435893400001));
#355366=CARTESIAN_POINT('Ctrl Pts',(2.20970117999994,2.2,-3.80435893400001));
#355367=CARTESIAN_POINT('Ctrl Pts',(2.20951021199994,12.2,-3.80233033200001));
#355368=CARTESIAN_POINT('Ctrl Pts',(2.20951021199994,5.2,-3.80233033200001));
#355369=CARTESIAN_POINT('Ctrl Pts',(2.20951021199994,2.2,-3.80233033200001));
#355370=CARTESIAN_POINT('Ctrl Pts',(2.20931738399994,12.2,-3.80030595700001));
#355371=CARTESIAN_POINT('Ctrl Pts',(2.20931738399994,5.2,-3.80030595700001));
#355372=CARTESIAN_POINT('Ctrl Pts',(2.20931738399994,2.2,-3.80030595700001));
#355373=CARTESIAN_POINT('Ctrl Pts',(2.20912270499994,12.2,-3.79828581200002));
#355374=CARTESIAN_POINT('Ctrl Pts',(2.20912270499994,5.2,-3.79828581200002));
#355375=CARTESIAN_POINT('Ctrl Pts',(2.20912270499994,2.2,-3.79828581200002));
#355376=CARTESIAN_POINT('Ctrl Pts',(2.20892618299994,12.2,-3.79626990800002));
#355377=CARTESIAN_POINT('Ctrl Pts',(2.20892618299994,5.2,-3.79626990800002));
#355378=CARTESIAN_POINT('Ctrl Pts',(2.20892618299994,2.2,-3.79626990800002));
#355379=CARTESIAN_POINT('Ctrl Pts',(2.20872782499994,12.2,-3.79425824700002));
#355380=CARTESIAN_POINT('Ctrl Pts',(2.20872782499994,5.2,-3.79425824700002));
#355381=CARTESIAN_POINT('Ctrl Pts',(2.20872782499994,2.2,-3.79425824700002));
#355382=CARTESIAN_POINT('Ctrl Pts',(2.20852764299994,12.2,-3.79225083900002));
#355383=CARTESIAN_POINT('Ctrl Pts',(2.20852764299994,5.2,-3.79225083900002));
#355384=CARTESIAN_POINT('Ctrl Pts',(2.20852764299994,2.2,-3.79225083900002));
#355385=CARTESIAN_POINT('Ctrl Pts',(2.20832564299994,12.2,-3.79024768800001));
#355386=CARTESIAN_POINT('Ctrl Pts',(2.20832564299994,5.2,-3.79024768800001));
#355387=CARTESIAN_POINT('Ctrl Pts',(2.20832564299994,2.2,-3.79024768800001));
#355388=CARTESIAN_POINT('Ctrl Pts',(2.20812183599994,12.2,-3.78824880200002));
#355389=CARTESIAN_POINT('Ctrl Pts',(2.20812183599994,5.2,-3.78824880200002));
#355390=CARTESIAN_POINT('Ctrl Pts',(2.20812183599994,2.2,-3.78824880200002));
#355391=CARTESIAN_POINT('Ctrl Pts',(2.20791622799994,12.2,-3.78625418600001));
#355392=CARTESIAN_POINT('Ctrl Pts',(2.20791622799994,5.2,-3.78625418600001));
#355393=CARTESIAN_POINT('Ctrl Pts',(2.20791622799994,2.2,-3.78625418600001));
#355394=CARTESIAN_POINT('Ctrl Pts',(2.20770883099994,12.2,-3.78426384700001));
#355395=CARTESIAN_POINT('Ctrl Pts',(2.20770883099994,5.2,-3.78426384700001));
#355396=CARTESIAN_POINT('Ctrl Pts',(2.20770883099994,2.2,-3.78426384700001));
#355397=CARTESIAN_POINT('Ctrl Pts',(2.20749965099994,12.2,-3.78227779100001));
#355398=CARTESIAN_POINT('Ctrl Pts',(2.20749965099994,5.2,-3.78227779100001));
#355399=CARTESIAN_POINT('Ctrl Pts',(2.20749965099994,2.2,-3.78227779100001));
#355400=CARTESIAN_POINT('Ctrl Pts',(2.20728869799994,12.2,-3.78029602500002));
#355401=CARTESIAN_POINT('Ctrl Pts',(2.20728869799994,5.2,-3.78029602500002));
#355402=CARTESIAN_POINT('Ctrl Pts',(2.20728869799994,2.2,-3.78029602500002));
#355403=CARTESIAN_POINT('Ctrl Pts',(2.20707598099994,12.2,-3.77831855500002));
#355404=CARTESIAN_POINT('Ctrl Pts',(2.20707598099994,5.2,-3.77831855500002));
#355405=CARTESIAN_POINT('Ctrl Pts',(2.20707598099994,2.2,-3.77831855500002));
#355406=CARTESIAN_POINT('Ctrl Pts',(2.20686150899994,12.2,-3.77634538800002));
#355407=CARTESIAN_POINT('Ctrl Pts',(2.20686150899994,5.2,-3.77634538800002));
#355408=CARTESIAN_POINT('Ctrl Pts',(2.20686150899994,2.2,-3.77634538800002));
#355409=CARTESIAN_POINT('Ctrl Pts',(2.20664529099994,12.2,-3.77437653000001));
#355410=CARTESIAN_POINT('Ctrl Pts',(2.20664529099994,5.2,-3.77437653000001));
#355411=CARTESIAN_POINT('Ctrl Pts',(2.20664529099994,2.2,-3.77437653000001));
#355412=CARTESIAN_POINT('Ctrl Pts',(2.20642733399994,12.2,-3.77241198700002));
#355413=CARTESIAN_POINT('Ctrl Pts',(2.20642733399994,5.2,-3.77241198700002));
#355414=CARTESIAN_POINT('Ctrl Pts',(2.20642733399994,2.2,-3.77241198700002));
#355415=CARTESIAN_POINT('Ctrl Pts',(2.20620764899994,12.2,-3.77045176500001));
#355416=CARTESIAN_POINT('Ctrl Pts',(2.20620764899994,5.2,-3.77045176500001));
#355417=CARTESIAN_POINT('Ctrl Pts',(2.20620764899994,2.2,-3.77045176500001));
#355418=CARTESIAN_POINT('Ctrl Pts',(2.20598624599994,12.2,-3.76849587100001));
#355419=CARTESIAN_POINT('Ctrl Pts',(2.20598624599994,5.2,-3.76849587100001));
#355420=CARTESIAN_POINT('Ctrl Pts',(2.20598624599994,2.2,-3.76849587100001));
#355421=CARTESIAN_POINT('Ctrl Pts',(2.20576313099994,12.2,-3.76654431200001));
#355422=CARTESIAN_POINT('Ctrl Pts',(2.20576313099994,5.2,-3.76654431200001));
#355423=CARTESIAN_POINT('Ctrl Pts',(2.20576313099994,2.2,-3.76654431200001));
#355424=CARTESIAN_POINT('Ctrl Pts',(2.20553831499994,12.2,-3.76459709300001));
#355425=CARTESIAN_POINT('Ctrl Pts',(2.20553831499994,5.2,-3.76459709300001));
#355426=CARTESIAN_POINT('Ctrl Pts',(2.20553831499994,2.2,-3.76459709300001));
#355427=CARTESIAN_POINT('Ctrl Pts',(2.20531180499994,12.2,-3.76265422200001));
#355428=CARTESIAN_POINT('Ctrl Pts',(2.20531180499994,5.2,-3.76265422200001));
#355429=CARTESIAN_POINT('Ctrl Pts',(2.20531180499994,2.2,-3.76265422200001));
#355430=CARTESIAN_POINT('Ctrl Pts',(2.20508361399994,12.2,-3.76071570400001));
#355431=CARTESIAN_POINT('Ctrl Pts',(2.20508361399994,5.2,-3.76071570400001));
#355432=CARTESIAN_POINT('Ctrl Pts',(2.20508361399994,2.2,-3.76071570400001));
#355433=CARTESIAN_POINT('Ctrl Pts',(2.20485374699994,12.2,-3.75878154600001));
#355434=CARTESIAN_POINT('Ctrl Pts',(2.20485374699994,5.2,-3.75878154600001));
#355435=CARTESIAN_POINT('Ctrl Pts',(2.20485374699994,2.2,-3.75878154600001));
#355436=CARTESIAN_POINT('Ctrl Pts',(2.20462221499994,12.2,-3.75685175400001));
#355437=CARTESIAN_POINT('Ctrl Pts',(2.20462221499994,5.2,-3.75685175400001));
#355438=CARTESIAN_POINT('Ctrl Pts',(2.20462221499994,2.2,-3.75685175400001));
#355439=CARTESIAN_POINT('Ctrl Pts',(2.20438902699994,12.2,-3.75492633400001));
#355440=CARTESIAN_POINT('Ctrl Pts',(2.20438902699994,5.2,-3.75492633400001));
#355441=CARTESIAN_POINT('Ctrl Pts',(2.20438902699994,2.2,-3.75492633400001));
#355442=CARTESIAN_POINT('Ctrl Pts',(2.20415419199994,12.2,-3.75300529300001));
#355443=CARTESIAN_POINT('Ctrl Pts',(2.20415419199994,5.2,-3.75300529300001));
#355444=CARTESIAN_POINT('Ctrl Pts',(2.20415419199994,2.2,-3.75300529300001));
#355445=CARTESIAN_POINT('Ctrl Pts',(2.20391771899994,12.2,-3.75108863800001));
#355446=CARTESIAN_POINT('Ctrl Pts',(2.20391771899994,5.2,-3.75108863800001));
#355447=CARTESIAN_POINT('Ctrl Pts',(2.20391771899994,2.2,-3.75108863800001));
#355448=CARTESIAN_POINT('Ctrl Pts',(2.20367961799994,12.2,-3.74917637400001));
#355449=CARTESIAN_POINT('Ctrl Pts',(2.20367961799994,5.2,-3.74917637400001));
#355450=CARTESIAN_POINT('Ctrl Pts',(2.20367961799994,2.2,-3.74917637400001));
#355451=CARTESIAN_POINT('Ctrl Pts',(2.20343989799994,12.2,-3.74726850800001));
#355452=CARTESIAN_POINT('Ctrl Pts',(2.20343989799994,5.2,-3.74726850800001));
#355453=CARTESIAN_POINT('Ctrl Pts',(2.20343989799994,2.2,-3.74726850800001));
#355454=CARTESIAN_POINT('Ctrl Pts',(2.20319856699994,12.2,-3.74536504600002));
#355455=CARTESIAN_POINT('Ctrl Pts',(2.20319856699994,5.2,-3.74536504600002));
#355456=CARTESIAN_POINT('Ctrl Pts',(2.20319856699994,2.2,-3.74536504600002));
#355457=CARTESIAN_POINT('Ctrl Pts',(2.20295563499994,12.2,-3.74346599500001));
#355458=CARTESIAN_POINT('Ctrl Pts',(2.20295563499994,5.2,-3.74346599500001));
#355459=CARTESIAN_POINT('Ctrl Pts',(2.20295563499994,2.2,-3.74346599500001));
#355460=CARTESIAN_POINT('Ctrl Pts',(2.20271111199994,12.2,-3.74157136100001));
#355461=CARTESIAN_POINT('Ctrl Pts',(2.20271111199994,5.2,-3.74157136100001));
#355462=CARTESIAN_POINT('Ctrl Pts',(2.20271111199994,2.2,-3.74157136100001));
#355463=CARTESIAN_POINT('Ctrl Pts',(2.20246500699994,12.2,-3.73968114900002));
#355464=CARTESIAN_POINT('Ctrl Pts',(2.20246500699994,5.2,-3.73968114900002));
#355465=CARTESIAN_POINT('Ctrl Pts',(2.20246500699994,2.2,-3.73968114900002));
#355466=CARTESIAN_POINT('Ctrl Pts',(2.20221732899994,12.2,-3.73779536900001));
#355467=CARTESIAN_POINT('Ctrl Pts',(2.20221732899994,5.2,-3.73779536900001));
#355468=CARTESIAN_POINT('Ctrl Pts',(2.20221732899994,2.2,-3.73779536900001));
#355469=CARTESIAN_POINT('Ctrl Pts',(2.20196808699994,12.2,-3.73591402400002));
#355470=CARTESIAN_POINT('Ctrl Pts',(2.20196808699994,5.2,-3.73591402400002));
#355471=CARTESIAN_POINT('Ctrl Pts',(2.20196808699994,2.2,-3.73591402400002));
#355472=CARTESIAN_POINT('Ctrl Pts',(2.20171729099994,12.2,-3.73403712000002));
#355473=CARTESIAN_POINT('Ctrl Pts',(2.20171729099994,5.2,-3.73403712000002));
#355474=CARTESIAN_POINT('Ctrl Pts',(2.20171729099994,2.2,-3.73403712000002));
#355475=CARTESIAN_POINT('Ctrl Pts',(2.20146495099994,12.2,-3.73216466500002));
#355476=CARTESIAN_POINT('Ctrl Pts',(2.20146495099994,5.2,-3.73216466500002));
#355477=CARTESIAN_POINT('Ctrl Pts',(2.20146495099994,2.2,-3.73216466500002));
#355478=CARTESIAN_POINT('Ctrl Pts',(2.20121107499994,12.2,-3.73029666600001));
#355479=CARTESIAN_POINT('Ctrl Pts',(2.20121107499994,5.2,-3.73029666600001));
#355480=CARTESIAN_POINT('Ctrl Pts',(2.20121107499994,2.2,-3.73029666600001));
#355481=CARTESIAN_POINT('Ctrl Pts',(2.20095567399994,12.2,-3.72843312700001));
#355482=CARTESIAN_POINT('Ctrl Pts',(2.20095567399994,5.2,-3.72843312700001));
#355483=CARTESIAN_POINT('Ctrl Pts',(2.20095567399994,2.2,-3.72843312700001));
#355484=CARTESIAN_POINT('Ctrl Pts',(2.20069875599994,12.2,-3.72657405600001));
#355485=CARTESIAN_POINT('Ctrl Pts',(2.20069875599994,5.2,-3.72657405600001));
#355486=CARTESIAN_POINT('Ctrl Pts',(2.20069875599994,2.2,-3.72657405600001));
#355487=CARTESIAN_POINT('Ctrl Pts',(2.20044033199994,12.2,-3.72471946000001));
#355488=CARTESIAN_POINT('Ctrl Pts',(2.20044033199994,5.2,-3.72471946000001));
#355489=CARTESIAN_POINT('Ctrl Pts',(2.20044033199994,2.2,-3.72471946000001));
#355490=CARTESIAN_POINT('Ctrl Pts',(2.20018040999994,12.2,-3.72286934200002));
#355491=CARTESIAN_POINT('Ctrl Pts',(2.20018040999994,5.2,-3.72286934200002));
#355492=CARTESIAN_POINT('Ctrl Pts',(2.20018040999994,2.2,-3.72286934200002));
#355493=CARTESIAN_POINT('Ctrl Pts',(2.19991900199994,12.2,-3.72102371200001));
#355494=CARTESIAN_POINT('Ctrl Pts',(2.19991900199994,5.2,-3.72102371200001));
#355495=CARTESIAN_POINT('Ctrl Pts',(2.19991900199994,2.2,-3.72102371200001));
#355496=CARTESIAN_POINT('Ctrl Pts',(2.19965611499994,12.2,-3.71918257500001));
#355497=CARTESIAN_POINT('Ctrl Pts',(2.19965611499994,5.2,-3.71918257500001));
#355498=CARTESIAN_POINT('Ctrl Pts',(2.19965611499994,2.2,-3.71918257500001));
#355499=CARTESIAN_POINT('Ctrl Pts',(2.19939175899994,12.2,-3.71734593700001));
#355500=CARTESIAN_POINT('Ctrl Pts',(2.19939175899994,5.2,-3.71734593700001));
#355501=CARTESIAN_POINT('Ctrl Pts',(2.19939175899994,2.2,-3.71734593700001));
#355502=CARTESIAN_POINT('Ctrl Pts',(2.19912594399994,12.2,-3.71551380500001));
#355503=CARTESIAN_POINT('Ctrl Pts',(2.19912594399994,5.2,-3.71551380500001));
#355504=CARTESIAN_POINT('Ctrl Pts',(2.19912594399994,2.2,-3.71551380500001));
#355505=CARTESIAN_POINT('Ctrl Pts',(2.19885868099994,12.2,-3.71368618300002));
#355506=CARTESIAN_POINT('Ctrl Pts',(2.19885868099994,5.2,-3.71368618300002));
#355507=CARTESIAN_POINT('Ctrl Pts',(2.19885868099994,2.2,-3.71368618300002));
#355508=CARTESIAN_POINT('Ctrl Pts',(2.19858997799994,12.2,-3.71186308000001));
#355509=CARTESIAN_POINT('Ctrl Pts',(2.19858997799994,5.2,-3.71186308000001));
#355510=CARTESIAN_POINT('Ctrl Pts',(2.19858997799994,2.2,-3.71186308000001));
#355511=CARTESIAN_POINT('Ctrl Pts',(2.19831984599994,12.2,-3.71004450200001));
#355512=CARTESIAN_POINT('Ctrl Pts',(2.19831984599994,5.2,-3.71004450200001));
#355513=CARTESIAN_POINT('Ctrl Pts',(2.19831984599994,2.2,-3.71004450200001));
#355514=CARTESIAN_POINT('Ctrl Pts',(2.19804829299994,12.2,-3.70823045400002));
#355515=CARTESIAN_POINT('Ctrl Pts',(2.19804829299994,5.2,-3.70823045400002));
#355516=CARTESIAN_POINT('Ctrl Pts',(2.19804829299994,2.2,-3.70823045400002));
#355517=CARTESIAN_POINT('Ctrl Pts',(2.19777532999994,12.2,-3.70642094300001));
#355518=CARTESIAN_POINT('Ctrl Pts',(2.19777532999994,5.2,-3.70642094300001));
#355519=CARTESIAN_POINT('Ctrl Pts',(2.19777532999994,2.2,-3.70642094300001));
#355520=CARTESIAN_POINT('Ctrl Pts',(2.19750096799994,12.2,-3.70461597600002));
#355521=CARTESIAN_POINT('Ctrl Pts',(2.19750096799994,5.2,-3.70461597600002));
#355522=CARTESIAN_POINT('Ctrl Pts',(2.19750096799994,2.2,-3.70461597600002));
#355523=CARTESIAN_POINT('Ctrl Pts',(2.19722521399994,12.2,-3.70281555800001));
#355524=CARTESIAN_POINT('Ctrl Pts',(2.19722521399994,5.2,-3.70281555800001));
#355525=CARTESIAN_POINT('Ctrl Pts',(2.19722521399994,2.2,-3.70281555800001));
#355526=CARTESIAN_POINT('Ctrl Pts',(2.19694808099994,12.2,-3.70101969500002));
#355527=CARTESIAN_POINT('Ctrl Pts',(2.19694808099994,5.2,-3.70101969500002));
#355528=CARTESIAN_POINT('Ctrl Pts',(2.19694808099994,2.2,-3.70101969500002));
#355529=CARTESIAN_POINT('Ctrl Pts',(2.19666957499994,12.2,-3.69922839500001));
#355530=CARTESIAN_POINT('Ctrl Pts',(2.19666957499994,5.2,-3.69922839500001));
#355531=CARTESIAN_POINT('Ctrl Pts',(2.19666957499994,2.2,-3.69922839500001));
#355532=CARTESIAN_POINT('Ctrl Pts',(2.19638970899994,12.2,-3.69744166300002));
#355533=CARTESIAN_POINT('Ctrl Pts',(2.19638970899994,5.2,-3.69744166300002));
#355534=CARTESIAN_POINT('Ctrl Pts',(2.19638970899994,2.2,-3.69744166300002));
#355535=CARTESIAN_POINT('Ctrl Pts',(2.19610849199994,12.2,-3.69565950700002));
#355536=CARTESIAN_POINT('Ctrl Pts',(2.19610849199994,5.2,-3.69565950700002));
#355537=CARTESIAN_POINT('Ctrl Pts',(2.19610849199994,2.2,-3.69565950700002));
#355538=CARTESIAN_POINT('Ctrl Pts',(2.19582593399994,12.2,-3.69388193000002));
#355539=CARTESIAN_POINT('Ctrl Pts',(2.19582593399994,5.2,-3.69388193000002));
#355540=CARTESIAN_POINT('Ctrl Pts',(2.19582593399994,2.2,-3.69388193000002));
#355541=CARTESIAN_POINT('Ctrl Pts',(2.19554204499994,12.2,-3.69210894200001));
#355542=CARTESIAN_POINT('Ctrl Pts',(2.19554204499994,5.2,-3.69210894200001));
#355543=CARTESIAN_POINT('Ctrl Pts',(2.19554204499994,2.2,-3.69210894200001));
#355544=CARTESIAN_POINT('Ctrl Pts',(2.19525683499994,12.2,-3.69034054600001));
#355545=CARTESIAN_POINT('Ctrl Pts',(2.19525683499994,5.2,-3.69034054600001));
#355546=CARTESIAN_POINT('Ctrl Pts',(2.19525683499994,2.2,-3.69034054600001));
#355547=CARTESIAN_POINT('Ctrl Pts',(2.19497031399994,12.2,-3.68857675100001));
#355548=CARTESIAN_POINT('Ctrl Pts',(2.19497031399994,5.2,-3.68857675100001));
#355549=CARTESIAN_POINT('Ctrl Pts',(2.19497031399994,2.2,-3.68857675100001));
#355550=CARTESIAN_POINT('Ctrl Pts',(2.19468249099994,12.2,-3.68681756100001));
#355551=CARTESIAN_POINT('Ctrl Pts',(2.19468249099994,5.2,-3.68681756100001));
#355552=CARTESIAN_POINT('Ctrl Pts',(2.19468249099994,2.2,-3.68681756100001));
#355553=CARTESIAN_POINT('Ctrl Pts',(2.19439337899995,12.2,-3.68506298400002));
#355554=CARTESIAN_POINT('Ctrl Pts',(2.19439337899995,5.2,-3.68506298400002));
#355555=CARTESIAN_POINT('Ctrl Pts',(2.19439337899995,2.2,-3.68506298400002));
#355556=CARTESIAN_POINT('Ctrl Pts',(2.19410298499994,12.2,-3.68331302600001));
#355557=CARTESIAN_POINT('Ctrl Pts',(2.19410298499994,5.2,-3.68331302600001));
#355558=CARTESIAN_POINT('Ctrl Pts',(2.19410298499994,2.2,-3.68331302600001));
#355559=CARTESIAN_POINT('Ctrl Pts',(2.19381131999994,12.2,-3.68156769100001));
#355560=CARTESIAN_POINT('Ctrl Pts',(2.19381131999994,5.2,-3.68156769100001));
#355561=CARTESIAN_POINT('Ctrl Pts',(2.19381131999994,2.2,-3.68156769100001));
#355562=CARTESIAN_POINT('Ctrl Pts',(2.19351839399994,12.2,-3.67982699000001));
#355563=CARTESIAN_POINT('Ctrl Pts',(2.19351839399994,5.2,-3.67982699000001));
#355564=CARTESIAN_POINT('Ctrl Pts',(2.19351839399994,2.2,-3.67982699000001));
#355565=CARTESIAN_POINT('Ctrl Pts',(2.19322421899994,12.2,-3.67809092400002));
#355566=CARTESIAN_POINT('Ctrl Pts',(2.19322421899994,5.2,-3.67809092400002));
#355567=CARTESIAN_POINT('Ctrl Pts',(2.19322421899994,2.2,-3.67809092400002));
#355568=CARTESIAN_POINT('Ctrl Pts',(2.19292880299994,12.2,-3.67635950300001));
#355569=CARTESIAN_POINT('Ctrl Pts',(2.19292880299994,5.2,-3.67635950300001));
#355570=CARTESIAN_POINT('Ctrl Pts',(2.19292880299994,2.2,-3.67635950300001));
#355571=CARTESIAN_POINT('Ctrl Pts',(2.19263215699994,12.2,-3.67463273100002));
#355572=CARTESIAN_POINT('Ctrl Pts',(2.19263215699994,5.2,-3.67463273100002));
#355573=CARTESIAN_POINT('Ctrl Pts',(2.19263215699994,2.2,-3.67463273100002));
#355574=CARTESIAN_POINT('Ctrl Pts',(2.19233429299994,12.2,-3.67291061600001));
#355575=CARTESIAN_POINT('Ctrl Pts',(2.19233429299994,5.2,-3.67291061600001));
#355576=CARTESIAN_POINT('Ctrl Pts',(2.19233429299994,2.2,-3.67291061600001));
#355577=CARTESIAN_POINT('Ctrl Pts',(2.19203521899995,12.2,-3.67119316200001));
#355578=CARTESIAN_POINT('Ctrl Pts',(2.19203521899995,5.2,-3.67119316200001));
#355579=CARTESIAN_POINT('Ctrl Pts',(2.19203521899995,2.2,-3.67119316200001));
#355580=CARTESIAN_POINT('Ctrl Pts',(2.19173494499994,12.2,-3.66948037700002));
#355581=CARTESIAN_POINT('Ctrl Pts',(2.19173494499994,5.2,-3.66948037700002));
#355582=CARTESIAN_POINT('Ctrl Pts',(2.19173494499994,2.2,-3.66948037700002));
#355583=CARTESIAN_POINT('Ctrl Pts',(2.19143348299994,12.2,-3.66777226800002));
#355584=CARTESIAN_POINT('Ctrl Pts',(2.19143348299994,5.2,-3.66777226800002));
#355585=CARTESIAN_POINT('Ctrl Pts',(2.19143348299994,2.2,-3.66777226800002));
#355586=CARTESIAN_POINT('Ctrl Pts',(2.19113084199994,12.2,-3.66606883900001));
#355587=CARTESIAN_POINT('Ctrl Pts',(2.19113084199994,5.2,-3.66606883900001));
#355588=CARTESIAN_POINT('Ctrl Pts',(2.19113084199994,2.2,-3.66606883900001));
#355589=CARTESIAN_POINT('Ctrl Pts',(2.19082703499994,12.2,-3.66437009700002));
#355590=CARTESIAN_POINT('Ctrl Pts',(2.19082703499994,5.2,-3.66437009700002));
#355591=CARTESIAN_POINT('Ctrl Pts',(2.19082703499994,2.2,-3.66437009700002));
#355592=CARTESIAN_POINT('Ctrl Pts',(2.19052206899994,12.2,-3.66267605000001));
#355593=CARTESIAN_POINT('Ctrl Pts',(2.19052206899994,5.2,-3.66267605000001));
#355594=CARTESIAN_POINT('Ctrl Pts',(2.19052206899994,2.2,-3.66267605000001));
#355595=CARTESIAN_POINT('Ctrl Pts',(2.19021595699994,12.2,-3.66098670100001));
#355596=CARTESIAN_POINT('Ctrl Pts',(2.19021595699994,5.2,-3.66098670100001));
#355597=CARTESIAN_POINT('Ctrl Pts',(2.19021595699994,2.2,-3.66098670100001));
#355598=CARTESIAN_POINT('Ctrl Pts',(2.18990870699994,12.2,-3.65930206000002));
#355599=CARTESIAN_POINT('Ctrl Pts',(2.18990870699994,5.2,-3.65930206000002));
#355600=CARTESIAN_POINT('Ctrl Pts',(2.18990870699994,2.2,-3.65930206000002));
#355601=CARTESIAN_POINT('Ctrl Pts',(2.18960033199994,12.2,-3.65762213000002));
#355602=CARTESIAN_POINT('Ctrl Pts',(2.18960033199994,5.2,-3.65762213000002));
#355603=CARTESIAN_POINT('Ctrl Pts',(2.18960033199994,2.2,-3.65762213000002));
#355604=CARTESIAN_POINT('Ctrl Pts',(2.18929084099994,12.2,-3.65594691900001));
#355605=CARTESIAN_POINT('Ctrl Pts',(2.18929084099994,5.2,-3.65594691900001));
#355606=CARTESIAN_POINT('Ctrl Pts',(2.18929084099994,2.2,-3.65594691900001));
#355607=CARTESIAN_POINT('Ctrl Pts',(2.18898024599994,12.2,-3.65427643200002));
#355608=CARTESIAN_POINT('Ctrl Pts',(2.18898024599994,5.2,-3.65427643200002));
#355609=CARTESIAN_POINT('Ctrl Pts',(2.18898024599994,2.2,-3.65427643200002));
#355610=CARTESIAN_POINT('Ctrl Pts',(2.18866855699994,12.2,-3.65261067600001));
#355611=CARTESIAN_POINT('Ctrl Pts',(2.18866855699994,5.2,-3.65261067600001));
#355612=CARTESIAN_POINT('Ctrl Pts',(2.18866855699994,2.2,-3.65261067600001));
#355613=CARTESIAN_POINT('Ctrl Pts',(2.18835578299994,12.2,-3.65094965700001));
#355614=CARTESIAN_POINT('Ctrl Pts',(2.18835578299994,5.2,-3.65094965700001));
#355615=CARTESIAN_POINT('Ctrl Pts',(2.18835578299994,2.2,-3.65094965700001));
#355616=CARTESIAN_POINT('Ctrl Pts',(2.18804193699994,12.2,-3.64929338100001));
#355617=CARTESIAN_POINT('Ctrl Pts',(2.18804193699994,5.2,-3.64929338100001));
#355618=CARTESIAN_POINT('Ctrl Pts',(2.18804193699994,2.2,-3.64929338100001));
#355619=CARTESIAN_POINT('Ctrl Pts',(2.18772702799995,12.2,-3.64764185600002));
#355620=CARTESIAN_POINT('Ctrl Pts',(2.18772702799995,5.2,-3.64764185600002));
#355621=CARTESIAN_POINT('Ctrl Pts',(2.18772702799995,2.2,-3.64764185600002));
#355622=CARTESIAN_POINT('Ctrl Pts',(2.18741106799994,12.2,-3.64599508600001));
#355623=CARTESIAN_POINT('Ctrl Pts',(2.18741106799994,5.2,-3.64599508600001));
#355624=CARTESIAN_POINT('Ctrl Pts',(2.18741106799994,2.2,-3.64599508600001));
#355625=CARTESIAN_POINT('Ctrl Pts',(2.18709406699995,12.2,-3.64435307700001));
#355626=CARTESIAN_POINT('Ctrl Pts',(2.18709406699995,5.2,-3.64435307700001));
#355627=CARTESIAN_POINT('Ctrl Pts',(2.18709406699995,2.2,-3.64435307700001));
#355628=CARTESIAN_POINT('Ctrl Pts',(2.18677603499994,12.2,-3.64271583700001));
#355629=CARTESIAN_POINT('Ctrl Pts',(2.18677603499994,5.2,-3.64271583700001));
#355630=CARTESIAN_POINT('Ctrl Pts',(2.18677603499994,2.2,-3.64271583700001));
#355631=CARTESIAN_POINT('Ctrl Pts',(2.18645698499994,12.2,-3.64108337100001));
#355632=CARTESIAN_POINT('Ctrl Pts',(2.18645698499994,5.2,-3.64108337100001));
#355633=CARTESIAN_POINT('Ctrl Pts',(2.18645698499994,2.2,-3.64108337100001));
#355634=CARTESIAN_POINT('Ctrl Pts',(2.18613692599994,12.2,-3.63945568500001));
#355635=CARTESIAN_POINT('Ctrl Pts',(2.18613692599994,5.2,-3.63945568500001));
#355636=CARTESIAN_POINT('Ctrl Pts',(2.18613692599994,2.2,-3.63945568500001));
#355637=CARTESIAN_POINT('Ctrl Pts',(2.18581586899994,12.2,-3.63783278600001));
#355638=CARTESIAN_POINT('Ctrl Pts',(2.18581586899994,5.2,-3.63783278600001));
#355639=CARTESIAN_POINT('Ctrl Pts',(2.18581586899994,2.2,-3.63783278600001));
#355640=CARTESIAN_POINT('Ctrl Pts',(2.18549382499994,12.2,-3.63621468100002));
#355641=CARTESIAN_POINT('Ctrl Pts',(2.18549382499994,5.2,-3.63621468100002));
#355642=CARTESIAN_POINT('Ctrl Pts',(2.18549382499994,2.2,-3.63621468100002));
#355643=CARTESIAN_POINT('Ctrl Pts',(2.18517080599994,12.2,-3.63460137400001));
#355644=CARTESIAN_POINT('Ctrl Pts',(2.18517080599994,5.2,-3.63460137400001));
#355645=CARTESIAN_POINT('Ctrl Pts',(2.18517080599994,2.2,-3.63460137400001));
#355646=CARTESIAN_POINT('Ctrl Pts',(2.18484682099994,12.2,-3.63299287100002));
#355647=CARTESIAN_POINT('Ctrl Pts',(2.18484682099994,5.2,-3.63299287100002));
#355648=CARTESIAN_POINT('Ctrl Pts',(2.18484682099994,2.2,-3.63299287100002));
#355649=CARTESIAN_POINT('Ctrl Pts',(2.18452188399994,12.2,-3.63138918100002));
#355650=CARTESIAN_POINT('Ctrl Pts',(2.18452188399994,5.2,-3.63138918100002));
#355651=CARTESIAN_POINT('Ctrl Pts',(2.18452188399994,2.2,-3.63138918100002));
#355652=CARTESIAN_POINT('Ctrl Pts',(2.18419600199994,12.2,-3.62979030800001));
#355653=CARTESIAN_POINT('Ctrl Pts',(2.18419600199994,5.2,-3.62979030800001));
#355654=CARTESIAN_POINT('Ctrl Pts',(2.18419600199994,2.2,-3.62979030800001));
#355655=CARTESIAN_POINT('Ctrl Pts',(2.18386918899994,12.2,-3.62819625900002));
#355656=CARTESIAN_POINT('Ctrl Pts',(2.18386918899994,5.2,-3.62819625900002));
#355657=CARTESIAN_POINT('Ctrl Pts',(2.18386918899994,2.2,-3.62819625900002));
#355658=CARTESIAN_POINT('Ctrl Pts',(2.18354145499994,12.2,-3.62660704000001));
#355659=CARTESIAN_POINT('Ctrl Pts',(2.18354145499994,5.2,-3.62660704000001));
#355660=CARTESIAN_POINT('Ctrl Pts',(2.18354145499994,2.2,-3.62660704000001));
#355661=CARTESIAN_POINT('Ctrl Pts',(2.18321280999994,12.2,-3.62502265600002));
#355662=CARTESIAN_POINT('Ctrl Pts',(2.18321280999994,5.2,-3.62502265600002));
#355663=CARTESIAN_POINT('Ctrl Pts',(2.18321280999994,2.2,-3.62502265600002));
#355664=CARTESIAN_POINT('Ctrl Pts',(2.18288326799994,12.2,-3.62344311600001));
#355665=CARTESIAN_POINT('Ctrl Pts',(2.18288326799994,5.2,-3.62344311600001));
#355666=CARTESIAN_POINT('Ctrl Pts',(2.18288326799994,2.2,-3.62344311600001));
#355667=CARTESIAN_POINT('Ctrl Pts',(2.18255283799994,12.2,-3.62186842300002));
#355668=CARTESIAN_POINT('Ctrl Pts',(2.18255283799994,5.2,-3.62186842300002));
#355669=CARTESIAN_POINT('Ctrl Pts',(2.18255283799994,2.2,-3.62186842300002));
#355670=CARTESIAN_POINT('Ctrl Pts',(2.18222153099994,12.2,-3.62029858500001));
#355671=CARTESIAN_POINT('Ctrl Pts',(2.18222153099994,5.2,-3.62029858500001));
#355672=CARTESIAN_POINT('Ctrl Pts',(2.18222153099994,2.2,-3.62029858500001));
#355673=CARTESIAN_POINT('Ctrl Pts',(2.18188935999994,12.2,-3.61873360700002));
#355674=CARTESIAN_POINT('Ctrl Pts',(2.18188935999994,5.2,-3.61873360700002));
#355675=CARTESIAN_POINT('Ctrl Pts',(2.18188935999994,2.2,-3.61873360700002));
#355676=CARTESIAN_POINT('Ctrl Pts',(2.18155633399994,12.2,-3.61717349600001));
#355677=CARTESIAN_POINT('Ctrl Pts',(2.18155633399994,5.2,-3.61717349600001));
#355678=CARTESIAN_POINT('Ctrl Pts',(2.18155633399994,2.2,-3.61717349600001));
#355679=CARTESIAN_POINT('Ctrl Pts',(2.18122246499994,12.2,-3.61561825900001));
#355680=CARTESIAN_POINT('Ctrl Pts',(2.18122246499994,5.2,-3.61561825900001));
#355681=CARTESIAN_POINT('Ctrl Pts',(2.18122246499994,2.2,-3.61561825900001));
#355682=CARTESIAN_POINT('Ctrl Pts',(2.18088776599994,12.2,-3.61406790100002));
#355683=CARTESIAN_POINT('Ctrl Pts',(2.18088776599994,5.2,-3.61406790100002));
#355684=CARTESIAN_POINT('Ctrl Pts',(2.18088776599994,2.2,-3.61406790100002));
#355685=CARTESIAN_POINT('Ctrl Pts',(2.18055224499994,12.2,-3.61252242700001));
#355686=CARTESIAN_POINT('Ctrl Pts',(2.18055224499994,5.2,-3.61252242700001));
#355687=CARTESIAN_POINT('Ctrl Pts',(2.18055224499994,2.2,-3.61252242700001));
#355688=CARTESIAN_POINT('Ctrl Pts',(2.18021591699994,12.2,-3.61098184500001));
#355689=CARTESIAN_POINT('Ctrl Pts',(2.18021591699994,5.2,-3.61098184500001));
#355690=CARTESIAN_POINT('Ctrl Pts',(2.18021591699994,2.2,-3.61098184500001));
#355691=CARTESIAN_POINT('Ctrl Pts',(2.17987879099994,12.2,-3.60944616000001));
#355692=CARTESIAN_POINT('Ctrl Pts',(2.17987879099994,5.2,-3.60944616000001));
#355693=CARTESIAN_POINT('Ctrl Pts',(2.17987879099994,2.2,-3.60944616000001));
#355694=CARTESIAN_POINT('Ctrl Pts',(2.17954087899995,12.2,-3.60791538000001));
#355695=CARTESIAN_POINT('Ctrl Pts',(2.17954087899995,5.2,-3.60791538000001));
#355696=CARTESIAN_POINT('Ctrl Pts',(2.17954087899995,2.2,-3.60791538000001));
#355697=CARTESIAN_POINT('Ctrl Pts',(2.17920219199994,12.2,-3.60638950800002));
#355698=CARTESIAN_POINT('Ctrl Pts',(2.17920219199994,5.2,-3.60638950800002));
#355699=CARTESIAN_POINT('Ctrl Pts',(2.17920219199994,2.2,-3.60638950800002));
#355700=CARTESIAN_POINT('Ctrl Pts',(2.17886274299994,12.2,-3.60486855300001));
#355701=CARTESIAN_POINT('Ctrl Pts',(2.17886274299994,5.2,-3.60486855300001));
#355702=CARTESIAN_POINT('Ctrl Pts',(2.17886274299994,2.2,-3.60486855300001));
#355703=CARTESIAN_POINT('Ctrl Pts',(2.17852254199994,12.2,-3.60335252000001));
#355704=CARTESIAN_POINT('Ctrl Pts',(2.17852254199994,5.2,-3.60335252000001));
#355705=CARTESIAN_POINT('Ctrl Pts',(2.17852254199994,2.2,-3.60335252000001));
#355706=CARTESIAN_POINT('Ctrl Pts',(2.17818160099994,12.2,-3.60184141400001));
#355707=CARTESIAN_POINT('Ctrl Pts',(2.17818160099994,5.2,-3.60184141400001));
#355708=CARTESIAN_POINT('Ctrl Pts',(2.17818160099994,2.2,-3.60184141400001));
#355709=CARTESIAN_POINT('Ctrl Pts',(2.17783993199994,12.2,-3.60033524400002));
#355710=CARTESIAN_POINT('Ctrl Pts',(2.17783993199994,5.2,-3.60033524400002));
#355711=CARTESIAN_POINT('Ctrl Pts',(2.17783993199994,2.2,-3.60033524400002));
#355712=CARTESIAN_POINT('Ctrl Pts',(2.17749754499994,12.2,-3.59883401300001));
#355713=CARTESIAN_POINT('Ctrl Pts',(2.17749754499994,5.2,-3.59883401300001));
#355714=CARTESIAN_POINT('Ctrl Pts',(2.17749754499994,2.2,-3.59883401300001));
#355715=CARTESIAN_POINT('Ctrl Pts',(2.17715445399994,12.2,-3.59733772900002));
#355716=CARTESIAN_POINT('Ctrl Pts',(2.17715445399994,5.2,-3.59733772900002));
#355717=CARTESIAN_POINT('Ctrl Pts',(2.17715445399994,2.2,-3.59733772900002));
#355718=CARTESIAN_POINT('Ctrl Pts',(2.17681066799994,12.2,-3.59584639700001));
#355719=CARTESIAN_POINT('Ctrl Pts',(2.17681066799994,5.2,-3.59584639700001));
#355720=CARTESIAN_POINT('Ctrl Pts',(2.17681066799994,2.2,-3.59584639700001));
#355721=CARTESIAN_POINT('Ctrl Pts',(2.17646620199994,12.2,-3.59436002300002));
#355722=CARTESIAN_POINT('Ctrl Pts',(2.17646620199994,5.2,-3.59436002300002));
#355723=CARTESIAN_POINT('Ctrl Pts',(2.17646620199994,2.2,-3.59436002300002));
#355724=CARTESIAN_POINT('Ctrl Pts',(2.17612106499994,12.2,-3.59287861500002));
#355725=CARTESIAN_POINT('Ctrl Pts',(2.17612106499994,5.2,-3.59287861500002));
#355726=CARTESIAN_POINT('Ctrl Pts',(2.17612106499994,2.2,-3.59287861500002));
#355727=CARTESIAN_POINT('Ctrl Pts',(2.17577526999994,12.2,-3.59140217700002));
#355728=CARTESIAN_POINT('Ctrl Pts',(2.17577526999994,5.2,-3.59140217700002));
#355729=CARTESIAN_POINT('Ctrl Pts',(2.17577526999994,2.2,-3.59140217700002));
#355730=CARTESIAN_POINT('Ctrl Pts',(2.17542882699994,12.2,-3.58993071600001));
#355731=CARTESIAN_POINT('Ctrl Pts',(2.17542882699994,5.2,-3.58993071600001));
#355732=CARTESIAN_POINT('Ctrl Pts',(2.17542882699994,2.2,-3.58993071600001));
#355733=CARTESIAN_POINT('Ctrl Pts',(2.17508175099994,12.2,-3.58846423800002));
#355734=CARTESIAN_POINT('Ctrl Pts',(2.17508175099994,5.2,-3.58846423800002));
#355735=CARTESIAN_POINT('Ctrl Pts',(2.17508175099994,2.2,-3.58846423800002));
#355736=CARTESIAN_POINT('Ctrl Pts',(2.17473405099994,12.2,-3.58700275000002));
#355737=CARTESIAN_POINT('Ctrl Pts',(2.17473405099994,5.2,-3.58700275000002));
#355738=CARTESIAN_POINT('Ctrl Pts',(2.17473405099994,2.2,-3.58700275000002));
#355739=CARTESIAN_POINT('Ctrl Pts',(2.17438574099994,12.2,-3.58554625600001));
#355740=CARTESIAN_POINT('Ctrl Pts',(2.17438574099994,5.2,-3.58554625600001));
#355741=CARTESIAN_POINT('Ctrl Pts',(2.17438574099994,2.2,-3.58554625600001));
#355742=CARTESIAN_POINT('Ctrl Pts',(2.17403682999994,12.2,-3.58409476300002));
#355743=CARTESIAN_POINT('Ctrl Pts',(2.17403682999994,5.2,-3.58409476300002));
#355744=CARTESIAN_POINT('Ctrl Pts',(2.17403682999994,2.2,-3.58409476300002));
#355745=CARTESIAN_POINT('Ctrl Pts',(2.17368733399994,12.2,-3.58264827700001));
#355746=CARTESIAN_POINT('Ctrl Pts',(2.17368733399994,5.2,-3.58264827700001));
#355747=CARTESIAN_POINT('Ctrl Pts',(2.17368733399994,2.2,-3.58264827700001));
#355748=CARTESIAN_POINT('Ctrl Pts',(2.17333726099994,12.2,-3.58120680500001));
#355749=CARTESIAN_POINT('Ctrl Pts',(2.17333726099994,5.2,-3.58120680500001));
#355750=CARTESIAN_POINT('Ctrl Pts',(2.17333726099994,2.2,-3.58120680500001));
#355751=CARTESIAN_POINT('Ctrl Pts',(2.17298662499994,12.2,-3.57977035300001));
#355752=CARTESIAN_POINT('Ctrl Pts',(2.17298662499994,5.2,-3.57977035300001));
#355753=CARTESIAN_POINT('Ctrl Pts',(2.17298662499994,2.2,-3.57977035300001));
#355754=CARTESIAN_POINT('Ctrl Pts',(2.17263543799994,12.2,-3.57833892500001));
#355755=CARTESIAN_POINT('Ctrl Pts',(2.17263543799994,5.2,-3.57833892500001));
#355756=CARTESIAN_POINT('Ctrl Pts',(2.17263543799994,2.2,-3.57833892500001));
#355757=CARTESIAN_POINT('Ctrl Pts',(2.17228371199994,12.2,-3.57691252900001));
#355758=CARTESIAN_POINT('Ctrl Pts',(2.17228371199994,5.2,-3.57691252900001));
#355759=CARTESIAN_POINT('Ctrl Pts',(2.17228371199994,2.2,-3.57691252900001));
#355760=CARTESIAN_POINT('Ctrl Pts',(2.17193145999994,12.2,-3.57549117100001));
#355761=CARTESIAN_POINT('Ctrl Pts',(2.17193145999994,5.2,-3.57549117100001));
#355762=CARTESIAN_POINT('Ctrl Pts',(2.17193145999994,2.2,-3.57549117100001));
#355763=CARTESIAN_POINT('Ctrl Pts',(2.17157869199994,12.2,-3.57407485600001));
#355764=CARTESIAN_POINT('Ctrl Pts',(2.17157869199994,5.2,-3.57407485600001));
#355765=CARTESIAN_POINT('Ctrl Pts',(2.17157869199994,2.2,-3.57407485600001));
#355766=CARTESIAN_POINT('Ctrl Pts',(2.17122542199994,12.2,-3.57266359000001));
#355767=CARTESIAN_POINT('Ctrl Pts',(2.17122542199994,5.2,-3.57266359000001));
#355768=CARTESIAN_POINT('Ctrl Pts',(2.17122542199994,2.2,-3.57266359000001));
#355769=CARTESIAN_POINT('Ctrl Pts',(2.17087166199994,12.2,-3.57125738100001));
#355770=CARTESIAN_POINT('Ctrl Pts',(2.17087166199994,5.2,-3.57125738100001));
#355771=CARTESIAN_POINT('Ctrl Pts',(2.17087166199994,2.2,-3.57125738100001));
#355772=CARTESIAN_POINT('Ctrl Pts',(2.17051742299994,12.2,-3.56985623300002));
#355773=CARTESIAN_POINT('Ctrl Pts',(2.17051742299994,5.2,-3.56985623300002));
#355774=CARTESIAN_POINT('Ctrl Pts',(2.17051742299994,2.2,-3.56985623300002));
#355775=CARTESIAN_POINT('Ctrl Pts',(2.17016271799995,12.2,-3.56846015200002));
#355776=CARTESIAN_POINT('Ctrl Pts',(2.17016271799995,5.2,-3.56846015200002));
#355777=CARTESIAN_POINT('Ctrl Pts',(2.17016271799995,2.2,-3.56846015200002));
#355778=CARTESIAN_POINT('Ctrl Pts',(2.16980755899994,12.2,-3.56706914600001));
#355779=CARTESIAN_POINT('Ctrl Pts',(2.16980755899994,5.2,-3.56706914600001));
#355780=CARTESIAN_POINT('Ctrl Pts',(2.16980755899994,2.2,-3.56706914600001));
#355781=CARTESIAN_POINT('Ctrl Pts',(2.16945195799994,12.2,-3.56568321900002));
#355782=CARTESIAN_POINT('Ctrl Pts',(2.16945195799994,5.2,-3.56568321900002));
#355783=CARTESIAN_POINT('Ctrl Pts',(2.16945195799994,2.2,-3.56568321900002));
#355784=CARTESIAN_POINT('Ctrl Pts',(2.16909592999994,12.2,-3.56430237800001));
#355785=CARTESIAN_POINT('Ctrl Pts',(2.16909592999994,5.2,-3.56430237800001));
#355786=CARTESIAN_POINT('Ctrl Pts',(2.16909592999994,2.2,-3.56430237800001));
#355787=CARTESIAN_POINT('Ctrl Pts',(2.16873948499994,12.2,-3.56292662800001));
#355788=CARTESIAN_POINT('Ctrl Pts',(2.16873948499994,5.2,-3.56292662800001));
#355789=CARTESIAN_POINT('Ctrl Pts',(2.16873948499994,2.2,-3.56292662800001));
#355790=CARTESIAN_POINT('Ctrl Pts',(2.16838263499994,12.2,-3.56155597700001));
#355791=CARTESIAN_POINT('Ctrl Pts',(2.16838263499994,5.2,-3.56155597700001));
#355792=CARTESIAN_POINT('Ctrl Pts',(2.16838263499994,2.2,-3.56155597700001));
#355793=CARTESIAN_POINT('Ctrl Pts',(2.16802539399994,12.2,-3.56019042900002));
#355794=CARTESIAN_POINT('Ctrl Pts',(2.16802539399994,5.2,-3.56019042900002));
#355795=CARTESIAN_POINT('Ctrl Pts',(2.16802539399994,2.2,-3.56019042900002));
#355796=CARTESIAN_POINT('Ctrl Pts',(2.16766777399994,12.2,-3.55882999100002));
#355797=CARTESIAN_POINT('Ctrl Pts',(2.16766777399994,5.2,-3.55882999100002));
#355798=CARTESIAN_POINT('Ctrl Pts',(2.16766777399994,2.2,-3.55882999100002));
#355799=CARTESIAN_POINT('Ctrl Pts',(2.16730978699994,12.2,-3.55747466800001));
#355800=CARTESIAN_POINT('Ctrl Pts',(2.16730978699994,5.2,-3.55747466800001));
#355801=CARTESIAN_POINT('Ctrl Pts',(2.16730978699994,2.2,-3.55747466800001));
#355802=CARTESIAN_POINT('Ctrl Pts',(2.16695144699994,12.2,-3.55612446800002));
#355803=CARTESIAN_POINT('Ctrl Pts',(2.16695144699994,5.2,-3.55612446800002));
#355804=CARTESIAN_POINT('Ctrl Pts',(2.16695144699994,2.2,-3.55612446800002));
#355805=CARTESIAN_POINT('Ctrl Pts',(2.16659276399994,12.2,-3.55477939500001));
#355806=CARTESIAN_POINT('Ctrl Pts',(2.16659276399994,5.2,-3.55477939500001));
#355807=CARTESIAN_POINT('Ctrl Pts',(2.16659276399994,2.2,-3.55477939500001));
#355808=CARTESIAN_POINT('Ctrl Pts',(2.16623375399994,12.2,-3.55343945600001));
#355809=CARTESIAN_POINT('Ctrl Pts',(2.16623375399994,5.2,-3.55343945600001));
#355810=CARTESIAN_POINT('Ctrl Pts',(2.16623375399994,2.2,-3.55343945600001));
#355811=CARTESIAN_POINT('Ctrl Pts',(2.16587442599994,12.2,-3.55210465600001));
#355812=CARTESIAN_POINT('Ctrl Pts',(2.16587442599994,5.2,-3.55210465600001));
#355813=CARTESIAN_POINT('Ctrl Pts',(2.16587442599994,2.2,-3.55210465600001));
#355814=CARTESIAN_POINT('Ctrl Pts',(2.16551479599994,12.2,-3.55077500300002));
#355815=CARTESIAN_POINT('Ctrl Pts',(2.16551479599994,5.2,-3.55077500300002));
#355816=CARTESIAN_POINT('Ctrl Pts',(2.16551479599994,2.2,-3.55077500300002));
#355817=CARTESIAN_POINT('Ctrl Pts',(2.16515487499994,12.2,-3.54945050100001));
#355818=CARTESIAN_POINT('Ctrl Pts',(2.16515487499994,5.2,-3.54945050100001));
#355819=CARTESIAN_POINT('Ctrl Pts',(2.16515487499994,2.2,-3.54945050100001));
#355820=CARTESIAN_POINT('Ctrl Pts',(2.16479467599994,12.2,-3.54813115700002));
#355821=CARTESIAN_POINT('Ctrl Pts',(2.16479467599994,5.2,-3.54813115700002));
#355822=CARTESIAN_POINT('Ctrl Pts',(2.16479467599994,2.2,-3.54813115700002));
#355823=CARTESIAN_POINT('Ctrl Pts',(2.16443421299994,12.2,-3.54681697600002));
#355824=CARTESIAN_POINT('Ctrl Pts',(2.16443421299994,5.2,-3.54681697600002));
#355825=CARTESIAN_POINT('Ctrl Pts',(2.16443421299994,2.2,-3.54681697600002));
#355826=CARTESIAN_POINT('Ctrl Pts',(2.16407349699994,12.2,-3.54550796500002));
#355827=CARTESIAN_POINT('Ctrl Pts',(2.16407349699994,5.2,-3.54550796500002));
#355828=CARTESIAN_POINT('Ctrl Pts',(2.16407349699994,2.2,-3.54550796500002));
#355829=CARTESIAN_POINT('Ctrl Pts',(2.16371254199994,12.2,-3.54420412900001));
#355830=CARTESIAN_POINT('Ctrl Pts',(2.16371254199994,5.2,-3.54420412900001));
#355831=CARTESIAN_POINT('Ctrl Pts',(2.16371254199994,2.2,-3.54420412900001));
#355832=CARTESIAN_POINT('Ctrl Pts',(2.16335136099994,12.2,-3.54290547500002));
#355833=CARTESIAN_POINT('Ctrl Pts',(2.16335136099994,5.2,-3.54290547500002));
#355834=CARTESIAN_POINT('Ctrl Pts',(2.16335136099994,2.2,-3.54290547500002));
#355835=CARTESIAN_POINT('Ctrl Pts',(2.16298996699994,12.2,-3.54161200800001));
#355836=CARTESIAN_POINT('Ctrl Pts',(2.16298996699994,5.2,-3.54161200800001));
#355837=CARTESIAN_POINT('Ctrl Pts',(2.16298996699994,2.2,-3.54161200800001));
#355838=CARTESIAN_POINT('Ctrl Pts',(2.16262837099995,12.2,-3.54032373500001));
#355839=CARTESIAN_POINT('Ctrl Pts',(2.16262837099995,5.2,-3.54032373500001));
#355840=CARTESIAN_POINT('Ctrl Pts',(2.16262837099995,2.2,-3.54032373500001));
#355841=CARTESIAN_POINT('Ctrl Pts',(2.16226658899994,12.2,-3.53904066100001));
#355842=CARTESIAN_POINT('Ctrl Pts',(2.16226658899994,5.2,-3.53904066100001));
#355843=CARTESIAN_POINT('Ctrl Pts',(2.16226658899994,2.2,-3.53904066100001));
#355844=CARTESIAN_POINT('Ctrl Pts',(2.16190463199994,12.2,-3.53776279200002));
#355845=CARTESIAN_POINT('Ctrl Pts',(2.16190463199994,5.2,-3.53776279200002));
#355846=CARTESIAN_POINT('Ctrl Pts',(2.16190463199994,2.2,-3.53776279200002));
#355847=CARTESIAN_POINT('Ctrl Pts',(2.16154251599994,12.2,-3.53649013400001));
#355848=CARTESIAN_POINT('Ctrl Pts',(2.16154251599994,5.2,-3.53649013400001));
#355849=CARTESIAN_POINT('Ctrl Pts',(2.16154251599994,2.2,-3.53649013400001));
#355850=CARTESIAN_POINT('Ctrl Pts',(2.16118024999994,12.2,-3.53522269300001));
#355851=CARTESIAN_POINT('Ctrl Pts',(2.16118024999994,5.2,-3.53522269300001));
#355852=CARTESIAN_POINT('Ctrl Pts',(2.16118024999994,2.2,-3.53522269300001));
#355853=CARTESIAN_POINT('Ctrl Pts',(2.16081784999994,12.2,-3.53396047500001));
#355854=CARTESIAN_POINT('Ctrl Pts',(2.16081784999994,5.2,-3.53396047500001));
#355855=CARTESIAN_POINT('Ctrl Pts',(2.16081784999994,2.2,-3.53396047500001));
#355856=CARTESIAN_POINT('Ctrl Pts',(2.16045532699995,12.2,-3.53270348700002));
#355857=CARTESIAN_POINT('Ctrl Pts',(2.16045532699995,5.2,-3.53270348700002));
#355858=CARTESIAN_POINT('Ctrl Pts',(2.16045532699995,2.2,-3.53270348700002));
#355859=CARTESIAN_POINT('Ctrl Pts',(2.16009269699994,12.2,-3.53145173300002));
#355860=CARTESIAN_POINT('Ctrl Pts',(2.16009269699994,5.2,-3.53145173300002));
#355861=CARTESIAN_POINT('Ctrl Pts',(2.16009269699994,2.2,-3.53145173300002));
#355862=CARTESIAN_POINT('Ctrl Pts',(2.15972997299994,12.2,-3.53020522000001));
#355863=CARTESIAN_POINT('Ctrl Pts',(2.15972997299994,5.2,-3.53020522000001));
#355864=CARTESIAN_POINT('Ctrl Pts',(2.15972997299994,2.2,-3.53020522000001));
#355865=CARTESIAN_POINT('Ctrl Pts',(2.15936716599994,12.2,-3.52896395300001));
#355866=CARTESIAN_POINT('Ctrl Pts',(2.15936716599994,5.2,-3.52896395300001));
#355867=CARTESIAN_POINT('Ctrl Pts',(2.15936716599994,2.2,-3.52896395300001));
#355868=CARTESIAN_POINT('Ctrl Pts',(2.15900428999994,12.2,-3.52772793900002));
#355869=CARTESIAN_POINT('Ctrl Pts',(2.15900428999994,5.2,-3.52772793900002));
#355870=CARTESIAN_POINT('Ctrl Pts',(2.15900428999994,2.2,-3.52772793900002));
#355871=CARTESIAN_POINT('Ctrl Pts',(2.15864135999994,12.2,-3.52649718400002));
#355872=CARTESIAN_POINT('Ctrl Pts',(2.15864135999994,5.2,-3.52649718400002));
#355873=CARTESIAN_POINT('Ctrl Pts',(2.15864135999994,2.2,-3.52649718400002));
#355874=CARTESIAN_POINT('Ctrl Pts',(2.15827838899994,12.2,-3.52527169200001));
#355875=CARTESIAN_POINT('Ctrl Pts',(2.15827838899994,5.2,-3.52527169200001));
#355876=CARTESIAN_POINT('Ctrl Pts',(2.15827838899994,2.2,-3.52527169200001));
#355877=CARTESIAN_POINT('Ctrl Pts',(2.15791538899994,12.2,-3.52405147100002));
#355878=CARTESIAN_POINT('Ctrl Pts',(2.15791538899994,5.2,-3.52405147100002));
#355879=CARTESIAN_POINT('Ctrl Pts',(2.15791538899994,2.2,-3.52405147100002));
#355880=CARTESIAN_POINT('Ctrl Pts',(2.15755237499994,12.2,-3.52283652600001));
#355881=CARTESIAN_POINT('Ctrl Pts',(2.15755237499994,5.2,-3.52283652600001));
#355882=CARTESIAN_POINT('Ctrl Pts',(2.15755237499994,2.2,-3.52283652600001));
#355883=CARTESIAN_POINT('Ctrl Pts',(2.15718935999994,12.2,-3.52162686400002));
#355884=CARTESIAN_POINT('Ctrl Pts',(2.15718935999994,5.2,-3.52162686400002));
#355885=CARTESIAN_POINT('Ctrl Pts',(2.15718935999994,2.2,-3.52162686400002));
#355886=CARTESIAN_POINT('Ctrl Pts',(2.15682635699994,12.2,-3.52042248900001));
#355887=CARTESIAN_POINT('Ctrl Pts',(2.15682635699994,5.2,-3.52042248900001));
#355888=CARTESIAN_POINT('Ctrl Pts',(2.15682635699994,2.2,-3.52042248900001));
#355889=CARTESIAN_POINT('Ctrl Pts',(2.15646338099994,12.2,-3.51922340700002));
#355890=CARTESIAN_POINT('Ctrl Pts',(2.15646338099994,5.2,-3.51922340700002));
#355891=CARTESIAN_POINT('Ctrl Pts',(2.15646338099994,2.2,-3.51922340700002));
#355892=CARTESIAN_POINT('Ctrl Pts',(2.15610044499994,12.2,-3.51802962600001));
#355893=CARTESIAN_POINT('Ctrl Pts',(2.15610044499994,5.2,-3.51802962600001));
#355894=CARTESIAN_POINT('Ctrl Pts',(2.15610044499994,2.2,-3.51802962600001));
#355895=CARTESIAN_POINT('Ctrl Pts',(2.15573756299994,12.2,-3.51684114900001));
#355896=CARTESIAN_POINT('Ctrl Pts',(2.15573756299994,5.2,-3.51684114900001));
#355897=CARTESIAN_POINT('Ctrl Pts',(2.15573756299994,2.2,-3.51684114900001));
#355898=CARTESIAN_POINT('Ctrl Pts',(2.15537474699994,12.2,-3.51565798400001));
#355899=CARTESIAN_POINT('Ctrl Pts',(2.15537474699994,5.2,-3.51565798400001));
#355900=CARTESIAN_POINT('Ctrl Pts',(2.15537474699994,2.2,-3.51565798400001));
#355901=CARTESIAN_POINT('Ctrl Pts',(2.15501201299995,12.2,-3.51448013600002));
#355902=CARTESIAN_POINT('Ctrl Pts',(2.15501201299995,5.2,-3.51448013600002));
#355903=CARTESIAN_POINT('Ctrl Pts',(2.15501201299995,2.2,-3.51448013600002));
#355904=CARTESIAN_POINT('Ctrl Pts',(2.15464937399994,12.2,-3.51330761100002));
#355905=CARTESIAN_POINT('Ctrl Pts',(2.15464937399994,5.2,-3.51330761100002));
#355906=CARTESIAN_POINT('Ctrl Pts',(2.15464937399994,2.2,-3.51330761100002));
#355907=CARTESIAN_POINT('Ctrl Pts',(2.15428684399994,12.2,-3.51214041500001));
#355908=CARTESIAN_POINT('Ctrl Pts',(2.15428684399994,5.2,-3.51214041500001));
#355909=CARTESIAN_POINT('Ctrl Pts',(2.15428684399994,2.2,-3.51214041500001));
#355910=CARTESIAN_POINT('Ctrl Pts',(2.15392443699994,12.2,-3.51097855400001));
#355911=CARTESIAN_POINT('Ctrl Pts',(2.15392443699994,5.2,-3.51097855400001));
#355912=CARTESIAN_POINT('Ctrl Pts',(2.15392443699994,2.2,-3.51097855400001));
#355913=CARTESIAN_POINT('Ctrl Pts',(2.15356216599994,12.2,-3.50982203300001));
#355914=CARTESIAN_POINT('Ctrl Pts',(2.15356216599994,5.2,-3.50982203300001));
#355915=CARTESIAN_POINT('Ctrl Pts',(2.15356216599994,2.2,-3.50982203300001));
#355916=CARTESIAN_POINT('Ctrl Pts',(2.15320004599994,12.2,-3.50867085800001));
#355917=CARTESIAN_POINT('Ctrl Pts',(2.15320004599994,5.2,-3.50867085800001));
#355918=CARTESIAN_POINT('Ctrl Pts',(2.15320004599994,2.2,-3.50867085800001));
#355919=CARTESIAN_POINT('Ctrl Pts',(2.15283809099994,12.2,-3.50752503500001));
#355920=CARTESIAN_POINT('Ctrl Pts',(2.15283809099994,5.2,-3.50752503500001));
#355921=CARTESIAN_POINT('Ctrl Pts',(2.15283809099994,2.2,-3.50752503500001));
#355922=CARTESIAN_POINT('Ctrl Pts',(2.15247631499994,12.2,-3.50638457100001));
#355923=CARTESIAN_POINT('Ctrl Pts',(2.15247631499994,5.2,-3.50638457100001));
#355924=CARTESIAN_POINT('Ctrl Pts',(2.15247631499994,2.2,-3.50638457100001));
#355925=CARTESIAN_POINT('Ctrl Pts',(2.15211473199994,12.2,-3.50524947100002));
#355926=CARTESIAN_POINT('Ctrl Pts',(2.15211473199994,5.2,-3.50524947100002));
#355927=CARTESIAN_POINT('Ctrl Pts',(2.15211473199994,2.2,-3.50524947100002));
#355928=CARTESIAN_POINT('Ctrl Pts',(2.15175335499994,12.2,-3.50411974000002));
#355929=CARTESIAN_POINT('Ctrl Pts',(2.15175335499994,5.2,-3.50411974000002));
#355930=CARTESIAN_POINT('Ctrl Pts',(2.15175335499994,2.2,-3.50411974000002));
#355931=CARTESIAN_POINT('Ctrl Pts',(2.15139219999994,12.2,-3.50299538300002));
#355932=CARTESIAN_POINT('Ctrl Pts',(2.15139219999994,5.2,-3.50299538300002));
#355933=CARTESIAN_POINT('Ctrl Pts',(2.15139219999994,2.2,-3.50299538300002));
#355934=CARTESIAN_POINT('Ctrl Pts',(2.15103127999994,12.2,-3.50187640800002));
#355935=CARTESIAN_POINT('Ctrl Pts',(2.15103127999994,5.2,-3.50187640800002));
#355936=CARTESIAN_POINT('Ctrl Pts',(2.15103127999994,2.2,-3.50187640800002));
#355937=CARTESIAN_POINT('Ctrl Pts',(2.15067060999994,12.2,-3.50076282000002));
#355938=CARTESIAN_POINT('Ctrl Pts',(2.15067060999994,5.2,-3.50076282000002));
#355939=CARTESIAN_POINT('Ctrl Pts',(2.15067060999994,2.2,-3.50076282000002));
#355940=CARTESIAN_POINT('Ctrl Pts',(2.15031020399994,12.2,-3.49965462500001));
#355941=CARTESIAN_POINT('Ctrl Pts',(2.15031020399994,5.2,-3.49965462500001));
#355942=CARTESIAN_POINT('Ctrl Pts',(2.15031020399994,2.2,-3.49965462500001));
#355943=CARTESIAN_POINT('Ctrl Pts',(2.14995007699994,12.2,-3.49855182900002));
#355944=CARTESIAN_POINT('Ctrl Pts',(2.14995007699994,5.2,-3.49855182900002));
#355945=CARTESIAN_POINT('Ctrl Pts',(2.14995007699994,2.2,-3.49855182900002));
#355946=CARTESIAN_POINT('Ctrl Pts',(2.14959024099994,12.2,-3.49745443600002));
#355947=CARTESIAN_POINT('Ctrl Pts',(2.14959024099994,5.2,-3.49745443600002));
#355948=CARTESIAN_POINT('Ctrl Pts',(2.14959024099994,2.2,-3.49745443600002));
#355949=CARTESIAN_POINT('Ctrl Pts',(2.14923071399994,12.2,-3.49636245400001));
#355950=CARTESIAN_POINT('Ctrl Pts',(2.14923071399994,5.2,-3.49636245400001));
#355951=CARTESIAN_POINT('Ctrl Pts',(2.14923071399994,2.2,-3.49636245400001));
#355952=CARTESIAN_POINT('Ctrl Pts',(2.14887150799994,12.2,-3.49527588800001));
#355953=CARTESIAN_POINT('Ctrl Pts',(2.14887150799994,5.2,-3.49527588800001));
#355954=CARTESIAN_POINT('Ctrl Pts',(2.14887150799994,2.2,-3.49527588800001));
#355955=CARTESIAN_POINT('Ctrl Pts',(2.14851263799994,12.2,-3.49419474300001));
#355956=CARTESIAN_POINT('Ctrl Pts',(2.14851263799994,5.2,-3.49419474300001));
#355957=CARTESIAN_POINT('Ctrl Pts',(2.14851263799994,2.2,-3.49419474300001));
#355958=CARTESIAN_POINT('Ctrl Pts',(2.14815411799994,12.2,-3.49311902500002));
#355959=CARTESIAN_POINT('Ctrl Pts',(2.14815411799994,5.2,-3.49311902500002));
#355960=CARTESIAN_POINT('Ctrl Pts',(2.14815411799994,2.2,-3.49311902500002));
#355961=CARTESIAN_POINT('Ctrl Pts',(2.14779596399994,12.2,-3.49204874100002));
#355962=CARTESIAN_POINT('Ctrl Pts',(2.14779596399994,5.2,-3.49204874100002));
#355963=CARTESIAN_POINT('Ctrl Pts',(2.14779596399994,2.2,-3.49204874100002));
#355964=CARTESIAN_POINT('Ctrl Pts',(2.14743819099994,12.2,-3.49098389500002));
#355965=CARTESIAN_POINT('Ctrl Pts',(2.14743819099994,5.2,-3.49098389500002));
#355966=CARTESIAN_POINT('Ctrl Pts',(2.14743819099994,2.2,-3.49098389500002));
#355967=CARTESIAN_POINT('Ctrl Pts',(2.14708081099994,12.2,-3.48992449400002));
#355968=CARTESIAN_POINT('Ctrl Pts',(2.14708081099994,5.2,-3.48992449400002));
#355969=CARTESIAN_POINT('Ctrl Pts',(2.14708081099994,2.2,-3.48992449400002));
#355970=CARTESIAN_POINT('Ctrl Pts',(2.14672384099994,12.2,-3.48887054300001));
#355971=CARTESIAN_POINT('Ctrl Pts',(2.14672384099994,5.2,-3.48887054300001));
#355972=CARTESIAN_POINT('Ctrl Pts',(2.14672384099994,2.2,-3.48887054300001));
#355973=CARTESIAN_POINT('Ctrl Pts',(2.14636729499994,12.2,-3.48782204800001));
#355974=CARTESIAN_POINT('Ctrl Pts',(2.14636729499994,5.2,-3.48782204800001));
#355975=CARTESIAN_POINT('Ctrl Pts',(2.14636729499994,2.2,-3.48782204800001));
#355976=CARTESIAN_POINT('Ctrl Pts',(2.14601118799994,12.2,-3.48677901500002));
#355977=CARTESIAN_POINT('Ctrl Pts',(2.14601118799994,5.2,-3.48677901500002));
#355978=CARTESIAN_POINT('Ctrl Pts',(2.14601118799994,2.2,-3.48677901500002));
#355979=CARTESIAN_POINT('Ctrl Pts',(2.14565553399995,12.2,-3.48574145000002));
#355980=CARTESIAN_POINT('Ctrl Pts',(2.14565553399995,5.2,-3.48574145000002));
#355981=CARTESIAN_POINT('Ctrl Pts',(2.14565553399995,2.2,-3.48574145000002));
#355982=CARTESIAN_POINT('Ctrl Pts',(2.14530034899994,12.2,-3.48470935700002));
#355983=CARTESIAN_POINT('Ctrl Pts',(2.14530034899994,5.2,-3.48470935700002));
#355984=CARTESIAN_POINT('Ctrl Pts',(2.14530034899994,2.2,-3.48470935700002));
#355985=CARTESIAN_POINT('Ctrl Pts',(2.14494564799994,12.2,-3.48368274400002));
#355986=CARTESIAN_POINT('Ctrl Pts',(2.14494564799994,5.2,-3.48368274400002));
#355987=CARTESIAN_POINT('Ctrl Pts',(2.14494564799994,2.2,-3.48368274400002));
#355988=CARTESIAN_POINT('Ctrl Pts',(2.14459144499994,12.2,-3.48266161500002));
#355989=CARTESIAN_POINT('Ctrl Pts',(2.14459144499994,5.2,-3.48266161500002));
#355990=CARTESIAN_POINT('Ctrl Pts',(2.14459144499994,2.2,-3.48266161500002));
#355991=CARTESIAN_POINT('Ctrl Pts',(2.14423775599994,12.2,-3.48164597700002));
#355992=CARTESIAN_POINT('Ctrl Pts',(2.14423775599994,5.2,-3.48164597700002));
#355993=CARTESIAN_POINT('Ctrl Pts',(2.14423775599994,2.2,-3.48164597700002));
#355994=CARTESIAN_POINT('Ctrl Pts',(2.14388459599994,12.2,-3.48063583400001));
#355995=CARTESIAN_POINT('Ctrl Pts',(2.14388459599994,5.2,-3.48063583400001));
#355996=CARTESIAN_POINT('Ctrl Pts',(2.14388459599994,2.2,-3.48063583400001));
#355997=CARTESIAN_POINT('Ctrl Pts',(2.14353197899994,12.2,-3.47963119300001));
#355998=CARTESIAN_POINT('Ctrl Pts',(2.14353197899994,5.2,-3.47963119300001));
#355999=CARTESIAN_POINT('Ctrl Pts',(2.14353197899994,2.2,-3.47963119300001));
#356000=CARTESIAN_POINT('Ctrl Pts',(2.14317992199994,12.2,-3.47863205900001));
#356001=CARTESIAN_POINT('Ctrl Pts',(2.14317992199994,5.2,-3.47863205900001));
#356002=CARTESIAN_POINT('Ctrl Pts',(2.14317992199994,2.2,-3.47863205900001));
#356003=CARTESIAN_POINT('Ctrl Pts',(2.14282843799994,12.2,-3.47763843900001));
#356004=CARTESIAN_POINT('Ctrl Pts',(2.14282843799994,5.2,-3.47763843900001));
#356005=CARTESIAN_POINT('Ctrl Pts',(2.14282843799994,2.2,-3.47763843900001));
#356006=CARTESIAN_POINT('Ctrl Pts',(2.14247754299994,12.2,-3.47665033700002));
#356007=CARTESIAN_POINT('Ctrl Pts',(2.14247754299994,5.2,-3.47665033700002));
#356008=CARTESIAN_POINT('Ctrl Pts',(2.14247754299994,2.2,-3.47665033700002));
#356009=CARTESIAN_POINT('Ctrl Pts',(2.14212725399994,12.2,-3.47566776000001));
#356010=CARTESIAN_POINT('Ctrl Pts',(2.14212725399994,5.2,-3.47566776000001));
#356011=CARTESIAN_POINT('Ctrl Pts',(2.14212725399994,2.2,-3.47566776000001));
#356012=CARTESIAN_POINT('Ctrl Pts',(2.14177758399994,12.2,-3.47469071200001));
#356013=CARTESIAN_POINT('Ctrl Pts',(2.14177758399994,5.2,-3.47469071200001));
#356014=CARTESIAN_POINT('Ctrl Pts',(2.14177758399994,2.2,-3.47469071200001));
#356015=CARTESIAN_POINT('Ctrl Pts',(2.14142854999994,12.2,-3.47371920000001));
#356016=CARTESIAN_POINT('Ctrl Pts',(2.14142854999994,5.2,-3.47371920000001));
#356017=CARTESIAN_POINT('Ctrl Pts',(2.14142854999994,2.2,-3.47371920000001));
#356018=CARTESIAN_POINT('Ctrl Pts',(2.14108016699994,12.2,-3.47275323000002));
#356019=CARTESIAN_POINT('Ctrl Pts',(2.14108016699994,5.2,-3.47275323000002));
#356020=CARTESIAN_POINT('Ctrl Pts',(2.14108016699994,2.2,-3.47275323000002));
#356021=CARTESIAN_POINT('Ctrl Pts',(2.14073244999994,12.2,-3.47179280600002));
#356022=CARTESIAN_POINT('Ctrl Pts',(2.14073244999994,5.2,-3.47179280600002));
#356023=CARTESIAN_POINT('Ctrl Pts',(2.14073244999994,2.2,-3.47179280600002));
#356024=CARTESIAN_POINT('Ctrl Pts',(2.14038541399994,12.2,-3.47083793500001));
#356025=CARTESIAN_POINT('Ctrl Pts',(2.14038541399994,5.2,-3.47083793500001));
#356026=CARTESIAN_POINT('Ctrl Pts',(2.14038541399994,2.2,-3.47083793500001));
#356027=CARTESIAN_POINT('Ctrl Pts',(2.14003907599994,12.2,-3.46988862200002));
#356028=CARTESIAN_POINT('Ctrl Pts',(2.14003907599994,5.2,-3.46988862200002));
#356029=CARTESIAN_POINT('Ctrl Pts',(2.14003907599994,2.2,-3.46988862200002));
#356030=CARTESIAN_POINT('Ctrl Pts',(2.13969345099994,12.2,-3.46894487300001));
#356031=CARTESIAN_POINT('Ctrl Pts',(2.13969345099994,5.2,-3.46894487300001));
#356032=CARTESIAN_POINT('Ctrl Pts',(2.13969345099994,2.2,-3.46894487300001));
#356033=CARTESIAN_POINT('Ctrl Pts',(2.13934855399994,12.2,-3.46800669400002));
#356034=CARTESIAN_POINT('Ctrl Pts',(2.13934855399994,5.2,-3.46800669400002));
#356035=CARTESIAN_POINT('Ctrl Pts',(2.13934855399994,2.2,-3.46800669400002));
#356036=CARTESIAN_POINT('Ctrl Pts',(2.13900440199994,12.2,-3.46707408900001));
#356037=CARTESIAN_POINT('Ctrl Pts',(2.13900440199994,5.2,-3.46707408900001));
#356038=CARTESIAN_POINT('Ctrl Pts',(2.13900440199994,2.2,-3.46707408900001));
#356039=CARTESIAN_POINT('Ctrl Pts',(2.13866100999994,12.2,-3.46614706600001));
#356040=CARTESIAN_POINT('Ctrl Pts',(2.13866100999994,5.2,-3.46614706600001));
#356041=CARTESIAN_POINT('Ctrl Pts',(2.13866100999994,2.2,-3.46614706600001));
#356042=CARTESIAN_POINT('Ctrl Pts',(2.13831839299994,12.2,-3.46522562800001));
#356043=CARTESIAN_POINT('Ctrl Pts',(2.13831839299994,5.2,-3.46522562800001));
#356044=CARTESIAN_POINT('Ctrl Pts',(2.13831839299994,2.2,-3.46522562800001));
#356045=CARTESIAN_POINT('Ctrl Pts',(2.13797656899994,12.2,-3.46430978300001));
#356046=CARTESIAN_POINT('Ctrl Pts',(2.13797656899994,5.2,-3.46430978300001));
#356047=CARTESIAN_POINT('Ctrl Pts',(2.13797656899994,2.2,-3.46430978300001));
#356048=CARTESIAN_POINT('Ctrl Pts',(2.13763555199994,12.2,-3.46339953500001));
#356049=CARTESIAN_POINT('Ctrl Pts',(2.13763555199994,5.2,-3.46339953500001));
#356050=CARTESIAN_POINT('Ctrl Pts',(2.13763555199994,2.2,-3.46339953500001));
#356051=CARTESIAN_POINT('Ctrl Pts',(2.13729535799994,12.2,-3.46249489000002));
#356052=CARTESIAN_POINT('Ctrl Pts',(2.13729535799994,5.2,-3.46249489000002));
#356053=CARTESIAN_POINT('Ctrl Pts',(2.13729535799994,2.2,-3.46249489000002));
#356054=CARTESIAN_POINT('Ctrl Pts',(2.13695600499994,12.2,-3.46159585300001));
#356055=CARTESIAN_POINT('Ctrl Pts',(2.13695600499994,5.2,-3.46159585300001));
#356056=CARTESIAN_POINT('Ctrl Pts',(2.13695600499994,2.2,-3.46159585300001));
#356057=CARTESIAN_POINT('Ctrl Pts',(2.13661750599994,12.2,-3.46070243100002));
#356058=CARTESIAN_POINT('Ctrl Pts',(2.13661750599994,5.2,-3.46070243100002));
#356059=CARTESIAN_POINT('Ctrl Pts',(2.13661750599994,2.2,-3.46070243100002));
#356060=CARTESIAN_POINT('Ctrl Pts',(2.13627987899994,12.2,-3.45981462900002));
#356061=CARTESIAN_POINT('Ctrl Pts',(2.13627987899994,5.2,-3.45981462900002));
#356062=CARTESIAN_POINT('Ctrl Pts',(2.13627987899994,2.2,-3.45981462900002));
#356063=CARTESIAN_POINT('Ctrl Pts',(2.13594314099994,12.2,-3.45893245100001));
#356064=CARTESIAN_POINT('Ctrl Pts',(2.13594314099994,5.2,-3.45893245100001));
#356065=CARTESIAN_POINT('Ctrl Pts',(2.13594314099994,2.2,-3.45893245100001));
#356066=CARTESIAN_POINT('Ctrl Pts',(2.13560730499994,12.2,-3.45805590500001));
#356067=CARTESIAN_POINT('Ctrl Pts',(2.13560730499994,5.2,-3.45805590500001));
#356068=CARTESIAN_POINT('Ctrl Pts',(2.13560730499994,2.2,-3.45805590500001));
#356069=CARTESIAN_POINT('Ctrl Pts',(2.13527238999994,12.2,-3.45718499500002));
#356070=CARTESIAN_POINT('Ctrl Pts',(2.13527238999994,5.2,-3.45718499500002));
#356071=CARTESIAN_POINT('Ctrl Pts',(2.13527238999994,2.2,-3.45718499500002));
#356072=CARTESIAN_POINT('Ctrl Pts',(2.13493841199994,12.2,-3.45631972700001));
#356073=CARTESIAN_POINT('Ctrl Pts',(2.13493841199994,5.2,-3.45631972700001));
#356074=CARTESIAN_POINT('Ctrl Pts',(2.13493841199994,2.2,-3.45631972700001));
#356075=CARTESIAN_POINT('Ctrl Pts',(2.13460538699994,12.2,-3.45546010700001));
#356076=CARTESIAN_POINT('Ctrl Pts',(2.13460538699994,5.2,-3.45546010700001));
#356077=CARTESIAN_POINT('Ctrl Pts',(2.13460538699994,2.2,-3.45546010700001));
#356078=CARTESIAN_POINT('Ctrl Pts',(2.13427332999994,12.2,-3.45460614000002));
#356079=CARTESIAN_POINT('Ctrl Pts',(2.13427332999994,5.2,-3.45460614000002));
#356080=CARTESIAN_POINT('Ctrl Pts',(2.13427332999994,2.2,-3.45460614000002));
#356081=CARTESIAN_POINT('Ctrl Pts',(2.13394225899994,12.2,-3.45375783200002));
#356082=CARTESIAN_POINT('Ctrl Pts',(2.13394225899994,5.2,-3.45375783200002));
#356083=CARTESIAN_POINT('Ctrl Pts',(2.13394225899994,2.2,-3.45375783200002));
#356084=CARTESIAN_POINT('Ctrl Pts',(2.13361218999994,12.2,-3.45291518600002));
#356085=CARTESIAN_POINT('Ctrl Pts',(2.13361218999994,5.2,-3.45291518600002));
#356086=CARTESIAN_POINT('Ctrl Pts',(2.13361218999994,2.2,-3.45291518600002));
#356087=CARTESIAN_POINT('Ctrl Pts',(2.13328313999994,12.2,-3.45207821100002));
#356088=CARTESIAN_POINT('Ctrl Pts',(2.13328313999994,5.2,-3.45207821100002));
#356089=CARTESIAN_POINT('Ctrl Pts',(2.13328313999994,2.2,-3.45207821100002));
#356090=CARTESIAN_POINT('Ctrl Pts',(2.13295512499994,12.2,-3.45124691100001));
#356091=CARTESIAN_POINT('Ctrl Pts',(2.13295512499994,5.2,-3.45124691100001));
#356092=CARTESIAN_POINT('Ctrl Pts',(2.13295512499994,2.2,-3.45124691100001));
#356093=CARTESIAN_POINT('Ctrl Pts',(2.13262816099994,12.2,-3.45042129200001));
#356094=CARTESIAN_POINT('Ctrl Pts',(2.13262816099994,5.2,-3.45042129200001));
#356095=CARTESIAN_POINT('Ctrl Pts',(2.13262816099994,2.2,-3.45042129200001));
#356096=CARTESIAN_POINT('Ctrl Pts',(2.13230226599994,12.2,-3.44960135800001));
#356097=CARTESIAN_POINT('Ctrl Pts',(2.13230226599994,5.2,-3.44960135800001));
#356098=CARTESIAN_POINT('Ctrl Pts',(2.13230226599994,2.2,-3.44960135800001));
#356099=CARTESIAN_POINT('Ctrl Pts',(2.13197745699994,12.2,-3.44878711700002));
#356100=CARTESIAN_POINT('Ctrl Pts',(2.13197745699994,5.2,-3.44878711700002));
#356101=CARTESIAN_POINT('Ctrl Pts',(2.13197745699994,2.2,-3.44878711700002));
#356102=CARTESIAN_POINT('Ctrl Pts',(2.13165374899994,12.2,-3.44797857200001));
#356103=CARTESIAN_POINT('Ctrl Pts',(2.13165374899994,5.2,-3.44797857200001));
#356104=CARTESIAN_POINT('Ctrl Pts',(2.13165374899994,2.2,-3.44797857200001));
#356105=CARTESIAN_POINT('Ctrl Pts',(2.13133115999994,12.2,-3.44717573000001));
#356106=CARTESIAN_POINT('Ctrl Pts',(2.13133115999994,5.2,-3.44717573000001));
#356107=CARTESIAN_POINT('Ctrl Pts',(2.13133115999994,2.2,-3.44717573000001));
#356108=CARTESIAN_POINT('Ctrl Pts',(2.13100970599994,12.2,-3.44637859500001));
#356109=CARTESIAN_POINT('Ctrl Pts',(2.13100970599994,5.2,-3.44637859500001));
#356110=CARTESIAN_POINT('Ctrl Pts',(2.13100970599994,2.2,-3.44637859500001));
#356111=CARTESIAN_POINT('Ctrl Pts',(2.13068940599995,12.2,-3.44558717500002));
#356112=CARTESIAN_POINT('Ctrl Pts',(2.13068940599995,5.2,-3.44558717500002));
#356113=CARTESIAN_POINT('Ctrl Pts',(2.13068940599995,2.2,-3.44558717500002));
#356114=CARTESIAN_POINT('Ctrl Pts',(2.13037027499994,12.2,-3.44480147200001));
#356115=CARTESIAN_POINT('Ctrl Pts',(2.13037027499994,5.2,-3.44480147200001));
#356116=CARTESIAN_POINT('Ctrl Pts',(2.13037027499994,2.2,-3.44480147200001));
#356117=CARTESIAN_POINT('Ctrl Pts',(2.13005233099994,12.2,-3.44402149500001));
#356118=CARTESIAN_POINT('Ctrl Pts',(2.13005233099994,5.2,-3.44402149500001));
#356119=CARTESIAN_POINT('Ctrl Pts',(2.13005233099994,2.2,-3.44402149500001));
#356120=CARTESIAN_POINT('Ctrl Pts',(2.12973558999995,12.2,-3.44324724700002));
#356121=CARTESIAN_POINT('Ctrl Pts',(2.12973558999995,5.2,-3.44324724700002));
#356122=CARTESIAN_POINT('Ctrl Pts',(2.12973558999995,2.2,-3.44324724700002));
#356123=CARTESIAN_POINT('Ctrl Pts',(2.12942007099994,12.2,-3.44247873500001));
#356124=CARTESIAN_POINT('Ctrl Pts',(2.12942007099994,5.2,-3.44247873500001));
#356125=CARTESIAN_POINT('Ctrl Pts',(2.12942007099994,2.2,-3.44247873500001));
#356126=CARTESIAN_POINT('Ctrl Pts',(2.12910578899994,12.2,-3.44171596300002));
#356127=CARTESIAN_POINT('Ctrl Pts',(2.12910578899994,5.2,-3.44171596300002));
#356128=CARTESIAN_POINT('Ctrl Pts',(2.12910578899994,2.2,-3.44171596300002));
#356129=CARTESIAN_POINT('Ctrl Pts',(2.12879276299994,12.2,-3.44095893700001));
#356130=CARTESIAN_POINT('Ctrl Pts',(2.12879276299994,5.2,-3.44095893700001));
#356131=CARTESIAN_POINT('Ctrl Pts',(2.12879276299994,2.2,-3.44095893700001));
#356132=CARTESIAN_POINT('Ctrl Pts',(2.12848100899994,12.2,-3.44020766300002));
#356133=CARTESIAN_POINT('Ctrl Pts',(2.12848100899994,5.2,-3.44020766300002));
#356134=CARTESIAN_POINT('Ctrl Pts',(2.12848100899994,2.2,-3.44020766300002));
#356135=CARTESIAN_POINT('Ctrl Pts',(2.12817054599994,12.2,-3.43946214500002));
#356136=CARTESIAN_POINT('Ctrl Pts',(2.12817054599994,5.2,-3.43946214500002));
#356137=CARTESIAN_POINT('Ctrl Pts',(2.12817054599994,2.2,-3.43946214500002));
#356138=CARTESIAN_POINT('Ctrl Pts',(2.12786138899994,12.2,-3.43872239000001));
#356139=CARTESIAN_POINT('Ctrl Pts',(2.12786138899994,5.2,-3.43872239000001));
#356140=CARTESIAN_POINT('Ctrl Pts',(2.12786138899994,2.2,-3.43872239000001));
#356141=CARTESIAN_POINT('Ctrl Pts',(2.12755355799994,12.2,-3.43798840300002));
#356142=CARTESIAN_POINT('Ctrl Pts',(2.12755355799994,5.2,-3.43798840300002));
#356143=CARTESIAN_POINT('Ctrl Pts',(2.12755355799994,2.2,-3.43798840300002));
#356144=CARTESIAN_POINT('Ctrl Pts',(2.12724706999994,12.2,-3.43726018800002));
#356145=CARTESIAN_POINT('Ctrl Pts',(2.12724706999994,5.2,-3.43726018800002));
#356146=CARTESIAN_POINT('Ctrl Pts',(2.12724706999994,2.2,-3.43726018800002));
#356147=CARTESIAN_POINT('Ctrl Pts',(2.12694194099994,12.2,-3.43653775300002));
#356148=CARTESIAN_POINT('Ctrl Pts',(2.12694194099994,5.2,-3.43653775300002));
#356149=CARTESIAN_POINT('Ctrl Pts',(2.12694194099994,2.2,-3.43653775300002));
#356150=CARTESIAN_POINT('Ctrl Pts',(2.12663818999994,12.2,-3.43582110000002));
#356151=CARTESIAN_POINT('Ctrl Pts',(2.12663818999994,5.2,-3.43582110000002));
#356152=CARTESIAN_POINT('Ctrl Pts',(2.12663818999994,2.2,-3.43582110000002));
#356153=CARTESIAN_POINT('Ctrl Pts',(2.12633583399994,12.2,-3.43511023700001));
#356154=CARTESIAN_POINT('Ctrl Pts',(2.12633583399994,5.2,-3.43511023700001));
#356155=CARTESIAN_POINT('Ctrl Pts',(2.12633583399994,2.2,-3.43511023700001));
#356156=CARTESIAN_POINT('Ctrl Pts',(2.12603489099994,12.2,-3.43440516800001));
#356157=CARTESIAN_POINT('Ctrl Pts',(2.12603489099994,5.2,-3.43440516800001));
#356158=CARTESIAN_POINT('Ctrl Pts',(2.12603489099994,2.2,-3.43440516800001));
#356159=CARTESIAN_POINT('Ctrl Pts',(2.12573537999994,12.2,-3.43370590000001));
#356160=CARTESIAN_POINT('Ctrl Pts',(2.12573537999994,5.2,-3.43370590000001));
#356161=CARTESIAN_POINT('Ctrl Pts',(2.12573537999994,2.2,-3.43370590000001));
#356162=CARTESIAN_POINT('Ctrl Pts',(2.12543731699994,12.2,-3.43301243700001));
#356163=CARTESIAN_POINT('Ctrl Pts',(2.12543731699994,5.2,-3.43301243700001));
#356164=CARTESIAN_POINT('Ctrl Pts',(2.12543731699994,2.2,-3.43301243700001));
#356165=CARTESIAN_POINT('Ctrl Pts',(2.12514071999994,12.2,-3.43232478400001));
#356166=CARTESIAN_POINT('Ctrl Pts',(2.12514071999994,5.2,-3.43232478400001));
#356167=CARTESIAN_POINT('Ctrl Pts',(2.12514071999994,2.2,-3.43232478400001));
#356168=CARTESIAN_POINT('Ctrl Pts',(2.12484560899994,12.2,-3.43164294800001));
#356169=CARTESIAN_POINT('Ctrl Pts',(2.12484560899994,5.2,-3.43164294800001));
#356170=CARTESIAN_POINT('Ctrl Pts',(2.12484560899994,2.2,-3.43164294800001));
#356171=CARTESIAN_POINT('Ctrl Pts',(2.12455199899994,12.2,-3.43096693100001));
#356172=CARTESIAN_POINT('Ctrl Pts',(2.12455199899994,5.2,-3.43096693100001));
#356173=CARTESIAN_POINT('Ctrl Pts',(2.12455199899994,2.2,-3.43096693100001));
#356174=CARTESIAN_POINT('Ctrl Pts',(2.12425991099995,12.2,-3.43029674300002));
#356175=CARTESIAN_POINT('Ctrl Pts',(2.12425991099995,5.2,-3.43029674300002));
#356176=CARTESIAN_POINT('Ctrl Pts',(2.12425991099995,2.2,-3.43029674300002));
#356177=CARTESIAN_POINT('Ctrl Pts',(2.12396936099994,12.2,-3.42963238600001));
#356178=CARTESIAN_POINT('Ctrl Pts',(2.12396936099994,5.2,-3.42963238600001));
#356179=CARTESIAN_POINT('Ctrl Pts',(2.12396936099994,2.2,-3.42963238600001));
#356180=CARTESIAN_POINT('Ctrl Pts',(2.12368036799994,12.2,-3.42897386600002));
#356181=CARTESIAN_POINT('Ctrl Pts',(2.12368036799994,5.2,-3.42897386600002));
#356182=CARTESIAN_POINT('Ctrl Pts',(2.12368036799994,2.2,-3.42897386600002));
#356183=CARTESIAN_POINT('Ctrl Pts',(2.12339295199994,12.2,-3.42832118800001));
#356184=CARTESIAN_POINT('Ctrl Pts',(2.12339295199994,5.2,-3.42832118800001));
#356185=CARTESIAN_POINT('Ctrl Pts',(2.12339295199994,2.2,-3.42832118800001));
#356186=CARTESIAN_POINT('Ctrl Pts',(2.12310712799994,12.2,-3.42767435900001));
#356187=CARTESIAN_POINT('Ctrl Pts',(2.12310712799994,5.2,-3.42767435900001));
#356188=CARTESIAN_POINT('Ctrl Pts',(2.12310712799994,2.2,-3.42767435900001));
#356189=CARTESIAN_POINT('Ctrl Pts',(2.12282291699994,12.2,-3.42703338200002));
#356190=CARTESIAN_POINT('Ctrl Pts',(2.12282291699994,5.2,-3.42703338200002));
#356191=CARTESIAN_POINT('Ctrl Pts',(2.12282291699994,2.2,-3.42703338200002));
#356192=CARTESIAN_POINT('Ctrl Pts',(2.12254033599994,12.2,-3.42639826400001));
#356193=CARTESIAN_POINT('Ctrl Pts',(2.12254033599994,5.2,-3.42639826400001));
#356194=CARTESIAN_POINT('Ctrl Pts',(2.12254033599994,2.2,-3.42639826400001));
#356195=CARTESIAN_POINT('Ctrl Pts',(2.12225940399994,12.2,-3.42576900900001));
#356196=CARTESIAN_POINT('Ctrl Pts',(2.12225940399994,5.2,-3.42576900900001));
#356197=CARTESIAN_POINT('Ctrl Pts',(2.12225940399994,2.2,-3.42576900900001));
#356198=CARTESIAN_POINT('Ctrl Pts',(2.12198013999994,12.2,-3.42514562300002));
#356199=CARTESIAN_POINT('Ctrl Pts',(2.12198013999994,5.2,-3.42514562300002));
#356200=CARTESIAN_POINT('Ctrl Pts',(2.12198013999994,2.2,-3.42514562300002));
#356201=CARTESIAN_POINT('Ctrl Pts',(2.12170256199994,12.2,-3.42452811200001));
#356202=CARTESIAN_POINT('Ctrl Pts',(2.12170256199994,5.2,-3.42452811200001));
#356203=CARTESIAN_POINT('Ctrl Pts',(2.12170256199994,2.2,-3.42452811200001));
#356204=CARTESIAN_POINT('Ctrl Pts',(2.12142668899994,12.2,-3.42391647900001));
#356205=CARTESIAN_POINT('Ctrl Pts',(2.12142668899994,5.2,-3.42391647900001));
#356206=CARTESIAN_POINT('Ctrl Pts',(2.12142668899994,2.2,-3.42391647900001));
#356207=CARTESIAN_POINT('Ctrl Pts',(2.12115253899994,12.2,-3.42331073200001));
#356208=CARTESIAN_POINT('Ctrl Pts',(2.12115253899994,5.2,-3.42331073200001));
#356209=CARTESIAN_POINT('Ctrl Pts',(2.12115253899994,2.2,-3.42331073200001));
#356210=CARTESIAN_POINT('Ctrl Pts',(2.12088013199994,12.2,-3.42271087300002));
#356211=CARTESIAN_POINT('Ctrl Pts',(2.12088013199994,5.2,-3.42271087300002));
#356212=CARTESIAN_POINT('Ctrl Pts',(2.12088013199994,2.2,-3.42271087300002));
#356213=CARTESIAN_POINT('Ctrl Pts',(2.12060948599994,12.2,-3.42211691100001));
#356214=CARTESIAN_POINT('Ctrl Pts',(2.12060948599994,5.2,-3.42211691100001));
#356215=CARTESIAN_POINT('Ctrl Pts',(2.12060948599994,2.2,-3.42211691100001));
#356216=CARTESIAN_POINT('Ctrl Pts',(2.12034061999994,12.2,-3.42152884800001));
#356217=CARTESIAN_POINT('Ctrl Pts',(2.12034061999994,5.2,-3.42152884800001));
#356218=CARTESIAN_POINT('Ctrl Pts',(2.12034061999994,2.2,-3.42152884800001));
#356219=CARTESIAN_POINT('Ctrl Pts',(2.12007355199994,12.2,-3.42094669100002));
#356220=CARTESIAN_POINT('Ctrl Pts',(2.12007355199994,5.2,-3.42094669100002));
#356221=CARTESIAN_POINT('Ctrl Pts',(2.12007355199994,2.2,-3.42094669100002));
#356222=CARTESIAN_POINT('Ctrl Pts',(2.11980830399995,12.2,-3.42037044400001));
#356223=CARTESIAN_POINT('Ctrl Pts',(2.11980830399995,5.2,-3.42037044400001));
#356224=CARTESIAN_POINT('Ctrl Pts',(2.11980830399995,2.2,-3.42037044400001));
#356225=CARTESIAN_POINT('Ctrl Pts',(2.11954489199994,12.2,-3.41980011300001));
#356226=CARTESIAN_POINT('Ctrl Pts',(2.11954489199994,5.2,-3.41980011300001));
#356227=CARTESIAN_POINT('Ctrl Pts',(2.11954489199994,2.2,-3.41980011300001));
#356228=CARTESIAN_POINT('Ctrl Pts',(2.11928333699994,12.2,-3.41923570400001));
#356229=CARTESIAN_POINT('Ctrl Pts',(2.11928333699994,5.2,-3.41923570400001));
#356230=CARTESIAN_POINT('Ctrl Pts',(2.11928333699994,2.2,-3.41923570400001));
#356231=CARTESIAN_POINT('Ctrl Pts',(2.11902365799994,12.2,-3.41867722100002));
#356232=CARTESIAN_POINT('Ctrl Pts',(2.11902365799994,5.2,-3.41867722100002));
#356233=CARTESIAN_POINT('Ctrl Pts',(2.11902365799994,2.2,-3.41867722100002));
#356234=CARTESIAN_POINT('Ctrl Pts',(2.11876587399995,12.2,-3.41812466800001));
#356235=CARTESIAN_POINT('Ctrl Pts',(2.11876587399995,5.2,-3.41812466800001));
#356236=CARTESIAN_POINT('Ctrl Pts',(2.11876587399995,2.2,-3.41812466800001));
#356237=CARTESIAN_POINT('Ctrl Pts',(2.11851000399994,12.2,-3.41757805300002));
#356238=CARTESIAN_POINT('Ctrl Pts',(2.11851000399994,5.2,-3.41757805300002));
#356239=CARTESIAN_POINT('Ctrl Pts',(2.11851000399994,2.2,-3.41757805300002));
#356240=CARTESIAN_POINT('Ctrl Pts',(2.11825606799994,12.2,-3.41703738000001));
#356241=CARTESIAN_POINT('Ctrl Pts',(2.11825606799994,5.2,-3.41703738000001));
#356242=CARTESIAN_POINT('Ctrl Pts',(2.11825606799994,2.2,-3.41703738000001));
#356243=CARTESIAN_POINT('Ctrl Pts',(2.11800408499994,12.2,-3.41650265300002));
#356244=CARTESIAN_POINT('Ctrl Pts',(2.11800408499994,5.2,-3.41650265300002));
#356245=CARTESIAN_POINT('Ctrl Pts',(2.11800408499994,2.2,-3.41650265300002));
#356246=CARTESIAN_POINT('Ctrl Pts',(2.11775407499994,12.2,-3.41597387700002));
#356247=CARTESIAN_POINT('Ctrl Pts',(2.11775407499994,5.2,-3.41597387700002));
#356248=CARTESIAN_POINT('Ctrl Pts',(2.11775407499994,2.2,-3.41597387700002));
#356249=CARTESIAN_POINT('Ctrl Pts',(2.11750605799994,12.2,-3.41545106000002));
#356250=CARTESIAN_POINT('Ctrl Pts',(2.11750605799994,5.2,-3.41545106000002));
#356251=CARTESIAN_POINT('Ctrl Pts',(2.11750605799994,2.2,-3.41545106000002));
#356252=CARTESIAN_POINT('Ctrl Pts',(2.11726005199994,12.2,-3.41493420500001));
#356253=CARTESIAN_POINT('Ctrl Pts',(2.11726005199994,5.2,-3.41493420500001));
#356254=CARTESIAN_POINT('Ctrl Pts',(2.11726005199994,2.2,-3.41493420500001));
#356255=CARTESIAN_POINT('Ctrl Pts',(2.11701607899994,12.2,-3.41442331700001));
#356256=CARTESIAN_POINT('Ctrl Pts',(2.11701607899994,5.2,-3.41442331700001));
#356257=CARTESIAN_POINT('Ctrl Pts',(2.11701607899994,2.2,-3.41442331700001));
#356258=CARTESIAN_POINT('Ctrl Pts',(2.11677415599994,12.2,-3.41391840100002));
#356259=CARTESIAN_POINT('Ctrl Pts',(2.11677415599994,5.2,-3.41391840100002));
#356260=CARTESIAN_POINT('Ctrl Pts',(2.11677415599994,2.2,-3.41391840100002));
#356261=CARTESIAN_POINT('Ctrl Pts',(2.11653430599994,12.2,-3.41341946400001));
#356262=CARTESIAN_POINT('Ctrl Pts',(2.11653430599994,5.2,-3.41341946400001));
#356263=CARTESIAN_POINT('Ctrl Pts',(2.11653430599994,2.2,-3.41341946400001));
#356264=CARTESIAN_POINT('Ctrl Pts',(2.11629654699994,12.2,-3.41292650800002));
#356265=CARTESIAN_POINT('Ctrl Pts',(2.11629654699994,5.2,-3.41292650800002));
#356266=CARTESIAN_POINT('Ctrl Pts',(2.11629654699994,2.2,-3.41292650800002));
#356267=CARTESIAN_POINT('Ctrl Pts',(2.11606089999994,12.2,-3.41243954100001));
#356268=CARTESIAN_POINT('Ctrl Pts',(2.11606089999994,5.2,-3.41243954100001));
#356269=CARTESIAN_POINT('Ctrl Pts',(2.11606089999994,2.2,-3.41243954100001));
#356270=CARTESIAN_POINT('Ctrl Pts',(2.11582738399994,12.2,-3.41195856600002));
#356271=CARTESIAN_POINT('Ctrl Pts',(2.11582738399994,5.2,-3.41195856600002));
#356272=CARTESIAN_POINT('Ctrl Pts',(2.11582738399994,2.2,-3.41195856600002));
#356273=CARTESIAN_POINT('Ctrl Pts',(2.11559601999994,12.2,-3.41148358900002));
#356274=CARTESIAN_POINT('Ctrl Pts',(2.11559601999994,5.2,-3.41148358900002));
#356275=CARTESIAN_POINT('Ctrl Pts',(2.11559601999994,2.2,-3.41148358900002));
#356276=CARTESIAN_POINT('Ctrl Pts',(2.11536682799994,12.2,-3.41101461600001));
#356277=CARTESIAN_POINT('Ctrl Pts',(2.11536682799994,5.2,-3.41101461600001));
#356278=CARTESIAN_POINT('Ctrl Pts',(2.11536682799994,2.2,-3.41101461600001));
#356279=CARTESIAN_POINT('Ctrl Pts',(2.11513982899994,12.2,-3.41055165000002));
#356280=CARTESIAN_POINT('Ctrl Pts',(2.11513982899994,5.2,-3.41055165000002));
#356281=CARTESIAN_POINT('Ctrl Pts',(2.11513982899994,2.2,-3.41055165000002));
#356282=CARTESIAN_POINT('Ctrl Pts',(2.11491504099994,12.2,-3.41009469700001));
#356283=CARTESIAN_POINT('Ctrl Pts',(2.11491504099994,5.2,-3.41009469700001));
#356284=CARTESIAN_POINT('Ctrl Pts',(2.11491504099994,2.2,-3.41009469700001));
#356285=CARTESIAN_POINT('Ctrl Pts',(2.11469248799994,12.2,-3.40964376300001));
#356286=CARTESIAN_POINT('Ctrl Pts',(2.11469248799994,5.2,-3.40964376300001));
#356287=CARTESIAN_POINT('Ctrl Pts',(2.11469248799994,2.2,-3.40964376300001));
#356288=CARTESIAN_POINT('Ctrl Pts',(2.11447218799994,12.2,-3.40919885100002));
#356289=CARTESIAN_POINT('Ctrl Pts',(2.11447218799994,5.2,-3.40919885100002));
#356290=CARTESIAN_POINT('Ctrl Pts',(2.11447218799994,2.2,-3.40919885100002));
#356291=CARTESIAN_POINT('Ctrl Pts',(2.11425416099994,12.2,-3.40875996800001));
#356292=CARTESIAN_POINT('Ctrl Pts',(2.11425416099994,5.2,-3.40875996800001));
#356293=CARTESIAN_POINT('Ctrl Pts',(2.11425416099994,2.2,-3.40875996800001));
#356294=CARTESIAN_POINT('Ctrl Pts',(2.11403842999994,12.2,-3.40832711800001));
#356295=CARTESIAN_POINT('Ctrl Pts',(2.11403842999994,5.2,-3.40832711800001));
#356296=CARTESIAN_POINT('Ctrl Pts',(2.11403842999994,2.2,-3.40832711800001));
#356297=CARTESIAN_POINT('Ctrl Pts',(2.11382501399994,12.2,-3.40790030600001));
#356298=CARTESIAN_POINT('Ctrl Pts',(2.11382501399994,5.2,-3.40790030600001));
#356299=CARTESIAN_POINT('Ctrl Pts',(2.11382501399994,2.2,-3.40790030600001));
#356300=CARTESIAN_POINT('Ctrl Pts',(2.11361393499994,12.2,-3.40747953700001));
#356301=CARTESIAN_POINT('Ctrl Pts',(2.11361393499994,5.2,-3.40747953700001));
#356302=CARTESIAN_POINT('Ctrl Pts',(2.11361393499994,2.2,-3.40747953700001));
#356303=CARTESIAN_POINT('Ctrl Pts',(2.11340521199994,12.2,-3.40706481700002));
#356304=CARTESIAN_POINT('Ctrl Pts',(2.11340521199994,5.2,-3.40706481700002));
#356305=CARTESIAN_POINT('Ctrl Pts',(2.11340521199994,2.2,-3.40706481700002));
#356306=CARTESIAN_POINT('Ctrl Pts',(2.11319886699994,12.2,-3.40665614900002));
#356307=CARTESIAN_POINT('Ctrl Pts',(2.11319886699994,5.2,-3.40665614900002));
#356308=CARTESIAN_POINT('Ctrl Pts',(2.11319886699994,2.2,-3.40665614900002));
#356309=CARTESIAN_POINT('Ctrl Pts',(2.11299492199994,12.2,-3.40625353900001));
#356310=CARTESIAN_POINT('Ctrl Pts',(2.11299492199994,5.2,-3.40625353900001));
#356311=CARTESIAN_POINT('Ctrl Pts',(2.11299492199994,2.2,-3.40625353900001));
#356312=CARTESIAN_POINT('Ctrl Pts',(2.11279339699994,12.2,-3.40585699300001));
#356313=CARTESIAN_POINT('Ctrl Pts',(2.11279339699994,5.2,-3.40585699300001));
#356314=CARTESIAN_POINT('Ctrl Pts',(2.11279339699994,2.2,-3.40585699300001));
#356315=CARTESIAN_POINT('Ctrl Pts',(2.11259431199994,12.2,-3.40546651500001));
#356316=CARTESIAN_POINT('Ctrl Pts',(2.11259431199994,5.2,-3.40546651500001));
#356317=CARTESIAN_POINT('Ctrl Pts',(2.11259431199994,2.2,-3.40546651500001));
#356318=CARTESIAN_POINT('Ctrl Pts',(2.11239769099994,12.2,-3.40508211000001));
#356319=CARTESIAN_POINT('Ctrl Pts',(2.11239769099994,5.2,-3.40508211000001));
#356320=CARTESIAN_POINT('Ctrl Pts',(2.11239769099994,2.2,-3.40508211000001));
#356321=CARTESIAN_POINT('Ctrl Pts',(2.11220355199994,12.2,-3.40470378200001));
#356322=CARTESIAN_POINT('Ctrl Pts',(2.11220355199994,5.2,-3.40470378200001));
#356323=CARTESIAN_POINT('Ctrl Pts',(2.11220355199994,2.2,-3.40470378200001));
#356324=CARTESIAN_POINT('Ctrl Pts',(2.11201191899994,12.2,-3.40433153700001));
#356325=CARTESIAN_POINT('Ctrl Pts',(2.11201191899994,5.2,-3.40433153700001));
#356326=CARTESIAN_POINT('Ctrl Pts',(2.11201191899994,2.2,-3.40433153700001));
#356327=CARTESIAN_POINT('Ctrl Pts',(2.11182281299994,12.2,-3.40396538000002));
#356328=CARTESIAN_POINT('Ctrl Pts',(2.11182281299994,5.2,-3.40396538000002));
#356329=CARTESIAN_POINT('Ctrl Pts',(2.11182281299994,2.2,-3.40396538000002));
#356330=CARTESIAN_POINT('Ctrl Pts',(2.11163625399994,12.2,-3.40360531600002));
#356331=CARTESIAN_POINT('Ctrl Pts',(2.11163625399994,5.2,-3.40360531600002));
#356332=CARTESIAN_POINT('Ctrl Pts',(2.11163625399994,2.2,-3.40360531600002));
#356333=CARTESIAN_POINT('Ctrl Pts',(2.11145226499994,12.2,-3.40325134900001));
#356334=CARTESIAN_POINT('Ctrl Pts',(2.11145226499994,5.2,-3.40325134900001));
#356335=CARTESIAN_POINT('Ctrl Pts',(2.11145226499994,2.2,-3.40325134900001));
#356336=CARTESIAN_POINT('Ctrl Pts',(2.11127086799995,12.2,-3.40290348400002));
#356337=CARTESIAN_POINT('Ctrl Pts',(2.11127086799995,5.2,-3.40290348400002));
#356338=CARTESIAN_POINT('Ctrl Pts',(2.11127086799995,2.2,-3.40290348400002));
#356339=CARTESIAN_POINT('Ctrl Pts',(2.11109208399994,12.2,-3.40256172700002));
#356340=CARTESIAN_POINT('Ctrl Pts',(2.11109208399994,5.2,-3.40256172700002));
#356341=CARTESIAN_POINT('Ctrl Pts',(2.11109208399994,2.2,-3.40256172700002));
#356342=CARTESIAN_POINT('Ctrl Pts',(2.11091593499994,12.2,-3.40222608100001));
#356343=CARTESIAN_POINT('Ctrl Pts',(2.11091593499994,5.2,-3.40222608100001));
#356344=CARTESIAN_POINT('Ctrl Pts',(2.11091593499994,2.2,-3.40222608100001));
#356345=CARTESIAN_POINT('Ctrl Pts',(2.11074244199994,12.2,-3.40189655400001));
#356346=CARTESIAN_POINT('Ctrl Pts',(2.11074244199994,5.2,-3.40189655400001));
#356347=CARTESIAN_POINT('Ctrl Pts',(2.11074244199994,2.2,-3.40189655400001));
#356348=CARTESIAN_POINT('Ctrl Pts',(2.11057162799994,12.2,-3.40157314800001));
#356349=CARTESIAN_POINT('Ctrl Pts',(2.11057162799994,5.2,-3.40157314800001));
#356350=CARTESIAN_POINT('Ctrl Pts',(2.11057162799994,2.2,-3.40157314800001));
#356351=CARTESIAN_POINT('Ctrl Pts',(2.11040351499994,12.2,-3.40125586800001));
#356352=CARTESIAN_POINT('Ctrl Pts',(2.11040351499994,5.2,-3.40125586800001));
#356353=CARTESIAN_POINT('Ctrl Pts',(2.11040351499994,2.2,-3.40125586800001));
#356354=CARTESIAN_POINT('Ctrl Pts',(2.11023812499994,12.2,-3.40094472100001));
#356355=CARTESIAN_POINT('Ctrl Pts',(2.11023812499994,5.2,-3.40094472100001));
#356356=CARTESIAN_POINT('Ctrl Pts',(2.11023812499994,2.2,-3.40094472100001));
#356357=CARTESIAN_POINT('Ctrl Pts',(2.11007547899994,12.2,-3.40063970900002));
#356358=CARTESIAN_POINT('Ctrl Pts',(2.11007547899994,5.2,-3.40063970900002));
#356359=CARTESIAN_POINT('Ctrl Pts',(2.11007547899994,2.2,-3.40063970900002));
#356360=CARTESIAN_POINT('Ctrl Pts',(2.10991560099994,12.2,-3.40034083900001));
#356361=CARTESIAN_POINT('Ctrl Pts',(2.10991560099994,5.2,-3.40034083900001));
#356362=CARTESIAN_POINT('Ctrl Pts',(2.10991560099994,2.2,-3.40034083900001));
#356363=CARTESIAN_POINT('Ctrl Pts',(2.10975851299994,12.2,-3.40004811500001));
#356364=CARTESIAN_POINT('Ctrl Pts',(2.10975851299994,5.2,-3.40004811500001));
#356365=CARTESIAN_POINT('Ctrl Pts',(2.10975851299994,2.2,-3.40004811500001));
#356366=CARTESIAN_POINT('Ctrl Pts',(2.10960423699994,12.2,-3.39976154100002));
#356367=CARTESIAN_POINT('Ctrl Pts',(2.10960423699994,5.2,-3.39976154100002));
#356368=CARTESIAN_POINT('Ctrl Pts',(2.10960423699994,2.2,-3.39976154100002));
#356369=CARTESIAN_POINT('Ctrl Pts',(2.10945279699994,12.2,-3.39948112300001));
#356370=CARTESIAN_POINT('Ctrl Pts',(2.10945279699994,5.2,-3.39948112300001));
#356371=CARTESIAN_POINT('Ctrl Pts',(2.10945279699994,2.2,-3.39948112300001));
#356372=CARTESIAN_POINT('Ctrl Pts',(2.10930421299994,12.2,-3.39920686600002));
#356373=CARTESIAN_POINT('Ctrl Pts',(2.10930421299994,5.2,-3.39920686600002));
#356374=CARTESIAN_POINT('Ctrl Pts',(2.10930421299994,2.2,-3.39920686600002));
#356375=CARTESIAN_POINT('Ctrl Pts',(2.10915850899994,12.2,-3.39893877300002));
#356376=CARTESIAN_POINT('Ctrl Pts',(2.10915850899994,5.2,-3.39893877300002));
#356377=CARTESIAN_POINT('Ctrl Pts',(2.10915850899994,2.2,-3.39893877300002));
#356378=CARTESIAN_POINT('Ctrl Pts',(2.10901570899994,12.2,-3.39867685100002));
#356379=CARTESIAN_POINT('Ctrl Pts',(2.10901570899994,5.2,-3.39867685100002));
#356380=CARTESIAN_POINT('Ctrl Pts',(2.10901570899994,2.2,-3.39867685100002));
#356381=CARTESIAN_POINT('Ctrl Pts',(2.10887583399994,12.2,-3.39842110400001));
#356382=CARTESIAN_POINT('Ctrl Pts',(2.10887583399994,5.2,-3.39842110400001));
#356383=CARTESIAN_POINT('Ctrl Pts',(2.10887583399994,2.2,-3.39842110400001));
#356384=CARTESIAN_POINT('Ctrl Pts',(2.10873890799994,12.2,-3.39817153600002));
#356385=CARTESIAN_POINT('Ctrl Pts',(2.10873890799994,5.2,-3.39817153600002));
#356386=CARTESIAN_POINT('Ctrl Pts',(2.10873890799994,2.2,-3.39817153600002));
#356387=CARTESIAN_POINT('Ctrl Pts',(2.10860495299994,12.2,-3.39792815200001));
#356388=CARTESIAN_POINT('Ctrl Pts',(2.10860495299994,5.2,-3.39792815200001));
#356389=CARTESIAN_POINT('Ctrl Pts',(2.10860495299994,2.2,-3.39792815200001));
#356390=CARTESIAN_POINT('Ctrl Pts',(2.10847399199994,12.2,-3.39769095600001));
#356391=CARTESIAN_POINT('Ctrl Pts',(2.10847399199994,5.2,-3.39769095600001));
#356392=CARTESIAN_POINT('Ctrl Pts',(2.10847399199994,2.2,-3.39769095600001));
#356393=CARTESIAN_POINT('Ctrl Pts',(2.10834605099994,12.2,-3.39745995500001));
#356394=CARTESIAN_POINT('Ctrl Pts',(2.10834605099994,5.2,-3.39745995500001));
#356395=CARTESIAN_POINT('Ctrl Pts',(2.10834605099994,2.2,-3.39745995500001));
#356396=CARTESIAN_POINT('Ctrl Pts',(2.10822115099994,12.2,-3.39723515100002));
#356397=CARTESIAN_POINT('Ctrl Pts',(2.10822115099994,5.2,-3.39723515100002));
#356398=CARTESIAN_POINT('Ctrl Pts',(2.10822115099994,2.2,-3.39723515100002));
#356399=CARTESIAN_POINT('Ctrl Pts',(2.10809931399994,12.2,-3.39701655100002));
#356400=CARTESIAN_POINT('Ctrl Pts',(2.10809931399994,5.2,-3.39701655100002));
#356401=CARTESIAN_POINT('Ctrl Pts',(2.10809931399994,2.2,-3.39701655100002));
#356402=CARTESIAN_POINT('Ctrl Pts',(2.10798056699994,12.2,-3.39680415900002));
#356403=CARTESIAN_POINT('Ctrl Pts',(2.10798056699994,5.2,-3.39680415900002));
#356404=CARTESIAN_POINT('Ctrl Pts',(2.10798056699994,2.2,-3.39680415900002));
#356405=CARTESIAN_POINT('Ctrl Pts',(2.10786493099994,12.2,-3.39659797800001));
#356406=CARTESIAN_POINT('Ctrl Pts',(2.10786493099994,5.2,-3.39659797800001));
#356407=CARTESIAN_POINT('Ctrl Pts',(2.10786493099994,2.2,-3.39659797800001));
#356408=CARTESIAN_POINT('Ctrl Pts',(2.10775242999994,12.2,-3.39639801400001));
#356409=CARTESIAN_POINT('Ctrl Pts',(2.10775242999994,5.2,-3.39639801400001));
#356410=CARTESIAN_POINT('Ctrl Pts',(2.10775242999994,2.2,-3.39639801400001));
#356411=CARTESIAN_POINT('Ctrl Pts',(2.10764308699994,12.2,-3.39620427400002));
#356412=CARTESIAN_POINT('Ctrl Pts',(2.10764308699994,5.2,-3.39620427400002));
#356413=CARTESIAN_POINT('Ctrl Pts',(2.10764308699994,2.2,-3.39620427400002));
#356414=CARTESIAN_POINT('Ctrl Pts',(2.10753692699994,12.2,-3.39601675800001));
#356415=CARTESIAN_POINT('Ctrl Pts',(2.10753692699994,5.2,-3.39601675800001));
#356416=CARTESIAN_POINT('Ctrl Pts',(2.10753692699994,2.2,-3.39601675800001));
#356417=CARTESIAN_POINT('Ctrl Pts',(2.10743397399995,12.2,-3.39583547300002));
#356418=CARTESIAN_POINT('Ctrl Pts',(2.10743397399995,5.2,-3.39583547300002));
#356419=CARTESIAN_POINT('Ctrl Pts',(2.10743397399995,2.2,-3.39583547300002));
#356420=CARTESIAN_POINT('Ctrl Pts',(2.10733425199995,12.2,-3.39566042500001));
#356421=CARTESIAN_POINT('Ctrl Pts',(2.10733425199995,5.2,-3.39566042500001));
#356422=CARTESIAN_POINT('Ctrl Pts',(2.10733425199995,2.2,-3.39566042500001));
#356423=CARTESIAN_POINT('Ctrl Pts',(2.10723778599994,12.2,-3.39549161700001));
#356424=CARTESIAN_POINT('Ctrl Pts',(2.10723778599994,5.2,-3.39549161700001));
#356425=CARTESIAN_POINT('Ctrl Pts',(2.10723778599994,2.2,-3.39549161700001));
#356426=CARTESIAN_POINT('Ctrl Pts',(2.10714459799994,12.2,-3.39532905300001));
#356427=CARTESIAN_POINT('Ctrl Pts',(2.10714459799994,5.2,-3.39532905300001));
#356428=CARTESIAN_POINT('Ctrl Pts',(2.10714459799994,2.2,-3.39532905300001));
#356429=CARTESIAN_POINT('Ctrl Pts',(2.10705471299994,12.2,-3.39517273800002));
#356430=CARTESIAN_POINT('Ctrl Pts',(2.10705471299994,5.2,-3.39517273800002));
#356431=CARTESIAN_POINT('Ctrl Pts',(2.10705471299994,2.2,-3.39517273800002));
#356432=CARTESIAN_POINT('Ctrl Pts',(2.10696815599994,12.2,-3.39502267900002));
#356433=CARTESIAN_POINT('Ctrl Pts',(2.10696815599994,5.2,-3.39502267900002));
#356434=CARTESIAN_POINT('Ctrl Pts',(2.10696815599994,2.2,-3.39502267900002));
#356435=CARTESIAN_POINT('Ctrl Pts',(2.10688494999994,12.2,-3.39487887700002));
#356436=CARTESIAN_POINT('Ctrl Pts',(2.10688494999994,5.2,-3.39487887700002));
#356437=CARTESIAN_POINT('Ctrl Pts',(2.10688494999994,2.2,-3.39487887700002));
#356438=CARTESIAN_POINT('Ctrl Pts',(2.10680511899994,12.2,-3.39474133800001));
#356439=CARTESIAN_POINT('Ctrl Pts',(2.10680511899994,5.2,-3.39474133800001));
#356440=CARTESIAN_POINT('Ctrl Pts',(2.10680511899994,2.2,-3.39474133800001));
#356441=CARTESIAN_POINT('Ctrl Pts',(2.10672868799994,12.2,-3.39461006600001));
#356442=CARTESIAN_POINT('Ctrl Pts',(2.10672868799994,5.2,-3.39461006600001));
#356443=CARTESIAN_POINT('Ctrl Pts',(2.10672868799994,2.2,-3.39461006600001));
#356444=CARTESIAN_POINT('Ctrl Pts',(2.10665568499994,12.2,-3.39448506800001));
#356445=CARTESIAN_POINT('Ctrl Pts',(2.10665568499994,5.2,-3.39448506800001));
#356446=CARTESIAN_POINT('Ctrl Pts',(2.10665568499994,2.2,-3.39448506800001));
#356447=CARTESIAN_POINT('Ctrl Pts',(2.10658613299994,12.2,-3.39436634600002));
#356448=CARTESIAN_POINT('Ctrl Pts',(2.10658613299994,5.2,-3.39436634600002));
#356449=CARTESIAN_POINT('Ctrl Pts',(2.10658613299994,2.2,-3.39436634600002));
#356450=CARTESIAN_POINT('Ctrl Pts',(2.10652005899994,12.2,-3.39425390500002));
#356451=CARTESIAN_POINT('Ctrl Pts',(2.10652005899994,5.2,-3.39425390500002));
#356452=CARTESIAN_POINT('Ctrl Pts',(2.10652005899994,2.2,-3.39425390500002));
#356453=CARTESIAN_POINT('Ctrl Pts',(2.10645748799994,12.2,-3.39414775200002));
#356454=CARTESIAN_POINT('Ctrl Pts',(2.10645748799994,5.2,-3.39414775200002));
#356455=CARTESIAN_POINT('Ctrl Pts',(2.10645748799994,2.2,-3.39414775200002));
#356456=CARTESIAN_POINT('Ctrl Pts',(2.10639844199994,12.2,-3.39404788800001));
#356457=CARTESIAN_POINT('Ctrl Pts',(2.10639844199994,5.2,-3.39404788800001));
#356458=CARTESIAN_POINT('Ctrl Pts',(2.10639844199994,2.2,-3.39404788800001));
#356459=CARTESIAN_POINT('Ctrl Pts',(2.10634294299994,12.2,-3.39395431800002));
#356460=CARTESIAN_POINT('Ctrl Pts',(2.10634294299994,5.2,-3.39395431800002));
#356461=CARTESIAN_POINT('Ctrl Pts',(2.10634294299994,2.2,-3.39395431800002));
#356462=CARTESIAN_POINT('Ctrl Pts',(2.10629101599995,12.2,-3.39386704700001));
#356463=CARTESIAN_POINT('Ctrl Pts',(2.10629101599995,5.2,-3.39386704700001));
#356464=CARTESIAN_POINT('Ctrl Pts',(2.10629101599995,2.2,-3.39386704700001));
#356465=CARTESIAN_POINT('Ctrl Pts',(2.10624268299994,12.2,-3.39378607900001));
#356466=CARTESIAN_POINT('Ctrl Pts',(2.10624268299994,5.2,-3.39378607900001));
#356467=CARTESIAN_POINT('Ctrl Pts',(2.10624268299994,2.2,-3.39378607900001));
#356468=CARTESIAN_POINT('Ctrl Pts',(2.10619797799994,12.2,-3.39371141900001));
#356469=CARTESIAN_POINT('Ctrl Pts',(2.10619797799994,5.2,-3.39371141900001));
#356470=CARTESIAN_POINT('Ctrl Pts',(2.10619797799994,2.2,-3.39371141900001));
#356471=CARTESIAN_POINT('Ctrl Pts',(2.10615692999994,12.2,-3.39364307200002));
#356472=CARTESIAN_POINT('Ctrl Pts',(2.10615692999994,5.2,-3.39364307200002));
#356473=CARTESIAN_POINT('Ctrl Pts',(2.10615692999994,2.2,-3.39364307200002));
#356474=CARTESIAN_POINT('Ctrl Pts',(2.10611957199994,12.2,-3.39358104500001));
#356475=CARTESIAN_POINT('Ctrl Pts',(2.10611957199994,5.2,-3.39358104500001));
#356476=CARTESIAN_POINT('Ctrl Pts',(2.10611957199994,2.2,-3.39358104500001));
#356477=CARTESIAN_POINT('Ctrl Pts',(2.10608593399995,12.2,-3.39352534100001));
#356478=CARTESIAN_POINT('Ctrl Pts',(2.10608593399995,5.2,-3.39352534100001));
#356479=CARTESIAN_POINT('Ctrl Pts',(2.10608593399995,2.2,-3.39352534100001));
#356480=CARTESIAN_POINT('Ctrl Pts',(2.10605603399994,12.2,-3.39347596500001));
#356481=CARTESIAN_POINT('Ctrl Pts',(2.10605603399994,5.2,-3.39347596500001));
#356482=CARTESIAN_POINT('Ctrl Pts',(2.10605603399994,2.2,-3.39347596500001));
#356483=CARTESIAN_POINT('Ctrl Pts',(2.10602708695768,12.2,-3.3934283110922));
#356484=CARTESIAN_POINT('Ctrl Pts',(2.10602708695768,5.2,-3.3934283110922));
#356485=CARTESIAN_POINT('Ctrl Pts',(2.10602708695768,2.2,-3.3934283110922));
#356486=CARTESIAN_POINT('Ctrl Pts',(2.106007235588,12.2,-3.39339577600012));
#356487=CARTESIAN_POINT('Ctrl Pts',(2.106007235588,5.2,-3.39339577600012));
#356488=CARTESIAN_POINT('Ctrl Pts',(2.106007235588,2.2,-3.39339577600012));
#356489=CARTESIAN_POINT('Ctrl Pts',(2.10599411145374,12.2,-3.3933743724075));
#356490=CARTESIAN_POINT('Ctrl Pts',(2.10599411145374,5.2,-3.3933743724075));
#356491=CARTESIAN_POINT('Ctrl Pts',(2.10599411145374,2.2,-3.3933743724075));
#356492=CARTESIAN_POINT('Ctrl Pts',(2.10598590620568,12.2,-3.39336105859039));
#356493=CARTESIAN_POINT('Ctrl Pts',(2.10598590620568,5.2,-3.39336105859039));
#356494=CARTESIAN_POINT('Ctrl Pts',(2.10598590620568,2.2,-3.39336105859039));
#356495=CARTESIAN_POINT('Ctrl Pts',(2.10598084399995,12.2,-3.39335283300001));
#356496=CARTESIAN_POINT('Ctrl Pts',(2.10598084399995,5.2,-3.39335283300001));
#356497=CARTESIAN_POINT('Ctrl Pts',(2.10598084399995,2.2,-3.39335283300001));
#356498=CARTESIAN_POINT('',(2.20867500599994,12.2,-4.20526511800002));
#356499=CARTESIAN_POINT('Origin',(-5.66300478732629E-14,15.2,-1.77635683940025E-14));
#356500=CARTESIAN_POINT('',(1.90498031899994,12.2,-4.35126992700001));
#356501=CARTESIAN_POINT('Ctrl Pts',(1.33499940099994,12.2,-3.76399239200001));
#356502=CARTESIAN_POINT('Ctrl Pts',(1.33499940099994,5.2,-3.76399239200001));
#356503=CARTESIAN_POINT('Ctrl Pts',(1.33499940099994,2.2,-3.76399239200001));
#356504=CARTESIAN_POINT('Ctrl Pts',(1.3350017138634,12.2,-3.76399883261967));
#356505=CARTESIAN_POINT('Ctrl Pts',(1.3350017138634,5.2,-3.76399883261967));
#356506=CARTESIAN_POINT('Ctrl Pts',(1.3350017138634,2.2,-3.76399883261967));
#356507=CARTESIAN_POINT('Ctrl Pts',(1.33500618571269,12.2,-3.76401128880897));
#356508=CARTESIAN_POINT('Ctrl Pts',(1.33500618571269,5.2,-3.76401128880897));
#356509=CARTESIAN_POINT('Ctrl Pts',(1.33500618571269,2.2,-3.76401128880897));
#356510=CARTESIAN_POINT('Ctrl Pts',(1.33501281737833,12.2,-3.76402975554743));
#356511=CARTESIAN_POINT('Ctrl Pts',(1.33501281737833,5.2,-3.76402975554743));
#356512=CARTESIAN_POINT('Ctrl Pts',(1.33501281737833,2.2,-3.76402975554743));
#356513=CARTESIAN_POINT('Ctrl Pts',(1.33502160885941,12.2,-3.76405426785898));
#356514=CARTESIAN_POINT('Ctrl Pts',(1.33502160885941,5.2,-3.76405426785898));
#356515=CARTESIAN_POINT('Ctrl Pts',(1.33502160885941,2.2,-3.76405426785898));
#356516=CARTESIAN_POINT('Ctrl Pts',(1.33503710099994,12.2,-3.76409681100002));
#356517=CARTESIAN_POINT('Ctrl Pts',(1.33503710099994,5.2,-3.76409681100002));
#356518=CARTESIAN_POINT('Ctrl Pts',(1.33503710099994,2.2,-3.76409681100002));
#356519=CARTESIAN_POINT('Ctrl Pts',(1.33505439099994,12.2,-3.76414411500001));
#356520=CARTESIAN_POINT('Ctrl Pts',(1.33505439099994,5.2,-3.76414411500001));
#356521=CARTESIAN_POINT('Ctrl Pts',(1.33505439099994,2.2,-3.76414411500001));
#356522=CARTESIAN_POINT('Ctrl Pts',(1.33507428099994,12.2,-3.76419830300001));
#356523=CARTESIAN_POINT('Ctrl Pts',(1.33507428099994,5.2,-3.76419830300001));
#356524=CARTESIAN_POINT('Ctrl Pts',(1.33507428099994,2.2,-3.76419830300001));
#356525=CARTESIAN_POINT('Ctrl Pts',(1.33509677799994,12.2,-3.76425936300001));
#356526=CARTESIAN_POINT('Ctrl Pts',(1.33509677799994,5.2,-3.76425936300001));
#356527=CARTESIAN_POINT('Ctrl Pts',(1.33509677799994,2.2,-3.76425936300001));
#356528=CARTESIAN_POINT('Ctrl Pts',(1.33512189099994,12.2,-3.76432727700001));
#356529=CARTESIAN_POINT('Ctrl Pts',(1.33512189099994,5.2,-3.76432727700001));
#356530=CARTESIAN_POINT('Ctrl Pts',(1.33512189099994,2.2,-3.76432727700001));
#356531=CARTESIAN_POINT('Ctrl Pts',(1.33514963499994,12.2,-3.76440201900001));
#356532=CARTESIAN_POINT('Ctrl Pts',(1.33514963499994,5.2,-3.76440201900001));
#356533=CARTESIAN_POINT('Ctrl Pts',(1.33514963499994,2.2,-3.76440201900001));
#356534=CARTESIAN_POINT('Ctrl Pts',(1.33518002599994,12.2,-3.76448356300001));
#356535=CARTESIAN_POINT('Ctrl Pts',(1.33518002599994,5.2,-3.76448356300001));
#356536=CARTESIAN_POINT('Ctrl Pts',(1.33518002599994,2.2,-3.76448356300001));
#356537=CARTESIAN_POINT('Ctrl Pts',(1.33521307799994,12.2,-3.76457187700002));
#356538=CARTESIAN_POINT('Ctrl Pts',(1.33521307799994,5.2,-3.76457187700002));
#356539=CARTESIAN_POINT('Ctrl Pts',(1.33521307799994,2.2,-3.76457187700002));
#356540=CARTESIAN_POINT('Ctrl Pts',(1.33524880699994,12.2,-3.76466693600001));
#356541=CARTESIAN_POINT('Ctrl Pts',(1.33524880699994,5.2,-3.76466693600001));
#356542=CARTESIAN_POINT('Ctrl Pts',(1.33524880699994,2.2,-3.76466693600001));
#356543=CARTESIAN_POINT('Ctrl Pts',(1.33528722599994,12.2,-3.76476871700001));
#356544=CARTESIAN_POINT('Ctrl Pts',(1.33528722599994,5.2,-3.76476871700001));
#356545=CARTESIAN_POINT('Ctrl Pts',(1.33528722599994,2.2,-3.76476871700001));
#356546=CARTESIAN_POINT('Ctrl Pts',(1.33532834499994,12.2,-3.76487719900001));
#356547=CARTESIAN_POINT('Ctrl Pts',(1.33532834499994,5.2,-3.76487719900001));
#356548=CARTESIAN_POINT('Ctrl Pts',(1.33532834499994,2.2,-3.76487719900001));
#356549=CARTESIAN_POINT('Ctrl Pts',(1.33537217499994,12.2,-3.76499236300001));
#356550=CARTESIAN_POINT('Ctrl Pts',(1.33537217499994,5.2,-3.76499236300001));
#356551=CARTESIAN_POINT('Ctrl Pts',(1.33537217499994,2.2,-3.76499236300001));
#356552=CARTESIAN_POINT('Ctrl Pts',(1.33541872699994,12.2,-3.76511418800002));
#356553=CARTESIAN_POINT('Ctrl Pts',(1.33541872699994,5.2,-3.76511418800002));
#356554=CARTESIAN_POINT('Ctrl Pts',(1.33541872699994,2.2,-3.76511418800002));
#356555=CARTESIAN_POINT('Ctrl Pts',(1.33546801399994,12.2,-3.76524265300001));
#356556=CARTESIAN_POINT('Ctrl Pts',(1.33546801399994,5.2,-3.76524265300001));
#356557=CARTESIAN_POINT('Ctrl Pts',(1.33546801399994,2.2,-3.76524265300001));
#356558=CARTESIAN_POINT('Ctrl Pts',(1.33552004599994,12.2,-3.76537773400001));
#356559=CARTESIAN_POINT('Ctrl Pts',(1.33552004599994,5.2,-3.76537773400001));
#356560=CARTESIAN_POINT('Ctrl Pts',(1.33552004599994,2.2,-3.76537773400001));
#356561=CARTESIAN_POINT('Ctrl Pts',(1.33557483799994,12.2,-3.76551940800002));
#356562=CARTESIAN_POINT('Ctrl Pts',(1.33557483799994,5.2,-3.76551940800002));
#356563=CARTESIAN_POINT('Ctrl Pts',(1.33557483799994,2.2,-3.76551940800002));
#356564=CARTESIAN_POINT('Ctrl Pts',(1.33563239999994,12.2,-3.76566765300002));
#356565=CARTESIAN_POINT('Ctrl Pts',(1.33563239999994,5.2,-3.76566765300002));
#356566=CARTESIAN_POINT('Ctrl Pts',(1.33563239999994,2.2,-3.76566765300002));
#356567=CARTESIAN_POINT('Ctrl Pts',(1.33569274599994,12.2,-3.76582244500002));
#356568=CARTESIAN_POINT('Ctrl Pts',(1.33569274599994,5.2,-3.76582244500002));
#356569=CARTESIAN_POINT('Ctrl Pts',(1.33569274599994,2.2,-3.76582244500002));
#356570=CARTESIAN_POINT('Ctrl Pts',(1.33575588799994,12.2,-3.76598376200001));
#356571=CARTESIAN_POINT('Ctrl Pts',(1.33575588799994,5.2,-3.76598376200001));
#356572=CARTESIAN_POINT('Ctrl Pts',(1.33575588799994,2.2,-3.76598376200001));
#356573=CARTESIAN_POINT('Ctrl Pts',(1.33582183599994,12.2,-3.76615158500002));
#356574=CARTESIAN_POINT('Ctrl Pts',(1.33582183599994,5.2,-3.76615158500002));
#356575=CARTESIAN_POINT('Ctrl Pts',(1.33582183599994,2.2,-3.76615158500002));
#356576=CARTESIAN_POINT('Ctrl Pts',(1.33589060099994,12.2,-3.76632588900002));
#356577=CARTESIAN_POINT('Ctrl Pts',(1.33589060099994,5.2,-3.76632588900002));
#356578=CARTESIAN_POINT('Ctrl Pts',(1.33589060099994,2.2,-3.76632588900002));
#356579=CARTESIAN_POINT('Ctrl Pts',(1.33596219699994,12.2,-3.76650665500001));
#356580=CARTESIAN_POINT('Ctrl Pts',(1.33596219699994,5.2,-3.76650665500001));
#356581=CARTESIAN_POINT('Ctrl Pts',(1.33596219699994,2.2,-3.76650665500001));
#356582=CARTESIAN_POINT('Ctrl Pts',(1.33603663199994,12.2,-3.76669386000001));
#356583=CARTESIAN_POINT('Ctrl Pts',(1.33603663199994,5.2,-3.76669386000001));
#356584=CARTESIAN_POINT('Ctrl Pts',(1.33603663199994,2.2,-3.76669386000001));
#356585=CARTESIAN_POINT('Ctrl Pts',(1.33611392099994,12.2,-3.76688748400001));
#356586=CARTESIAN_POINT('Ctrl Pts',(1.33611392099994,5.2,-3.76688748400001));
#356587=CARTESIAN_POINT('Ctrl Pts',(1.33611392099994,2.2,-3.76688748400001));
#356588=CARTESIAN_POINT('Ctrl Pts',(1.33619407199994,12.2,-3.76708750200001));
#356589=CARTESIAN_POINT('Ctrl Pts',(1.33619407199994,5.2,-3.76708750200001));
#356590=CARTESIAN_POINT('Ctrl Pts',(1.33619407199994,2.2,-3.76708750200001));
#356591=CARTESIAN_POINT('Ctrl Pts',(1.33627709999994,12.2,-3.76729389500001));
#356592=CARTESIAN_POINT('Ctrl Pts',(1.33627709999994,5.2,-3.76729389500001));
#356593=CARTESIAN_POINT('Ctrl Pts',(1.33627709999994,2.2,-3.76729389500001));
#356594=CARTESIAN_POINT('Ctrl Pts',(1.33636301299994,12.2,-3.76750664100001));
#356595=CARTESIAN_POINT('Ctrl Pts',(1.33636301299994,5.2,-3.76750664100001));
#356596=CARTESIAN_POINT('Ctrl Pts',(1.33636301299994,2.2,-3.76750664100001));
#356597=CARTESIAN_POINT('Ctrl Pts',(1.33645182399994,12.2,-3.76772571800001));
#356598=CARTESIAN_POINT('Ctrl Pts',(1.33645182399994,5.2,-3.76772571800001));
#356599=CARTESIAN_POINT('Ctrl Pts',(1.33645182399994,2.2,-3.76772571800001));
#356600=CARTESIAN_POINT('Ctrl Pts',(1.33654354399994,12.2,-3.76795110400002));
#356601=CARTESIAN_POINT('Ctrl Pts',(1.33654354399994,5.2,-3.76795110400002));
#356602=CARTESIAN_POINT('Ctrl Pts',(1.33654354399994,2.2,-3.76795110400002));
#356603=CARTESIAN_POINT('Ctrl Pts',(1.33663818299994,12.2,-3.76818277900002));
#356604=CARTESIAN_POINT('Ctrl Pts',(1.33663818299994,5.2,-3.76818277900002));
#356605=CARTESIAN_POINT('Ctrl Pts',(1.33663818299994,2.2,-3.76818277900002));
#356606=CARTESIAN_POINT('Ctrl Pts',(1.33673575299994,12.2,-3.76842072200001));
#356607=CARTESIAN_POINT('Ctrl Pts',(1.33673575299994,5.2,-3.76842072200001));
#356608=CARTESIAN_POINT('Ctrl Pts',(1.33673575299994,2.2,-3.76842072200001));
#356609=CARTESIAN_POINT('Ctrl Pts',(1.33683626499994,12.2,-3.76866491200001));
#356610=CARTESIAN_POINT('Ctrl Pts',(1.33683626499994,5.2,-3.76866491200001));
#356611=CARTESIAN_POINT('Ctrl Pts',(1.33683626499994,2.2,-3.76866491200001));
#356612=CARTESIAN_POINT('Ctrl Pts',(1.33693972899994,12.2,-3.76891532600002));
#356613=CARTESIAN_POINT('Ctrl Pts',(1.33693972899994,5.2,-3.76891532600002));
#356614=CARTESIAN_POINT('Ctrl Pts',(1.33693972899994,2.2,-3.76891532600002));
#356615=CARTESIAN_POINT('Ctrl Pts',(1.33704615599994,12.2,-3.76917194300002));
#356616=CARTESIAN_POINT('Ctrl Pts',(1.33704615599994,5.2,-3.76917194300002));
#356617=CARTESIAN_POINT('Ctrl Pts',(1.33704615599994,2.2,-3.76917194300002));
#356618=CARTESIAN_POINT('Ctrl Pts',(1.33715555799994,12.2,-3.76943474500001));
#356619=CARTESIAN_POINT('Ctrl Pts',(1.33715555799994,5.2,-3.76943474500001));
#356620=CARTESIAN_POINT('Ctrl Pts',(1.33715555799994,2.2,-3.76943474500001));
#356621=CARTESIAN_POINT('Ctrl Pts',(1.33726794299994,12.2,-3.76970370800001));
#356622=CARTESIAN_POINT('Ctrl Pts',(1.33726794299994,5.2,-3.76970370800001));
#356623=CARTESIAN_POINT('Ctrl Pts',(1.33726794299994,2.2,-3.76970370800001));
#356624=CARTESIAN_POINT('Ctrl Pts',(1.33738332499994,12.2,-3.76997881300001));
#356625=CARTESIAN_POINT('Ctrl Pts',(1.33738332499994,5.2,-3.76997881300001));
#356626=CARTESIAN_POINT('Ctrl Pts',(1.33738332499994,2.2,-3.76997881300001));
#356627=CARTESIAN_POINT('Ctrl Pts',(1.33750171199994,12.2,-3.77026003800002));
#356628=CARTESIAN_POINT('Ctrl Pts',(1.33750171199994,5.2,-3.77026003800002));
#356629=CARTESIAN_POINT('Ctrl Pts',(1.33750171199994,2.2,-3.77026003800002));
#356630=CARTESIAN_POINT('Ctrl Pts',(1.33762311599994,12.2,-3.77054736200002));
#356631=CARTESIAN_POINT('Ctrl Pts',(1.33762311599994,5.2,-3.77054736200002));
#356632=CARTESIAN_POINT('Ctrl Pts',(1.33762311599994,2.2,-3.77054736200002));
#356633=CARTESIAN_POINT('Ctrl Pts',(1.33774754599994,12.2,-3.77084076600001));
#356634=CARTESIAN_POINT('Ctrl Pts',(1.33774754599994,5.2,-3.77084076600001));
#356635=CARTESIAN_POINT('Ctrl Pts',(1.33774754599994,2.2,-3.77084076600001));
#356636=CARTESIAN_POINT('Ctrl Pts',(1.33787501399994,12.2,-3.77114022700002));
#356637=CARTESIAN_POINT('Ctrl Pts',(1.33787501399994,5.2,-3.77114022700002));
#356638=CARTESIAN_POINT('Ctrl Pts',(1.33787501399994,2.2,-3.77114022700002));
#356639=CARTESIAN_POINT('Ctrl Pts',(1.33800552899994,12.2,-3.77144572600002));
#356640=CARTESIAN_POINT('Ctrl Pts',(1.33800552899994,5.2,-3.77144572600002));
#356641=CARTESIAN_POINT('Ctrl Pts',(1.33800552899994,2.2,-3.77144572600002));
#356642=CARTESIAN_POINT('Ctrl Pts',(1.33813910099994,12.2,-3.77175724400002));
#356643=CARTESIAN_POINT('Ctrl Pts',(1.33813910099994,5.2,-3.77175724400002));
#356644=CARTESIAN_POINT('Ctrl Pts',(1.33813910099994,2.2,-3.77175724400002));
#356645=CARTESIAN_POINT('Ctrl Pts',(1.33827574299994,12.2,-3.77207475700001));
#356646=CARTESIAN_POINT('Ctrl Pts',(1.33827574299994,5.2,-3.77207475700001));
#356647=CARTESIAN_POINT('Ctrl Pts',(1.33827574299994,2.2,-3.77207475700001));
#356648=CARTESIAN_POINT('Ctrl Pts',(1.33841546199994,12.2,-3.77239824600001));
#356649=CARTESIAN_POINT('Ctrl Pts',(1.33841546199994,5.2,-3.77239824600001));
#356650=CARTESIAN_POINT('Ctrl Pts',(1.33841546199994,2.2,-3.77239824600001));
#356651=CARTESIAN_POINT('Ctrl Pts',(1.33855826899994,12.2,-3.77272769200002));
#356652=CARTESIAN_POINT('Ctrl Pts',(1.33855826899994,5.2,-3.77272769200002));
#356653=CARTESIAN_POINT('Ctrl Pts',(1.33855826899994,2.2,-3.77272769200002));
#356654=CARTESIAN_POINT('Ctrl Pts',(1.33870417499994,12.2,-3.77306307200001));
#356655=CARTESIAN_POINT('Ctrl Pts',(1.33870417499994,5.2,-3.77306307200001));
#356656=CARTESIAN_POINT('Ctrl Pts',(1.33870417499994,2.2,-3.77306307200001));
#356657=CARTESIAN_POINT('Ctrl Pts',(1.33885318899994,12.2,-3.77340436900001));
#356658=CARTESIAN_POINT('Ctrl Pts',(1.33885318899994,5.2,-3.77340436900001));
#356659=CARTESIAN_POINT('Ctrl Pts',(1.33885318899994,2.2,-3.77340436900001));
#356660=CARTESIAN_POINT('Ctrl Pts',(1.33900532099994,12.2,-3.77375156100001));
#356661=CARTESIAN_POINT('Ctrl Pts',(1.33900532099994,5.2,-3.77375156100001));
#356662=CARTESIAN_POINT('Ctrl Pts',(1.33900532099994,2.2,-3.77375156100001));
#356663=CARTESIAN_POINT('Ctrl Pts',(1.33916058199994,12.2,-3.77410462700002));
#356664=CARTESIAN_POINT('Ctrl Pts',(1.33916058199994,5.2,-3.77410462700002));
#356665=CARTESIAN_POINT('Ctrl Pts',(1.33916058199994,2.2,-3.77410462700002));
#356666=CARTESIAN_POINT('Ctrl Pts',(1.33931897899994,12.2,-3.77446354900002));
#356667=CARTESIAN_POINT('Ctrl Pts',(1.33931897899994,5.2,-3.77446354900002));
#356668=CARTESIAN_POINT('Ctrl Pts',(1.33931897899994,2.2,-3.77446354900002));
#356669=CARTESIAN_POINT('Ctrl Pts',(1.33948052599994,12.2,-3.77482830500002));
#356670=CARTESIAN_POINT('Ctrl Pts',(1.33948052599994,5.2,-3.77482830500002));
#356671=CARTESIAN_POINT('Ctrl Pts',(1.33948052599994,2.2,-3.77482830500002));
#356672=CARTESIAN_POINT('Ctrl Pts',(1.33964522999994,12.2,-3.77519887600001));
#356673=CARTESIAN_POINT('Ctrl Pts',(1.33964522999994,5.2,-3.77519887600001));
#356674=CARTESIAN_POINT('Ctrl Pts',(1.33964522999994,2.2,-3.77519887600001));
#356675=CARTESIAN_POINT('Ctrl Pts',(1.33981309999994,12.2,-3.77557524300002));
#356676=CARTESIAN_POINT('Ctrl Pts',(1.33981309999994,5.2,-3.77557524300002));
#356677=CARTESIAN_POINT('Ctrl Pts',(1.33981309999994,2.2,-3.77557524300002));
#356678=CARTESIAN_POINT('Ctrl Pts',(1.33998414699994,12.2,-3.77595738500001));
#356679=CARTESIAN_POINT('Ctrl Pts',(1.33998414699994,5.2,-3.77595738500001));
#356680=CARTESIAN_POINT('Ctrl Pts',(1.33998414699994,2.2,-3.77595738500001));
#356681=CARTESIAN_POINT('Ctrl Pts',(1.34015838099994,12.2,-3.77634528200002));
#356682=CARTESIAN_POINT('Ctrl Pts',(1.34015838099994,5.2,-3.77634528200002));
#356683=CARTESIAN_POINT('Ctrl Pts',(1.34015838099994,2.2,-3.77634528200002));
#356684=CARTESIAN_POINT('Ctrl Pts',(1.34033580999994,12.2,-3.77673891500002));
#356685=CARTESIAN_POINT('Ctrl Pts',(1.34033580999994,5.2,-3.77673891500002));
#356686=CARTESIAN_POINT('Ctrl Pts',(1.34033580999994,2.2,-3.77673891500002));
#356687=CARTESIAN_POINT('Ctrl Pts',(1.34051644399994,12.2,-3.77713826300001));
#356688=CARTESIAN_POINT('Ctrl Pts',(1.34051644399994,5.2,-3.77713826300001));
#356689=CARTESIAN_POINT('Ctrl Pts',(1.34051644399994,2.2,-3.77713826300001));
#356690=CARTESIAN_POINT('Ctrl Pts',(1.34070029299994,12.2,-3.77754330800002));
#356691=CARTESIAN_POINT('Ctrl Pts',(1.34070029299994,5.2,-3.77754330800002));
#356692=CARTESIAN_POINT('Ctrl Pts',(1.34070029299994,2.2,-3.77754330800002));
#356693=CARTESIAN_POINT('Ctrl Pts',(1.34088736599994,12.2,-3.77795402900002));
#356694=CARTESIAN_POINT('Ctrl Pts',(1.34088736599994,5.2,-3.77795402900002));
#356695=CARTESIAN_POINT('Ctrl Pts',(1.34088736599994,2.2,-3.77795402900002));
#356696=CARTESIAN_POINT('Ctrl Pts',(1.34107767199994,12.2,-3.77837040700001));
#356697=CARTESIAN_POINT('Ctrl Pts',(1.34107767199994,5.2,-3.77837040700001));
#356698=CARTESIAN_POINT('Ctrl Pts',(1.34107767199994,2.2,-3.77837040700001));
#356699=CARTESIAN_POINT('Ctrl Pts',(1.34127121999994,12.2,-3.77879242300001));
#356700=CARTESIAN_POINT('Ctrl Pts',(1.34127121999994,5.2,-3.77879242300001));
#356701=CARTESIAN_POINT('Ctrl Pts',(1.34127121999994,2.2,-3.77879242300001));
#356702=CARTESIAN_POINT('Ctrl Pts',(1.34146801999994,12.2,-3.77922005700002));
#356703=CARTESIAN_POINT('Ctrl Pts',(1.34146801999994,5.2,-3.77922005700002));
#356704=CARTESIAN_POINT('Ctrl Pts',(1.34146801999994,2.2,-3.77922005700002));
#356705=CARTESIAN_POINT('Ctrl Pts',(1.34166807999994,12.2,-3.77965329000002));
#356706=CARTESIAN_POINT('Ctrl Pts',(1.34166807999994,5.2,-3.77965329000002));
#356707=CARTESIAN_POINT('Ctrl Pts',(1.34166807999994,2.2,-3.77965329000002));
#356708=CARTESIAN_POINT('Ctrl Pts',(1.34187141099994,12.2,-3.78009210100001));
#356709=CARTESIAN_POINT('Ctrl Pts',(1.34187141099994,5.2,-3.78009210100001));
#356710=CARTESIAN_POINT('Ctrl Pts',(1.34187141099994,2.2,-3.78009210100001));
#356711=CARTESIAN_POINT('Ctrl Pts',(1.34207802099994,12.2,-3.78053647300002));
#356712=CARTESIAN_POINT('Ctrl Pts',(1.34207802099994,5.2,-3.78053647300002));
#356713=CARTESIAN_POINT('Ctrl Pts',(1.34207802099994,2.2,-3.78053647300002));
#356714=CARTESIAN_POINT('Ctrl Pts',(1.34228791699994,12.2,-3.78098638700001));
#356715=CARTESIAN_POINT('Ctrl Pts',(1.34228791699994,5.2,-3.78098638700001));
#356716=CARTESIAN_POINT('Ctrl Pts',(1.34228791699994,2.2,-3.78098638700001));
#356717=CARTESIAN_POINT('Ctrl Pts',(1.34250111099994,12.2,-3.78144182100002));
#356718=CARTESIAN_POINT('Ctrl Pts',(1.34250111099994,5.2,-3.78144182100002));
#356719=CARTESIAN_POINT('Ctrl Pts',(1.34250111099994,2.2,-3.78144182100002));
#356720=CARTESIAN_POINT('Ctrl Pts',(1.34271760999994,12.2,-3.78190275800002));
#356721=CARTESIAN_POINT('Ctrl Pts',(1.34271760999994,5.2,-3.78190275800002));
#356722=CARTESIAN_POINT('Ctrl Pts',(1.34271760999994,2.2,-3.78190275800002));
#356723=CARTESIAN_POINT('Ctrl Pts',(1.34293742399994,12.2,-3.78236917900002));
#356724=CARTESIAN_POINT('Ctrl Pts',(1.34293742399994,5.2,-3.78236917900002));
#356725=CARTESIAN_POINT('Ctrl Pts',(1.34293742399994,2.2,-3.78236917900002));
#356726=CARTESIAN_POINT('Ctrl Pts',(1.34316056099994,12.2,-3.78284106400002));
#356727=CARTESIAN_POINT('Ctrl Pts',(1.34316056099994,5.2,-3.78284106400002));
#356728=CARTESIAN_POINT('Ctrl Pts',(1.34316056099994,2.2,-3.78284106400002));
#356729=CARTESIAN_POINT('Ctrl Pts',(1.34338702999994,12.2,-3.78331839300001));
#356730=CARTESIAN_POINT('Ctrl Pts',(1.34338702999994,5.2,-3.78331839300001));
#356731=CARTESIAN_POINT('Ctrl Pts',(1.34338702999994,2.2,-3.78331839300001));
#356732=CARTESIAN_POINT('Ctrl Pts',(1.34361683999994,12.2,-3.78380114900001));
#356733=CARTESIAN_POINT('Ctrl Pts',(1.34361683999994,5.2,-3.78380114900001));
#356734=CARTESIAN_POINT('Ctrl Pts',(1.34361683999994,2.2,-3.78380114900001));
#356735=CARTESIAN_POINT('Ctrl Pts',(1.34384999799994,12.2,-3.78428931300002));
#356736=CARTESIAN_POINT('Ctrl Pts',(1.34384999799994,5.2,-3.78428931300002));
#356737=CARTESIAN_POINT('Ctrl Pts',(1.34384999799994,2.2,-3.78428931300002));
#356738=CARTESIAN_POINT('Ctrl Pts',(1.34408651399994,12.2,-3.78478286600001));
#356739=CARTESIAN_POINT('Ctrl Pts',(1.34408651399994,5.2,-3.78478286600001));
#356740=CARTESIAN_POINT('Ctrl Pts',(1.34408651399994,2.2,-3.78478286600001));
#356741=CARTESIAN_POINT('Ctrl Pts',(1.34432639799994,12.2,-3.78528178900002));
#356742=CARTESIAN_POINT('Ctrl Pts',(1.34432639799994,5.2,-3.78528178900002));
#356743=CARTESIAN_POINT('Ctrl Pts',(1.34432639799994,2.2,-3.78528178900002));
#356744=CARTESIAN_POINT('Ctrl Pts',(1.34456965499994,12.2,-3.78578606200001));
#356745=CARTESIAN_POINT('Ctrl Pts',(1.34456965499994,5.2,-3.78578606200001));
#356746=CARTESIAN_POINT('Ctrl Pts',(1.34456965499994,2.2,-3.78578606200001));
#356747=CARTESIAN_POINT('Ctrl Pts',(1.34481629599994,12.2,-3.78629566700001));
#356748=CARTESIAN_POINT('Ctrl Pts',(1.34481629599994,5.2,-3.78629566700001));
#356749=CARTESIAN_POINT('Ctrl Pts',(1.34481629599994,2.2,-3.78629566700001));
#356750=CARTESIAN_POINT('Ctrl Pts',(1.34506632799994,12.2,-3.78681058700002));
#356751=CARTESIAN_POINT('Ctrl Pts',(1.34506632799994,5.2,-3.78681058700002));
#356752=CARTESIAN_POINT('Ctrl Pts',(1.34506632799994,2.2,-3.78681058700002));
#356753=CARTESIAN_POINT('Ctrl Pts',(1.34531975999994,12.2,-3.78733080100002));
#356754=CARTESIAN_POINT('Ctrl Pts',(1.34531975999994,5.2,-3.78733080100002));
#356755=CARTESIAN_POINT('Ctrl Pts',(1.34531975999994,2.2,-3.78733080100002));
#356756=CARTESIAN_POINT('Ctrl Pts',(1.34557660099994,12.2,-3.78785629200001));
#356757=CARTESIAN_POINT('Ctrl Pts',(1.34557660099994,5.2,-3.78785629200001));
#356758=CARTESIAN_POINT('Ctrl Pts',(1.34557660099994,2.2,-3.78785629200001));
#356759=CARTESIAN_POINT('Ctrl Pts',(1.34583685899994,12.2,-3.78838704100001));
#356760=CARTESIAN_POINT('Ctrl Pts',(1.34583685899994,5.2,-3.78838704100001));
#356761=CARTESIAN_POINT('Ctrl Pts',(1.34583685899994,2.2,-3.78838704100001));
#356762=CARTESIAN_POINT('Ctrl Pts',(1.34610053999994,12.2,-3.78892302900002));
#356763=CARTESIAN_POINT('Ctrl Pts',(1.34610053999994,5.2,-3.78892302900002));
#356764=CARTESIAN_POINT('Ctrl Pts',(1.34610053999994,2.2,-3.78892302900002));
#356765=CARTESIAN_POINT('Ctrl Pts',(1.34636765499994,12.2,-3.78946423800001));
#356766=CARTESIAN_POINT('Ctrl Pts',(1.34636765499994,5.2,-3.78946423800001));
#356767=CARTESIAN_POINT('Ctrl Pts',(1.34636765499994,2.2,-3.78946423800001));
#356768=CARTESIAN_POINT('Ctrl Pts',(1.34663820999994,12.2,-3.79001065000002));
#356769=CARTESIAN_POINT('Ctrl Pts',(1.34663820999994,5.2,-3.79001065000002));
#356770=CARTESIAN_POINT('Ctrl Pts',(1.34663820999994,2.2,-3.79001065000002));
#356771=CARTESIAN_POINT('Ctrl Pts',(1.34691221499994,12.2,-3.79056224700001));
#356772=CARTESIAN_POINT('Ctrl Pts',(1.34691221499994,5.2,-3.79056224700001));
#356773=CARTESIAN_POINT('Ctrl Pts',(1.34691221499994,2.2,-3.79056224700001));
#356774=CARTESIAN_POINT('Ctrl Pts',(1.34718967599994,12.2,-3.79111900900002));
#356775=CARTESIAN_POINT('Ctrl Pts',(1.34718967599994,5.2,-3.79111900900002));
#356776=CARTESIAN_POINT('Ctrl Pts',(1.34718967599994,2.2,-3.79111900900002));
#356777=CARTESIAN_POINT('Ctrl Pts',(1.34747060299994,12.2,-3.79168091900001));
#356778=CARTESIAN_POINT('Ctrl Pts',(1.34747060299994,5.2,-3.79168091900001));
#356779=CARTESIAN_POINT('Ctrl Pts',(1.34747060299994,2.2,-3.79168091900001));
#356780=CARTESIAN_POINT('Ctrl Pts',(1.34775500299994,12.2,-3.79224795900001));
#356781=CARTESIAN_POINT('Ctrl Pts',(1.34775500299994,5.2,-3.79224795900001));
#356782=CARTESIAN_POINT('Ctrl Pts',(1.34775500299994,2.2,-3.79224795900001));
#356783=CARTESIAN_POINT('Ctrl Pts',(1.34804288399994,12.2,-3.79282010900001));
#356784=CARTESIAN_POINT('Ctrl Pts',(1.34804288399994,5.2,-3.79282010900001));
#356785=CARTESIAN_POINT('Ctrl Pts',(1.34804288399994,2.2,-3.79282010900001));
#356786=CARTESIAN_POINT('Ctrl Pts',(1.34833425199994,12.2,-3.79339735300002));
#356787=CARTESIAN_POINT('Ctrl Pts',(1.34833425199994,5.2,-3.79339735300002));
#356788=CARTESIAN_POINT('Ctrl Pts',(1.34833425199994,2.2,-3.79339735300002));
#356789=CARTESIAN_POINT('Ctrl Pts',(1.34862911799994,12.2,-3.79397967200001));
#356790=CARTESIAN_POINT('Ctrl Pts',(1.34862911799994,5.2,-3.79397967200001));
#356791=CARTESIAN_POINT('Ctrl Pts',(1.34862911799994,2.2,-3.79397967200001));
#356792=CARTESIAN_POINT('Ctrl Pts',(1.34892748699994,12.2,-3.79456704900001));
#356793=CARTESIAN_POINT('Ctrl Pts',(1.34892748699994,5.2,-3.79456704900001));
#356794=CARTESIAN_POINT('Ctrl Pts',(1.34892748699994,2.2,-3.79456704900001));
#356795=CARTESIAN_POINT('Ctrl Pts',(1.34922936899994,12.2,-3.79515946400002));
#356796=CARTESIAN_POINT('Ctrl Pts',(1.34922936899994,5.2,-3.79515946400002));
#356797=CARTESIAN_POINT('Ctrl Pts',(1.34922936899994,2.2,-3.79515946400002));
#356798=CARTESIAN_POINT('Ctrl Pts',(1.34953476899994,12.2,-3.79575690100001));
#356799=CARTESIAN_POINT('Ctrl Pts',(1.34953476899994,5.2,-3.79575690100001));
#356800=CARTESIAN_POINT('Ctrl Pts',(1.34953476899994,2.2,-3.79575690100001));
#356801=CARTESIAN_POINT('Ctrl Pts',(1.34984369799994,12.2,-3.79635934100001));
#356802=CARTESIAN_POINT('Ctrl Pts',(1.34984369799994,5.2,-3.79635934100001));
#356803=CARTESIAN_POINT('Ctrl Pts',(1.34984369799994,2.2,-3.79635934100001));
#356804=CARTESIAN_POINT('Ctrl Pts',(1.35015615999994,12.2,-3.79696676700001));
#356805=CARTESIAN_POINT('Ctrl Pts',(1.35015615999994,5.2,-3.79696676700001));
#356806=CARTESIAN_POINT('Ctrl Pts',(1.35015615999994,2.2,-3.79696676700001));
#356807=CARTESIAN_POINT('Ctrl Pts',(1.35047216499994,12.2,-3.79757915900001));
#356808=CARTESIAN_POINT('Ctrl Pts',(1.35047216499994,5.2,-3.79757915900001));
#356809=CARTESIAN_POINT('Ctrl Pts',(1.35047216499994,2.2,-3.79757915900001));
#356810=CARTESIAN_POINT('Ctrl Pts',(1.35079171899994,12.2,-3.79819650200002));
#356811=CARTESIAN_POINT('Ctrl Pts',(1.35079171899994,5.2,-3.79819650200002));
#356812=CARTESIAN_POINT('Ctrl Pts',(1.35079171899994,2.2,-3.79819650200002));
#356813=CARTESIAN_POINT('Ctrl Pts',(1.35111483199994,12.2,-3.79881877700001));
#356814=CARTESIAN_POINT('Ctrl Pts',(1.35111483199994,5.2,-3.79881877700001));
#356815=CARTESIAN_POINT('Ctrl Pts',(1.35111483199994,2.2,-3.79881877700001));
#356816=CARTESIAN_POINT('Ctrl Pts',(1.35144150699994,12.2,-3.79944596600001));
#356817=CARTESIAN_POINT('Ctrl Pts',(1.35144150699994,5.2,-3.79944596600001));
#356818=CARTESIAN_POINT('Ctrl Pts',(1.35144150699994,2.2,-3.79944596600001));
#356819=CARTESIAN_POINT('Ctrl Pts',(1.35177175599994,12.2,-3.80007805200002));
#356820=CARTESIAN_POINT('Ctrl Pts',(1.35177175599994,5.2,-3.80007805200002));
#356821=CARTESIAN_POINT('Ctrl Pts',(1.35177175599994,2.2,-3.80007805200002));
#356822=CARTESIAN_POINT('Ctrl Pts',(1.35210558299994,12.2,-3.80071501700002));
#356823=CARTESIAN_POINT('Ctrl Pts',(1.35210558299994,5.2,-3.80071501700002));
#356824=CARTESIAN_POINT('Ctrl Pts',(1.35210558299994,2.2,-3.80071501700002));
#356825=CARTESIAN_POINT('Ctrl Pts',(1.35244299699994,12.2,-3.80135684400001));
#356826=CARTESIAN_POINT('Ctrl Pts',(1.35244299699994,5.2,-3.80135684400001));
#356827=CARTESIAN_POINT('Ctrl Pts',(1.35244299699994,2.2,-3.80135684400001));
#356828=CARTESIAN_POINT('Ctrl Pts',(1.35278400499994,12.2,-3.80200351400001));
#356829=CARTESIAN_POINT('Ctrl Pts',(1.35278400499994,5.2,-3.80200351400001));
#356830=CARTESIAN_POINT('Ctrl Pts',(1.35278400499994,2.2,-3.80200351400001));
#356831=CARTESIAN_POINT('Ctrl Pts',(1.35312861199994,12.2,-3.80265501100002));
#356832=CARTESIAN_POINT('Ctrl Pts',(1.35312861199994,5.2,-3.80265501100002));
#356833=CARTESIAN_POINT('Ctrl Pts',(1.35312861199994,2.2,-3.80265501100002));
#356834=CARTESIAN_POINT('Ctrl Pts',(1.35347682899994,12.2,-3.80331131700002));
#356835=CARTESIAN_POINT('Ctrl Pts',(1.35347682899994,5.2,-3.80331131700002));
#356836=CARTESIAN_POINT('Ctrl Pts',(1.35347682899994,2.2,-3.80331131700002));
#356837=CARTESIAN_POINT('Ctrl Pts',(1.35382865999994,12.2,-3.80397241500001));
#356838=CARTESIAN_POINT('Ctrl Pts',(1.35382865999994,5.2,-3.80397241500001));
#356839=CARTESIAN_POINT('Ctrl Pts',(1.35382865999994,2.2,-3.80397241500001));
#356840=CARTESIAN_POINT('Ctrl Pts',(1.35418411299994,12.2,-3.80463828700002));
#356841=CARTESIAN_POINT('Ctrl Pts',(1.35418411299994,5.2,-3.80463828700002));
#356842=CARTESIAN_POINT('Ctrl Pts',(1.35418411299994,2.2,-3.80463828700002));
#356843=CARTESIAN_POINT('Ctrl Pts',(1.35454319599994,12.2,-3.80530891600001));
#356844=CARTESIAN_POINT('Ctrl Pts',(1.35454319599994,5.2,-3.80530891600001));
#356845=CARTESIAN_POINT('Ctrl Pts',(1.35454319599994,2.2,-3.80530891600001));
#356846=CARTESIAN_POINT('Ctrl Pts',(1.35490591599994,12.2,-3.80598428600001));
#356847=CARTESIAN_POINT('Ctrl Pts',(1.35490591599994,5.2,-3.80598428600001));
#356848=CARTESIAN_POINT('Ctrl Pts',(1.35490591599994,2.2,-3.80598428600001));
#356849=CARTESIAN_POINT('Ctrl Pts',(1.35527227699994,12.2,-3.80666437600001));
#356850=CARTESIAN_POINT('Ctrl Pts',(1.35527227699994,5.2,-3.80666437600001));
#356851=CARTESIAN_POINT('Ctrl Pts',(1.35527227699994,2.2,-3.80666437600001));
#356852=CARTESIAN_POINT('Ctrl Pts',(1.35564228799994,12.2,-3.80734917300002));
#356853=CARTESIAN_POINT('Ctrl Pts',(1.35564228799994,5.2,-3.80734917300002));
#356854=CARTESIAN_POINT('Ctrl Pts',(1.35564228799994,2.2,-3.80734917300002));
#356855=CARTESIAN_POINT('Ctrl Pts',(1.35601595799994,12.2,-3.80803865800001));
#356856=CARTESIAN_POINT('Ctrl Pts',(1.35601595799994,5.2,-3.80803865800001));
#356857=CARTESIAN_POINT('Ctrl Pts',(1.35601595799994,2.2,-3.80803865800001));
#356858=CARTESIAN_POINT('Ctrl Pts',(1.35639328999994,12.2,-3.80873281300001));
#356859=CARTESIAN_POINT('Ctrl Pts',(1.35639328999994,5.2,-3.80873281300001));
#356860=CARTESIAN_POINT('Ctrl Pts',(1.35639328999994,2.2,-3.80873281300001));
#356861=CARTESIAN_POINT('Ctrl Pts',(1.35677429299994,12.2,-3.80943162300001));
#356862=CARTESIAN_POINT('Ctrl Pts',(1.35677429299994,5.2,-3.80943162300001));
#356863=CARTESIAN_POINT('Ctrl Pts',(1.35677429299994,2.2,-3.80943162300001));
#356864=CARTESIAN_POINT('Ctrl Pts',(1.35715897299994,12.2,-3.81013506900001));
#356865=CARTESIAN_POINT('Ctrl Pts',(1.35715897299994,5.2,-3.81013506900001));
#356866=CARTESIAN_POINT('Ctrl Pts',(1.35715897299994,2.2,-3.81013506900001));
#356867=CARTESIAN_POINT('Ctrl Pts',(1.35754733699994,12.2,-3.81084313500001));
#356868=CARTESIAN_POINT('Ctrl Pts',(1.35754733699994,5.2,-3.81084313500001));
#356869=CARTESIAN_POINT('Ctrl Pts',(1.35754733699994,2.2,-3.81084313500001));
#356870=CARTESIAN_POINT('Ctrl Pts',(1.35793939099994,12.2,-3.81155580400002));
#356871=CARTESIAN_POINT('Ctrl Pts',(1.35793939099994,5.2,-3.81155580400002));
#356872=CARTESIAN_POINT('Ctrl Pts',(1.35793939099994,2.2,-3.81155580400002));
#356873=CARTESIAN_POINT('Ctrl Pts',(1.35833514199994,12.2,-3.81227305800001));
#356874=CARTESIAN_POINT('Ctrl Pts',(1.35833514199994,5.2,-3.81227305800001));
#356875=CARTESIAN_POINT('Ctrl Pts',(1.35833514199994,2.2,-3.81227305800001));
#356876=CARTESIAN_POINT('Ctrl Pts',(1.35873459799994,12.2,-3.81299488200002));
#356877=CARTESIAN_POINT('Ctrl Pts',(1.35873459799994,5.2,-3.81299488200002));
#356878=CARTESIAN_POINT('Ctrl Pts',(1.35873459799994,2.2,-3.81299488200002));
#356879=CARTESIAN_POINT('Ctrl Pts',(1.35913776399994,12.2,-3.81372125800001));
#356880=CARTESIAN_POINT('Ctrl Pts',(1.35913776399994,5.2,-3.81372125800001));
#356881=CARTESIAN_POINT('Ctrl Pts',(1.35913776399994,2.2,-3.81372125800001));
#356882=CARTESIAN_POINT('Ctrl Pts',(1.35954464599994,12.2,-3.81445216800001));
#356883=CARTESIAN_POINT('Ctrl Pts',(1.35954464599994,5.2,-3.81445216800001));
#356884=CARTESIAN_POINT('Ctrl Pts',(1.35954464599994,2.2,-3.81445216800001));
#356885=CARTESIAN_POINT('Ctrl Pts',(1.35995525099994,12.2,-3.81518759900001));
#356886=CARTESIAN_POINT('Ctrl Pts',(1.35995525099994,5.2,-3.81518759900001));
#356887=CARTESIAN_POINT('Ctrl Pts',(1.35995525099994,2.2,-3.81518759900001));
#356888=CARTESIAN_POINT('Ctrl Pts',(1.36036958699994,12.2,-3.81592753000001));
#356889=CARTESIAN_POINT('Ctrl Pts',(1.36036958699994,5.2,-3.81592753000001));
#356890=CARTESIAN_POINT('Ctrl Pts',(1.36036958699994,2.2,-3.81592753000001));
#356891=CARTESIAN_POINT('Ctrl Pts',(1.36078765799994,12.2,-3.81667194600002));
#356892=CARTESIAN_POINT('Ctrl Pts',(1.36078765799994,5.2,-3.81667194600002));
#356893=CARTESIAN_POINT('Ctrl Pts',(1.36078765799994,2.2,-3.81667194600002));
#356894=CARTESIAN_POINT('Ctrl Pts',(1.36120947099994,12.2,-3.81742083100002));
#356895=CARTESIAN_POINT('Ctrl Pts',(1.36120947099994,5.2,-3.81742083100002));
#356896=CARTESIAN_POINT('Ctrl Pts',(1.36120947099994,2.2,-3.81742083100002));
#356897=CARTESIAN_POINT('Ctrl Pts',(1.36163503399994,12.2,-3.81817416700001));
#356898=CARTESIAN_POINT('Ctrl Pts',(1.36163503399994,5.2,-3.81817416700001));
#356899=CARTESIAN_POINT('Ctrl Pts',(1.36163503399994,2.2,-3.81817416700001));
#356900=CARTESIAN_POINT('Ctrl Pts',(1.36206435199994,12.2,-3.81893193900002));
#356901=CARTESIAN_POINT('Ctrl Pts',(1.36206435199994,5.2,-3.81893193900002));
#356902=CARTESIAN_POINT('Ctrl Pts',(1.36206435199994,2.2,-3.81893193900002));
#356903=CARTESIAN_POINT('Ctrl Pts',(1.36249743099994,12.2,-3.81969412900002));
#356904=CARTESIAN_POINT('Ctrl Pts',(1.36249743099994,5.2,-3.81969412900002));
#356905=CARTESIAN_POINT('Ctrl Pts',(1.36249743099994,2.2,-3.81969412900002));
#356906=CARTESIAN_POINT('Ctrl Pts',(1.36293427699994,12.2,-3.82046072100001));
#356907=CARTESIAN_POINT('Ctrl Pts',(1.36293427699994,5.2,-3.82046072100001));
#356908=CARTESIAN_POINT('Ctrl Pts',(1.36293427699994,2.2,-3.82046072100001));
#356909=CARTESIAN_POINT('Ctrl Pts',(1.36337489599994,12.2,-3.82123169900002));
#356910=CARTESIAN_POINT('Ctrl Pts',(1.36337489599994,5.2,-3.82123169900002));
#356911=CARTESIAN_POINT('Ctrl Pts',(1.36337489599994,2.2,-3.82123169900002));
#356912=CARTESIAN_POINT('Ctrl Pts',(1.36381929499994,12.2,-3.82200704600002));
#356913=CARTESIAN_POINT('Ctrl Pts',(1.36381929499994,5.2,-3.82200704600002));
#356914=CARTESIAN_POINT('Ctrl Pts',(1.36381929499994,2.2,-3.82200704600002));
#356915=CARTESIAN_POINT('Ctrl Pts',(1.36426748099994,12.2,-3.82278674500002));
#356916=CARTESIAN_POINT('Ctrl Pts',(1.36426748099994,5.2,-3.82278674500002));
#356917=CARTESIAN_POINT('Ctrl Pts',(1.36426748099994,2.2,-3.82278674500002));
#356918=CARTESIAN_POINT('Ctrl Pts',(1.36471945699994,12.2,-3.82357078100001));
#356919=CARTESIAN_POINT('Ctrl Pts',(1.36471945699994,5.2,-3.82357078100001));
#356920=CARTESIAN_POINT('Ctrl Pts',(1.36471945699994,2.2,-3.82357078100001));
#356921=CARTESIAN_POINT('Ctrl Pts',(1.36517523299994,12.2,-3.82435913800002));
#356922=CARTESIAN_POINT('Ctrl Pts',(1.36517523299994,5.2,-3.82435913800002));
#356923=CARTESIAN_POINT('Ctrl Pts',(1.36517523299994,2.2,-3.82435913800002));
#356924=CARTESIAN_POINT('Ctrl Pts',(1.36563481099994,12.2,-3.82515179700002));
#356925=CARTESIAN_POINT('Ctrl Pts',(1.36563481099994,5.2,-3.82515179700002));
#356926=CARTESIAN_POINT('Ctrl Pts',(1.36563481099994,2.2,-3.82515179700002));
#356927=CARTESIAN_POINT('Ctrl Pts',(1.36609819999994,12.2,-3.82594874400001));
#356928=CARTESIAN_POINT('Ctrl Pts',(1.36609819999994,5.2,-3.82594874400001));
#356929=CARTESIAN_POINT('Ctrl Pts',(1.36609819999994,2.2,-3.82594874400001));
#356930=CARTESIAN_POINT('Ctrl Pts',(1.36656540399994,12.2,-3.82674996100001));
#356931=CARTESIAN_POINT('Ctrl Pts',(1.36656540399994,5.2,-3.82674996100001));
#356932=CARTESIAN_POINT('Ctrl Pts',(1.36656540399994,2.2,-3.82674996100001));
#356933=CARTESIAN_POINT('Ctrl Pts',(1.36703642999994,12.2,-3.82755543500001));
#356934=CARTESIAN_POINT('Ctrl Pts',(1.36703642999994,5.2,-3.82755543500001));
#356935=CARTESIAN_POINT('Ctrl Pts',(1.36703642999994,2.2,-3.82755543500001));
#356936=CARTESIAN_POINT('Ctrl Pts',(1.36751128299994,12.2,-3.82836514600001));
#356937=CARTESIAN_POINT('Ctrl Pts',(1.36751128299994,5.2,-3.82836514600001));
#356938=CARTESIAN_POINT('Ctrl Pts',(1.36751128299994,2.2,-3.82836514600001));
#356939=CARTESIAN_POINT('Ctrl Pts',(1.36798996999994,12.2,-3.82917908000001));
#356940=CARTESIAN_POINT('Ctrl Pts',(1.36798996999994,5.2,-3.82917908000001));
#356941=CARTESIAN_POINT('Ctrl Pts',(1.36798996999994,2.2,-3.82917908000001));
#356942=CARTESIAN_POINT('Ctrl Pts',(1.36847249499994,12.2,-3.82999722100001));
#356943=CARTESIAN_POINT('Ctrl Pts',(1.36847249499994,5.2,-3.82999722100001));
#356944=CARTESIAN_POINT('Ctrl Pts',(1.36847249499994,2.2,-3.82999722100001));
#356945=CARTESIAN_POINT('Ctrl Pts',(1.36895886499994,12.2,-3.83081955200002));
#356946=CARTESIAN_POINT('Ctrl Pts',(1.36895886499994,5.2,-3.83081955200002));
#356947=CARTESIAN_POINT('Ctrl Pts',(1.36895886499994,2.2,-3.83081955200002));
#356948=CARTESIAN_POINT('Ctrl Pts',(1.36944908599994,12.2,-3.83164605800001));
#356949=CARTESIAN_POINT('Ctrl Pts',(1.36944908599994,5.2,-3.83164605800001));
#356950=CARTESIAN_POINT('Ctrl Pts',(1.36944908599994,2.2,-3.83164605800001));
#356951=CARTESIAN_POINT('Ctrl Pts',(1.36994316299994,12.2,-3.83247672100001));
#356952=CARTESIAN_POINT('Ctrl Pts',(1.36994316299994,5.2,-3.83247672100001));
#356953=CARTESIAN_POINT('Ctrl Pts',(1.36994316299994,2.2,-3.83247672100001));
#356954=CARTESIAN_POINT('Ctrl Pts',(1.37044110099994,12.2,-3.83331152800002));
#356955=CARTESIAN_POINT('Ctrl Pts',(1.37044110099994,5.2,-3.83331152800002));
#356956=CARTESIAN_POINT('Ctrl Pts',(1.37044110099994,2.2,-3.83331152800002));
#356957=CARTESIAN_POINT('Ctrl Pts',(1.37094290799994,12.2,-3.83415046100001));
#356958=CARTESIAN_POINT('Ctrl Pts',(1.37094290799994,5.2,-3.83415046100001));
#356959=CARTESIAN_POINT('Ctrl Pts',(1.37094290799994,2.2,-3.83415046100001));
#356960=CARTESIAN_POINT('Ctrl Pts',(1.37144858499994,12.2,-3.83499350300001));
#356961=CARTESIAN_POINT('Ctrl Pts',(1.37144858499994,5.2,-3.83499350300001));
#356962=CARTESIAN_POINT('Ctrl Pts',(1.37144858499994,2.2,-3.83499350300001));
#356963=CARTESIAN_POINT('Ctrl Pts',(1.37195814299994,12.2,-3.83584064200001));
#356964=CARTESIAN_POINT('Ctrl Pts',(1.37195814299994,5.2,-3.83584064200001));
#356965=CARTESIAN_POINT('Ctrl Pts',(1.37195814299994,2.2,-3.83584064200001));
#356966=CARTESIAN_POINT('Ctrl Pts',(1.37247158399994,12.2,-3.83669185900001));
#356967=CARTESIAN_POINT('Ctrl Pts',(1.37247158399994,5.2,-3.83669185900001));
#356968=CARTESIAN_POINT('Ctrl Pts',(1.37247158399994,2.2,-3.83669185900001));
#356969=CARTESIAN_POINT('Ctrl Pts',(1.37298891399994,12.2,-3.83754713800001));
#356970=CARTESIAN_POINT('Ctrl Pts',(1.37298891399994,5.2,-3.83754713800001));
#356971=CARTESIAN_POINT('Ctrl Pts',(1.37298891399994,2.2,-3.83754713800001));
#356972=CARTESIAN_POINT('Ctrl Pts',(1.37351013899994,12.2,-3.83840646500001));
#356973=CARTESIAN_POINT('Ctrl Pts',(1.37351013899994,5.2,-3.83840646500001));
#356974=CARTESIAN_POINT('Ctrl Pts',(1.37351013899994,2.2,-3.83840646500001));
#356975=CARTESIAN_POINT('Ctrl Pts',(1.37403526399994,12.2,-3.83926982500002));
#356976=CARTESIAN_POINT('Ctrl Pts',(1.37403526399994,5.2,-3.83926982500002));
#356977=CARTESIAN_POINT('Ctrl Pts',(1.37403526399994,2.2,-3.83926982500002));
#356978=CARTESIAN_POINT('Ctrl Pts',(1.37456429499994,12.2,-3.84013719900001));
#356979=CARTESIAN_POINT('Ctrl Pts',(1.37456429499994,5.2,-3.84013719900001));
#356980=CARTESIAN_POINT('Ctrl Pts',(1.37456429499994,2.2,-3.84013719900001));
#356981=CARTESIAN_POINT('Ctrl Pts',(1.37509723699994,12.2,-3.84100857400002));
#356982=CARTESIAN_POINT('Ctrl Pts',(1.37509723699994,5.2,-3.84100857400002));
#356983=CARTESIAN_POINT('Ctrl Pts',(1.37509723699994,2.2,-3.84100857400002));
#356984=CARTESIAN_POINT('Ctrl Pts',(1.37563409399994,12.2,-3.84188393300001));
#356985=CARTESIAN_POINT('Ctrl Pts',(1.37563409399994,5.2,-3.84188393300001));
#356986=CARTESIAN_POINT('Ctrl Pts',(1.37563409399994,2.2,-3.84188393300001));
#356987=CARTESIAN_POINT('Ctrl Pts',(1.37617487299994,12.2,-3.84276326100002));
#356988=CARTESIAN_POINT('Ctrl Pts',(1.37617487299994,5.2,-3.84276326100002));
#356989=CARTESIAN_POINT('Ctrl Pts',(1.37617487299994,2.2,-3.84276326100002));
#356990=CARTESIAN_POINT('Ctrl Pts',(1.37671957899994,12.2,-3.84364654300001));
#356991=CARTESIAN_POINT('Ctrl Pts',(1.37671957899994,5.2,-3.84364654300001));
#356992=CARTESIAN_POINT('Ctrl Pts',(1.37671957899994,2.2,-3.84364654300001));
#356993=CARTESIAN_POINT('Ctrl Pts',(1.37726821599994,12.2,-3.84453376200002));
#356994=CARTESIAN_POINT('Ctrl Pts',(1.37726821599994,5.2,-3.84453376200002));
#356995=CARTESIAN_POINT('Ctrl Pts',(1.37726821599994,2.2,-3.84453376200002));
#356996=CARTESIAN_POINT('Ctrl Pts',(1.37782079099994,12.2,-3.84542490400001));
#356997=CARTESIAN_POINT('Ctrl Pts',(1.37782079099994,5.2,-3.84542490400001));
#356998=CARTESIAN_POINT('Ctrl Pts',(1.37782079099994,2.2,-3.84542490400001));
#356999=CARTESIAN_POINT('Ctrl Pts',(1.37837730699994,12.2,-3.84631995400001));
#357000=CARTESIAN_POINT('Ctrl Pts',(1.37837730699994,5.2,-3.84631995400001));
#357001=CARTESIAN_POINT('Ctrl Pts',(1.37837730699994,2.2,-3.84631995400001));
#357002=CARTESIAN_POINT('Ctrl Pts',(1.37893776999994,12.2,-3.84721889300002));
#357003=CARTESIAN_POINT('Ctrl Pts',(1.37893776999994,5.2,-3.84721889300002));
#357004=CARTESIAN_POINT('Ctrl Pts',(1.37893776999994,2.2,-3.84721889300002));
#357005=CARTESIAN_POINT('Ctrl Pts',(1.37950218599994,12.2,-3.84812170900001));
#357006=CARTESIAN_POINT('Ctrl Pts',(1.37950218599994,5.2,-3.84812170900001));
#357007=CARTESIAN_POINT('Ctrl Pts',(1.37950218599994,2.2,-3.84812170900001));
#357008=CARTESIAN_POINT('Ctrl Pts',(1.38007055999994,12.2,-3.84902838500001));
#357009=CARTESIAN_POINT('Ctrl Pts',(1.38007055999994,5.2,-3.84902838500001));
#357010=CARTESIAN_POINT('Ctrl Pts',(1.38007055999994,2.2,-3.84902838500001));
#357011=CARTESIAN_POINT('Ctrl Pts',(1.38064289399994,12.2,-3.84993890800001));
#357012=CARTESIAN_POINT('Ctrl Pts',(1.38064289399994,5.2,-3.84993890800001));
#357013=CARTESIAN_POINT('Ctrl Pts',(1.38064289399994,2.2,-3.84993890800001));
#357014=CARTESIAN_POINT('Ctrl Pts',(1.38121919799994,12.2,-3.85085325900001));
#357015=CARTESIAN_POINT('Ctrl Pts',(1.38121919799994,5.2,-3.85085325900001));
#357016=CARTESIAN_POINT('Ctrl Pts',(1.38121919799994,2.2,-3.85085325900001));
#357017=CARTESIAN_POINT('Ctrl Pts',(1.38179947199994,12.2,-3.85177142500002));
#357018=CARTESIAN_POINT('Ctrl Pts',(1.38179947199994,5.2,-3.85177142500002));
#357019=CARTESIAN_POINT('Ctrl Pts',(1.38179947199994,2.2,-3.85177142500002));
#357020=CARTESIAN_POINT('Ctrl Pts',(1.38238372299994,12.2,-3.85269339200002));
#357021=CARTESIAN_POINT('Ctrl Pts',(1.38238372299994,5.2,-3.85269339200002));
#357022=CARTESIAN_POINT('Ctrl Pts',(1.38238372299994,2.2,-3.85269339200002));
#357023=CARTESIAN_POINT('Ctrl Pts',(1.38297195699994,12.2,-3.85361914100002));
#357024=CARTESIAN_POINT('Ctrl Pts',(1.38297195699994,5.2,-3.85361914100002));
#357025=CARTESIAN_POINT('Ctrl Pts',(1.38297195699994,2.2,-3.85361914100002));
#357026=CARTESIAN_POINT('Ctrl Pts',(1.38356417799994,12.2,-3.85454866000002));
#357027=CARTESIAN_POINT('Ctrl Pts',(1.38356417799994,5.2,-3.85454866000002));
#357028=CARTESIAN_POINT('Ctrl Pts',(1.38356417799994,2.2,-3.85454866000002));
#357029=CARTESIAN_POINT('Ctrl Pts',(1.38416038999994,12.2,-3.85548193300002));
#357030=CARTESIAN_POINT('Ctrl Pts',(1.38416038999994,5.2,-3.85548193300002));
#357031=CARTESIAN_POINT('Ctrl Pts',(1.38416038999994,2.2,-3.85548193300002));
#357032=CARTESIAN_POINT('Ctrl Pts',(1.38476059799994,12.2,-3.85641894400001));
#357033=CARTESIAN_POINT('Ctrl Pts',(1.38476059799994,5.2,-3.85641894400001));
#357034=CARTESIAN_POINT('Ctrl Pts',(1.38476059799994,2.2,-3.85641894400001));
#357035=CARTESIAN_POINT('Ctrl Pts',(1.38536480699994,12.2,-3.85735967900001));
#357036=CARTESIAN_POINT('Ctrl Pts',(1.38536480699994,5.2,-3.85735967900001));
#357037=CARTESIAN_POINT('Ctrl Pts',(1.38536480699994,2.2,-3.85735967900001));
#357038=CARTESIAN_POINT('Ctrl Pts',(1.38597302199994,12.2,-3.85830412200002));
#357039=CARTESIAN_POINT('Ctrl Pts',(1.38597302199994,5.2,-3.85830412200002));
#357040=CARTESIAN_POINT('Ctrl Pts',(1.38597302199994,2.2,-3.85830412200002));
#357041=CARTESIAN_POINT('Ctrl Pts',(1.38658524799994,12.2,-3.85925225800001));
#357042=CARTESIAN_POINT('Ctrl Pts',(1.38658524799994,5.2,-3.85925225800001));
#357043=CARTESIAN_POINT('Ctrl Pts',(1.38658524799994,2.2,-3.85925225800001));
#357044=CARTESIAN_POINT('Ctrl Pts',(1.38720148999994,12.2,-3.86020407300002));
#357045=CARTESIAN_POINT('Ctrl Pts',(1.38720148999994,5.2,-3.86020407300002));
#357046=CARTESIAN_POINT('Ctrl Pts',(1.38720148999994,2.2,-3.86020407300002));
#357047=CARTESIAN_POINT('Ctrl Pts',(1.38782174999994,12.2,-3.86115955100002));
#357048=CARTESIAN_POINT('Ctrl Pts',(1.38782174999994,5.2,-3.86115955100002));
#357049=CARTESIAN_POINT('Ctrl Pts',(1.38782174999994,2.2,-3.86115955100002));
#357050=CARTESIAN_POINT('Ctrl Pts',(1.38844603399994,12.2,-3.86211867800001));
#357051=CARTESIAN_POINT('Ctrl Pts',(1.38844603399994,5.2,-3.86211867800001));
#357052=CARTESIAN_POINT('Ctrl Pts',(1.38844603399994,2.2,-3.86211867800001));
#357053=CARTESIAN_POINT('Ctrl Pts',(1.38907434899994,12.2,-3.86308143800001));
#357054=CARTESIAN_POINT('Ctrl Pts',(1.38907434899994,5.2,-3.86308143800001));
#357055=CARTESIAN_POINT('Ctrl Pts',(1.38907434899994,2.2,-3.86308143800001));
#357056=CARTESIAN_POINT('Ctrl Pts',(1.38970669599994,12.2,-3.86404781700001));
#357057=CARTESIAN_POINT('Ctrl Pts',(1.38970669599994,5.2,-3.86404781700001));
#357058=CARTESIAN_POINT('Ctrl Pts',(1.38970669599994,2.2,-3.86404781700001));
#357059=CARTESIAN_POINT('Ctrl Pts',(1.39034308099994,12.2,-3.86501779900001));
#357060=CARTESIAN_POINT('Ctrl Pts',(1.39034308099994,5.2,-3.86501779900001));
#357061=CARTESIAN_POINT('Ctrl Pts',(1.39034308099994,2.2,-3.86501779900001));
#357062=CARTESIAN_POINT('Ctrl Pts',(1.39098350899994,12.2,-3.86599137000001));
#357063=CARTESIAN_POINT('Ctrl Pts',(1.39098350899994,5.2,-3.86599137000001));
#357064=CARTESIAN_POINT('Ctrl Pts',(1.39098350899994,2.2,-3.86599137000001));
#357065=CARTESIAN_POINT('Ctrl Pts',(1.39162798299994,12.2,-3.86696851600002));
#357066=CARTESIAN_POINT('Ctrl Pts',(1.39162798299994,5.2,-3.86696851600002));
#357067=CARTESIAN_POINT('Ctrl Pts',(1.39162798299994,2.2,-3.86696851600002));
#357068=CARTESIAN_POINT('Ctrl Pts',(1.39227650999994,12.2,-3.86794922000002));
#357069=CARTESIAN_POINT('Ctrl Pts',(1.39227650999994,5.2,-3.86794922000002));
#357070=CARTESIAN_POINT('Ctrl Pts',(1.39227650999994,2.2,-3.86794922000002));
#357071=CARTESIAN_POINT('Ctrl Pts',(1.39292909199994,12.2,-3.86893347000001));
#357072=CARTESIAN_POINT('Ctrl Pts',(1.39292909199994,5.2,-3.86893347000001));
#357073=CARTESIAN_POINT('Ctrl Pts',(1.39292909199994,2.2,-3.86893347000001));
#357074=CARTESIAN_POINT('Ctrl Pts',(1.39358573299994,12.2,-3.86992124900001));
#357075=CARTESIAN_POINT('Ctrl Pts',(1.39358573299994,5.2,-3.86992124900001));
#357076=CARTESIAN_POINT('Ctrl Pts',(1.39358573299994,2.2,-3.86992124900001));
#357077=CARTESIAN_POINT('Ctrl Pts',(1.39424643899994,12.2,-3.87091254300001));
#357078=CARTESIAN_POINT('Ctrl Pts',(1.39424643899994,5.2,-3.87091254300001));
#357079=CARTESIAN_POINT('Ctrl Pts',(1.39424643899994,2.2,-3.87091254300001));
#357080=CARTESIAN_POINT('Ctrl Pts',(1.39491121399994,12.2,-3.87190733700002));
#357081=CARTESIAN_POINT('Ctrl Pts',(1.39491121399994,5.2,-3.87190733700002));
#357082=CARTESIAN_POINT('Ctrl Pts',(1.39491121399994,2.2,-3.87190733700002));
#357083=CARTESIAN_POINT('Ctrl Pts',(1.39558006099994,12.2,-3.87290561800001));
#357084=CARTESIAN_POINT('Ctrl Pts',(1.39558006099994,5.2,-3.87290561800001));
#357085=CARTESIAN_POINT('Ctrl Pts',(1.39558006099994,2.2,-3.87290561800001));
#357086=CARTESIAN_POINT('Ctrl Pts',(1.39625298699994,12.2,-3.87390736900001));
#357087=CARTESIAN_POINT('Ctrl Pts',(1.39625298699994,5.2,-3.87390736900001));
#357088=CARTESIAN_POINT('Ctrl Pts',(1.39625298699994,2.2,-3.87390736900001));
#357089=CARTESIAN_POINT('Ctrl Pts',(1.39692999299994,12.2,-3.87491257700002));
#357090=CARTESIAN_POINT('Ctrl Pts',(1.39692999299994,5.2,-3.87491257700002));
#357091=CARTESIAN_POINT('Ctrl Pts',(1.39692999299994,2.2,-3.87491257700002));
#357092=CARTESIAN_POINT('Ctrl Pts',(1.39761108399994,12.2,-3.87592122700001));
#357093=CARTESIAN_POINT('Ctrl Pts',(1.39761108399994,5.2,-3.87592122700001));
#357094=CARTESIAN_POINT('Ctrl Pts',(1.39761108399994,2.2,-3.87592122700001));
#357095=CARTESIAN_POINT('Ctrl Pts',(1.39829626699994,12.2,-3.87693330500001));
#357096=CARTESIAN_POINT('Ctrl Pts',(1.39829626699994,5.2,-3.87693330500001));
#357097=CARTESIAN_POINT('Ctrl Pts',(1.39829626699994,2.2,-3.87693330500001));
#357098=CARTESIAN_POINT('Ctrl Pts',(1.39898554099994,12.2,-3.87794879600001));
#357099=CARTESIAN_POINT('Ctrl Pts',(1.39898554099994,5.2,-3.87794879600001));
#357100=CARTESIAN_POINT('Ctrl Pts',(1.39898554099994,2.2,-3.87794879600001));
#357101=CARTESIAN_POINT('Ctrl Pts',(1.39967891499994,12.2,-3.87896768400001));
#357102=CARTESIAN_POINT('Ctrl Pts',(1.39967891499994,5.2,-3.87896768400001));
#357103=CARTESIAN_POINT('Ctrl Pts',(1.39967891499994,2.2,-3.87896768400001));
#357104=CARTESIAN_POINT('Ctrl Pts',(1.40037638999994,12.2,-3.87998995800002));
#357105=CARTESIAN_POINT('Ctrl Pts',(1.40037638999994,5.2,-3.87998995800002));
#357106=CARTESIAN_POINT('Ctrl Pts',(1.40037638999994,2.2,-3.87998995800002));
#357107=CARTESIAN_POINT('Ctrl Pts',(1.40107797099994,12.2,-3.88101560100001));
#357108=CARTESIAN_POINT('Ctrl Pts',(1.40107797099994,5.2,-3.88101560100001));
#357109=CARTESIAN_POINT('Ctrl Pts',(1.40107797099994,2.2,-3.88101560100001));
#357110=CARTESIAN_POINT('Ctrl Pts',(1.40178366299994,12.2,-3.88204459900001));
#357111=CARTESIAN_POINT('Ctrl Pts',(1.40178366299994,5.2,-3.88204459900001));
#357112=CARTESIAN_POINT('Ctrl Pts',(1.40178366299994,2.2,-3.88204459900001));
#357113=CARTESIAN_POINT('Ctrl Pts',(1.40249346899994,12.2,-3.88307693800002));
#357114=CARTESIAN_POINT('Ctrl Pts',(1.40249346899994,5.2,-3.88307693800002));
#357115=CARTESIAN_POINT('Ctrl Pts',(1.40249346899994,2.2,-3.88307693800002));
#357116=CARTESIAN_POINT('Ctrl Pts',(1.40320739299994,12.2,-3.88411260400002));
#357117=CARTESIAN_POINT('Ctrl Pts',(1.40320739299994,5.2,-3.88411260400002));
#357118=CARTESIAN_POINT('Ctrl Pts',(1.40320739299994,2.2,-3.88411260400002));
#357119=CARTESIAN_POINT('Ctrl Pts',(1.40392543799994,12.2,-3.88515158100001));
#357120=CARTESIAN_POINT('Ctrl Pts',(1.40392543799994,5.2,-3.88515158100001));
#357121=CARTESIAN_POINT('Ctrl Pts',(1.40392543799994,2.2,-3.88515158100001));
#357122=CARTESIAN_POINT('Ctrl Pts',(1.40464760899994,12.2,-3.88619385700002));
#357123=CARTESIAN_POINT('Ctrl Pts',(1.40464760899994,5.2,-3.88619385700002));
#357124=CARTESIAN_POINT('Ctrl Pts',(1.40464760899994,2.2,-3.88619385700002));
#357125=CARTESIAN_POINT('Ctrl Pts',(1.40537391099994,12.2,-3.88723941700002));
#357126=CARTESIAN_POINT('Ctrl Pts',(1.40537391099994,5.2,-3.88723941700002));
#357127=CARTESIAN_POINT('Ctrl Pts',(1.40537391099994,2.2,-3.88723941700002));
#357128=CARTESIAN_POINT('Ctrl Pts',(1.40610434499994,12.2,-3.88828824600001));
#357129=CARTESIAN_POINT('Ctrl Pts',(1.40610434499994,5.2,-3.88828824600001));
#357130=CARTESIAN_POINT('Ctrl Pts',(1.40610434499994,2.2,-3.88828824600001));
#357131=CARTESIAN_POINT('Ctrl Pts',(1.40683891699994,12.2,-3.88934033000002));
#357132=CARTESIAN_POINT('Ctrl Pts',(1.40683891699994,5.2,-3.88934033000002));
#357133=CARTESIAN_POINT('Ctrl Pts',(1.40683891699994,2.2,-3.88934033000002));
#357134=CARTESIAN_POINT('Ctrl Pts',(1.40757762999994,12.2,-3.89039565500001));
#357135=CARTESIAN_POINT('Ctrl Pts',(1.40757762999994,5.2,-3.89039565500001));
#357136=CARTESIAN_POINT('Ctrl Pts',(1.40757762999994,2.2,-3.89039565500001));
#357137=CARTESIAN_POINT('Ctrl Pts',(1.40832048899994,12.2,-3.89145420800002));
#357138=CARTESIAN_POINT('Ctrl Pts',(1.40832048899994,5.2,-3.89145420800002));
#357139=CARTESIAN_POINT('Ctrl Pts',(1.40832048899994,2.2,-3.89145420800002));
#357140=CARTESIAN_POINT('Ctrl Pts',(1.40906749599994,12.2,-3.89251597300001));
#357141=CARTESIAN_POINT('Ctrl Pts',(1.40906749599994,5.2,-3.89251597300001));
#357142=CARTESIAN_POINT('Ctrl Pts',(1.40906749599994,2.2,-3.89251597300001));
#357143=CARTESIAN_POINT('Ctrl Pts',(1.40981865399994,12.2,-3.89358093600002));
#357144=CARTESIAN_POINT('Ctrl Pts',(1.40981865399994,5.2,-3.89358093600002));
#357145=CARTESIAN_POINT('Ctrl Pts',(1.40981865399994,2.2,-3.89358093600002));
#357146=CARTESIAN_POINT('Ctrl Pts',(1.41057396999994,12.2,-3.89464908600001));
#357147=CARTESIAN_POINT('Ctrl Pts',(1.41057396999994,5.2,-3.89464908600001));
#357148=CARTESIAN_POINT('Ctrl Pts',(1.41057396999994,2.2,-3.89464908600001));
#357149=CARTESIAN_POINT('Ctrl Pts',(1.41133344599994,12.2,-3.89572040500001));
#357150=CARTESIAN_POINT('Ctrl Pts',(1.41133344599994,5.2,-3.89572040500001));
#357151=CARTESIAN_POINT('Ctrl Pts',(1.41133344599994,2.2,-3.89572040500001));
#357152=CARTESIAN_POINT('Ctrl Pts',(1.41209708399994,12.2,-3.89679488000001));
#357153=CARTESIAN_POINT('Ctrl Pts',(1.41209708399994,5.2,-3.89679488000001));
#357154=CARTESIAN_POINT('Ctrl Pts',(1.41209708399994,2.2,-3.89679488000001));
#357155=CARTESIAN_POINT('Ctrl Pts',(1.41286488899994,12.2,-3.89787249900001));
#357156=CARTESIAN_POINT('Ctrl Pts',(1.41286488899994,5.2,-3.89787249900001));
#357157=CARTESIAN_POINT('Ctrl Pts',(1.41286488899994,2.2,-3.89787249900001));
#357158=CARTESIAN_POINT('Ctrl Pts',(1.41363686599994,12.2,-3.89895324600001));
#357159=CARTESIAN_POINT('Ctrl Pts',(1.41363686599994,5.2,-3.89895324600001));
#357160=CARTESIAN_POINT('Ctrl Pts',(1.41363686599994,2.2,-3.89895324600001));
#357161=CARTESIAN_POINT('Ctrl Pts',(1.41441301599994,12.2,-3.90003710800002));
#357162=CARTESIAN_POINT('Ctrl Pts',(1.41441301599994,5.2,-3.90003710800002));
#357163=CARTESIAN_POINT('Ctrl Pts',(1.41441301599994,2.2,-3.90003710800002));
#357164=CARTESIAN_POINT('Ctrl Pts',(1.41519334299994,12.2,-3.90112407000001));
#357165=CARTESIAN_POINT('Ctrl Pts',(1.41519334299994,5.2,-3.90112407000001));
#357166=CARTESIAN_POINT('Ctrl Pts',(1.41519334299994,2.2,-3.90112407000001));
#357167=CARTESIAN_POINT('Ctrl Pts',(1.41597785299994,12.2,-3.90221412000002));
#357168=CARTESIAN_POINT('Ctrl Pts',(1.41597785299994,5.2,-3.90221412000002));
#357169=CARTESIAN_POINT('Ctrl Pts',(1.41597785299994,2.2,-3.90221412000002));
#357170=CARTESIAN_POINT('Ctrl Pts',(1.41676654599994,12.2,-3.90330724300001));
#357171=CARTESIAN_POINT('Ctrl Pts',(1.41676654599994,5.2,-3.90330724300001));
#357172=CARTESIAN_POINT('Ctrl Pts',(1.41676654599994,2.2,-3.90330724300001));
#357173=CARTESIAN_POINT('Ctrl Pts',(1.41755942799994,12.2,-3.90440342500002));
#357174=CARTESIAN_POINT('Ctrl Pts',(1.41755942799994,5.2,-3.90440342500002));
#357175=CARTESIAN_POINT('Ctrl Pts',(1.41755942799994,2.2,-3.90440342500002));
#357176=CARTESIAN_POINT('Ctrl Pts',(1.41835650099994,12.2,-3.90550265100002));
#357177=CARTESIAN_POINT('Ctrl Pts',(1.41835650099994,5.2,-3.90550265100002));
#357178=CARTESIAN_POINT('Ctrl Pts',(1.41835650099994,2.2,-3.90550265100002));
#357179=CARTESIAN_POINT('Ctrl Pts',(1.41915776899994,12.2,-3.90660491100002));
#357180=CARTESIAN_POINT('Ctrl Pts',(1.41915776899994,5.2,-3.90660491100002));
#357181=CARTESIAN_POINT('Ctrl Pts',(1.41915776899994,2.2,-3.90660491100002));
#357182=CARTESIAN_POINT('Ctrl Pts',(1.41996323499994,12.2,-3.90771018600002));
#357183=CARTESIAN_POINT('Ctrl Pts',(1.41996323499994,5.2,-3.90771018600002));
#357184=CARTESIAN_POINT('Ctrl Pts',(1.41996323499994,2.2,-3.90771018600002));
#357185=CARTESIAN_POINT('Ctrl Pts',(1.42077290399994,12.2,-3.90881846700001));
#357186=CARTESIAN_POINT('Ctrl Pts',(1.42077290399994,5.2,-3.90881846700001));
#357187=CARTESIAN_POINT('Ctrl Pts',(1.42077290399994,2.2,-3.90881846700001));
#357188=CARTESIAN_POINT('Ctrl Pts',(1.42158677699994,12.2,-3.90992973900001));
#357189=CARTESIAN_POINT('Ctrl Pts',(1.42158677699994,5.2,-3.90992973900001));
#357190=CARTESIAN_POINT('Ctrl Pts',(1.42158677699994,2.2,-3.90992973900001));
#357191=CARTESIAN_POINT('Ctrl Pts',(1.42240485899994,12.2,-3.91104398600001));
#357192=CARTESIAN_POINT('Ctrl Pts',(1.42240485899994,5.2,-3.91104398600001));
#357193=CARTESIAN_POINT('Ctrl Pts',(1.42240485899994,2.2,-3.91104398600001));
#357194=CARTESIAN_POINT('Ctrl Pts',(1.42322715199994,12.2,-3.91216119700001));
#357195=CARTESIAN_POINT('Ctrl Pts',(1.42322715199994,5.2,-3.91216119700001));
#357196=CARTESIAN_POINT('Ctrl Pts',(1.42322715199994,2.2,-3.91216119700001));
#357197=CARTESIAN_POINT('Ctrl Pts',(1.42405365899994,12.2,-3.91328135700002));
#357198=CARTESIAN_POINT('Ctrl Pts',(1.42405365899994,5.2,-3.91328135700002));
#357199=CARTESIAN_POINT('Ctrl Pts',(1.42405365899994,2.2,-3.91328135700002));
#357200=CARTESIAN_POINT('Ctrl Pts',(1.42488438499994,12.2,-3.91440445300002));
#357201=CARTESIAN_POINT('Ctrl Pts',(1.42488438499994,5.2,-3.91440445300002));
#357202=CARTESIAN_POINT('Ctrl Pts',(1.42488438499994,2.2,-3.91440445300002));
#357203=CARTESIAN_POINT('Ctrl Pts',(1.42571933199994,12.2,-3.91553047100002));
#357204=CARTESIAN_POINT('Ctrl Pts',(1.42571933199994,5.2,-3.91553047100002));
#357205=CARTESIAN_POINT('Ctrl Pts',(1.42571933199994,2.2,-3.91553047100002));
#357206=CARTESIAN_POINT('Ctrl Pts',(1.42655850299994,12.2,-3.91665939700002));
#357207=CARTESIAN_POINT('Ctrl Pts',(1.42655850299994,5.2,-3.91665939700002));
#357208=CARTESIAN_POINT('Ctrl Pts',(1.42655850299994,2.2,-3.91665939700002));
#357209=CARTESIAN_POINT('Ctrl Pts',(1.42740190199994,12.2,-3.91779121900001));
#357210=CARTESIAN_POINT('Ctrl Pts',(1.42740190199994,5.2,-3.91779121900001));
#357211=CARTESIAN_POINT('Ctrl Pts',(1.42740190199994,2.2,-3.91779121900001));
#357212=CARTESIAN_POINT('Ctrl Pts',(1.42824953199994,12.2,-3.91892592300001));
#357213=CARTESIAN_POINT('Ctrl Pts',(1.42824953199994,5.2,-3.91892592300001));
#357214=CARTESIAN_POINT('Ctrl Pts',(1.42824953199994,2.2,-3.91892592300001));
#357215=CARTESIAN_POINT('Ctrl Pts',(1.42910139499994,12.2,-3.92006349400001));
#357216=CARTESIAN_POINT('Ctrl Pts',(1.42910139499994,5.2,-3.92006349400001));
#357217=CARTESIAN_POINT('Ctrl Pts',(1.42910139499994,2.2,-3.92006349400001));
#357218=CARTESIAN_POINT('Ctrl Pts',(1.42995749499994,12.2,-3.92120392000002));
#357219=CARTESIAN_POINT('Ctrl Pts',(1.42995749499994,5.2,-3.92120392000002));
#357220=CARTESIAN_POINT('Ctrl Pts',(1.42995749499994,2.2,-3.92120392000002));
#357221=CARTESIAN_POINT('Ctrl Pts',(1.43081783499994,12.2,-3.92234718700001));
#357222=CARTESIAN_POINT('Ctrl Pts',(1.43081783499994,5.2,-3.92234718700001));
#357223=CARTESIAN_POINT('Ctrl Pts',(1.43081783499994,2.2,-3.92234718700001));
#357224=CARTESIAN_POINT('Ctrl Pts',(1.43168241799994,12.2,-3.92349328200002));
#357225=CARTESIAN_POINT('Ctrl Pts',(1.43168241799994,5.2,-3.92349328200002));
#357226=CARTESIAN_POINT('Ctrl Pts',(1.43168241799994,2.2,-3.92349328200002));
#357227=CARTESIAN_POINT('Ctrl Pts',(1.43255124699994,12.2,-3.92464219200001));
#357228=CARTESIAN_POINT('Ctrl Pts',(1.43255124699994,5.2,-3.92464219200001));
#357229=CARTESIAN_POINT('Ctrl Pts',(1.43255124699994,2.2,-3.92464219200001));
#357230=CARTESIAN_POINT('Ctrl Pts',(1.43342432399994,12.2,-3.92579390100002));
#357231=CARTESIAN_POINT('Ctrl Pts',(1.43342432399994,5.2,-3.92579390100002));
#357232=CARTESIAN_POINT('Ctrl Pts',(1.43342432399994,2.2,-3.92579390100002));
#357233=CARTESIAN_POINT('Ctrl Pts',(1.43430165399994,12.2,-3.92694840000001));
#357234=CARTESIAN_POINT('Ctrl Pts',(1.43430165399994,5.2,-3.92694840000001));
#357235=CARTESIAN_POINT('Ctrl Pts',(1.43430165399994,2.2,-3.92694840000001));
#357236=CARTESIAN_POINT('Ctrl Pts',(1.43518323799994,12.2,-3.92810567100002));
#357237=CARTESIAN_POINT('Ctrl Pts',(1.43518323799994,5.2,-3.92810567100002));
#357238=CARTESIAN_POINT('Ctrl Pts',(1.43518323799994,2.2,-3.92810567100002));
#357239=CARTESIAN_POINT('Ctrl Pts',(1.43606908099994,12.2,-3.92926570500002));
#357240=CARTESIAN_POINT('Ctrl Pts',(1.43606908099994,5.2,-3.92926570500002));
#357241=CARTESIAN_POINT('Ctrl Pts',(1.43606908099994,2.2,-3.92926570500002));
#357242=CARTESIAN_POINT('Ctrl Pts',(1.43695918299994,12.2,-3.93042848500002));
#357243=CARTESIAN_POINT('Ctrl Pts',(1.43695918299994,5.2,-3.93042848500002));
#357244=CARTESIAN_POINT('Ctrl Pts',(1.43695918299994,2.2,-3.93042848500002));
#357245=CARTESIAN_POINT('Ctrl Pts',(1.43785354899994,12.2,-3.93159400000001));
#357246=CARTESIAN_POINT('Ctrl Pts',(1.43785354899994,5.2,-3.93159400000001));
#357247=CARTESIAN_POINT('Ctrl Pts',(1.43785354899994,2.2,-3.93159400000001));
#357248=CARTESIAN_POINT('Ctrl Pts',(1.43875218099994,12.2,-3.93276223700001));
#357249=CARTESIAN_POINT('Ctrl Pts',(1.43875218099994,5.2,-3.93276223700001));
#357250=CARTESIAN_POINT('Ctrl Pts',(1.43875218099994,2.2,-3.93276223700001));
#357251=CARTESIAN_POINT('Ctrl Pts',(1.43965508299994,12.2,-3.93393318100001));
#357252=CARTESIAN_POINT('Ctrl Pts',(1.43965508299994,5.2,-3.93393318100001));
#357253=CARTESIAN_POINT('Ctrl Pts',(1.43965508299994,2.2,-3.93393318100001));
#357254=CARTESIAN_POINT('Ctrl Pts',(1.44056225699994,12.2,-3.93510682000001));
#357255=CARTESIAN_POINT('Ctrl Pts',(1.44056225699994,5.2,-3.93510682000001));
#357256=CARTESIAN_POINT('Ctrl Pts',(1.44056225699994,2.2,-3.93510682000001));
#357257=CARTESIAN_POINT('Ctrl Pts',(1.44147370499994,12.2,-3.93628314200001));
#357258=CARTESIAN_POINT('Ctrl Pts',(1.44147370499994,5.2,-3.93628314200001));
#357259=CARTESIAN_POINT('Ctrl Pts',(1.44147370499994,2.2,-3.93628314200001));
#357260=CARTESIAN_POINT('Ctrl Pts',(1.44238943099994,12.2,-3.93746213100002));
#357261=CARTESIAN_POINT('Ctrl Pts',(1.44238943099994,5.2,-3.93746213100002));
#357262=CARTESIAN_POINT('Ctrl Pts',(1.44238943099994,2.2,-3.93746213100002));
#357263=CARTESIAN_POINT('Ctrl Pts',(1.44330943599994,12.2,-3.93864377500002));
#357264=CARTESIAN_POINT('Ctrl Pts',(1.44330943599994,5.2,-3.93864377500002));
#357265=CARTESIAN_POINT('Ctrl Pts',(1.44330943599994,2.2,-3.93864377500002));
#357266=CARTESIAN_POINT('Ctrl Pts',(1.44423372399994,12.2,-3.93982806200002));
#357267=CARTESIAN_POINT('Ctrl Pts',(1.44423372399994,5.2,-3.93982806200002));
#357268=CARTESIAN_POINT('Ctrl Pts',(1.44423372399994,2.2,-3.93982806200002));
#357269=CARTESIAN_POINT('Ctrl Pts',(1.44516229799994,12.2,-3.94101497900001));
#357270=CARTESIAN_POINT('Ctrl Pts',(1.44516229799994,5.2,-3.94101497900001));
#357271=CARTESIAN_POINT('Ctrl Pts',(1.44516229799994,2.2,-3.94101497900001));
#357272=CARTESIAN_POINT('Ctrl Pts',(1.44609515999994,12.2,-3.94220451100002));
#357273=CARTESIAN_POINT('Ctrl Pts',(1.44609515999994,5.2,-3.94220451100002));
#357274=CARTESIAN_POINT('Ctrl Pts',(1.44609515999994,2.2,-3.94220451100002));
#357275=CARTESIAN_POINT('Ctrl Pts',(1.44703231299994,12.2,-3.94339664700002));
#357276=CARTESIAN_POINT('Ctrl Pts',(1.44703231299994,5.2,-3.94339664700002));
#357277=CARTESIAN_POINT('Ctrl Pts',(1.44703231299994,2.2,-3.94339664700002));
#357278=CARTESIAN_POINT('Ctrl Pts',(1.44797375899994,12.2,-3.94459137300001));
#357279=CARTESIAN_POINT('Ctrl Pts',(1.44797375899994,5.2,-3.94459137300001));
#357280=CARTESIAN_POINT('Ctrl Pts',(1.44797375899994,2.2,-3.94459137300001));
#357281=CARTESIAN_POINT('Ctrl Pts',(1.44891950099994,12.2,-3.94578867600002));
#357282=CARTESIAN_POINT('Ctrl Pts',(1.44891950099994,5.2,-3.94578867600002));
#357283=CARTESIAN_POINT('Ctrl Pts',(1.44891950099994,2.2,-3.94578867600002));
#357284=CARTESIAN_POINT('Ctrl Pts',(1.44986954099994,12.2,-3.94698854300001));
#357285=CARTESIAN_POINT('Ctrl Pts',(1.44986954099994,5.2,-3.94698854300001));
#357286=CARTESIAN_POINT('Ctrl Pts',(1.44986954099994,2.2,-3.94698854300001));
#357287=CARTESIAN_POINT('Ctrl Pts',(1.45082388399994,12.2,-3.94819096100001));
#357288=CARTESIAN_POINT('Ctrl Pts',(1.45082388399994,5.2,-3.94819096100001));
#357289=CARTESIAN_POINT('Ctrl Pts',(1.45082388399994,2.2,-3.94819096100001));
#357290=CARTESIAN_POINT('Ctrl Pts',(1.45178252799994,12.2,-3.94939591800001));
#357291=CARTESIAN_POINT('Ctrl Pts',(1.45178252799994,5.2,-3.94939591800001));
#357292=CARTESIAN_POINT('Ctrl Pts',(1.45178252799994,2.2,-3.94939591800001));
#357293=CARTESIAN_POINT('Ctrl Pts',(1.45274548099994,12.2,-3.95060340000001));
#357294=CARTESIAN_POINT('Ctrl Pts',(1.45274548099994,5.2,-3.95060340000001));
#357295=CARTESIAN_POINT('Ctrl Pts',(1.45274548099994,2.2,-3.95060340000001));
#357296=CARTESIAN_POINT('Ctrl Pts',(1.45371273999994,12.2,-3.95181339600001));
#357297=CARTESIAN_POINT('Ctrl Pts',(1.45371273999994,5.2,-3.95181339600001));
#357298=CARTESIAN_POINT('Ctrl Pts',(1.45371273999994,2.2,-3.95181339600001));
#357299=CARTESIAN_POINT('Ctrl Pts',(1.45468431199994,12.2,-3.95302589000002));
#357300=CARTESIAN_POINT('Ctrl Pts',(1.45468431199994,5.2,-3.95302589000002));
#357301=CARTESIAN_POINT('Ctrl Pts',(1.45468431199994,2.2,-3.95302589000002));
#357302=CARTESIAN_POINT('Ctrl Pts',(1.45566019599994,12.2,-3.95424087200002));
#357303=CARTESIAN_POINT('Ctrl Pts',(1.45566019599994,5.2,-3.95424087200002));
#357304=CARTESIAN_POINT('Ctrl Pts',(1.45566019599994,2.2,-3.95424087200002));
#357305=CARTESIAN_POINT('Ctrl Pts',(1.45664039699994,12.2,-3.95545832800002));
#357306=CARTESIAN_POINT('Ctrl Pts',(1.45664039699994,5.2,-3.95545832800002));
#357307=CARTESIAN_POINT('Ctrl Pts',(1.45664039699994,2.2,-3.95545832800002));
#357308=CARTESIAN_POINT('Ctrl Pts',(1.45762491499994,12.2,-3.95667824600002));
#357309=CARTESIAN_POINT('Ctrl Pts',(1.45762491499994,5.2,-3.95667824600002));
#357310=CARTESIAN_POINT('Ctrl Pts',(1.45762491499994,2.2,-3.95667824600002));
#357311=CARTESIAN_POINT('Ctrl Pts',(1.45861375399994,12.2,-3.95790061100001));
#357312=CARTESIAN_POINT('Ctrl Pts',(1.45861375399994,5.2,-3.95790061100001));
#357313=CARTESIAN_POINT('Ctrl Pts',(1.45861375399994,2.2,-3.95790061100001));
#357314=CARTESIAN_POINT('Ctrl Pts',(1.45960691699994,12.2,-3.95912541200001));
#357315=CARTESIAN_POINT('Ctrl Pts',(1.45960691699994,5.2,-3.95912541200001));
#357316=CARTESIAN_POINT('Ctrl Pts',(1.45960691699994,2.2,-3.95912541200001));
#357317=CARTESIAN_POINT('Ctrl Pts',(1.46060440399994,12.2,-3.96035263700002));
#357318=CARTESIAN_POINT('Ctrl Pts',(1.46060440399994,5.2,-3.96035263700002));
#357319=CARTESIAN_POINT('Ctrl Pts',(1.46060440399994,2.2,-3.96035263700002));
#357320=CARTESIAN_POINT('Ctrl Pts',(1.46160621899994,12.2,-3.96158227200001));
#357321=CARTESIAN_POINT('Ctrl Pts',(1.46160621899994,5.2,-3.96158227200001));
#357322=CARTESIAN_POINT('Ctrl Pts',(1.46160621899994,2.2,-3.96158227200001));
#357323=CARTESIAN_POINT('Ctrl Pts',(1.46261236399994,12.2,-3.96281430500002));
#357324=CARTESIAN_POINT('Ctrl Pts',(1.46261236399994,5.2,-3.96281430500002));
#357325=CARTESIAN_POINT('Ctrl Pts',(1.46261236399994,2.2,-3.96281430500002));
#357326=CARTESIAN_POINT('Ctrl Pts',(1.46362284099994,12.2,-3.96404872300002));
#357327=CARTESIAN_POINT('Ctrl Pts',(1.46362284099994,5.2,-3.96404872300002));
#357328=CARTESIAN_POINT('Ctrl Pts',(1.46362284099994,2.2,-3.96404872300002));
#357329=CARTESIAN_POINT('Ctrl Pts',(1.46463765199994,12.2,-3.96528551300001));
#357330=CARTESIAN_POINT('Ctrl Pts',(1.46463765199994,5.2,-3.96528551300001));
#357331=CARTESIAN_POINT('Ctrl Pts',(1.46463765199994,2.2,-3.96528551300001));
#357332=CARTESIAN_POINT('Ctrl Pts',(1.46565679899994,12.2,-3.96652466400001));
#357333=CARTESIAN_POINT('Ctrl Pts',(1.46565679899994,5.2,-3.96652466400001));
#357334=CARTESIAN_POINT('Ctrl Pts',(1.46565679899994,2.2,-3.96652466400001));
#357335=CARTESIAN_POINT('Ctrl Pts',(1.46668028599994,12.2,-3.96776616100002));
#357336=CARTESIAN_POINT('Ctrl Pts',(1.46668028599994,5.2,-3.96776616100002));
#357337=CARTESIAN_POINT('Ctrl Pts',(1.46668028599994,2.2,-3.96776616100002));
#357338=CARTESIAN_POINT('Ctrl Pts',(1.46770811399994,12.2,-3.96900999400001));
#357339=CARTESIAN_POINT('Ctrl Pts',(1.46770811399994,5.2,-3.96900999400001));
#357340=CARTESIAN_POINT('Ctrl Pts',(1.46770811399994,2.2,-3.96900999400001));
#357341=CARTESIAN_POINT('Ctrl Pts',(1.46874028399994,12.2,-3.97025614800001));
#357342=CARTESIAN_POINT('Ctrl Pts',(1.46874028399994,5.2,-3.97025614800001));
#357343=CARTESIAN_POINT('Ctrl Pts',(1.46874028399994,2.2,-3.97025614800001));
#357344=CARTESIAN_POINT('Ctrl Pts',(1.46977679999994,12.2,-3.97150461300001));
#357345=CARTESIAN_POINT('Ctrl Pts',(1.46977679999994,5.2,-3.97150461300001));
#357346=CARTESIAN_POINT('Ctrl Pts',(1.46977679999994,2.2,-3.97150461300001));
#357347=CARTESIAN_POINT('Ctrl Pts',(1.47081766299994,12.2,-3.97275537400001));
#357348=CARTESIAN_POINT('Ctrl Pts',(1.47081766299994,5.2,-3.97275537400001));
#357349=CARTESIAN_POINT('Ctrl Pts',(1.47081766299994,2.2,-3.97275537400001));
#357350=CARTESIAN_POINT('Ctrl Pts',(1.47186287499994,12.2,-3.97400842000001));
#357351=CARTESIAN_POINT('Ctrl Pts',(1.47186287499994,5.2,-3.97400842000001));
#357352=CARTESIAN_POINT('Ctrl Pts',(1.47186287499994,2.2,-3.97400842000001));
#357353=CARTESIAN_POINT('Ctrl Pts',(1.47291243899994,12.2,-3.97526373800002));
#357354=CARTESIAN_POINT('Ctrl Pts',(1.47291243899994,5.2,-3.97526373800002));
#357355=CARTESIAN_POINT('Ctrl Pts',(1.47291243899994,2.2,-3.97526373800002));
#357356=CARTESIAN_POINT('Ctrl Pts',(1.47396635599994,12.2,-3.97652131600001));
#357357=CARTESIAN_POINT('Ctrl Pts',(1.47396635599994,5.2,-3.97652131600001));
#357358=CARTESIAN_POINT('Ctrl Pts',(1.47396635599994,2.2,-3.97652131600001));
#357359=CARTESIAN_POINT('Ctrl Pts',(1.47502462999994,12.2,-3.97778114100001));
#357360=CARTESIAN_POINT('Ctrl Pts',(1.47502462999994,5.2,-3.97778114100001));
#357361=CARTESIAN_POINT('Ctrl Pts',(1.47502462999994,2.2,-3.97778114100001));
#357362=CARTESIAN_POINT('Ctrl Pts',(1.47608725999994,12.2,-3.97904320100002));
#357363=CARTESIAN_POINT('Ctrl Pts',(1.47608725999994,5.2,-3.97904320100002));
#357364=CARTESIAN_POINT('Ctrl Pts',(1.47608725999994,2.2,-3.97904320100002));
#357365=CARTESIAN_POINT('Ctrl Pts',(1.47715424999994,12.2,-3.98030748400001));
#357366=CARTESIAN_POINT('Ctrl Pts',(1.47715424999994,5.2,-3.98030748400001));
#357367=CARTESIAN_POINT('Ctrl Pts',(1.47715424999994,2.2,-3.98030748400001));
#357368=CARTESIAN_POINT('Ctrl Pts',(1.47822560099994,12.2,-3.98157397600002));
#357369=CARTESIAN_POINT('Ctrl Pts',(1.47822560099994,5.2,-3.98157397600002));
#357370=CARTESIAN_POINT('Ctrl Pts',(1.47822560099994,2.2,-3.98157397600002));
#357371=CARTESIAN_POINT('Ctrl Pts',(1.47930131499994,12.2,-3.98284266800002));
#357372=CARTESIAN_POINT('Ctrl Pts',(1.47930131499994,5.2,-3.98284266800002));
#357373=CARTESIAN_POINT('Ctrl Pts',(1.47930131499994,2.2,-3.98284266800002));
#357374=CARTESIAN_POINT('Ctrl Pts',(1.48038139499994,12.2,-3.98411354400002));
#357375=CARTESIAN_POINT('Ctrl Pts',(1.48038139499994,5.2,-3.98411354400002));
#357376=CARTESIAN_POINT('Ctrl Pts',(1.48038139499994,2.2,-3.98411354400002));
#357377=CARTESIAN_POINT('Ctrl Pts',(1.48146584299994,12.2,-3.98538659300002));
#357378=CARTESIAN_POINT('Ctrl Pts',(1.48146584299994,5.2,-3.98538659300002));
#357379=CARTESIAN_POINT('Ctrl Pts',(1.48146584299994,2.2,-3.98538659300002));
#357380=CARTESIAN_POINT('Ctrl Pts',(1.48255465899994,12.2,-3.98666180400001));
#357381=CARTESIAN_POINT('Ctrl Pts',(1.48255465899994,5.2,-3.98666180400001));
#357382=CARTESIAN_POINT('Ctrl Pts',(1.48255465899994,2.2,-3.98666180400001));
#357383=CARTESIAN_POINT('Ctrl Pts',(1.48364784799994,12.2,-3.98793916300002));
#357384=CARTESIAN_POINT('Ctrl Pts',(1.48364784799994,5.2,-3.98793916300002));
#357385=CARTESIAN_POINT('Ctrl Pts',(1.48364784799994,2.2,-3.98793916300002));
#357386=CARTESIAN_POINT('Ctrl Pts',(1.48474540799994,12.2,-3.98921865900002));
#357387=CARTESIAN_POINT('Ctrl Pts',(1.48474540799994,5.2,-3.98921865900002));
#357388=CARTESIAN_POINT('Ctrl Pts',(1.48474540799994,2.2,-3.98921865900002));
#357389=CARTESIAN_POINT('Ctrl Pts',(1.48584734199994,12.2,-3.99050027900001));
#357390=CARTESIAN_POINT('Ctrl Pts',(1.48584734199994,5.2,-3.99050027900001));
#357391=CARTESIAN_POINT('Ctrl Pts',(1.48584734199994,2.2,-3.99050027900001));
#357392=CARTESIAN_POINT('Ctrl Pts',(1.48695365399994,12.2,-3.99178401100002));
#357393=CARTESIAN_POINT('Ctrl Pts',(1.48695365399994,5.2,-3.99178401100002));
#357394=CARTESIAN_POINT('Ctrl Pts',(1.48695365399994,2.2,-3.99178401100002));
#357395=CARTESIAN_POINT('Ctrl Pts',(1.48806434399994,12.2,-3.99306984300001));
#357396=CARTESIAN_POINT('Ctrl Pts',(1.48806434399994,5.2,-3.99306984300001));
#357397=CARTESIAN_POINT('Ctrl Pts',(1.48806434399994,2.2,-3.99306984300001));
#357398=CARTESIAN_POINT('Ctrl Pts',(1.48917941399994,12.2,-3.99435776200002));
#357399=CARTESIAN_POINT('Ctrl Pts',(1.48917941399994,5.2,-3.99435776200002));
#357400=CARTESIAN_POINT('Ctrl Pts',(1.48917941399994,2.2,-3.99435776200002));
#357401=CARTESIAN_POINT('Ctrl Pts',(1.49029886499994,12.2,-3.99564775700001));
#357402=CARTESIAN_POINT('Ctrl Pts',(1.49029886499994,5.2,-3.99564775700001));
#357403=CARTESIAN_POINT('Ctrl Pts',(1.49029886499994,2.2,-3.99564775700001));
#357404=CARTESIAN_POINT('Ctrl Pts',(1.49142269999994,12.2,-3.99693981600001));
#357405=CARTESIAN_POINT('Ctrl Pts',(1.49142269999994,5.2,-3.99693981600001));
#357406=CARTESIAN_POINT('Ctrl Pts',(1.49142269999994,2.2,-3.99693981600001));
#357407=CARTESIAN_POINT('Ctrl Pts',(1.49255091999994,12.2,-3.99823392700001));
#357408=CARTESIAN_POINT('Ctrl Pts',(1.49255091999994,5.2,-3.99823392700001));
#357409=CARTESIAN_POINT('Ctrl Pts',(1.49255091999994,2.2,-3.99823392700001));
#357410=CARTESIAN_POINT('Ctrl Pts',(1.49368352799994,12.2,-3.99953007600002));
#357411=CARTESIAN_POINT('Ctrl Pts',(1.49368352799994,5.2,-3.99953007600002));
#357412=CARTESIAN_POINT('Ctrl Pts',(1.49368352799994,2.2,-3.99953007600002));
#357413=CARTESIAN_POINT('Ctrl Pts',(1.49482052299994,12.2,-4.00082825200001));
#357414=CARTESIAN_POINT('Ctrl Pts',(1.49482052299994,5.2,-4.00082825200001));
#357415=CARTESIAN_POINT('Ctrl Pts',(1.49482052299994,2.2,-4.00082825200001));
#357416=CARTESIAN_POINT('Ctrl Pts',(1.49596190899994,12.2,-4.00212844500001));
#357417=CARTESIAN_POINT('Ctrl Pts',(1.49596190899994,5.2,-4.00212844500001));
#357418=CARTESIAN_POINT('Ctrl Pts',(1.49596190899994,2.2,-4.00212844500001));
#357419=CARTESIAN_POINT('Ctrl Pts',(1.49710768599994,12.2,-4.00343064000001));
#357420=CARTESIAN_POINT('Ctrl Pts',(1.49710768599994,5.2,-4.00343064000001));
#357421=CARTESIAN_POINT('Ctrl Pts',(1.49710768599994,2.2,-4.00343064000001));
#357422=CARTESIAN_POINT('Ctrl Pts',(1.49825785799994,12.2,-4.00473482600002));
#357423=CARTESIAN_POINT('Ctrl Pts',(1.49825785799994,5.2,-4.00473482600002));
#357424=CARTESIAN_POINT('Ctrl Pts',(1.49825785799994,2.2,-4.00473482600002));
#357425=CARTESIAN_POINT('Ctrl Pts',(1.49941242399994,12.2,-4.00604099200002));
#357426=CARTESIAN_POINT('Ctrl Pts',(1.49941242399994,5.2,-4.00604099200002));
#357427=CARTESIAN_POINT('Ctrl Pts',(1.49941242399994,2.2,-4.00604099200002));
#357428=CARTESIAN_POINT('Ctrl Pts',(1.50057138599994,12.2,-4.00734912400001));
#357429=CARTESIAN_POINT('Ctrl Pts',(1.50057138599994,5.2,-4.00734912400001));
#357430=CARTESIAN_POINT('Ctrl Pts',(1.50057138599994,2.2,-4.00734912400001));
#357431=CARTESIAN_POINT('Ctrl Pts',(1.50173474699994,12.2,-4.00865921200001));
#357432=CARTESIAN_POINT('Ctrl Pts',(1.50173474699994,5.2,-4.00865921200001));
#357433=CARTESIAN_POINT('Ctrl Pts',(1.50173474699994,2.2,-4.00865921200001));
#357434=CARTESIAN_POINT('Ctrl Pts',(1.50290250699994,12.2,-4.00997124400002));
#357435=CARTESIAN_POINT('Ctrl Pts',(1.50290250699994,5.2,-4.00997124400002));
#357436=CARTESIAN_POINT('Ctrl Pts',(1.50290250699994,2.2,-4.00997124400002));
#357437=CARTESIAN_POINT('Ctrl Pts',(1.50407466899994,12.2,-4.01128520700002));
#357438=CARTESIAN_POINT('Ctrl Pts',(1.50407466899994,5.2,-4.01128520700002));
#357439=CARTESIAN_POINT('Ctrl Pts',(1.50407466899994,2.2,-4.01128520700002));
#357440=CARTESIAN_POINT('Ctrl Pts',(1.50525123399994,12.2,-4.01260108900001));
#357441=CARTESIAN_POINT('Ctrl Pts',(1.50525123399994,5.2,-4.01260108900001));
#357442=CARTESIAN_POINT('Ctrl Pts',(1.50525123399994,2.2,-4.01260108900001));
#357443=CARTESIAN_POINT('Ctrl Pts',(1.50643220199994,12.2,-4.01391888000001));
#357444=CARTESIAN_POINT('Ctrl Pts',(1.50643220199994,5.2,-4.01391888000001));
#357445=CARTESIAN_POINT('Ctrl Pts',(1.50643220199994,2.2,-4.01391888000001));
#357446=CARTESIAN_POINT('Ctrl Pts',(1.50761757599994,12.2,-4.01523856600001));
#357447=CARTESIAN_POINT('Ctrl Pts',(1.50761757599994,5.2,-4.01523856600001));
#357448=CARTESIAN_POINT('Ctrl Pts',(1.50761757599994,2.2,-4.01523856600001));
#357449=CARTESIAN_POINT('Ctrl Pts',(1.50880735699994,12.2,-4.01656013600002));
#357450=CARTESIAN_POINT('Ctrl Pts',(1.50880735699994,5.2,-4.01656013600002));
#357451=CARTESIAN_POINT('Ctrl Pts',(1.50880735699994,2.2,-4.01656013600002));
#357452=CARTESIAN_POINT('Ctrl Pts',(1.51000154599994,12.2,-4.01788357900001));
#357453=CARTESIAN_POINT('Ctrl Pts',(1.51000154599994,5.2,-4.01788357900001));
#357454=CARTESIAN_POINT('Ctrl Pts',(1.51000154599994,2.2,-4.01788357900001));
#357455=CARTESIAN_POINT('Ctrl Pts',(1.51120014499994,12.2,-4.01920888300001));
#357456=CARTESIAN_POINT('Ctrl Pts',(1.51120014499994,5.2,-4.01920888300001));
#357457=CARTESIAN_POINT('Ctrl Pts',(1.51120014499994,2.2,-4.01920888300001));
#357458=CARTESIAN_POINT('Ctrl Pts',(1.51240315599994,12.2,-4.02053603400002));
#357459=CARTESIAN_POINT('Ctrl Pts',(1.51240315599994,5.2,-4.02053603400002));
#357460=CARTESIAN_POINT('Ctrl Pts',(1.51240315599994,2.2,-4.02053603400002));
#357461=CARTESIAN_POINT('Ctrl Pts',(1.51361057999994,12.2,-4.02186502300002));
#357462=CARTESIAN_POINT('Ctrl Pts',(1.51361057999994,5.2,-4.02186502300002));
#357463=CARTESIAN_POINT('Ctrl Pts',(1.51361057999994,2.2,-4.02186502300002));
#357464=CARTESIAN_POINT('Ctrl Pts',(1.51482241599994,12.2,-4.02319583700002));
#357465=CARTESIAN_POINT('Ctrl Pts',(1.51482241599994,5.2,-4.02319583700002));
#357466=CARTESIAN_POINT('Ctrl Pts',(1.51482241599994,2.2,-4.02319583700002));
#357467=CARTESIAN_POINT('Ctrl Pts',(1.51603866899994,12.2,-4.02452846500001));
#357468=CARTESIAN_POINT('Ctrl Pts',(1.51603866899994,5.2,-4.02452846500001));
#357469=CARTESIAN_POINT('Ctrl Pts',(1.51603866899994,2.2,-4.02452846500001));
#357470=CARTESIAN_POINT('Ctrl Pts',(1.51725933799994,12.2,-4.02586289400002));
#357471=CARTESIAN_POINT('Ctrl Pts',(1.51725933799994,5.2,-4.02586289400002));
#357472=CARTESIAN_POINT('Ctrl Pts',(1.51725933799994,2.2,-4.02586289400002));
#357473=CARTESIAN_POINT('Ctrl Pts',(1.51848442499994,12.2,-4.02719911400002));
#357474=CARTESIAN_POINT('Ctrl Pts',(1.51848442499994,5.2,-4.02719911400002));
#357475=CARTESIAN_POINT('Ctrl Pts',(1.51848442499994,2.2,-4.02719911400002));
#357476=CARTESIAN_POINT('Ctrl Pts',(1.51971393199994,12.2,-4.02853711200001));
#357477=CARTESIAN_POINT('Ctrl Pts',(1.51971393199994,5.2,-4.02853711200001));
#357478=CARTESIAN_POINT('Ctrl Pts',(1.51971393199994,2.2,-4.02853711200001));
#357479=CARTESIAN_POINT('Ctrl Pts',(1.52094785799994,12.2,-4.02987687700001));
#357480=CARTESIAN_POINT('Ctrl Pts',(1.52094785799994,5.2,-4.02987687700001));
#357481=CARTESIAN_POINT('Ctrl Pts',(1.52094785799994,2.2,-4.02987687700001));
#357482=CARTESIAN_POINT('Ctrl Pts',(1.52218620699994,12.2,-4.03121839800002));
#357483=CARTESIAN_POINT('Ctrl Pts',(1.52218620699994,5.2,-4.03121839800002));
#357484=CARTESIAN_POINT('Ctrl Pts',(1.52218620699994,2.2,-4.03121839800002));
#357485=CARTESIAN_POINT('Ctrl Pts',(1.52342897699994,12.2,-4.03256166200002));
#357486=CARTESIAN_POINT('Ctrl Pts',(1.52342897699994,5.2,-4.03256166200002));
#357487=CARTESIAN_POINT('Ctrl Pts',(1.52342897699994,2.2,-4.03256166200002));
#357488=CARTESIAN_POINT('Ctrl Pts',(1.52467617299994,12.2,-4.03390665700002));
#357489=CARTESIAN_POINT('Ctrl Pts',(1.52467617299994,5.2,-4.03390665700002));
#357490=CARTESIAN_POINT('Ctrl Pts',(1.52467617299994,2.2,-4.03390665700002));
#357491=CARTESIAN_POINT('Ctrl Pts',(1.52592779299994,12.2,-4.03525337300001));
#357492=CARTESIAN_POINT('Ctrl Pts',(1.52592779299994,5.2,-4.03525337300001));
#357493=CARTESIAN_POINT('Ctrl Pts',(1.52592779299994,2.2,-4.03525337300001));
#357494=CARTESIAN_POINT('Ctrl Pts',(1.52718384099994,12.2,-4.03660179900001));
#357495=CARTESIAN_POINT('Ctrl Pts',(1.52718384099994,5.2,-4.03660179900001));
#357496=CARTESIAN_POINT('Ctrl Pts',(1.52718384099994,2.2,-4.03660179900001));
#357497=CARTESIAN_POINT('Ctrl Pts',(1.52844431499994,12.2,-4.03795192300001));
#357498=CARTESIAN_POINT('Ctrl Pts',(1.52844431499994,5.2,-4.03795192300001));
#357499=CARTESIAN_POINT('Ctrl Pts',(1.52844431499994,2.2,-4.03795192300001));
#357500=CARTESIAN_POINT('Ctrl Pts',(1.52970921799994,12.2,-4.03930373100001));
#357501=CARTESIAN_POINT('Ctrl Pts',(1.52970921799994,5.2,-4.03930373100001));
#357502=CARTESIAN_POINT('Ctrl Pts',(1.52970921799994,2.2,-4.03930373100001));
#357503=CARTESIAN_POINT('Ctrl Pts',(1.53097855199994,12.2,-4.04065721500002));
#357504=CARTESIAN_POINT('Ctrl Pts',(1.53097855199994,5.2,-4.04065721500002));
#357505=CARTESIAN_POINT('Ctrl Pts',(1.53097855199994,2.2,-4.04065721500002));
#357506=CARTESIAN_POINT('Ctrl Pts',(1.53225231499994,12.2,-4.04201236100001));
#357507=CARTESIAN_POINT('Ctrl Pts',(1.53225231499994,5.2,-4.04201236100001));
#357508=CARTESIAN_POINT('Ctrl Pts',(1.53225231499994,2.2,-4.04201236100001));
#357509=CARTESIAN_POINT('Ctrl Pts',(1.53353051099994,12.2,-4.04336915800001));
#357510=CARTESIAN_POINT('Ctrl Pts',(1.53353051099994,5.2,-4.04336915800001));
#357511=CARTESIAN_POINT('Ctrl Pts',(1.53353051099994,2.2,-4.04336915800001));
#357512=CARTESIAN_POINT('Ctrl Pts',(1.53481314099994,12.2,-4.04472759700001));
#357513=CARTESIAN_POINT('Ctrl Pts',(1.53481314099994,5.2,-4.04472759700001));
#357514=CARTESIAN_POINT('Ctrl Pts',(1.53481314099994,2.2,-4.04472759700001));
#357515=CARTESIAN_POINT('Ctrl Pts',(1.53610020399994,12.2,-4.04608766400001));
#357516=CARTESIAN_POINT('Ctrl Pts',(1.53610020399994,5.2,-4.04608766400001));
#357517=CARTESIAN_POINT('Ctrl Pts',(1.53610020399994,2.2,-4.04608766400001));
#357518=CARTESIAN_POINT('Ctrl Pts',(1.53739170199994,12.2,-4.04744934700001));
#357519=CARTESIAN_POINT('Ctrl Pts',(1.53739170199994,5.2,-4.04744934700001));
#357520=CARTESIAN_POINT('Ctrl Pts',(1.53739170199994,2.2,-4.04744934700001));
#357521=CARTESIAN_POINT('Ctrl Pts',(1.53868763599994,12.2,-4.04881263700001));
#357522=CARTESIAN_POINT('Ctrl Pts',(1.53868763599994,5.2,-4.04881263700001));
#357523=CARTESIAN_POINT('Ctrl Pts',(1.53868763599994,2.2,-4.04881263700001));
#357524=CARTESIAN_POINT('Ctrl Pts',(1.53998800799994,12.2,-4.05017752100001));
#357525=CARTESIAN_POINT('Ctrl Pts',(1.53998800799994,5.2,-4.05017752100001));
#357526=CARTESIAN_POINT('Ctrl Pts',(1.53998800799994,2.2,-4.05017752100001));
#357527=CARTESIAN_POINT('Ctrl Pts',(1.54129281699994,12.2,-4.05154398900001));
#357528=CARTESIAN_POINT('Ctrl Pts',(1.54129281699994,5.2,-4.05154398900001));
#357529=CARTESIAN_POINT('Ctrl Pts',(1.54129281699994,2.2,-4.05154398900001));
#357530=CARTESIAN_POINT('Ctrl Pts',(1.54260206699994,12.2,-4.05291202800001));
#357531=CARTESIAN_POINT('Ctrl Pts',(1.54260206699994,5.2,-4.05291202800001));
#357532=CARTESIAN_POINT('Ctrl Pts',(1.54260206699994,2.2,-4.05291202800001));
#357533=CARTESIAN_POINT('Ctrl Pts',(1.54391575499994,12.2,-4.05428162800002));
#357534=CARTESIAN_POINT('Ctrl Pts',(1.54391575499994,5.2,-4.05428162800002));
#357535=CARTESIAN_POINT('Ctrl Pts',(1.54391575499994,2.2,-4.05428162800002));
#357536=CARTESIAN_POINT('Ctrl Pts',(1.54523388499994,12.2,-4.05565277800001));
#357537=CARTESIAN_POINT('Ctrl Pts',(1.54523388499994,5.2,-4.05565277800001));
#357538=CARTESIAN_POINT('Ctrl Pts',(1.54523388499994,2.2,-4.05565277800001));
#357539=CARTESIAN_POINT('Ctrl Pts',(1.54655645699994,12.2,-4.05702546500001));
#357540=CARTESIAN_POINT('Ctrl Pts',(1.54655645699994,5.2,-4.05702546500001));
#357541=CARTESIAN_POINT('Ctrl Pts',(1.54655645699994,2.2,-4.05702546500001));
#357542=CARTESIAN_POINT('Ctrl Pts',(1.54788346999994,12.2,-4.05839967900001));
#357543=CARTESIAN_POINT('Ctrl Pts',(1.54788346999994,5.2,-4.05839967900001));
#357544=CARTESIAN_POINT('Ctrl Pts',(1.54788346999994,2.2,-4.05839967900001));
#357545=CARTESIAN_POINT('Ctrl Pts',(1.54921492799994,12.2,-4.05977540800002));
#357546=CARTESIAN_POINT('Ctrl Pts',(1.54921492799994,5.2,-4.05977540800002));
#357547=CARTESIAN_POINT('Ctrl Pts',(1.54921492799994,2.2,-4.05977540800002));
#357548=CARTESIAN_POINT('Ctrl Pts',(1.55055082999994,12.2,-4.06115264200002));
#357549=CARTESIAN_POINT('Ctrl Pts',(1.55055082999994,5.2,-4.06115264200002));
#357550=CARTESIAN_POINT('Ctrl Pts',(1.55055082999994,2.2,-4.06115264200002));
#357551=CARTESIAN_POINT('Ctrl Pts',(1.55189117799994,12.2,-4.06253136800002));
#357552=CARTESIAN_POINT('Ctrl Pts',(1.55189117799994,5.2,-4.06253136800002));
#357553=CARTESIAN_POINT('Ctrl Pts',(1.55189117799994,2.2,-4.06253136800002));
#357554=CARTESIAN_POINT('Ctrl Pts',(1.55323597199994,12.2,-4.06391157600002));
#357555=CARTESIAN_POINT('Ctrl Pts',(1.55323597199994,5.2,-4.06391157600002));
#357556=CARTESIAN_POINT('Ctrl Pts',(1.55323597199994,2.2,-4.06391157600002));
#357557=CARTESIAN_POINT('Ctrl Pts',(1.55458521299994,12.2,-4.06529325500002));
#357558=CARTESIAN_POINT('Ctrl Pts',(1.55458521299994,5.2,-4.06529325500002));
#357559=CARTESIAN_POINT('Ctrl Pts',(1.55458521299994,2.2,-4.06529325500002));
#357560=CARTESIAN_POINT('Ctrl Pts',(1.55593890099994,12.2,-4.06667639400002));
#357561=CARTESIAN_POINT('Ctrl Pts',(1.55593890099994,5.2,-4.06667639400002));
#357562=CARTESIAN_POINT('Ctrl Pts',(1.55593890099994,2.2,-4.06667639400002));
#357563=CARTESIAN_POINT('Ctrl Pts',(1.55729703799994,12.2,-4.06806098100001));
#357564=CARTESIAN_POINT('Ctrl Pts',(1.55729703799994,5.2,-4.06806098100001));
#357565=CARTESIAN_POINT('Ctrl Pts',(1.55729703799994,2.2,-4.06806098100001));
#357566=CARTESIAN_POINT('Ctrl Pts',(1.55865962399994,12.2,-4.06944700500001));
#357567=CARTESIAN_POINT('Ctrl Pts',(1.55865962399994,5.2,-4.06944700500001));
#357568=CARTESIAN_POINT('Ctrl Pts',(1.55865962399994,2.2,-4.06944700500001));
#357569=CARTESIAN_POINT('Ctrl Pts',(1.56002665999994,12.2,-4.07083445600001));
#357570=CARTESIAN_POINT('Ctrl Pts',(1.56002665999994,5.2,-4.07083445600001));
#357571=CARTESIAN_POINT('Ctrl Pts',(1.56002665999994,2.2,-4.07083445600001));
#357572=CARTESIAN_POINT('Ctrl Pts',(1.56139814699994,12.2,-4.07222332200002));
#357573=CARTESIAN_POINT('Ctrl Pts',(1.56139814699994,5.2,-4.07222332200002));
#357574=CARTESIAN_POINT('Ctrl Pts',(1.56139814699994,2.2,-4.07222332200002));
#357575=CARTESIAN_POINT('Ctrl Pts',(1.56277408499994,12.2,-4.07361359200001));
#357576=CARTESIAN_POINT('Ctrl Pts',(1.56277408499994,5.2,-4.07361359200001));
#357577=CARTESIAN_POINT('Ctrl Pts',(1.56277408499994,2.2,-4.07361359200001));
#357578=CARTESIAN_POINT('Ctrl Pts',(1.56415447499994,12.2,-4.07500525400001));
#357579=CARTESIAN_POINT('Ctrl Pts',(1.56415447499994,5.2,-4.07500525400001));
#357580=CARTESIAN_POINT('Ctrl Pts',(1.56415447499994,2.2,-4.07500525400001));
#357581=CARTESIAN_POINT('Ctrl Pts',(1.56553931899994,12.2,-4.07639829800001));
#357582=CARTESIAN_POINT('Ctrl Pts',(1.56553931899994,5.2,-4.07639829800001));
#357583=CARTESIAN_POINT('Ctrl Pts',(1.56553931899994,2.2,-4.07639829800001));
#357584=CARTESIAN_POINT('Ctrl Pts',(1.56692861499994,12.2,-4.07779271500001));
#357585=CARTESIAN_POINT('Ctrl Pts',(1.56692861499994,5.2,-4.07779271500001));
#357586=CARTESIAN_POINT('Ctrl Pts',(1.56692861499994,2.2,-4.07779271500001));
#357587=CARTESIAN_POINT('Ctrl Pts',(1.56832236499994,12.2,-4.07918848900001));
#357588=CARTESIAN_POINT('Ctrl Pts',(1.56832236499994,5.2,-4.07918848900001));
#357589=CARTESIAN_POINT('Ctrl Pts',(1.56832236499994,2.2,-4.07918848900001));
#357590=CARTESIAN_POINT('Ctrl Pts',(1.56972057099994,12.2,-4.08058561400002));
#357591=CARTESIAN_POINT('Ctrl Pts',(1.56972057099994,5.2,-4.08058561400002));
#357592=CARTESIAN_POINT('Ctrl Pts',(1.56972057099994,2.2,-4.08058561400002));
#357593=CARTESIAN_POINT('Ctrl Pts',(1.57112323099994,12.2,-4.08198407600001));
#357594=CARTESIAN_POINT('Ctrl Pts',(1.57112323099994,5.2,-4.08198407600001));
#357595=CARTESIAN_POINT('Ctrl Pts',(1.57112323099994,2.2,-4.08198407600001));
#357596=CARTESIAN_POINT('Ctrl Pts',(1.57253034799994,12.2,-4.08338386600001));
#357597=CARTESIAN_POINT('Ctrl Pts',(1.57253034799994,5.2,-4.08338386600001));
#357598=CARTESIAN_POINT('Ctrl Pts',(1.57253034799994,2.2,-4.08338386600001));
#357599=CARTESIAN_POINT('Ctrl Pts',(1.57394192199994,12.2,-4.08478497100001));
#357600=CARTESIAN_POINT('Ctrl Pts',(1.57394192199994,5.2,-4.08478497100001));
#357601=CARTESIAN_POINT('Ctrl Pts',(1.57394192199994,2.2,-4.08478497100001));
#357602=CARTESIAN_POINT('Ctrl Pts',(1.57535795099994,12.2,-4.08618738200001));
#357603=CARTESIAN_POINT('Ctrl Pts',(1.57535795099994,5.2,-4.08618738200001));
#357604=CARTESIAN_POINT('Ctrl Pts',(1.57535795099994,2.2,-4.08618738200001));
#357605=CARTESIAN_POINT('Ctrl Pts',(1.57677843899994,12.2,-4.08759108600002));
#357606=CARTESIAN_POINT('Ctrl Pts',(1.57677843899994,5.2,-4.08759108600002));
#357607=CARTESIAN_POINT('Ctrl Pts',(1.57677843899994,2.2,-4.08759108600002));
#357608=CARTESIAN_POINT('Ctrl Pts',(1.57820338499994,12.2,-4.08899607600001));
#357609=CARTESIAN_POINT('Ctrl Pts',(1.57820338499994,5.2,-4.08899607600001));
#357610=CARTESIAN_POINT('Ctrl Pts',(1.57820338499994,2.2,-4.08899607600001));
#357611=CARTESIAN_POINT('Ctrl Pts',(1.57963278999994,12.2,-4.09040233600001));
#357612=CARTESIAN_POINT('Ctrl Pts',(1.57963278999994,5.2,-4.09040233600001));
#357613=CARTESIAN_POINT('Ctrl Pts',(1.57963278999994,2.2,-4.09040233600001));
#357614=CARTESIAN_POINT('Ctrl Pts',(1.58106665399994,12.2,-4.09180985900001));
#357615=CARTESIAN_POINT('Ctrl Pts',(1.58106665399994,5.2,-4.09180985900001));
#357616=CARTESIAN_POINT('Ctrl Pts',(1.58106665399994,2.2,-4.09180985900001));
#357617=CARTESIAN_POINT('Ctrl Pts',(1.58250497699994,12.2,-4.09321863300002));
#357618=CARTESIAN_POINT('Ctrl Pts',(1.58250497699994,5.2,-4.09321863300002));
#357619=CARTESIAN_POINT('Ctrl Pts',(1.58250497699994,2.2,-4.09321863300002));
#357620=CARTESIAN_POINT('Ctrl Pts',(1.58394776099994,12.2,-4.09462864600001));
#357621=CARTESIAN_POINT('Ctrl Pts',(1.58394776099994,5.2,-4.09462864600001));
#357622=CARTESIAN_POINT('Ctrl Pts',(1.58394776099994,2.2,-4.09462864600001));
#357623=CARTESIAN_POINT('Ctrl Pts',(1.58539500399994,12.2,-4.09603988900002));
#357624=CARTESIAN_POINT('Ctrl Pts',(1.58539500399994,5.2,-4.09603988900002));
#357625=CARTESIAN_POINT('Ctrl Pts',(1.58539500399994,2.2,-4.09603988900002));
#357626=CARTESIAN_POINT('Ctrl Pts',(1.58684670899994,12.2,-4.09745235000001));
#357627=CARTESIAN_POINT('Ctrl Pts',(1.58684670899994,5.2,-4.09745235000001));
#357628=CARTESIAN_POINT('Ctrl Pts',(1.58684670899994,2.2,-4.09745235000001));
#357629=CARTESIAN_POINT('Ctrl Pts',(1.58830287599994,12.2,-4.09886601900002));
#357630=CARTESIAN_POINT('Ctrl Pts',(1.58830287599994,5.2,-4.09886601900002));
#357631=CARTESIAN_POINT('Ctrl Pts',(1.58830287599994,2.2,-4.09886601900002));
#357632=CARTESIAN_POINT('Ctrl Pts',(1.58976350399994,12.2,-4.10028088500002));
#357633=CARTESIAN_POINT('Ctrl Pts',(1.58976350399994,5.2,-4.10028088500002));
#357634=CARTESIAN_POINT('Ctrl Pts',(1.58976350399994,2.2,-4.10028088500002));
#357635=CARTESIAN_POINT('Ctrl Pts',(1.59122859499994,12.2,-4.10169693700002));
#357636=CARTESIAN_POINT('Ctrl Pts',(1.59122859499994,5.2,-4.10169693700002));
#357637=CARTESIAN_POINT('Ctrl Pts',(1.59122859499994,2.2,-4.10169693700002));
#357638=CARTESIAN_POINT('Ctrl Pts',(1.59269814799994,12.2,-4.10311416500001));
#357639=CARTESIAN_POINT('Ctrl Pts',(1.59269814799994,5.2,-4.10311416500001));
#357640=CARTESIAN_POINT('Ctrl Pts',(1.59269814799994,2.2,-4.10311416500001));
#357641=CARTESIAN_POINT('Ctrl Pts',(1.59417216399994,12.2,-4.10453255700002));
#357642=CARTESIAN_POINT('Ctrl Pts',(1.59417216399994,5.2,-4.10453255700002));
#357643=CARTESIAN_POINT('Ctrl Pts',(1.59417216399994,2.2,-4.10453255700002));
#357644=CARTESIAN_POINT('Ctrl Pts',(1.59565064299994,12.2,-4.10595210300002));
#357645=CARTESIAN_POINT('Ctrl Pts',(1.59565064299994,5.2,-4.10595210300002));
#357646=CARTESIAN_POINT('Ctrl Pts',(1.59565064299994,2.2,-4.10595210300002));
#357647=CARTESIAN_POINT('Ctrl Pts',(1.59713358599994,12.2,-4.10737279300001));
#357648=CARTESIAN_POINT('Ctrl Pts',(1.59713358599994,5.2,-4.10737279300001));
#357649=CARTESIAN_POINT('Ctrl Pts',(1.59713358599994,2.2,-4.10737279300001));
#357650=CARTESIAN_POINT('Ctrl Pts',(1.59862099399994,12.2,-4.10879461600001));
#357651=CARTESIAN_POINT('Ctrl Pts',(1.59862099399994,5.2,-4.10879461600001));
#357652=CARTESIAN_POINT('Ctrl Pts',(1.59862099399994,2.2,-4.10879461600001));
#357653=CARTESIAN_POINT('Ctrl Pts',(1.60011286499994,12.2,-4.11021756100002));
#357654=CARTESIAN_POINT('Ctrl Pts',(1.60011286499994,5.2,-4.11021756100002));
#357655=CARTESIAN_POINT('Ctrl Pts',(1.60011286499994,2.2,-4.11021756100002));
#357656=CARTESIAN_POINT('Ctrl Pts',(1.60160920099994,12.2,-4.11164161700002));
#357657=CARTESIAN_POINT('Ctrl Pts',(1.60160920099994,5.2,-4.11164161700002));
#357658=CARTESIAN_POINT('Ctrl Pts',(1.60160920099994,2.2,-4.11164161700002));
#357659=CARTESIAN_POINT('Ctrl Pts',(1.60311000199994,12.2,-4.11306677500002));
#357660=CARTESIAN_POINT('Ctrl Pts',(1.60311000199994,5.2,-4.11306677500002));
#357661=CARTESIAN_POINT('Ctrl Pts',(1.60311000199994,2.2,-4.11306677500002));
#357662=CARTESIAN_POINT('Ctrl Pts',(1.60461526699994,12.2,-4.11449302300001));
#357663=CARTESIAN_POINT('Ctrl Pts',(1.60461526699994,5.2,-4.11449302300001));
#357664=CARTESIAN_POINT('Ctrl Pts',(1.60461526699994,2.2,-4.11449302300001));
#357665=CARTESIAN_POINT('Ctrl Pts',(1.60612499799994,12.2,-4.11592035000002));
#357666=CARTESIAN_POINT('Ctrl Pts',(1.60612499799994,5.2,-4.11592035000002));
#357667=CARTESIAN_POINT('Ctrl Pts',(1.60612499799994,2.2,-4.11592035000002));
#357668=CARTESIAN_POINT('Ctrl Pts',(1.60763919499994,12.2,-4.11734874700001));
#357669=CARTESIAN_POINT('Ctrl Pts',(1.60763919499994,5.2,-4.11734874700001));
#357670=CARTESIAN_POINT('Ctrl Pts',(1.60763919499994,2.2,-4.11734874700001));
#357671=CARTESIAN_POINT('Ctrl Pts',(1.60915785699994,12.2,-4.11877820300001));
#357672=CARTESIAN_POINT('Ctrl Pts',(1.60915785699994,5.2,-4.11877820300001));
#357673=CARTESIAN_POINT('Ctrl Pts',(1.60915785699994,2.2,-4.11877820300001));
#357674=CARTESIAN_POINT('Ctrl Pts',(1.61068098599994,12.2,-4.12020870600001));
#357675=CARTESIAN_POINT('Ctrl Pts',(1.61068098599994,5.2,-4.12020870600001));
#357676=CARTESIAN_POINT('Ctrl Pts',(1.61068098599994,2.2,-4.12020870600001));
#357677=CARTESIAN_POINT('Ctrl Pts',(1.61220857999994,12.2,-4.12164024700001));
#357678=CARTESIAN_POINT('Ctrl Pts',(1.61220857999994,5.2,-4.12164024700001));
#357679=CARTESIAN_POINT('Ctrl Pts',(1.61220857999994,2.2,-4.12164024700001));
#357680=CARTESIAN_POINT('Ctrl Pts',(1.61374064099994,12.2,-4.12307281500001));
#357681=CARTESIAN_POINT('Ctrl Pts',(1.61374064099994,5.2,-4.12307281500001));
#357682=CARTESIAN_POINT('Ctrl Pts',(1.61374064099994,2.2,-4.12307281500001));
#357683=CARTESIAN_POINT('Ctrl Pts',(1.61527716799994,12.2,-4.12450640100001));
#357684=CARTESIAN_POINT('Ctrl Pts',(1.61527716799994,5.2,-4.12450640100001));
#357685=CARTESIAN_POINT('Ctrl Pts',(1.61527716799994,2.2,-4.12450640100001));
#357686=CARTESIAN_POINT('Ctrl Pts',(1.61681816199994,12.2,-4.12594099200001));
#357687=CARTESIAN_POINT('Ctrl Pts',(1.61681816199994,5.2,-4.12594099200001));
#357688=CARTESIAN_POINT('Ctrl Pts',(1.61681816199994,2.2,-4.12594099200001));
#357689=CARTESIAN_POINT('Ctrl Pts',(1.61836362299994,12.2,-4.12737657900001));
#357690=CARTESIAN_POINT('Ctrl Pts',(1.61836362299994,5.2,-4.12737657900001));
#357691=CARTESIAN_POINT('Ctrl Pts',(1.61836362299994,2.2,-4.12737657900001));
#357692=CARTESIAN_POINT('Ctrl Pts',(1.61991354999994,12.2,-4.12881315000002));
#357693=CARTESIAN_POINT('Ctrl Pts',(1.61991354999994,5.2,-4.12881315000002));
#357694=CARTESIAN_POINT('Ctrl Pts',(1.61991354999994,2.2,-4.12881315000002));
#357695=CARTESIAN_POINT('Ctrl Pts',(1.62146794399994,12.2,-4.13025069800002));
#357696=CARTESIAN_POINT('Ctrl Pts',(1.62146794399994,5.2,-4.13025069800002));
#357697=CARTESIAN_POINT('Ctrl Pts',(1.62146794399994,2.2,-4.13025069800002));
#357698=CARTESIAN_POINT('Ctrl Pts',(1.62302680599994,12.2,-4.13168921000001));
#357699=CARTESIAN_POINT('Ctrl Pts',(1.62302680599994,5.2,-4.13168921000001));
#357700=CARTESIAN_POINT('Ctrl Pts',(1.62302680599994,2.2,-4.13168921000001));
#357701=CARTESIAN_POINT('Ctrl Pts',(1.62459013399994,12.2,-4.13312867500002));
#357702=CARTESIAN_POINT('Ctrl Pts',(1.62459013399994,5.2,-4.13312867500002));
#357703=CARTESIAN_POINT('Ctrl Pts',(1.62459013399994,2.2,-4.13312867500002));
#357704=CARTESIAN_POINT('Ctrl Pts',(1.62615792899994,12.2,-4.13456908500001));
#357705=CARTESIAN_POINT('Ctrl Pts',(1.62615792899994,5.2,-4.13456908500001));
#357706=CARTESIAN_POINT('Ctrl Pts',(1.62615792899994,2.2,-4.13456908500001));
#357707=CARTESIAN_POINT('Ctrl Pts',(1.62773019199994,12.2,-4.13601042800002));
#357708=CARTESIAN_POINT('Ctrl Pts',(1.62773019199994,5.2,-4.13601042800002));
#357709=CARTESIAN_POINT('Ctrl Pts',(1.62773019199994,2.2,-4.13601042800002));
#357710=CARTESIAN_POINT('Ctrl Pts',(1.62930692199994,12.2,-4.13745269500001));
#357711=CARTESIAN_POINT('Ctrl Pts',(1.62930692199994,5.2,-4.13745269500001));
#357712=CARTESIAN_POINT('Ctrl Pts',(1.62930692199994,2.2,-4.13745269500001));
#357713=CARTESIAN_POINT('Ctrl Pts',(1.63088811899994,12.2,-4.13889587300002));
#357714=CARTESIAN_POINT('Ctrl Pts',(1.63088811899994,5.2,-4.13889587300002));
#357715=CARTESIAN_POINT('Ctrl Pts',(1.63088811899994,2.2,-4.13889587300002));
#357716=CARTESIAN_POINT('Ctrl Pts',(1.63247378299994,12.2,-4.14033995500001));
#357717=CARTESIAN_POINT('Ctrl Pts',(1.63247378299994,5.2,-4.14033995500001));
#357718=CARTESIAN_POINT('Ctrl Pts',(1.63247378299994,2.2,-4.14033995500001));
#357719=CARTESIAN_POINT('Ctrl Pts',(1.63406391499994,12.2,-4.14178492800001));
#357720=CARTESIAN_POINT('Ctrl Pts',(1.63406391499994,5.2,-4.14178492800001));
#357721=CARTESIAN_POINT('Ctrl Pts',(1.63406391499994,2.2,-4.14178492800001));
#357722=CARTESIAN_POINT('Ctrl Pts',(1.63565851299994,12.2,-4.14323078500002));
#357723=CARTESIAN_POINT('Ctrl Pts',(1.63565851299994,5.2,-4.14323078500002));
#357724=CARTESIAN_POINT('Ctrl Pts',(1.63565851299994,2.2,-4.14323078500002));
#357725=CARTESIAN_POINT('Ctrl Pts',(1.63725757899994,12.2,-4.14467751100001));
#357726=CARTESIAN_POINT('Ctrl Pts',(1.63725757899994,5.2,-4.14467751100001));
#357727=CARTESIAN_POINT('Ctrl Pts',(1.63725757899994,2.2,-4.14467751100001));
#357728=CARTESIAN_POINT('Ctrl Pts',(1.63886111099994,12.2,-4.14612510000001));
#357729=CARTESIAN_POINT('Ctrl Pts',(1.63886111099994,5.2,-4.14612510000001));
#357730=CARTESIAN_POINT('Ctrl Pts',(1.63886111099994,2.2,-4.14612510000001));
#357731=CARTESIAN_POINT('Ctrl Pts',(1.64046911099994,12.2,-4.14757353900002));
#357732=CARTESIAN_POINT('Ctrl Pts',(1.64046911099994,5.2,-4.14757353900002));
#357733=CARTESIAN_POINT('Ctrl Pts',(1.64046911099994,2.2,-4.14757353900002));
#357734=CARTESIAN_POINT('Ctrl Pts',(1.64208157799994,12.2,-4.14902282000002));
#357735=CARTESIAN_POINT('Ctrl Pts',(1.64208157799994,5.2,-4.14902282000002));
#357736=CARTESIAN_POINT('Ctrl Pts',(1.64208157799994,2.2,-4.14902282000002));
#357737=CARTESIAN_POINT('Ctrl Pts',(1.64369851099994,12.2,-4.15047293100002));
#357738=CARTESIAN_POINT('Ctrl Pts',(1.64369851099994,5.2,-4.15047293100002));
#357739=CARTESIAN_POINT('Ctrl Pts',(1.64369851099994,2.2,-4.15047293100002));
#357740=CARTESIAN_POINT('Ctrl Pts',(1.64531990999994,12.2,-4.15192386300001));
#357741=CARTESIAN_POINT('Ctrl Pts',(1.64531990999994,5.2,-4.15192386300001));
#357742=CARTESIAN_POINT('Ctrl Pts',(1.64531990999994,2.2,-4.15192386300001));
#357743=CARTESIAN_POINT('Ctrl Pts',(1.64694577699994,12.2,-4.15337560500001));
#357744=CARTESIAN_POINT('Ctrl Pts',(1.64694577699994,5.2,-4.15337560500001));
#357745=CARTESIAN_POINT('Ctrl Pts',(1.64694577699994,2.2,-4.15337560500001));
#357746=CARTESIAN_POINT('Ctrl Pts',(1.64857610999994,12.2,-4.15482814800002));
#357747=CARTESIAN_POINT('Ctrl Pts',(1.64857610999994,5.2,-4.15482814800002));
#357748=CARTESIAN_POINT('Ctrl Pts',(1.64857610999994,2.2,-4.15482814800002));
#357749=CARTESIAN_POINT('Ctrl Pts',(1.65021090999994,12.2,-4.15628148000001));
#357750=CARTESIAN_POINT('Ctrl Pts',(1.65021090999994,5.2,-4.15628148000001));
#357751=CARTESIAN_POINT('Ctrl Pts',(1.65021090999994,2.2,-4.15628148000001));
#357752=CARTESIAN_POINT('Ctrl Pts',(1.65185017399994,12.2,-4.15773559300002));
#357753=CARTESIAN_POINT('Ctrl Pts',(1.65185017399994,5.2,-4.15773559300002));
#357754=CARTESIAN_POINT('Ctrl Pts',(1.65185017399994,2.2,-4.15773559300002));
#357755=CARTESIAN_POINT('Ctrl Pts',(1.65349390499994,12.2,-4.15919047500001));
#357756=CARTESIAN_POINT('Ctrl Pts',(1.65349390499994,5.2,-4.15919047500001));
#357757=CARTESIAN_POINT('Ctrl Pts',(1.65349390499994,2.2,-4.15919047500001));
#357758=CARTESIAN_POINT('Ctrl Pts',(1.65514210199994,12.2,-4.16064611800001));
#357759=CARTESIAN_POINT('Ctrl Pts',(1.65514210199994,5.2,-4.16064611800001));
#357760=CARTESIAN_POINT('Ctrl Pts',(1.65514210199994,2.2,-4.16064611800001));
#357761=CARTESIAN_POINT('Ctrl Pts',(1.65679476399994,12.2,-4.16210250900001));
#357762=CARTESIAN_POINT('Ctrl Pts',(1.65679476399994,5.2,-4.16210250900001));
#357763=CARTESIAN_POINT('Ctrl Pts',(1.65679476399994,2.2,-4.16210250900001));
#357764=CARTESIAN_POINT('Ctrl Pts',(1.65845189099994,12.2,-4.16355964100001));
#357765=CARTESIAN_POINT('Ctrl Pts',(1.65845189099994,5.2,-4.16355964100001));
#357766=CARTESIAN_POINT('Ctrl Pts',(1.65845189099994,2.2,-4.16355964100001));
#357767=CARTESIAN_POINT('Ctrl Pts',(1.66011348299994,12.2,-4.16501750200001));
#357768=CARTESIAN_POINT('Ctrl Pts',(1.66011348299994,5.2,-4.16501750200001));
#357769=CARTESIAN_POINT('Ctrl Pts',(1.66011348299994,2.2,-4.16501750200001));
#357770=CARTESIAN_POINT('Ctrl Pts',(1.66177954099994,12.2,-4.16647608300002));
#357771=CARTESIAN_POINT('Ctrl Pts',(1.66177954099994,5.2,-4.16647608300002));
#357772=CARTESIAN_POINT('Ctrl Pts',(1.66177954099994,2.2,-4.16647608300002));
#357773=CARTESIAN_POINT('Ctrl Pts',(1.66345006199994,12.2,-4.16793537300002));
#357774=CARTESIAN_POINT('Ctrl Pts',(1.66345006199994,5.2,-4.16793537300002));
#357775=CARTESIAN_POINT('Ctrl Pts',(1.66345006199994,2.2,-4.16793537300002));
#357776=CARTESIAN_POINT('Ctrl Pts',(1.66512504799994,12.2,-4.16939536200001));
#357777=CARTESIAN_POINT('Ctrl Pts',(1.66512504799994,5.2,-4.16939536200001));
#357778=CARTESIAN_POINT('Ctrl Pts',(1.66512504799994,2.2,-4.16939536200001));
#357779=CARTESIAN_POINT('Ctrl Pts',(1.66680449799994,12.2,-4.17085604100001));
#357780=CARTESIAN_POINT('Ctrl Pts',(1.66680449799994,5.2,-4.17085604100001));
#357781=CARTESIAN_POINT('Ctrl Pts',(1.66680449799994,2.2,-4.17085604100001));
#357782=CARTESIAN_POINT('Ctrl Pts',(1.66848840999994,12.2,-4.17231740000001));
#357783=CARTESIAN_POINT('Ctrl Pts',(1.66848840999994,5.2,-4.17231740000001));
#357784=CARTESIAN_POINT('Ctrl Pts',(1.66848840999994,2.2,-4.17231740000001));
#357785=CARTESIAN_POINT('Ctrl Pts',(1.67017678699994,12.2,-4.17377942800002));
#357786=CARTESIAN_POINT('Ctrl Pts',(1.67017678699994,5.2,-4.17377942800002));
#357787=CARTESIAN_POINT('Ctrl Pts',(1.67017678699994,2.2,-4.17377942800002));
#357788=CARTESIAN_POINT('Ctrl Pts',(1.67186962599994,12.2,-4.17524211600002));
#357789=CARTESIAN_POINT('Ctrl Pts',(1.67186962599994,5.2,-4.17524211600002));
#357790=CARTESIAN_POINT('Ctrl Pts',(1.67186962599994,2.2,-4.17524211600002));
#357791=CARTESIAN_POINT('Ctrl Pts',(1.67356692799994,12.2,-4.17670545400001));
#357792=CARTESIAN_POINT('Ctrl Pts',(1.67356692799994,5.2,-4.17670545400001));
#357793=CARTESIAN_POINT('Ctrl Pts',(1.67356692799994,2.2,-4.17670545400001));
#357794=CARTESIAN_POINT('Ctrl Pts',(1.67526869299994,12.2,-4.17816943100001));
#357795=CARTESIAN_POINT('Ctrl Pts',(1.67526869299994,5.2,-4.17816943100001));
#357796=CARTESIAN_POINT('Ctrl Pts',(1.67526869299994,2.2,-4.17816943100001));
#357797=CARTESIAN_POINT('Ctrl Pts',(1.67697491899994,12.2,-4.17963403800002));
#357798=CARTESIAN_POINT('Ctrl Pts',(1.67697491899994,5.2,-4.17963403800002));
#357799=CARTESIAN_POINT('Ctrl Pts',(1.67697491899994,2.2,-4.17963403800002));
#357800=CARTESIAN_POINT('Ctrl Pts',(1.67868560699994,12.2,-4.18109926600001));
#357801=CARTESIAN_POINT('Ctrl Pts',(1.67868560699994,5.2,-4.18109926600001));
#357802=CARTESIAN_POINT('Ctrl Pts',(1.67868560699994,2.2,-4.18109926600001));
#357803=CARTESIAN_POINT('Ctrl Pts',(1.68040075599994,12.2,-4.18256510300001));
#357804=CARTESIAN_POINT('Ctrl Pts',(1.68040075599994,5.2,-4.18256510300001));
#357805=CARTESIAN_POINT('Ctrl Pts',(1.68040075599994,2.2,-4.18256510300001));
#357806=CARTESIAN_POINT('Ctrl Pts',(1.68212036499994,12.2,-4.18403154100002));
#357807=CARTESIAN_POINT('Ctrl Pts',(1.68212036499994,5.2,-4.18403154100002));
#357808=CARTESIAN_POINT('Ctrl Pts',(1.68212036499994,2.2,-4.18403154100002));
#357809=CARTESIAN_POINT('Ctrl Pts',(1.68384443399994,12.2,-4.18549856900002));
#357810=CARTESIAN_POINT('Ctrl Pts',(1.68384443399994,5.2,-4.18549856900002));
#357811=CARTESIAN_POINT('Ctrl Pts',(1.68384443399994,2.2,-4.18549856900002));
#357812=CARTESIAN_POINT('Ctrl Pts',(1.68557296399995,12.2,-4.18696617800002));
#357813=CARTESIAN_POINT('Ctrl Pts',(1.68557296399995,5.2,-4.18696617800002));
#357814=CARTESIAN_POINT('Ctrl Pts',(1.68557296399995,2.2,-4.18696617800002));
#357815=CARTESIAN_POINT('Ctrl Pts',(1.68730595299994,12.2,-4.18843435700001));
#357816=CARTESIAN_POINT('Ctrl Pts',(1.68730595299994,5.2,-4.18843435700001));
#357817=CARTESIAN_POINT('Ctrl Pts',(1.68730595299994,2.2,-4.18843435700001));
#357818=CARTESIAN_POINT('Ctrl Pts',(1.68904340099994,12.2,-4.18990309800002));
#357819=CARTESIAN_POINT('Ctrl Pts',(1.68904340099994,5.2,-4.18990309800002));
#357820=CARTESIAN_POINT('Ctrl Pts',(1.68904340099994,2.2,-4.18990309800002));
#357821=CARTESIAN_POINT('Ctrl Pts',(1.69078530699994,12.2,-4.19137238900001));
#357822=CARTESIAN_POINT('Ctrl Pts',(1.69078530699994,5.2,-4.19137238900001));
#357823=CARTESIAN_POINT('Ctrl Pts',(1.69078530699994,2.2,-4.19137238900001));
#357824=CARTESIAN_POINT('Ctrl Pts',(1.69253167099994,12.2,-4.19284222200002));
#357825=CARTESIAN_POINT('Ctrl Pts',(1.69253167099994,5.2,-4.19284222200002));
#357826=CARTESIAN_POINT('Ctrl Pts',(1.69253167099994,2.2,-4.19284222200002));
#357827=CARTESIAN_POINT('Ctrl Pts',(1.69428249199994,12.2,-4.19431258800001));
#357828=CARTESIAN_POINT('Ctrl Pts',(1.69428249199994,5.2,-4.19431258800001));
#357829=CARTESIAN_POINT('Ctrl Pts',(1.69428249199994,2.2,-4.19431258800001));
#357830=CARTESIAN_POINT('Ctrl Pts',(1.69603777099994,12.2,-4.19578347300002));
#357831=CARTESIAN_POINT('Ctrl Pts',(1.69603777099994,5.2,-4.19578347300002));
#357832=CARTESIAN_POINT('Ctrl Pts',(1.69603777099994,2.2,-4.19578347300002));
#357833=CARTESIAN_POINT('Ctrl Pts',(1.69779750599994,12.2,-4.19725487200001));
#357834=CARTESIAN_POINT('Ctrl Pts',(1.69779750599994,5.2,-4.19725487200001));
#357835=CARTESIAN_POINT('Ctrl Pts',(1.69779750599994,2.2,-4.19725487200001));
#357836=CARTESIAN_POINT('Ctrl Pts',(1.69956169599994,12.2,-4.19872677300001));
#357837=CARTESIAN_POINT('Ctrl Pts',(1.69956169599994,5.2,-4.19872677300001));
#357838=CARTESIAN_POINT('Ctrl Pts',(1.69956169599994,2.2,-4.19872677300001));
#357839=CARTESIAN_POINT('Ctrl Pts',(1.70133034199994,12.2,-4.20019916800001));
#357840=CARTESIAN_POINT('Ctrl Pts',(1.70133034199994,5.2,-4.20019916800001));
#357841=CARTESIAN_POINT('Ctrl Pts',(1.70133034199994,2.2,-4.20019916800001));
#357842=CARTESIAN_POINT('Ctrl Pts',(1.70310344299994,12.2,-4.20167204400002));
#357843=CARTESIAN_POINT('Ctrl Pts',(1.70310344299994,5.2,-4.20167204400002));
#357844=CARTESIAN_POINT('Ctrl Pts',(1.70310344299994,2.2,-4.20167204400002));
#357845=CARTESIAN_POINT('Ctrl Pts',(1.70488099799994,12.2,-4.20314539500001));
#357846=CARTESIAN_POINT('Ctrl Pts',(1.70488099799994,5.2,-4.20314539500001));
#357847=CARTESIAN_POINT('Ctrl Pts',(1.70488099799994,2.2,-4.20314539500001));
#357848=CARTESIAN_POINT('Ctrl Pts',(1.70666300699994,12.2,-4.20461920900001));
#357849=CARTESIAN_POINT('Ctrl Pts',(1.70666300699994,5.2,-4.20461920900001));
#357850=CARTESIAN_POINT('Ctrl Pts',(1.70666300699994,2.2,-4.20461920900001));
#357851=CARTESIAN_POINT('Ctrl Pts',(1.70844946899994,12.2,-4.20609347800001));
#357852=CARTESIAN_POINT('Ctrl Pts',(1.70844946899994,5.2,-4.20609347800001));
#357853=CARTESIAN_POINT('Ctrl Pts',(1.70844946899994,2.2,-4.20609347800001));
#357854=CARTESIAN_POINT('Ctrl Pts',(1.71024038299994,12.2,-4.20756819000002));
#357855=CARTESIAN_POINT('Ctrl Pts',(1.71024038299994,5.2,-4.20756819000002));
#357856=CARTESIAN_POINT('Ctrl Pts',(1.71024038299994,2.2,-4.20756819000002));
#357857=CARTESIAN_POINT('Ctrl Pts',(1.71203574899994,12.2,-4.20904333800001));
#357858=CARTESIAN_POINT('Ctrl Pts',(1.71203574899994,5.2,-4.20904333800001));
#357859=CARTESIAN_POINT('Ctrl Pts',(1.71203574899994,2.2,-4.20904333800001));
#357860=CARTESIAN_POINT('Ctrl Pts',(1.71383556599994,12.2,-4.21051891000001));
#357861=CARTESIAN_POINT('Ctrl Pts',(1.71383556599994,5.2,-4.21051891000001));
#357862=CARTESIAN_POINT('Ctrl Pts',(1.71383556599994,2.2,-4.21051891000001));
#357863=CARTESIAN_POINT('Ctrl Pts',(1.71563983299994,12.2,-4.21199489900001));
#357864=CARTESIAN_POINT('Ctrl Pts',(1.71563983299994,5.2,-4.21199489900001));
#357865=CARTESIAN_POINT('Ctrl Pts',(1.71563983299994,2.2,-4.21199489900001));
#357866=CARTESIAN_POINT('Ctrl Pts',(1.71744855099994,12.2,-4.21347129300001));
#357867=CARTESIAN_POINT('Ctrl Pts',(1.71744855099994,5.2,-4.21347129300001));
#357868=CARTESIAN_POINT('Ctrl Pts',(1.71744855099994,2.2,-4.21347129300001));
#357869=CARTESIAN_POINT('Ctrl Pts',(1.71926171599994,12.2,-4.21494808400002));
#357870=CARTESIAN_POINT('Ctrl Pts',(1.71926171599994,5.2,-4.21494808400002));
#357871=CARTESIAN_POINT('Ctrl Pts',(1.71926171599994,2.2,-4.21494808400002));
#357872=CARTESIAN_POINT('Ctrl Pts',(1.72107933099995,12.2,-4.21642526200001));
#357873=CARTESIAN_POINT('Ctrl Pts',(1.72107933099995,5.2,-4.21642526200001));
#357874=CARTESIAN_POINT('Ctrl Pts',(1.72107933099995,2.2,-4.21642526200001));
#357875=CARTESIAN_POINT('Ctrl Pts',(1.72290139399994,12.2,-4.21790281800002));
#357876=CARTESIAN_POINT('Ctrl Pts',(1.72290139399994,5.2,-4.21790281800002));
#357877=CARTESIAN_POINT('Ctrl Pts',(1.72290139399994,2.2,-4.21790281800002));
#357878=CARTESIAN_POINT('Ctrl Pts',(1.72472790399994,12.2,-4.21938074100002));
#357879=CARTESIAN_POINT('Ctrl Pts',(1.72472790399994,5.2,-4.21938074100002));
#357880=CARTESIAN_POINT('Ctrl Pts',(1.72472790399994,2.2,-4.21938074100002));
#357881=CARTESIAN_POINT('Ctrl Pts',(1.72655885999994,12.2,-4.22085902300001));
#357882=CARTESIAN_POINT('Ctrl Pts',(1.72655885999994,5.2,-4.22085902300001));
#357883=CARTESIAN_POINT('Ctrl Pts',(1.72655885999994,2.2,-4.22085902300001));
#357884=CARTESIAN_POINT('Ctrl Pts',(1.72839426199994,12.2,-4.22233765400001));
#357885=CARTESIAN_POINT('Ctrl Pts',(1.72839426199994,5.2,-4.22233765400001));
#357886=CARTESIAN_POINT('Ctrl Pts',(1.72839426199994,2.2,-4.22233765400001));
#357887=CARTESIAN_POINT('Ctrl Pts',(1.73023410699994,12.2,-4.22381662300001));
#357888=CARTESIAN_POINT('Ctrl Pts',(1.73023410699994,5.2,-4.22381662300001));
#357889=CARTESIAN_POINT('Ctrl Pts',(1.73023410699994,2.2,-4.22381662300001));
#357890=CARTESIAN_POINT('Ctrl Pts',(1.73207839799994,12.2,-4.22529592300001));
#357891=CARTESIAN_POINT('Ctrl Pts',(1.73207839799994,5.2,-4.22529592300001));
#357892=CARTESIAN_POINT('Ctrl Pts',(1.73207839799994,2.2,-4.22529592300001));
#357893=CARTESIAN_POINT('Ctrl Pts',(1.73392713099994,12.2,-4.22677554400002));
#357894=CARTESIAN_POINT('Ctrl Pts',(1.73392713099994,5.2,-4.22677554400002));
#357895=CARTESIAN_POINT('Ctrl Pts',(1.73392713099994,2.2,-4.22677554400002));
#357896=CARTESIAN_POINT('Ctrl Pts',(1.73578030799994,12.2,-4.22825547500001));
#357897=CARTESIAN_POINT('Ctrl Pts',(1.73578030799994,5.2,-4.22825547500001));
#357898=CARTESIAN_POINT('Ctrl Pts',(1.73578030799994,2.2,-4.22825547500001));
#357899=CARTESIAN_POINT('Ctrl Pts',(1.73763792599994,12.2,-4.22973570900002));
#357900=CARTESIAN_POINT('Ctrl Pts',(1.73763792599994,5.2,-4.22973570900002));
#357901=CARTESIAN_POINT('Ctrl Pts',(1.73763792599994,2.2,-4.22973570900002));
#357902=CARTESIAN_POINT('Ctrl Pts',(1.73949998499994,12.2,-4.23121623300001));
#357903=CARTESIAN_POINT('Ctrl Pts',(1.73949998499994,5.2,-4.23121623300001));
#357904=CARTESIAN_POINT('Ctrl Pts',(1.73949998499994,2.2,-4.23121623300001));
#357905=CARTESIAN_POINT('Ctrl Pts',(1.74136648399994,12.2,-4.23269704200001));
#357906=CARTESIAN_POINT('Ctrl Pts',(1.74136648399994,5.2,-4.23269704200001));
#357907=CARTESIAN_POINT('Ctrl Pts',(1.74136648399994,2.2,-4.23269704200001));
#357908=CARTESIAN_POINT('Ctrl Pts',(1.74323742199994,12.2,-4.23417812300002));
#357909=CARTESIAN_POINT('Ctrl Pts',(1.74323742199994,5.2,-4.23417812300002));
#357910=CARTESIAN_POINT('Ctrl Pts',(1.74323742199994,2.2,-4.23417812300002));
#357911=CARTESIAN_POINT('Ctrl Pts',(1.74511279899994,12.2,-4.23565947000001));
#357912=CARTESIAN_POINT('Ctrl Pts',(1.74511279899994,5.2,-4.23565947000001));
#357913=CARTESIAN_POINT('Ctrl Pts',(1.74511279899994,2.2,-4.23565947000001));
#357914=CARTESIAN_POINT('Ctrl Pts',(1.74699261299994,12.2,-4.23714107000002));
#357915=CARTESIAN_POINT('Ctrl Pts',(1.74699261299994,5.2,-4.23714107000002));
#357916=CARTESIAN_POINT('Ctrl Pts',(1.74699261299994,2.2,-4.23714107000002));
#357917=CARTESIAN_POINT('Ctrl Pts',(1.74887686499994,12.2,-4.23862291600001));
#357918=CARTESIAN_POINT('Ctrl Pts',(1.74887686499994,5.2,-4.23862291600001));
#357919=CARTESIAN_POINT('Ctrl Pts',(1.74887686499994,2.2,-4.23862291600001));
#357920=CARTESIAN_POINT('Ctrl Pts',(1.75076555099994,12.2,-4.24010499800001));
#357921=CARTESIAN_POINT('Ctrl Pts',(1.75076555099994,5.2,-4.24010499800001));
#357922=CARTESIAN_POINT('Ctrl Pts',(1.75076555099994,2.2,-4.24010499800001));
#357923=CARTESIAN_POINT('Ctrl Pts',(1.75265867299994,12.2,-4.24158730600002));
#357924=CARTESIAN_POINT('Ctrl Pts',(1.75265867299994,5.2,-4.24158730600002));
#357925=CARTESIAN_POINT('Ctrl Pts',(1.75265867299994,2.2,-4.24158730600002));
#357926=CARTESIAN_POINT('Ctrl Pts',(1.75455622899995,12.2,-4.24306983200001));
#357927=CARTESIAN_POINT('Ctrl Pts',(1.75455622899995,5.2,-4.24306983200001));
#357928=CARTESIAN_POINT('Ctrl Pts',(1.75455622899995,2.2,-4.24306983200001));
#357929=CARTESIAN_POINT('Ctrl Pts',(1.75645821799994,12.2,-4.24455256600002));
#357930=CARTESIAN_POINT('Ctrl Pts',(1.75645821799994,5.2,-4.24455256600002));
#357931=CARTESIAN_POINT('Ctrl Pts',(1.75645821799994,2.2,-4.24455256600002));
#357932=CARTESIAN_POINT('Ctrl Pts',(1.75836463899994,12.2,-4.24603550000001));
#357933=CARTESIAN_POINT('Ctrl Pts',(1.75836463899994,5.2,-4.24603550000001));
#357934=CARTESIAN_POINT('Ctrl Pts',(1.75836463899994,2.2,-4.24603550000001));
#357935=CARTESIAN_POINT('Ctrl Pts',(1.76027549299994,12.2,-4.24751862300001));
#357936=CARTESIAN_POINT('Ctrl Pts',(1.76027549299994,5.2,-4.24751862300001));
#357937=CARTESIAN_POINT('Ctrl Pts',(1.76027549299994,2.2,-4.24751862300001));
#357938=CARTESIAN_POINT('Ctrl Pts',(1.76219077499994,12.2,-4.24900192600001));
#357939=CARTESIAN_POINT('Ctrl Pts',(1.76219077499994,5.2,-4.24900192600001));
#357940=CARTESIAN_POINT('Ctrl Pts',(1.76219077499994,2.2,-4.24900192600001));
#357941=CARTESIAN_POINT('Ctrl Pts',(1.76411048799994,12.2,-4.25048540000001));
#357942=CARTESIAN_POINT('Ctrl Pts',(1.76411048799994,5.2,-4.25048540000001));
#357943=CARTESIAN_POINT('Ctrl Pts',(1.76411048799994,2.2,-4.25048540000001));
#357944=CARTESIAN_POINT('Ctrl Pts',(1.76603462799994,12.2,-4.25196903500002));
#357945=CARTESIAN_POINT('Ctrl Pts',(1.76603462799994,5.2,-4.25196903500002));
#357946=CARTESIAN_POINT('Ctrl Pts',(1.76603462799994,2.2,-4.25196903500002));
#357947=CARTESIAN_POINT('Ctrl Pts',(1.76796319599994,12.2,-4.25345282400002));
#357948=CARTESIAN_POINT('Ctrl Pts',(1.76796319599994,5.2,-4.25345282400002));
#357949=CARTESIAN_POINT('Ctrl Pts',(1.76796319599994,2.2,-4.25345282400002));
#357950=CARTESIAN_POINT('Ctrl Pts',(1.76989619099994,12.2,-4.25493675600002));
#357951=CARTESIAN_POINT('Ctrl Pts',(1.76989619099994,5.2,-4.25493675600002));
#357952=CARTESIAN_POINT('Ctrl Pts',(1.76989619099994,2.2,-4.25493675600002));
#357953=CARTESIAN_POINT('Ctrl Pts',(1.77183361099994,12.2,-4.25642082300001));
#357954=CARTESIAN_POINT('Ctrl Pts',(1.77183361099994,5.2,-4.25642082300001));
#357955=CARTESIAN_POINT('Ctrl Pts',(1.77183361099994,2.2,-4.25642082300001));
#357956=CARTESIAN_POINT('Ctrl Pts',(1.77377545599994,12.2,-4.25790501400002));
#357957=CARTESIAN_POINT('Ctrl Pts',(1.77377545599994,5.2,-4.25790501400002));
#357958=CARTESIAN_POINT('Ctrl Pts',(1.77377545599994,2.2,-4.25790501400002));
#357959=CARTESIAN_POINT('Ctrl Pts',(1.77572172399994,12.2,-4.25938932200001));
#357960=CARTESIAN_POINT('Ctrl Pts',(1.77572172399994,5.2,-4.25938932200001));
#357961=CARTESIAN_POINT('Ctrl Pts',(1.77572172399994,2.2,-4.25938932200001));
#357962=CARTESIAN_POINT('Ctrl Pts',(1.77767241399994,12.2,-4.26087373600001));
#357963=CARTESIAN_POINT('Ctrl Pts',(1.77767241399994,5.2,-4.26087373600001));
#357964=CARTESIAN_POINT('Ctrl Pts',(1.77767241399994,2.2,-4.26087373600001));
#357965=CARTESIAN_POINT('Ctrl Pts',(1.77962752599994,12.2,-4.26235824800001));
#357966=CARTESIAN_POINT('Ctrl Pts',(1.77962752599994,5.2,-4.26235824800001));
#357967=CARTESIAN_POINT('Ctrl Pts',(1.77962752599994,2.2,-4.26235824800001));
#357968=CARTESIAN_POINT('Ctrl Pts',(1.78158705699994,12.2,-4.26384284800001));
#357969=CARTESIAN_POINT('Ctrl Pts',(1.78158705699994,5.2,-4.26384284800001));
#357970=CARTESIAN_POINT('Ctrl Pts',(1.78158705699994,2.2,-4.26384284800001));
#357971=CARTESIAN_POINT('Ctrl Pts',(1.78355100899994,12.2,-4.26532752900001));
#357972=CARTESIAN_POINT('Ctrl Pts',(1.78355100899994,5.2,-4.26532752900001));
#357973=CARTESIAN_POINT('Ctrl Pts',(1.78355100899994,2.2,-4.26532752900001));
#357974=CARTESIAN_POINT('Ctrl Pts',(1.78551937799994,12.2,-4.26681227900001));
#357975=CARTESIAN_POINT('Ctrl Pts',(1.78551937799994,5.2,-4.26681227900001));
#357976=CARTESIAN_POINT('Ctrl Pts',(1.78551937799994,2.2,-4.26681227900001));
#357977=CARTESIAN_POINT('Ctrl Pts',(1.78749216399994,12.2,-4.26829709100002));
#357978=CARTESIAN_POINT('Ctrl Pts',(1.78749216399994,5.2,-4.26829709100002));
#357979=CARTESIAN_POINT('Ctrl Pts',(1.78749216399994,2.2,-4.26829709100002));
#357980=CARTESIAN_POINT('Ctrl Pts',(1.78946936699994,12.2,-4.26978195500002));
#357981=CARTESIAN_POINT('Ctrl Pts',(1.78946936699994,5.2,-4.26978195500002));
#357982=CARTESIAN_POINT('Ctrl Pts',(1.78946936699994,2.2,-4.26978195500002));
#357983=CARTESIAN_POINT('Ctrl Pts',(1.79145098399994,12.2,-4.27126686200001));
#357984=CARTESIAN_POINT('Ctrl Pts',(1.79145098399994,5.2,-4.27126686200001));
#357985=CARTESIAN_POINT('Ctrl Pts',(1.79145098399994,2.2,-4.27126686200001));
#357986=CARTESIAN_POINT('Ctrl Pts',(1.79343701399994,12.2,-4.27275180300001));
#357987=CARTESIAN_POINT('Ctrl Pts',(1.79343701399994,5.2,-4.27275180300001));
#357988=CARTESIAN_POINT('Ctrl Pts',(1.79343701399994,2.2,-4.27275180300001));
#357989=CARTESIAN_POINT('Ctrl Pts',(1.79542745799994,12.2,-4.27423677000002));
#357990=CARTESIAN_POINT('Ctrl Pts',(1.79542745799994,5.2,-4.27423677000002));
#357991=CARTESIAN_POINT('Ctrl Pts',(1.79542745799994,2.2,-4.27423677000002));
#357992=CARTESIAN_POINT('Ctrl Pts',(1.79742231299994,12.2,-4.27572175300002));
#357993=CARTESIAN_POINT('Ctrl Pts',(1.79742231299994,5.2,-4.27572175300002));
#357994=CARTESIAN_POINT('Ctrl Pts',(1.79742231299994,2.2,-4.27572175300002));
#357995=CARTESIAN_POINT('Ctrl Pts',(1.79942157699994,12.2,-4.27720674200001));
#357996=CARTESIAN_POINT('Ctrl Pts',(1.79942157699994,5.2,-4.27720674200001));
#357997=CARTESIAN_POINT('Ctrl Pts',(1.79942157699994,2.2,-4.27720674200001));
#357998=CARTESIAN_POINT('Ctrl Pts',(1.80142525099994,12.2,-4.27869173000001));
#357999=CARTESIAN_POINT('Ctrl Pts',(1.80142525099994,5.2,-4.27869173000001));
#358000=CARTESIAN_POINT('Ctrl Pts',(1.80142525099994,2.2,-4.27869173000001));
#358001=CARTESIAN_POINT('Ctrl Pts',(1.80343333299994,12.2,-4.28017670600001));
#358002=CARTESIAN_POINT('Ctrl Pts',(1.80343333299994,5.2,-4.28017670600001));
#358003=CARTESIAN_POINT('Ctrl Pts',(1.80343333299994,2.2,-4.28017670600001));
#358004=CARTESIAN_POINT('Ctrl Pts',(1.80544582299994,12.2,-4.28166166300001));
#358005=CARTESIAN_POINT('Ctrl Pts',(1.80544582299994,5.2,-4.28166166300001));
#358006=CARTESIAN_POINT('Ctrl Pts',(1.80544582299994,2.2,-4.28166166300001));
#358007=CARTESIAN_POINT('Ctrl Pts',(1.80746271699994,12.2,-4.28314659200002));
#358008=CARTESIAN_POINT('Ctrl Pts',(1.80746271699994,5.2,-4.28314659200002));
#358009=CARTESIAN_POINT('Ctrl Pts',(1.80746271699994,2.2,-4.28314659200002));
#358010=CARTESIAN_POINT('Ctrl Pts',(1.80948401499994,12.2,-4.28463148200001));
#358011=CARTESIAN_POINT('Ctrl Pts',(1.80948401499994,5.2,-4.28463148200001));
#358012=CARTESIAN_POINT('Ctrl Pts',(1.80948401499994,2.2,-4.28463148200001));
#358013=CARTESIAN_POINT('Ctrl Pts',(1.81150971699994,12.2,-4.28611632600001));
#358014=CARTESIAN_POINT('Ctrl Pts',(1.81150971699994,5.2,-4.28611632600001));
#358015=CARTESIAN_POINT('Ctrl Pts',(1.81150971699994,2.2,-4.28611632600001));
#358016=CARTESIAN_POINT('Ctrl Pts',(1.81353981999994,12.2,-4.28760111400001));
#358017=CARTESIAN_POINT('Ctrl Pts',(1.81353981999994,5.2,-4.28760111400001));
#358018=CARTESIAN_POINT('Ctrl Pts',(1.81353981999994,2.2,-4.28760111400001));
#358019=CARTESIAN_POINT('Ctrl Pts',(1.81557432299994,12.2,-4.28908583800002));
#358020=CARTESIAN_POINT('Ctrl Pts',(1.81557432299994,5.2,-4.28908583800002));
#358021=CARTESIAN_POINT('Ctrl Pts',(1.81557432299994,2.2,-4.28908583800002));
#358022=CARTESIAN_POINT('Ctrl Pts',(1.81761322799994,12.2,-4.29057048800002));
#358023=CARTESIAN_POINT('Ctrl Pts',(1.81761322799994,5.2,-4.29057048800002));
#358024=CARTESIAN_POINT('Ctrl Pts',(1.81761322799994,2.2,-4.29057048800002));
#358025=CARTESIAN_POINT('Ctrl Pts',(1.81965652899994,12.2,-4.29205505700001));
#358026=CARTESIAN_POINT('Ctrl Pts',(1.81965652899994,5.2,-4.29205505700001));
#358027=CARTESIAN_POINT('Ctrl Pts',(1.81965652899994,2.2,-4.29205505700001));
#358028=CARTESIAN_POINT('Ctrl Pts',(1.82170422599994,12.2,-4.29353953400001));
#358029=CARTESIAN_POINT('Ctrl Pts',(1.82170422599994,5.2,-4.29353953400001));
#358030=CARTESIAN_POINT('Ctrl Pts',(1.82170422599994,2.2,-4.29353953400001));
#358031=CARTESIAN_POINT('Ctrl Pts',(1.82375632099994,12.2,-4.29502391100002));
#358032=CARTESIAN_POINT('Ctrl Pts',(1.82375632099994,5.2,-4.29502391100002));
#358033=CARTESIAN_POINT('Ctrl Pts',(1.82375632099994,2.2,-4.29502391100002));
#358034=CARTESIAN_POINT('Ctrl Pts',(1.82581280899994,12.2,-4.29650817900002));
#358035=CARTESIAN_POINT('Ctrl Pts',(1.82581280899994,5.2,-4.29650817900002));
#358036=CARTESIAN_POINT('Ctrl Pts',(1.82581280899994,2.2,-4.29650817900002));
#358037=CARTESIAN_POINT('Ctrl Pts',(1.82787368999994,12.2,-4.29799233100002));
#358038=CARTESIAN_POINT('Ctrl Pts',(1.82787368999994,5.2,-4.29799233100002));
#358039=CARTESIAN_POINT('Ctrl Pts',(1.82787368999994,2.2,-4.29799233100002));
#358040=CARTESIAN_POINT('Ctrl Pts',(1.82993896199994,12.2,-4.29947635400001));
#358041=CARTESIAN_POINT('Ctrl Pts',(1.82993896199994,5.2,-4.29947635400001));
#358042=CARTESIAN_POINT('Ctrl Pts',(1.82993896199994,2.2,-4.29947635400001));
#358043=CARTESIAN_POINT('Ctrl Pts',(1.83200862499994,12.2,-4.30096024400001));
#358044=CARTESIAN_POINT('Ctrl Pts',(1.83200862499994,5.2,-4.30096024400001));
#358045=CARTESIAN_POINT('Ctrl Pts',(1.83200862499994,2.2,-4.30096024400001));
#358046=CARTESIAN_POINT('Ctrl Pts',(1.83408267599994,12.2,-4.30244399000001));
#358047=CARTESIAN_POINT('Ctrl Pts',(1.83408267599994,5.2,-4.30244399000001));
#358048=CARTESIAN_POINT('Ctrl Pts',(1.83408267599994,2.2,-4.30244399000001));
#358049=CARTESIAN_POINT('Ctrl Pts',(1.83616111599994,12.2,-4.30392758200002));
#358050=CARTESIAN_POINT('Ctrl Pts',(1.83616111599994,5.2,-4.30392758200002));
#358051=CARTESIAN_POINT('Ctrl Pts',(1.83616111599994,2.2,-4.30392758200002));
#358052=CARTESIAN_POINT('Ctrl Pts',(1.83824394199994,12.2,-4.30541101400001));
#358053=CARTESIAN_POINT('Ctrl Pts',(1.83824394199994,5.2,-4.30541101400001));
#358054=CARTESIAN_POINT('Ctrl Pts',(1.83824394199994,2.2,-4.30541101400001));
#358055=CARTESIAN_POINT('Ctrl Pts',(1.84033115299994,12.2,-4.30689427400001));
#358056=CARTESIAN_POINT('Ctrl Pts',(1.84033115299994,5.2,-4.30689427400001));
#358057=CARTESIAN_POINT('Ctrl Pts',(1.84033115299994,2.2,-4.30689427400001));
#358058=CARTESIAN_POINT('Ctrl Pts',(1.84242274599994,12.2,-4.30837735600001));
#358059=CARTESIAN_POINT('Ctrl Pts',(1.84242274599994,5.2,-4.30837735600001));
#358060=CARTESIAN_POINT('Ctrl Pts',(1.84242274599994,2.2,-4.30837735600001));
#358061=CARTESIAN_POINT('Ctrl Pts',(1.84451872199994,12.2,-4.30986025000001));
#358062=CARTESIAN_POINT('Ctrl Pts',(1.84451872199994,5.2,-4.30986025000001));
#358063=CARTESIAN_POINT('Ctrl Pts',(1.84451872199994,2.2,-4.30986025000001));
#358064=CARTESIAN_POINT('Ctrl Pts',(1.84661907999994,12.2,-4.31134294700001));
#358065=CARTESIAN_POINT('Ctrl Pts',(1.84661907999994,5.2,-4.31134294700001));
#358066=CARTESIAN_POINT('Ctrl Pts',(1.84661907999994,2.2,-4.31134294700001));
#358067=CARTESIAN_POINT('Ctrl Pts',(1.84872381499994,12.2,-4.31282544000001));
#358068=CARTESIAN_POINT('Ctrl Pts',(1.84872381499994,5.2,-4.31282544000001));
#358069=CARTESIAN_POINT('Ctrl Pts',(1.84872381499994,2.2,-4.31282544000001));
#358070=CARTESIAN_POINT('Ctrl Pts',(1.85083292899994,12.2,-4.31430771700001));
#358071=CARTESIAN_POINT('Ctrl Pts',(1.85083292899994,5.2,-4.31430771700001));
#358072=CARTESIAN_POINT('Ctrl Pts',(1.85083292899994,2.2,-4.31430771700001));
#358073=CARTESIAN_POINT('Ctrl Pts',(1.85294641899994,12.2,-4.31578977400001));
#358074=CARTESIAN_POINT('Ctrl Pts',(1.85294641899994,5.2,-4.31578977400001));
#358075=CARTESIAN_POINT('Ctrl Pts',(1.85294641899994,2.2,-4.31578977400001));
#358076=CARTESIAN_POINT('Ctrl Pts',(1.85506428499994,12.2,-4.31727159900001));
#358077=CARTESIAN_POINT('Ctrl Pts',(1.85506428499994,5.2,-4.31727159900001));
#358078=CARTESIAN_POINT('Ctrl Pts',(1.85506428499994,2.2,-4.31727159900001));
#358079=CARTESIAN_POINT('Ctrl Pts',(1.85718652399994,12.2,-4.31875318500001));
#358080=CARTESIAN_POINT('Ctrl Pts',(1.85718652399994,5.2,-4.31875318500001));
#358081=CARTESIAN_POINT('Ctrl Pts',(1.85718652399994,2.2,-4.31875318500001));
#358082=CARTESIAN_POINT('Ctrl Pts',(1.85931313599994,12.2,-4.32023452300001));
#358083=CARTESIAN_POINT('Ctrl Pts',(1.85931313599994,5.2,-4.32023452300001));
#358084=CARTESIAN_POINT('Ctrl Pts',(1.85931313599994,2.2,-4.32023452300001));
#358085=CARTESIAN_POINT('Ctrl Pts',(1.86144411799994,12.2,-4.32171560400001));
#358086=CARTESIAN_POINT('Ctrl Pts',(1.86144411799994,5.2,-4.32171560400001));
#358087=CARTESIAN_POINT('Ctrl Pts',(1.86144411799994,2.2,-4.32171560400001));
#358088=CARTESIAN_POINT('Ctrl Pts',(1.86357946799994,12.2,-4.32319641900001));
#358089=CARTESIAN_POINT('Ctrl Pts',(1.86357946799994,5.2,-4.32319641900001));
#358090=CARTESIAN_POINT('Ctrl Pts',(1.86357946799994,2.2,-4.32319641900001));
#358091=CARTESIAN_POINT('Ctrl Pts',(1.86571918699994,12.2,-4.32467695700002));
#358092=CARTESIAN_POINT('Ctrl Pts',(1.86571918699994,5.2,-4.32467695700002));
#358093=CARTESIAN_POINT('Ctrl Pts',(1.86571918699994,2.2,-4.32467695700002));
#358094=CARTESIAN_POINT('Ctrl Pts',(1.86786327099994,12.2,-4.32615721200001));
#358095=CARTESIAN_POINT('Ctrl Pts',(1.86786327099994,5.2,-4.32615721200001));
#358096=CARTESIAN_POINT('Ctrl Pts',(1.86786327099994,2.2,-4.32615721200001));
#358097=CARTESIAN_POINT('Ctrl Pts',(1.87001172099994,12.2,-4.32763717500002));
#358098=CARTESIAN_POINT('Ctrl Pts',(1.87001172099994,5.2,-4.32763717500002));
#358099=CARTESIAN_POINT('Ctrl Pts',(1.87001172099994,2.2,-4.32763717500002));
#358100=CARTESIAN_POINT('Ctrl Pts',(1.87216453299994,12.2,-4.32911683800001));
#358101=CARTESIAN_POINT('Ctrl Pts',(1.87216453299994,5.2,-4.32911683800001));
#358102=CARTESIAN_POINT('Ctrl Pts',(1.87216453299994,2.2,-4.32911683800001));
#358103=CARTESIAN_POINT('Ctrl Pts',(1.87432170699994,12.2,-4.33059619400002));
#358104=CARTESIAN_POINT('Ctrl Pts',(1.87432170699994,5.2,-4.33059619400002));
#358105=CARTESIAN_POINT('Ctrl Pts',(1.87432170699994,2.2,-4.33059619400002));
#358106=CARTESIAN_POINT('Ctrl Pts',(1.87648324099994,12.2,-4.33207523400001));
#358107=CARTESIAN_POINT('Ctrl Pts',(1.87648324099994,5.2,-4.33207523400001));
#358108=CARTESIAN_POINT('Ctrl Pts',(1.87648324099994,2.2,-4.33207523400001));
#358109=CARTESIAN_POINT('Ctrl Pts',(1.87864913399994,12.2,-4.33355395000001));
#358110=CARTESIAN_POINT('Ctrl Pts',(1.87864913399994,5.2,-4.33355395000001));
#358111=CARTESIAN_POINT('Ctrl Pts',(1.87864913399994,2.2,-4.33355395000001));
#358112=CARTESIAN_POINT('Ctrl Pts',(1.88081938399994,12.2,-4.33503233500002));
#358113=CARTESIAN_POINT('Ctrl Pts',(1.88081938399994,5.2,-4.33503233500002));
#358114=CARTESIAN_POINT('Ctrl Pts',(1.88081938399994,2.2,-4.33503233500002));
#358115=CARTESIAN_POINT('Ctrl Pts',(1.88299399099994,12.2,-4.33651037800002));
#358116=CARTESIAN_POINT('Ctrl Pts',(1.88299399099994,5.2,-4.33651037800002));
#358117=CARTESIAN_POINT('Ctrl Pts',(1.88299399099994,2.2,-4.33651037800002));
#358118=CARTESIAN_POINT('Ctrl Pts',(1.88517294999994,12.2,-4.33798806900001));
#358119=CARTESIAN_POINT('Ctrl Pts',(1.88517294999994,5.2,-4.33798806900001));
#358120=CARTESIAN_POINT('Ctrl Pts',(1.88517294999994,2.2,-4.33798806900001));
#358121=CARTESIAN_POINT('Ctrl Pts',(1.88735626099994,12.2,-4.33946539900001));
#358122=CARTESIAN_POINT('Ctrl Pts',(1.88735626099994,5.2,-4.33946539900001));
#358123=CARTESIAN_POINT('Ctrl Pts',(1.88735626099994,2.2,-4.33946539900001));
#358124=CARTESIAN_POINT('Ctrl Pts',(1.88954392399994,12.2,-4.34094235600002));
#358125=CARTESIAN_POINT('Ctrl Pts',(1.88954392399994,5.2,-4.34094235600002));
#358126=CARTESIAN_POINT('Ctrl Pts',(1.88954392399994,2.2,-4.34094235600002));
#358127=CARTESIAN_POINT('Ctrl Pts',(1.89173593299994,12.2,-4.34241893000001));
#358128=CARTESIAN_POINT('Ctrl Pts',(1.89173593299994,5.2,-4.34241893000001));
#358129=CARTESIAN_POINT('Ctrl Pts',(1.89173593299994,2.2,-4.34241893000001));
#358130=CARTESIAN_POINT('Ctrl Pts',(1.89393228799994,12.2,-4.34389511400001));
#358131=CARTESIAN_POINT('Ctrl Pts',(1.89393228799994,5.2,-4.34389511400001));
#358132=CARTESIAN_POINT('Ctrl Pts',(1.89393228799994,2.2,-4.34389511400001));
#358133=CARTESIAN_POINT('Ctrl Pts',(1.89613298899994,12.2,-4.34537090000001));
#358134=CARTESIAN_POINT('Ctrl Pts',(1.89613298899994,5.2,-4.34537090000001));
#358135=CARTESIAN_POINT('Ctrl Pts',(1.89613298899994,2.2,-4.34537090000001));
#358136=CARTESIAN_POINT('Ctrl Pts',(1.89833803499994,12.2,-4.34684628800001));
#358137=CARTESIAN_POINT('Ctrl Pts',(1.89833803499994,5.2,-4.34684628800001));
#358138=CARTESIAN_POINT('Ctrl Pts',(1.89833803499994,2.2,-4.34684628800001));
#358139=CARTESIAN_POINT('Ctrl Pts',(1.90054742399994,12.2,-4.34832127200002));
#358140=CARTESIAN_POINT('Ctrl Pts',(1.90054742399994,5.2,-4.34832127200002));
#358141=CARTESIAN_POINT('Ctrl Pts',(1.90054742399994,2.2,-4.34832127200002));
#358142=CARTESIAN_POINT('Ctrl Pts',(1.90231840999994,12.2,-4.34950093700001));
#358143=CARTESIAN_POINT('Ctrl Pts',(1.90231840999994,5.2,-4.34950093700001));
#358144=CARTESIAN_POINT('Ctrl Pts',(1.90231840999994,2.2,-4.34950093700001));
#358145=CARTESIAN_POINT('Ctrl Pts',(1.90364860499994,12.2,-4.35038550300002));
#358146=CARTESIAN_POINT('Ctrl Pts',(1.90364860499994,5.2,-4.35038550300002));
#358147=CARTESIAN_POINT('Ctrl Pts',(1.90364860499994,2.2,-4.35038550300002));
#358148=CARTESIAN_POINT('Ctrl Pts',(1.90453626899994,12.2,-4.35097513300001));
#358149=CARTESIAN_POINT('Ctrl Pts',(1.90453626899994,5.2,-4.35097513300001));
#358150=CARTESIAN_POINT('Ctrl Pts',(1.90453626899994,2.2,-4.35097513300001));
#358151=CARTESIAN_POINT('Ctrl Pts',(1.90498031899994,12.2,-4.35126992800001));
#358152=CARTESIAN_POINT('Ctrl Pts',(1.90498031899994,5.2,-4.35126992800001));
#358153=CARTESIAN_POINT('Ctrl Pts',(1.90498031899994,2.2,-4.35126992800001));
#358154=CARTESIAN_POINT('Origin',(-5.66300478732629E-14,15.2,-1.77635683940025E-14));
#358155=CARTESIAN_POINT('Origin',(-5.66300478732629E-14,15.4,-1.77635683940025E-14));
#358156=CARTESIAN_POINT('',(-3.28892417320473,15.4,-1.19707050039253));
#358157=CARTESIAN_POINT('',(-3.28892417320473,15.4,-1.19707050039253));
#358158=CARTESIAN_POINT('Origin',(-5.66300478732629E-14,15.4,-1.77635683940025E-14));
#358159=CARTESIAN_POINT('Origin',(-5.66300478732629E-14,15.4,-1.77635683940025E-14));
#358160=CARTESIAN_POINT('',(0.,0.,0.));
#358161=CARTESIAN_POINT('Origin',(0.,0.,-3.33333333333333));
#358162=CARTESIAN_POINT('',(-1.76666666666667,2.16354267849366E-16,-3.5));
#358163=CARTESIAN_POINT('Origin',(0.,0.,-3.5));
#358164=CARTESIAN_POINT('',(-1.6,-1.95943487863577E-16,-3.33333333333333));
#358165=CARTESIAN_POINT('Origin',(-1.76666666666667,-2.16354267849366E-16,
-3.33333333333333));
#358166=CARTESIAN_POINT('Origin',(0.,0.,-3.33333333333333));
#358167=CARTESIAN_POINT('Origin',(0.,0.,-3.5));
#358168=CARTESIAN_POINT('',(2.23333333333333,-2.73504451809576E-16,-3.5));
#358169=CARTESIAN_POINT('Origin',(0.,0.,-3.5));
#358170=CARTESIAN_POINT('Origin',(0.,0.,0.));
#358171=CARTESIAN_POINT('',(-1.6,-1.95943487863577E-16,-3.));
#358172=CARTESIAN_POINT('',(-1.6,-1.95943487863577E-16,0.));
#358173=CARTESIAN_POINT('',(-1.57109375,-0.302761339524943,-3.));
#358174=CARTESIAN_POINT('Origin',(0.,0.,-3.));
#358175=CARTESIAN_POINT('',(-1.57109375,-0.302761339524943,3.));
#358176=CARTESIAN_POINT('',(-1.57109375,-0.302761339524943,0.));
#358177=CARTESIAN_POINT('',(-1.6,-1.95943487863577E-16,3.));
#358178=CARTESIAN_POINT('Origin',(0.,0.,3.));
#358179=CARTESIAN_POINT('',(-1.6,-1.95943487863577E-16,3.33333333333333));
#358180=CARTESIAN_POINT('',(-1.6,-1.95943487863577E-16,0.));
#358181=CARTESIAN_POINT('',(1.6,-1.95943487863577E-16,3.33333333333333));
#358182=CARTESIAN_POINT('Origin',(0.,0.,3.33333333333333));
#358183=CARTESIAN_POINT('Origin',(0.,0.,3.33333333333333));
#358184=CARTESIAN_POINT('',(-1.57109375,0.302761339524943,3.));
#358185=CARTESIAN_POINT('Origin',(0.,0.,3.));
#358186=CARTESIAN_POINT('',(-1.57109375,0.302761339524943,-3.));
#358187=CARTESIAN_POINT('',(-1.57109375,0.302761339524943,0.));
#358188=CARTESIAN_POINT('Origin',(0.,0.,-3.));
#358189=CARTESIAN_POINT('',(0.896846448245593,-1.32501564076401,-3.));
#358190=CARTESIAN_POINT('',(1.32501564076401,-0.896846448245593,-3.));
#358191=CARTESIAN_POINT('Origin',(0.,0.,-3.));
#358192=CARTESIAN_POINT('',(1.32501564076401,-0.896846448245593,3.));
#358193=CARTESIAN_POINT('',(1.32501564076401,-0.896846448245593,0.));
#358194=CARTESIAN_POINT('',(0.896846448245593,-1.32501564076401,3.));
#358195=CARTESIAN_POINT('Origin',(0.,0.,3.));
#358196=CARTESIAN_POINT('',(0.896846448245593,-1.32501564076401,0.));
#358197=CARTESIAN_POINT('',(-0.302761339524943,-1.57109375,-3.));
#358198=CARTESIAN_POINT('',(0.302761339524943,-1.57109375,-3.));
#358199=CARTESIAN_POINT('Origin',(0.,0.,-3.));
#358200=CARTESIAN_POINT('',(0.302761339524943,-1.57109375,3.));
#358201=CARTESIAN_POINT('',(0.302761339524943,-1.57109375,0.));
#358202=CARTESIAN_POINT('',(-0.302761339524943,-1.57109375,3.));
#358203=CARTESIAN_POINT('Origin',(0.,0.,3.));
#358204=CARTESIAN_POINT('',(-0.302761339524943,-1.57109375,0.));
#358205=CARTESIAN_POINT('',(-1.32501564076401,-0.896846448245593,-3.));
#358206=CARTESIAN_POINT('',(-0.896846448245593,-1.32501564076401,-3.));
#358207=CARTESIAN_POINT('Origin',(0.,0.,-3.));
#358208=CARTESIAN_POINT('',(-0.896846448245593,-1.32501564076401,3.));
#358209=CARTESIAN_POINT('',(-0.896846448245593,-1.32501564076401,0.));
#358210=CARTESIAN_POINT('',(-1.32501564076401,-0.896846448245593,3.));
#358211=CARTESIAN_POINT('Origin',(0.,0.,3.));
#358212=CARTESIAN_POINT('',(-1.32501564076401,-0.896846448245593,0.));
#358213=CARTESIAN_POINT('',(-0.896846448245593,1.32501564076401,-3.));
#358214=CARTESIAN_POINT('',(-1.32501564076401,0.896846448245593,-3.));
#358215=CARTESIAN_POINT('Origin',(0.,0.,-3.));
#358216=CARTESIAN_POINT('',(-1.32501564076401,0.896846448245593,3.));
#358217=CARTESIAN_POINT('',(-1.32501564076401,0.896846448245593,0.));
#358218=CARTESIAN_POINT('',(-0.896846448245593,1.32501564076401,3.));
#358219=CARTESIAN_POINT('Origin',(0.,0.,3.));
#358220=CARTESIAN_POINT('',(-0.896846448245593,1.32501564076401,0.));
#358221=CARTESIAN_POINT('',(0.302761339524943,1.57109375,-3.));
#358222=CARTESIAN_POINT('',(-0.302761339524943,1.57109375,-3.));
#358223=CARTESIAN_POINT('Origin',(0.,0.,-3.));
#358224=CARTESIAN_POINT('',(-0.302761339524943,1.57109375,3.));
#358225=CARTESIAN_POINT('',(-0.302761339524943,1.57109375,0.));
#358226=CARTESIAN_POINT('',(0.302761339524943,1.57109375,3.));
#358227=CARTESIAN_POINT('Origin',(0.,0.,3.));
#358228=CARTESIAN_POINT('',(0.302761339524943,1.57109375,0.));
#358229=CARTESIAN_POINT('',(1.32501564076401,0.896846448245593,-3.));
#358230=CARTESIAN_POINT('',(0.896846448245593,1.32501564076401,-3.));
#358231=CARTESIAN_POINT('Origin',(0.,0.,-3.));
#358232=CARTESIAN_POINT('',(0.896846448245593,1.32501564076401,3.));
#358233=CARTESIAN_POINT('',(0.896846448245593,1.32501564076401,0.));
#358234=CARTESIAN_POINT('',(1.32501564076401,0.896846448245593,3.));
#358235=CARTESIAN_POINT('Origin',(0.,0.,3.));
#358236=CARTESIAN_POINT('',(1.32501564076401,0.896846448245593,0.));
#358237=CARTESIAN_POINT('',(1.57109375,-0.302761339524943,-3.));
#358238=CARTESIAN_POINT('',(1.57109375,0.302761339524943,-3.));
#358239=CARTESIAN_POINT('Origin',(0.,0.,-3.));
#358240=CARTESIAN_POINT('',(1.57109375,0.302761339524943,3.));
#358241=CARTESIAN_POINT('',(1.57109375,0.302761339524943,0.));
#358242=CARTESIAN_POINT('',(1.57109375,-0.302761339524943,3.));
#358243=CARTESIAN_POINT('Origin',(0.,0.,3.));
#358244=CARTESIAN_POINT('',(1.57109375,-0.302761339524943,0.));
#358245=CARTESIAN_POINT('Origin',(0.,0.,-3.33333333333333));
#358246=CARTESIAN_POINT('',(2.4,-2.93915231795365E-16,-3.33333333333333));
#358247=CARTESIAN_POINT('Origin',(2.23333333333333,-2.73504451809575E-16,
-3.33333333333333));
#358248=CARTESIAN_POINT('',(-2.4,2.93915231795365E-16,-3.33333333333333));
#358249=CARTESIAN_POINT('Origin',(0.,0.,-3.33333333333333));
#358250=CARTESIAN_POINT('Origin',(0.,0.,-3.33333333333333));
#358251=CARTESIAN_POINT('Origin',(0.,0.,0.));
#358252=CARTESIAN_POINT('',(-2.4,-2.93915231795365E-16,3.33333333333333));
#358253=CARTESIAN_POINT('Origin',(0.,0.,3.33333333333333));
#358254=CARTESIAN_POINT('',(-2.4,-2.93915231795365E-16,3.));
#358255=CARTESIAN_POINT('',(-2.4,-2.93915231795365E-16,0.));
#358256=CARTESIAN_POINT('',(-2.37109375,-0.371368319476685,3.));
#358257=CARTESIAN_POINT('Origin',(0.,0.,3.));
#358258=CARTESIAN_POINT('',(-2.37109375,-0.371368319476685,-3.));
#358259=CARTESIAN_POINT('',(-2.37109375,-0.371368319476685,0.));
#358260=CARTESIAN_POINT('',(-2.4,-2.93915231795365E-16,-3.));
#358261=CARTESIAN_POINT('Origin',(0.,0.,-3.));
#358262=CARTESIAN_POINT('',(-2.4,-2.93915231795365E-16,0.));
#358263=CARTESIAN_POINT('',(-2.37109375,0.371368319476686,-3.));
#358264=CARTESIAN_POINT('Origin',(0.,0.,-3.));
#358265=CARTESIAN_POINT('',(-2.37109375,0.371368319476686,3.));
#358266=CARTESIAN_POINT('',(-2.37109375,0.371368319476686,0.));
#358267=CARTESIAN_POINT('Origin',(0.,0.,3.));
#358268=CARTESIAN_POINT('',(1.93921352647386,-1.41401941243422,-3.));
#358269=CARTESIAN_POINT('',(1.41401941243422,-1.93921352647386,-3.));
#358270=CARTESIAN_POINT('Origin',(0.,0.,-3.));
#358271=CARTESIAN_POINT('',(1.41401941243422,-1.93921352647386,3.));
#358272=CARTESIAN_POINT('',(1.41401941243422,-1.93921352647386,0.));
#358273=CARTESIAN_POINT('',(1.93921352647386,-1.41401941243422,3.));
#358274=CARTESIAN_POINT('Origin',(0.,0.,3.));
#358275=CARTESIAN_POINT('',(1.93921352647386,-1.41401941243422,0.));
#358276=CARTESIAN_POINT('',(0.371368319476685,-2.37109375,-3.));
#358277=CARTESIAN_POINT('',(-0.371368319476686,-2.37109375,-3.));
#358278=CARTESIAN_POINT('Origin',(0.,0.,-3.));
#358279=CARTESIAN_POINT('',(-0.371368319476686,-2.37109375,3.));
#358280=CARTESIAN_POINT('',(-0.371368319476686,-2.37109375,0.));
#358281=CARTESIAN_POINT('',(0.371368319476685,-2.37109375,3.));
#358282=CARTESIAN_POINT('Origin',(0.,0.,3.));
#358283=CARTESIAN_POINT('',(0.371368319476685,-2.37109375,0.));
#358284=CARTESIAN_POINT('',(-1.41401941243422,-1.93921352647386,-3.));
#358285=CARTESIAN_POINT('',(-1.93921352647386,-1.41401941243422,-3.));
#358286=CARTESIAN_POINT('Origin',(0.,0.,-3.));
#358287=CARTESIAN_POINT('',(-1.93921352647386,-1.41401941243422,3.));
#358288=CARTESIAN_POINT('',(-1.93921352647386,-1.41401941243422,0.));
#358289=CARTESIAN_POINT('',(-1.41401941243422,-1.93921352647386,3.));
#358290=CARTESIAN_POINT('Origin',(0.,0.,3.));
#358291=CARTESIAN_POINT('',(-1.41401941243422,-1.93921352647386,0.));
#358292=CARTESIAN_POINT('',(-1.93921352647386,1.41401941243422,-3.));
#358293=CARTESIAN_POINT('',(-1.41401941243422,1.93921352647386,-3.));
#358294=CARTESIAN_POINT('Origin',(0.,0.,-3.));
#358295=CARTESIAN_POINT('',(-1.41401941243422,1.93921352647386,3.));
#358296=CARTESIAN_POINT('',(-1.41401941243422,1.93921352647386,0.));
#358297=CARTESIAN_POINT('',(-1.93921352647386,1.41401941243422,3.));
#358298=CARTESIAN_POINT('Origin',(0.,0.,3.));
#358299=CARTESIAN_POINT('',(-1.93921352647386,1.41401941243422,0.));
#358300=CARTESIAN_POINT('',(-0.371368319476685,2.37109375,-3.));
#358301=CARTESIAN_POINT('',(0.371368319476686,2.37109375,-3.));
#358302=CARTESIAN_POINT('Origin',(0.,0.,-3.));
#358303=CARTESIAN_POINT('',(0.371368319476686,2.37109375,3.));
#358304=CARTESIAN_POINT('',(0.371368319476686,2.37109375,0.));
#358305=CARTESIAN_POINT('',(-0.371368319476685,2.37109375,3.));
#358306=CARTESIAN_POINT('Origin',(0.,0.,3.));
#358307=CARTESIAN_POINT('',(-0.371368319476685,2.37109375,0.));
#358308=CARTESIAN_POINT('',(1.41401941243422,1.93921352647386,-3.));
#358309=CARTESIAN_POINT('',(1.93921352647386,1.41401941243422,-3.));
#358310=CARTESIAN_POINT('Origin',(0.,0.,-3.));
#358311=CARTESIAN_POINT('',(1.93921352647386,1.41401941243422,3.));
#358312=CARTESIAN_POINT('',(1.93921352647386,1.41401941243422,0.));
#358313=CARTESIAN_POINT('',(1.41401941243422,1.93921352647386,3.));
#358314=CARTESIAN_POINT('Origin',(0.,0.,3.));
#358315=CARTESIAN_POINT('',(1.41401941243422,1.93921352647386,0.));
#358316=CARTESIAN_POINT('',(2.37109375,0.371368319476686,-3.));
#358317=CARTESIAN_POINT('',(2.37109375,-0.371368319476686,-3.));
#358318=CARTESIAN_POINT('Origin',(0.,0.,-3.));
#358319=CARTESIAN_POINT('',(2.37109375,-0.371368319476686,3.));
#358320=CARTESIAN_POINT('',(2.37109375,-0.371368319476686,0.));
#358321=CARTESIAN_POINT('',(2.37109375,0.371368319476686,3.));
#358322=CARTESIAN_POINT('Origin',(0.,0.,3.));
#358323=CARTESIAN_POINT('',(2.37109375,0.371368319476686,0.));
#358324=CARTESIAN_POINT('Origin',(0.,0.,3.33333333333333));
#358325=CARTESIAN_POINT('',(-2.23333333333333,2.73504451809576E-16,3.5));
#358326=CARTESIAN_POINT('Origin',(0.,0.,3.5));
#358327=CARTESIAN_POINT('Origin',(-2.23333333333333,-2.73504451809575E-16,
3.33333333333333));
#358328=CARTESIAN_POINT('Origin',(0.,0.,3.5));
#358329=CARTESIAN_POINT('',(1.76666666666667,-2.16354267849366E-16,3.5));
#358330=CARTESIAN_POINT('Origin',(0.,0.,3.5));
#358331=CARTESIAN_POINT('Origin',(0.,0.,3.33333333333333));
#358332=CARTESIAN_POINT('Origin',(1.76666666666667,-2.16354267849366E-16,
3.33333333333333));
#358333=CARTESIAN_POINT('Origin',(1.41421356237309,-1.4142135623731,3.));
#358334=CARTESIAN_POINT('Origin',(1.41421356237309,-1.4142135623731,3.));
#358335=CARTESIAN_POINT('Origin',(1.41421356237309,-1.4142135623731,3.));
#358336=CARTESIAN_POINT('Origin',(1.41421356237309,-1.4142135623731,0.));
#358337=CARTESIAN_POINT('Origin',(1.41421356237309,-1.4142135623731,-3.));
#358338=CARTESIAN_POINT('Origin',(1.41421356237309,-1.4142135623731,-3.));
#358339=CARTESIAN_POINT('Origin',(1.41421356237309,-1.4142135623731,-3.));
#358340=CARTESIAN_POINT('Origin',(1.41421356237309,-1.4142135623731,0.));
#358341=CARTESIAN_POINT('Origin',(-3.67394039744206E-16,-2.,3.));
#358342=CARTESIAN_POINT('Origin',(-3.67394039744206E-16,-2.,3.));
#358343=CARTESIAN_POINT('Origin',(-3.67394039744206E-16,-2.,3.));
#358344=CARTESIAN_POINT('Origin',(-3.67394039744206E-16,-2.,0.));
#358345=CARTESIAN_POINT('Origin',(-3.67394039744206E-16,-2.,-3.));
#358346=CARTESIAN_POINT('Origin',(-3.67394039744206E-16,-2.,-3.));
#358347=CARTESIAN_POINT('Origin',(-3.67394039744206E-16,-2.,-3.));
#358348=CARTESIAN_POINT('Origin',(-3.67394039744206E-16,-2.,0.));
#358349=CARTESIAN_POINT('Origin',(-1.4142135623731,-1.41421356237309,3.));
#358350=CARTESIAN_POINT('Origin',(-1.4142135623731,-1.41421356237309,3.));
#358351=CARTESIAN_POINT('Origin',(-1.4142135623731,-1.41421356237309,3.));
#358352=CARTESIAN_POINT('Origin',(-1.4142135623731,-1.41421356237309,0.));
#358353=CARTESIAN_POINT('Origin',(-1.4142135623731,-1.41421356237309,-3.));
#358354=CARTESIAN_POINT('Origin',(-1.4142135623731,-1.41421356237309,-3.));
#358355=CARTESIAN_POINT('Origin',(-1.4142135623731,-1.41421356237309,-3.));
#358356=CARTESIAN_POINT('Origin',(-1.4142135623731,-1.41421356237309,0.));
#358357=CARTESIAN_POINT('Origin',(-2.,2.44929359829471E-16,3.));
#358358=CARTESIAN_POINT('Origin',(-2.,2.44929359829471E-16,3.));
#358359=CARTESIAN_POINT('Origin',(-2.,2.44929359829471E-16,3.));
#358360=CARTESIAN_POINT('Origin',(-2.,2.44929359829471E-16,0.));
#358361=CARTESIAN_POINT('Origin',(-2.,2.44929359829471E-16,-3.));
#358362=CARTESIAN_POINT('Origin',(-2.,2.44929359829471E-16,-3.));
#358363=CARTESIAN_POINT('Origin',(-2.,2.44929359829471E-16,-3.));
#358364=CARTESIAN_POINT('Origin',(-2.,2.44929359829471E-16,0.));
#358365=CARTESIAN_POINT('Origin',(-1.41421356237309,1.4142135623731,3.));
#358366=CARTESIAN_POINT('Origin',(-1.41421356237309,1.4142135623731,3.));
#358367=CARTESIAN_POINT('Origin',(-1.41421356237309,1.4142135623731,3.));
#358368=CARTESIAN_POINT('Origin',(-1.41421356237309,1.4142135623731,0.));
#358369=CARTESIAN_POINT('Origin',(-1.41421356237309,1.4142135623731,-3.));
#358370=CARTESIAN_POINT('Origin',(-1.41421356237309,1.4142135623731,-3.));
#358371=CARTESIAN_POINT('Origin',(-1.41421356237309,1.4142135623731,-3.));
#358372=CARTESIAN_POINT('Origin',(-1.41421356237309,1.4142135623731,0.));
#358373=CARTESIAN_POINT('Origin',(1.22464679914735E-16,2.,3.));
#358374=CARTESIAN_POINT('Origin',(1.22464679914735E-16,2.,3.));
#358375=CARTESIAN_POINT('Origin',(1.22464679914735E-16,2.,3.));
#358376=CARTESIAN_POINT('Origin',(1.22464679914735E-16,2.,0.));
#358377=CARTESIAN_POINT('Origin',(1.22464679914735E-16,2.,-3.));
#358378=CARTESIAN_POINT('Origin',(1.22464679914735E-16,2.,-3.));
#358379=CARTESIAN_POINT('Origin',(1.22464679914735E-16,2.,-3.));
#358380=CARTESIAN_POINT('Origin',(1.22464679914735E-16,2.,0.));
#358381=CARTESIAN_POINT('Origin',(1.4142135623731,1.4142135623731,3.));
#358382=CARTESIAN_POINT('Origin',(1.4142135623731,1.4142135623731,3.));
#358383=CARTESIAN_POINT('Origin',(1.4142135623731,1.4142135623731,3.));
#358384=CARTESIAN_POINT('Origin',(1.4142135623731,1.4142135623731,0.));
#358385=CARTESIAN_POINT('Origin',(1.4142135623731,1.4142135623731,-3.));
#358386=CARTESIAN_POINT('Origin',(1.4142135623731,1.4142135623731,-3.));
#358387=CARTESIAN_POINT('Origin',(1.4142135623731,1.4142135623731,-3.));
#358388=CARTESIAN_POINT('Origin',(1.4142135623731,1.4142135623731,0.));
#358389=CARTESIAN_POINT('Origin',(2.,0.,3.));
#358390=CARTESIAN_POINT('Origin',(2.,0.,3.));
#358391=CARTESIAN_POINT('Origin',(2.,0.,3.));
#358392=CARTESIAN_POINT('Origin',(2.,0.,0.));
#358393=CARTESIAN_POINT('Origin',(2.,0.,-3.));
#358394=CARTESIAN_POINT('Origin',(2.,0.,-3.));
#358395=CARTESIAN_POINT('Origin',(2.,0.,-3.));
#358396=CARTESIAN_POINT('Origin',(2.,0.,0.));
#358397=CARTESIAN_POINT('Origin',(2.,0.,-2.9625));
#358398=CARTESIAN_POINT('',(1.5,6.12323399573676E-17,-2.95));
#358399=CARTESIAN_POINT('Origin',(2.,0.,-2.95));
#358400=CARTESIAN_POINT('',(1.525,-5.81707229594993E-17,-2.975));
#358401=CARTESIAN_POINT('',(1.5125,-5.97015314584335E-17,-2.9625));
#358402=CARTESIAN_POINT('Origin',(2.,0.,-2.975));
#358403=CARTESIAN_POINT('Origin',(2.,0.,0.));
#358404=CARTESIAN_POINT('',(1.5,-6.12323399573676E-17,2.95));
#358405=CARTESIAN_POINT('Origin',(2.,0.,2.95));
#358406=CARTESIAN_POINT('',(1.5,-6.12323399573677E-17,0.));
#358407=CARTESIAN_POINT('Origin',(2.,0.,-2.975));
#358408=CARTESIAN_POINT('Origin',(2.,0.,2.9625));
#358409=CARTESIAN_POINT('',(1.525,5.81707229594993E-17,2.975));
#358410=CARTESIAN_POINT('',(1.5125,5.97015314584335E-17,2.9625));
#358411=CARTESIAN_POINT('Origin',(2.,0.,2.975));
#358412=CARTESIAN_POINT('Origin',(2.,0.,2.975));
#358413=CARTESIAN_POINT('Origin',(1.4142135623731,1.4142135623731,-2.9625));
#358414=CARTESIAN_POINT('',(1.06066017177982,1.06066017177982,-2.95));
#358415=CARTESIAN_POINT('Origin',(1.4142135623731,1.4142135623731,-2.95));
#358416=CARTESIAN_POINT('',(1.07833784130949,1.07833784130949,-2.975));
#358417=CARTESIAN_POINT('',(1.06949900654466,1.06949900654466,-2.9625));
#358418=CARTESIAN_POINT('Origin',(1.4142135623731,1.4142135623731,-2.975));
#358419=CARTESIAN_POINT('Origin',(1.4142135623731,1.4142135623731,0.));
#358420=CARTESIAN_POINT('',(1.06066017177982,1.06066017177982,2.95));
#358421=CARTESIAN_POINT('Origin',(1.4142135623731,1.4142135623731,2.95));
#358422=CARTESIAN_POINT('',(1.06066017177983,1.06066017177983,0.));
#358423=CARTESIAN_POINT('Origin',(1.4142135623731,1.4142135623731,-2.975));
#358424=CARTESIAN_POINT('Origin',(1.4142135623731,1.4142135623731,2.9625));
#358425=CARTESIAN_POINT('',(1.07833784130949,1.07833784130949,2.975));
#358426=CARTESIAN_POINT('',(1.06949900654466,1.06949900654466,2.9625));
#358427=CARTESIAN_POINT('Origin',(1.4142135623731,1.4142135623731,2.975));
#358428=CARTESIAN_POINT('Origin',(1.4142135623731,1.4142135623731,2.975));
#358429=CARTESIAN_POINT('Origin',(1.22464679914735E-16,2.,-2.9625));
#358430=CARTESIAN_POINT('',(3.06161699786839E-17,1.5,-2.95));
#358431=CARTESIAN_POINT('Origin',(1.22464679914735E-16,2.,-2.95));
#358432=CARTESIAN_POINT('',(1.51550041394485E-16,1.525,-2.975));
#358433=CARTESIAN_POINT('',(1.52315445643952E-16,1.5125,-2.9625));
#358434=CARTESIAN_POINT('Origin',(1.22464679914735E-16,2.,-2.975));
#358435=CARTESIAN_POINT('Origin',(1.22464679914735E-16,2.,0.));
#358436=CARTESIAN_POINT('',(1.53080849893419E-16,1.5,2.95));
#358437=CARTESIAN_POINT('Origin',(1.22464679914735E-16,2.,2.95));
#358438=CARTESIAN_POINT('',(1.53080849893419E-16,1.5,0.));
#358439=CARTESIAN_POINT('Origin',(1.22464679914735E-16,2.,-2.975));
#358440=CARTESIAN_POINT('Origin',(1.22464679914735E-16,2.,2.9625));
#358441=CARTESIAN_POINT('',(3.52085954754864E-17,1.525,2.975));
#358442=CARTESIAN_POINT('',(3.29123827270848E-17,1.5125,2.9625));
#358443=CARTESIAN_POINT('Origin',(1.22464679914735E-16,2.,2.975));
#358444=CARTESIAN_POINT('Origin',(1.22464679914735E-16,2.,2.975));
#358445=CARTESIAN_POINT('Origin',(-1.41421356237309,1.4142135623731,-2.9625));
#358446=CARTESIAN_POINT('',(-1.06066017177982,1.06066017177982,-2.95));
#358447=CARTESIAN_POINT('Origin',(-1.41421356237309,1.4142135623731,-2.95));
#358448=CARTESIAN_POINT('',(-1.07833784130949,1.07833784130949,-2.975));
#358449=CARTESIAN_POINT('',(-1.06949900654465,1.06949900654466,-2.9625));
#358450=CARTESIAN_POINT('Origin',(-1.41421356237309,1.4142135623731,-2.975));
#358451=CARTESIAN_POINT('Origin',(-1.41421356237309,1.4142135623731,0.));
#358452=CARTESIAN_POINT('',(-1.06066017177982,1.06066017177982,2.95));
#358453=CARTESIAN_POINT('Origin',(-1.41421356237309,1.4142135623731,2.95));
#358454=CARTESIAN_POINT('',(-1.06066017177982,1.06066017177983,0.));
#358455=CARTESIAN_POINT('Origin',(-1.41421356237309,1.4142135623731,-2.975));
#358456=CARTESIAN_POINT('Origin',(-1.41421356237309,1.4142135623731,2.9625));
#358457=CARTESIAN_POINT('',(-1.07833784130949,1.07833784130949,2.975));
#358458=CARTESIAN_POINT('',(-1.06949900654465,1.06949900654466,2.9625));
#358459=CARTESIAN_POINT('Origin',(-1.41421356237309,1.4142135623731,2.975));
#358460=CARTESIAN_POINT('Origin',(-1.41421356237309,1.4142135623731,2.975));
#358461=CARTESIAN_POINT('Origin',(-2.,2.44929359829471E-16,-2.9625));
#358462=CARTESIAN_POINT('',(-1.5,1.22464679914735E-16,-2.95));
#358463=CARTESIAN_POINT('Origin',(-2.,2.44929359829471E-16,-2.95));
#358464=CARTESIAN_POINT('',(-1.525,2.44929359829471E-16,-2.975));
#358465=CARTESIAN_POINT('',(-1.5125,2.44929359829471E-16,-2.9625));
#358466=CARTESIAN_POINT('Origin',(-2.,2.44929359829471E-16,-2.975));
#358467=CARTESIAN_POINT('Origin',(-2.,2.44929359829471E-16,0.));
#358468=CARTESIAN_POINT('',(-1.5,2.44929359829471E-16,2.95));
#358469=CARTESIAN_POINT('Origin',(-2.,2.44929359829471E-16,2.95));
#358470=CARTESIAN_POINT('',(-1.5,2.44929359829471E-16,0.));
#358471=CARTESIAN_POINT('Origin',(-2.,2.44929359829471E-16,-2.975));
#358472=CARTESIAN_POINT('Origin',(-2.,2.44929359829471E-16,2.9625));
#358473=CARTESIAN_POINT('',(-1.525,1.28587913910472E-16,2.975));
#358474=CARTESIAN_POINT('',(-1.5125,1.25526296912604E-16,2.9625));
#358475=CARTESIAN_POINT('Origin',(-2.,2.44929359829471E-16,2.975));
#358476=CARTESIAN_POINT('Origin',(-2.,2.44929359829471E-16,2.975));
#358477=CARTESIAN_POINT('Origin',(-1.4142135623731,-1.41421356237309,-2.9625));
#358478=CARTESIAN_POINT('',(-1.06066017177982,-1.06066017177982,-2.95));
#358479=CARTESIAN_POINT('Origin',(-1.4142135623731,-1.41421356237309,-2.95));
#358480=CARTESIAN_POINT('',(-1.07833784130949,-1.07833784130949,-2.975));
#358481=CARTESIAN_POINT('',(-1.06949900654466,-1.06949900654465,-2.9625));
#358482=CARTESIAN_POINT('Origin',(-1.4142135623731,-1.41421356237309,-2.975));
#358483=CARTESIAN_POINT('Origin',(-1.4142135623731,-1.41421356237309,0.));
#358484=CARTESIAN_POINT('',(-1.06066017177982,-1.06066017177982,2.95));
#358485=CARTESIAN_POINT('Origin',(-1.4142135623731,-1.41421356237309,2.95));
#358486=CARTESIAN_POINT('',(-1.06066017177983,-1.06066017177982,0.));
#358487=CARTESIAN_POINT('Origin',(-1.4142135623731,-1.41421356237309,-2.975));
#358488=CARTESIAN_POINT('Origin',(-1.4142135623731,-1.41421356237309,2.9625));
#358489=CARTESIAN_POINT('',(-1.07833784130949,-1.07833784130949,2.975));
#358490=CARTESIAN_POINT('',(-1.06949900654466,-1.06949900654465,2.9625));
#358491=CARTESIAN_POINT('Origin',(-1.4142135623731,-1.41421356237309,2.975));
#358492=CARTESIAN_POINT('Origin',(-1.4142135623731,-1.41421356237309,2.975));
#358493=CARTESIAN_POINT('Origin',(-3.67394039744206E-16,-2.,-2.9625));
#358494=CARTESIAN_POINT('',(-2.14313189850787E-16,-1.5,-2.95));
#358495=CARTESIAN_POINT('Origin',(-3.67394039744206E-16,-2.,-2.95));
#358496=CARTESIAN_POINT('',(-3.38308678264456E-16,-1.525,-2.975));
#358497=CARTESIAN_POINT('',(-3.37543274014989E-16,-1.5125,-2.9625));
#358498=CARTESIAN_POINT('Origin',(-3.67394039744206E-16,-2.,-2.975));
#358499=CARTESIAN_POINT('Origin',(-3.67394039744206E-16,-2.,0.));
#358500=CARTESIAN_POINT('',(-3.36777869765522E-16,-1.5,2.95));
#358501=CARTESIAN_POINT('Origin',(-3.67394039744206E-16,-2.,2.95));
#358502=CARTESIAN_POINT('',(-3.36777869765522E-16,-1.5,0.));
#358503=CARTESIAN_POINT('Origin',(-3.67394039744206E-16,-2.,-2.975));
#358504=CARTESIAN_POINT('Origin',(-3.67394039744206E-16,-2.,2.9625));
#358505=CARTESIAN_POINT('',(-2.21967232345458E-16,-1.525,2.975));
#358506=CARTESIAN_POINT('',(-2.18140211098122E-16,-1.5125,2.9625));
#358507=CARTESIAN_POINT('Origin',(-3.67394039744206E-16,-2.,2.975));
#358508=CARTESIAN_POINT('Origin',(-3.67394039744206E-16,-2.,2.975));
#358509=CARTESIAN_POINT('Origin',(1.41421356237309,-1.4142135623731,-2.9625));
#358510=CARTESIAN_POINT('',(1.06066017177982,-1.06066017177982,-2.95));
#358511=CARTESIAN_POINT('Origin',(1.41421356237309,-1.4142135623731,-2.95));
#358512=CARTESIAN_POINT('',(1.07833784130948,-1.07833784130949,-2.975));
#358513=CARTESIAN_POINT('',(1.06949900654465,-1.06949900654466,-2.9625));
#358514=CARTESIAN_POINT('Origin',(1.41421356237309,-1.4142135623731,-2.975));
#358515=CARTESIAN_POINT('Origin',(1.41421356237309,-1.4142135623731,0.));
#358516=CARTESIAN_POINT('',(1.06066017177982,-1.06066017177982,2.95));
#358517=CARTESIAN_POINT('Origin',(1.41421356237309,-1.4142135623731,2.95));
#358518=CARTESIAN_POINT('',(1.06066017177982,-1.06066017177983,0.));
#358519=CARTESIAN_POINT('Origin',(1.41421356237309,-1.4142135623731,-2.975));
#358520=CARTESIAN_POINT('Origin',(1.41421356237309,-1.4142135623731,2.9625));
#358521=CARTESIAN_POINT('',(1.07833784130948,-1.07833784130949,2.975));
#358522=CARTESIAN_POINT('',(1.06949900654465,-1.06949900654466,2.9625));
#358523=CARTESIAN_POINT('Origin',(1.41421356237309,-1.4142135623731,2.975));
#358524=CARTESIAN_POINT('Origin',(1.41421356237309,-1.4142135623731,2.975));
#358525=CARTESIAN_POINT('',(0.,0.,0.));
#358526=CARTESIAN_POINT('',(0.,0.,0.));
#358527=CARTESIAN_POINT('Origin',(-1.38777878078146E-16,-5.55111512312578E-15,
-17.91875));
#358528=CARTESIAN_POINT('',(2.44788436161308E-14,-1.17524047358083,-2.2));
#358529=CARTESIAN_POINT('',(2.45772990711711E-14,-1.17524047358083,-2.1375));
#358530=CARTESIAN_POINT('',(-4.21481204576211E-16,-1.17524047358085,-17.91875));
#358531=CARTESIAN_POINT('',(-1.43925448419918E-16,-1.17524047358083,-1.7));
#358532=CARTESIAN_POINT('Ctrl Pts',(-1.43925448419918E-16,-1.17524047358083,
-2.2));
#358533=CARTESIAN_POINT('Ctrl Pts',(0.678525403784434,-1.17524047358083,
-2.15833333333333));
#358534=CARTESIAN_POINT('Ctrl Pts',(1.01778810567665,-0.587620236790415,
-2.11666666666667));
#358535=CARTESIAN_POINT('Ctrl Pts',(1.35705080756887,-1.00219152102279E-15,
-2.075));
#358536=CARTESIAN_POINT('Ctrl Pts',(1.01778810567665,0.587620236790412,
-2.03333333333333));
#358537=CARTESIAN_POINT('Ctrl Pts',(0.678525403784435,1.17524047358083,
-1.99166666666667));
#358538=CARTESIAN_POINT('Ctrl Pts',(0.,1.17524047358083,-1.95));
#358539=CARTESIAN_POINT('Ctrl Pts',(-0.678525403784434,1.17524047358083,
-1.90833333333333));
#358540=CARTESIAN_POINT('Ctrl Pts',(-1.01778810567665,0.587620236790413,
-1.86666666666667));
#358541=CARTESIAN_POINT('Ctrl Pts',(-1.35705080756887,-7.79083855215448E-16,
-1.825));
#358542=CARTESIAN_POINT('Ctrl Pts',(-1.01778810567665,-0.587620236790415,
-1.78333333333333));
#358543=CARTESIAN_POINT('Ctrl Pts',(-0.678525403784435,-1.17524047358083,
-1.74166666666667));
#358544=CARTESIAN_POINT('Ctrl Pts',(-1.43925448419918E-16,-1.17524047358083,
-1.7));
#358545=CARTESIAN_POINT('',(-0.823407874165082,-0.838564036615828,-1.7));
#358546=CARTESIAN_POINT('Origin',(-1.01413306947856E-15,-1.11022302462516E-15,
-1.7));
#358547=CARTESIAN_POINT('Ctrl Pts',(-1.43925448419918E-16,-1.17524047358083,
-2.1375));
#358548=CARTESIAN_POINT('Ctrl Pts',(0.678525403784434,-1.17524047358083,
-2.09583333333333));
#358549=CARTESIAN_POINT('Ctrl Pts',(1.01778810567665,-0.587620236790415,
-2.05416666666667));
#358550=CARTESIAN_POINT('Ctrl Pts',(1.35705080756887,-1.02951000095943E-15,
-2.0125));
#358551=CARTESIAN_POINT('Ctrl Pts',(1.01778810567665,0.587620236790413,
-1.97083333333333));
#358552=CARTESIAN_POINT('Ctrl Pts',(0.678525403784435,1.17524047358083,
-1.92916666666667));
#358553=CARTESIAN_POINT('Ctrl Pts',(0.,1.17524047358083,-1.8875));
#358554=CARTESIAN_POINT('Ctrl Pts',(-0.678525403784434,1.17524047358083,
-1.84583333333333));
#358555=CARTESIAN_POINT('Ctrl Pts',(-1.01778810567665,0.587620236790414,
-1.80416666666667));
#358556=CARTESIAN_POINT('Ctrl Pts',(-1.35705080756887,-8.0640233515209E-16,
-1.7625));
#358557=CARTESIAN_POINT('Ctrl Pts',(-1.01778810567665,-0.587620236790415,
-1.72083333333333));
#358558=CARTESIAN_POINT('Ctrl Pts',(-0.937699045799837,-0.726338557627484,
-1.71099716760418));
#358559=CARTESIAN_POINT('Ctrl Pts',(-0.823407874165082,-0.838564036615828,
-1.7));
#358560=CARTESIAN_POINT('Origin',(-1.38777878078146E-16,-5.55111512312578E-15,
-17.91875));
#358561=CARTESIAN_POINT('',(2.36911999758087E-14,-1.17524047358083,-2.7));
#358562=CARTESIAN_POINT('',(2.37896554308489E-14,-1.17524047358083,-2.6375));
#358563=CARTESIAN_POINT('',(-4.21481204576211E-16,-1.17524047358085,-17.91875));
#358564=CARTESIAN_POINT('Ctrl Pts',(-1.43925448419918E-16,-1.17524047358083,
-2.7));
#358565=CARTESIAN_POINT('Ctrl Pts',(0.678525403784434,-1.17524047358083,
-2.65833333333333));
#358566=CARTESIAN_POINT('Ctrl Pts',(1.01778810567665,-0.587620236790415,
-2.61666666666667));
#358567=CARTESIAN_POINT('Ctrl Pts',(1.35705080756887,-7.83643681529645E-16,
-2.575));
#358568=CARTESIAN_POINT('Ctrl Pts',(1.01778810567665,0.587620236790413,
-2.53333333333334));
#358569=CARTESIAN_POINT('Ctrl Pts',(0.678525403784435,1.17524047358083,
-2.49166666666667));
#358570=CARTESIAN_POINT('Ctrl Pts',(0.,1.17524047358083,-2.45));
#358571=CARTESIAN_POINT('Ctrl Pts',(-0.678525403784434,1.17524047358083,
-2.40833333333333));
#358572=CARTESIAN_POINT('Ctrl Pts',(-1.01778810567665,0.587620236790414,
-2.36666666666667));
#358573=CARTESIAN_POINT('Ctrl Pts',(-1.35705080756887,-5.60536015722306E-16,
-2.325));
#358574=CARTESIAN_POINT('Ctrl Pts',(-1.01778810567665,-0.587620236790415,
-2.28333333333333));
#358575=CARTESIAN_POINT('Ctrl Pts',(-0.678525403784435,-1.17524047358083,
-2.24166666666667));
#358576=CARTESIAN_POINT('Ctrl Pts',(-1.43925448419918E-16,-1.17524047358083,
-2.2));
#358577=CARTESIAN_POINT('Ctrl Pts',(-1.43925448419918E-16,-1.17524047358083,
-2.6375));
#358578=CARTESIAN_POINT('Ctrl Pts',(0.678525403784434,-1.17524047358083,
-2.59583333333333));
#358579=CARTESIAN_POINT('Ctrl Pts',(1.01778810567665,-0.587620236790415,
-2.55416666666667));
#358580=CARTESIAN_POINT('Ctrl Pts',(1.35705080756887,-8.10962161466288E-16,
-2.5125));
#358581=CARTESIAN_POINT('Ctrl Pts',(1.01778810567665,0.587620236790413,
-2.47083333333334));
#358582=CARTESIAN_POINT('Ctrl Pts',(0.678525403784435,1.17524047358083,
-2.42916666666667));
#358583=CARTESIAN_POINT('Ctrl Pts',(0.,1.17524047358083,-2.3875));
#358584=CARTESIAN_POINT('Ctrl Pts',(-0.678525403784434,1.17524047358083,
-2.34583333333333));
#358585=CARTESIAN_POINT('Ctrl Pts',(-1.01778810567665,0.587620236790414,
-2.30416666666667));
#358586=CARTESIAN_POINT('Ctrl Pts',(-1.35705080756887,-5.87854495658949E-16,
-2.2625));
#358587=CARTESIAN_POINT('Ctrl Pts',(-1.01778810567665,-0.587620236790415,
-2.22083333333333));
#358588=CARTESIAN_POINT('Ctrl Pts',(-0.678525403784435,-1.17524047358083,
-2.17916666666667));
#358589=CARTESIAN_POINT('Ctrl Pts',(-1.43925448419918E-16,-1.17524047358083,
-2.1375));
#358590=CARTESIAN_POINT('Origin',(-1.38777878078146E-16,-5.55111512312578E-15,
-17.91875));
#358591=CARTESIAN_POINT('',(2.29035563354865E-14,-1.17524047358083,-3.2));
#358592=CARTESIAN_POINT('',(2.30020117905267E-14,-1.17524047358083,-3.1375));
#358593=CARTESIAN_POINT('',(-4.21481204576211E-16,-1.17524047358085,-17.91875));
#358594=CARTESIAN_POINT('Ctrl Pts',(-1.43925448419918E-16,-1.17524047358083,
-3.2));
#358595=CARTESIAN_POINT('Ctrl Pts',(0.678525403784434,-1.17524047358083,
-3.15833333333333));
#358596=CARTESIAN_POINT('Ctrl Pts',(1.01778810567665,-0.587620236790415,
-3.11666666666667));
#358597=CARTESIAN_POINT('Ctrl Pts',(1.35705080756887,-5.65095842036504E-16,
-3.075));
#358598=CARTESIAN_POINT('Ctrl Pts',(1.01778810567665,0.587620236790413,
-3.03333333333333));
#358599=CARTESIAN_POINT('Ctrl Pts',(0.678525403784435,1.17524047358083,
-2.99166666666667));
#358600=CARTESIAN_POINT('Ctrl Pts',(0.,1.17524047358083,-2.95));
#358601=CARTESIAN_POINT('Ctrl Pts',(-0.678525403784434,1.17524047358083,
-2.90833333333333));
#358602=CARTESIAN_POINT('Ctrl Pts',(-1.01778810567665,0.587620236790414,
-2.86666666666667));
#358603=CARTESIAN_POINT('Ctrl Pts',(-1.35705080756887,-3.41988176229165E-16,
-2.825));
#358604=CARTESIAN_POINT('Ctrl Pts',(-1.01778810567665,-0.587620236790414,
-2.78333333333333));
#358605=CARTESIAN_POINT('Ctrl Pts',(-0.678525403784435,-1.17524047358083,
-2.74166666666667));
#358606=CARTESIAN_POINT('Ctrl Pts',(-1.43925448419918E-16,-1.17524047358083,
-2.7));
#358607=CARTESIAN_POINT('Ctrl Pts',(-1.43925448419918E-16,-1.17524047358083,
-3.1375));
#358608=CARTESIAN_POINT('Ctrl Pts',(0.678525403784434,-1.17524047358083,
-3.09583333333333));
#358609=CARTESIAN_POINT('Ctrl Pts',(1.01778810567665,-0.587620236790415,
-3.05416666666667));
#358610=CARTESIAN_POINT('Ctrl Pts',(1.35705080756887,-5.92414321973146E-16,
-3.0125));
#358611=CARTESIAN_POINT('Ctrl Pts',(1.01778810567665,0.587620236790413,
-2.97083333333333));
#358612=CARTESIAN_POINT('Ctrl Pts',(0.678525403784435,1.17524047358083,
-2.92916666666667));
#358613=CARTESIAN_POINT('Ctrl Pts',(0.,1.17524047358083,-2.8875));
#358614=CARTESIAN_POINT('Ctrl Pts',(-0.678525403784434,1.17524047358083,
-2.84583333333333));
#358615=CARTESIAN_POINT('Ctrl Pts',(-1.01778810567665,0.587620236790414,
-2.80416666666667));
#358616=CARTESIAN_POINT('Ctrl Pts',(-1.35705080756887,-3.69306656165807E-16,
-2.7625));
#358617=CARTESIAN_POINT('Ctrl Pts',(-1.01778810567665,-0.587620236790414,
-2.72083333333333));
#358618=CARTESIAN_POINT('Ctrl Pts',(-0.678525403784435,-1.17524047358083,
-2.67916666666667));
#358619=CARTESIAN_POINT('Ctrl Pts',(-1.43925448419918E-16,-1.17524047358083,
-2.6375));
#358620=CARTESIAN_POINT('Origin',(-1.38777878078146E-16,-5.55111512312578E-15,
-17.91875));
#358621=CARTESIAN_POINT('',(2.21159126951643E-14,-1.17524047358083,-3.7));
#358622=CARTESIAN_POINT('',(2.22143681502045E-14,-1.17524047358083,-3.6375));
#358623=CARTESIAN_POINT('',(-4.21481204576211E-16,-1.17524047358085,-17.91875));
#358624=CARTESIAN_POINT('Ctrl Pts',(-1.43925448419918E-16,-1.17524047358083,
-3.7));
#358625=CARTESIAN_POINT('Ctrl Pts',(0.678525403784434,-1.17524047358083,
-3.65833333333333));
#358626=CARTESIAN_POINT('Ctrl Pts',(1.01778810567665,-0.587620236790415,
-3.61666666666667));
#358627=CARTESIAN_POINT('Ctrl Pts',(1.35705080756887,-3.46548002543362E-16,
-3.575));
#358628=CARTESIAN_POINT('Ctrl Pts',(1.01778810567665,0.587620236790413,
-3.53333333333333));
#358629=CARTESIAN_POINT('Ctrl Pts',(0.678525403784435,1.17524047358083,
-3.49166666666667));
#358630=CARTESIAN_POINT('Ctrl Pts',(0.,1.17524047358083,-3.45));
#358631=CARTESIAN_POINT('Ctrl Pts',(-0.678525403784434,1.17524047358083,
-3.40833333333333));
#358632=CARTESIAN_POINT('Ctrl Pts',(-1.01778810567665,0.587620236790414,
-3.36666666666667));
#358633=CARTESIAN_POINT('Ctrl Pts',(-1.35705080756887,-1.23440336736023E-16,
-3.325));
#358634=CARTESIAN_POINT('Ctrl Pts',(-1.01778810567665,-0.587620236790414,
-3.28333333333333));
#358635=CARTESIAN_POINT('Ctrl Pts',(-0.678525403784435,-1.17524047358083,
-3.24166666666667));
#358636=CARTESIAN_POINT('Ctrl Pts',(-1.43925448419918E-16,-1.17524047358083,
-3.2));
#358637=CARTESIAN_POINT('Ctrl Pts',(-1.43925448419918E-16,-1.17524047358083,
-3.6375));
#358638=CARTESIAN_POINT('Ctrl Pts',(0.678525403784434,-1.17524047358083,
-3.59583333333333));
#358639=CARTESIAN_POINT('Ctrl Pts',(1.01778810567665,-0.587620236790415,
-3.55416666666667));
#358640=CARTESIAN_POINT('Ctrl Pts',(1.35705080756887,-3.73866482480005E-16,
-3.5125));
#358641=CARTESIAN_POINT('Ctrl Pts',(1.01778810567665,0.587620236790413,
-3.47083333333333));
#358642=CARTESIAN_POINT('Ctrl Pts',(0.678525403784435,1.17524047358083,
-3.42916666666667));
#358643=CARTESIAN_POINT('Ctrl Pts',(0.,1.17524047358083,-3.3875));
#358644=CARTESIAN_POINT('Ctrl Pts',(-0.678525403784434,1.17524047358083,
-3.34583333333333));
#358645=CARTESIAN_POINT('Ctrl Pts',(-1.01778810567665,0.587620236790414,
-3.30416666666667));
#358646=CARTESIAN_POINT('Ctrl Pts',(-1.35705080756887,-1.50758816672666E-16,
-3.2625));
#358647=CARTESIAN_POINT('Ctrl Pts',(-1.01778810567665,-0.587620236790414,
-3.22083333333333));
#358648=CARTESIAN_POINT('Ctrl Pts',(-0.678525403784435,-1.17524047358083,
-3.17916666666667));
#358649=CARTESIAN_POINT('Ctrl Pts',(-1.43925448419918E-16,-1.17524047358083,
-3.1375));
#358650=CARTESIAN_POINT('Origin',(-1.38777878078146E-16,-5.55111512312578E-15,
-17.91875));
#358651=CARTESIAN_POINT('',(2.13282690548421E-14,-1.17524047358083,-4.2));
#358652=CARTESIAN_POINT('',(2.14267245098824E-14,-1.17524047358083,-4.1375));
#358653=CARTESIAN_POINT('',(-4.21481204576211E-16,-1.17524047358085,-17.91875));
#358654=CARTESIAN_POINT('Ctrl Pts',(-1.43925448419918E-16,-1.17524047358083,
-4.2));
#358655=CARTESIAN_POINT('Ctrl Pts',(0.678525403784434,-1.17524047358083,
-4.15833333333333));
#358656=CARTESIAN_POINT('Ctrl Pts',(1.01778810567665,-0.587620236790415,
-4.11666666666667));
#358657=CARTESIAN_POINT('Ctrl Pts',(1.35705080756887,-1.28000163050222E-16,
-4.075));
#358658=CARTESIAN_POINT('Ctrl Pts',(1.01778810567665,0.587620236790413,
-4.03333333333333));
#358659=CARTESIAN_POINT('Ctrl Pts',(0.678525403784435,1.17524047358083,
-3.99166666666667));
#358660=CARTESIAN_POINT('Ctrl Pts',(0.,1.17524047358083,-3.95));
#358661=CARTESIAN_POINT('Ctrl Pts',(-0.678525403784434,1.17524047358083,
-3.90833333333334));
#358662=CARTESIAN_POINT('Ctrl Pts',(-1.01778810567665,0.587620236790414,
-3.86666666666667));
#358663=CARTESIAN_POINT('Ctrl Pts',(-1.35705080756887,9.5107502757118E-17,
-3.825));
#358664=CARTESIAN_POINT('Ctrl Pts',(-1.01778810567665,-0.587620236790414,
-3.78333333333333));
#358665=CARTESIAN_POINT('Ctrl Pts',(-0.678525403784435,-1.17524047358083,
-3.74166666666667));
#358666=CARTESIAN_POINT('Ctrl Pts',(-1.43925448419918E-16,-1.17524047358083,
-3.7));
#358667=CARTESIAN_POINT('Ctrl Pts',(-1.43925448419918E-16,-1.17524047358083,
-4.1375));
#358668=CARTESIAN_POINT('Ctrl Pts',(0.678525403784434,-1.17524047358083,
-4.09583333333333));
#358669=CARTESIAN_POINT('Ctrl Pts',(1.01778810567665,-0.587620236790415,
-4.05416666666667));
#358670=CARTESIAN_POINT('Ctrl Pts',(1.35705080756887,-1.55318642986864E-16,
-4.0125));
#358671=CARTESIAN_POINT('Ctrl Pts',(1.01778810567665,0.587620236790414,
-3.97083333333333));
#358672=CARTESIAN_POINT('Ctrl Pts',(0.678525403784435,1.17524047358083,
-3.92916666666667));
#358673=CARTESIAN_POINT('Ctrl Pts',(0.,1.17524047358083,-3.8875));
#358674=CARTESIAN_POINT('Ctrl Pts',(-0.678525403784434,1.17524047358083,
-3.84583333333333));
#358675=CARTESIAN_POINT('Ctrl Pts',(-1.01778810567665,0.587620236790414,
-3.80416666666667));
#358676=CARTESIAN_POINT('Ctrl Pts',(-1.35705080756887,6.77890228204754E-17,
-3.7625));
#358677=CARTESIAN_POINT('Ctrl Pts',(-1.01778810567665,-0.587620236790414,
-3.72083333333333));
#358678=CARTESIAN_POINT('Ctrl Pts',(-0.678525403784435,-1.17524047358083,
-3.67916666666667));
#358679=CARTESIAN_POINT('Ctrl Pts',(-1.43925448419918E-16,-1.17524047358083,
-3.6375));
#358680=CARTESIAN_POINT('Origin',(-1.38777878078146E-16,-5.55111512312578E-15,
-17.91875));
#358681=CARTESIAN_POINT('',(2.05406254145199E-14,-1.17524047358083,-4.7));
#358682=CARTESIAN_POINT('',(2.06390808695602E-14,-1.17524047358083,-4.6375));
#358683=CARTESIAN_POINT('',(-4.21481204576211E-16,-1.17524047358085,-17.91875));
#358684=CARTESIAN_POINT('Ctrl Pts',(-1.43925448419918E-16,-1.17524047358083,
-4.7));
#358685=CARTESIAN_POINT('Ctrl Pts',(0.678525403784434,-1.17524047358083,
-4.65833333333333));
#358686=CARTESIAN_POINT('Ctrl Pts',(1.01778810567665,-0.587620236790414,
-4.61666666666667));
#358687=CARTESIAN_POINT('Ctrl Pts',(1.35705080756887,9.05476764429197E-17,
-4.575));
#358688=CARTESIAN_POINT('Ctrl Pts',(1.01778810567665,0.587620236790414,
-4.53333333333333));
#358689=CARTESIAN_POINT('Ctrl Pts',(0.678525403784435,1.17524047358083,
-4.49166666666667));
#358690=CARTESIAN_POINT('Ctrl Pts',(0.,1.17524047358083,-4.45));
#358691=CARTESIAN_POINT('Ctrl Pts',(-0.678525403784434,1.17524047358083,
-4.40833333333333));
#358692=CARTESIAN_POINT('Ctrl Pts',(-1.01778810567665,0.587620236790414,
-4.36666666666667));
#358693=CARTESIAN_POINT('Ctrl Pts',(-1.35705080756887,3.13655342250259E-16,
-4.325));
#358694=CARTESIAN_POINT('Ctrl Pts',(-1.01778810567665,-0.587620236790414,
-4.28333333333333));
#358695=CARTESIAN_POINT('Ctrl Pts',(-0.678525403784435,-1.17524047358083,
-4.24166666666667));
#358696=CARTESIAN_POINT('Ctrl Pts',(-1.43925448419918E-16,-1.17524047358083,
-4.2));
#358697=CARTESIAN_POINT('Ctrl Pts',(-1.43925448419918E-16,-1.17524047358083,
-4.6375));
#358698=CARTESIAN_POINT('Ctrl Pts',(0.678525403784434,-1.17524047358083,
-4.59583333333333));
#358699=CARTESIAN_POINT('Ctrl Pts',(1.01778810567665,-0.587620236790414,
-4.55416666666667));
#358700=CARTESIAN_POINT('Ctrl Pts',(1.35705080756887,6.32291965062771E-17,
-4.5125));
#358701=CARTESIAN_POINT('Ctrl Pts',(1.01778810567665,0.587620236790414,
-4.47083333333333));
#358702=CARTESIAN_POINT('Ctrl Pts',(0.678525403784435,1.17524047358083,
-4.42916666666667));
#358703=CARTESIAN_POINT('Ctrl Pts',(0.,1.17524047358083,-4.3875));
#358704=CARTESIAN_POINT('Ctrl Pts',(-0.678525403784434,1.17524047358083,
-4.34583333333333));
#358705=CARTESIAN_POINT('Ctrl Pts',(-1.01778810567665,0.587620236790415,
-4.30416666666667));
#358706=CARTESIAN_POINT('Ctrl Pts',(-1.35705080756887,2.86336862313616E-16,
-4.2625));
#358707=CARTESIAN_POINT('Ctrl Pts',(-1.01778810567665,-0.587620236790414,
-4.22083333333333));
#358708=CARTESIAN_POINT('Ctrl Pts',(-0.678525403784435,-1.17524047358083,
-4.17916666666667));
#358709=CARTESIAN_POINT('Ctrl Pts',(-1.43925448419918E-16,-1.17524047358083,
-4.1375));
#358710=CARTESIAN_POINT('Origin',(-1.38777878078146E-16,-5.55111512312578E-15,
-17.91875));
#358711=CARTESIAN_POINT('',(1.97529817741977E-14,-1.17524047358083,-5.2));
#358712=CARTESIAN_POINT('',(1.9851437229238E-14,-1.17524047358083,-5.1375));
#358713=CARTESIAN_POINT('',(-4.21481204576211E-16,-1.17524047358085,-17.91875));
#358714=CARTESIAN_POINT('Ctrl Pts',(-1.43925448419918E-16,-1.17524047358083,
-5.2));
#358715=CARTESIAN_POINT('Ctrl Pts',(0.678525403784434,-1.17524047358083,
-5.15833333333333));
#358716=CARTESIAN_POINT('Ctrl Pts',(1.01778810567665,-0.587620236790414,
-5.11666666666667));
#358717=CARTESIAN_POINT('Ctrl Pts',(1.35705080756887,3.09095515936061E-16,
-5.075));
#358718=CARTESIAN_POINT('Ctrl Pts',(1.01778810567665,0.587620236790414,
-5.03333333333333));
#358719=CARTESIAN_POINT('Ctrl Pts',(0.678525403784435,1.17524047358083,
-4.99166666666667));
#358720=CARTESIAN_POINT('Ctrl Pts',(0.,1.17524047358083,-4.95));
#358721=CARTESIAN_POINT('Ctrl Pts',(-0.678525403784434,1.17524047358083,
-4.90833333333333));
#358722=CARTESIAN_POINT('Ctrl Pts',(-1.01778810567665,0.587620236790415,
-4.86666666666667));
#358723=CARTESIAN_POINT('Ctrl Pts',(-1.35705080756887,5.322031817434E-16,
-4.825));
#358724=CARTESIAN_POINT('Ctrl Pts',(-1.01778810567665,-0.587620236790414,
-4.78333333333333));
#358725=CARTESIAN_POINT('Ctrl Pts',(-0.678525403784435,-1.17524047358083,
-4.74166666666667));
#358726=CARTESIAN_POINT('Ctrl Pts',(-1.43925448419918E-16,-1.17524047358083,
-4.7));
#358727=CARTESIAN_POINT('Ctrl Pts',(-1.43925448419918E-16,-1.17524047358083,
-5.1375));
#358728=CARTESIAN_POINT('Ctrl Pts',(0.678525403784434,-1.17524047358083,
-5.09583333333333));
#358729=CARTESIAN_POINT('Ctrl Pts',(1.01778810567665,-0.587620236790414,
-5.05416666666667));
#358730=CARTESIAN_POINT('Ctrl Pts',(1.35705080756887,2.81777035999419E-16,
-5.0125));
#358731=CARTESIAN_POINT('Ctrl Pts',(1.01778810567665,0.587620236790414,
-4.97083333333333));
#358732=CARTESIAN_POINT('Ctrl Pts',(0.678525403784435,1.17524047358083,
-4.92916666666667));
#358733=CARTESIAN_POINT('Ctrl Pts',(0.,1.17524047358083,-4.8875));
#358734=CARTESIAN_POINT('Ctrl Pts',(-0.678525403784434,1.17524047358083,
-4.84583333333333));
#358735=CARTESIAN_POINT('Ctrl Pts',(-1.01778810567665,0.587620236790415,
-4.80416666666667));
#358736=CARTESIAN_POINT('Ctrl Pts',(-1.35705080756887,5.04884701806758E-16,
-4.7625));
#358737=CARTESIAN_POINT('Ctrl Pts',(-1.01778810567665,-0.587620236790414,
-4.72083333333333));
#358738=CARTESIAN_POINT('Ctrl Pts',(-0.678525403784435,-1.17524047358083,
-4.67916666666667));
#358739=CARTESIAN_POINT('Ctrl Pts',(-1.43925448419918E-16,-1.17524047358083,
-4.6375));
#358740=CARTESIAN_POINT('Origin',(-1.38777878078146E-16,-5.55111512312578E-15,
-17.91875));
#358741=CARTESIAN_POINT('',(1.89653381338755E-14,-1.17524047358083,-5.7));
#358742=CARTESIAN_POINT('',(1.90637935889158E-14,-1.17524047358083,-5.6375));
#358743=CARTESIAN_POINT('',(-4.21481204576211E-16,-1.17524047358085,-17.91875));
#358744=CARTESIAN_POINT('Ctrl Pts',(-1.43925448419918E-16,-1.17524047358083,
-5.7));
#358745=CARTESIAN_POINT('Ctrl Pts',(0.678525403784434,-1.17524047358083,
-5.65833333333333));
#358746=CARTESIAN_POINT('Ctrl Pts',(1.01778810567665,-0.587620236790414,
-5.61666666666667));
#358747=CARTESIAN_POINT('Ctrl Pts',(1.35705080756887,5.27643355429203E-16,
-5.575));
#358748=CARTESIAN_POINT('Ctrl Pts',(1.01778810567665,0.587620236790414,
-5.53333333333334));
#358749=CARTESIAN_POINT('Ctrl Pts',(0.678525403784435,1.17524047358083,
-5.49166666666667));
#358750=CARTESIAN_POINT('Ctrl Pts',(0.,1.17524047358083,-5.45));
#358751=CARTESIAN_POINT('Ctrl Pts',(-0.678525403784434,1.17524047358083,
-5.40833333333333));
#358752=CARTESIAN_POINT('Ctrl Pts',(-1.01778810567665,0.587620236790415,
-5.36666666666667));
#358753=CARTESIAN_POINT('Ctrl Pts',(-1.35705080756887,7.50751021236542E-16,
-5.325));
#358754=CARTESIAN_POINT('Ctrl Pts',(-1.01778810567665,-0.587620236790413,
-5.28333333333333));
#358755=CARTESIAN_POINT('Ctrl Pts',(-0.678525403784435,-1.17524047358083,
-5.24166666666667));
#358756=CARTESIAN_POINT('Ctrl Pts',(-1.43925448419918E-16,-1.17524047358083,
-5.2));
#358757=CARTESIAN_POINT('Ctrl Pts',(-1.43925448419918E-16,-1.17524047358083,
-5.6375));
#358758=CARTESIAN_POINT('Ctrl Pts',(0.678525403784434,-1.17524047358083,
-5.59583333333333));
#358759=CARTESIAN_POINT('Ctrl Pts',(1.01778810567665,-0.587620236790414,
-5.55416666666667));
#358760=CARTESIAN_POINT('Ctrl Pts',(1.35705080756887,5.0032487549256E-16,
-5.5125));
#358761=CARTESIAN_POINT('Ctrl Pts',(1.01778810567665,0.587620236790414,
-5.47083333333333));
#358762=CARTESIAN_POINT('Ctrl Pts',(0.678525403784435,1.17524047358083,
-5.42916666666667));
#358763=CARTESIAN_POINT('Ctrl Pts',(0.,1.17524047358083,-5.3875));
#358764=CARTESIAN_POINT('Ctrl Pts',(-0.678525403784434,1.17524047358083,
-5.34583333333333));
#358765=CARTESIAN_POINT('Ctrl Pts',(-1.01778810567665,0.587620236790415,
-5.30416666666667));
#358766=CARTESIAN_POINT('Ctrl Pts',(-1.35705080756887,7.23432541299899E-16,
-5.2625));
#358767=CARTESIAN_POINT('Ctrl Pts',(-1.01778810567665,-0.587620236790413,
-5.22083333333333));
#358768=CARTESIAN_POINT('Ctrl Pts',(-0.678525403784435,-1.17524047358083,
-5.17916666666667));
#358769=CARTESIAN_POINT('Ctrl Pts',(-1.43925448419918E-16,-1.17524047358083,
-5.1375));
#358770=CARTESIAN_POINT('Origin',(-1.38777878078146E-16,-5.55111512312578E-15,
-17.91875));
#358771=CARTESIAN_POINT('',(1.81776944935533E-14,-1.17524047358083,-6.2));
#358772=CARTESIAN_POINT('',(1.82761499485936E-14,-1.17524047358083,-6.1375));
#358773=CARTESIAN_POINT('',(-4.21481204576211E-16,-1.17524047358085,-17.91875));
#358774=CARTESIAN_POINT('Ctrl Pts',(-1.43925448419918E-16,-1.17524047358083,
-6.2));
#358775=CARTESIAN_POINT('Ctrl Pts',(0.678525403784434,-1.17524047358083,
-6.15833333333334));
#358776=CARTESIAN_POINT('Ctrl Pts',(1.01778810567665,-0.587620236790414,
-6.11666666666667));
#358777=CARTESIAN_POINT('Ctrl Pts',(1.35705080756887,7.46191194922343E-16,
-6.075));
#358778=CARTESIAN_POINT('Ctrl Pts',(1.01778810567665,0.587620236790414,
-6.03333333333333));
#358779=CARTESIAN_POINT('Ctrl Pts',(0.678525403784435,1.17524047358083,
-5.99166666666667));
#358780=CARTESIAN_POINT('Ctrl Pts',(0.,1.17524047358083,-5.95));
#358781=CARTESIAN_POINT('Ctrl Pts',(-0.678525403784434,1.17524047358083,
-5.90833333333333));
#358782=CARTESIAN_POINT('Ctrl Pts',(-1.01778810567665,0.587620236790415,
-5.86666666666667));
#358783=CARTESIAN_POINT('Ctrl Pts',(-1.35705080756887,9.69298860729681E-16,
-5.825));
#358784=CARTESIAN_POINT('Ctrl Pts',(-1.01778810567665,-0.587620236790413,
-5.78333333333333));
#358785=CARTESIAN_POINT('Ctrl Pts',(-0.678525403784435,-1.17524047358083,
-5.74166666666667));
#358786=CARTESIAN_POINT('Ctrl Pts',(-1.43925448419918E-16,-1.17524047358083,
-5.7));
#358787=CARTESIAN_POINT('Ctrl Pts',(-1.43925448419918E-16,-1.17524047358083,
-6.1375));
#358788=CARTESIAN_POINT('Ctrl Pts',(0.678525403784434,-1.17524047358083,
-6.09583333333334));
#358789=CARTESIAN_POINT('Ctrl Pts',(1.01778810567665,-0.587620236790414,
-6.05416666666667));
#358790=CARTESIAN_POINT('Ctrl Pts',(1.35705080756887,7.18872714985701E-16,
-6.0125));
#358791=CARTESIAN_POINT('Ctrl Pts',(1.01778810567665,0.587620236790414,
-5.97083333333333));
#358792=CARTESIAN_POINT('Ctrl Pts',(0.678525403784435,1.17524047358083,
-5.92916666666667));
#358793=CARTESIAN_POINT('Ctrl Pts',(0.,1.17524047358083,-5.8875));
#358794=CARTESIAN_POINT('Ctrl Pts',(-0.678525403784434,1.17524047358083,
-5.84583333333334));
#358795=CARTESIAN_POINT('Ctrl Pts',(-1.01778810567665,0.587620236790415,
-5.80416666666667));
#358796=CARTESIAN_POINT('Ctrl Pts',(-1.35705080756887,9.41980380793039E-16,
-5.7625));
#358797=CARTESIAN_POINT('Ctrl Pts',(-1.01778810567665,-0.587620236790413,
-5.72083333333333));
#358798=CARTESIAN_POINT('Ctrl Pts',(-0.678525403784435,-1.17524047358083,
-5.67916666666667));
#358799=CARTESIAN_POINT('Ctrl Pts',(-1.43925448419918E-16,-1.17524047358083,
-5.6375));
#358800=CARTESIAN_POINT('Origin',(-1.38777878078146E-16,-5.55111512312578E-15,
-17.91875));
#358801=CARTESIAN_POINT('',(1.73900508532311E-14,-1.17524047358083,-6.7));
#358802=CARTESIAN_POINT('',(1.74885063082714E-14,-1.17524047358083,-6.6375));
#358803=CARTESIAN_POINT('',(-4.21481204576211E-16,-1.17524047358085,-17.91875));
#358804=CARTESIAN_POINT('Ctrl Pts',(-1.43925448419918E-16,-1.17524047358083,
-6.7));
#358805=CARTESIAN_POINT('Ctrl Pts',(0.678525403784434,-1.17524047358083,
-6.65833333333333));
#358806=CARTESIAN_POINT('Ctrl Pts',(1.01778810567665,-0.587620236790414,
-6.61666666666667));
#358807=CARTESIAN_POINT('Ctrl Pts',(1.35705080756887,9.64739034415485E-16,
-6.575));
#358808=CARTESIAN_POINT('Ctrl Pts',(1.01778810567665,0.587620236790414,
-6.53333333333333));
#358809=CARTESIAN_POINT('Ctrl Pts',(0.678525403784435,1.17524047358083,
-6.49166666666667));
#358810=CARTESIAN_POINT('Ctrl Pts',(0.,1.17524047358083,-6.45));
#358811=CARTESIAN_POINT('Ctrl Pts',(-0.678525403784434,1.17524047358083,
-6.40833333333334));
#358812=CARTESIAN_POINT('Ctrl Pts',(-1.01778810567665,0.587620236790415,
-6.36666666666667));
#358813=CARTESIAN_POINT('Ctrl Pts',(-1.35705080756887,1.18784670022282E-15,
-6.325));
#358814=CARTESIAN_POINT('Ctrl Pts',(-1.01778810567665,-0.587620236790413,
-6.28333333333333));
#358815=CARTESIAN_POINT('Ctrl Pts',(-0.678525403784435,-1.17524047358083,
-6.24166666666667));
#358816=CARTESIAN_POINT('Ctrl Pts',(-1.43925448419918E-16,-1.17524047358083,
-6.2));
#358817=CARTESIAN_POINT('Ctrl Pts',(-1.43925448419918E-16,-1.17524047358083,
-6.6375));
#358818=CARTESIAN_POINT('Ctrl Pts',(0.678525403784434,-1.17524047358083,
-6.59583333333333));
#358819=CARTESIAN_POINT('Ctrl Pts',(1.01778810567665,-0.587620236790414,
-6.55416666666667));
#358820=CARTESIAN_POINT('Ctrl Pts',(1.35705080756887,9.37420554478842E-16,
-6.5125));
#358821=CARTESIAN_POINT('Ctrl Pts',(1.01778810567665,0.587620236790415,
-6.47083333333333));
#358822=CARTESIAN_POINT('Ctrl Pts',(0.678525403784435,1.17524047358083,
-6.42916666666667));
#358823=CARTESIAN_POINT('Ctrl Pts',(0.,1.17524047358083,-6.3875));
#358824=CARTESIAN_POINT('Ctrl Pts',(-0.678525403784434,1.17524047358083,
-6.34583333333333));
#358825=CARTESIAN_POINT('Ctrl Pts',(-1.01778810567665,0.587620236790415,
-6.30416666666667));
#358826=CARTESIAN_POINT('Ctrl Pts',(-1.35705080756887,1.16052822028618E-15,
-6.2625));
#358827=CARTESIAN_POINT('Ctrl Pts',(-1.01778810567665,-0.587620236790413,
-6.22083333333333));
#358828=CARTESIAN_POINT('Ctrl Pts',(-0.678525403784435,-1.17524047358083,
-6.17916666666667));
#358829=CARTESIAN_POINT('Ctrl Pts',(-1.43925448419918E-16,-1.17524047358083,
-6.1375));
#358830=CARTESIAN_POINT('Origin',(-1.38777878078146E-16,-5.55111512312578E-15,
-17.91875));
#358831=CARTESIAN_POINT('',(1.66024072129089E-14,-1.17524047358083,-7.2));
#358832=CARTESIAN_POINT('',(1.67008626679492E-14,-1.17524047358083,-7.1375));
#358833=CARTESIAN_POINT('',(-4.21481204576211E-16,-1.17524047358085,-17.91875));
#358834=CARTESIAN_POINT('Ctrl Pts',(-1.43925448419918E-16,-1.17524047358083,
-7.2));
#358835=CARTESIAN_POINT('Ctrl Pts',(0.678525403784434,-1.17524047358083,
-7.15833333333333));
#358836=CARTESIAN_POINT('Ctrl Pts',(1.01778810567665,-0.587620236790413,
-7.11666666666667));
#358837=CARTESIAN_POINT('Ctrl Pts',(1.35705080756887,1.18328687390863E-15,
-7.075));
#358838=CARTESIAN_POINT('Ctrl Pts',(1.01778810567665,0.587620236790415,
-7.03333333333333));
#358839=CARTESIAN_POINT('Ctrl Pts',(0.678525403784435,1.17524047358083,
-6.99166666666667));
#358840=CARTESIAN_POINT('Ctrl Pts',(0.,1.17524047358083,-6.95));
#358841=CARTESIAN_POINT('Ctrl Pts',(-0.678525403784434,1.17524047358083,
-6.90833333333333));
#358842=CARTESIAN_POINT('Ctrl Pts',(-1.01778810567665,0.587620236790415,
-6.86666666666667));
#358843=CARTESIAN_POINT('Ctrl Pts',(-1.35705080756887,1.40639453971596E-15,
-6.825));
#358844=CARTESIAN_POINT('Ctrl Pts',(-1.01778810567665,-0.587620236790413,
-6.78333333333333));
#358845=CARTESIAN_POINT('Ctrl Pts',(-0.678525403784435,-1.17524047358083,
-6.74166666666667));
#358846=CARTESIAN_POINT('Ctrl Pts',(-1.43925448419918E-16,-1.17524047358083,
-6.7));
#358847=CARTESIAN_POINT('Ctrl Pts',(-1.43925448419918E-16,-1.17524047358083,
-7.1375));
#358848=CARTESIAN_POINT('Ctrl Pts',(0.678525403784434,-1.17524047358083,
-7.09583333333333));
#358849=CARTESIAN_POINT('Ctrl Pts',(1.01778810567665,-0.587620236790413,
-7.05416666666667));
#358850=CARTESIAN_POINT('Ctrl Pts',(1.35705080756887,1.15596839397198E-15,
-7.0125));
#358851=CARTESIAN_POINT('Ctrl Pts',(1.01778810567665,0.587620236790415,
-6.97083333333333));
#358852=CARTESIAN_POINT('Ctrl Pts',(0.678525403784435,1.17524047358083,
-6.92916666666667));
#358853=CARTESIAN_POINT('Ctrl Pts',(0.,1.17524047358083,-6.8875));
#358854=CARTESIAN_POINT('Ctrl Pts',(-0.678525403784434,1.17524047358083,
-6.84583333333333));
#358855=CARTESIAN_POINT('Ctrl Pts',(-1.01778810567665,0.587620236790416,
-6.80416666666667));
#358856=CARTESIAN_POINT('Ctrl Pts',(-1.35705080756887,1.37907605977932E-15,
-6.7625));
#358857=CARTESIAN_POINT('Ctrl Pts',(-1.01778810567665,-0.587620236790413,
-6.72083333333333));
#358858=CARTESIAN_POINT('Ctrl Pts',(-0.678525403784435,-1.17524047358083,
-6.67916666666667));
#358859=CARTESIAN_POINT('Ctrl Pts',(-1.43925448419918E-16,-1.17524047358083,
-6.6375));
#358860=CARTESIAN_POINT('Origin',(-1.38777878078146E-16,-5.55111512312578E-15,
-17.91875));
#358861=CARTESIAN_POINT('',(1.58147635725867E-14,-1.17524047358083,-7.7));
#358862=CARTESIAN_POINT('',(1.5913219027627E-14,-1.17524047358083,-7.6375));
#358863=CARTESIAN_POINT('',(-4.21481204576211E-16,-1.17524047358085,-17.91875));
#358864=CARTESIAN_POINT('Ctrl Pts',(-1.43925448419918E-16,-1.17524047358083,
-7.7));
#358865=CARTESIAN_POINT('Ctrl Pts',(0.678525403784434,-1.17524047358083,
-7.65833333333334));
#358866=CARTESIAN_POINT('Ctrl Pts',(1.01778810567665,-0.587620236790413,
-7.61666666666667));
#358867=CARTESIAN_POINT('Ctrl Pts',(1.35705080756887,1.40183471340177E-15,
-7.575));
#358868=CARTESIAN_POINT('Ctrl Pts',(1.01778810567665,0.587620236790415,
-7.53333333333333));
#358869=CARTESIAN_POINT('Ctrl Pts',(0.678525403784435,1.17524047358083,
-7.49166666666667));
#358870=CARTESIAN_POINT('Ctrl Pts',(0.,1.17524047358083,-7.45));
#358871=CARTESIAN_POINT('Ctrl Pts',(-0.678525403784434,1.17524047358083,
-7.40833333333333));
#358872=CARTESIAN_POINT('Ctrl Pts',(-1.01778810567665,0.587620236790416,
-7.36666666666667));
#358873=CARTESIAN_POINT('Ctrl Pts',(-1.35705080756887,1.62494237920911E-15,
-7.325));
#358874=CARTESIAN_POINT('Ctrl Pts',(-1.01778810567665,-0.587620236790412,
-7.28333333333333));
#358875=CARTESIAN_POINT('Ctrl Pts',(-0.678525403784435,-1.17524047358083,
-7.24166666666667));
#358876=CARTESIAN_POINT('Ctrl Pts',(-1.43925448419918E-16,-1.17524047358083,
-7.2));
#358877=CARTESIAN_POINT('Ctrl Pts',(-1.43925448419918E-16,-1.17524047358083,
-7.6375));
#358878=CARTESIAN_POINT('Ctrl Pts',(0.678525403784434,-1.17524047358083,
-7.59583333333333));
#358879=CARTESIAN_POINT('Ctrl Pts',(1.01778810567665,-0.587620236790413,
-7.55416666666667));
#358880=CARTESIAN_POINT('Ctrl Pts',(1.35705080756887,1.37451623346513E-15,
-7.5125));
#358881=CARTESIAN_POINT('Ctrl Pts',(1.01778810567665,0.587620236790415,
-7.47083333333333));
#358882=CARTESIAN_POINT('Ctrl Pts',(0.678525403784435,1.17524047358083,
-7.42916666666667));
#358883=CARTESIAN_POINT('Ctrl Pts',(0.,1.17524047358083,-7.3875));
#358884=CARTESIAN_POINT('Ctrl Pts',(-0.678525403784434,1.17524047358083,
-7.34583333333333));
#358885=CARTESIAN_POINT('Ctrl Pts',(-1.01778810567665,0.587620236790416,
-7.30416666666667));
#358886=CARTESIAN_POINT('Ctrl Pts',(-1.35705080756887,1.59762389927246E-15,
-7.2625));
#358887=CARTESIAN_POINT('Ctrl Pts',(-1.01778810567665,-0.587620236790412,
-7.22083333333333));
#358888=CARTESIAN_POINT('Ctrl Pts',(-0.678525403784435,-1.17524047358083,
-7.17916666666667));
#358889=CARTESIAN_POINT('Ctrl Pts',(-1.43925448419918E-16,-1.17524047358083,
-7.1375));
#358890=CARTESIAN_POINT('Origin',(-1.38777878078146E-16,-5.55111512312578E-15,
-17.91875));
#358891=CARTESIAN_POINT('',(1.50271199322645E-14,-1.17524047358083,-8.2));
#358892=CARTESIAN_POINT('',(1.51255753873048E-14,-1.17524047358083,-8.1375));
#358893=CARTESIAN_POINT('',(-4.21481204576211E-16,-1.17524047358085,-17.91875));
#358894=CARTESIAN_POINT('Ctrl Pts',(-1.43925448419918E-16,-1.17524047358083,
-8.2));
#358895=CARTESIAN_POINT('Ctrl Pts',(0.678525403784434,-1.17524047358083,
-8.15833333333333));
#358896=CARTESIAN_POINT('Ctrl Pts',(1.01778810567665,-0.587620236790413,
-8.11666666666667));
#358897=CARTESIAN_POINT('Ctrl Pts',(1.35705080756887,1.62038255289491E-15,
-8.075));
#358898=CARTESIAN_POINT('Ctrl Pts',(1.01778810567665,0.587620236790415,
-8.03333333333333));
#358899=CARTESIAN_POINT('Ctrl Pts',(0.678525403784435,1.17524047358083,
-7.99166666666667));
#358900=CARTESIAN_POINT('Ctrl Pts',(0.,1.17524047358083,-7.95));
#358901=CARTESIAN_POINT('Ctrl Pts',(-0.678525403784434,1.17524047358083,
-7.90833333333333));
#358902=CARTESIAN_POINT('Ctrl Pts',(-1.01778810567665,0.587620236790416,
-7.86666666666667));
#358903=CARTESIAN_POINT('Ctrl Pts',(-1.35705080756887,1.84349021870225E-15,
-7.825));
#358904=CARTESIAN_POINT('Ctrl Pts',(-1.01778810567665,-0.587620236790412,
-7.78333333333333));
#358905=CARTESIAN_POINT('Ctrl Pts',(-0.678525403784435,-1.17524047358083,
-7.74166666666667));
#358906=CARTESIAN_POINT('Ctrl Pts',(-1.43925448419918E-16,-1.17524047358083,
-7.7));
#358907=CARTESIAN_POINT('Ctrl Pts',(-1.43925448419918E-16,-1.17524047358083,
-8.1375));
#358908=CARTESIAN_POINT('Ctrl Pts',(0.678525403784434,-1.17524047358083,
-8.09583333333333));
#358909=CARTESIAN_POINT('Ctrl Pts',(1.01778810567665,-0.587620236790413,
-8.05416666666667));
#358910=CARTESIAN_POINT('Ctrl Pts',(1.35705080756887,1.59306407295827E-15,
-8.0125));
#358911=CARTESIAN_POINT('Ctrl Pts',(1.01778810567665,0.587620236790415,
-7.97083333333334));
#358912=CARTESIAN_POINT('Ctrl Pts',(0.678525403784435,1.17524047358083,
-7.92916666666667));
#358913=CARTESIAN_POINT('Ctrl Pts',(0.,1.17524047358083,-7.8875));
#358914=CARTESIAN_POINT('Ctrl Pts',(-0.678525403784434,1.17524047358083,
-7.84583333333333));
#358915=CARTESIAN_POINT('Ctrl Pts',(-1.01778810567665,0.587620236790416,
-7.80416666666667));
#358916=CARTESIAN_POINT('Ctrl Pts',(-1.35705080756887,1.8161717387656E-15,
-7.7625));
#358917=CARTESIAN_POINT('Ctrl Pts',(-1.01778810567665,-0.587620236790412,
-7.72083333333334));
#358918=CARTESIAN_POINT('Ctrl Pts',(-0.678525403784435,-1.17524047358083,
-7.67916666666667));
#358919=CARTESIAN_POINT('Ctrl Pts',(-1.43925448419918E-16,-1.17524047358083,
-7.6375));
#358920=CARTESIAN_POINT('Origin',(-1.38777878078146E-16,-5.55111512312578E-15,
-17.91875));
#358921=CARTESIAN_POINT('',(1.42394762919424E-14,-1.17524047358083,-8.7));
#358922=CARTESIAN_POINT('',(1.43379317469826E-14,-1.17524047358083,-8.6375));
#358923=CARTESIAN_POINT('',(-4.21481204576211E-16,-1.17524047358085,-17.91875));
#358924=CARTESIAN_POINT('Ctrl Pts',(-1.43925448419918E-16,-1.17524047358083,
-8.7));
#358925=CARTESIAN_POINT('Ctrl Pts',(0.678525403784434,-1.17524047358083,
-8.65833333333333));
#358926=CARTESIAN_POINT('Ctrl Pts',(1.01778810567665,-0.587620236790413,
-8.61666666666667));
#358927=CARTESIAN_POINT('Ctrl Pts',(1.35705080756887,1.83893039238805E-15,
-8.575));
#358928=CARTESIAN_POINT('Ctrl Pts',(1.01778810567665,0.587620236790415,
-8.53333333333333));
#358929=CARTESIAN_POINT('Ctrl Pts',(0.678525403784435,1.17524047358083,
-8.49166666666667));
#358930=CARTESIAN_POINT('Ctrl Pts',(0.,1.17524047358083,-8.45));
#358931=CARTESIAN_POINT('Ctrl Pts',(-0.678525403784434,1.17524047358083,
-8.40833333333333));
#358932=CARTESIAN_POINT('Ctrl Pts',(-1.01778810567665,0.587620236790416,
-8.36666666666667));
#358933=CARTESIAN_POINT('Ctrl Pts',(-1.35705080756887,2.06203805819539E-15,
-8.325));
#358934=CARTESIAN_POINT('Ctrl Pts',(-1.01778810567665,-0.587620236790412,
-8.28333333333333));
#358935=CARTESIAN_POINT('Ctrl Pts',(-0.678525403784435,-1.17524047358083,
-8.24166666666667));
#358936=CARTESIAN_POINT('Ctrl Pts',(-1.43925448419918E-16,-1.17524047358083,
-8.2));
#358937=CARTESIAN_POINT('Ctrl Pts',(-1.43925448419918E-16,-1.17524047358083,
-8.6375));
#358938=CARTESIAN_POINT('Ctrl Pts',(0.678525403784434,-1.17524047358083,
-8.59583333333333));
#358939=CARTESIAN_POINT('Ctrl Pts',(1.01778810567665,-0.587620236790413,
-8.55416666666667));
#358940=CARTESIAN_POINT('Ctrl Pts',(1.35705080756887,1.81161191245141E-15,
-8.5125));
#358941=CARTESIAN_POINT('Ctrl Pts',(1.01778810567665,0.587620236790415,
-8.47083333333333));
#358942=CARTESIAN_POINT('Ctrl Pts',(0.678525403784435,1.17524047358083,
-8.42916666666667));
#358943=CARTESIAN_POINT('Ctrl Pts',(0.,1.17524047358083,-8.3875));
#358944=CARTESIAN_POINT('Ctrl Pts',(-0.678525403784434,1.17524047358083,
-8.34583333333333));
#358945=CARTESIAN_POINT('Ctrl Pts',(-1.01778810567665,0.587620236790416,
-8.30416666666667));
#358946=CARTESIAN_POINT('Ctrl Pts',(-1.35705080756887,2.03471957825875E-15,
-8.2625));
#358947=CARTESIAN_POINT('Ctrl Pts',(-1.01778810567665,-0.587620236790412,
-8.22083333333333));
#358948=CARTESIAN_POINT('Ctrl Pts',(-0.678525403784435,-1.17524047358083,
-8.17916666666667));
#358949=CARTESIAN_POINT('Ctrl Pts',(-1.43925448419918E-16,-1.17524047358083,
-8.1375));
#358950=CARTESIAN_POINT('Origin',(-1.38777878078146E-16,-5.55111512312578E-15,
-17.91875));
#358951=CARTESIAN_POINT('',(1.34518326516202E-14,-1.17524047358083,-9.2));
#358952=CARTESIAN_POINT('',(1.35502881066604E-14,-1.17524047358083,-9.1375));
#358953=CARTESIAN_POINT('',(-4.21481204576211E-16,-1.17524047358085,-17.91875));
#358954=CARTESIAN_POINT('Ctrl Pts',(-1.43925448419918E-16,-1.17524047358083,
-9.2));
#358955=CARTESIAN_POINT('Ctrl Pts',(0.678525403784434,-1.17524047358083,
-9.15833333333333));
#358956=CARTESIAN_POINT('Ctrl Pts',(1.01778810567665,-0.587620236790412,
-9.11666666666667));
#358957=CARTESIAN_POINT('Ctrl Pts',(1.35705080756887,2.05747823188119E-15,
-9.075));
#358958=CARTESIAN_POINT('Ctrl Pts',(1.01778810567665,0.587620236790415,
-9.03333333333333));
#358959=CARTESIAN_POINT('Ctrl Pts',(0.678525403784435,1.17524047358083,
-8.99166666666667));
#358960=CARTESIAN_POINT('Ctrl Pts',(0.,1.17524047358083,-8.95));
#358961=CARTESIAN_POINT('Ctrl Pts',(-0.678525403784434,1.17524047358083,
-8.90833333333333));
#358962=CARTESIAN_POINT('Ctrl Pts',(-1.01778810567665,0.587620236790416,
-8.86666666666667));
#358963=CARTESIAN_POINT('Ctrl Pts',(-1.35705080756887,2.28058589768853E-15,
-8.825));
#358964=CARTESIAN_POINT('Ctrl Pts',(-1.01778810567665,-0.587620236790412,
-8.78333333333333));
#358965=CARTESIAN_POINT('Ctrl Pts',(-0.678525403784435,-1.17524047358083,
-8.74166666666667));
#358966=CARTESIAN_POINT('Ctrl Pts',(-1.43925448419918E-16,-1.17524047358083,
-8.7));
#358967=CARTESIAN_POINT('Ctrl Pts',(-1.43925448419918E-16,-1.17524047358083,
-9.1375));
#358968=CARTESIAN_POINT('Ctrl Pts',(0.678525403784434,-1.17524047358083,
-9.09583333333333));
#358969=CARTESIAN_POINT('Ctrl Pts',(1.01778810567665,-0.587620236790412,
-9.05416666666667));
#358970=CARTESIAN_POINT('Ctrl Pts',(1.35705080756887,2.03015975194455E-15,
-9.0125));
#358971=CARTESIAN_POINT('Ctrl Pts',(1.01778810567665,0.587620236790416,
-8.97083333333333));
#358972=CARTESIAN_POINT('Ctrl Pts',(0.678525403784435,1.17524047358083,
-8.92916666666667));
#358973=CARTESIAN_POINT('Ctrl Pts',(0.,1.17524047358083,-8.8875));
#358974=CARTESIAN_POINT('Ctrl Pts',(-0.678525403784434,1.17524047358083,
-8.84583333333333));
#358975=CARTESIAN_POINT('Ctrl Pts',(-1.01778810567665,0.587620236790416,
-8.80416666666667));
#358976=CARTESIAN_POINT('Ctrl Pts',(-1.35705080756887,2.25326741775189E-15,
-8.7625));
#358977=CARTESIAN_POINT('Ctrl Pts',(-1.01778810567665,-0.587620236790412,
-8.72083333333333));
#358978=CARTESIAN_POINT('Ctrl Pts',(-0.678525403784435,-1.17524047358083,
-8.67916666666667));
#358979=CARTESIAN_POINT('Ctrl Pts',(-1.43925448419918E-16,-1.17524047358083,
-8.6375));
#358980=CARTESIAN_POINT('Origin',(-1.38777878078146E-16,-5.55111512312578E-15,
-17.91875));
#358981=CARTESIAN_POINT('',(1.2664189011298E-14,-1.17524047358083,-9.7));
#358982=CARTESIAN_POINT('',(1.27626444663382E-14,-1.17524047358083,-9.6375));
#358983=CARTESIAN_POINT('',(-4.21481204576211E-16,-1.17524047358085,-17.91875));
#358984=CARTESIAN_POINT('Ctrl Pts',(-1.43925448419918E-16,-1.17524047358083,
-9.7));
#358985=CARTESIAN_POINT('Ctrl Pts',(0.678525403784434,-1.17524047358083,
-9.65833333333333));
#358986=CARTESIAN_POINT('Ctrl Pts',(1.01778810567665,-0.587620236790412,
-9.61666666666667));
#358987=CARTESIAN_POINT('Ctrl Pts',(1.35705080756887,2.27602607137433E-15,
-9.575));
#358988=CARTESIAN_POINT('Ctrl Pts',(1.01778810567665,0.587620236790416,
-9.53333333333333));
#358989=CARTESIAN_POINT('Ctrl Pts',(0.678525403784435,1.17524047358083,
-9.49166666666667));
#358990=CARTESIAN_POINT('Ctrl Pts',(0.,1.17524047358083,-9.45));
#358991=CARTESIAN_POINT('Ctrl Pts',(-0.678525403784434,1.17524047358083,
-9.40833333333333));
#358992=CARTESIAN_POINT('Ctrl Pts',(-1.01778810567665,0.587620236790417,
-9.36666666666667));
#358993=CARTESIAN_POINT('Ctrl Pts',(-1.35705080756887,2.49913373718167E-15,
-9.325));
#358994=CARTESIAN_POINT('Ctrl Pts',(-1.01778810567665,-0.587620236790411,
-9.28333333333333));
#358995=CARTESIAN_POINT('Ctrl Pts',(-0.678525403784435,-1.17524047358083,
-9.24166666666667));
#358996=CARTESIAN_POINT('Ctrl Pts',(-1.43925448419918E-16,-1.17524047358083,
-9.2));
#358997=CARTESIAN_POINT('Ctrl Pts',(-1.43925448419918E-16,-1.17524047358083,
-9.6375));
#358998=CARTESIAN_POINT('Ctrl Pts',(0.678525403784434,-1.17524047358083,
-9.59583333333333));
#358999=CARTESIAN_POINT('Ctrl Pts',(1.01778810567665,-0.587620236790412,
-9.55416666666667));
#359000=CARTESIAN_POINT('Ctrl Pts',(1.35705080756887,2.24870759143769E-15,
-9.5125));
#359001=CARTESIAN_POINT('Ctrl Pts',(1.01778810567665,0.587620236790416,
-9.47083333333333));
#359002=CARTESIAN_POINT('Ctrl Pts',(0.678525403784435,1.17524047358083,
-9.42916666666667));
#359003=CARTESIAN_POINT('Ctrl Pts',(0.,1.17524047358083,-9.3875));
#359004=CARTESIAN_POINT('Ctrl Pts',(-0.678525403784434,1.17524047358083,
-9.34583333333333));
#359005=CARTESIAN_POINT('Ctrl Pts',(-1.01778810567665,0.587620236790417,
-9.30416666666667));
#359006=CARTESIAN_POINT('Ctrl Pts',(-1.35705080756887,2.47181525724503E-15,
-9.2625));
#359007=CARTESIAN_POINT('Ctrl Pts',(-1.01778810567665,-0.587620236790412,
-9.22083333333333));
#359008=CARTESIAN_POINT('Ctrl Pts',(-0.678525403784435,-1.17524047358083,
-9.17916666666667));
#359009=CARTESIAN_POINT('Ctrl Pts',(-1.43925448419918E-16,-1.17524047358083,
-9.1375));
#359010=CARTESIAN_POINT('Origin',(-1.38777878078146E-16,-5.55111512312578E-15,
-17.91875));
#359011=CARTESIAN_POINT('',(1.18765453709758E-14,-1.17524047358083,-10.2));
#359012=CARTESIAN_POINT('',(1.19750008260161E-14,-1.17524047358083,-10.1375));
#359013=CARTESIAN_POINT('',(-4.21481204576211E-16,-1.17524047358085,-17.91875));
#359014=CARTESIAN_POINT('Ctrl Pts',(-1.43925448419918E-16,-1.17524047358083,
-10.2));
#359015=CARTESIAN_POINT('Ctrl Pts',(0.678525403784434,-1.17524047358083,
-10.1583333333333));
#359016=CARTESIAN_POINT('Ctrl Pts',(1.01778810567665,-0.587620236790412,
-10.1166666666667));
#359017=CARTESIAN_POINT('Ctrl Pts',(1.35705080756887,2.49457391086747E-15,
-10.075));
#359018=CARTESIAN_POINT('Ctrl Pts',(1.01778810567665,0.587620236790416,
-10.0333333333333));
#359019=CARTESIAN_POINT('Ctrl Pts',(0.678525403784435,1.17524047358083,
-9.99166666666667));
#359020=CARTESIAN_POINT('Ctrl Pts',(0.,1.17524047358083,-9.95));
#359021=CARTESIAN_POINT('Ctrl Pts',(-0.678525403784434,1.17524047358083,
-9.90833333333333));
#359022=CARTESIAN_POINT('Ctrl Pts',(-1.01778810567665,0.587620236790417,
-9.86666666666667));
#359023=CARTESIAN_POINT('Ctrl Pts',(-1.35705080756887,2.71768157667481E-15,
-9.825));
#359024=CARTESIAN_POINT('Ctrl Pts',(-1.01778810567665,-0.587620236790411,
-9.78333333333333));
#359025=CARTESIAN_POINT('Ctrl Pts',(-0.678525403784435,-1.17524047358083,
-9.74166666666667));
#359026=CARTESIAN_POINT('Ctrl Pts',(-1.43925448419918E-16,-1.17524047358083,
-9.7));
#359027=CARTESIAN_POINT('Ctrl Pts',(-1.43925448419918E-16,-1.17524047358083,
-10.1375));
#359028=CARTESIAN_POINT('Ctrl Pts',(0.678525403784434,-1.17524047358083,
-10.0958333333333));
#359029=CARTESIAN_POINT('Ctrl Pts',(1.01778810567665,-0.587620236790412,
-10.0541666666667));
#359030=CARTESIAN_POINT('Ctrl Pts',(1.35705080756887,2.46725543093083E-15,
-10.0125));
#359031=CARTESIAN_POINT('Ctrl Pts',(1.01778810567665,0.587620236790416,
-9.97083333333333));
#359032=CARTESIAN_POINT('Ctrl Pts',(0.678525403784435,1.17524047358083,
-9.92916666666667));
#359033=CARTESIAN_POINT('Ctrl Pts',(0.,1.17524047358083,-9.8875));
#359034=CARTESIAN_POINT('Ctrl Pts',(-0.678525403784434,1.17524047358083,
-9.84583333333333));
#359035=CARTESIAN_POINT('Ctrl Pts',(-1.01778810567665,0.587620236790417,
-9.80416666666667));
#359036=CARTESIAN_POINT('Ctrl Pts',(-1.35705080756887,2.69036309673817E-15,
-9.7625));
#359037=CARTESIAN_POINT('Ctrl Pts',(-1.01778810567665,-0.587620236790411,
-9.72083333333333));
#359038=CARTESIAN_POINT('Ctrl Pts',(-0.678525403784435,-1.17524047358083,
-9.67916666666667));
#359039=CARTESIAN_POINT('Ctrl Pts',(-1.43925448419918E-16,-1.17524047358083,
-9.6375));
#359040=CARTESIAN_POINT('Origin',(-1.38777878078146E-16,-5.55111512312578E-15,
-17.91875));
#359041=CARTESIAN_POINT('',(1.10889017306536E-14,-1.17524047358083,-10.7));
#359042=CARTESIAN_POINT('',(1.11873571856939E-14,-1.17524047358083,-10.6375));
#359043=CARTESIAN_POINT('',(-4.21481204576211E-16,-1.17524047358085,-17.91875));
#359044=CARTESIAN_POINT('Ctrl Pts',(-1.43925448419918E-16,-1.17524047358083,
-10.7));
#359045=CARTESIAN_POINT('Ctrl Pts',(0.678525403784434,-1.17524047358083,
-10.6583333333333));
#359046=CARTESIAN_POINT('Ctrl Pts',(1.01778810567665,-0.587620236790412,
-10.6166666666667));
#359047=CARTESIAN_POINT('Ctrl Pts',(1.35705080756887,2.71312175036061E-15,
-10.575));
#359048=CARTESIAN_POINT('Ctrl Pts',(1.01778810567665,0.587620236790416,
-10.5333333333333));
#359049=CARTESIAN_POINT('Ctrl Pts',(0.678525403784435,1.17524047358083,
-10.4916666666667));
#359050=CARTESIAN_POINT('Ctrl Pts',(0.,1.17524047358083,-10.45));
#359051=CARTESIAN_POINT('Ctrl Pts',(-0.678525403784434,1.17524047358083,
-10.4083333333333));
#359052=CARTESIAN_POINT('Ctrl Pts',(-1.01778810567665,0.587620236790417,
-10.3666666666667));
#359053=CARTESIAN_POINT('Ctrl Pts',(-1.35705080756887,2.93622941616795E-15,
-10.325));
#359054=CARTESIAN_POINT('Ctrl Pts',(-1.01778810567665,-0.587620236790411,
-10.2833333333333));
#359055=CARTESIAN_POINT('Ctrl Pts',(-0.678525403784435,-1.17524047358083,
-10.2416666666667));
#359056=CARTESIAN_POINT('Ctrl Pts',(-1.43925448419918E-16,-1.17524047358083,
-10.2));
#359057=CARTESIAN_POINT('Ctrl Pts',(-1.43925448419918E-16,-1.17524047358083,
-10.6375));
#359058=CARTESIAN_POINT('Ctrl Pts',(0.678525403784434,-1.17524047358083,
-10.5958333333333));
#359059=CARTESIAN_POINT('Ctrl Pts',(1.01778810567665,-0.587620236790412,
-10.5541666666667));
#359060=CARTESIAN_POINT('Ctrl Pts',(1.35705080756887,2.68580327042397E-15,
-10.5125));
#359061=CARTESIAN_POINT('Ctrl Pts',(1.01778810567665,0.587620236790416,
-10.4708333333333));
#359062=CARTESIAN_POINT('Ctrl Pts',(0.678525403784435,1.17524047358083,
-10.4291666666667));
#359063=CARTESIAN_POINT('Ctrl Pts',(0.,1.17524047358083,-10.3875));
#359064=CARTESIAN_POINT('Ctrl Pts',(-0.678525403784434,1.17524047358083,
-10.3458333333333));
#359065=CARTESIAN_POINT('Ctrl Pts',(-1.01778810567665,0.587620236790417,
-10.3041666666667));
#359066=CARTESIAN_POINT('Ctrl Pts',(-1.35705080756887,2.90891093623131E-15,
-10.2625));
#359067=CARTESIAN_POINT('Ctrl Pts',(-1.01778810567665,-0.587620236790411,
-10.2208333333333));
#359068=CARTESIAN_POINT('Ctrl Pts',(-0.678525403784435,-1.17524047358083,
-10.1791666666667));
#359069=CARTESIAN_POINT('Ctrl Pts',(-1.43925448419918E-16,-1.17524047358083,
-10.1375));
#359070=CARTESIAN_POINT('Origin',(-1.38777878078146E-16,-5.55111512312578E-15,
-17.91875));
#359071=CARTESIAN_POINT('',(1.03012580903314E-14,-1.17524047358082,-11.2));
#359072=CARTESIAN_POINT('',(1.03997135453717E-14,-1.17524047358083,-11.1375));
#359073=CARTESIAN_POINT('',(-4.21481204576211E-16,-1.17524047358085,-17.91875));
#359074=CARTESIAN_POINT('Ctrl Pts',(-1.43925448419918E-16,-1.17524047358082,
-11.2));
#359075=CARTESIAN_POINT('Ctrl Pts',(0.678525403784434,-1.17524047358083,
-11.1583333333333));
#359076=CARTESIAN_POINT('Ctrl Pts',(1.01778810567665,-0.587620236790411,
-11.1166666666667));
#359077=CARTESIAN_POINT('Ctrl Pts',(1.35705080756887,2.93166958985376E-15,
-11.075));
#359078=CARTESIAN_POINT('Ctrl Pts',(1.01778810567665,0.587620236790416,
-11.0333333333333));
#359079=CARTESIAN_POINT('Ctrl Pts',(0.678525403784435,1.17524047358083,
-10.9916666666667));
#359080=CARTESIAN_POINT('Ctrl Pts',(0.,1.17524047358083,-10.95));
#359081=CARTESIAN_POINT('Ctrl Pts',(-0.678525403784434,1.17524047358083,
-10.9083333333333));
#359082=CARTESIAN_POINT('Ctrl Pts',(-1.01778810567665,0.587620236790417,
-10.8666666666667));
#359083=CARTESIAN_POINT('Ctrl Pts',(-1.35705080756887,3.15477725566109E-15,
-10.825));
#359084=CARTESIAN_POINT('Ctrl Pts',(-1.01778810567665,-0.587620236790411,
-10.7833333333333));
#359085=CARTESIAN_POINT('Ctrl Pts',(-0.678525403784435,-1.17524047358083,
-10.7416666666667));
#359086=CARTESIAN_POINT('Ctrl Pts',(-1.43925448419918E-16,-1.17524047358083,
-10.7));
#359087=CARTESIAN_POINT('Ctrl Pts',(-1.43925448419918E-16,-1.17524047358083,
-11.1375));
#359088=CARTESIAN_POINT('Ctrl Pts',(0.678525403784434,-1.17524047358083,
-11.0958333333333));
#359089=CARTESIAN_POINT('Ctrl Pts',(1.01778810567665,-0.587620236790412,
-11.0541666666667));
#359090=CARTESIAN_POINT('Ctrl Pts',(1.35705080756887,2.90435110991711E-15,
-11.0125));
#359091=CARTESIAN_POINT('Ctrl Pts',(1.01778810567665,0.587620236790416,
-10.9708333333333));
#359092=CARTESIAN_POINT('Ctrl Pts',(0.678525403784435,1.17524047358083,
-10.9291666666667));
#359093=CARTESIAN_POINT('Ctrl Pts',(0.,1.17524047358083,-10.8875));
#359094=CARTESIAN_POINT('Ctrl Pts',(-0.678525403784434,1.17524047358083,
-10.8458333333333));
#359095=CARTESIAN_POINT('Ctrl Pts',(-1.01778810567665,0.587620236790417,
-10.8041666666667));
#359096=CARTESIAN_POINT('Ctrl Pts',(-1.35705080756887,3.12745877572445E-15,
-10.7625));
#359097=CARTESIAN_POINT('Ctrl Pts',(-1.01778810567665,-0.587620236790411,
-10.7208333333333));
#359098=CARTESIAN_POINT('Ctrl Pts',(-0.678525403784435,-1.17524047358083,
-10.6791666666667));
#359099=CARTESIAN_POINT('Ctrl Pts',(-1.43925448419918E-16,-1.17524047358083,
-10.6375));
#359100=CARTESIAN_POINT('Origin',(-1.38777878078146E-16,-5.55111512312578E-15,
-17.91875));
#359101=CARTESIAN_POINT('',(9.5136144500092E-15,-1.17524047358082,-11.7));
#359102=CARTESIAN_POINT('',(9.61206990504947E-15,-1.17524047358083,-11.6375));
#359103=CARTESIAN_POINT('',(-4.21481204576211E-16,-1.17524047358085,-17.91875));
#359104=CARTESIAN_POINT('Ctrl Pts',(-1.43925448419918E-16,-1.17524047358082,
-11.7));
#359105=CARTESIAN_POINT('Ctrl Pts',(0.678525403784434,-1.17524047358083,
-11.6583333333333));
#359106=CARTESIAN_POINT('Ctrl Pts',(1.01778810567665,-0.587620236790411,
-11.6166666666667));
#359107=CARTESIAN_POINT('Ctrl Pts',(1.35705080756887,3.1502174293469E-15,
-11.575));
#359108=CARTESIAN_POINT('Ctrl Pts',(1.01778810567665,0.587620236790417,
-11.5333333333333));
#359109=CARTESIAN_POINT('Ctrl Pts',(0.678525403784435,1.17524047358083,
-11.4916666666667));
#359110=CARTESIAN_POINT('Ctrl Pts',(0.,1.17524047358083,-11.45));
#359111=CARTESIAN_POINT('Ctrl Pts',(-0.678525403784434,1.17524047358083,
-11.4083333333333));
#359112=CARTESIAN_POINT('Ctrl Pts',(-1.01778810567665,0.587620236790417,
-11.3666666666667));
#359113=CARTESIAN_POINT('Ctrl Pts',(-1.35705080756887,3.37332509515423E-15,
-11.325));
#359114=CARTESIAN_POINT('Ctrl Pts',(-1.01778810567665,-0.587620236790411,
-11.2833333333333));
#359115=CARTESIAN_POINT('Ctrl Pts',(-0.678525403784435,-1.17524047358082,
-11.2416666666667));
#359116=CARTESIAN_POINT('Ctrl Pts',(-1.43925448419918E-16,-1.17524047358082,
-11.2));
#359117=CARTESIAN_POINT('Ctrl Pts',(-1.43925448419918E-16,-1.17524047358083,
-11.6375));
#359118=CARTESIAN_POINT('Ctrl Pts',(0.678525403784434,-1.17524047358083,
-11.5958333333333));
#359119=CARTESIAN_POINT('Ctrl Pts',(1.01778810567665,-0.587620236790411,
-11.5541666666667));
#359120=CARTESIAN_POINT('Ctrl Pts',(1.35705080756887,3.12289894941025E-15,
-11.5125));
#359121=CARTESIAN_POINT('Ctrl Pts',(1.01778810567665,0.587620236790417,
-11.4708333333333));
#359122=CARTESIAN_POINT('Ctrl Pts',(0.678525403784435,1.17524047358083,
-11.4291666666667));
#359123=CARTESIAN_POINT('Ctrl Pts',(0.,1.17524047358083,-11.3875));
#359124=CARTESIAN_POINT('Ctrl Pts',(-0.678525403784434,1.17524047358083,
-11.3458333333333));
#359125=CARTESIAN_POINT('Ctrl Pts',(-1.01778810567665,0.587620236790418,
-11.3041666666667));
#359126=CARTESIAN_POINT('Ctrl Pts',(-1.35705080756887,3.34600661521759E-15,
-11.2625));
#359127=CARTESIAN_POINT('Ctrl Pts',(-1.01778810567665,-0.587620236790411,
-11.2208333333333));
#359128=CARTESIAN_POINT('Ctrl Pts',(-0.678525403784435,-1.17524047358083,
-11.1791666666667));
#359129=CARTESIAN_POINT('Ctrl Pts',(-1.43925448419918E-16,-1.17524047358083,
-11.1375));
#359130=CARTESIAN_POINT('Origin',(-1.38777878078146E-16,-5.55111512312578E-15,
-17.91875));
#359131=CARTESIAN_POINT('',(8.72597080968701E-15,-1.17524047358082,-12.2));
#359132=CARTESIAN_POINT('',(8.82442626472729E-15,-1.17524047358082,-12.1375));
#359133=CARTESIAN_POINT('',(-4.21481204576211E-16,-1.17524047358085,-17.91875));
#359134=CARTESIAN_POINT('Ctrl Pts',(-1.43925448419918E-16,-1.17524047358082,
-12.2));
#359135=CARTESIAN_POINT('Ctrl Pts',(0.678525403784434,-1.17524047358082,
-12.1583333333333));
#359136=CARTESIAN_POINT('Ctrl Pts',(1.01778810567665,-0.587620236790411,
-12.1166666666667));
#359137=CARTESIAN_POINT('Ctrl Pts',(1.35705080756887,3.36876526884004E-15,
-12.075));
#359138=CARTESIAN_POINT('Ctrl Pts',(1.01778810567665,0.587620236790417,
-12.0333333333333));
#359139=CARTESIAN_POINT('Ctrl Pts',(0.678525403784435,1.17524047358083,
-11.9916666666667));
#359140=CARTESIAN_POINT('Ctrl Pts',(0.,1.17524047358083,-11.95));
#359141=CARTESIAN_POINT('Ctrl Pts',(-0.678525403784434,1.17524047358083,
-11.9083333333333));
#359142=CARTESIAN_POINT('Ctrl Pts',(-1.01778810567665,0.587620236790418,
-11.8666666666667));
#359143=CARTESIAN_POINT('Ctrl Pts',(-1.35705080756887,3.59187293464738E-15,
-11.825));
#359144=CARTESIAN_POINT('Ctrl Pts',(-1.01778810567665,-0.58762023679041,
-11.7833333333333));
#359145=CARTESIAN_POINT('Ctrl Pts',(-0.678525403784435,-1.17524047358082,
-11.7416666666667));
#359146=CARTESIAN_POINT('Ctrl Pts',(-1.43925448419918E-16,-1.17524047358082,
-11.7));
#359147=CARTESIAN_POINT('Ctrl Pts',(-1.43925448419918E-16,-1.17524047358082,
-12.1375));
#359148=CARTESIAN_POINT('Ctrl Pts',(0.678525403784434,-1.17524047358083,
-12.0958333333333));
#359149=CARTESIAN_POINT('Ctrl Pts',(1.01778810567665,-0.587620236790411,
-12.0541666666667));
#359150=CARTESIAN_POINT('Ctrl Pts',(1.35705080756887,3.34144678890339E-15,
-12.0125));
#359151=CARTESIAN_POINT('Ctrl Pts',(1.01778810567665,0.587620236790417,
-11.9708333333333));
#359152=CARTESIAN_POINT('Ctrl Pts',(0.678525403784435,1.17524047358083,
-11.9291666666667));
#359153=CARTESIAN_POINT('Ctrl Pts',(0.,1.17524047358083,-11.8875));
#359154=CARTESIAN_POINT('Ctrl Pts',(-0.678525403784434,1.17524047358083,
-11.8458333333333));
#359155=CARTESIAN_POINT('Ctrl Pts',(-1.01778810567665,0.587620236790418,
-11.8041666666667));
#359156=CARTESIAN_POINT('Ctrl Pts',(-1.35705080756887,3.56455445471073E-15,
-11.7625));
#359157=CARTESIAN_POINT('Ctrl Pts',(-1.01778810567665,-0.587620236790411,
-11.7208333333333));
#359158=CARTESIAN_POINT('Ctrl Pts',(-0.678525403784435,-1.17524047358083,
-11.6791666666667));
#359159=CARTESIAN_POINT('Ctrl Pts',(-1.43925448419918E-16,-1.17524047358083,
-11.6375));
#359160=CARTESIAN_POINT('Origin',(-1.38777878078146E-16,-5.55111512312578E-15,
-17.91875));
#359161=CARTESIAN_POINT('',(7.93832716936482E-15,-1.17524047358082,-12.7));
#359162=CARTESIAN_POINT('',(8.03678262440509E-15,-1.17524047358082,-12.6375));
#359163=CARTESIAN_POINT('',(-4.21481204576211E-16,-1.17524047358085,-17.91875));
#359164=CARTESIAN_POINT('Ctrl Pts',(-1.43925448419918E-16,-1.17524047358082,
-12.7));
#359165=CARTESIAN_POINT('Ctrl Pts',(0.678525403784434,-1.17524047358082,
-12.6583333333333));
#359166=CARTESIAN_POINT('Ctrl Pts',(1.01778810567665,-0.587620236790411,
-12.6166666666667));
#359167=CARTESIAN_POINT('Ctrl Pts',(1.35705080756887,3.58731310833318E-15,
-12.575));
#359168=CARTESIAN_POINT('Ctrl Pts',(1.01778810567665,0.587620236790417,
-12.5333333333333));
#359169=CARTESIAN_POINT('Ctrl Pts',(0.678525403784435,1.17524047358083,
-12.4916666666667));
#359170=CARTESIAN_POINT('Ctrl Pts',(0.,1.17524047358083,-12.45));
#359171=CARTESIAN_POINT('Ctrl Pts',(-0.678525403784434,1.17524047358083,
-12.4083333333333));
#359172=CARTESIAN_POINT('Ctrl Pts',(-1.01778810567665,0.587620236790418,
-12.3666666666667));
#359173=CARTESIAN_POINT('Ctrl Pts',(-1.35705080756887,3.81042077414052E-15,
-12.325));
#359174=CARTESIAN_POINT('Ctrl Pts',(-1.01778810567665,-0.58762023679041,
-12.2833333333333));
#359175=CARTESIAN_POINT('Ctrl Pts',(-0.678525403784435,-1.17524047358082,
-12.2416666666667));
#359176=CARTESIAN_POINT('Ctrl Pts',(-1.43925448419918E-16,-1.17524047358082,
-12.2));
#359177=CARTESIAN_POINT('Ctrl Pts',(-1.43925448419918E-16,-1.17524047358082,
-12.6375));
#359178=CARTESIAN_POINT('Ctrl Pts',(0.678525403784434,-1.17524047358083,
-12.5958333333333));
#359179=CARTESIAN_POINT('Ctrl Pts',(1.01778810567665,-0.587620236790411,
-12.5541666666667));
#359180=CARTESIAN_POINT('Ctrl Pts',(1.35705080756887,3.55999462839654E-15,
-12.5125));
#359181=CARTESIAN_POINT('Ctrl Pts',(1.01778810567665,0.587620236790417,
-12.4708333333333));
#359182=CARTESIAN_POINT('Ctrl Pts',(0.678525403784435,1.17524047358083,
-12.4291666666667));
#359183=CARTESIAN_POINT('Ctrl Pts',(0.,1.17524047358083,-12.3875));
#359184=CARTESIAN_POINT('Ctrl Pts',(-0.678525403784434,1.17524047358083,
-12.3458333333333));
#359185=CARTESIAN_POINT('Ctrl Pts',(-1.01778810567665,0.587620236790418,
-12.3041666666667));
#359186=CARTESIAN_POINT('Ctrl Pts',(-1.35705080756887,3.78310229420388E-15,
-12.2625));
#359187=CARTESIAN_POINT('Ctrl Pts',(-1.01778810567665,-0.58762023679041,
-12.2208333333333));
#359188=CARTESIAN_POINT('Ctrl Pts',(-0.678525403784435,-1.17524047358082,
-12.1791666666667));
#359189=CARTESIAN_POINT('Ctrl Pts',(-1.43925448419918E-16,-1.17524047358082,
-12.1375));
#359190=CARTESIAN_POINT('Origin',(-1.38777878078146E-16,-5.55111512312578E-15,
-17.91875));
#359191=CARTESIAN_POINT('',(7.15068352904263E-15,-1.17524047358082,-13.2));
#359192=CARTESIAN_POINT('',(7.2491389840829E-15,-1.17524047358082,-13.1375));
#359193=CARTESIAN_POINT('',(-4.21481204576211E-16,-1.17524047358085,-17.91875));
#359194=CARTESIAN_POINT('Ctrl Pts',(-1.43925448419918E-16,-1.17524047358082,
-13.2));
#359195=CARTESIAN_POINT('Ctrl Pts',(0.678525403784434,-1.17524047358082,
-13.1583333333333));
#359196=CARTESIAN_POINT('Ctrl Pts',(1.01778810567665,-0.587620236790411,
-13.1166666666667));
#359197=CARTESIAN_POINT('Ctrl Pts',(1.35705080756887,3.80586094782632E-15,
-13.075));
#359198=CARTESIAN_POINT('Ctrl Pts',(1.01778810567665,0.587620236790417,
-13.0333333333333));
#359199=CARTESIAN_POINT('Ctrl Pts',(0.678525403784435,1.17524047358083,
-12.9916666666667));
#359200=CARTESIAN_POINT('Ctrl Pts',(0.,1.17524047358083,-12.95));
#359201=CARTESIAN_POINT('Ctrl Pts',(-0.678525403784434,1.17524047358083,
-12.9083333333333));
#359202=CARTESIAN_POINT('Ctrl Pts',(-1.01778810567665,0.587620236790418,
-12.8666666666667));
#359203=CARTESIAN_POINT('Ctrl Pts',(-1.35705080756887,4.02896861363366E-15,
-12.825));
#359204=CARTESIAN_POINT('Ctrl Pts',(-1.01778810567665,-0.58762023679041,
-12.7833333333333));
#359205=CARTESIAN_POINT('Ctrl Pts',(-0.678525403784435,-1.17524047358082,
-12.7416666666667));
#359206=CARTESIAN_POINT('Ctrl Pts',(-1.43925448419918E-16,-1.17524047358082,
-12.7));
#359207=CARTESIAN_POINT('Ctrl Pts',(-1.43925448419918E-16,-1.17524047358082,
-13.1375));
#359208=CARTESIAN_POINT('Ctrl Pts',(0.678525403784434,-1.17524047358082,
-13.0958333333333));
#359209=CARTESIAN_POINT('Ctrl Pts',(1.01778810567665,-0.587620236790411,
-13.0541666666667));
#359210=CARTESIAN_POINT('Ctrl Pts',(1.35705080756887,3.77854246788968E-15,
-13.0125));
#359211=CARTESIAN_POINT('Ctrl Pts',(1.01778810567665,0.587620236790417,
-12.9708333333333));
#359212=CARTESIAN_POINT('Ctrl Pts',(0.678525403784435,1.17524047358083,
-12.9291666666667));
#359213=CARTESIAN_POINT('Ctrl Pts',(0.,1.17524047358083,-12.8875));
#359214=CARTESIAN_POINT('Ctrl Pts',(-0.678525403784434,1.17524047358083,
-12.8458333333333));
#359215=CARTESIAN_POINT('Ctrl Pts',(-1.01778810567665,0.587620236790418,
-12.8041666666667));
#359216=CARTESIAN_POINT('Ctrl Pts',(-1.35705080756887,4.00165013369702E-15,
-12.7625));
#359217=CARTESIAN_POINT('Ctrl Pts',(-1.01778810567665,-0.58762023679041,
-12.7208333333333));
#359218=CARTESIAN_POINT('Ctrl Pts',(-0.678525403784435,-1.17524047358082,
-12.6791666666667));
#359219=CARTESIAN_POINT('Ctrl Pts',(-1.43925448419918E-16,-1.17524047358082,
-12.6375));
#359220=CARTESIAN_POINT('Origin',(-1.38777878078146E-16,-5.55111512312578E-15,
-17.91875));
#359221=CARTESIAN_POINT('',(6.36303988872043E-15,-1.17524047358082,-13.7));
#359222=CARTESIAN_POINT('',(6.46149534376071E-15,-1.17524047358082,-13.6375));
#359223=CARTESIAN_POINT('',(-4.21481204576211E-16,-1.17524047358085,-17.91875));
#359224=CARTESIAN_POINT('Ctrl Pts',(-1.43925448419918E-16,-1.17524047358082,
-13.7));
#359225=CARTESIAN_POINT('Ctrl Pts',(0.678525403784434,-1.17524047358082,
-13.6583333333333));
#359226=CARTESIAN_POINT('Ctrl Pts',(1.01778810567665,-0.58762023679041,
-13.6166666666667));
#359227=CARTESIAN_POINT('Ctrl Pts',(1.35705080756887,4.02440878731946E-15,
-13.575));
#359228=CARTESIAN_POINT('Ctrl Pts',(1.01778810567665,0.587620236790417,
-13.5333333333333));
#359229=CARTESIAN_POINT('Ctrl Pts',(0.678525403784435,1.17524047358083,
-13.4916666666667));
#359230=CARTESIAN_POINT('Ctrl Pts',(0.,1.17524047358083,-13.45));
#359231=CARTESIAN_POINT('Ctrl Pts',(-0.678525403784434,1.17524047358083,
-13.4083333333333));
#359232=CARTESIAN_POINT('Ctrl Pts',(-1.01778810567665,0.587620236790418,
-13.3666666666667));
#359233=CARTESIAN_POINT('Ctrl Pts',(-1.35705080756887,4.2475164531268E-15,
-13.325));
#359234=CARTESIAN_POINT('Ctrl Pts',(-1.01778810567665,-0.58762023679041,
-13.2833333333333));
#359235=CARTESIAN_POINT('Ctrl Pts',(-0.678525403784435,-1.17524047358082,
-13.2416666666667));
#359236=CARTESIAN_POINT('Ctrl Pts',(-1.43925448419918E-16,-1.17524047358082,
-13.2));
#359237=CARTESIAN_POINT('Ctrl Pts',(-1.43925448419918E-16,-1.17524047358082,
-13.6375));
#359238=CARTESIAN_POINT('Ctrl Pts',(0.678525403784434,-1.17524047358082,
-13.5958333333333));
#359239=CARTESIAN_POINT('Ctrl Pts',(1.01778810567665,-0.58762023679041,
-13.5541666666667));
#359240=CARTESIAN_POINT('Ctrl Pts',(1.35705080756887,3.99709030738282E-15,
-13.5125));
#359241=CARTESIAN_POINT('Ctrl Pts',(1.01778810567665,0.587620236790418,
-13.4708333333333));
#359242=CARTESIAN_POINT('Ctrl Pts',(0.678525403784435,1.17524047358083,
-13.4291666666667));
#359243=CARTESIAN_POINT('Ctrl Pts',(0.,1.17524047358083,-13.3875));
#359244=CARTESIAN_POINT('Ctrl Pts',(-0.678525403784434,1.17524047358083,
-13.3458333333333));
#359245=CARTESIAN_POINT('Ctrl Pts',(-1.01778810567665,0.587620236790419,
-13.3041666666667));
#359246=CARTESIAN_POINT('Ctrl Pts',(-1.35705080756887,4.22019797319016E-15,
-13.2625));
#359247=CARTESIAN_POINT('Ctrl Pts',(-1.01778810567665,-0.58762023679041,
-13.2208333333333));
#359248=CARTESIAN_POINT('Ctrl Pts',(-0.678525403784435,-1.17524047358082,
-13.1791666666667));
#359249=CARTESIAN_POINT('Ctrl Pts',(-1.43925448419918E-16,-1.17524047358082,
-13.1375));
#359250=CARTESIAN_POINT('Origin',(-1.38777878078146E-16,-5.55111512312578E-15,
-17.91875));
#359251=CARTESIAN_POINT('',(5.57539624839824E-15,-1.17524047358082,-14.2));
#359252=CARTESIAN_POINT('',(5.67385170343851E-15,-1.17524047358082,-14.1375));
#359253=CARTESIAN_POINT('',(-4.21481204576211E-16,-1.17524047358085,-17.91875));
#359254=CARTESIAN_POINT('Ctrl Pts',(-1.43925448419918E-16,-1.17524047358082,
-14.2));
#359255=CARTESIAN_POINT('Ctrl Pts',(0.678525403784434,-1.17524047358082,
-14.1583333333333));
#359256=CARTESIAN_POINT('Ctrl Pts',(1.01778810567665,-0.58762023679041,
-14.1166666666667));
#359257=CARTESIAN_POINT('Ctrl Pts',(1.35705080756887,4.2429566268126E-15,
-14.075));
#359258=CARTESIAN_POINT('Ctrl Pts',(1.01778810567665,0.587620236790418,
-14.0333333333333));
#359259=CARTESIAN_POINT('Ctrl Pts',(0.678525403784435,1.17524047358083,
-13.9916666666667));
#359260=CARTESIAN_POINT('Ctrl Pts',(0.,1.17524047358083,-13.95));
#359261=CARTESIAN_POINT('Ctrl Pts',(-0.678525403784434,1.17524047358083,
-13.9083333333333));
#359262=CARTESIAN_POINT('Ctrl Pts',(-1.01778810567665,0.587620236790419,
-13.8666666666667));
#359263=CARTESIAN_POINT('Ctrl Pts',(-1.35705080756887,4.46606429261994E-15,
-13.825));
#359264=CARTESIAN_POINT('Ctrl Pts',(-1.01778810567665,-0.58762023679041,
-13.7833333333333));
#359265=CARTESIAN_POINT('Ctrl Pts',(-0.678525403784435,-1.17524047358082,
-13.7416666666667));
#359266=CARTESIAN_POINT('Ctrl Pts',(-1.43925448419918E-16,-1.17524047358082,
-13.7));
#359267=CARTESIAN_POINT('Ctrl Pts',(-1.43925448419918E-16,-1.17524047358082,
-14.1375));
#359268=CARTESIAN_POINT('Ctrl Pts',(0.678525403784434,-1.17524047358082,
-14.0958333333333));
#359269=CARTESIAN_POINT('Ctrl Pts',(1.01778810567665,-0.58762023679041,
-14.0541666666667));
#359270=CARTESIAN_POINT('Ctrl Pts',(1.35705080756887,4.21563814687596E-15,
-14.0125));
#359271=CARTESIAN_POINT('Ctrl Pts',(1.01778810567665,0.587620236790418,
-13.9708333333333));
#359272=CARTESIAN_POINT('Ctrl Pts',(0.678525403784435,1.17524047358083,
-13.9291666666667));
#359273=CARTESIAN_POINT('Ctrl Pts',(0.,1.17524047358083,-13.8875));
#359274=CARTESIAN_POINT('Ctrl Pts',(-0.678525403784434,1.17524047358083,
-13.8458333333333));
#359275=CARTESIAN_POINT('Ctrl Pts',(-1.01778810567665,0.587620236790419,
-13.8041666666667));
#359276=CARTESIAN_POINT('Ctrl Pts',(-1.35705080756887,4.4387458126833E-15,
-13.7625));
#359277=CARTESIAN_POINT('Ctrl Pts',(-1.01778810567665,-0.58762023679041,
-13.7208333333333));
#359278=CARTESIAN_POINT('Ctrl Pts',(-0.678525403784435,-1.17524047358082,
-13.6791666666667));
#359279=CARTESIAN_POINT('Ctrl Pts',(-1.43925448419918E-16,-1.17524047358082,
-13.6375));
#359280=CARTESIAN_POINT('Origin',(-1.38777878078146E-16,-5.55111512312578E-15,
-17.91875));
#359281=CARTESIAN_POINT('',(4.78775260807605E-15,-1.17524047358082,-14.7));
#359282=CARTESIAN_POINT('',(4.88620806311632E-15,-1.17524047358082,-14.6375));
#359283=CARTESIAN_POINT('',(-4.21481204576211E-16,-1.17524047358085,-17.91875));
#359284=CARTESIAN_POINT('Ctrl Pts',(-1.43925448419918E-16,-1.17524047358082,
-14.7));
#359285=CARTESIAN_POINT('Ctrl Pts',(0.678525403784434,-1.17524047358082,
-14.6583333333333));
#359286=CARTESIAN_POINT('Ctrl Pts',(1.01778810567665,-0.58762023679041,
-14.6166666666667));
#359287=CARTESIAN_POINT('Ctrl Pts',(1.35705080756887,4.46150446630574E-15,
-14.575));
#359288=CARTESIAN_POINT('Ctrl Pts',(1.01778810567665,0.587620236790418,
-14.5333333333333));
#359289=CARTESIAN_POINT('Ctrl Pts',(0.678525403784435,1.17524047358083,
-14.4916666666667));
#359290=CARTESIAN_POINT('Ctrl Pts',(0.,1.17524047358083,-14.45));
#359291=CARTESIAN_POINT('Ctrl Pts',(-0.678525403784434,1.17524047358083,
-14.4083333333333));
#359292=CARTESIAN_POINT('Ctrl Pts',(-1.01778810567665,0.587620236790419,
-14.3666666666667));
#359293=CARTESIAN_POINT('Ctrl Pts',(-1.35705080756887,4.68461213211308E-15,
-14.325));
#359294=CARTESIAN_POINT('Ctrl Pts',(-1.01778810567665,-0.587620236790409,
-14.2833333333333));
#359295=CARTESIAN_POINT('Ctrl Pts',(-0.678525403784435,-1.17524047358082,
-14.2416666666667));
#359296=CARTESIAN_POINT('Ctrl Pts',(-1.43925448419918E-16,-1.17524047358082,
-14.2));
#359297=CARTESIAN_POINT('Ctrl Pts',(-1.43925448419918E-16,-1.17524047358082,
-14.6375));
#359298=CARTESIAN_POINT('Ctrl Pts',(0.678525403784434,-1.17524047358082,
-14.5958333333333));
#359299=CARTESIAN_POINT('Ctrl Pts',(1.01778810567665,-0.58762023679041,
-14.5541666666667));
#359300=CARTESIAN_POINT('Ctrl Pts',(1.35705080756887,4.4341859863691E-15,
-14.5125));
#359301=CARTESIAN_POINT('Ctrl Pts',(1.01778810567665,0.587620236790418,
-14.4708333333333));
#359302=CARTESIAN_POINT('Ctrl Pts',(0.678525403784435,1.17524047358083,
-14.4291666666667));
#359303=CARTESIAN_POINT('Ctrl Pts',(0.,1.17524047358083,-14.3875));
#359304=CARTESIAN_POINT('Ctrl Pts',(-0.678525403784434,1.17524047358083,
-14.3458333333333));
#359305=CARTESIAN_POINT('Ctrl Pts',(-1.01778810567665,0.587620236790419,
-14.3041666666667));
#359306=CARTESIAN_POINT('Ctrl Pts',(-1.35705080756887,4.65729365217644E-15,
-14.2625));
#359307=CARTESIAN_POINT('Ctrl Pts',(-1.01778810567665,-0.587620236790409,
-14.2208333333333));
#359308=CARTESIAN_POINT('Ctrl Pts',(-0.678525403784435,-1.17524047358082,
-14.1791666666667));
#359309=CARTESIAN_POINT('Ctrl Pts',(-1.43925448419918E-16,-1.17524047358082,
-14.1375));
#359310=CARTESIAN_POINT('Origin',(-1.38777878078146E-16,-5.55111512312578E-15,
-17.91875));
#359311=CARTESIAN_POINT('',(4.00010896775386E-15,-1.17524047358082,-15.2));
#359312=CARTESIAN_POINT('',(4.09856442279413E-15,-1.17524047358082,-15.1375));
#359313=CARTESIAN_POINT('',(-4.21481204576211E-16,-1.17524047358085,-17.91875));
#359314=CARTESIAN_POINT('Ctrl Pts',(-1.43925448419918E-16,-1.17524047358082,
-15.2));
#359315=CARTESIAN_POINT('Ctrl Pts',(0.678525403784434,-1.17524047358082,
-15.1583333333333));
#359316=CARTESIAN_POINT('Ctrl Pts',(1.01778810567665,-0.58762023679041,
-15.1166666666667));
#359317=CARTESIAN_POINT('Ctrl Pts',(1.35705080756887,4.68005230579889E-15,
-15.075));
#359318=CARTESIAN_POINT('Ctrl Pts',(1.01778810567665,0.587620236790418,
-15.0333333333333));
#359319=CARTESIAN_POINT('Ctrl Pts',(0.678525403784435,1.17524047358083,
-14.9916666666667));
#359320=CARTESIAN_POINT('Ctrl Pts',(0.,1.17524047358083,-14.95));
#359321=CARTESIAN_POINT('Ctrl Pts',(-0.678525403784434,1.17524047358083,
-14.9083333333333));
#359322=CARTESIAN_POINT('Ctrl Pts',(-1.01778810567665,0.587620236790419,
-14.8666666666667));
#359323=CARTESIAN_POINT('Ctrl Pts',(-1.35705080756887,4.90315997160622E-15,
-14.825));
#359324=CARTESIAN_POINT('Ctrl Pts',(-1.01778810567665,-0.587620236790409,
-14.7833333333333));
#359325=CARTESIAN_POINT('Ctrl Pts',(-0.678525403784435,-1.17524047358082,
-14.7416666666667));
#359326=CARTESIAN_POINT('Ctrl Pts',(-1.43925448419918E-16,-1.17524047358082,
-14.7));
#359327=CARTESIAN_POINT('Ctrl Pts',(-1.43925448419918E-16,-1.17524047358082,
-15.1375));
#359328=CARTESIAN_POINT('Ctrl Pts',(0.678525403784434,-1.17524047358082,
-15.0958333333333));
#359329=CARTESIAN_POINT('Ctrl Pts',(1.01778810567665,-0.58762023679041,
-15.0541666666667));
#359330=CARTESIAN_POINT('Ctrl Pts',(1.35705080756887,4.65273382586224E-15,
-15.0125));
#359331=CARTESIAN_POINT('Ctrl Pts',(1.01778810567665,0.587620236790418,
-14.9708333333333));
#359332=CARTESIAN_POINT('Ctrl Pts',(0.678525403784435,1.17524047358083,
-14.9291666666667));
#359333=CARTESIAN_POINT('Ctrl Pts',(0.,1.17524047358083,-14.8875));
#359334=CARTESIAN_POINT('Ctrl Pts',(-0.678525403784434,1.17524047358083,
-14.8458333333333));
#359335=CARTESIAN_POINT('Ctrl Pts',(-1.01778810567665,0.587620236790419,
-14.8041666666667));
#359336=CARTESIAN_POINT('Ctrl Pts',(-1.35705080756887,4.87584149166958E-15,
-14.7625));
#359337=CARTESIAN_POINT('Ctrl Pts',(-1.01778810567665,-0.587620236790409,
-14.7208333333333));
#359338=CARTESIAN_POINT('Ctrl Pts',(-0.678525403784435,-1.17524047358082,
-14.6791666666667));
#359339=CARTESIAN_POINT('Ctrl Pts',(-1.43925448419918E-16,-1.17524047358082,
-14.6375));
#359340=CARTESIAN_POINT('Origin',(-1.38777878078146E-16,-5.55111512312578E-15,
-17.91875));
#359341=CARTESIAN_POINT('',(3.21246532743166E-15,-1.17524047358082,-15.7));
#359342=CARTESIAN_POINT('',(3.31092078247193E-15,-1.17524047358082,-15.6375));
#359343=CARTESIAN_POINT('',(-4.21481204576211E-16,-1.17524047358085,-17.91875));
#359344=CARTESIAN_POINT('Ctrl Pts',(-1.43925448419918E-16,-1.17524047358082,
-15.7));
#359345=CARTESIAN_POINT('Ctrl Pts',(0.678525403784434,-1.17524047358082,
-15.6583333333333));
#359346=CARTESIAN_POINT('Ctrl Pts',(1.01778810567665,-0.587620236790409,
-15.6166666666667));
#359347=CARTESIAN_POINT('Ctrl Pts',(1.35705080756887,4.89860014529203E-15,
-15.575));
#359348=CARTESIAN_POINT('Ctrl Pts',(1.01778810567665,0.587620236790418,
-15.5333333333333));
#359349=CARTESIAN_POINT('Ctrl Pts',(0.678525403784435,1.17524047358083,
-15.4916666666667));
#359350=CARTESIAN_POINT('Ctrl Pts',(0.,1.17524047358083,-15.45));
#359351=CARTESIAN_POINT('Ctrl Pts',(-0.678525403784434,1.17524047358083,
-15.4083333333333));
#359352=CARTESIAN_POINT('Ctrl Pts',(-1.01778810567665,0.587620236790419,
-15.3666666666667));
#359353=CARTESIAN_POINT('Ctrl Pts',(-1.35705080756887,5.12170781109936E-15,
-15.325));
#359354=CARTESIAN_POINT('Ctrl Pts',(-1.01778810567665,-0.587620236790409,
-15.2833333333333));
#359355=CARTESIAN_POINT('Ctrl Pts',(-0.678525403784435,-1.17524047358082,
-15.2416666666667));
#359356=CARTESIAN_POINT('Ctrl Pts',(-1.43925448419918E-16,-1.17524047358082,
-15.2));
#359357=CARTESIAN_POINT('Ctrl Pts',(-1.43925448419918E-16,-1.17524047358082,
-15.6375));
#359358=CARTESIAN_POINT('Ctrl Pts',(0.678525403784434,-1.17524047358082,
-15.5958333333333));
#359359=CARTESIAN_POINT('Ctrl Pts',(1.01778810567665,-0.58762023679041,
-15.5541666666667));
#359360=CARTESIAN_POINT('Ctrl Pts',(1.35705080756887,4.87128166535538E-15,
-15.5125));
#359361=CARTESIAN_POINT('Ctrl Pts',(1.01778810567665,0.587620236790418,
-15.4708333333333));
#359362=CARTESIAN_POINT('Ctrl Pts',(0.678525403784435,1.17524047358083,
-15.4291666666667));
#359363=CARTESIAN_POINT('Ctrl Pts',(0.,1.17524047358083,-15.3875));
#359364=CARTESIAN_POINT('Ctrl Pts',(-0.678525403784434,1.17524047358083,
-15.3458333333333));
#359365=CARTESIAN_POINT('Ctrl Pts',(-1.01778810567665,0.587620236790419,
-15.3041666666667));
#359366=CARTESIAN_POINT('Ctrl Pts',(-1.35705080756887,5.09438933116272E-15,
-15.2625));
#359367=CARTESIAN_POINT('Ctrl Pts',(-1.01778810567665,-0.587620236790409,
-15.2208333333333));
#359368=CARTESIAN_POINT('Ctrl Pts',(-0.678525403784435,-1.17524047358082,
-15.1791666666667));
#359369=CARTESIAN_POINT('Ctrl Pts',(-1.43925448419918E-16,-1.17524047358082,
-15.1375));
#359370=CARTESIAN_POINT('Origin',(-1.38777878078146E-16,-5.55111512312578E-15,
-17.91875));
#359371=CARTESIAN_POINT('',(2.42482168710947E-15,-1.17524047358082,-16.2));
#359372=CARTESIAN_POINT('',(2.52327714214975E-15,-1.17524047358082,-16.1375));
#359373=CARTESIAN_POINT('',(-4.21481204576211E-16,-1.17524047358085,-17.91875));
#359374=CARTESIAN_POINT('Ctrl Pts',(-1.43925448419918E-16,-1.17524047358082,
-16.2));
#359375=CARTESIAN_POINT('Ctrl Pts',(0.678525403784434,-1.17524047358082,
-16.1583333333333));
#359376=CARTESIAN_POINT('Ctrl Pts',(1.01778810567665,-0.587620236790409,
-16.1166666666667));
#359377=CARTESIAN_POINT('Ctrl Pts',(1.35705080756887,5.11714798478517E-15,
-16.075));
#359378=CARTESIAN_POINT('Ctrl Pts',(1.01778810567665,0.587620236790419,
-16.0333333333333));
#359379=CARTESIAN_POINT('Ctrl Pts',(0.678525403784435,1.17524047358083,
-15.9916666666667));
#359380=CARTESIAN_POINT('Ctrl Pts',(0.,1.17524047358083,-15.95));
#359381=CARTESIAN_POINT('Ctrl Pts',(-0.678525403784434,1.17524047358083,
-15.9083333333333));
#359382=CARTESIAN_POINT('Ctrl Pts',(-1.01778810567665,0.58762023679042,
-15.8666666666667));
#359383=CARTESIAN_POINT('Ctrl Pts',(-1.35705080756887,5.34025565059251E-15,
-15.825));
#359384=CARTESIAN_POINT('Ctrl Pts',(-1.01778810567665,-0.587620236790409,
-15.7833333333333));
#359385=CARTESIAN_POINT('Ctrl Pts',(-0.678525403784435,-1.17524047358082,
-15.7416666666667));
#359386=CARTESIAN_POINT('Ctrl Pts',(-1.43925448419918E-16,-1.17524047358082,
-15.7));
#359387=CARTESIAN_POINT('Ctrl Pts',(-1.43925448419918E-16,-1.17524047358082,
-16.1375));
#359388=CARTESIAN_POINT('Ctrl Pts',(0.678525403784434,-1.17524047358082,
-16.0958333333333));
#359389=CARTESIAN_POINT('Ctrl Pts',(1.01778810567665,-0.587620236790409,
-16.0541666666667));
#359390=CARTESIAN_POINT('Ctrl Pts',(1.35705080756887,5.08982950484852E-15,
-16.0125));
#359391=CARTESIAN_POINT('Ctrl Pts',(1.01778810567665,0.587620236790419,
-15.9708333333333));
#359392=CARTESIAN_POINT('Ctrl Pts',(0.678525403784435,1.17524047358083,
-15.9291666666667));
#359393=CARTESIAN_POINT('Ctrl Pts',(0.,1.17524047358083,-15.8875));
#359394=CARTESIAN_POINT('Ctrl Pts',(-0.678525403784434,1.17524047358083,
-15.8458333333333));
#359395=CARTESIAN_POINT('Ctrl Pts',(-1.01778810567665,0.58762023679042,
-15.8041666666667));
#359396=CARTESIAN_POINT('Ctrl Pts',(-1.35705080756887,5.31293717065586E-15,
-15.7625));
#359397=CARTESIAN_POINT('Ctrl Pts',(-1.01778810567665,-0.587620236790409,
-15.7208333333333));
#359398=CARTESIAN_POINT('Ctrl Pts',(-0.678525403784435,-1.17524047358082,
-15.6791666666667));
#359399=CARTESIAN_POINT('Ctrl Pts',(-1.43925448419918E-16,-1.17524047358082,
-15.6375));
#359400=CARTESIAN_POINT('Origin',(-1.38777878078146E-16,-5.55111512312578E-15,
-17.91875));
#359401=CARTESIAN_POINT('',(1.63717804678728E-15,-1.17524047358082,-16.7));
#359402=CARTESIAN_POINT('',(1.73563350182756E-15,-1.17524047358082,-16.6375));
#359403=CARTESIAN_POINT('',(-4.21481204576211E-16,-1.17524047358085,-17.91875));
#359404=CARTESIAN_POINT('Ctrl Pts',(-1.43925448419918E-16,-1.17524047358082,
-16.7));
#359405=CARTESIAN_POINT('Ctrl Pts',(0.678525403784434,-1.17524047358082,
-16.6583333333333));
#359406=CARTESIAN_POINT('Ctrl Pts',(1.01778810567665,-0.587620236790409,
-16.6166666666667));
#359407=CARTESIAN_POINT('Ctrl Pts',(1.35705080756887,5.33569582427831E-15,
-16.575));
#359408=CARTESIAN_POINT('Ctrl Pts',(1.01778810567665,0.587620236790419,
-16.5333333333333));
#359409=CARTESIAN_POINT('Ctrl Pts',(0.678525403784435,1.17524047358083,
-16.4916666666667));
#359410=CARTESIAN_POINT('Ctrl Pts',(0.,1.17524047358083,-16.45));
#359411=CARTESIAN_POINT('Ctrl Pts',(-0.678525403784434,1.17524047358083,
-16.4083333333333));
#359412=CARTESIAN_POINT('Ctrl Pts',(-1.01778810567665,0.58762023679042,
-16.3666666666667));
#359413=CARTESIAN_POINT('Ctrl Pts',(-1.35705080756887,5.55880349008565E-15,
-16.325));
#359414=CARTESIAN_POINT('Ctrl Pts',(-1.01778810567665,-0.587620236790408,
-16.2833333333333));
#359415=CARTESIAN_POINT('Ctrl Pts',(-0.678525403784435,-1.17524047358082,
-16.2416666666667));
#359416=CARTESIAN_POINT('Ctrl Pts',(-1.43925448419918E-16,-1.17524047358082,
-16.2));
#359417=CARTESIAN_POINT('Ctrl Pts',(-1.43925448419918E-16,-1.17524047358082,
-16.6375));
#359418=CARTESIAN_POINT('Ctrl Pts',(0.678525403784434,-1.17524047358082,
-16.5958333333333));
#359419=CARTESIAN_POINT('Ctrl Pts',(1.01778810567665,-0.587620236790409,
-16.5541666666667));
#359420=CARTESIAN_POINT('Ctrl Pts',(1.35705080756887,5.30837734434166E-15,
-16.5125));
#359421=CARTESIAN_POINT('Ctrl Pts',(1.01778810567665,0.587620236790419,
-16.4708333333333));
#359422=CARTESIAN_POINT('Ctrl Pts',(0.678525403784435,1.17524047358083,
-16.4291666666667));
#359423=CARTESIAN_POINT('Ctrl Pts',(0.,1.17524047358083,-16.3875));
#359424=CARTESIAN_POINT('Ctrl Pts',(-0.678525403784434,1.17524047358083,
-16.3458333333333));
#359425=CARTESIAN_POINT('Ctrl Pts',(-1.01778810567665,0.58762023679042,
-16.3041666666667));
#359426=CARTESIAN_POINT('Ctrl Pts',(-1.35705080756887,5.53148501014901E-15,
-16.2625));
#359427=CARTESIAN_POINT('Ctrl Pts',(-1.01778810567665,-0.587620236790409,
-16.2208333333333));
#359428=CARTESIAN_POINT('Ctrl Pts',(-0.678525403784435,-1.17524047358082,
-16.1791666666667));
#359429=CARTESIAN_POINT('Ctrl Pts',(-1.43925448419918E-16,-1.17524047358082,
-16.1375));
#359430=CARTESIAN_POINT('Origin',(-1.38777878078146E-16,-5.55111512312578E-15,
-17.91875));
#359431=CARTESIAN_POINT('',(8.49534406465091E-16,-1.17524047358082,-17.2));
#359432=CARTESIAN_POINT('',(9.47989861505363E-16,-1.17524047358082,-17.1375));
#359433=CARTESIAN_POINT('',(-4.21481204576211E-16,-1.17524047358085,-17.91875));
#359434=CARTESIAN_POINT('Ctrl Pts',(-1.43925448419918E-16,-1.17524047358082,
-17.2));
#359435=CARTESIAN_POINT('Ctrl Pts',(0.678525403784434,-1.17524047358082,
-17.1583333333333));
#359436=CARTESIAN_POINT('Ctrl Pts',(1.01778810567665,-0.587620236790409,
-17.1166666666667));
#359437=CARTESIAN_POINT('Ctrl Pts',(1.35705080756887,5.55424366377145E-15,
-17.075));
#359438=CARTESIAN_POINT('Ctrl Pts',(1.01778810567665,0.587620236790419,
-17.0333333333333));
#359439=CARTESIAN_POINT('Ctrl Pts',(0.678525403784435,1.17524047358083,
-16.9916666666667));
#359440=CARTESIAN_POINT('Ctrl Pts',(0.,1.17524047358083,-16.95));
#359441=CARTESIAN_POINT('Ctrl Pts',(-0.678525403784434,1.17524047358083,
-16.9083333333333));
#359442=CARTESIAN_POINT('Ctrl Pts',(-1.01778810567665,0.58762023679042,
-16.8666666666667));
#359443=CARTESIAN_POINT('Ctrl Pts',(-1.35705080756887,5.77735132957879E-15,
-16.825));
#359444=CARTESIAN_POINT('Ctrl Pts',(-1.01778810567665,-0.587620236790408,
-16.7833333333333));
#359445=CARTESIAN_POINT('Ctrl Pts',(-0.678525403784435,-1.17524047358082,
-16.7416666666667));
#359446=CARTESIAN_POINT('Ctrl Pts',(-1.43925448419918E-16,-1.17524047358082,
-16.7));
#359447=CARTESIAN_POINT('Ctrl Pts',(-1.43925448419918E-16,-1.17524047358082,
-17.1375));
#359448=CARTESIAN_POINT('Ctrl Pts',(0.678525403784434,-1.17524047358082,
-17.0958333333333));
#359449=CARTESIAN_POINT('Ctrl Pts',(1.01778810567665,-0.587620236790409,
-17.0541666666667));
#359450=CARTESIAN_POINT('Ctrl Pts',(1.35705080756887,5.52692518383481E-15,
-17.0125));
#359451=CARTESIAN_POINT('Ctrl Pts',(1.01778810567665,0.587620236790419,
-16.9708333333333));
#359452=CARTESIAN_POINT('Ctrl Pts',(0.678525403784435,1.17524047358083,
-16.9291666666667));
#359453=CARTESIAN_POINT('Ctrl Pts',(0.,1.17524047358083,-16.8875));
#359454=CARTESIAN_POINT('Ctrl Pts',(-0.678525403784434,1.17524047358083,
-16.8458333333333));
#359455=CARTESIAN_POINT('Ctrl Pts',(-1.01778810567665,0.58762023679042,
-16.8041666666667));
#359456=CARTESIAN_POINT('Ctrl Pts',(-1.35705080756887,5.75003284964215E-15,
-16.7625));
#359457=CARTESIAN_POINT('Ctrl Pts',(-1.01778810567665,-0.587620236790408,
-16.7208333333333));
#359458=CARTESIAN_POINT('Ctrl Pts',(-0.678525403784435,-1.17524047358082,
-16.6791666666667));
#359459=CARTESIAN_POINT('Ctrl Pts',(-1.43925448419918E-16,-1.17524047358082,
-16.6375));
#359460=CARTESIAN_POINT('Origin',(-1.38777878078146E-16,-5.55111512312578E-15,
-17.91875));
#359461=CARTESIAN_POINT('',(4.25993338715498E-16,-1.17524047358085,-17.6497595264195));
#359462=CARTESIAN_POINT('',(1.60346221183174E-16,-1.17524047358082,-17.6375));
#359463=CARTESIAN_POINT('',(-4.21481204576211E-16,-1.17524047358085,-17.91875));
#359464=CARTESIAN_POINT('',(0.689217670442693,-0.951929185124621,-17.6497595264192));
#359465=CARTESIAN_POINT('Origin',(1.61565205658576E-12,-4.96575003339217E-12,
-17.6497595264242));
#359466=CARTESIAN_POINT('Ctrl Pts',(0.689217670442693,-0.951929185124621,
-17.6497595264192));
#359467=CARTESIAN_POINT('Ctrl Pts',(0.892378271989712,-0.80483644050495,
-17.6320689189856));
#359468=CARTESIAN_POINT('Ctrl Pts',(1.01778810567665,-0.587620236790409,
-17.6166666666667));
#359469=CARTESIAN_POINT('Ctrl Pts',(1.35705080756887,5.77279150326459E-15,
-17.575));
#359470=CARTESIAN_POINT('Ctrl Pts',(1.01778810567665,0.587620236790419,
-17.5333333333333));
#359471=CARTESIAN_POINT('Ctrl Pts',(0.678525403784435,1.17524047358083,
-17.4916666666667));
#359472=CARTESIAN_POINT('Ctrl Pts',(0.,1.17524047358083,-17.45));
#359473=CARTESIAN_POINT('Ctrl Pts',(-0.678525403784434,1.17524047358083,
-17.4083333333333));
#359474=CARTESIAN_POINT('Ctrl Pts',(-1.01778810567665,0.58762023679042,
-17.3666666666667));
#359475=CARTESIAN_POINT('Ctrl Pts',(-1.35705080756887,5.99589916907193E-15,
-17.325));
#359476=CARTESIAN_POINT('Ctrl Pts',(-1.01778810567665,-0.587620236790408,
-17.2833333333333));
#359477=CARTESIAN_POINT('Ctrl Pts',(-0.678525403784435,-1.17524047358082,
-17.2416666666667));
#359478=CARTESIAN_POINT('Ctrl Pts',(-1.43925448419918E-16,-1.17524047358082,
-17.2));
#359479=CARTESIAN_POINT('Ctrl Pts',(-1.43925448419918E-16,-1.17524047358082,
-17.6375));
#359480=CARTESIAN_POINT('Ctrl Pts',(0.678525403784434,-1.17524047358082,
-17.5958333333333));
#359481=CARTESIAN_POINT('Ctrl Pts',(1.01778810567665,-0.587620236790409,
-17.5541666666667));
#359482=CARTESIAN_POINT('Ctrl Pts',(1.35705080756887,5.74547302332795E-15,
-17.5125));
#359483=CARTESIAN_POINT('Ctrl Pts',(1.01778810567665,0.587620236790419,
-17.4708333333333));
#359484=CARTESIAN_POINT('Ctrl Pts',(0.678525403784435,1.17524047358083,
-17.4291666666667));
#359485=CARTESIAN_POINT('Ctrl Pts',(0.,1.17524047358083,-17.3875));
#359486=CARTESIAN_POINT('Ctrl Pts',(-0.678525403784434,1.17524047358083,
-17.3458333333333));
#359487=CARTESIAN_POINT('Ctrl Pts',(-1.01778810567665,0.58762023679042,
-17.3041666666667));
#359488=CARTESIAN_POINT('Ctrl Pts',(-1.35705080756887,5.96858068913529E-15,
-17.2625));
#359489=CARTESIAN_POINT('Ctrl Pts',(-1.01778810567665,-0.587620236790408,
-17.2208333333333));
#359490=CARTESIAN_POINT('Ctrl Pts',(-0.678525403784435,-1.17524047358082,
-17.1791666666667));
#359491=CARTESIAN_POINT('Ctrl Pts',(-1.43925448419918E-16,-1.17524047358082,
-17.1375));
#359492=CARTESIAN_POINT('Origin',(0.,1.30104260698261E-15,-17.7));
#359493=CARTESIAN_POINT('',(-1.83697019872102E-16,-1.5,-1.95));
#359494=CARTESIAN_POINT('',(-6.61501184751346E-14,-1.5,-1.88750000000001));
#359495=CARTESIAN_POINT('',(-1.83697019872103E-16,-1.5,-17.7));
#359496=CARTESIAN_POINT('',(0.,1.49999999999999,-1.7));
#359497=CARTESIAN_POINT('Ctrl Pts',(-1.83697019872102E-16,-1.5,-1.95));
#359498=CARTESIAN_POINT('Ctrl Pts',(0.866025403784435,-1.5,-1.90833333333333));
#359499=CARTESIAN_POINT('Ctrl Pts',(1.29903810567665,-0.749999999999999,
-1.86666666666667));
#359500=CARTESIAN_POINT('Ctrl Pts',(1.73205080756887,-1.1803518232214E-15,
-1.825));
#359501=CARTESIAN_POINT('Ctrl Pts',(1.29903810567666,0.749999999999996,
-1.78333333333333));
#359502=CARTESIAN_POINT('Ctrl Pts',(0.866025403784437,1.49999999999999,
-1.74166666666667));
#359503=CARTESIAN_POINT('Ctrl Pts',(0.,1.49999999999999,-1.7));
#359504=CARTESIAN_POINT('',(1.05094390383304,1.07028823734365,-1.7));
#359505=CARTESIAN_POINT('Origin',(0.,0.,-1.7));
#359506=CARTESIAN_POINT('Ctrl Pts',(1.05094390383304,1.07028823734365,-1.7));
#359507=CARTESIAN_POINT('Ctrl Pts',(1.14778830372624,0.975194198058742,
-1.70730092945357));
#359508=CARTESIAN_POINT('Ctrl Pts',(1.23123736281864,0.867435515515267,
-1.71430913802694));
#359509=CARTESIAN_POINT('Ctrl Pts',(1.36688476559254,0.632484953062897,
-1.72736194705207));
#359510=CARTESIAN_POINT('Ctrl Pts',(1.41846105744624,0.506328944455555,
-1.73437061419692));
#359511=CARTESIAN_POINT('Ctrl Pts',(1.50131107274971,0.18544000545117,-1.75219777747494));
#359512=CARTESIAN_POINT('Ctrl Pts',(1.51267225119167,-0.0118599651810934,
-1.76315888695451));
#359513=CARTESIAN_POINT('Ctrl Pts',(1.45854265849392,-0.402738183258619,
-1.78487434351437));
#359514=CARTESIAN_POINT('Ctrl Pts',(1.39237486911582,-0.592268370697173,
-1.79529456539463));
#359515=CARTESIAN_POINT('Ctrl Pts',(1.19416446946585,-0.927559693188778,
-1.81414461554112));
#359516=CARTESIAN_POINT('Ctrl Pts',(1.06665301676792,-1.07173833930981,
-1.8242844755617));
#359517=CARTESIAN_POINT('Ctrl Pts',(0.758646728034023,-1.3090883887425,
-1.84569649196644));
#359518=CARTESIAN_POINT('Ctrl Pts',(0.579280583753319,-1.39774711600699,
-1.85678899203078));
#359519=CARTESIAN_POINT('Ctrl Pts',(0.261088126463976,-1.48292231711216,
-1.87446401157843));
#359520=CARTESIAN_POINT('Ctrl Pts',(0.130699839833624,-1.50000000000001,
-1.88121170102409));
#359521=CARTESIAN_POINT('Ctrl Pts',(-1.34267597040605E-13,-1.5,-1.88750000000001));
#359522=CARTESIAN_POINT('Origin',(0.,1.30104260698261E-15,-17.7));
#359523=CARTESIAN_POINT('',(-9.90402146771155E-14,-1.5,-2.45000000000001));
#359524=CARTESIAN_POINT('',(-9.90925172839362E-14,-1.5,-2.38750000000001));
#359525=CARTESIAN_POINT('',(-1.83697019872103E-16,-1.5,-17.7));
#359526=CARTESIAN_POINT('Ctrl Pts',(-1.9671764217577E-13,-1.5,-2.45000000000001));
#359527=CARTESIAN_POINT('Ctrl Pts',(0.13402462108747,-1.50000000000002,
-2.44355173741143));
#359528=CARTESIAN_POINT('Ctrl Pts',(0.267693944681743,-1.48204243818681,
-2.43662174791999));
#359529=CARTESIAN_POINT('Ctrl Pts',(0.588398068733159,-1.39391513012925,
-2.418743882778));
#359530=CARTESIAN_POINT('Ctrl Pts',(0.767066381476009,-1.30415324991582,
-2.40765431401171));
#359531=CARTESIAN_POINT('Ctrl Pts',(1.07336246827429,-1.06499776836812,
-2.38627442884388));
#359532=CARTESIAN_POINT('Ctrl Pts',(1.19989176294859,-0.920114875846726,
-2.37616226052323));
#359533=CARTESIAN_POINT('Ctrl Pts',(1.39597225273381,-0.583731732015755,
-2.35738435734234));
#359534=CARTESIAN_POINT('Ctrl Pts',(1.46097640834344,-0.393813415120927,
-2.34687852306227));
#359535=CARTESIAN_POINT('Ctrl Pts',(1.51270125975872,-0.00273603458184616,
-2.32515200192121));
#359536=CARTESIAN_POINT('Ctrl Pts',(1.50016560131882,0.194373847288857,
-2.31420145292839));
#359537=CARTESIAN_POINT('Ctrl Pts',(1.40151516251111,0.567386311023262,
-2.29347853827648));
#359538=CARTESIAN_POINT('Ctrl Pts',(1.31838001246478,0.740295537016906,
-2.28453348967375));
#359539=CARTESIAN_POINT('Ctrl Pts',(1.0867276214625,1.05289539990168,-2.26470477929054));
#359540=CARTESIAN_POINT('Ctrl Pts',(0.937699507927868,1.18754656333423,
-2.25379435073969));
#359541=CARTESIAN_POINT('Ctrl Pts',(0.600554016430472,1.38807100973555,
-2.23200330720587));
#359542=CARTESIAN_POINT('Ctrl Pts',(0.416746893615161,1.45387169407227,
-2.22133208609904));
#359543=CARTESIAN_POINT('Ctrl Pts',(0.0343336710579792,1.51202215612334,
-2.20131793073775));
#359544=CARTESIAN_POINT('Ctrl Pts',(-0.160626851633572,1.50385916690459,
-2.1923790360782));
#359545=CARTESIAN_POINT('Ctrl Pts',(-0.541938187767889,1.41271939452019,
-2.17150152552067));
#359546=CARTESIAN_POINT('Ctrl Pts',(-0.724074881041112,1.32860097202541,
-2.16040184693271));
#359547=CARTESIAN_POINT('Ctrl Pts',(-1.03892987114642,1.09871648363606,
-2.13886769892525));
#359548=CARTESIAN_POINT('Ctrl Pts',(-1.17039619602381,0.957469831855792,
-2.12861900431547));
#359549=CARTESIAN_POINT('Ctrl Pts',(-1.37806863845292,0.625379279765833,
-2.10940262171244));
#359550=CARTESIAN_POINT('Ctrl Pts',(-1.44923266130069,0.435817040915999,
-2.09921205782865));
#359551=CARTESIAN_POINT('Ctrl Pts',(-1.51212785796491,0.0441443608115303,
-2.07745246448952));
#359552=CARTESIAN_POINT('Ctrl Pts',(-1.50493731564591,-0.153773201783428,
-2.06645704434535));
#359553=CARTESIAN_POINT('Ctrl Pts',(-1.4162035687073,-0.529582002360993,
-2.0455787776466));
#359554=CARTESIAN_POINT('Ctrl Pts',(-1.33783840494363,-0.704459485177441,
-2.03646512790282));
#359555=CARTESIAN_POINT('Ctrl Pts',(-1.11489389214297,-1.02301975413814,
-2.01688980866948));
#359556=CARTESIAN_POINT('Ctrl Pts',(-0.969591515547866,-1.16164946042504,
-2.00604811964142));
#359557=CARTESIAN_POINT('Ctrl Pts',(-0.680123042456934,-1.34464086446392,
-1.9870379666797));
#359558=CARTESIAN_POINT('Ctrl Pts',(-0.548326703601818,-1.40355542471544,
-1.97906039680748));
#359559=CARTESIAN_POINT('Ctrl Pts',(-0.276687652879418,-1.48077724317562,
-1.96384610637328));
#359560=CARTESIAN_POINT('Ctrl Pts',(-0.138651093382613,-1.5,-1.95667085384066));
#359561=CARTESIAN_POINT('Ctrl Pts',(-3.52148865623292E-14,-1.5,-1.95));
#359562=CARTESIAN_POINT('Ctrl Pts',(-1.32116539930397E-13,-1.5,-1.88750000000001));
#359563=CARTESIAN_POINT('Ctrl Pts',(-0.0630459354937167,-1.49999999999999,
-1.89053329898572));
#359564=CARTESIAN_POINT('Ctrl Pts',(-0.126153654145855,-1.49602560948929,
-1.89367997025144));
#359565=CARTESIAN_POINT('Ctrl Pts',(-0.380391049639784,-1.46374247408504,
-1.90680872640654));
#359566=CARTESIAN_POINT('Ctrl Pts',(-0.565328631914033,-1.40272109928616,
-1.91740157817117));
#359567=CARTESIAN_POINT('Ctrl Pts',(-0.908590211261669,-1.21025079912723,
-1.93926315583438));
#359568=CARTESIAN_POINT('Ctrl Pts',(-1.06213966579464,-1.07801640891699,
-1.95032398491593));
#359569=CARTESIAN_POINT('Ctrl Pts',(-1.30190549243595,-0.768979436081477,
-1.97044408398529));
#359570=CARTESIAN_POINT('Ctrl Pts',(-1.3889317576496,-0.597629494593554,
-1.97929836141147));
#359571=CARTESIAN_POINT('Ctrl Pts',(-1.49553456304681,-0.226916662076369,
-1.99989351877353));
#359572=CARTESIAN_POINT('Ctrl Pts',(-1.51234048224347,-0.0305584413693756,
-2.01080230881281));
#359573=CARTESIAN_POINT('Ctrl Pts',(-1.46940043446806,0.361063630422814,
-2.03255909057905));
#359574=CARTESIAN_POINT('Ctrl Pts',(-1.40867884223088,0.552407827581791,
-2.04318932375454));
#359575=CARTESIAN_POINT('Ctrl Pts',(-1.22029994828342,0.892772080145689,
-2.06209844889699));
#359576=CARTESIAN_POINT('Ctrl Pts',(-1.09735642690313,1.04020596571789,
-2.07193135778637));
#359577=CARTESIAN_POINT('Ctrl Pts',(-0.797217630311482,1.28587258658769,
-2.09319586517218));
#359578=CARTESIAN_POINT('Ctrl Pts',(-0.621124840206183,1.37957647161791,
-2.1042710191816));
#359579=CARTESIAN_POINT('Ctrl Pts',(-0.244153347521547,1.49293041144923,
-2.12555678913066));
#359580=CARTESIAN_POINT('Ctrl Pts',(-0.0471526458057884,1.51202381890725,
-2.13489737230127));
#359581=CARTESIAN_POINT('Ctrl Pts',(0.33946412644781,1.47370339852615,-2.15456293655079));
#359582=CARTESIAN_POINT('Ctrl Pts',(0.525520914200402,1.41804336382786,
-2.1650607100002));
#359583=CARTESIAN_POINT('Ctrl Pts',(0.873141096667831,1.23597292300454,
-2.18684310607224));
#359584=CARTESIAN_POINT('Ctrl Pts',(1.02999901103478,1.10865716365545,-2.19792648486674));
#359585=CARTESIAN_POINT('Ctrl Pts',(1.27886345971825,0.806867253437241,
-2.21828303429828));
#359586=CARTESIAN_POINT('Ctrl Pts',(1.371146755331,0.637561816499381,-2.22707989908337));
#359587=CARTESIAN_POINT('Ctrl Pts',(1.48829207763262,0.269974513241264,
-2.24750141593104));
#359588=CARTESIAN_POINT('Ctrl Pts',(1.51072886710611,0.0747545175846843,
-2.2583469712453));
#359589=CARTESIAN_POINT('Ctrl Pts',(1.47944113616424,-0.317448794119751,
-2.28013604411777));
#359590=CARTESIAN_POINT('Ctrl Pts',(1.42439209642333,-0.510539588190993,
-2.29086331045506));
#359591=CARTESIAN_POINT('Ctrl Pts',(1.24625240280759,-0.856112386695717,
-2.31006179926088));
#359592=CARTESIAN_POINT('Ctrl Pts',(1.12794162744611,-1.00690142291868,
-2.31953470045029));
#359593=CARTESIAN_POINT('Ctrl Pts',(0.836017749690881,-1.26089744854786,
-2.34063533972373));
#359594=CARTESIAN_POINT('Ctrl Pts',(0.663421738107635,-1.35965436438064,
-2.3516826168648));
#359595=CARTESIAN_POINT('Ctrl Pts',(0.322789903704657,-1.47382168933245,
-2.37124258822072));
#359596=CARTESIAN_POINT('Ctrl Pts',(0.161815744149655,-1.50000000000002,
-2.37971463637968));
#359597=CARTESIAN_POINT('Ctrl Pts',(-1.94774751882676E-13,-1.5,-2.38750000000001));
#359598=CARTESIAN_POINT('Origin',(0.,1.30104260698261E-15,-17.7));
#359599=CARTESIAN_POINT('',(-8.25256904935245E-14,-1.5,-2.95000000000001));
#359600=CARTESIAN_POINT('',(-1.78584683734892E-16,-1.5,-2.8875));
#359601=CARTESIAN_POINT('',(-1.83697019872103E-16,-1.5,-17.7));
#359602=CARTESIAN_POINT('Ctrl Pts',(-1.61849700308636E-13,-1.5,-2.95000000000001));
#359603=CARTESIAN_POINT('Ctrl Pts',(0.165288383140628,-1.50000000000002,
-2.94204755895832));
#359604=CARTESIAN_POINT('Ctrl Pts',(0.329658389342383,-1.47268563787592,
-2.93338057106647));
#359605=CARTESIAN_POINT('Ctrl Pts',(0.672640418581653,-1.35509817342272,
-2.91361252203373));
#359606=CARTESIAN_POINT('Ctrl Pts',(0.844448431113153,-1.25524630653446,
-2.90257274220761));
#359607=CARTESIAN_POINT('Ctrl Pts',(1.13455909306952,-0.999432396303687,
-2.88150884452548));
#359608=CARTESIAN_POINT('Ctrl Pts',(1.25185338819377,-0.847895132696047,
-2.87210528514977));
#359609=CARTESIAN_POINT('Ctrl Pts',(1.42771316089353,-0.501179875879174,
-2.85284332643772));
#359610=CARTESIAN_POINT('Ctrl Pts',(1.48149535181862,-0.307724647052924,
-2.84209581372515));
#359611=CARTESIAN_POINT('Ctrl Pts',(1.51019581240691,0.0845604829928128,
-2.82030219538927));
#359612=CARTESIAN_POINT('Ctrl Pts',(1.48651547065014,0.279506231582944,
-2.80947187602315));
#359613=CARTESIAN_POINT('Ctrl Pts',(1.36703139770437,0.646388427216387,
-2.7890895318213));
#359614=CARTESIAN_POINT('Ctrl Pts',(1.27356576840097,0.815243309367391,
-2.78029548078564));
#359615=CARTESIAN_POINT('Ctrl Pts',(1.02267248733059,1.11539498923852,-2.7598868255089));
#359616=CARTESIAN_POINT('Ctrl Pts',(0.865093561537473,1.24159755754438,
-2.74879967900941));
#359617=CARTESIAN_POINT('Ctrl Pts',(0.516538142626489,1.42132404965192,
-2.72703739603956));
#359618=CARTESIAN_POINT('Ctrl Pts',(0.330251435818131,1.47577996610756,
-2.71656200833338));
#359619=CARTESIAN_POINT('Ctrl Pts',(-0.0568477531729474,1.51173860477736,
-2.6969388388453));
#359620=CARTESIAN_POINT('Ctrl Pts',(-0.254103822357107,1.49131850056533,
-2.68753327138459));
#359621=CARTESIAN_POINT('Ctrl Pts',(-0.630514143493244,1.37529133677861,
-2.66620024459326));
#359622=CARTESIAN_POINT('Ctrl Pts',(-0.805847286381485,1.28046165486068,
-2.65513036699184));
#359623=CARTESIAN_POINT('Ctrl Pts',(-1.10417677040217,1.03294703285061,
-2.63390157683268));
#359624=CARTESIAN_POINT('Ctrl Pts',(-1.22609577350809,0.884778776179429,
-2.62415437645441));
#359625=CARTESIAN_POINT('Ctrl Pts',(-1.41223190619847,0.54326288429914,
-2.60518127134995));
#359626=CARTESIAN_POINT('Ctrl Pts',(-1.47171370609588,0.351520774197525,
-2.59452893189986));
#359627=CARTESIAN_POINT('Ctrl Pts',(-1.51209751636429,-0.0402586447386417,
-2.57276340862563));
#359628=CARTESIAN_POINT('Ctrl Pts',(-1.49405206137872,-0.236380762456758,
-2.56186773541907));
#359629=CARTESIAN_POINT('Ctrl Pts',(-1.38513458137321,-0.606414827864824,
-2.54131028734084));
#359630=CARTESIAN_POINT('Ctrl Pts',(-1.2969640075808,-0.777313818812451,
-2.53247482605294));
#359631=CARTESIAN_POINT('Ctrl Pts',(-1.05520727397145,-1.08477866057793,
-2.51230260973492));
#359632=CARTESIAN_POINT('Ctrl Pts',(-0.900923590882587,-1.21594716801792,
-2.50123606292023));
#359633=CARTESIAN_POINT('Ctrl Pts',(-0.556685633384153,-1.40615771484799,
-2.47939028016714));
#359634=CARTESIAN_POINT('Ctrl Pts',(-0.37149097115162,-1.46601150780009,
-2.46881749246633));
#359635=CARTESIAN_POINT('Ctrl Pts',(-0.120167666258793,-1.4963939642998,
-2.45588173719688));
#359636=CARTESIAN_POINT('Ctrl Pts',(-0.0600530205189941,-1.49999999999999,
-2.45288930229686));
#359637=CARTESIAN_POINT('Ctrl Pts',(-1.97896732334359E-13,-1.5,-2.45000000000001));
#359638=CARTESIAN_POINT('Ctrl Pts',(-1.98001337548E-13,-1.5,-2.38750000000001));
#359639=CARTESIAN_POINT('Ctrl Pts',(-0.0354619996939313,-1.5,-2.38920616625578));
#359640=CARTESIAN_POINT('Ctrl Pts',(-0.0709610799037976,-1.49874248423541,
-2.39094904754232));
#359641=CARTESIAN_POINT('Ctrl Pts',(-0.297872095609908,-1.48260149916315,
-2.4023146695721));
#359642=CARTESIAN_POINT('Ctrl Pts',(-0.484903676285203,-1.43236976673905,
-2.41270855659359));
#359643=CARTESIAN_POINT('Ctrl Pts',(-0.83661435230043,-1.26088978502587,
-2.43439357720847));
#359644=CARTESIAN_POINT('Ctrl Pts',(-0.99665928184499,-1.13861690195684,
-2.44549021144553));
#359645=CARTESIAN_POINT('Ctrl Pts',(-1.25463111003332,-0.844246553149174,
-2.46607884094973));
#359646=CARTESIAN_POINT('Ctrl Pts',(-1.35225256821551,-0.676952070131101,
-2.47489155165953));
#359647=CARTESIAN_POINT('Ctrl Pts',(-1.47986428692361,-0.312552254437961,
-2.49513598586471));
#359648=CARTESIAN_POINT('Ctrl Pts',(-1.50784766080662,-0.118620346000367,
-2.5059099807779));
#359649=CARTESIAN_POINT('Ctrl Pts',(-1.48813911227417,0.27381573292194,
-2.52771198516247));
#359650=CARTESIAN_POINT('Ctrl Pts',(-1.43878040665445,0.468471388304962,
-2.5385261882393));
#359651=CARTESIAN_POINT('Ctrl Pts',(-1.27086766016973,0.819118665189983,
-2.55800659251069));
#359652=CARTESIAN_POINT('Ctrl Pts',(-1.1570763481502,0.973268823233719,
-2.56719871666685));
#359653=CARTESIAN_POINT('Ctrl Pts',(-0.873239887321544,1.23531833702727,
-2.58813395791655));
#359654=CARTESIAN_POINT('Ctrl Pts',(-0.704201890786818,1.33890131196317,
-2.5991441071761));
#359655=CARTESIAN_POINT('Ctrl Pts',(-0.332586384393808,1.47625092023645,
-2.62083873346016));
#359656=CARTESIAN_POINT('Ctrl Pts',(-0.133240227340225,1.50736305210793,
-2.63088494734811));
#359657=CARTESIAN_POINT('Ctrl Pts',(0.257535381626867,1.49007251733879,
-2.65016644023308));
#359658=CARTESIAN_POINT('Ctrl Pts',(0.445359126004437,1.44508610081268,
-2.66045273702907));
#359659=CARTESIAN_POINT('Ctrl Pts',(0.800717433943054,1.28389709171077,
-2.68202739406638));
#359660=CARTESIAN_POINT('Ctrl Pts',(0.963688186958386,1.16655655682656,
-2.693127787379));
#359661=CARTESIAN_POINT('Ctrl Pts',(1.23037332501627,0.879446537972054,
-2.71393396036773));
#359662=CARTESIAN_POINT('Ctrl Pts',(1.33317837581294,0.71405706917474,-2.72283016282377));
#359663=CARTESIAN_POINT('Ctrl Pts',(1.47073067960114,0.352758008589517,
-2.74290233285627));
#359664=CARTESIAN_POINT('Ctrl Pts',(1.50393194006517,0.160192748766035,
-2.75360040284647));
#359665=CARTESIAN_POINT('Ctrl Pts',(1.49520969110581,-0.232146380068924,
-2.77539702111507));
#359666=CARTESIAN_POINT('Ctrl Pts',(1.45129899090333,-0.428128946154902,
-2.78628494145318));
#359667=CARTESIAN_POINT('Ctrl Pts',(1.29315560005151,-0.783500996520054,
-2.80602783314013));
#359668=CARTESIAN_POINT('Ctrl Pts',(1.18359106897811,-0.940876127785583,
-2.81502322947043));
#359669=CARTESIAN_POINT('Ctrl Pts',(0.90736895290096,-1.21038374162605,
-2.83579929483321));
#359670=CARTESIAN_POINT('Ctrl Pts',(0.741778816430195,-1.31837276364729,
-2.8467659490449));
#359671=CARTESIAN_POINT('Ctrl Pts',(0.38197060730477,-1.46320976555244,
-2.86810047963075));
#359672=CARTESIAN_POINT('Ctrl Pts',(0.191810212068219,-1.5,-2.87827152686909));
#359673=CARTESIAN_POINT('Ctrl Pts',(1.04083408558608E-15,-1.5,-2.8875));
#359674=CARTESIAN_POINT('Origin',(0.,1.30104260698261E-15,-17.7));
#359675=CARTESIAN_POINT('',(-2.30626176757078E-16,-1.5,-3.45));
#359676=CARTESIAN_POINT('',(3.27638141250644E-14,-1.5,-3.3875));
#359677=CARTESIAN_POINT('',(-1.83697019872103E-16,-1.5,-17.7));
#359678=CARTESIAN_POINT('Ctrl Pts',(-1.2490009027033E-15,-1.5,-3.45));
#359679=CARTESIAN_POINT('Ctrl Pts',(0.194839574775211,-1.5,-3.44062577658789));
#359680=CARTESIAN_POINT('Ctrl Pts',(0.387930314093105,-1.46203733311044,
-3.4302811755361));
#359681=CARTESIAN_POINT('Ctrl Pts',(0.749532372686592,-1.31396321843056,
-3.40877041852818));
#359682=CARTESIAN_POINT('Ctrl Pts',(0.914390188142045,-1.20507006247664,
-3.39781388329645));
#359683=CARTESIAN_POINT('Ctrl Pts',(1.18902016837216,-0.934017544320743,
-3.37707150559656));
#359684=CARTESIAN_POINT('Ctrl Pts',(1.29770352229627,-0.775960061968662,
-3.36810889233159));
#359685=CARTESIAN_POINT('Ctrl Pts',(1.4537863214166,-0.419607064539616,
-3.34831150358553));
#359686=CARTESIAN_POINT('Ctrl Pts',(1.49654731889376,-0.22336553782117,
-3.33740919654562));
#359687=CARTESIAN_POINT('Ctrl Pts',(1.50296332271505,0.168913881670837,
-3.31561589546273));
#359688=CARTESIAN_POINT('Ctrl Pts',(1.46867222228306,0.361174373701028,
-3.3049347570166));
#359689=CARTESIAN_POINT('Ctrl Pts',(1.32903047402259,0.721812101030813,
-3.2848993277205));
#359690=CARTESIAN_POINT('Ctrl Pts',(1.22512055917265,0.88680186686731,-3.27597692186157));
#359691=CARTESIAN_POINT('Ctrl Pts',(0.956596926263572,1.17235797709162,
-3.25512545837668));
#359692=CARTESIAN_POINT('Ctrl Pts',(0.793024621943816,1.28864441531711,
-3.24402540337617));
#359693=CARTESIAN_POINT('Ctrl Pts',(0.436930598254616,1.44764249247397,
-3.222476208419));
#359694=CARTESIAN_POINT('Ctrl Pts',(0.248957567346252,1.49151587549274,
-3.21221364666887));
#359695=CARTESIAN_POINT('Ctrl Pts',(-0.14223671704898,1.50659840697105,
-3.19297334367772));
#359696=CARTESIAN_POINT('Ctrl Pts',(-0.341836891795151,1.47419638644906,
-3.18283659783216));
#359697=CARTESIAN_POINT('Ctrl Pts',(-0.712841222585338,1.33430327539119,
-3.16110072389287));
#359698=CARTESIAN_POINT('Ctrl Pts',(-0.881101165984585,1.22970378321009,
-3.15009977214211));
#359699=CARTESIAN_POINT('Ctrl Pts',(-1.16320142576591,0.965943362945885,
-3.12920053872451));
#359700=CARTESIAN_POINT('Ctrl Pts',(-1.27602687227312,0.811063267079022,
-3.12005907039326));
#359701=CARTESIAN_POINT('Ctrl Pts',(-1.44172429156805,0.459333958594898,
-3.10051855325525));
#359702=CARTESIAN_POINT('Ctrl Pts',(-1.48984827443744,0.264363031137791,
-3.0896868350632));
#359703=CARTESIAN_POINT('Ctrl Pts',(-1.50705846407638,-0.128078201215698,
-3.06788454437689));
#359704=CARTESIAN_POINT('Ctrl Pts',(-1.47788469594228,-0.321711687080483,
-3.05712712849551));
#359705=CARTESIAN_POINT('Ctrl Pts',(-1.34801380858588,-0.685413434451986,
-3.03692147586376));
#359706=CARTESIAN_POINT('Ctrl Pts',(-1.24922467390369,-0.852274225083107,
-3.02809573278294));
#359707=CARTESIAN_POINT('Ctrl Pts',(-0.989277642706516,-1.14501350029092,
-3.00745737887967));
#359708=CARTESIAN_POINT('Ctrl Pts',(-0.828558780463521,-1.26617753568454,
-2.99635912136486));
#359709=CARTESIAN_POINT('Ctrl Pts',(-0.475998210173412,-1.43533829293318,
-2.9746976330944));
#359710=CARTESIAN_POINT('Ctrl Pts',(-0.288774906769266,-1.48438540427964,
-2.96432742794986));
#359711=CARTESIAN_POINT('Ctrl Pts',(-0.0649141658325175,-1.49894762113898,
-2.95315241700592));
#359712=CARTESIAN_POINT('Ctrl Pts',(-0.0324407882280855,-1.5,-2.95156080815135));
#359713=CARTESIAN_POINT('Ctrl Pts',(-1.64867683967177E-13,-1.5,-2.95000000000001));
#359714=CARTESIAN_POINT('Ctrl Pts',(-1.73472347597681E-16,-1.5,-2.8875));
#359715=CARTESIAN_POINT('Ctrl Pts',(-0.00680225146496058,-1.5,-2.8878272734762));
#359716=CARTESIAN_POINT('Ctrl Pts',(-0.0136064557941092,-1.49995372940945,
-2.88815592620393));
#359717=CARTESIAN_POINT('Ctrl Pts',(-0.211233729968314,-1.49726414908849,
-2.89773898343038));
#359718=CARTESIAN_POINT('Ctrl Pts',(-0.399784487207624,-1.4582757419572,
-2.90789364727691));
#359719=CARTESIAN_POINT('Ctrl Pts',(-0.758949723752875,-1.30892323684144,
-2.92932267347481));
#359720=CARTESIAN_POINT('Ctrl Pts',(-0.925082722468769,-1.19729391658118,
-2.94041656555398));
#359721=CARTESIAN_POINT('Ctrl Pts',(-1.2016354215255,-0.918618321764496,
-2.961463202236));
#359722=CARTESIAN_POINT('Ctrl Pts',(-1.31041923475783,-0.755369011804498,
-2.97053505489987));
#359723=CARTESIAN_POINT('Ctrl Pts',(-1.45915684505256,-0.397648821272951,
-2.99040839881829));
#359724=CARTESIAN_POINT('Ctrl Pts',(-1.49816125722044,-0.206784743462552,
-3.00101195869664));
#359725=CARTESIAN_POINT('Ctrl Pts',(-1.50178248966322,0.186871424042968,
-3.02288174578028));
#359726=CARTESIAN_POINT('Ctrl Pts',(-1.46334013568441,0.385907260634357,
-3.03393929225757));
#359727=CARTESIAN_POINT('Ctrl Pts',(-1.31431367096058,0.747558741474286,
-3.05403104119312));
#359728=CARTESIAN_POINT('Ctrl Pts',(-1.20891120623186,0.908187109041197,
-3.06289698550034));
#359729=CARTESIAN_POINT('Ctrl Pts',(-0.940219556538581,1.18495896237142,
-3.08351252556057));
#359730=CARTESIAN_POINT('Ctrl Pts',(-0.778126123883215,1.29717127951698,
-3.09442825828496));
#359731=CARTESIAN_POINT('Ctrl Pts',(-0.416887645352554,1.4545471223638,
-3.11617990387692));
#359732=CARTESIAN_POINT('Ctrl Pts',(-0.220672017695724,1.49694110218437,
-3.12679794321473));
#359733=CARTESIAN_POINT('Ctrl Pts',(0.168346646154897,1.50261480167819,
-3.1456722151696));
#359734=CARTESIAN_POINT('Ctrl Pts',(0.357434014427285,1.46917687899588,
-3.15555324984303));
#359735=CARTESIAN_POINT('Ctrl Pts',(0.719875708815306,1.33072603506776,
-3.17683709077051));
#359736=CARTESIAN_POINT('Ctrl Pts',(0.888744481011991,1.2244139174965,-3.18791490773795));
#359737=CARTESIAN_POINT('Ctrl Pts',(1.17428852738021,0.953635167188392,
-3.2091747840273));
#359738=CARTESIAN_POINT('Ctrl Pts',(1.28863081923191,0.792333496165166,
-3.21848147243537));
#359739=CARTESIAN_POINT('Ctrl Pts',(1.44750540073537,0.437938742750646,
-3.23817006984728));
#359740=CARTESIAN_POINT('Ctrl Pts',(1.49169755897839,0.248761868219999,
-3.24867989621009));
#359741=CARTESIAN_POINT('Ctrl Pts',(1.50646529866692,-0.143512298964429,
-3.27047290549811));
#359742=CARTESIAN_POINT('Ctrl Pts',(1.4739124382648,-0.342972525396591,
-3.28155402918879));
#359743=CARTESIAN_POINT('Ctrl Pts',(1.33565999918759,-0.708876004675973,
-3.30188200025986));
#359744=CARTESIAN_POINT('Ctrl Pts',(1.23464257562583,-0.873013653000563,
-3.31068194396756));
#359745=CARTESIAN_POINT('Ctrl Pts',(0.973902526018742,-1.15734155812929,
-3.331124802818));
#359746=CARTESIAN_POINT('Ctrl Pts',(0.815587524526735,-1.27386548968896,
-3.34197851275534));
#359747=CARTESIAN_POINT('Ctrl Pts',(0.459622713352567,-1.44161889024216,
-3.36376469440016));
#359748=CARTESIAN_POINT('Ctrl Pts',(0.264706404361307,-1.4897894342995,
-3.37448068035721));
#359749=CARTESIAN_POINT('Ctrl Pts',(0.0440258635328815,-1.49951579390308,
-3.38536835448388));
#359750=CARTESIAN_POINT('Ctrl Pts',(0.0220047927330057,-1.5,-3.38644129391602));
#359751=CARTESIAN_POINT('Ctrl Pts',(6.57113252700009E-14,-1.5,-3.3875));
#359752=CARTESIAN_POINT('Origin',(0.,1.30104260698261E-15,-17.7));
#359753=CARTESIAN_POINT('',(4.93129457402405E-14,-1.5,-3.94999999999999));
#359754=CARTESIAN_POINT('',(9.87353479164595E-14,-1.5,-3.8875));
#359755=CARTESIAN_POINT('',(-1.83697019872103E-16,-1.5,-17.7));
#359756=CARTESIAN_POINT('Ctrl Pts',(9.88095885003532E-14,-1.5,-3.94999999999999));
#359757=CARTESIAN_POINT('Ctrl Pts',(0.0252363046513762,-1.5,-3.94878581772634));
#359758=CARTESIAN_POINT('Ctrl Pts',(0.0504931155048277,-1.49936313763594,
-3.94755295822627));
#359759=CARTESIAN_POINT('Ctrl Pts',(0.274351419805314,-1.48804434710496,
-3.93646815969084));
#359760=CARTESIAN_POINT('Ctrl Pts',(0.468958796760554,-1.4386100389388,
-3.92573193267472));
#359761=CARTESIAN_POINT('Ctrl Pts',(0.823724856932467,-1.26860007743464,
-3.90394074371575));
#359762=CARTESIAN_POINT('Ctrl Pts',(0.98119478738767,-1.15114526004823,
-3.89310183433799));
#359763=CARTESIAN_POINT('Ctrl Pts',(1.2401797942288,-0.86516491335197,-3.87269751386733));
#359764=CARTESIAN_POINT('Ctrl Pts',(1.34022968995924,-0.700242027381734,
-3.86390233485444));
#359765=CARTESIAN_POINT('Ctrl Pts',(1.47608668686549,-0.333411407452506,
-3.84352285596948));
#359766=CARTESIAN_POINT('Ctrl Pts',(1.50733450778141,-0.133879754122094,
-3.83243776411779));
#359767=CARTESIAN_POINT('Ctrl Pts',(1.49010447480495,0.258046256224327,
-3.81066409687632));
#359768=CARTESIAN_POINT('Ctrl Pts',(1.44477012137807,0.446830042571911,
-3.8001761087459));
#359769=CARTESIAN_POINT('Ctrl Pts',(1.28364395592772,0.800475544085902,
-3.78052913643957));
#359770=CARTESIAN_POINT('Ctrl Pts',(1.16804841780491,0.961342385648734,
-3.77116046721349));
#359771=CARTESIAN_POINT('Ctrl Pts',(0.880501965450157,1.2303334256396,-3.74985390874111));
#359772=CARTESIAN_POINT('Ctrl Pts',(0.711043389639699,1.33544695234033,
-3.73878100902493));
#359773=CARTESIAN_POINT('Ctrl Pts',(0.347914392787633,1.47144820878648,
-3.71753214433895));
#359774=CARTESIAN_POINT('Ctrl Pts',(0.158707277139125,1.50365303014975,
-3.70773728049114));
#359775=CARTESIAN_POINT('Ctrl Pts',(-0.230192531608629,1.49550768211014,
-3.68880007005102));
#359776=CARTESIAN_POINT('Ctrl Pts',(-0.426142613523374,1.45186383770904,
-3.67816008832811));
#359777=CARTESIAN_POINT('Ctrl Pts',(-0.786268478591804,1.29223388845718,
-3.6563993593095));
#359778=CARTESIAN_POINT('Ctrl Pts',(-0.947556031090891,1.17908082335176,
-3.64549626762443));
#359779=CARTESIAN_POINT('Ctrl Pts',(-1.21453656609161,0.9006732389317,-3.62491761663351));
#359780=CARTESIAN_POINT('Ctrl Pts',(-1.31899490525424,0.739296289883646,
-3.61607201610451));
#359781=CARTESIAN_POINT('Ctrl Pts',(-1.46571371508099,0.376722917367835,
-3.59592905096475));
#359782=CARTESIAN_POINT('Ctrl Pts',(-1.50289217353618,0.177581924215279,
-3.58486566245628));
#359783=CARTESIAN_POINT('Ctrl Pts',(-1.49687413194325,-0.215803765191046,
-3.5630109019337));
#359784=CARTESIAN_POINT('Ctrl Pts',(-1.45675185089939,-0.406317737064526,
-3.55242679238518));
#359785=CARTESIAN_POINT('Ctrl Pts',(-1.30584168430246,-0.76333179073737,
-3.53259267829224));
#359786=CARTESIAN_POINT('Ctrl Pts',(-1.19587799087183,-0.926164735135001,
-3.52347657513065));
#359787=CARTESIAN_POINT('Ctrl Pts',(-0.917401819753913,-1.20316849336213,
-3.50238383526119));
#359788=CARTESIAN_POINT('Ctrl Pts',(-0.750671697114279,-1.3136693089406,
-3.49129256139612));
#359789=CARTESIAN_POINT('Ctrl Pts',(-0.390805454198223,-1.46069276297905,
-3.46989450387673));
#359790=CARTESIAN_POINT('Ctrl Pts',(-0.202134426667967,-1.49850529477196,
-3.45976671672697));
#359791=CARTESIAN_POINT('Ctrl Pts',(-0.00760865885340758,-1.49998552947111,
-3.45036647372877));
#359792=CARTESIAN_POINT('Ctrl Pts',(-0.00380401527166274,-1.5,-3.45018302077009));
#359793=CARTESIAN_POINT('Ctrl Pts',(-2.77555333642052E-16,-1.5,-3.45));
#359794=CARTESIAN_POINT('Ctrl Pts',(6.57113252700015E-14,-1.5,-3.3875));
#359795=CARTESIAN_POINT('Ctrl Pts',(-0.16761611737248,-1.5,-3.39556443420713));
#359796=CARTESIAN_POINT('Ctrl Pts',(-0.334213726482098,-1.47190970465187,
-3.40436015139458));
#359797=CARTESIAN_POINT('Ctrl Pts',(-0.678945946275743,-1.35197959587786,
-3.42427747996298));
#359798=CARTESIAN_POINT('Ctrl Pts',(-0.85046217873718,-1.25121188156459,
-3.43532866172018));
#359799=CARTESIAN_POINT('Ctrl Pts',(-1.1451974958732,-0.988730720393048,
-3.4568002646434));
#359800=CARTESIAN_POINT('Ctrl Pts',(-1.26534098283104,-0.82943209907657,
-3.46642043894027));
#359801=CARTESIAN_POINT('Ctrl Pts',(-1.43453600430935,-0.478503581222086,
-3.48591646770996));
#359802=CARTESIAN_POINT('Ctrl Pts',(-1.48393134676266,-0.291181964977092,
-3.49632322416801));
#359803=CARTESIAN_POINT('Ctrl Pts',(-1.50994025159247,0.0993750919537776,
-3.51802083844195));
#359804=CARTESIAN_POINT('Ctrl Pts',(-1.4833573561422,0.299094962127195,
-3.52911638678492));
#359805=CARTESIAN_POINT('Ctrl Pts',(-1.35609196549547,0.669195420552612,
-3.5496775233641));
#359806=CARTESIAN_POINT('Ctrl Pts',(-1.25949329466154,0.836949511057635,
-3.55848453146984));
#359807=CARTESIAN_POINT('Ctrl Pts',(-1.00676462571169,1.12877695229422,
-3.57875026303614));
#359808=CARTESIAN_POINT('Ctrl Pts',(-0.85233765382573,1.24948843320678,
-3.5895332308772));
#359809=CARTESIAN_POINT('Ctrl Pts',(-0.501943041270044,1.42743993730768,
-3.61133469687014));
#359810=CARTESIAN_POINT('Ctrl Pts',(-0.308500469336784,1.48134423889683,
-3.62213904866248));
#359811=CARTESIAN_POINT('Ctrl Pts',(0.0792170696405466,1.50989463401122,
-3.64158618398494));
#359812=CARTESIAN_POINT('Ctrl Pts',(0.269529698574956,1.48776003391195,
-3.65080775272698));
#359813=CARTESIAN_POINT('Ctrl Pts',(0.638048212583981,1.37167077299751,
-3.67176280969109));
#359814=CARTESIAN_POINT('Ctrl Pts',(0.811997675149301,1.27641844396522,
-3.68277785513955));
#359815=CARTESIAN_POINT('Ctrl Pts',(1.1157031316742,1.02227239288957,-3.70444950325934));
#359816=CARTESIAN_POINT('Ctrl Pts',(1.24163378932754,0.864955149023215,
-3.71444693616545));
#359817=CARTESIAN_POINT('Ctrl Pts',(1.42087250911037,0.517479170344761,
-3.73375115720314));
#359818=CARTESIAN_POINT('Ctrl Pts',(1.47524805007958,0.332091519884599,
-3.7440504711176));
#359819=CARTESIAN_POINT('Ctrl Pts',(1.51207615194257,-0.0565007591672,-3.76563893106491));
#359820=CARTESIAN_POINT('Ctrl Pts',(1.49126859977781,-0.256308138098137,
-3.77673934100552));
#359821=CARTESIAN_POINT('Ctrl Pts',(1.37471246826402,-0.630365116330303,
-3.79752028424064));
#359822=CARTESIAN_POINT('Ctrl Pts',(1.28238542201467,-0.801673142681147,
-3.80640323435747));
#359823=CARTESIAN_POINT('Ctrl Pts',(1.0373700788615,-1.10062417721052,-3.82649573595481));
#359824=CARTESIAN_POINT('Ctrl Pts',(0.88675666197649,-1.22521801098215,
-3.83720306718031));
#359825=CARTESIAN_POINT('Ctrl Pts',(0.541955371827883,-1.41273746701526,
-3.85900120076603));
#359826=CARTESIAN_POINT('Ctrl Pts',(0.350082293045064,-1.47207493742894,
-3.8698809616402));
#359827=CARTESIAN_POINT('Ctrl Pts',(0.10154674091477,-1.4974249080659,-3.88254279981836));
#359828=CARTESIAN_POINT('Ctrl Pts',(0.0507470353532034,-1.5,-3.8850584321232));
#359829=CARTESIAN_POINT('Ctrl Pts',(1.97654392852791E-13,-1.5,-3.8875));
#359830=CARTESIAN_POINT('Origin',(0.,1.30104260698261E-15,-17.7));
#359831=CARTESIAN_POINT('',(9.87177402016726E-14,-1.5,-4.44999999999999));
#359832=CARTESIAN_POINT('',(1.6283941103285E-14,-1.5,-4.3875));
#359833=CARTESIAN_POINT('',(-1.83697019872103E-16,-1.5,-17.7));
#359834=CARTESIAN_POINT('Ctrl Pts',(1.97619177423217E-13,-1.5,-4.44999999999999));
#359835=CARTESIAN_POINT('Ctrl Pts',(0.0536659410771262,-1.5,-4.44741799620606));
#359836=CARTESIAN_POINT('Ctrl Pts',(0.1073867709094,-1.49712018000069,-4.44475335657562));
#359837=CARTESIAN_POINT('Ctrl Pts',(0.35869308253257,-1.47000106983716,
-4.43190906740457));
#359838=CARTESIAN_POINT('Ctrl Pts',(0.550220156758184,-1.40953987858202,
-4.4210147392146));
#359839=CARTESIAN_POINT('Ctrl Pts',(0.893825668233847,-1.22005325383621,
-4.39921949398176));
#359840=CARTESIAN_POINT('Ctrl Pts',(1.04363434848904,-1.09466695908024,
-4.38852886786029));
#359841=CARTESIAN_POINT('Ctrl Pts',(1.28703766229849,-0.794239658280263,
-4.3684729176645));
#359842=CARTESIAN_POINT('Ctrl Pts',(1.37846968947488,-0.62217906936543,
-4.35956550385356));
#359843=CARTESIAN_POINT('Ctrl Pts',(1.49277156972031,-0.247307197039821,
-4.33873928872436));
#359844=CARTESIAN_POINT('Ctrl Pts',(1.5123698773978,-0.0475019270911679,
-4.32763899594943));
#359845=CARTESIAN_POINT('Ctrl Pts',(1.47328339087223,0.340641046412763,
-4.30607549742144));
#359846=CARTESIAN_POINT('Ctrl Pts',(1.41787176708579,0.525606384079794,
-4.29579964532883));
#359847=CARTESIAN_POINT('Ctrl Pts',(1.23652112732012,0.872346283609986,
-4.27653631757715));
#359848=CARTESIAN_POINT('Ctrl Pts',(1.109355542849,1.02924165184833,-4.26645051422282));
#359849=CARTESIAN_POINT('Ctrl Pts',(0.803761806030416,1.28160144517232,
-4.24473763444591));
#359850=CARTESIAN_POINT('Ctrl Pts',(0.629319521599276,1.37567974358715,
-4.23373149005597));
#359851=CARTESIAN_POINT('Ctrl Pts',(0.260188389018742,1.48942342421312,
-4.21281211347512));
#359852=CARTESIAN_POINT('Ctrl Pts',(0.0697293660230309,1.5103645083182,
-4.20364275869574));
#359853=CARTESIAN_POINT('Ctrl Pts',(-0.317821920574179,1.47937306722689,
-4.18413581536196));
#359854=CARTESIAN_POINT('Ctrl Pts',(-0.510927176963519,1.4242498582582,
-4.17331383413297));
#359855=CARTESIAN_POINT('Ctrl Pts',(-0.860093885236144,1.24414368954539,
-4.15151159391762));
#359856=CARTESIAN_POINT('Ctrl Pts',(-1.01367636304737,1.1225539271368,-4.14074486010845));
#359857=CARTESIAN_POINT('Ctrl Pts',(-1.26468576506506,0.829129986433944,
-4.12051749960359));
#359858=CARTESIAN_POINT('Ctrl Pts',(-1.36033356412408,0.660590476072913,
-4.11169947089286));
#359859=CARTESIAN_POINT('Ctrl Pts',(-1.48522288246882,0.28960013190703,
-4.09108889621698));
#359860=CARTESIAN_POINT('Ctrl Pts',(-1.51052027468975,0.0898468405231036,
-4.07999149114009));
#359861=CARTESIAN_POINT('Ctrl Pts',(-1.48209844719908,-0.300298759920324,
-4.0583167355599));
#359862=CARTESIAN_POINT('Ctrl Pts',(-1.43159003781814,-0.487201763436985,
-4.04793323536453));
#359863=CARTESIAN_POINT('Ctrl Pts',(-1.26016510721411,-0.837370550868243,
-4.02847941384058));
#359864=CARTESIAN_POINT('Ctrl Pts',(-1.13874891978242,-0.996232451394284,
-4.01878162596472));
#359865=CARTESIAN_POINT('Ctrl Pts',(-0.842023813037466,-1.25688555572448,
-3.99726506860101));
#359866=CARTESIAN_POINT('Ctrl Pts',(-0.669954807064273,-1.35643867491598,
-3.9862210302692));
#359867=CARTESIAN_POINT('Ctrl Pts',(-0.327676386565897,-1.4730079980737,
-3.96651511533044));
#359868=CARTESIAN_POINT('Ctrl Pts',(-0.16430845139944,-1.5,-3.9579052940538));
#359869=CARTESIAN_POINT('Ctrl Pts',(9.88095885003532E-14,-1.5,-3.94999999999999));
#359870=CARTESIAN_POINT('Ctrl Pts',(1.96613558767211E-13,-1.5,-3.8875));
#359871=CARTESIAN_POINT('Ctrl Pts',(-0.138634473684809,-1.5,-3.89417005422507));
#359872=CARTESIAN_POINT('Ctrl Pts',(-0.276824301836837,-1.48078591559129,
-3.90135243999896));
#359873=CARTESIAN_POINT('Ctrl Pts',(-0.599047816188526,-1.38906927158903,
-3.91940311061709));
#359874=CARTESIAN_POINT('Ctrl Pts',(-0.775129142386704,-1.29905433022896,
-3.93037524241151));
#359875=CARTESIAN_POINT('Ctrl Pts',(-1.0850704461416,-1.0545952725511,-3.95207782972111));
#359876=CARTESIAN_POINT('Ctrl Pts',(-1.21512345799834,-0.901650532435833,
-3.96240830375363));
#359877=CARTESIAN_POINT('Ctrl Pts',(-1.40419865894282,-0.560954377034411,
-3.9813358679426));
#359878=CARTESIAN_POINT('Ctrl Pts',(-1.46410683422466,-0.377903713047335,
-3.99150534927522));
#359879=CARTESIAN_POINT('Ctrl Pts',(-1.51302559794633,0.00812305449483835,
-4.01295128080534));
#359880=CARTESIAN_POINT('Ctrl Pts',(-1.49870712012392,0.207835929291366,
-4.02404644051625));
#359881=CARTESIAN_POINT('Ctrl Pts',(-1.39430286120284,0.586210525188623,
-4.04506725139943));
#359882=CARTESIAN_POINT('Ctrl Pts',(-1.30678759085172,0.761592770298813,
-4.0541158407846));
#359883=CARTESIAN_POINT('Ctrl Pts',(-1.07041521160284,1.06840943409679,
-4.07401099728912));
#359884=CARTESIAN_POINT('Ctrl Pts',(-0.924144716585857,1.19717501877484,
-4.08462526155845));
#359885=CARTESIAN_POINT('Ctrl Pts',(-0.584243801589745,1.39605139479538,
-4.10650309573436));
#359886=CARTESIAN_POINT('Ctrl Pts',(-0.39235336545844,1.46163492695531,
-4.11755719342952));
#359887=CARTESIAN_POINT('Ctrl Pts',(-0.00444466178164925,1.51202609255691,
-4.13762021423696));
#359888=CARTESIAN_POINT('Ctrl Pts',(0.187267707385404,1.5003931503397,-4.14649900092975));
#359889=CARTESIAN_POINT('Ctrl Pts',(0.560989217050382,1.4047981157727,-4.16713510307386));
#359890=CARTESIAN_POINT('Ctrl Pts',(0.73898084414497,1.3198739653424,-4.17805773340386));
#359891=CARTESIAN_POINT('Ctrl Pts',(1.05510406697226,1.08455338950986,-4.19980390171558));
#359892=CARTESIAN_POINT('Ctrl Pts',(1.18939206035747,0.93534677759051,-4.21040946391861));
#359893=CARTESIAN_POINT('Ctrl Pts',(1.38764837771989,0.6005357697735,-4.22924838120778));
#359894=CARTESIAN_POINT('Ctrl Pts',(1.45260179965292,0.419773285277553,
-4.23917926192909));
#359895=CARTESIAN_POINT('Ctrl Pts',(1.51253535323791,0.0363127431133576,
-4.26048262538265));
#359896=CARTESIAN_POINT('Ctrl Pts',(1.50415187691205,-0.163133846561529,
-4.2715629914757));
#359897=CARTESIAN_POINT('Ctrl Pts',(1.41099361663282,-0.545336891269971,
-4.2927964939595));
#359898=CARTESIAN_POINT('Ctrl Pts',(1.32791096548009,-0.72452520745869,
-4.3020698874256));
#359899=CARTESIAN_POINT('Ctrl Pts',(1.09943657015848,-1.03842500385281,
-4.32178180568448));
#359900=CARTESIAN_POINT('Ctrl Pts',(0.957189594028571,-1.17083620866552,
-4.33230375553705));
#359901=CARTESIAN_POINT('Ctrl Pts',(0.623996435521955,-1.37865567349936,
-4.3541072817621));
#359902=CARTESIAN_POINT('Ctrl Pts',(0.434652990837125,-1.44953602151726,
-4.36518597104799));
#359903=CARTESIAN_POINT('Ctrl Pts',(0.158428898702364,-1.49372931639775,
-4.37970340040167));
#359904=CARTESIAN_POINT('Ctrl Pts',(0.0791936740651888,-1.5,-4.38368979258003));
#359905=CARTESIAN_POINT('Ctrl Pts',(3.2751579226442E-14,-1.5,-4.3875));
#359906=CARTESIAN_POINT('Origin',(0.,1.30104260698261E-15,-17.7));
#359907=CARTESIAN_POINT('',(-2.30626176757078E-16,-1.5,-4.95));
#359908=CARTESIAN_POINT('',(-1.78584683734892E-16,-1.5,-4.8875));
#359909=CARTESIAN_POINT('',(-1.83697019872103E-16,-1.5,-17.7));
#359910=CARTESIAN_POINT('Ctrl Pts',(-2.77555333642053E-16,-1.5,-4.95));
#359911=CARTESIAN_POINT('Ctrl Pts',(0.0824958291875462,-1.5,-4.94603091756763));
#359912=CARTESIAN_POINT('Ctrl Pts',(0.16502570294818,-1.49319553879669,
-4.9418711843537));
#359913=CARTESIAN_POINT('Ctrl Pts',(0.444096067626895,-1.44665240227896,
-4.92715154026959));
#359914=CARTESIAN_POINT('Ctrl Pts',(0.632848634143494,-1.37459550558921,
-4.91606859771527));
#359915=CARTESIAN_POINT('Ctrl Pts',(0.964504827724244,-1.16479808605149,
-4.89428407556348));
#359916=CARTESIAN_POINT('Ctrl Pts',(1.10583642355268,-1.03158532803245,
-4.88378390159935));
#359917=CARTESIAN_POINT('Ctrl Pts',(1.33252634451301,-0.716098755421027,
-4.86411376178606));
#359918=CARTESIAN_POINT('Ctrl Pts',(1.41460159353572,-0.536039844954454,
-4.85477999138629));
#359919=CARTESIAN_POINT('Ctrl Pts',(1.50520018725126,-0.152988353758026,
-4.83349935298649));
#359920=CARTESIAN_POINT('Ctrl Pts',(1.51224315648876,0.0463741466220205,
-4.82242365852093));
#359921=CARTESIAN_POINT('Ctrl Pts',(1.44982998827206,0.42920448401609,-4.80115530644348));
#359922=CARTESIAN_POINT('Ctrl Pts',(1.38374422633269,0.609450013770549,
-4.79131292474764));
#359923=CARTESIAN_POINT('Ctrl Pts',(1.18339834352113,0.94292020681763,-4.77241071804865));
#359924=CARTESIAN_POINT('Ctrl Pts',(1.04815459284978,1.09127271927741,-4.76178289693674));
#359925=CARTESIAN_POINT('Ctrl Pts',(0.730623388172348,1.32450073202695,
-4.74002711381898));
#359926=CARTESIAN_POINT('Ctrl Pts',(0.5522144858791,1.40825391101116,-4.72911693431124));
#359927=CARTESIAN_POINT('Ctrl Pts',(0.177928023099586,1.50154238307282,
-4.70851772202843));
#359928=CARTESIAN_POINT('Ctrl Pts',(-0.0139591409807751,1.51198141638455,
-4.69966120763815));
#359929=CARTESIAN_POINT('Ctrl Pts',(-0.401514993380857,1.45912695278427,
-4.67954673845126));
#359930=CARTESIAN_POINT('Ctrl Pts',(-0.592867515187272,1.39239251750419,
-4.66848655164));
#359931=CARTESIAN_POINT('Ctrl Pts',(-0.931339951890241,1.19156772223471,
-4.6466233224011));
#359932=CARTESIAN_POINT('Ctrl Pts',(-1.07674957092274,1.06200494067013,
-4.63602833268893));
#359933=CARTESIAN_POINT('Ctrl Pts',(-1.31142404779312,0.753657216867543,
-4.6161723371061));
#359934=CARTESIAN_POINT('Ctrl Pts',(-1.39798967723732,0.577463336149325,
-4.60708129645266));
#359935=CARTESIAN_POINT('Ctrl Pts',(-1.49998770387374,0.198255910766289,
-4.58601421726472));
#359936=CARTESIAN_POINT('Ctrl Pts',(-1.51303031281888,-0.00141426859624101,
-4.57492142952236));
#359937=CARTESIAN_POINT('Ctrl Pts',(-1.46174252827966,-0.386891834351265,
-4.55350600920264));
#359938=CARTESIAN_POINT('Ctrl Pts',(-1.40075443310616,-0.569462491014262,
-4.54336319494358));
#359939=CARTESIAN_POINT('Ctrl Pts',(-1.2097054101922,-0.908902260595766,
-4.52450542996683));
#359940=CARTESIAN_POINT('Ctrl Pts',(-1.07875028277293,-1.06105747797526,
-4.51409424501289));
#359941=CARTESIAN_POINT('Ctrl Pts',(-0.767453057130266,-1.30358685489508,
-4.49238002312433));
#359942=CARTESIAN_POINT('Ctrl Pts',(-0.59095150297832,-1.39251717571052,
-4.48141780145151));
#359943=CARTESIAN_POINT('Ctrl Pts',(-0.271091858127589,-1.48157818723245,
-4.46355463012667));
#359944=CARTESIAN_POINT('Ctrl Pts',(-0.1357462741014,-1.5,-4.45653109565784));
#359945=CARTESIAN_POINT('Ctrl Pts',(1.94948224230274E-13,-1.5,-4.44999999999999));
#359946=CARTESIAN_POINT('Ctrl Pts',(3.19883008970123E-14,-1.5,-4.3875));
#359947=CARTESIAN_POINT('Ctrl Pts',(-0.110913948001448,-1.5,-4.3928363498113));
#359948=CARTESIAN_POINT('Ctrl Pts',(-0.22171316120533,-1.48770112800956,
-4.39850881477519));
#359949=CARTESIAN_POINT('Ctrl Pts',(-0.520412566157265,-1.42025452881046,
-4.41475351324092));
#359950=CARTESIAN_POINT('Ctrl Pts',(-0.700262820478156,-1.34073678233728,
-4.42561538892734));
#359951=CARTESIAN_POINT('Ctrl Pts',(-1.02275295061583,-1.11512001893908,
-4.44739833486446));
#359952=CARTESIAN_POINT('Ctrl Pts',(-1.16139496410988,-0.969898058418966,
-4.45810269519655));
#359953=CARTESIAN_POINT('Ctrl Pts',(-1.36924497449003,-0.641294126202712,
-4.47723077048956));
#359954=CARTESIAN_POINT('Ctrl Pts',(-1.43939885340151,-0.462875501925603,
-4.48678469433752));
#359955=CARTESIAN_POINT('Ctrl Pts',(-1.51065089300875,-0.0823363359099725,
-4.50792575911617));
#359956=CARTESIAN_POINT('Ctrl Pts',(-1.50838929550509,0.116653856281524,
-4.51898076979347));
#359957=CARTESIAN_POINT('Ctrl Pts',(-1.42698523896123,0.502681634254046,
-4.54042675745861));
#359958=CARTESIAN_POINT('Ctrl Pts',(-1.34852730843035,0.685879509405817,
-4.55000449155034));
#359959=CARTESIAN_POINT('Ctrl Pts',(-1.12820822467234,1.00699066427407,
-4.56952435271185));
#359960=CARTESIAN_POINT('Ctrl Pts',(-0.990161090964451,1.1429983335144,
-4.57994413934133));
#359961=CARTESIAN_POINT('Ctrl Pts',(-0.664051435313271,1.359727791393,-4.60165436018314));
#359962=CARTESIAN_POINT('Ctrl Pts',(-0.477452246906336,1.43592323106179,
-4.61274865781205));
#359963=CARTESIAN_POINT('Ctrl Pts',(-0.0930687907855808,1.50933861512221,
-4.63328163169123));
#359964=CARTESIAN_POINT('Ctrl Pts',(0.10039406181527,1.50886913682122,-4.64208384663953));
#359965=CARTESIAN_POINT('Ctrl Pts',(0.479189862593641,1.43461329576912,
-4.66237133035325));
#359966=CARTESIAN_POINT('Ctrl Pts',(0.660746812570658,1.36056626338781,
-4.67316335519238));
#359967=CARTESIAN_POINT('Ctrl Pts',(0.989336327789165,1.14487714546879,
-4.69496399000104));
#359968=CARTESIAN_POINT('Ctrl Pts',(1.13223308767084,1.00379293970986,-4.7057581192819));
#359969=CARTESIAN_POINT('Ctrl Pts',(1.34966095067724,0.681520941085277,
-4.72517112218003));
#359970=CARTESIAN_POINT('Ctrl Pts',(1.4250185150892,0.505369135961604,-4.73442393689107));
#359971=CARTESIAN_POINT('Ctrl Pts',(1.50740755905354,0.12781366438924,-4.75539924086731));
#359972=CARTESIAN_POINT('Ctrl Pts',(1.51117028761309,-0.0705449898243242,
-4.7664191661014));
#359973=CARTESIAN_POINT('Ctrl Pts',(1.44150798589776,-0.460208330221321,
-4.78806712945679));
#359974=CARTESIAN_POINT('Ctrl Pts',(1.36767342503713,-0.647437735766871,
-4.79801549654008));
#359975=CARTESIAN_POINT('Ctrl Pts',(1.15540391526562,-0.97556578511997,
-4.81734298612827));
#359976=CARTESIAN_POINT('Ctrl Pts',(1.02153769413881,-1.11495558673436,
-4.82765556662891));
#359977=CARTESIAN_POINT('Ctrl Pts',(0.702557269234278,-1.34015190852106,
-4.84925797286061));
#359978=CARTESIAN_POINT('Ctrl Pts',(0.518771176498625,-1.42143586031683,
-4.86035827292002));
#359979=CARTESIAN_POINT('Ctrl Pts',(0.217682547012256,-1.48814623858313,
-4.87669747242329));
#359980=CARTESIAN_POINT('Ctrl Pts',(0.108887916867443,-1.5,-4.88226112765709));
#359981=CARTESIAN_POINT('Ctrl Pts',(5.20417042793042E-16,-1.5,-4.8875));
#359982=CARTESIAN_POINT('Origin',(0.,1.30104260698261E-15,-17.7));
#359983=CARTESIAN_POINT('',(-1.6606372482269E-14,-1.5,-5.45));
#359984=CARTESIAN_POINT('',(-1.15641779244756E-13,-1.5,-5.38750000000002));
#359985=CARTESIAN_POINT('',(-1.83697019872103E-16,-1.5,-17.7));
#359986=CARTESIAN_POINT('Ctrl Pts',(-3.49373308061729E-14,-1.5,-5.45));
#359987=CARTESIAN_POINT('Ctrl Pts',(0.112003054863257,-1.5,-5.44461125051039));
#359988=CARTESIAN_POINT('Ctrl Pts',(0.223888553312252,-1.48745840617422,
-5.43887977935007));
#359989=CARTESIAN_POINT('Ctrl Pts',(0.527484059848593,-1.41820836785807,
-5.42234942155599));
#359990=CARTESIAN_POINT('Ctrl Pts',(0.71065598432425,-1.33585682220828,
-5.41124901529594));
#359991=CARTESIAN_POINT('Ctrl Pts',(1.0280958134585,-1.1088922984854,-5.38967161429235));
#359992=CARTESIAN_POINT('Ctrl Pts',(1.16106421329996,-0.968800792091161,
-5.37938273843899));
#359993=CARTESIAN_POINT('Ctrl Pts',(1.37161220704221,-0.639185045545452,
-5.36009675040735));
#359994=CARTESIAN_POINT('Ctrl Pts',(1.44444942378393,-0.451084517844767,
-5.35006025099132));
#359995=CARTESIAN_POINT('Ctrl Pts',(1.51158275655079,-0.0606628262206041,
-5.3283701570122));
#359996=CARTESIAN_POINT('Ctrl Pts',(1.50653511735836,0.137537473385722,
-5.31735902925629));
#359997=CARTESIAN_POINT('Ctrl Pts',(1.42176877315086,0.51444241460095,-5.29641986585545));
#359998=CARTESIAN_POINT('Ctrl Pts',(1.34528814091645,0.690115321675696,
-5.28722200247804));
#359999=CARTESIAN_POINT('Ctrl Pts',(1.12579830690998,1.01100565571827,-5.26774817252563));
#360000=CARTESIAN_POINT('Ctrl Pts',(0.981998413662409,1.15117848208361,
-5.25693590731471));
#360001=CARTESIAN_POINT('Ctrl Pts',(0.652130702799262,1.36469994382362,
-5.23513398796106));
#360002=CARTESIAN_POINT('Ctrl Pts',(0.470226250634372,1.43756025114342,
-5.22435820850016));
#360003=CARTESIAN_POINT('Ctrl Pts',(0.0908983809121798,1.50949658439628,
-5.20410955637965));
#360004=CARTESIAN_POINT('Ctrl Pts',(-0.102771112168562,1.50873485121521,
-5.1952980573163));
#360005=CARTESIAN_POINT('Ctrl Pts',(-0.486735105734459,1.43278497407186,
-5.17471486225306));
#360006=CARTESIAN_POINT('Ctrl Pts',(-0.672716466221491,1.35544265410054,
-5.16361843209763));
#360007=CARTESIAN_POINT('Ctrl Pts',(-0.997249614247433,1.13679935361176,
-5.14193089871957));
#360008=CARTESIAN_POINT('Ctrl Pts',(-1.13436838857621,1.00002407254916,
-5.13153445525092));
#360009=CARTESIAN_POINT('Ctrl Pts',(-1.35289485609955,0.677341621182997,
-5.11205719425328));
#360010=CARTESIAN_POINT('Ctrl Pts',(-1.43032859685897,0.493252080276599,
-5.10240289334864));
#360011=CARTESIAN_POINT('Ctrl Pts',(-1.50912976100891,0.106402252737442,
-5.08091123626313));
#360012=CARTESIAN_POINT('Ctrl Pts',(-1.5100477769608,-0.0924628700686707,
-5.06986317388501));
#360013=CARTESIAN_POINT('Ctrl Pts',(-1.43631256065921,-0.47234599370819,
-5.04875855590504));
#360014=CARTESIAN_POINT('Ctrl Pts',(-1.36500630795286,-0.650255823971049,
-5.03927790150147));
#360015=CARTESIAN_POINT('Ctrl Pts',(-1.15503253800454,-0.977467677855987,
-5.02008631562113));
#360016=CARTESIAN_POINT('Ctrl Pts',(-1.01543885274056,-1.12178581026751,
-5.00936127429601));
#360017=CARTESIAN_POINT('Ctrl Pts',(-0.691573620226702,-1.34522157913518,
-4.98757275189638));
#360018=CARTESIAN_POINT('Ctrl Pts',(-0.511331921199436,-1.42353235932602,
-4.97672556965892));
#360019=CARTESIAN_POINT('Ctrl Pts',(-0.215424642031656,-1.48839116583224,
-4.96068709053796));
#360020=CARTESIAN_POINT('Ctrl Pts',(-0.10775705142673,-1.5,-4.95518446355402));
#360021=CARTESIAN_POINT('Ctrl Pts',(1.38777878078145E-16,-1.5,-4.95));
#360022=CARTESIAN_POINT('Ctrl Pts',(-1.73472347597681E-16,-1.5,-4.8875));
#360023=CARTESIAN_POINT('Ctrl Pts',(-0.0829656057906737,-1.5,-4.89149168456973));
#360024=CARTESIAN_POINT('Ctrl Pts',(-0.165966768441516,-1.49311782380902,
-4.8956762514306));
#360025=CARTESIAN_POINT('Ctrl Pts',(-0.439227699570691,-1.44727789145615,
-4.91009685556371));
#360026=CARTESIAN_POINT('Ctrl Pts',(-0.622270263803716,-1.37851388291316,
-4.92081360638988));
#360027=CARTESIAN_POINT('Ctrl Pts',(-0.956428468696735,-1.17251273596787,
-4.9426130546006));
#360028=CARTESIAN_POINT('Ctrl Pts',(-1.10329198121541,-1.03552308732051,
-4.95348429665915));
#360029=CARTESIAN_POINT('Ctrl Pts',(-1.32985979386102,-0.719427485276971,
-4.97316547901764));
#360030=CARTESIAN_POINT('Ctrl Pts',(-1.41020596056088,-0.545375198674591,
-4.98220137785146));
#360031=CARTESIAN_POINT('Ctrl Pts',(-1.50308025472817,-0.170724223102751,
-5.00301532093878));
#360032=CARTESIAN_POINT('Ctrl Pts',(-1.51250478259511,0.0268736369112289,
-5.01399297982845));
#360033=CARTESIAN_POINT('Ctrl Pts',(-1.4544187016606,0.417393905079721,
-5.03568855028225));
#360034=CARTESIAN_POINT('Ctrl Pts',(-1.38634030608345,0.606270546843181,
-5.04597385278133));
#360035=CARTESIAN_POINT('Ctrl Pts',(-1.1846371610216,0.939735762001864,
-5.06494122251611));
#360036=CARTESIAN_POINT('Ctrl Pts',(-1.05551747552987,1.08274092934074,
-5.07512586204022));
#360037=CARTESIAN_POINT('Ctrl Pts',(-0.744718802559787,1.31709337644969,
-5.09658896036294));
#360038=CARTESIAN_POINT('Ctrl Pts',(-0.564218319239696,1.40392501056514,
-5.10768528375229));
#360039=CARTESIAN_POINT('Ctrl Pts',(-0.184060619143443,1.50125952084737,
-5.12867936602277));
#360040=CARTESIAN_POINT('Ctrl Pts',(0.0114524548753373,1.51245558484093,
-5.13770501802434));
#360041=CARTESIAN_POINT('Ctrl Pts',(0.395073662217544,1.45987301241593,
-5.15762262897996));
#360042=CARTESIAN_POINT('Ctrl Pts',(0.579570311002179,1.39692338827322,
-5.16824782880396));
#360043=CARTESIAN_POINT('Ctrl Pts',(0.921186075424326,1.20072738827768,
-5.19013371382177));
#360044=CARTESIAN_POINT('Ctrl Pts',(1.07350611906356,1.06673918590758,-5.20118410984856));
#360045=CARTESIAN_POINT('Ctrl Pts',(1.30997188084597,0.755112591702573,
-5.22121736840029));
#360046=CARTESIAN_POINT('Ctrl Pts',(1.39510822563865,0.583010368031759,
-5.23011053510939));
#360047=CARTESIAN_POINT('Ctrl Pts',(1.49786420173597,0.2111788391675,-5.25076784226851));
#360048=CARTESIAN_POINT('Ctrl Pts',(1.51260656519268,0.0144454872595902,
-5.26169747293006));
#360049=CARTESIAN_POINT('Ctrl Pts',(1.46542190804958,-0.37687821172446,
-5.28343767842918));
#360050=CARTESIAN_POINT('Ctrl Pts',(1.40264741672388,-0.567543360101546,
-5.29403018667235));
#360051=CARTESIAN_POINT('Ctrl Pts',(1.21054777309602,-0.905983865282138,
-5.31283243696015));
#360052=CARTESIAN_POINT('Ctrl Pts',(1.08589197369939,-1.05219972926723,
-5.32281610164694));
#360053=CARTESIAN_POINT('Ctrl Pts',(0.7827393931996,-1.2947706165297,-5.34413961717843));
#360054=CARTESIAN_POINT('Ctrl Pts',(0.605394774261556,-1.38658325786445,
-5.35522246528355));
#360055=CARTESIAN_POINT('Ctrl Pts',(0.280057864526816,-1.48033499714547,
-5.37347945963131));
#360056=CARTESIAN_POINT('Ctrl Pts',(0.140251536173992,-1.50000000000002,
-5.38075214481965));
#360057=CARTESIAN_POINT('Ctrl Pts',(-2.30961083591552E-13,-1.5,-5.38750000000002));
#360058=CARTESIAN_POINT('Origin',(0.,1.30104260698261E-15,-17.7));
#360059=CARTESIAN_POINT('',(-1.1555473864945E-13,-1.5,-5.95000000000001));
#360060=CARTESIAN_POINT('',(-4.9687592688114E-14,-1.5,-5.88750000000001));
#360061=CARTESIAN_POINT('',(-1.83697019872103E-16,-1.5,-17.7));
#360062=CARTESIAN_POINT('Ctrl Pts',(-2.30475361018279E-13,-1.5,-5.95000000000001));
#360063=CARTESIAN_POINT('Ctrl Pts',(0.143779545010459,-1.50000000000002,
-5.94308240341535));
#360064=CARTESIAN_POINT('Ctrl Pts',(0.287058207428915,-1.47933314649523,
-5.93561482629158));
#360065=CARTESIAN_POINT('Ctrl Pts',(0.614977937901949,-1.3823400805608,
-5.91714352907164));
#360066=CARTESIAN_POINT('Ctrl Pts',(0.791562999441172,-1.28937447526274,
-5.90606519841215));
#360067=CARTESIAN_POINT('Ctrl Pts',(1.09288206406366,-1.04491758451658,
-5.88477750896878));
#360068=CARTESIAN_POINT('Ctrl Pts',(1.21649528049569,-0.897961460651119,
-5.8748867478139));
#360069=CARTESIAN_POINT('Ctrl Pts',(1.40633352386383,-0.558349785555567,
-5.85601943253082));
#360070=CARTESIAN_POINT('Ctrl Pts',(1.46786090845376,-0.367269115374562,
-5.84540383974299));
#360071=CARTESIAN_POINT('Ctrl Pts',(1.5124652514401,0.0242414874161168,
-5.82365325069906));
#360072=CARTESIAN_POINT('Ctrl Pts',(1.49646765222344,0.220749313774995,
-5.81273614923468));
#360073=CARTESIAN_POINT('Ctrl Pts',(1.39137263960931,0.591902024894406,
-5.79211655417249));
#360074=CARTESIAN_POINT('Ctrl Pts',(1.30508888504187,0.763546397778705,
-5.78324816276405));
#360075=CARTESIAN_POINT('Ctrl Pts',(1.06661784566857,1.07360181688628,-5.76316206900194));
#360076=CARTESIAN_POINT('Ctrl Pts',(0.913548925461279,1.20652625226537,
-5.75210519171755));
#360077=CARTESIAN_POINT('Ctrl Pts',(0.570929032520845,1.40046132775147,
-5.73023379900248));
#360078=CARTESIAN_POINT('Ctrl Pts',(0.386162258818603,1.46224032027028,
-5.71962812033243));
#360079=CARTESIAN_POINT('Ctrl Pts',(0.0020511110498958,1.51253564557089,
-5.69975047174939));
#360080=CARTESIAN_POINT('Ctrl Pts',(-0.193693773628809,1.50008576426874,
-5.69068328631201));
#360081=CARTESIAN_POINT('Ctrl Pts',(-0.57336323662806,1.40019673354727,
-5.66964173545871));
#360082=CARTESIAN_POINT('Ctrl Pts',(-0.753177752293143,1.31225510532934,
-5.65854758253404));
#360083=CARTESIAN_POINT('Ctrl Pts',(-1.06228592207914,1.07608047106221,
-5.63711520227373));
#360084=CARTESIAN_POINT('Ctrl Pts',(-1.19043130071785,0.932361348999917,
-5.6269576070343));
#360085=CARTESIAN_POINT('Ctrl Pts',(-1.39001769707367,0.597784099544736,
-5.60806118957755));
#360086=CARTESIAN_POINT('Ctrl Pts',(-1.45693782306663,0.408508818217555,
-5.59769493434537));
#360087=CARTESIAN_POINT('Ctrl Pts',(-1.51262413695321,0.017766922124366,
-5.57598705122908));
#360088=CARTESIAN_POINT('Ctrl Pts',(-1.50202431525068,-0.179652463492326,
-5.56501930758371));
#360089=CARTESIAN_POINT('Ctrl Pts',(-1.40696945108533,-0.553688053995312,
-5.54423955255577));
#360090=CARTESIAN_POINT('Ctrl Pts',(-1.32557396250141,-0.727307733847383,
-5.53524038106649));
#360091=CARTESIAN_POINT('Ctrl Pts',(-1.09709073135385,-1.04209159986641,
-5.51550348020415));
#360092=CARTESIAN_POINT('Ctrl Pts',(-0.949408156168324,-1.17820536526802,
-5.50461716106483));
#360093=CARTESIAN_POINT('Ctrl Pts',(-0.614115170311688,-1.38215057165094,
-5.48282022513961));
#360094=CARTESIAN_POINT('Ctrl Pts',(-0.430779341403753,-1.44980022913289,
-5.47212031880633));
#360095=CARTESIAN_POINT('Ctrl Pts',(-0.160222428209957,-1.49358660537016,
-5.45788685502222));
#360096=CARTESIAN_POINT('Ctrl Pts',(-0.0800898247096889,-1.5,-5.45385332348796));
#360097=CARTESIAN_POINT('Ctrl Pts',(-3.30290479446659E-14,-1.5,-5.45));
#360098=CARTESIAN_POINT('Ctrl Pts',(-2.31099861469641E-13,-1.5,-5.38750000000002));
#360099=CARTESIAN_POINT('Ctrl Pts',(-0.0544776219942335,-1.49999999999999,
-5.39012105581027));
#360100=CARTESIAN_POINT('Ctrl Pts',(-0.109014443643155,-1.49703241159562,
-5.39282739287651));
#360101=CARTESIAN_POINT('Ctrl Pts',(-0.354873801016226,-1.47009450804401,
-5.40540458182202));
#360102=CARTESIAN_POINT('Ctrl Pts',(-0.540528018569387,-1.41241816543501,
-5.41593899515675));
#360103=CARTESIAN_POINT('Ctrl Pts',(-0.886546361924947,-1.22642949223115,
-5.43775316249693));
#360104=CARTESIAN_POINT('Ctrl Pts',(-1.0421788809374,-1.09725665011376,
-5.4488291700624));
#360105=CARTESIAN_POINT('Ctrl Pts',(-1.28763428030429,-0.792732570084186,
-5.46909765069365));
#360106=CARTESIAN_POINT('Ctrl Pts',(-1.37793947069467,-0.622665885247676,
-5.47790745081961));
#360107=CARTESIAN_POINT('Ctrl Pts',(-1.49114532153187,-0.253900482485394,
-5.49839441763973));
#360108=CARTESIAN_POINT('Ctrl Pts',(-1.51148259208429,-0.0582363393241967,
-5.50926464781536));
#360109=CARTESIAN_POINT('Ctrl Pts',(-1.47583816671478,0.333790424102859,
-5.53104391245019));
#360110=CARTESIAN_POINT('Ctrl Pts',(-1.41866188921323,0.526248347454362,
-5.54173601930305));
#360111=CARTESIAN_POINT('Ctrl Pts',(-1.23668878520016,0.869885949917901,
-5.56082699721769));
#360112=CARTESIAN_POINT('Ctrl Pts',(-1.11665679439315,1.01941802933088,
-5.57042532574517));
#360113=CARTESIAN_POINT('Ctrl Pts',(-0.821671034046308,1.2703276538985,
-5.59158754655066));
#360114=CARTESIAN_POINT('Ctrl Pts',(-0.647757502348754,1.36721878187072,
-5.60264638546722));
#360115=CARTESIAN_POINT('Ctrl Pts',(-0.272405721158414,1.48817955152494,
-5.62406552783909));
#360116=CARTESIAN_POINT('Ctrl Pts',(-0.074673845245232,1.51105565975916,
-5.63360015128558));
#360117=CARTESIAN_POINT('Ctrl Pts',(0.313302899921245,1.47944286236704,
-5.65314482440157));
#360118=CARTESIAN_POINT('Ctrl Pts',(0.499991719515697,1.42719956174785,
-5.66357809721717));
#360119=CARTESIAN_POINT('Ctrl Pts',(0.850224187064647,1.25178798296355,
-5.68530120852382));
#360120=CARTESIAN_POINT('Ctrl Pts',(1.00910707112899,1.12763903021001,-5.69639404686843));
#360121=CARTESIAN_POINT('Ctrl Pts',(1.26371524628725,0.830508905492942,
-5.7168975029827));
#360122=CARTESIAN_POINT('Ctrl Pts',(1.35935615291476,0.662474592684624,
-5.725695855962));
#360123=CARTESIAN_POINT('Ctrl Pts',(1.48311189740595,0.296891183797457,
-5.74600604534461));
#360124=CARTESIAN_POINT('Ctrl Pts',(1.50905759985487,0.102466567398649,
-5.75680741292233));
#360125=CARTESIAN_POINT('Ctrl Pts',(1.48508337510517,-0.289923734161056,
-5.77860687412009));
#360126=CARTESIAN_POINT('Ctrl Pts',(1.4336222203805,-0.484022734140751,
-5.78939015189674));
#360127=CARTESIAN_POINT('Ctrl Pts',(1.26193465712244,-0.832812097053497,
-5.80876733872522));
#360128=CARTESIAN_POINT('Ctrl Pts',(1.14648703796586,-0.985720116124361,
-5.81805406433748));
#360129=CARTESIAN_POINT('Ctrl Pts',(0.859679290268612,-1.24482706900436,
-5.83905052389015));
#360130=CARTESIAN_POINT('Ctrl Pts',(0.689321243795664,-1.34665430569042,
-5.85007541357502));
#360131=CARTESIAN_POINT('Ctrl Pts',(0.342146130245309,-1.47055648458404,
-5.8702206112052));
#360132=CARTESIAN_POINT('Ctrl Pts',(0.171606945087988,-1.50000000000001,
-5.87924355700489));
#360133=CARTESIAN_POINT('Ctrl Pts',(-9.70404312461426E-14,-1.5,-5.88750000000001));
#360134=CARTESIAN_POINT('Origin',(0.,1.30104260698261E-15,-17.7));
#360135=CARTESIAN_POINT('',(-4.96354202156783E-14,-1.5,-6.45));
#360136=CARTESIAN_POINT('',(-1.14379898485726E-8,-1.5,-6.38750000110063));
#360137=CARTESIAN_POINT('',(-1.83697019872103E-16,-1.5,-17.7));
#360138=CARTESIAN_POINT('Ctrl Pts',(-9.71098201851817E-14,-1.5,-6.45));
#360139=CARTESIAN_POINT('Ctrl Pts',(0.175083992004288,-1.50000000000001,
-6.44157626750713));
#360140=CARTESIAN_POINT('Ctrl Pts',(0.349012600883344,-1.46935064435116,
-6.43235675242051));
#360141=CARTESIAN_POINT('Ctrl Pts',(0.698448698264349,-1.34192367911046,
-6.4120048624232));
#360142=CARTESIAN_POINT('Ctrl Pts',(0.868000054047873,-1.23901878590965,
-6.40098884975903));
#360143=CARTESIAN_POINT('Ctrl Pts',(1.15298812289309,-0.978107547609196,
-6.3800298205065));
#360144=CARTESIAN_POINT('Ctrl Pts',(1.26742086259517,-0.824439858150199,
-6.37080221434165));
#360145=CARTESIAN_POINT('Ctrl Pts',(1.43679909501675,-0.474511758410586,
-6.35136176435611));
#360146=CARTESIAN_POINT('Ctrl Pts',(1.48697426927758,-0.280069300941365,
-6.34055940560782));
#360147=CARTESIAN_POINT('Ctrl Pts',(1.50833762378054,0.112354555701641,
-6.31875808023877));
#360148=CARTESIAN_POINT('Ctrl Pts',(1.48114395458428,0.306480120986939,
-6.30797332661181));
#360149=CARTESIAN_POINT('Ctrl Pts',(1.35502834861227,0.671340068733185,
-6.28770332951479));
#360150=CARTESIAN_POINT('Ctrl Pts',(1.25817688371938,0.83892209174003,-6.27889733877137));
#360151=CARTESIAN_POINT('Ctrl Pts',(1.00151140779071,1.13436656063906,-6.25834172450036));
#360152=CARTESIAN_POINT('Ctrl Pts',(0.841915584426592,1.25736979765705,
-6.2472464102848));
#360153=CARTESIAN_POINT('Ctrl Pts',(0.490774324217669,1.43037919615442,
-6.2255463019011));
#360154=CARTESIAN_POINT('Ctrl Pts',(0.303873417810742,1.48139293571001,
-6.21513697952796));
#360155=CARTESIAN_POINT('Ctrl Pts',(-0.0845860546829974,1.51058699485786,
-6.19563626835606));
#360156=CARTESIAN_POINT('Ctrl Pts',(-0.282585859991757,1.48633548906874,
-6.18602451172392));
#360157=CARTESIAN_POINT('Ctrl Pts',(-0.657333674027615,1.36262073996644,
-6.16455792830621));
#360158=CARTESIAN_POINT('Ctrl Pts',(-0.830444938790861,1.26458819942875,
-6.15350598257092));
#360159=CARTESIAN_POINT('Ctrl Pts',(-1.123561669514,1.01179206850437,-6.13238128254078));
#360160=CARTESIAN_POINT('Ctrl Pts',(-1.24254226875119,0.861493674918274,
-6.12286075971764));
#360161=CARTESIAN_POINT('Ctrl Pts',(-1.42217784205403,0.516673906685671,
-6.10370410592694));
#360162=CARTESIAN_POINT('Ctrl Pts',(-1.47805742018399,0.323827072437385,
-6.09299039291315));
#360163=CARTESIAN_POINT('Ctrl Pts',(-1.51104430075671,-0.0683131724668348,
-6.0712048237518));
#360164=CARTESIAN_POINT('Ctrl Pts',(-1.4894255194257,-0.263709025874027,
-6.06034949856251));
#360165=CARTESIAN_POINT('Ctrl Pts',(-1.3738163973829,-0.631757166629868,
-6.03990237963163));
#360166=CARTESIAN_POINT('Ctrl Pts',(-1.28230645468386,-0.801359093595513,
-6.0311016899108));
#360167=CARTESIAN_POINT('Ctrl Pts',(-1.03477263294274,-1.10421895362498,
-6.01077943946978));
#360168=CARTESIAN_POINT('Ctrl Pts',(-0.878390960016799,-1.23226158064842,
-5.99969878308356));
#360169=CARTESIAN_POINT('Ctrl Pts',(-0.531391503965922,-1.41586444003544,
-5.97790368454285));
#360170=CARTESIAN_POINT('Ctrl Pts',(-0.345489435132126,-1.47231253454326,
-5.96739146446062));
#360171=CARTESIAN_POINT('Ctrl Pts',(-0.102728496078983,-1.49736480502456,
-5.95501572693244));
#360172=CARTESIAN_POINT('Ctrl Pts',(-0.051335855383024,-1.49999999999999,
-5.9524698974937));
#360173=CARTESIAN_POINT('Ctrl Pts',(-2.30925780279027E-13,-1.5,-5.95000000000001));
#360174=CARTESIAN_POINT('Ctrl Pts',(-9.9191488356356E-14,-1.5,-5.88750000000001));
#360175=CARTESIAN_POINT('Ctrl Pts',(-0.0269718101574132,-1.5,-5.88879768182125));
#360176=CARTESIAN_POINT('Ctrl Pts',(-0.0539680776807263,-1.49927253331153,
-5.89011674775609));
#360177=CARTESIAN_POINT('Ctrl Pts',(-0.272282822061387,-1.48747218509173,
-5.900948208243));
#360178=CARTESIAN_POINT('Ctrl Pts',(-0.459834248908589,-1.44057020960743,
-5.91127461312677));
#360179=CARTESIAN_POINT('Ctrl Pts',(-0.813895030288931,-1.27561647138715,
-5.93289141869728));
#360180=CARTESIAN_POINT('Ctrl Pts',(-0.975814709361218,-1.15646792700745,
-5.94399146467723));
#360181=CARTESIAN_POINT('Ctrl Pts',(-1.23932740362783,-0.866694814313302,
-5.96471897822176));
#360182=CARTESIAN_POINT('Ctrl Pts',(-1.34023526021138,-0.700614022507633,
-5.9735769987496));
#360183=CARTESIAN_POINT('Ctrl Pts',(-1.4741757383099,-0.338179606973961,
-5.99371224405703));
#360184=CARTESIAN_POINT('Ctrl Pts',(-1.5054872376406,-0.145101799609199,
-6.00443878891062));
#360185=CARTESIAN_POINT('Ctrl Pts',(-1.49277552777813,0.2473083510385,-6.0262393528355));
#360186=CARTESIAN_POINT('Ctrl Pts',(-1.44688097502016,0.442826888870478,
-6.03710149382616));
#360187=CARTESIAN_POINT('Ctrl Pts',(-1.28518148216548,0.796493179373089,
-6.05674962107631));
#360188=CARTESIAN_POINT('Ctrl Pts',(-1.17408797917394,0.952692543573725,
-6.0658086808636));
#360189=CARTESIAN_POINT('Ctrl Pts',(-0.895106809654988,1.21951117217202,
-6.08664279721249));
#360190=CARTESIAN_POINT('Ctrl Pts',(-0.728256791418487,1.32591928233535,
-6.09762615329562));
#360191=CARTESIAN_POINT('Ctrl Pts',(-0.360421700012662,1.46957484044234,
-6.11931405955197));
#360192=CARTESIAN_POINT('Ctrl Pts',(-0.162675208069435,1.50434210548157,
-6.12955267136142));
#360193=CARTESIAN_POINT('Ctrl Pts',(0.227015314260759,1.49497783819363,
-6.14856178389453));
#360194=CARTESIAN_POINT('Ctrl Pts',(0.415339942011079,1.45394779639172,
-6.15876228015514));
#360195=CARTESIAN_POINT('Ctrl Pts',(0.77325279948223,1.30055810332152,-6.1802431953466));
#360196=CARTESIAN_POINT('Ctrl Pts',(0.938331290737864,1.18697628345601,
-6.19134058851207));
#360197=CARTESIAN_POINT('Ctrl Pts',(1.21153599193554,0.905412640553713,
-6.21230636812995));
#360198=CARTESIAN_POINT('Ctrl Pts',(1.31827759787906,0.741438308234929,
-6.22130898287587));
#360199=CARTESIAN_POINT('Ctrl Pts',(1.4632278868835,0.382495696924617,-6.24125023905977));
#360200=CARTESIAN_POINT('Ctrl Pts',(1.50027611261485,0.191036499153384,
-6.25188686115817));
#360201=CARTESIAN_POINT('Ctrl Pts',(1.49970970905734,-0.203057380420697,
-6.27378096557895));
#360202=CARTESIAN_POINT('Ctrl Pts',(1.45906238606611,-0.401891328845657,
-6.28482729604701));
#360203=CARTESIAN_POINT('Ctrl Pts',(1.30601490646584,-0.76192210186722,
-6.30482900565931));
#360204=CARTESIAN_POINT('Ctrl Pts',(1.19896038848152,-0.921249982630647,
-6.3137386020422));
#360205=CARTESIAN_POINT('Ctrl Pts',(0.927276772408091,-1.19514856435085,
-6.33441828005174));
#360206=CARTESIAN_POINT('Ctrl Pts',(0.763784138561927,-1.30569906008895,
-6.34535517016904));
#360207=CARTESIAN_POINT('Ctrl Pts',(0.400630272163701,-1.4591064707294,
-6.3670887356748));
#360208=CARTESIAN_POINT('Ctrl Pts',(0.20396914448713,-1.49930646016053,
-6.37766726496482));
#360209=CARTESIAN_POINT('Ctrl Pts',(0.00344368467581672,-1.49999703548051,
-6.38733423329604));
#360210=CARTESIAN_POINT('Ctrl Pts',(0.00172177422024196,-1.50000000001316,
-6.38741716109958));
#360211=CARTESIAN_POINT('Ctrl Pts',(-1.14645005182519E-8,-1.5,-6.38750000055159));
#360212=CARTESIAN_POINT('Origin',(0.,1.30104260698261E-15,-17.7));
#360213=CARTESIAN_POINT('',(-2.30626176757078E-16,-1.5,-6.95));
#360214=CARTESIAN_POINT('',(6.57929491076618E-14,-1.5,-6.8875));
#360215=CARTESIAN_POINT('',(-1.83697019872103E-16,-1.5,-17.7));
#360216=CARTESIAN_POINT('Ctrl Pts',(-2.77555333642053E-16,-1.5,-6.95));
#360217=CARTESIAN_POINT('Ctrl Pts',(0.00515159578593097,-1.5,-6.94975214373219));
#360218=CARTESIAN_POINT('Ctrl Pts',(0.010304272039539,-1.49997346107028,
-6.94950349828783));
#360219=CARTESIAN_POINT('Ctrl Pts',(0.214260531892348,-1.49787153589899,
-6.93963226135011));
#360220=CARTESIAN_POINT('Ctrl Pts',(0.410650232159253,-1.45631954863341,
-6.92902923562202));
#360221=CARTESIAN_POINT('Ctrl Pts',(0.772629447971819,-1.30046493189594,
-6.90728420757178));
#360222=CARTESIAN_POINT('Ctrl Pts',(0.935262174360835,-1.18888880266618,
-6.89636019995208));
#360223=CARTESIAN_POINT('Ctrl Pts',(1.20510378879389,-0.91321930699475,
-6.87571995323359));
#360224=CARTESIAN_POINT('Ctrl Pts',(1.31114101911631,-0.753092043636084,
-6.86683844686865));
#360225=CARTESIAN_POINT('Ctrl Pts',(1.46171506667493,-0.392062181413054,
-6.8467812323007));
#360226=CARTESIAN_POINT('Ctrl Pts',(1.50100567367457,-0.193101237105326,
-6.83572784650583));
#360227=CARTESIAN_POINT('Ctrl Pts',(1.49899449390294,0.200728458918543,
-6.81384841894895));
#360228=CARTESIAN_POINT('Ctrl Pts',(1.46074172941662,0.391823837709976,
-6.80323200901609));
#360229=CARTESIAN_POINT('Ctrl Pts',(1.31346150399244,0.750015710321186,
-6.78333246053769));
#360230=CARTESIAN_POINT('Ctrl Pts',(1.20546573420867,0.913544113679387,
-6.77428843846535));
#360231=CARTESIAN_POINT('Ctrl Pts',(0.930202151523462,1.19333499796725,
-6.75327284416057));
#360232=CARTESIAN_POINT('Ctrl Pts',(0.76447291305119,1.30571788673004,-6.74217744554678));
#360233=CARTESIAN_POINT('Ctrl Pts',(0.405785068228597,1.45662740857059,
-6.72072813740426));
#360234=CARTESIAN_POINT('Ctrl Pts',(0.217318862830531,1.49640270302223,
-6.71055568357896));
#360235=CARTESIAN_POINT('Ctrl Pts',(-0.172280751492315,1.50326942561258,
-6.69162032110099));
#360236=CARTESIAN_POINT('Ctrl Pts',(-0.369786999912835,1.46724472857059,
-6.68129874602062));
#360237=CARTESIAN_POINT('Ctrl Pts',(-0.736576190809934,1.3212977908628,
-6.6595975112426));
#360238=CARTESIAN_POINT('Ctrl Pts',(-0.90265365361906,1.21391640988091,
-6.64862428944928));
#360239=CARTESIAN_POINT('Ctrl Pts',(-1.17993993444525,0.945444154140981,
-6.62782578438337));
#360240=CARTESIAN_POINT('Ctrl Pts',(-1.29009387847771,0.788523511290764,
-6.61880686173835));
#360241=CARTESIAN_POINT('Ctrl Pts',(-1.44961106078853,0.433808503038918,
-6.59910047239102));
#360242=CARTESIAN_POINT('Ctrl Pts',(-1.49428821956553,0.238002628385505,
-6.58822236824361));
#360243=CARTESIAN_POINT('Ctrl Pts',(-1.50455029243796,-0.154368756750338,
-6.56642395795829));
#360244=CARTESIAN_POINT('Ctrl Pts',(-1.4720777523692,-0.34713404641117,
-6.55571477519935));
#360245=CARTESIAN_POINT('Ctrl Pts',(-1.33591987514471,-0.708872612955237,
-6.53561818816913));
#360246=CARTESIAN_POINT('Ctrl Pts',(-1.23384917159286,-0.874528906852802,
-6.52673779297838));
#360247=CARTESIAN_POINT('Ctrl Pts',(-0.968389679515266,-1.16267051032679,
-6.50596193378105));
#360248=CARTESIAN_POINT('Ctrl Pts',(-0.805823049353649,-1.28071119538738,
-6.49486153522228));
#360249=CARTESIAN_POINT('Ctrl Pts',(-0.450961842860782,-1.44335706912135,
-6.47327032652743));
#360250=CARTESIAN_POINT('Ctrl Pts',(-0.263241103996375,-1.48908431124072,
-6.46296840709779));
#360251=CARTESIAN_POINT('Ctrl Pts',(-0.0479753228231705,-1.49942508266729,
-6.45232418372142));
#360252=CARTESIAN_POINT('Ctrl Pts',(-0.0239775839369867,-1.5,-6.45115362204504));
#360253=CARTESIAN_POINT('Ctrl Pts',(-9.90871434114846E-14,-1.5,-6.45));
#360254=CARTESIAN_POINT('Ctrl Pts',(-1.14645056295548E-8,-1.5,-6.38750000055159));
#360255=CARTESIAN_POINT('Ctrl Pts',(-0.188662808098288,-1.49999999855805,
-6.39657704362686));
#360256=CARTESIAN_POINT('Ctrl Pts',(-0.375732974423939,-1.46440555920762,
-6.40656619562707));
#360257=CARTESIAN_POINT('Ctrl Pts',(-0.735347843155412,-1.32227358290303,
-6.42781628451887));
#360258=CARTESIAN_POINT('Ctrl Pts',(-0.903158276318748,-1.21385890059538,
-6.43890158670183));
#360259=CARTESIAN_POINT('Ctrl Pts',(-1.18516837418757,-0.939951322299202,
-6.46007834770329));
#360260=CARTESIAN_POINT('Ctrl Pts',(-1.29731274704456,-0.777883541388106,
-6.46928424770068));
#360261=CARTESIAN_POINT('Ctrl Pts',(-1.45220861002616,-0.422174255720655,
-6.48904587468221));
#360262=CARTESIAN_POINT('Ctrl Pts',(-1.4943732657924,-0.232318949561423,
-6.49959339169105));
#360263=CARTESIAN_POINT('Ctrl Pts',(-1.50477749816427,0.160533971298007,
-6.52141855396102));
#360264=CARTESIAN_POINT('Ctrl Pts',(-1.46991553600497,0.359847718473458,
-6.53249153991521));
#360265=CARTESIAN_POINT('Ctrl Pts',(-1.32743228933234,0.724097389575991,
-6.55272763275424));
#360266=CARTESIAN_POINT('Ctrl Pts',(-1.2246997029697,0.886852632687246,
-6.56154473675361));
#360267=CARTESIAN_POINT('Ctrl Pts',(-0.960848483996669,1.16823777752605,
-6.58205553846858));
#360268=CARTESIAN_POINT('Ctrl Pts',(-0.801045091118743,1.28309300914337,
-6.59293450589369));
#360269=CARTESIAN_POINT('Ctrl Pts',(-0.442985771522919,1.44681577111778,
-6.61470949743918));
#360270=CARTESIAN_POINT('Ctrl Pts',(-0.247541356316228,1.49273587299906,
-6.62538837963571));
#360271=CARTESIAN_POINT('Ctrl Pts',(0.141128398861992,1.50538917073519,
-6.64443974244321));
#360272=CARTESIAN_POINT('Ctrl Pts',(0.33056170368414,1.47542526933006,-6.65408678879133));
#360273=CARTESIAN_POINT('Ctrl Pts',(0.694924367490722,1.34387056049742,
-6.67527149309486));
#360274=CARTESIAN_POINT('Ctrl Pts',(0.865432912391379,1.24094139575771,
-6.68633423275131));
#360275=CARTESIAN_POINT('Ctrl Pts',(1.1566065168039,0.975216686342843,-6.70772457125354));
#360276=CARTESIAN_POINT('Ctrl Pts',(1.27448706127016,0.815139456408861,
-6.71721447464397));
#360277=CARTESIAN_POINT('Ctrl Pts',(1.4396870268363,0.462859443663064,-6.73678558646318));
#360278=CARTESIAN_POINT('Ctrl Pts',(1.48707811155273,0.274803502370941,
-6.74723313875718));
#360279=CARTESIAN_POINT('Ctrl Pts',(1.50874950767428,-0.116454945609269,
-6.76896971920053));
#360280=CARTESIAN_POINT('Ctrl Pts',(1.47985938284906,-0.316094836591576,
-6.7800608242551));
#360281=CARTESIAN_POINT('Ctrl Pts',(1.34833870965213,-0.684586646548388,
-6.80053259147493));
#360282=CARTESIAN_POINT('Ctrl Pts',(1.25003415541057,-0.850935687480155,
-6.80932813941981));
#360283=CARTESIAN_POINT('Ctrl Pts',(0.994214333933481,-1.13988251133932,
-6.82966257698205));
#360284=CARTESIAN_POINT('Ctrl Pts',(0.838278058707002,-1.25899700110724,
-6.84047380034881));
#360285=CARTESIAN_POINT('Ctrl Pts',(0.485704654348464,-1.43304486849454,
-6.86227165915808));
#360286=CARTESIAN_POINT('Ctrl Pts',(0.291674266058639,-1.4847475596941,
-6.87304313643391));
#360287=CARTESIAN_POINT('Ctrl Pts',(0.0621266763099901,-1.49903597661885,
-6.88448415046514));
#360288=CARTESIAN_POINT('Ctrl Pts',(0.0310490691749192,-1.5,-6.88600615096282));
#360289=CARTESIAN_POINT('Ctrl Pts',(1.31769595235196E-13,-1.5,-6.8875));
#360290=CARTESIAN_POINT('Origin',(0.,1.30104260698261E-15,-17.7));
#360291=CARTESIAN_POINT('',(8.22032160180837E-14,-1.5,-7.44999999999999));
#360292=CARTESIAN_POINT('',(8.22728221294406E-14,-1.5,-7.3875));
#360293=CARTESIAN_POINT('',(-1.83697019872103E-16,-1.5,-17.7));
#360294=CARTESIAN_POINT('Ctrl Pts',(1.6459012905604E-13,-1.5,-7.44999999999999));
#360295=CARTESIAN_POINT('Ctrl Pts',(0.03455812447074,-1.5,-7.44833732146117));
#360296=CARTESIAN_POINT('Ctrl Pts',(0.0691497002760394,-1.49880576977359,
-7.44663986043241));
#360297=CARTESIAN_POINT('Ctrl Pts',(0.302114127086169,-1.48265937575617,
-7.43498284327662));
#360298=CARTESIAN_POINT('Ctrl Pts',(0.495782990150613,-1.42959048582248,
-7.42419080992647));
#360299=CARTESIAN_POINT('Ctrl Pts',(0.847010260809035,-1.25311844319053,
-7.4023903788038));
#360300=CARTESIAN_POINT('Ctrl Pts',(1.00201236847691,-1.13301134049999,
-7.39159652801348));
#360301=CARTESIAN_POINT('Ctrl Pts',(1.25591620604731,-0.842277268864258,
-7.37130462749836));
#360302=CARTESIAN_POINT('Ctrl Pts',(1.35316374690191,-0.675058625776248,
-7.36250325698756));
#360303=CARTESIAN_POINT('Ctrl Pts',(1.48204932028991,-0.30556823892079,
-7.34197601327337));
#360304=CARTESIAN_POINT('Ctrl Pts',(1.50950991824371,-0.105875768471577,
-7.3308819871373));
#360305=CARTESIAN_POINT('Ctrl Pts',(1.48515003725264,0.284953719955094,
-7.30916923778026));
#360306=CARTESIAN_POINT('Ctrl Pts',(1.43651615666324,0.47255725663361,-7.2987468190759));
#360307=CARTESIAN_POINT('Ctrl Pts',(1.26884196249976,0.824001710507948,
-7.27922212719399));
#360308=CARTESIAN_POINT('Ctrl Pts',(1.14956252123489,0.98359727785109,-7.26965287265012));
#360309=CARTESIAN_POINT('Ctrl Pts',(0.856183569542317,1.24731793580582,
-7.24821209742352));
#360310=CARTESIAN_POINT('Ctrl Pts',(0.685048336856938,1.34891069025598,
-7.23715632874501));
#360311=CARTESIAN_POINT('Ctrl Pts',(0.319942559610042,1.47775569881861,
-7.21601114083136));
#360312=CARTESIAN_POINT('Ctrl Pts',(0.130365721284194,1.50635212239085,
-7.20644867153388));
#360313=CARTESIAN_POINT('Ctrl Pts',(-0.258154573885091,1.49093809666085,
-7.1873278127357));
#360314=CARTESIAN_POINT('Ctrl Pts',(-0.453275731059376,1.44362633538023,
-7.17662582609297));
#360315=CARTESIAN_POINT('Ctrl Pts',(-0.810045874231628,1.27740919884723,
-7.15484357189489));
#360316=CARTESIAN_POINT('Ctrl Pts',(-0.968931336943506,1.1615203888964,
-7.14398005789622));
#360317=CARTESIAN_POINT('Ctrl Pts',(-1.2308607245362,0.8783153976357,-7.12351116904715));
#360318=CARTESIAN_POINT('Ctrl Pts',(-1.33253379305841,0.71470765501183,
-7.11470598083397));
#360319=CARTESIAN_POINT('Ctrl Pts',(-1.47240593241364,0.349434861517134,
-7.09441304786204));
#360320=CARTESIAN_POINT('Ctrl Pts',(-1.50584219290995,0.150027641038111,
-7.08333486894654));
#360321=CARTESIAN_POINT('Ctrl Pts',(-1.49274278900061,-0.242473565082339,
-7.0615292463843));
#360322=CARTESIAN_POINT('Ctrl Pts',(-1.44932531302366,-0.431912567947767,
-7.05100485733622));
#360323=CARTESIAN_POINT('Ctrl Pts',(-1.29197362459708,-0.786811895684146,
-7.03128822801753));
#360324=CARTESIAN_POINT('Ctrl Pts',(-1.17847511117939,-0.94840711761969,
-7.02202143473327));
#360325=CARTESIAN_POINT('Ctrl Pts',(-0.894284412677067,-1.22038798917765,
-7.00079327916653));
#360326=CARTESIAN_POINT('Ctrl Pts',(-0.725818321526072,-1.32750722822041,
-6.98971241615906));
#360327=CARTESIAN_POINT('Ctrl Pts',(-0.368653448389195,-1.46575000433356,
-6.96868823607392));
#360328=CARTESIAN_POINT('Ctrl Pts',(-0.185069197507755,-1.5,-6.95890414591665));
#360329=CARTESIAN_POINT('Ctrl Pts',(1.28369537222284E-15,-1.5,-6.95));
#360330=CARTESIAN_POINT('Ctrl Pts',(1.30728761149612E-13,-1.5,-6.8875));
#360331=CARTESIAN_POINT('Ctrl Pts',(-0.158390152479677,-1.5,-6.89512054976426));
#360332=CARTESIAN_POINT('Ctrl Pts',(-0.315971192569039,-1.47491827510613,
-6.90339888567089));
#360333=CARTESIAN_POINT('Ctrl Pts',(-0.653783527509526,-1.3642731496121,
-6.92272536492185));
#360334=CARTESIAN_POINT('Ctrl Pts',(-0.826821260072185,-1.2669016416291,
-6.93375541082207));
#360335=CARTESIAN_POINT('Ctrl Pts',(-1.12709975345344,-1.00954237554425,
-6.95535143507322));
#360336=CARTESIAN_POINT('Ctrl Pts',(-1.25080423509296,-0.851464098715239,
-6.96519643896028));
#360337=CARTESIAN_POINT('Ctrl Pts',(-1.42620834036991,-0.502660638698363,
-6.98457440896122));
#360338=CARTESIAN_POINT('Ctrl Pts',(-1.47869263683948,-0.316519978066789,
-6.99491555677408));
#360339=CARTESIAN_POINT('Ctrl Pts',(-1.51140509127975,0.0728561626068144,
-7.01654756458928));
#360340=CARTESIAN_POINT('Ctrl Pts',(-1.48839713759346,0.272649213524213,
-7.02764717852914));
#360341=CARTESIAN_POINT('Ctrl Pts',(-1.36775008530669,0.645211339832847,
-7.04834507443517));
#360342=CARTESIAN_POINT('Ctrl Pts',(-1.27379537939998,0.815157568179255,
-7.05719109035035));
#360343=CARTESIAN_POINT('Ctrl Pts',(-1.02584434032439,1.11140911599787,
-7.07734984994165));
#360344=CARTESIAN_POINT('Ctrl Pts',(-0.873772080737687,1.23454293921033,
-7.0880868139205));
#360345=CARTESIAN_POINT('Ctrl Pts',(-0.526816590516345,1.41845091857688,
-7.10988827270924));
#360346=CARTESIAN_POINT('Ctrl Pts',(-0.334329224715241,1.47573134939196,
-7.12074044849251));
#360347=CARTESIAN_POINT('Ctrl Pts',(0.0529135656295898,1.51105373279578,
-7.14035285324656));
#360348=CARTESIAN_POINT('Ctrl Pts',(0.243639774933199,1.49222541955791,
-7.14943808470476));
#360349=CARTESIAN_POINT('Ctrl Pts',(0.613841908736108,1.38262455643514,
-7.17029391159198));
#360350=CARTESIAN_POINT('Ctrl Pts',(0.78913569727102,1.2906254016952,-7.18128327000125));
#360351=CARTESIAN_POINT('Ctrl Pts',(1.09805587513349,1.04144027019704,-7.20306800819678));
#360352=CARTESIAN_POINT('Ctrl Pts',(1.22741158823864,0.885293034339754,
-7.2133170536478));
#360353=CARTESIAN_POINT('Ctrl Pts',(1.41248141808405,0.539858055493316,
-7.23250788580594));
#360354=CARTESIAN_POINT('Ctrl Pts',(1.46970787911335,0.355649358979269,
-7.24274170227894));
#360355=CARTESIAN_POINT('Ctrl Pts',(1.51275662636364,-0.0316722665942642,
-7.26425957036636));
#360356=CARTESIAN_POINT('Ctrl Pts',(1.4952830293338,-0.23145665075453,-7.27535870281971));
#360357=CARTESIAN_POINT('Ctrl Pts',(1.38495302486129,-0.607748939222347,
-7.29626382995681));
#360358=CARTESIAN_POINT('Ctrl Pts',(1.29509509903591,-0.781139147078928,
-7.30522135096988));
#360359=CARTESIAN_POINT('Ctrl Pts',(1.05452240507017,-1.08414839220289,
-7.32521283358061));
#360360=CARTESIAN_POINT('Ctrl Pts',(0.906132804005084,-1.21091027722153,
-7.33587339506334));
#360361=CARTESIAN_POINT('Ctrl Pts',(0.564648562678366,-1.40382350051254,
-7.35766176393148));
#360362=CARTESIAN_POINT('Ctrl Pts',(0.373743734336722,-1.46624765479896,
-7.36858068105327));
#360363=CARTESIAN_POINT('Ctrl Pts',(0.117614019873121,-1.49654541479466,
-7.38174533213034));
#360364=CARTESIAN_POINT('Ctrl Pts',(0.0587783367701221,-1.5,-7.38467202595361));
#360365=CARTESIAN_POINT('Ctrl Pts',(1.64729341278753E-13,-1.5,-7.3875));
#360366=CARTESIAN_POINT('Origin',(0.,1.30104260698261E-15,-17.7));
#360367=CARTESIAN_POINT('',(6.58274699238299E-14,-1.5,-7.94999999999999));
#360368=CARTESIAN_POINT('',(-6.48430451891059E-15,-1.5,-7.8875));
#360369=CARTESIAN_POINT('',(-1.83697019872103E-16,-1.5,-17.7));
#360370=CARTESIAN_POINT('Ctrl Pts',(1.31838636867532E-13,-1.5,-7.94999999999999));
#360371=CARTESIAN_POINT('Ctrl Pts',(0.0622836217362446,-1.5,-7.94700337785203));
#360372=CARTESIAN_POINT('Ctrl Pts',(0.124625046031404,-1.4961211374503,
-7.94389622849522));
#360373=CARTESIAN_POINT('Ctrl Pts',(0.385989404538987,-1.46334076996953,
-7.93041076417012));
#360374=CARTESIAN_POINT('Ctrl Pts',(0.57824906146685,-1.39855788367082,
-7.91936114249391));
#360375=CARTESIAN_POINT('Ctrl Pts',(0.919134390997817,-1.20103864507334,
-7.89747364391336));
#360376=CARTESIAN_POINT('Ctrl Pts',(1.06599946847489,-1.07282927383352,
-7.88684622315537));
#360377=CARTESIAN_POINT('Ctrl Pts',(1.3035473165281,-0.767075269261111,
-7.86692403019345));
#360378=CARTESIAN_POINT('Ctrl Pts',(1.3917190920234,-0.592252778217645,
-7.8579029321232));
#360379=CARTESIAN_POINT('Ctrl Pts',(1.49778553788722,-0.214457793011997,
-7.83691432183399));
#360380=CARTESIAN_POINT('Ctrl Pts',(1.51298718653284,-0.014720015692516,
-7.82581777864958));
#360381=CARTESIAN_POINT('Ctrl Pts',(1.46570987294793,0.37167827682238,-7.80435120684319));
#360382=CARTESIAN_POINT('Ctrl Pts',(1.40655075449925,0.555057249933396,
-7.7941634861148));
#360383=CARTESIAN_POINT('Ctrl Pts',(1.2188455871199,0.896615758666252,-7.77518801340742));
#360384=CARTESIAN_POINT('Ctrl Pts',(1.08941924203679,1.05010363320528,-7.7649118290207));
#360385=CARTESIAN_POINT('Ctrl Pts',(0.780422341329571,1.29589316828388,
-7.74321772161835));
#360386=CARTESIAN_POINT('Ctrl Pts',(0.604635461528741,1.38665718104324,
-7.73223894884395));
#360387=CARTESIAN_POINT('Ctrl Pts',(0.233805272802087,1.49380325165562,
-7.71142109333097));
#360388=CARTESIAN_POINT('Ctrl Pts',(0.0429155053270266,1.51137658317992,
-7.70238078941218));
#360389=CARTESIAN_POINT('Ctrl Pts',(-0.344135327230572,1.47347614001839,
-7.68270600746043));
#360390=CARTESIAN_POINT('Ctrl Pts',(-0.536243143563457,1.41491503845189,
-7.67183651857192));
#360391=CARTESIAN_POINT('Ctrl Pts',(-0.881862737716797,1.22875704214068,
-7.65003683264203));
#360392=CARTESIAN_POINT('Ctrl Pts',(-1.03302891469827,1.10471282610045,
-7.63931817389319));
#360393=CARTESIAN_POINT('Ctrl Pts',(-1.27915452935369,0.806781048157432,
-7.61920056701624));
#360394=CARTESIAN_POINT('Ctrl Pts',(-1.37209747555576,0.635989373106926,
-7.61033274295038));
#360395=CARTESIAN_POINT('Ctrl Pts',(-1.49020295425105,0.262496115259053,
-7.58958311751438));
#360396=CARTESIAN_POINT('Ctrl Pts',(-1.51184297998452,0.0626914013643946,
-7.57848285563134));
#360397=CARTESIAN_POINT('Ctrl Pts',(-1.47657100600956,-0.326202548982423,
-7.55687763616763));
#360398=CARTESIAN_POINT('Ctrl Pts',(-1.42291007553314,-0.511877428139616,
-7.54656236510334));
#360399=CARTESIAN_POINT('Ctrl Pts',(-1.24512333107803,-0.859857421184804,
-7.5272301432675));
#360400=CARTESIAN_POINT('Ctrl Pts',(-1.12003804942027,-1.01746355631494,
-7.5172916458803));
#360401=CARTESIAN_POINT('Ctrl Pts',(-0.817630476530446,-1.27283083493107,
-7.49564851922878));
#360402=CARTESIAN_POINT('Ctrl Pts',(-0.644023691645171,-1.36888750420052,
-7.48462761808352));
#360403=CARTESIAN_POINT('Ctrl Pts',(-0.308938681843284,-1.47603136537536,
-7.46552961466667));
#360404=CARTESIAN_POINT('Ctrl Pts',(-0.15483694149587,-1.5,-7.4574495958211));
#360405=CARTESIAN_POINT('Ctrl Pts',(1.6976003935909E-13,-1.5,-7.44999999999999));
#360406=CARTESIAN_POINT('Ctrl Pts',(1.64139535296925E-13,-1.5,-7.3875));
#360407=CARTESIAN_POINT('Ctrl Pts',(-0.130711946418685,-1.5,-7.39378888145426));
#360408=CARTESIAN_POINT('Ctrl Pts',(-0.26109431040442,-1.48291923269925,
-7.40053637162469));
#360409=CARTESIAN_POINT('Ctrl Pts',(-0.576783675113658,-1.39841762954913,
-7.41807225002012));
#360410=CARTESIAN_POINT('Ctrl Pts',(-0.754002495834011,-1.31138315363872,
-7.42901631883833));
#360411=CARTESIAN_POINT('Ctrl Pts',(-1.0676374910888,-1.07223563176754,
-7.45074907630178));
#360412=CARTESIAN_POINT('Ctrl Pts',(-1.20015471344121,-0.921468937328372,
-7.46130728125954));
#360413=CARTESIAN_POINT('Ctrl Pts',(-1.39462578116005,-0.584246741581453,
-7.48004184768993));
#360414=CARTESIAN_POINT('Ctrl Pts',(-1.45748819449554,-0.402528118290563,
-7.49013732676164));
#360415=CARTESIAN_POINT('Ctrl Pts',(-1.5128948459604,-0.0180421993557636,
-7.51149765559135));
#360416=CARTESIAN_POINT('Ctrl Pts',(-1.5020740026234,0.181534635375859,
-7.52258525752089));
#360417=CARTESIAN_POINT('Ctrl Pts',(-1.40428067204569,0.562179549005838,
-7.543732197167));
#360418=CARTESIAN_POINT('Ctrl Pts',(-1.31937269119552,0.739795325885163,
-7.55290485529489));
#360419=CARTESIAN_POINT('Ctrl Pts',(-1.0876546246449,1.0507980282835,-7.57269235992532));
#360420=CARTESIAN_POINT('Ctrl Pts',(-0.943749465253424,1.18173131505699,
-7.5832530358784));
#360421=CARTESIAN_POINT('Ctrl Pts',(-0.607782292460559,1.3859150267921,
-7.60508903378639));
#360422=CARTESIAN_POINT('Ctrl Pts',(-0.41737912000973,1.45463755092375,
-7.6161587696958));
#360423=CARTESIAN_POINT('Ctrl Pts',(-0.0304488659793696,1.51176518887962,
-7.63636183905474));
#360424=CARTESIAN_POINT('Ctrl Pts',(0.161748775563658,1.50339693636403,
-7.64518778224929));
#360425=CARTESIAN_POINT('Ctrl Pts',(0.537002395637976,1.41409610431455,
-7.66572275913103));
#360426=CARTESIAN_POINT('Ctrl Pts',(0.716114530205454,1.3323705443853,-7.67661045016581));
#360427=CARTESIAN_POINT('Ctrl Pts',(1.03604574905603,1.10277800527287,-7.69838071864051));
#360428=CARTESIAN_POINT('Ctrl Pts',(1.17292778376266,0.955916148964611,
-7.70904595461449));
#360429=CARTESIAN_POINT('Ctrl Pts',(1.37687637469735,0.624772142429321,
-7.72805688039689));
#360430=CARTESIAN_POINT('Ctrl Pts',(1.44491471501658,0.445409432145121,
-7.7377550315475));
#360431=CARTESIAN_POINT('Ctrl Pts',(1.51158414892893,0.0636737338260033,
-7.75896257034301));
#360432=CARTESIAN_POINT('Ctrl Pts',(1.50684319464338,-0.135523662450533,
-7.77002909235837));
#360433=CARTESIAN_POINT('Ctrl Pts',(1.42065840926741,-0.520017926624075,
-7.79138988481246));
#360434=CARTESIAN_POINT('Ctrl Pts',(1.34031972299538,-0.701581490106598,
-7.80083554531923));
#360435=CARTESIAN_POINT('Ctrl Pts',(1.11669567601627,-1.01978268009016,
-7.82043358423994));
#360436=CARTESIAN_POINT('Ctrl Pts',(0.976941627781406,-1.15435347368589,
-7.83089558162055));
#360437=CARTESIAN_POINT('Ctrl Pts',(0.647943350348728,-1.36751217147121,
-7.85264559356225));
#360438=CARTESIAN_POINT('Ctrl Pts',(0.460218660943862,-1.44157281839024,
-7.86373474208457));
#360439=CARTESIAN_POINT('Ctrl Pts',(0.176319080109958,-1.49223079408003,
-7.87880103302739));
#360440=CARTESIAN_POINT('Ctrl Pts',(0.0881508891495514,-1.5,-7.88325883836835));
#360441=CARTESIAN_POINT('Ctrl Pts',(-1.73472347597681E-16,-1.5,-7.8875));
#360442=CARTESIAN_POINT('Origin',(0.,1.30104260698261E-15,-17.7));
#360443=CARTESIAN_POINT('',(1.62838980068328E-14,-1.5,-8.45));
#360444=CARTESIAN_POINT('',(-3.3120983492535E-14,-1.5,-8.38750000000001));
#360445=CARTESIAN_POINT('',(-1.83697019872103E-16,-1.5,-17.7));
#360446=CARTESIAN_POINT('Ctrl Pts',(3.27514930335377E-14,-1.5,-8.45));
#360447=CARTESIAN_POINT('Ctrl Pts',(0.0919060245909611,-1.5,-8.44557816933018));
#360448=CARTESIAN_POINT('Ctrl Pts',(0.183815329080158,-1.49155484907763,
-8.44092159333058));
#360449=CARTESIAN_POINT('Ctrl Pts',(0.470889171269676,-1.43810172702746,
-8.42562493771262));
#360450=CARTESIAN_POINT('Ctrl Pts',(0.657920267443974,-1.36271842253387,
-8.41453241922198));
#360451=CARTESIAN_POINT('Ctrl Pts',(0.985135825347778,-1.14734611051077,
-8.39280668912922));
#360452=CARTESIAN_POINT('Ctrl Pts',(1.123835536039,-1.01188384306565,-8.38237065542485));
#360453=CARTESIAN_POINT('Ctrl Pts',(1.34541672627809,-0.691881954295951,
-8.36282088408414));
#360454=CARTESIAN_POINT('Ctrl Pts',(1.42459400378327,-0.509309679182099,
-8.35329498217678));
#360455=CARTESIAN_POINT('Ctrl Pts',(1.50782651039528,-0.123864807282884,
-8.33188137818238));
#360456=CARTESIAN_POINT('Ctrl Pts',(1.51103461398953,0.0752080911527746,
-8.32082177271373));
#360457=CARTESIAN_POINT('Ctrl Pts',(1.44153190399057,0.456206191994516,
-8.29965521155586));
#360458=CARTESIAN_POINT('Ctrl Pts',(1.37218726699645,0.634984418918529,
-8.2900476012505));
#360459=CARTESIAN_POINT('Ctrl Pts',(1.16582929948974,0.964562380147401,
-8.27096425554225));
#360460=CARTESIAN_POINT('Ctrl Pts',(1.02785859315551,1.11041463298508,-8.26027468537101));
#360461=CARTESIAN_POINT('Ctrl Pts',(0.706342100872746,1.33755660851709,
-8.23849621660331));
#360462=CARTESIAN_POINT('Ctrl Pts',(0.526771233312194,1.41792015918229,
-8.22762428835778));
#360463=CARTESIAN_POINT('Ctrl Pts',(0.150875651795156,1.50454645245795,
-8.20713271783545));
#360464=CARTESIAN_POINT('Ctrl Pts',(-0.0415361031340621,1.51152080393762,
-8.1983216156378));
#360465=CARTESIAN_POINT('Ctrl Pts',(-0.428035479493202,1.45151678832234,
-8.17805937751105));
#360466=CARTESIAN_POINT('Ctrl Pts',(-0.617788120056051,1.38146223334104,
-8.16698393947476));
#360467=CARTESIAN_POINT('Ctrl Pts',(-0.952049697448619,1.17503292634832,
-8.14516762441768));
#360468=CARTESIAN_POINT('Ctrl Pts',(-1.09493439388521,1.04318612453353,
-8.1346306700936));
#360469=CARTESIAN_POINT('Ctrl Pts',(-1.32465451950825,0.730397000890158,
-8.1148896686285));
#360470=CARTESIAN_POINT('Ctrl Pts',(-1.40843905179061,0.55181414724647,
-8.10565634151369));
#360471=CARTESIAN_POINT('Ctrl Pts',(-1.50338010817072,0.170207103404275,
-8.08445595018912));
#360472=CARTESIAN_POINT('Ctrl Pts',(-1.51269957457772,-0.0292929547662327,
-8.07337261362409));
#360473=CARTESIAN_POINT('Ctrl Pts',(-1.45449801295143,-0.413190375994559,
-8.0520449791114));
#360474=CARTESIAN_POINT('Ctrl Pts',(-1.39033334183595,-0.594315098362038,
-8.04205035803207));
#360475=CARTESIAN_POINT('Ctrl Pts',(-1.1935325018415,-0.93005646632443,
-8.02325562409304));
#360476=CARTESIAN_POINT('Ctrl Pts',(-1.05991258445926,-1.07985343287618,
-8.01266580597191));
#360477=CARTESIAN_POINT('Ctrl Pts',(-0.744776913013553,-1.31662456257156,
-7.99092685808533));
#360478=CARTESIAN_POINT('Ctrl Pts',(-0.567079977833594,-1.40236211515631,
-7.9799958116224));
#360479=CARTESIAN_POINT('Ctrl Pts',(-0.254270975061089,-1.48380485968209,
-7.96268348300038));
#360480=CARTESIAN_POINT('Ctrl Pts',(-0.127278002173556,-1.5,-7.95612366573474));
#360481=CARTESIAN_POINT('Ctrl Pts',(1.32081845460874E-13,-1.5,-7.94999999999999));
#360482=CARTESIAN_POINT('Ctrl Pts',(-2.55004350968591E-15,-1.5,-7.8875));
#360483=CARTESIAN_POINT('Ctrl Pts',(-0.10237969393186,-1.5,-7.89242574532093));
#360484=CARTESIAN_POINT('Ctrl Pts',(-0.204707722448345,-1.489520686643,
-7.8976400969261));
#360485=CARTESIAN_POINT('Ctrl Pts',(-0.495809132059467,-1.42898472088833,
-7.91332727463043));
#360486=CARTESIAN_POINT('Ctrl Pts',(-0.676699620390658,-1.35273472674166,
-7.92414842770105));
#360487=CARTESIAN_POINT('Ctrl Pts',(-1.00287409426353,-1.13303498676165,
-7.94594427494716));
#360488=CARTESIAN_POINT('Ctrl Pts',(-1.14407565723151,-0.990271945330059,
-7.95670347835272));
#360489=CARTESIAN_POINT('Ctrl Pts',(-1.3576613618609,-0.665443132622998,
-7.97600264793315));
#360490=CARTESIAN_POINT('Ctrl Pts',(-1.43092922096547,-0.488390490422837,
-7.98536719497652));
#360491=CARTESIAN_POINT('Ctrl Pts',(-1.50886956974448,-0.109630465307728,
-8.00640941859402));
#360492=CARTESIAN_POINT('Ctrl Pts',(-1.51022654561875,0.0890022614738588,
-8.01744457008189));
#360493=CARTESIAN_POINT('Ctrl Pts',(-1.43585304738513,0.47722941824748,
-8.0390127454582));
#360494=CARTESIAN_POINT('Ctrl Pts',(-1.36016227437668,0.662838498285955,
-8.04880467590354));
#360495=CARTESIAN_POINT('Ctrl Pts',(-1.14467434096634,0.988173006718972,
-8.06820941361236));
#360496=CARTESIAN_POINT('Ctrl Pts',(-1.00913285985506,1.12623053363248,
-8.07856558746601));
#360497=CARTESIAN_POINT('Ctrl Pts',(-0.687286816935304,1.34808086137161,
-8.10021292152966));
#360498=CARTESIAN_POINT('Ctrl Pts',(-0.502364143957666,1.42734931561428,
-8.1113119192883));
#360499=CARTESIAN_POINT('Ctrl Pts',(-0.119122736408198,1.50757862908486,
-8.13197922214693));
#360500=CARTESIAN_POINT('Ctrl Pts',(0.0749006733276469,1.51042123685776,
-8.14081418152409));
#360501=CARTESIAN_POINT('Ctrl Pts',(0.455115960360642,1.442388450537,-8.16099709767065));
#360502=CARTESIAN_POINT('Ctrl Pts',(0.637587446377473,1.37152637789345,
-8.17174465204168));
#360503=CARTESIAN_POINT('Ctrl Pts',(0.969571590709034,1.16166609369766,
-8.19354669897183));
#360504=CARTESIAN_POINT('Ctrl Pts',(1.11487635577431,1.023038867733,-8.20438843401737));
#360505=CARTESIAN_POINT('Ctrl Pts',(1.33782638530658,0.704482335029449,
-8.22396391488966));
#360506=CARTESIAN_POINT('Ctrl Pts',(1.4161945616287,0.529606115593179,-8.23307743802261));
#360507=CARTESIAN_POINT('Ctrl Pts',(1.50493462866019,0.153799071573299,
-8.25395560713482));
#360508=CARTESIAN_POINT('Ctrl Pts',(1.51212858296256,-0.0441180221961207,
-8.26495100123312));
#360509=CARTESIAN_POINT('Ctrl Pts',(1.44924015520889,-0.435792680293736,
-8.28671070446077));
#360510=CARTESIAN_POINT('Ctrl Pts',(1.37807880670724,-0.625357255423701,
-8.29690152070481));
#360511=CARTESIAN_POINT('Ctrl Pts',(1.17041094760942,-0.957451741924483,
-8.3161177920814));
#360512=CARTESIAN_POINT('Ctrl Pts',(1.03894701909247,-1.09870021797266,
-8.32636642207035));
#360513=CARTESIAN_POINT('Ctrl Pts',(0.724096160060608,-1.32858932692728,
-8.34790049967047));
#360514=CARTESIAN_POINT('Ctrl Pts',(0.541961125988814,-1.41271054922394,
-8.35900017620234));
#360515=CARTESIAN_POINT('Ctrl Pts',(0.234231915043067,-1.48626832059935,
-8.37584907619419));
#360516=CARTESIAN_POINT('Ctrl Pts',(0.117197432864771,-1.50000000000001,
-8.38186133588227));
#360517=CARTESIAN_POINT('Ctrl Pts',(-6.44276298977786E-14,-1.5,-8.38750000000001));
#360518=CARTESIAN_POINT('Origin',(0.,1.30104260698261E-15,-17.7));
#360519=CARTESIAN_POINT('',(-4.96354202156784E-14,-1.5,-8.95));
#360520=CARTESIAN_POINT('',(-1.15641779244756E-13,-1.5,-8.88750000000002));
#360521=CARTESIAN_POINT('',(-1.83697019872103E-16,-1.5,-17.7));
#360522=CARTESIAN_POINT('Ctrl Pts',(-9.75608482889356E-14,-1.5,-8.95));
#360523=CARTESIAN_POINT('Ctrl Pts',(0.12285708034588,-1.50000000000001,
-8.94408903596587));
#360524=CARTESIAN_POINT('Ctrl Pts',(0.245494453006151,-1.48491021249227,
-8.93776948185859));
#360525=CARTESIAN_POINT('Ctrl Pts',(0.557659907759538,-1.40655610297248,
-8.92057391137191));
#360526=CARTESIAN_POINT('Ctrl Pts',(0.738647166664289,-1.32052182799538,
-8.90947631684627));
#360527=CARTESIAN_POINT('Ctrl Pts',(1.05064900131988,-1.0874803941173,-8.88799174841416));
#360528=CARTESIAN_POINT('Ctrl Pts',(1.18046342086137,-0.944990066599894,
-8.87778798458865));
#360529=CARTESIAN_POINT('Ctrl Pts',(1.38367733959653,-0.61232870455309,
-8.85877025697472));
#360530=CARTESIAN_POINT('Ctrl Pts',(1.45258311498454,-0.42374149198048,
-8.84854119399891));
#360531=CARTESIAN_POINT('Ctrl Pts',(1.5123857666276,-0.0333883641337487,
-8.82685490911854));
#360532=CARTESIAN_POINT('Ctrl Pts',(1.50380314579772,0.164332980671071,
-8.81587038996271));
#360533=CARTESIAN_POINT('Ctrl Pts',(1.41248988489652,0.539422119867692,
-8.79503210445179));
#360534=CARTESIAN_POINT('Ctrl Pts',(1.33289232409031,0.713784931995395,
-8.78596811928743));
#360535=CARTESIAN_POINT('Ctrl Pts',(1.10769266361828,1.03081373272249,-8.76632683999544));
#360536=CARTESIAN_POINT('Ctrl Pts',(0.961416840844422,1.16842525458379,
-8.75546659891697));
#360537=CARTESIAN_POINT('Ctrl Pts',(0.628076109264871,1.375889546242,-8.73366583850069));
#360538=CARTESIAN_POINT('Ctrl Pts',(0.44524688013909,1.44544802847379,-8.72293728305107));
#360539=CARTESIAN_POINT('Ctrl Pts',(0.0644587751524896,1.51093518733999,
-8.7027975190616));
#360540=CARTESIAN_POINT('Ctrl Pts',(-0.129800484908925,1.50672943834416,
-8.69394190010097));
#360541=CARTESIAN_POINT('Ctrl Pts',(-0.512558713165532,1.42370009868172,
-8.67322006571158));
#360542=CARTESIAN_POINT('Ctrl Pts',(-0.696778221911868,1.3431785199936,
-8.66212008994541));
#360543=CARTESIAN_POINT('Ctrl Pts',(-1.01684912889306,1.11924664383361,
-8.64050034135996));
#360544=CARTESIAN_POINT('Ctrl Pts',(-1.15135203977399,0.980359631790227,
-8.63017109448621));
#360545=CARTESIAN_POINT('Ctrl Pts',(-1.36484372826175,0.653290534438722,
-8.61081421813049));
#360546=CARTESIAN_POINT('Ctrl Pts',(-1.43938443401498,0.466677723103864,
-8.60092654017244));
#360547=CARTESIAN_POINT('Ctrl Pts',(-1.510838369229,0.0775569667310619,
-8.57930872037395));
#360548=CARTESIAN_POINT('Ctrl Pts',(-1.50798869035152,-0.120909140047158,
-8.56828282555293));
#360549=CARTESIAN_POINT('Ctrl Pts',(-1.42728835970505,-0.498923829940028,
-8.54728200944777));
#360550=CARTESIAN_POINT('Ctrl Pts',(-1.3527258432058,-0.6754168702095,-8.53798813941484));
#360551=CARTESIAN_POINT('Ctrl Pts',(-1.13675898689194,-0.998663807739,-8.51861834759773));
#360552=CARTESIAN_POINT('Ctrl Pts',(-0.994504962094306,-1.14038938093043,
-8.507837326161));
#360553=CARTESIAN_POINT('Ctrl Pts',(-0.666828702371811,-1.35760795376376,
-8.48603814551915));
#360554=CARTESIAN_POINT('Ctrl Pts',(-0.48552228395892,-1.4324939668161,
-8.47523486936688));
#360555=CARTESIAN_POINT('Ctrl Pts',(-0.197627808105292,-1.49023483420086,
-8.45977962695627));
#360556=CARTESIAN_POINT('Ctrl Pts',(-0.0988289996479366,-1.5,-8.45475491246254));
#360557=CARTESIAN_POINT('Ctrl Pts',(3.27514930335377E-14,-1.5,-8.45));
#360558=CARTESIAN_POINT('Ctrl Pts',(-6.60582699651979E-14,-1.5,-8.38750000000001));
#360559=CARTESIAN_POINT('Ctrl Pts',(-0.0753177345365689,-1.5,-8.39112372619246));
#360560=CARTESIAN_POINT('Ctrl Pts',(-0.150687448593511,-1.49432802738698,
-8.39490750804556));
#360561=CARTESIAN_POINT('Ctrl Pts',(-0.416724607344908,-1.45387804366168,
-8.40883083747289));
#360562=CARTESIAN_POINT('Ctrl Pts',(-0.600532463051642,-1.38808029394905,
-8.41950201232364));
#360563=CARTESIAN_POINT('Ctrl Pts',(-0.937680864741628,-1.18756128620999,
-8.44129304480022));
#360564=CARTESIAN_POINT('Ctrl Pts',(-1.08671110052146,-1.05291245336646,
-8.45220351071906));
#360565=CARTESIAN_POINT('Ctrl Pts',(-1.31836851280872,-0.740316064545367,
-8.47203236618718));
#360566=CARTESIAN_POINT('Ctrl Pts',(-1.4015064228706,-0.567407959064957,
-8.48097733560751));
#360567=CARTESIAN_POINT('Ctrl Pts',(-1.50016254659718,-0.194397121232557,
-8.50170015993153));
#360568=CARTESIAN_POINT('Ctrl Pts',(-1.51270126349758,0.0027122562987613,
-8.51265068090549));
#360569=CARTESIAN_POINT('Ctrl Pts',(-1.46098267953079,0.393790137894556,
-8.53437722988303));
#360570=CARTESIAN_POINT('Ctrl Pts',(-1.39598155896985,0.583709457498217,
-8.54488329085926));
#360571=CARTESIAN_POINT('Ctrl Pts',(-1.19990662713579,0.92009542914897,
-8.56366100518365));
#360572=CARTESIAN_POINT('Ctrl Pts',(-1.07337989682116,1.06498014824303,
-8.57377310086461));
#360573=CARTESIAN_POINT('Ctrl Pts',(-0.767088280050412,1.30414031891685,
-8.59515290122164));
#360574=CARTESIAN_POINT('Ctrl Pts',(-0.588421794296112,1.39390506697201,
-8.60624246174918));
#360575=CARTESIAN_POINT('Ctrl Pts',(-0.209575637272476,1.49801643981653,
-8.62736168855644));
#360576=CARTESIAN_POINT('Ctrl Pts',(-0.0134428537343731,1.51254306759813,
-8.63650481185376));
#360577=CARTESIAN_POINT('Ctrl Pts',(0.371467798904194,1.46601734040751,
-8.65631621557418));
#360578=CARTESIAN_POINT('Ctrl Pts',(0.556663120472392,1.40616658614029,
-8.66688895058939));
#360579=CARTESIAN_POINT('Ctrl Pts',(0.9009035992305,1.21596192414218,-8.68873469117908));
#360580=CARTESIAN_POINT('Ctrl Pts',(1.05518918317806,1.08479619456351,-8.69980125228606));
#360581=CARTESIAN_POINT('Ctrl Pts',(1.29695109115979,0.777335448538104,
-8.71997360378563));
#360582=CARTESIAN_POINT('Ctrl Pts',(1.3851246432063,0.60643762686481,-8.72880902072974));
#360583=CARTESIAN_POINT('Ctrl Pts',(1.49404813319494,0.236405329345541,
-8.74936637059192));
#360584=CARTESIAN_POINT('Ctrl Pts',(1.51209680439187,0.0402838347975675,
-8.76026200917792));
#360585=CARTESIAN_POINT('Ctrl Pts',(1.47171963321517,-0.351495970951461,
-8.78202755394175));
#360586=CARTESIAN_POINT('Ctrl Pts',(1.41224105671491,-0.543239103722307,
-8.7926799502068));
#360587=CARTESIAN_POINT('Ctrl Pts',(1.2261107511641,-0.884757979971881,
-8.81165322110956));
#360588=CARTESIAN_POINT('Ctrl Pts',(1.10419440264631,-1.03292814495696,
-8.82140020383724));
#360589=CARTESIAN_POINT('Ctrl Pts',(0.805869612369571,-1.28044755098058,
-8.8426289010578));
#360590=CARTESIAN_POINT('Ctrl Pts',(0.630538448004124,-1.37528014404724,
-8.85369876433274));
#360591=CARTESIAN_POINT('Ctrl Pts',(0.298471493246989,-1.4776451341655,
-8.87251881509031));
#360592=CARTESIAN_POINT('Ctrl Pts',(0.149535379941175,-1.50000000000002,
-8.88030547567814));
#360593=CARTESIAN_POINT('Ctrl Pts',(-2.32973362823685E-13,-1.5,-8.88750000000002));
#360594=CARTESIAN_POINT('Origin',(0.,1.30104260698261E-15,-17.7));
#360595=CARTESIAN_POINT('',(-1.23881389363399E-13,-1.5,-9.45000000000001));
#360596=CARTESIAN_POINT('',(-1.6641110470755E-14,-1.5,-9.38750000000001));
#360597=CARTESIAN_POINT('',(-1.83697019872103E-16,-1.5,-17.7));
#360598=CARTESIAN_POINT('Ctrl Pts',(-2.47232789796215E-13,-1.5,-9.45000000000001));
#360599=CARTESIAN_POINT('Ctrl Pts',(0.153335778247755,-1.50000000000002,
-9.44262262892935));
#360600=CARTESIAN_POINT('Ctrl Pts',(0.306002085618831,-1.47649420208641,
-9.43462452896035));
#360601=CARTESIAN_POINT('Ctrl Pts',(0.640761324790949,-1.37052596697953,
-9.4155748554699));
#360602=CARTESIAN_POINT('Ctrl Pts',(0.815254691016666,-1.27447028179578,
-9.40451132599572));
#360603=CARTESIAN_POINT('Ctrl Pts',(1.11160042974155,-1.02493836354319,
-9.38332194281987));
#360604=CARTESIAN_POINT('Ctrl Pts',(1.23239895244512,-0.875962061462964,
-9.37366455897016));
#360605=CARTESIAN_POINT('Ctrl Pts',(1.41606815869254,-0.533186370882533,
-9.35462146504903));
#360606=CARTESIAN_POINT('Ctrl Pts',(1.47418437701841,-0.341016503325073,
-9.34394536129583));
#360607=CARTESIAN_POINT('Ctrl Pts',(1.51175878871156,0.0509164925721334,
-9.32217130596821));
#360608=CARTESIAN_POINT('Ctrl Pts',(1.49235380541641,0.246770303443136,
-9.3112905386976));
#360609=CARTESIAN_POINT('Ctrl Pts',(1.38089384609243,0.616053945194668,
-9.29077478082252));
#360610=CARTESIAN_POINT('Ctrl Pts',(1.29146002028184,0.786459001367279,
-9.2819559824918));
#360611=CARTESIAN_POINT('Ctrl Pts',(1.04751200092349,1.09218476693379,-9.26172664556122));
#360612=CARTESIAN_POINT('Ctrl Pts',(0.892426789909005,1.22217335825025,
-9.2506543106641));
#360613=CARTESIAN_POINT('Ctrl Pts',(0.547128742727475,1.40988634583528,
-9.22882690096806));
#360614=CARTESIAN_POINT('Ctrl Pts',(0.36165896926966,1.46845139547383,-9.21827667539762));
#360615=CARTESIAN_POINT('Ctrl Pts',(-0.0237796560834993,1.51246183502246,
-9.19850973867929));
#360616=CARTESIAN_POINT('Ctrl Pts',(-0.22017516771744,1.4965421493116,-9.18931076589611));
#360617=CARTESIAN_POINT('Ctrl Pts',(-0.598458835159482,1.38960499905061,
-9.16814010806433));
#360618=CARTESIAN_POINT('Ctrl Pts',(-0.776347226521873,1.29862832019234,
-9.15705431887615));
#360619=CARTESIAN_POINT('Ctrl Pts',(-1.08082195073198,1.05742257052299,
-9.13570511216443));
#360620=CARTESIAN_POINT('Ctrl Pts',(-1.20623129179855,0.911739110792384,
-9.1256521728218));
#360621=CARTESIAN_POINT('Ctrl Pts',(-1.39995741045566,0.574144676287531,
-9.10689692646042));
#360622=CARTESIAN_POINT('Ctrl Pts',(-1.4636276388161,0.383783756873773,
-9.09632131982632));
#360623=CARTESIAN_POINT('Ctrl Pts',(-1.5126690241621,-0.00739484925308877,
-9.07458917504149));
#360624=CARTESIAN_POINT('Ctrl Pts',(-1.49883142016827,-0.204285647767434,
-9.06365079734625));
#360625=CARTESIAN_POINT('Ctrl Pts',(-1.39775968728795,-0.576603269734524,
-9.04296648501475));
#360626=CARTESIAN_POINT('Ctrl Pts',(-1.31344625078534,-0.749036025861445,
-9.03405332259749));
#360627=CARTESIAN_POINT('Ctrl Pts',(-1.07842187507997,-1.06178743086891,
-9.0140581680212));
#360628=CARTESIAN_POINT('Ctrl Pts',(-0.92664358218245,-1.19653654936018,
-9.0030127004302));
#360629=CARTESIAN_POINT('Ctrl Pts',(-0.585757273911393,-1.39435192995385,
-8.98111692859344));
#360630=CARTESIAN_POINT('Ctrl Pts',(-0.401458959921958,-1.45814093494388,
-8.97047795502207));
#360631=CARTESIAN_POINT('Ctrl Pts',(-0.140359897804498,-1.49507947307301,
-8.95688975003526));
#360632=CARTESIAN_POINT('Ctrl Pts',(-0.0701507731510393,-1.5,-8.95337513064688));
#360633=CARTESIAN_POINT('Ctrl Pts',(-9.90871434114846E-14,-1.5,-8.95));
#360634=CARTESIAN_POINT('Ctrl Pts',(-2.31099861469641E-13,-1.5,-8.88750000000002));
#360635=CARTESIAN_POINT('Ctrl Pts',(-0.0462362988015458,-1.49999999999999,
-8.88972454496329));
#360636=CARTESIAN_POINT('Ctrl Pts',(-0.0925241731482299,-1.49786231858749,
-8.89201095139538));
#360637=CARTESIAN_POINT('Ctrl Pts',(-0.330227573982773,-1.47578526622149,
-8.90406071305492));
#360638=CARTESIAN_POINT('Ctrl Pts',(-0.516514865900817,-1.42133246726656,
-8.91453604231496));
#360639=CARTESIAN_POINT('Ctrl Pts',(-0.865072685483243,-1.24161204761194,
-8.93629827210792));
#360640=CARTESIAN_POINT('Ctrl Pts',(-1.02265346756099,-1.1154123654225,
-8.94738542774805));
#360641=CARTESIAN_POINT('Ctrl Pts',(-1.27355199468674,-0.815264932438499,
-8.96779421745666));
#360642=CARTESIAN_POINT('Ctrl Pts',(-1.36702068629316,-0.64641121301876,
-8.97658826594341));
#360643=CARTESIAN_POINT('Ctrl Pts',(-1.48651080122788,-0.279530844467869,
-8.99697050864068));
#360644=CARTESIAN_POINT('Ctrl Pts',(-1.51019435270887,-0.0845858145439524,
-9.0078007880809));
#360645=CARTESIAN_POINT('Ctrl Pts',(-1.48150057665828,0.307699504671352,
-9.02959441692619));
#360646=CARTESIAN_POINT('Ctrl Pts',(-1.42772166223408,0.501155664052166,
-9.04034198133624));
#360647=CARTESIAN_POINT('Ctrl Pts',(-1.2518677835424,0.847873866069245,
-9.05960410367052));
#360648=CARTESIAN_POINT('Ctrl Pts',(-1.13457610937044,0.999413064688373,
-9.06900748883903));
#360649=CARTESIAN_POINT('Ctrl Pts',(-0.844470127281307,1.25523165752531,
-9.09007129143333));
#360650=CARTESIAN_POINT('Ctrl Pts',(-0.672664155995585,1.35508634082449,
-9.1011110512836));
#360651=CARTESIAN_POINT('Ctrl Pts',(-0.29890801101406,1.48323177510825,
-9.12265299759007));
#360652=CARTESIAN_POINT('Ctrl Pts',(-0.100474031127314,1.50970308148693,
-9.13239641088221));
#360653=CARTESIAN_POINT('Ctrl Pts',(0.288751466663172,1.48438992600939,
-9.15182617458365));
#360654=CARTESIAN_POINT('Ctrl Pts',(0.475975254188957,1.43534586575904,
-9.16219631826783));
#360655=CARTESIAN_POINT('Ctrl Pts',(0.828537993751511,1.26619108559502,
-9.18385774487733));
#360656=CARTESIAN_POINT('Ctrl Pts',(0.989258581834231,1.14502990997947,
-9.19495600598836));
#360657=CARTESIAN_POINT('Ctrl Pts',(1.24921069463572,0.852294842000582,
-9.21559448751297));
#360658=CARTESIAN_POINT('Ctrl Pts',(1.34800283882696,0.685435165555885,
-9.22442026858023));
#360659=CARTESIAN_POINT('Ctrl Pts',(1.47787953383756,0.321735217753049,
-9.24462582123595));
#360660=CARTESIAN_POINT('Ctrl Pts',(1.50705635882641,0.128102508318784,
-9.25538319398229));
#360661=CARTESIAN_POINT('Ctrl Pts',(1.48985259088274,-0.264338716780145,
-9.27718548426557));
#360662=CARTESIAN_POINT('Ctrl Pts',(1.4417317848399,-0.459310444280137,
-9.28801724688994));
#360663=CARTESIAN_POINT('Ctrl Pts',(1.2730166596941,-0.817460642341476,
-9.30791448011514));
#360664=CARTESIAN_POINT('Ctrl Pts',(1.15477104626469,-0.977412057057087,
-9.31742472038381));
#360665=CARTESIAN_POINT('Ctrl Pts',(0.863020796908887,-1.24261409236543,
-9.33882828400363));
#360666=CARTESIAN_POINT('Ctrl Pts',(0.692347529270165,-1.3451944222219,
-9.34988925902865));
#360667=CARTESIAN_POINT('Ctrl Pts',(0.343997953858306,-1.47022374519527,
-9.37012227253926));
#360668=CARTESIAN_POINT('Ctrl Pts',(0.172569709406923,-1.5,-9.379197235985));
#360669=CARTESIAN_POINT('Ctrl Pts',(-4.01068067645838E-14,-1.5,-9.38750000000001));
#360670=CARTESIAN_POINT('Origin',(0.,1.30104260698261E-15,-17.7));
#360671=CARTESIAN_POINT('',(-2.19086391586799E-15,-1.5,-9.95));
#360672=CARTESIAN_POINT('',(1.6283941103285E-14,-1.5,-9.8875));
#360673=CARTESIAN_POINT('',(-1.83697019872103E-16,-1.5,-17.7));
#360674=CARTESIAN_POINT('Ctrl Pts',(9.0205620750794E-16,-1.5,-9.95));
#360675=CARTESIAN_POINT('Ctrl Pts',(0.178088883907783,-1.5,-9.94143169457801));
#360676=CARTESIAN_POINT('Ctrl Pts',(0.354890543523405,-1.46828714038846,
-9.93204440799667));
#360677=CARTESIAN_POINT('Ctrl Pts',(0.707188235513081,-1.33748407770702,
-9.91146105898009));
#360678=CARTESIAN_POINT('Ctrl Pts',(0.876901019913129,-1.23289333983374,
-9.90039045055931));
#360679=CARTESIAN_POINT('Ctrl Pts',(1.16531814612726,-0.964683033771861,
-9.87906368882493));
#360680=CARTESIAN_POINT('Ctrl Pts',(1.28146042125905,-0.80400547991937,
-9.86966697110663));
#360681=CARTESIAN_POINT('Ctrl Pts',(1.44356501014691,-0.450686773216476,
-9.85003815406758));
#360682=CARTESIAN_POINT('Ctrl Pts',(1.4893945075153,-0.26207584969327,-9.8395597694274));
#360683=CARTESIAN_POINT('Ctrl Pts',(1.50769287712137,0.129694242943233,
-9.81779476428093));
#360684=CARTESIAN_POINT('Ctrl Pts',(1.47701174301179,0.329254357118478,
-9.80670809127119));
#360685=CARTESIAN_POINT('Ctrl Pts',(1.34219595633325,0.696485874846017,
-9.78630634028633));
#360686=CARTESIAN_POINT('Ctrl Pts',(1.24256584198251,0.861750648578542,
-9.77751212565835));
#360687=CARTESIAN_POINT('Ctrl Pts',(0.981262552504138,1.15186543864246,
-9.75688142110808));
#360688=CARTESIAN_POINT('Ctrl Pts',(0.81982443484921,1.27182850496678,-9.74578191859663));
#360689=CARTESIAN_POINT('Ctrl Pts',(0.466363054652606,1.43848111664446,
-9.72414676079964));
#360690=CARTESIAN_POINT('Ctrl Pts',(0.278941091517629,1.486248760098,-9.71380253840915));
#360691=CARTESIAN_POINT('Ctrl Pts',(-0.110776066338477,1.50904249147282,
-9.69441910370462));
#360692=CARTESIAN_POINT('Ctrl Pts',(-0.309494515954199,1.48112142747415,
-9.68458503336604));
#360693=CARTESIAN_POINT('Ctrl Pts',(-0.682591741918069,1.35009195881611,
-9.66299467724964));
#360694=CARTESIAN_POINT('Ctrl Pts',(-0.853538502154639,1.24906072552042,
-9.6519635742659));
#360695=CARTESIAN_POINT('Ctrl Pts',(-1.14168220498132,0.991282903465424,
-9.63093975884279));
#360696=CARTESIAN_POINT('Ctrl Pts',(-1.25787602833459,0.838930564299269,
-9.62160725357218));
#360697=CARTESIAN_POINT('Ctrl Pts',(-1.43125415993856,0.490979030161277,
-9.60227661278674));
#360698=CARTESIAN_POINT('Ctrl Pts',(-1.4836561814186,0.297137277323276,
-9.59150762651796));
#360699=CARTESIAN_POINT('Ctrl Pts',(-1.50954408604807,-0.0952173356098048,
-9.56971014802168));
#360700=CARTESIAN_POINT('Ctrl Pts',(-1.48451466629367,-0.289856099442056,
-9.55889688336433));
#360701=CARTESIAN_POINT('Ctrl Pts',(-1.36248851592326,-0.655967083629947,
-9.53855738424278));
#360702=CARTESIAN_POINT('Ctrl Pts',(-1.2677308612976,-0.824333298495162,
-9.52976224898876));
#360703=CARTESIAN_POINT('Ctrl Pts',(-1.01462826501303,-1.122691452766,-9.50929711813978));
#360704=CARTESIAN_POINT('Ctrl Pts',(-0.856271298649763,-1.24767507522504,
-9.49820639775275));
#360705=CARTESIAN_POINT('Ctrl Pts',(-0.506712953658665,-1.42483897430644,
-9.47646704461899));
#360706=CARTESIAN_POINT('Ctrl Pts',(-0.320184146078453,-1.47798021095492,
-9.46601652771752));
#360707=CARTESIAN_POINT('Ctrl Pts',(-0.0858209378369455,-1.4981608111566,
-9.45418015037584));
#360708=CARTESIAN_POINT('Ctrl Pts',(-0.0428867375032626,-1.49999999999999,
-9.45206338912018));
#360709=CARTESIAN_POINT('Ctrl Pts',(-2.47579081706926E-13,-1.5,-9.45000000000001));
#360710=CARTESIAN_POINT('Ctrl Pts',(-3.30985239216378E-14,-1.5,-9.38750000000001));
#360711=CARTESIAN_POINT('Ctrl Pts',(-0.0171879221613554,-1.5,-9.38832695429056));
#360712=CARTESIAN_POINT('Ctrl Pts',(-0.0343863909262785,-1.49970457697492,
-9.38916262219996));
#360713=CARTESIAN_POINT('Ctrl Pts',(-0.250311720287671,-1.49227409270073,
-9.39975773679355));
#360714=CARTESIAN_POINT('Ctrl Pts',(-0.445672776424722,-1.44599066373983,
-9.41044270079384));
#360715=CARTESIAN_POINT('Ctrl Pts',(-0.803397413409704,-1.28161610511915,
-9.43221969537712));
#360716=CARTESIAN_POINT('Ctrl Pts',(-0.962961932043072,-1.16649051245719,
-9.44309467998879));
#360717=CARTESIAN_POINT('Ctrl Pts',(-1.22631205474749,-0.884630222891906,
-9.46359457116292));
#360718=CARTESIAN_POINT('Ctrl Pts',(-1.32876836835458,-0.721653146130807,
-9.47240815854829));
#360719=CARTESIAN_POINT('Ctrl Pts',(-1.47057152631181,-0.357136234696439,
-9.49265909807242));
#360720=CARTESIAN_POINT('Ctrl Pts',(-1.50506196885152,-0.15779718640125,
-9.50373348964438));
#360721=CARTESIAN_POINT('Ctrl Pts',(-1.49395509078595,0.234965830650891,
-9.52555365725838));
#360722=CARTESIAN_POINT('Ctrl Pts',(-1.45146365973432,0.424713455348534,
-9.53609519196381));
#360723=CARTESIAN_POINT('Ctrl Pts',(-1.29592806047573,0.780212191090157,
-9.55584512172724));
#360724=CARTESIAN_POINT('Ctrl Pts',(-1.18343171231967,0.942156962082107,
-9.56506647525157));
#360725=CARTESIAN_POINT('Ctrl Pts',(-0.900853795573068,1.21556403974649,
-9.58625665265619));
#360726=CARTESIAN_POINT('Ctrl Pts',(-0.732871823156846,1.32364199490675,
-9.59734085449343));
#360727=CARTESIAN_POINT('Ctrl Pts',(-0.3714565780336,1.46571489439951,-9.61867592301221));
#360728=CARTESIAN_POINT('Ctrl Pts',(-0.182540101167985,1.50097459620851,
-9.62869046317083));
#360729=CARTESIAN_POINT('Ctrl Pts',(0.20664431190765,1.49894039450732,-9.64747161257811));
#360730=CARTESIAN_POINT('Ctrl Pts',(0.403235829399321,1.45838890762508,
-9.65805655656464));
#360731=CARTESIAN_POINT('Ctrl Pts',(0.766086052666307,1.30434472367595,
-9.67979320118089));
#360732=CARTESIAN_POINT('Ctrl Pts',(0.929355839681309,1.19352709430535,
-9.69072678995371));
#360733=CARTESIAN_POINT('Ctrl Pts',(1.200561091853,0.919167994853228,-9.71139624482852));
#360734=CARTESIAN_POINT('Ctrl Pts',(1.30735135435701,0.759632901639449,
-9.72029817213114));
#360735=CARTESIAN_POINT('Ctrl Pts',(1.45975713369087,0.399342269902501,
-9.74031431833875));
#360736=CARTESIAN_POINT('Ctrl Pts',(1.50005236242994,0.200474510687348,
-9.75136252718404));
#360737=CARTESIAN_POINT('Ctrl Pts',(1.49994954594571,-0.193552388316353,
-9.77325291046203));
#360738=CARTESIAN_POINT('Ctrl Pts',(1.46258844278961,-0.384917892848863,
-9.7838843273805));
#360739=CARTESIAN_POINT('Ctrl Pts',(1.31703360372687,-0.743666104827207,
-9.80381478360152));
#360740=CARTESIAN_POINT('Ctrl Pts',(1.20996724864347,-0.907524756776458,
-9.81282777796199));
#360741=CARTESIAN_POINT('Ctrl Pts',(0.93622857431212,-1.18862962920031,
-9.83380650474984));
#360742=CARTESIAN_POINT('Ctrl Pts',(0.770980617984793,-1.30190105127316,
-9.84490342914647));
#360743=CARTESIAN_POINT('Ctrl Pts',(0.412865291114638,-1.45464829026131,
-9.8663762397047));
#360744=CARTESIAN_POINT('Ctrl Pts',(0.224503174727305,-1.49535315172199,
-9.87656950685095));
#360745=CARTESIAN_POINT('Ctrl Pts',(0.0223606200870313,-1.49987505737306,
-9.88642070353594));
#360746=CARTESIAN_POINT('Ctrl Pts',(0.0111777862199557,-1.5,-9.88696220850975));
#360747=CARTESIAN_POINT('Ctrl Pts',(3.27515792264421E-14,-1.5,-9.8875));
#360748=CARTESIAN_POINT('Origin',(0.,1.30104260698261E-15,-17.7));
#360749=CARTESIAN_POINT('',(1.63031148958116E-14,-1.5,-10.45));
#360750=CARTESIAN_POINT('',(1.15223986389916E-13,-1.5,-10.3875));
#360751=CARTESIAN_POINT('',(-1.83697019872103E-16,-1.5,-17.7));
#360752=CARTESIAN_POINT('Ctrl Pts',(3.27899268114953E-14,-1.5,-10.45));
#360753=CARTESIAN_POINT('Ctrl Pts',(0.01800321797007,-1.5,-10.4491338197716));
#360754=CARTESIAN_POINT('Ctrl Pts',(0.036018717336121,-1.49967588627835,
-10.4482580454952));
#360755=CARTESIAN_POINT('Ctrl Pts',(0.245176324002544,-1.49213603731342,
-10.4379855052036));
#360756=CARTESIAN_POINT('Ctrl Pts',(0.433213044337886,-1.44875303070621,
-10.4277335007614));
#360757=CARTESIAN_POINT('Ctrl Pts',(0.789626966193958,-1.29072102809195,
-10.4061957501005));
#360758=CARTESIAN_POINT('Ctrl Pts',(0.953462163785975,-1.17489982808324,
-10.3950959699253));
#360759=CARTESIAN_POINT('Ctrl Pts',(1.22279469101575,-0.890029900886932,
-10.3742246491339));
#360760=CARTESIAN_POINT('Ctrl Pts',(1.32719200334045,-0.725215812482133,
-10.3652897673601));
#360761=CARTESIAN_POINT('Ctrl Pts',(1.4677522320276,-0.364869843745343,
-10.3452705468747));
#360762=CARTESIAN_POINT('Ctrl Pts',(1.50252159412429,-0.172745227268556,
-10.3345969570705));
#360763=CARTESIAN_POINT('Ctrl Pts',(1.49711892910183,0.219503631488235,
-10.3128053538062));
#360764=CARTESIAN_POINT('Ctrl Pts',(1.45486376302284,0.415856788035936,
-10.3018968451091));
#360765=CARTESIAN_POINT('Ctrl Pts',(1.29968754567509,0.772639620470973,
-10.2820755766405));
#360766=CARTESIAN_POINT('Ctrl Pts',(1.19139079377124,0.930997563987972,
-10.2731264395137));
#360767=CARTESIAN_POINT('Ctrl Pts',(0.91745975897177,1.20272674065901,-10.2523988937717));
#360768=CARTESIAN_POINT('Ctrl Pts',(0.752924634535686,1.31201491874155,
-10.2414469111818));
#360769=CARTESIAN_POINT('Ctrl Pts',(0.388240902110138,1.46246727905665,
-10.2197218246937));
#360770=CARTESIAN_POINT('Ctrl Pts',(0.191231504278741,1.50097064803793,
-10.2092275924849));
#360771=CARTESIAN_POINT('Ctrl Pts',(-0.198141883730837,1.49903212712652,
-10.1904400088166));
#360772=CARTESIAN_POINT('Ctrl Pts',(-0.386863356846977,1.46173524340097,
-10.1803241181599));
#360773=CARTESIAN_POINT('Ctrl Pts',(-0.747032332294729,1.31573401601126,
-10.1589398905994));
#360774=CARTESIAN_POINT('Ctrl Pts',(-0.914021954701355,1.2057289890355,
-10.1478499034516));
#360775=CARTESIAN_POINT('Ctrl Pts',(-1.19334053336476,0.929460378453624,
-10.1267370539982));
#360776=CARTESIAN_POINT('Ctrl Pts',(-1.30382251768123,0.766809790070398,
-10.1176005438928));
#360777=CARTESIAN_POINT('Ctrl Pts',(-1.45568345644507,0.41010588820822,
-10.097783660456));
#360778=CARTESIAN_POINT('Ctrl Pts',(-1.49629394058661,0.219747119591232,
-10.0872081733106));
#360779=CARTESIAN_POINT('Ctrl Pts',(-1.50335959946284,-0.17351577030611,
-10.065360234983));
#360780=CARTESIAN_POINT('Ctrl Pts',(-1.4667340049793,-0.372700342129076,
-10.0542944254373));
#360781=CARTESIAN_POINT('Ctrl Pts',(-1.32102533310306,-0.735675355437794,
-10.0341291469201));
#360782=CARTESIAN_POINT('Ctrl Pts',(-1.21697939084774,-0.897380503251673,
-10.0252913787072));
#360783=CARTESIAN_POINT('Ctrl Pts',(-0.950746497495352,-1.17650109767429,
-10.0047288928085));
#360784=CARTESIAN_POINT('Ctrl Pts',(-0.789812328683005,-1.29006299093454,
-9.99383144696635));
#360785=CARTESIAN_POINT('Ctrl Pts',(-0.430176479334777,-1.45067426469028,
-9.97206703482607));
#360786=CARTESIAN_POINT('Ctrl Pts',(-0.234344862574323,-1.49486307251423,
-9.9614176148877));
#360787=CARTESIAN_POINT('Ctrl Pts',(-0.0237105811411076,-1.49985951562273,
-9.95114467821085));
#360788=CARTESIAN_POINT('Ctrl Pts',(-0.0118526244172869,-1.5,-9.95057025965816));
#360789=CARTESIAN_POINT('Ctrl Pts',(-1.83697019872103E-16,-1.5,-9.95));
#360790=CARTESIAN_POINT('Ctrl Pts',(3.30985239216375E-14,-1.5,-9.8875));
#360791=CARTESIAN_POINT('Ctrl Pts',(-0.187391350651986,-1.5,-9.8965158705619));
#360792=CARTESIAN_POINT('Ctrl Pts',(-0.373271716031661,-1.46488681977112,
-9.90643440992845));
#360793=CARTESIAN_POINT('Ctrl Pts',(-0.730415627561203,-1.32472660344816,
-9.92751084372584));
#360794=CARTESIAN_POINT('Ctrl Pts',(-0.897065962568103,-1.21806574589348,
-9.93849161330598));
#360795=CARTESIAN_POINT('Ctrl Pts',(-1.17560811243111,-0.950818237745173,
-9.95931652063266));
#360796=CARTESIAN_POINT('Ctrl Pts',(-1.28645814636411,-0.794432345547403,
-9.96836486969182));
#360797=CARTESIAN_POINT('Ctrl Pts',(-1.44759303621033,-0.440494147717617,
-9.98802810290458));
#360798=CARTESIAN_POINT('Ctrl Pts',(-1.49317264952211,-0.244900486810878,
-9.9988944173994));
#360799=CARTESIAN_POINT('Ctrl Pts',(-1.50525018136636,0.147501105949109,
-10.0206945058861));
#360800=CARTESIAN_POINT('Ctrl Pts',(-1.47363789770394,0.340498678165481,
-10.0314165932314));
#360801=CARTESIAN_POINT('Ctrl Pts',(-1.33912346631036,0.702753338863711,
-10.0515418521591));
#360802=CARTESIAN_POINT('Ctrl Pts',(-1.23791519188803,0.868724225890744,
-10.0604053393911));
#360803=CARTESIAN_POINT('Ctrl Pts',(-0.973898850623588,1.15807608173006,
-10.0811453830838));
#360804=CARTESIAN_POINT('Ctrl Pts',(-0.811811210270145,1.27693851831173,
-10.0922455626658));
#360805=CARTESIAN_POINT('Ctrl Pts',(-0.457542083654513,1.44129593240477,
-10.1138558276921));
#360806=CARTESIAN_POINT('Ctrl Pts',(-0.269946185863268,1.48789423348432,
-10.124175936785));
#360807=CARTESIAN_POINT('Ctrl Pts',(0.120218128411184,1.50837654819066,
-10.1435166792942));
#360808=CARTESIAN_POINT('Ctrl Pts',(0.319199220425388,1.47911929755378,
-10.1534374991655));
#360809=CARTESIAN_POINT('Ctrl Pts',(0.691681259174506,1.34543867622126,
-10.1750719002031));
#360810=CARTESIAN_POINT('Ctrl Pts',(0.861831633536728,1.24333257808737,
-10.1860945444102));
#360811=CARTESIAN_POINT('Ctrl Pts',(1.1481697352069,0.983759282179983,-10.2070813620809));
#360812=CARTESIAN_POINT('Ctrl Pts',(1.26335525816127,0.830655508701343,
-10.2163524717388));
#360813=CARTESIAN_POINT('Ctrl Pts',(1.43444753592443,0.481571973138974,
-10.2357460014923));
#360814=CARTESIAN_POINT('Ctrl Pts',(1.48557727677494,0.287383561155462,
-10.2465342466025));
#360815=CARTESIAN_POINT('Ctrl Pts',(1.50887812224303,-0.105017066405158,
-10.268334281467));
#360816=CARTESIAN_POINT('Ctrl Pts',(1.48261031635569,-0.29936531384347,
-10.2791314063246));
#360817=CARTESIAN_POINT('Ctrl Pts',(1.35824595797596,-0.66476252932804,
-10.2994312516293));
#360818=CARTESIAN_POINT('Ctrl Pts',(1.26229343677386,-0.832680156076931,
-10.3082312163757));
#360819=CARTESIAN_POINT('Ctrl Pts',(1.00715502141771,-1.12937665709337,
-10.3287481385806));
#360820=CARTESIAN_POINT('Ctrl Pts',(0.848087752530656,-1.25323088458357,
-10.3398416613312));
#360821=CARTESIAN_POINT('Ctrl Pts',(0.497619683529373,-1.42802417610503,
-10.3615589333718));
#360822=CARTESIAN_POINT('Ctrl Pts',(0.31087547433655,-1.47995085278223,
-10.3719860760112));
#360823=CARTESIAN_POINT('Ctrl Pts',(0.0796161717872997,-1.49841710025498,
-10.3836254957115));
#360824=CARTESIAN_POINT('Ctrl Pts',(0.0397864392775881,-1.5,-10.3855857740478));
#360825=CARTESIAN_POINT('Ctrl Pts',(2.30631669799704E-13,-1.5,-10.3875));
#360826=CARTESIAN_POINT('Origin',(0.,1.30104260698261E-15,-17.7));
#360827=CARTESIAN_POINT('',(1.317107983056E-13,-1.5,-10.95));
#360828=CARTESIAN_POINT('',(5.75201446850214E-14,-1.5,-10.8875));
#360829=CARTESIAN_POINT('',(-1.83697019872103E-16,-1.5,-17.7));
#360830=CARTESIAN_POINT('Ctrl Pts',(2.63605293631073E-13,-1.5,-10.95));
#360831=CARTESIAN_POINT('Ctrl Pts',(0.0448692205490244,-1.5,-10.9478412286198));
#360832=CARTESIAN_POINT('Ctrl Pts',(0.0897883947290352,-1.49798685366247,
-10.9456241331128));
#360833=CARTESIAN_POINT('Ctrl Pts',(0.326130241143317,-1.47668935698625,
-10.9336615335956));
#360834=CARTESIAN_POINT('Ctrl Pts',(0.512517207445259,-1.42277176749051,
-10.9231962756789));
#360835=CARTESIAN_POINT('Ctrl Pts',(0.861485590365093,-1.24409415842851,
-10.9014432596091));
#360836=CARTESIAN_POINT('Ctrl Pts',(1.0193842596546,-1.11839026997729,-10.8903545816616));
#360837=CARTESIAN_POINT('Ctrl Pts',(1.27118292100986,-0.818972364535948,
-10.8699227488787));
#360838=CARTESIAN_POINT('Ctrl Pts',(1.36517744621195,-0.650317979971595,
-10.8611287766651));
#360839=CARTESIAN_POINT('Ctrl Pts',(1.48570385405768,-0.283751401839029,
-10.8407639667688));
#360840=CARTESIAN_POINT('Ctrl Pts',(1.50993769550051,-0.0889304081784544,
-10.8299405782321));
#360841=CARTESIAN_POINT('Ctrl Pts',(1.48239044708045,0.303385663179708,
-10.8081452409345));
#360842=CARTESIAN_POINT('Ctrl Pts',(1.42917377802666,0.497000591068319,
-10.7973888560518));
#360843=CARTESIAN_POINT('Ctrl Pts',(1.25433111678225,0.844223459760498,
-10.77809869668));
#360844=CARTESIAN_POINT('Ctrl Pts',(1.13748859571032,0.996094699681933,
-10.7687248150311));
#360845=CARTESIAN_POINT('Ctrl Pts',(0.848184943334172,1.25271538512326,
-10.747677334193));
#360846=CARTESIAN_POINT('Ctrl Pts',(0.676729486327462,1.35305218831829,
-10.7366410462495));
#360847=CARTESIAN_POINT('Ctrl Pts',(0.303241548629432,1.48237719193206,
-10.7150792382572));
#360848=CARTESIAN_POINT('Ctrl Pts',(0.104691386215296,1.5094409775268,-10.7052992160435));
#360849=CARTESIAN_POINT('Ctrl Pts',(-0.284735860779223,1.48515889892904,
-10.6858883867034));
#360850=CARTESIAN_POINT('Ctrl Pts',(-0.472041837113309,1.43663743886913,
-10.6755288053803));
#360851=CARTESIAN_POINT('Ctrl Pts',(-0.82497464331873,1.26850671189686,
-10.6538780198531));
#360852=CARTESIAN_POINT('Ctrl Pts',(-0.985990085787427,1.14783565807325,
-10.6427791870481));
#360853=CARTESIAN_POINT('Ctrl Pts',(-1.2468121626535,0.855821697819146,
-10.622118880128));
#360854=CARTESIAN_POINT('Ctrl Pts',(-1.34611994644716,0.689152655142687,
-10.613286258619));
#360855=CARTESIAN_POINT('Ctrl Pts',(-1.47699056819011,0.325761067320561,
-10.5930978370734));
#360856=CARTESIAN_POINT('Ctrl Pts',(-1.50669029213086,0.13226193594449,
-10.5823478853302));
#360857=CARTESIAN_POINT('Ctrl Pts',(-1.49058546546239,-0.260176469562684,
-10.560545751691));
#360858=CARTESIAN_POINT('Ctrl Pts',(-1.4430085552882,-0.455284347048996,
-10.5497064251639));
#360859=CARTESIAN_POINT('Ctrl Pts',(-1.27829239399112,-0.807490951113278,
-10.5301393916048));
#360860=CARTESIAN_POINT('Ctrl Pts',(-1.16589334752476,-0.962694609105648,
-10.5210192195837));
#360861=CARTESIAN_POINT('Ctrl Pts',(-0.884560332267287,-1.22720912557693,
-10.5001359531186));
#360862=CARTESIAN_POINT('Ctrl Pts',(-0.716645770489744,-1.33225560479891,
-10.4891392022422));
#360863=CARTESIAN_POINT('Ctrl Pts',(-0.362775121859122,-1.46685847888272,
-10.4683746239972));
#360864=CARTESIAN_POINT('Ctrl Pts',(-0.182059082850492,-1.5,-10.4587593217077));
#360865=CARTESIAN_POINT('Ctrl Pts',(3.46944695195361E-14,-1.5,-10.45));
#360866=CARTESIAN_POINT('Ctrl Pts',(2.30631669799704E-13,-1.5,-10.3875));
#360867=CARTESIAN_POINT('Ctrl Pts',(-0.156867334913038,-1.5,-10.3950472831699));
#360868=CARTESIAN_POINT('Ctrl Pts',(-0.312996144541852,-1.47539873316522,
-10.4032424025487));
#360869=CARTESIAN_POINT('Ctrl Pts',(-0.650223892518879,-1.36604243343655,
-10.4225049551306));
#360870=CARTESIAN_POINT('Ctrl Pts',(-0.823931750309691,-1.26885709450723,
-10.4335620710833));
#360871=CARTESIAN_POINT('Ctrl Pts',(-1.11843697167113,-1.01746168046079,
-10.4547146660983));
#360872=CARTESIAN_POINT('Ctrl Pts',(-1.23819841939332,-0.867732857684848,
-10.4642926190175));
#360873=CARTESIAN_POINT('Ctrl Pts',(-1.41957125919433,-0.523791050021272,
-10.483400497221));
#360874=CARTESIAN_POINT('Ctrl Pts',(-1.47641469054851,-0.331232362429373,
-10.4940982020873));
#360875=CARTESIAN_POINT('Ctrl Pts',(-1.51137640912421,0.0608252823475351,
-10.5158791823526));
#360876=CARTESIAN_POINT('Ctrl Pts',(-1.49070968039528,0.256421290917001,
-10.5267456272732));
#360877=CARTESIAN_POINT('Ctrl Pts',(-1.37688636532436,0.625002839747036,
-10.5472223799859));
#360878=CARTESIAN_POINT('Ctrl Pts',(-1.28627223103907,0.794950005365961,
-10.5560294763567));
#360879=CARTESIAN_POINT('Ctrl Pts',(-1.0402832110233,1.09904761991128,-10.57631178456));
#360880=CARTESIAN_POINT('Ctrl Pts',(-0.884457742076792,1.22793088704675,
-10.587389031684));
#360881=CARTESIAN_POINT('Ctrl Pts',(-0.538186167339719,1.41330793124745,
-10.6091983929301));
#360882=CARTESIAN_POINT('Ctrl Pts',(-0.352467598787901,1.4706692453251,
-10.6197271515612));
#360883=CARTESIAN_POINT('Ctrl Pts',(0.0334616791587361,1.51232318565235,
-10.6394522365017));
#360884=CARTESIAN_POINT('Ctrl Pts',(0.230106048856906,1.49509292939401,
-10.6487072899543));
#360885=CARTESIAN_POINT('Ctrl Pts',(0.607853032724975,1.38550236547394,
-10.6699258325206));
#360886=CARTESIAN_POINT('Ctrl Pts',(0.785003725931987,1.29339373943508,
-10.681007572167));
#360887=CARTESIAN_POINT('Ctrl Pts',(1.08768672851293,1.05033904654925,-10.7023219341654));
#360888=CARTESIAN_POINT('Ctrl Pts',(1.21207525087308,0.903933814333612,
-10.7122814547593));
#360889=CARTESIAN_POINT('Ctrl Pts',(1.40359638285787,0.565193125659586,
-10.7311003819078));
#360890=CARTESIAN_POINT('Ctrl Pts',(1.46605202366308,0.374420850721505,
-10.7416988416266));
#360891=CARTESIAN_POINT('Ctrl Pts',(1.51257644147676,-0.0169523031762115,
-10.7634417946209));
#360892=CARTESIAN_POINT('Ctrl Pts',(1.49751265962048,-0.213628692405403,
-10.7743682606892));
#360893=CARTESIAN_POINT('Ctrl Pts',(1.39415801382123,-0.585286893574757,
-10.7950159385319));
#360894=CARTESIAN_POINT('Ctrl Pts',(1.3087285026964,-0.757271802011755,
-10.803902431723));
#360895=CARTESIAN_POINT('Ctrl Pts',(1.07174988329698,-1.06849726548678,
-10.8239492226281));
#360896=CARTESIAN_POINT('Ctrl Pts',(0.919237776017449,-1.20221397668855,
-10.8350013178997));
#360897=CARTESIAN_POINT('Ctrl Pts',(0.577364012719776,-1.39783262154744,
-10.8568835782515));
#360898=CARTESIAN_POINT('Ctrl Pts',(0.392797634352501,-1.46048316846745,
-10.867503825241));
#360899=CARTESIAN_POINT('Ctrl Pts',(0.134513137431451,-1.49548113240844,
-10.8809027095581));
#360900=CARTESIAN_POINT('Ctrl Pts',(0.0672263389796428,-1.5,-10.8842655712578));
#360901=CARTESIAN_POINT('Ctrl Pts',(1.15223986389915E-13,-1.5,-10.8875));
#360902=CARTESIAN_POINT('Origin',(0.,1.30104260698261E-15,-17.7));
#360903=CARTESIAN_POINT('',(3.27899268114954E-14,-1.5,-11.45));
#360904=CARTESIAN_POINT('',(3.91179454725655E-8,-1.5,-11.3874999962359));
#360905=CARTESIAN_POINT('',(-1.83697019872103E-16,-1.5,-17.7));
#360906=CARTESIAN_POINT('Ctrl Pts',(6.5763550642863E-14,-1.5,-11.45));
#360907=CARTESIAN_POINT('Ctrl Pts',(0.0740159308911273,-1.5,-11.4464389068646));
#360908=CARTESIAN_POINT('Ctrl Pts',(0.148085783009549,-1.49452238116345,
-11.4427230633642));
#360909=CARTESIAN_POINT('Ctrl Pts',(0.412883068505858,-1.45496702756496,
-11.4288842382035));
#360910=CARTESIAN_POINT('Ctrl Pts',(0.596816517544713,-1.38967503608798,
-11.4182210695807));
#360911=CARTESIAN_POINT('Ctrl Pts',(0.934465047856721,-1.19009377843804,
-11.3964320232681));
#360912=CARTESIAN_POINT('Ctrl Pts',(1.08386040428747,-1.05584703782725,
-11.3855151597025));
#360913=CARTESIAN_POINT('Ctrl Pts',(1.3163827898316,-0.743849748068237,
-11.3656613298297));
#360914=CARTESIAN_POINT('Ctrl Pts',(1.39999632380265,-0.571134425145102,
-11.3567296902858));
#360915=CARTESIAN_POINT('Ctrl Pts',(1.49963117977393,-0.198403894113652,
-11.3360224385619));
#360916=CARTESIAN_POINT('Ctrl Pts',(1.51269633696756,-0.00138204992871142,
-11.3250767805516));
#360917=CARTESIAN_POINT('Ctrl Pts',(1.46205695157743,0.38978071904039,-11.3033455156089));
#360918=CARTESIAN_POINT('Ctrl Pts',(1.39757861373038,0.579872013608144,
-11.2928001431373));
#360919=CARTESIAN_POINT('Ctrl Pts',(1.20246123135251,0.916743535558502,
-11.2740550114243));
#360920=CARTESIAN_POINT('Ctrl Pts',(1.07637641317381,1.06194208376696,-11.2639554597755));
#360921=CARTESIAN_POINT('Ctrl Pts',(0.770855479402225,1.30190841028484,
-11.2425903457037));
#360922=CARTESIAN_POINT('Ctrl Pts',(0.59250422151623,1.39216640819344,-11.2315022501992));
#360923=CARTESIAN_POINT('Ctrl Pts',(0.213885504663574,1.49742599847879,
-11.2103620711834));
#360924=CARTESIAN_POINT('Ctrl Pts',(0.0176462582822069,1.51251835619341,
-11.2011967381139));
#360925=CARTESIAN_POINT('Ctrl Pts',(-0.367479610380647,1.46701539997117,
-11.1814033901124));
#360926=CARTESIAN_POINT('Ctrl Pts',(-0.552787639076062,1.40768754034473,
-11.1708397573241));
#360927=CARTESIAN_POINT('Ctrl Pts',(-0.897460445162141,1.2184958232013,
-11.1490013537333));
#360928=CARTESIAN_POINT('Ctrl Pts',(-1.05207235524188,1.08780840341489,
-11.137932378636));
#360929=CARTESIAN_POINT('Ctrl Pts',(-1.29472412660984,0.781052781557282,
-11.1177368003468));
#360930=CARTESIAN_POINT('Ctrl Pts',(-1.3834101935851,0.610355838142167,
-11.1089086576746));
#360931=CARTESIAN_POINT('Ctrl Pts',(-1.49336680388985,0.240627863692861,
-11.0883682146496));
#360932=CARTESIAN_POINT('Ctrl Pts',(-1.51196816894718,0.0446142718790937,
-11.0774785706599));
#360933=CARTESIAN_POINT('Ctrl Pts',(-1.47273239710866,-0.347230352946177,
-11.0557094248363));
#360934=CARTESIAN_POINT('Ctrl Pts',(-1.4138082514145,-0.539148472729819,
-11.0450473070706));
#360935=CARTESIAN_POINT('Ctrl Pts',(-1.22867993426292,-0.881179913042688,
-11.0260455603865));
#360936=CARTESIAN_POINT('Ctrl Pts',(-1.10721948916014,-1.02967824115973,
-11.016335615811));
#360937=CARTESIAN_POINT('Ctrl Pts',(-0.809701240101673,-1.27801893022418,
-10.9951229099051));
#360938=CARTESIAN_POINT('Ctrl Pts',(-0.634710650244654,-1.37335103067755,
-10.9840555573236));
#360939=CARTESIAN_POINT('Ctrl Pts',(-0.30154176022217,-1.47717946544105,
-10.9651418384408));
#360940=CARTESIAN_POINT('Ctrl Pts',(-0.151084567659519,-1.5,-10.9572690596507));
#360941=CARTESIAN_POINT('Ctrl Pts',(2.63605293631073E-13,-1.5,-10.95));
#360942=CARTESIAN_POINT('Ctrl Pts',(1.16087695012368E-13,-1.5,-10.8875));
#360943=CARTESIAN_POINT('Ctrl Pts',(-0.12607676064798,-1.5,-10.8935658709749));
#360944=CARTESIAN_POINT('Ctrl Pts',(-0.25189800249301,-1.48410901447996,
-10.9000608645601));
#360945=CARTESIAN_POINT('Ctrl Pts',(-0.566554888468781,-1.40297903034609,
-10.9174534117155));
#360946=CARTESIAN_POINT('Ctrl Pts',(-0.746880905326093,-1.31586358480684,
-10.9285492247339));
#360947=CARTESIAN_POINT('Ctrl Pts',(-1.05724907259812,-1.08104490954594,
-10.9500045611236));
#360948=CARTESIAN_POINT('Ctrl Pts',(-1.18612043822808,-0.937856887421639,
-10.9601823326524));
#360949=CARTESIAN_POINT('Ctrl Pts',(-1.38728387069208,-0.604106562997156,
-10.9791316551545));
#360950=CARTESIAN_POINT('Ctrl Pts',(-1.45506683222575,-0.415127521990897,
-10.9894373598894));
#360951=CARTESIAN_POINT('Ctrl Pts',(-1.51254045432257,-0.0245493613436996,
-11.011136146592));
#360952=CARTESIAN_POINT('Ctrl Pts',(-1.50281578535621,0.173003596323905,
-11.0221113109069));
#360953=CARTESIAN_POINT('Ctrl Pts',(-1.40938478588014,0.547497830146236,
-11.0429165461192));
#360954=CARTESIAN_POINT('Ctrl Pts',(-1.3287711275756,0.721439543544025,
-11.0519427899709));
#360955=CARTESIAN_POINT('Ctrl Pts',(-1.10171477651428,1.03720116470672,
-11.0716381998982));
#360956=CARTESIAN_POINT('Ctrl Pts',(-0.954641944826474,1.17396799633267,
-11.0825133234683));
#360957=CARTESIAN_POINT('Ctrl Pts',(-0.62019323119029,1.37944559625263,
-11.1043122058145));
#360958=CARTESIAN_POINT('Ctrl Pts',(-0.437075268034176,1.44792561276039,
-11.1150246956054));
#360959=CARTESIAN_POINT('Ctrl Pts',(-0.055816838742389,1.51130709733111,
-11.1351285971309));
#360960=CARTESIAN_POINT('Ctrl Pts',(0.138640459998841,1.50597001067819,
-11.1440045086118));
#360961=CARTESIAN_POINT('Ctrl Pts',(0.520991754899377,1.42061906677836,
-11.1647712534176));
#360962=CARTESIAN_POINT('Ctrl Pts',(0.704622020668317,1.33906284634774,
-11.1758716192662));
#360963=CARTESIAN_POINT('Ctrl Pts',(1.02321105261424,1.1134153046469,-11.1974677284819));
#360964=CARTESIAN_POINT('Ctrl Pts',(1.15684899515003,0.973846282386629,
-11.207774304275));
#360965=CARTESIAN_POINT('Ctrl Pts',(1.36868058691161,0.645339360696826,
-11.2270912487547));
#360966=CARTESIAN_POINT('Ctrl Pts',(1.44226174592408,0.457888647055234,
-11.2370617418303));
#360967=CARTESIAN_POINT('Ctrl Pts',(1.51128132170044,0.0680317382552205,
-11.2587204589858));
#360968=CARTESIAN_POINT('Ctrl Pts',(1.50719160437547,-0.130287409999096,
-11.2697381894444));
#360969=CARTESIAN_POINT('Ctrl Pts',(1.42419767371233,-0.507677808311096,
-11.290704322684));
#360970=CARTESIAN_POINT('Ctrl Pts',(1.34855478158873,-0.683707597950999,
-11.2999428388736));
#360971=CARTESIAN_POINT('Ctrl Pts',(1.13060284376123,-1.00562906491852,
-11.3193713193429));
#360972=CARTESIAN_POINT('Ctrl Pts',(0.987476097404956,-1.14648231893667,
-11.330170098527));
#360973=CARTESIAN_POINT('Ctrl Pts',(0.658560520626497,-1.36162150541419,
-11.3519711451064));
#360974=CARTESIAN_POINT('Ctrl Pts',(0.4769145726165,-1.43536720848172,-11.3627590816067));
#360975=CARTESIAN_POINT('Ctrl Pts',(0.191716665583194,-1.49081159186927,
-11.3780207940673));
#360976=CARTESIAN_POINT('Ctrl Pts',(0.0958654997424546,-1.49999999749403,
-11.3828876689235));
#360977=CARTESIAN_POINT('Ctrl Pts',(3.92107660876271E-8,-1.5,-11.3874999981135));
#360978=CARTESIAN_POINT('Origin',(0.,1.30104260698261E-15,-17.7));
#360979=CARTESIAN_POINT('',(-7.75932627375354E-15,-1.5,-11.95));
#360980=CARTESIAN_POINT('',(-5.78875387247644E-14,-1.5,-11.8875));
#360981=CARTESIAN_POINT('',(-1.83697019872103E-16,-1.5,-17.7));
#360982=CARTESIAN_POINT('Ctrl Pts',(-1.69829428298129E-14,-1.5,-11.95));
#360983=CARTESIAN_POINT('Ctrl Pts',(0.100881833600506,-1.5,-11.9451463205179));
#360984=CARTESIAN_POINT('Ctrl Pts',(0.201721389943112,-1.48982502247338,
-11.9400120368366));
#360985=CARTESIAN_POINT('Ctrl Pts',(0.491473166153889,-1.43047394711926,
-11.9244227070218));
#360986=CARTESIAN_POINT('Ctrl Pts',(0.672540326423178,-1.3547990422388,
-11.9136090285204));
#360987=CARTESIAN_POINT('Ctrl Pts',(0.999350570959909,-1.13614461453851,
-11.8918116291962));
#360988=CARTESIAN_POINT('Ctrl Pts',(1.140997017159,-0.993818203206639,-11.8810431499501));
#360989=CARTESIAN_POINT('Ctrl Pts',(1.35558757929163,-0.669655885635057,
-11.8617141478942));
#360990=CARTESIAN_POINT('Ctrl Pts',(1.42940163132548,-0.492839924587643,
-11.8523799958104));
#360991=CARTESIAN_POINT('Ctrl Pts',(1.50850787934159,-0.114393961960379,
-11.8313552201089));
#360992=CARTESIAN_POINT('Ctrl Pts',(1.51049547604303,0.0841697409274456,
-11.8203239032818));
#360993=CARTESIAN_POINT('Ctrl Pts',(1.43735398200173,0.472775402794805,
-11.7987346998447));
#360994=CARTESIAN_POINT('Ctrl Pts',(1.36214842931913,0.658807877229377,
-11.7889028447167));
#360995=CARTESIAN_POINT('Ctrl Pts',(1.1475035811994,0.984875713542306,-11.7695182997489));
#360996=CARTESIAN_POINT('Ctrl Pts',(1.01240051157657,1.12328481092082,-11.7591734531316));
#360997=CARTESIAN_POINT('Ctrl Pts',(0.691303249455659,1.34601671031323,
-11.7375376566995));
#360998=CARTESIAN_POINT('Ctrl Pts',(0.50667682107433,1.42581559724676,-11.7264381777742));
#360999=CARTESIAN_POINT('Ctrl Pts',(0.12363865838816,1.50722857034544,-11.7057477741045));
#361000=CARTESIAN_POINT('Ctrl Pts',(-0.0704840469712229,1.51064725154874,
-11.6969045916964));
#361001=CARTESIAN_POINT('Ctrl Pts',(-0.450942230229227,1.44369139174563,
-11.6767399038253));
#361002=CARTESIAN_POINT('Ctrl Pts',(-0.633566219118868,1.37338076711471,
-11.6660003301567));
#361003=CARTESIAN_POINT('Ctrl Pts',(-0.966126547831251,1.16453331691648,
-11.6441986958203));
#361004=CARTESIAN_POINT('Ctrl Pts',(-1.11184311893041,1.02633504569465,
-11.6333490631573));
#361005=CARTESIAN_POINT('Ctrl Pts',(-1.33574551993269,0.708424259098842,
-11.6137456986831));
#361006=CARTESIAN_POINT('Ctrl Pts',(-1.41463392551725,0.533765819933085,
-11.6046536566629));
#361007=CARTESIAN_POINT('Ctrl Pts',(-1.50446432303768,0.158262306638579,
-11.5837923503688));
#361008=CARTESIAN_POINT('Ctrl Pts',(-1.51224681783949,-0.0395730290779647,
-11.5728014983845));
#361009=CARTESIAN_POINT('Ctrl Pts',(-1.45052698303864,-0.431588209997764,
-11.5510228772223));
#361010=CARTESIAN_POINT('Ctrl Pts',(-1.37982744089299,-0.621556200146737,
-11.5407881953655));
#361011=CARTESIAN_POINT('Ctrl Pts',(-1.17295041156061,-0.954329063619033,
-11.521591128999));
#361012=CARTESIAN_POINT('Ctrl Pts',(-1.04190006093877,-1.09589150221479,
-11.5113536761039));
#361013=CARTESIAN_POINT('Ctrl Pts',(-0.727762512368969,-1.326576265309,
-11.4898318161655));
#361014=CARTESIAN_POINT('Ctrl Pts',(-0.545914193739363,-1.41117979458698,
-11.4787325368206));
#361015=CARTESIAN_POINT('Ctrl Pts',(-0.237063288725948,-1.48593301082516,
-11.461796462496));
#361016=CARTESIAN_POINT('Ctrl Pts',(-0.118619887738532,-1.5,-11.4557071020098));
#361017=CARTESIAN_POINT('Ctrl Pts',(6.81746326058885E-14,-1.5,-11.45));
#361018=CARTESIAN_POINT('Ctrl Pts',(3.92107660876271E-8,-1.5,-11.3874999981135));
#361019=CARTESIAN_POINT('Ctrl Pts',(-0.0950530796326291,-1.50000000248474,
-11.3920732434951));
#361020=CARTESIAN_POINT('Ctrl Pts',(-0.190095831220883,-1.49096664224319,
-11.3968969165483));
#361021=CARTESIAN_POINT('Ctrl Pts',(-0.479809379763385,-1.43513269158633,
-11.4123867092254));
#361022=CARTESIAN_POINT('Ctrl Pts',(-0.666252458474244,-1.35864583147218,
-11.4234815910354));
#361023=CARTESIAN_POINT('Ctrl Pts',(-0.991963171491764,-1.14142976957814,
-11.445186134519));
#361024=CARTESIAN_POINT('Ctrl Pts',(-1.129775168227,-1.00522676258199,-11.4556000341644));
#361025=CARTESIAN_POINT('Ctrl Pts',(-1.34963990277553,-0.683716883318096,
-11.475109111117));
#361026=CARTESIAN_POINT('Ctrl Pts',(-1.42783852471113,-0.500293352745201,
-11.4847059248475));
#361027=CARTESIAN_POINT('Ctrl Pts',(-1.50858351472943,-0.114056565279965,
-11.5061635241511));
#361028=CARTESIAN_POINT('Ctrl Pts',(-1.51050448345982,0.0849027709680435,
-11.5172168206094));
#361029=CARTESIAN_POINT('Ctrl Pts',(-1.43862290569877,0.465276123774864,
-11.5383486735431));
#361030=CARTESIAN_POINT('Ctrl Pts',(-1.36817728516983,0.643565573521427,
-11.5478836944957));
#361031=CARTESIAN_POINT('Ctrl Pts',(-1.15978950001239,0.971817636837456,
-11.5670278693537));
#361032=CARTESIAN_POINT('Ctrl Pts',(-1.02090607423869,1.11681147207431,
-11.5777375078261));
#361033=CARTESIAN_POINT('Ctrl Pts',(-0.698066542869175,1.3418770776122,
-11.5995219543972));
#361034=CARTESIAN_POINT('Ctrl Pts',(-0.518116473811858,1.42108953555501,
-11.6103801521854));
#361035=CARTESIAN_POINT('Ctrl Pts',(-0.141683055304006,1.50545774145914,
-11.6308348747528));
#361036=CARTESIAN_POINT('Ctrl Pts',(0.0509131338252352,1.51125195179322,
-11.6396370050768));
#361037=CARTESIAN_POINT('Ctrl Pts',(0.437041528852499,1.44881299277959,
-11.6599490316725));
#361038=CARTESIAN_POINT('Ctrl Pts',(0.62623629134813,1.37763484275265,-11.6710288397613));
#361039=CARTESIAN_POINT('Ctrl Pts',(0.959042063487257,1.169314430107,-11.692827643068));
#361040=CARTESIAN_POINT('Ctrl Pts',(1.10105809980976,1.03670005261147,-11.7033441255096));
#361041=CARTESIAN_POINT('Ctrl Pts',(1.32908189525078,0.722399107477091,
-11.7230455072922));
#361042=CARTESIAN_POINT('Ctrl Pts',(1.41191038943793,0.542991320198872,
-11.7323338155445));
#361043=CARTESIAN_POINT('Ctrl Pts',(1.50442295622243,0.160573439476918,
-11.7535792533624));
#361044=CARTESIAN_POINT('Ctrl Pts',(1.51246790529916,-0.0388527502376838,
-11.7646584861243));
#361045=CARTESIAN_POINT('Ctrl Pts',(1.45190806340713,-0.422154644343116,
-11.7859530357969));
#361046=CARTESIAN_POINT('Ctrl Pts',(1.38666899163276,-0.60278637597622,
-11.7958612563664));
#361047=CARTESIAN_POINT('Ctrl Pts',(1.18788554968428,-0.937259716387997,
-11.8147161552989));
#361048=CARTESIAN_POINT('Ctrl Pts',(1.05335607453411,-1.08625159653144,
-11.8253273710272));
#361049=CARTESIAN_POINT('Ctrl Pts',(0.73687657244448,-1.32104540776602,
-11.8470760484829));
#361050=CARTESIAN_POINT('Ctrl Pts',(0.558779034676864,-1.40567451730944,
-11.8579955788624));
#361051=CARTESIAN_POINT('Ctrl Pts',(0.248449127703398,-1.4845415311917,
-11.8751170838587));
#361052=CARTESIAN_POINT('Ctrl Pts',(0.124349321223437,-1.50000000000001,
-11.8815172404932));
#361053=CARTESIAN_POINT('Ctrl Pts',(-1.15081555396301E-13,-1.5,-11.8875));
#361054=CARTESIAN_POINT('Origin',(0.,1.30104260698261E-15,-17.7));
#361055=CARTESIAN_POINT('',(-7.43743506404469E-14,-1.5,-12.45));
#361056=CARTESIAN_POINT('',(-9.08611625561309E-14,-1.5,-12.3875));
#361057=CARTESIAN_POINT('',(-1.83697019872103E-16,-1.5,-17.7));
#361058=CARTESIAN_POINT('Ctrl Pts',(-1.49255607873044E-13,-1.5,-12.45));
#361059=CARTESIAN_POINT('Ctrl Pts',(0.129273918175039,-1.50000000000001,
-12.4437803057119));
#361060=CARTESIAN_POINT('Ctrl Pts',(0.25823729718224,-1.48329297796134,
-12.4371114683009));
#361061=CARTESIAN_POINT('Ctrl Pts',(0.572723955290597,-1.40007740134056,
-12.4196691781129));
#361062=CARTESIAN_POINT('Ctrl Pts',(0.750144096931693,-1.3135856707735,
-12.4087304994969));
#361063=CARTESIAN_POINT('Ctrl Pts',(1.06435712568823,-1.07547182691069,
-12.3869986446617));
#361064=CARTESIAN_POINT('Ctrl Pts',(1.19735454561133,-0.925129649588097,
-12.3764236317199));
#361065=CARTESIAN_POINT('Ctrl Pts',(1.39280290168056,-0.588526364225109,
-12.357670027044));
#361066=CARTESIAN_POINT('Ctrl Pts',(1.45623457230694,-0.407063441158707,
-12.3476146356199));
#361067=CARTESIAN_POINT('Ctrl Pts',(1.51282311873122,-0.0227616208969719,
-12.3262645344943));
#361068=CARTESIAN_POINT('Ctrl Pts',(1.50263225416625,0.176784345586005,
-12.3151786474674));
#361069=CARTESIAN_POINT('Ctrl Pts',(1.40603464232576,0.557833883882915,
-12.2940092286732));
#361070=CARTESIAN_POINT('Ctrl Pts',(1.3215977154996,0.735854831854552,-12.2848116544044));
#361071=CARTESIAN_POINT('Ctrl Pts',(1.09071795642565,1.04760785595713,-12.2650436405916));
#361072=CARTESIAN_POINT('Ctrl Pts',(0.947240611682627,1.17892568620947,
-12.2544928661171));
#361073=CARTESIAN_POINT('Ctrl Pts',(0.611987873045726,1.3840540163624,-12.232665002038));
#361074=CARTESIAN_POINT('Ctrl Pts',(0.421856785171934,1.45333657814123,
-12.2215928002026));
#361075=CARTESIAN_POINT('Ctrl Pts',(0.0351065239375032,1.51167222359196,
-12.2013648349873));
#361076=CARTESIAN_POINT('Ctrl Pts',(-0.157180541384606,1.50388936038236,
-12.1925456854651));
#361077=CARTESIAN_POINT('Ctrl Pts',(-0.532704648611216,1.41571270707977,
-12.1720289219516));
#361078=CARTESIAN_POINT('Ctrl Pts',(-0.71201086726083,1.33455944470295,
-12.1611477901963));
#361079=CARTESIAN_POINT('Ctrl Pts',(-1.03261081878757,1.10599576904317,
-12.139373926846));
#361080=CARTESIAN_POINT('Ctrl Pts',(-1.16995145118631,0.959557326068837,
-12.1286983880618));
#361081=CARTESIAN_POINT('Ctrl Pts',(-1.3749134520388,0.629070993015123,
-12.1096569732798));
#361082=CARTESIAN_POINT('Ctrl Pts',(-1.44350117252979,0.449954696299029,
-12.0999974831277));
#361083=CARTESIAN_POINT('Ctrl Pts',(-1.51136358881569,0.0685287076069453,
-12.0788071504226));
#361084=CARTESIAN_POINT('Ctrl Pts',(-1.50726802756032,-0.130617691366746,
-12.0677434615907));
#361085=CARTESIAN_POINT('Ctrl Pts',(-1.42232495427812,-0.515513190831157,
-12.0463603782871));
#361086=CARTESIAN_POINT('Ctrl Pts',(-1.34247474812846,-0.697500796762078,
-12.0368814909687));
#361087=CARTESIAN_POINT('Ctrl Pts',(-1.11971067389336,-1.01646080816819,
-12.0173037491331));
#361088=CARTESIAN_POINT('Ctrl Pts',(-0.980400167431732,-1.15140818962697,
-12.006852630892));
#361089=CARTESIAN_POINT('Ctrl Pts',(-0.652151238334278,-1.36550129028978,
-11.9851127163534));
#361090=CARTESIAN_POINT('Ctrl Pts',(-0.46471769226152,-1.44011995248529,
-11.9740220750469));
#361091=CARTESIAN_POINT('Ctrl Pts',(-0.179477568288609,-1.49194945314334,
-11.958858744832));
#361092=CARTESIAN_POINT('Ctrl Pts',(-0.0897329405635131,-1.5,-11.9543172781158));
#361093=CARTESIAN_POINT('Ctrl Pts',(-1.66705089355558E-14,-1.5,-11.95));
#361094=CARTESIAN_POINT('Ctrl Pts',(-1.15591380429657E-13,-1.5,-11.8875));
#361095=CARTESIAN_POINT('Ctrl Pts',(-0.0652848605868303,-1.49999999999999,
-11.8906410193195));
#361096=CARTESIAN_POINT('Ctrl Pts',(-0.130627004965125,-1.49573835196629,
-11.8939031738187));
#361097=CARTESIAN_POINT('Ctrl Pts',(-0.394661743495974,-1.46100883160568,
-11.9075712599982));
#361098=CARTESIAN_POINT('Ctrl Pts',(-0.586417356539178,-1.39513512522614,
-11.9186269314095));
#361099=CARTESIAN_POINT('Ctrl Pts',(-0.925959609152179,-1.19576722898065,
-11.940501162773));
#361100=CARTESIAN_POINT('Ctrl Pts',(-1.07201374331102,-1.06680038780183,
-11.9511106078341));
#361101=CARTESIAN_POINT('Ctrl Pts',(-1.30795895391836,-0.759598097932127,
-11.9709959240131));
#361102=CARTESIAN_POINT('Ctrl Pts',(-1.39523546176121,-0.584012000755381,
-11.980054888847));
#361103=CARTESIAN_POINT('Ctrl Pts',(-1.49903493494599,-0.20542738546847,
-12.001087367474));
#361104=CARTESIAN_POINT('Ctrl Pts',(-1.51303243828964,-0.00572450358818515,
-12.0121819720229));
#361105=CARTESIAN_POINT('Ctrl Pts',(-1.46351743699624,0.380165488829691,
-12.033620304935));
#361106=CARTESIAN_POINT('Ctrl Pts',(-1.40333733761183,0.563096032260082,
-12.0437831129034));
#361107=CARTESIAN_POINT('Ctrl Pts',(-1.2137649769442,0.903477291464536,
-12.0626931828592));
#361108=CARTESIAN_POINT('Ctrl Pts',(-1.08348466334011,1.05622395116131,
-12.0730437073621));
#361109=CARTESIAN_POINT('Ctrl Pts',(-0.773201313986828,1.30019840059802,
-12.0947492900082));
#361110=CARTESIAN_POINT('Ctrl Pts',(-0.597013697489189,1.38994075745238,
-12.1057189639052));
#361111=CARTESIAN_POINT('Ctrl Pts',(-0.225668498337577,1.49505966223445,
-12.1265052877069));
#361112=CARTESIAN_POINT('Ctrl Pts',(-0.0346407051353212,1.51159478969829,
-12.1355112708055));
#361113=CARTESIAN_POINT('Ctrl Pts',(0.352246354109036,1.47155875118354,
-12.1552374953032));
#361114=CARTESIAN_POINT('Ctrl Pts',(0.544033157216475,1.41193882215949,
-12.1661209513095));
#361115=CARTESIAN_POINT('Ctrl Pts',(0.888535142663614,1.22392451774981,
-12.1879184303793));
#361116=CARTESIAN_POINT('Ctrl Pts',(1.03894680127538,1.09913115010637,-12.1986215971129));
#361117=CARTESIAN_POINT('Ctrl Pts',(1.28355750724515,0.799809154688375,
-12.2187049350638));
#361118=CARTESIAN_POINT('Ctrl Pts',(1.37565998347666,0.628312544963968,
-12.227593747502));
#361119=CARTESIAN_POINT('Ctrl Pts',(1.4916507986338,0.254050617991306,-12.2483860767783));
#361120=CARTESIAN_POINT('Ctrl Pts',(1.51215487649894,0.0542431023100071,
-12.2594864943161));
#361121=CARTESIAN_POINT('Ctrl Pts',(1.47475977951007,-0.334237654454839,
-12.2810687585809));
#361122=CARTESIAN_POINT('Ctrl Pts',(1.4201240034924,-0.519519887009746,
-12.291362215945));
#361123=CARTESIAN_POINT('Ctrl Pts',(1.24035558751452,-0.866811580439447,
-12.3106561989133));
#361124=CARTESIAN_POINT('Ctrl Pts',(1.11411578699525,-1.02402320319891,
-12.3206755015169));
#361125=CARTESIAN_POINT('Ctrl Pts',(0.809936777076213,-1.27772235058463,
-12.3423575194936));
#361126=CARTESIAN_POINT('Ctrl Pts',(0.635863081781533,-1.37268067289867,
-12.3533703752388));
#361127=CARTESIAN_POINT('Ctrl Pts',(0.303076447178655,-1.47693942444835,
-12.3722776560933));
#361128=CARTESIAN_POINT('Ctrl Pts',(0.151876448244223,-1.50000000000002,
-12.3801928409769));
#361129=CARTESIAN_POINT('Ctrl Pts',(-1.83152104593631E-13,-1.5,-12.3875));
#361130=CARTESIAN_POINT('Origin',(0.,1.30104260698261E-15,-17.7));
#361131=CARTESIAN_POINT('',(-5.78875387247644E-14,-1.5,-12.95));
#361132=CARTESIAN_POINT('',(-1.83697019872103E-16,-1.5,-12.8875));
#361133=CARTESIAN_POINT('',(-1.83697019872103E-16,-1.5,-17.7));
#361134=CARTESIAN_POINT('Ctrl Pts',(-1.16399945238044E-13,-1.5,-12.95));
#361135=CARTESIAN_POINT('Ctrl Pts',(0.158876952576763,-1.50000000000001,
-12.9423560290551));
#361136=CARTESIAN_POINT('Ctrl Pts',(0.316934376671936,-1.47476380404689,
-12.9340504822496));
#361137=CARTESIAN_POINT('Ctrl Pts',(0.655117690859527,-1.36363573904858,
-12.914692739265));
#361138=CARTESIAN_POINT('Ctrl Pts',(0.828076727203405,-1.26608438701772,
-12.9036614839704));
#361139=CARTESIAN_POINT('Ctrl Pts',(1.12806327860616,-1.00845306391603,
-12.8820719486449));
#361140=CARTESIAN_POINT('Ctrl Pts',(1.25157899640202,-0.850310207670071,
-12.8722394559816));
#361141=CARTESIAN_POINT('Ctrl Pts',(1.42665630726749,-0.501394151761404,
-12.8528552306534));
#361142=CARTESIAN_POINT('Ctrl Pts',(1.47897883859234,-0.315190147192983,
-12.8425105637329));
#361143=CARTESIAN_POINT('Ctrl Pts',(1.51133966887728,0.0742508797942082,
-12.8208749511225));
#361144=CARTESIAN_POINT('Ctrl Pts',(1.48814391899043,0.274041623011249,
-12.8097754653882));
#361145=CARTESIAN_POINT('Ctrl Pts',(1.3671483554754,0.646475451295437,-12.7890846971502));
#361146=CARTESIAN_POINT('Ctrl Pts',(1.2730547677852,0.816305903343349,-12.7802413787577));
#361147=CARTESIAN_POINT('Ctrl Pts',(1.02485301882479,1.11232624886059,-12.7600769791676));
#361148=CARTESIAN_POINT('Ctrl Pts',(0.872656584289035,1.23533438080045,
-12.749337532243));
#361149=CARTESIAN_POINT('Ctrl Pts',(0.525518549519603,1.41893221299394,
-12.7275359059748));
#361150=CARTESIAN_POINT('Ctrl Pts',(0.33297967954763,1.47603634600655,-12.7166861493571));
#361151=CARTESIAN_POINT('Ctrl Pts',(-0.0542890167421315,1.51100424642432,
-12.6970823449523));
#361152=CARTESIAN_POINT('Ctrl Pts',(-0.244992999672171,1.49200322269456,
-12.6879906361045));
#361153=CARTESIAN_POINT('Ctrl Pts',(-0.615108227667013,1.38206416992609,
-12.6671295963181));
#361154=CARTESIAN_POINT('Ctrl Pts',(-0.790333414720495,1.2898950332486,
-12.6561388167787));
#361155=CARTESIAN_POINT('Ctrl Pts',(-1.09754102144741,1.04161475435297,
-12.6344616094948));
#361156=CARTESIAN_POINT('Ctrl Pts',(-1.2257837313118,0.887112892370766,
-12.6242840495761));
#361157=CARTESIAN_POINT('Ctrl Pts',(-1.41090380162242,0.543948766362077,
-12.605219375909));
#361158=CARTESIAN_POINT('Ctrl Pts',(-1.4686507071494,0.359961059105703,
-12.594997836617));
#361159=CARTESIAN_POINT('Ctrl Pts',(-1.51283723657042,-0.0271168915276431,
-12.5734935060262));
#361160=CARTESIAN_POINT('Ctrl Pts',(-1.49597450164886,-0.226891212692761,
-12.5623949326282));
#361161=CARTESIAN_POINT('Ctrl Pts',(-1.3867891322557,-0.603589178432375,
-12.5414672678648));
#361162=CARTESIAN_POINT('Ctrl Pts',(-1.29738422067913,-0.77736340783658,
-12.5324936660921));
#361163=CARTESIAN_POINT('Ctrl Pts',(-1.05762498672902,-1.08111224118951,
-12.5125207769772));
#361164=CARTESIAN_POINT('Ctrl Pts',(-0.909644569683913,-1.20826568059143,
-12.5018690258592));
#361165=CARTESIAN_POINT('Ctrl Pts',(-0.568774928134204,-1.40215707843199,
-12.4800830554213));
#361166=CARTESIAN_POINT('Ctrl Pts',(-0.378052343015115,-1.46514290080414,
-12.4691573045894));
#361167=CARTESIAN_POINT('Ctrl Pts',(-0.12054655675434,-1.49637094630723,
-12.455900605963));
#361168=CARTESIAN_POINT('Ctrl Pts',(-0.0602444439907949,-1.49999999999999,
-12.4528985121629));
#361169=CARTESIAN_POINT('Ctrl Pts',(-1.48565004261022E-13,-1.5,-12.45));
#361170=CARTESIAN_POINT('Ctrl Pts',(-1.8153862809239E-13,-1.5,-12.3875));
#361171=CARTESIAN_POINT('Ctrl Pts',(-0.0374929816783926,-1.5,-12.3893038819221));
#361172=CARTESIAN_POINT('Ctrl Pts',(-0.0750234464464321,-1.49859432408929,
-12.3911486138032));
#361173=CARTESIAN_POINT('Ctrl Pts',(-0.310834813771295,-1.48085636003662,
-12.4029868147272));
#361174=CARTESIAN_POINT('Ctrl Pts',(-0.504193695961855,-1.42664676038125,
-12.4137956204967));
#361175=CARTESIAN_POINT('Ctrl Pts',(-0.854282208926748,-1.2481551406557,
-12.435597362478));
#361176=CARTESIAN_POINT('Ctrl Pts',(-1.00849825756739,-1.12722328348696,
-12.4463763038324));
#361177=CARTESIAN_POINT('Ctrl Pts',(-1.26079688771879,-0.834996038406131,
-12.4666324508097));
#361178=CARTESIAN_POINT('Ctrl Pts',(-1.35715776934335,-0.667045853726193,
-12.4754418970152));
#361179=CARTESIAN_POINT('Ctrl Pts',(-1.48382942208322,-0.296722390016991,
-12.4960154227769));
#361180=CARTESIAN_POINT('Ctrl Pts',(-1.51009088547731,-0.0969934152972635,
-12.507111476928));
#361181=CARTESIAN_POINT('Ctrl Pts',(-1.48347839072346,0.293462146888296,
-12.5288034526049));
#361182=CARTESIAN_POINT('Ctrl Pts',(-1.43380448896476,0.480679727579932,
-12.53920442931));
#361183=CARTESIAN_POINT('Ctrl Pts',(-1.26405217312614,0.831418736778474,
-12.5586899298211));
#361184=CARTESIAN_POINT('Ctrl Pts',(-1.14359126239354,0.990608365372646,
-12.568329172106));
#361185=CARTESIAN_POINT('Ctrl Pts',(-0.848358771487759,1.25263385222588,
-12.5898120376934));
#361186=CARTESIAN_POINT('Ctrl Pts',(-0.67670373428794,1.35309855913209,
-12.6008614808243));
#361187=CARTESIAN_POINT('Ctrl Pts',(-0.310977376334873,1.47966238232852,
-12.6219731601809));
#361188=CARTESIAN_POINT('Ctrl Pts',(-0.121276295927422,1.50710633513481,
-12.6314676932935));
#361189=CARTESIAN_POINT('Ctrl Pts',(0.267112603342264,1.48936011891211,
-12.6506470133728));
#361190=CARTESIAN_POINT('Ctrl Pts',(0.461952664132715,1.44087424484157,
-12.6613680900036));
#361191=CARTESIAN_POINT('Ctrl Pts',(0.817619890410771,1.27255732995747,
-12.6831556072643));
#361192=CARTESIAN_POINT('Ctrl Pts',(0.97572465732348,1.15580070930254,-12.6940056658717));
#361193=CARTESIAN_POINT('Ctrl Pts',(1.23602733972881,0.871060496173528,
-12.7144389348828));
#361194=CARTESIAN_POINT('Ctrl Pts',(1.33680365595805,0.706727529185695,
-12.7232373594897));
#361195=CARTESIAN_POINT('Ctrl Pts',(1.47445973273482,0.340592604871063,
-12.7435781886183));
#361196=CARTESIAN_POINT('Ctrl Pts',(1.50668752861793,0.141113819903124,
-12.7546603433388));
#361197=CARTESIAN_POINT('Ctrl Pts',(1.49130621154247,-0.251075049662532,
-12.7764486138702));
#361198=CARTESIAN_POINT('Ctrl Pts',(1.44682930119438,-0.440154664538035,
-12.7869530369188));
#361199=CARTESIAN_POINT('Ctrl Pts',(1.28739409514771,-0.794363222880267,
-12.8066312901601));
#361200=CARTESIAN_POINT('Ctrl Pts',(1.1727403962829,-0.955556720159954,
-12.8159530769364));
#361201=CARTESIAN_POINT('Ctrl Pts',(0.88669793180305,-1.22589150798183,
-12.8372246010871));
#361202=CARTESIAN_POINT('Ctrl Pts',(0.717681680755148,-1.33190577252514,
-12.8483012399388));
#361203=CARTESIAN_POINT('Ctrl Pts',(0.362630102147741,-1.46687280253244,
-12.8691327511461));
#361204=CARTESIAN_POINT('Ctrl Pts',(0.182013319335047,-1.5,-12.8787428800905));
#361205=CARTESIAN_POINT('Ctrl Pts',(-1.59594559789866E-15,-1.5,-12.8875));
#361206=CARTESIAN_POINT('Origin',(0.,1.30104260698261E-15,-17.7));
#361207=CARTESIAN_POINT('',(6.17379976491385E-9,-1.5,-13.4499999994059));
#361208=CARTESIAN_POINT('',(3.27899268114955E-14,-1.5,-13.3875));
#361209=CARTESIAN_POINT('',(-1.83697019872103E-16,-1.5,-17.7));
#361210=CARTESIAN_POINT('Ctrl Pts',(1.23475991584132E-8,-1.5,-13.4499999994059));
#361211=CARTESIAN_POINT('Ctrl Pts',(0.189148975563307,-1.49999999844298,
-13.4408995656269));
#361212=CARTESIAN_POINT('Ctrl Pts',(0.376690429974303,-1.46422167503491,
-13.4308826308776));
#361213=CARTESIAN_POINT('Ctrl Pts',(0.736633814777829,-1.32156048455152,
-13.409602035855));
#361214=CARTESIAN_POINT('Ctrl Pts',(0.904354826486513,-1.21297087800871,
-13.3985161769573));
#361215=CARTESIAN_POINT('Ctrl Pts',(1.18606966936468,-0.938803382033804,
-13.3773464014827));
#361216=CARTESIAN_POINT('Ctrl Pts',(1.29803119767387,-0.776671648115806,
-13.3681484248953));
#361217=CARTESIAN_POINT('Ctrl Pts',(1.45259433871836,-0.42085298006497,
-13.3483807211147));
#361218=CARTESIAN_POINT('Ctrl Pts',(1.49458892567519,-0.23094188314,-13.3378301046189));
#361219=CARTESIAN_POINT('Ctrl Pts',(1.50462756389352,0.161957317004072,
-13.3160023712775));
#361220=CARTESIAN_POINT('Ctrl Pts',(1.46957234297039,0.3612576400713,-13.3049301311071));
#361221=CARTESIAN_POINT('Ctrl Pts',(1.32673541454486,0.725368121781877,
-13.2847017710121));
#361222=CARTESIAN_POINT('Ctrl Pts',(1.22385906373864,0.888008057584638,
-13.2758827228365));
#361223=CARTESIAN_POINT('Ctrl Pts',(0.959747099080752,1.16914578135365,
-13.2553662487964));
#361224=CARTESIAN_POINT('Ctrl Pts',(0.799819539093315,1.28386008899408,
-13.2444852219334));
#361225=CARTESIAN_POINT('Ctrl Pts',(0.441586475710377,1.44724329476693,
-13.2227113032527));
#361226=CARTESIAN_POINT('Ctrl Pts',(0.246098944072605,1.49297421001171,
-13.2120356018003));
#361227=CARTESIAN_POINT('Ctrl Pts',(-0.142590608807902,1.50525249012568,
-13.1929937036315));
#361228=CARTESIAN_POINT('Ctrl Pts',(-0.332004710784623,1.47510255039801,
-13.1833348200824));
#361229=CARTESIAN_POINT('Ctrl Pts',(-0.696265710086782,1.34317897081802,
-13.162144760705));
#361230=CARTESIAN_POINT('Ctrl Pts',(-0.866688171311859,1.24006818470157,
-13.151081117713));
#361231=CARTESIAN_POINT('Ctrl Pts',(-1.1575612640928,0.974071462272501,
-13.1296976816664));
#361232=CARTESIAN_POINT('Ctrl Pts',(-1.27525175459758,0.813928698898369,
-13.1202182610499));
#361233=CARTESIAN_POINT('Ctrl Pts',(-1.44011441929941,0.461535143221553,
-13.1006408412901));
#361234=CARTESIAN_POINT('Ctrl Pts',(-1.48733570237035,0.273418130482792,
-13.0901898961379));
#361235=CARTESIAN_POINT('Ctrl Pts',(-1.50864005363079,-0.117897423145407,
-13.0684501431586));
#361236=CARTESIAN_POINT('Ctrl Pts',(-1.47955490051629,-0.317529377045197,
-13.057359479053));
#361237=CARTESIAN_POINT('Ctrl Pts',(-1.34767507955946,-0.685884446848146,
-13.0368953085084));
#361238=CARTESIAN_POINT('Ctrl Pts',(-1.24922625664541,-0.852115139450408,
-13.028100227978));
#361239=CARTESIAN_POINT('Ctrl Pts',(-0.993144863791779,-1.14081747479882,
-13.0077599969045));
#361240=CARTESIAN_POINT('Ctrl Pts',(-0.83708138983694,-1.25979574668122,
-12.9969464375163));
#361241=CARTESIAN_POINT('Ctrl Pts',(-0.484325304368011,-1.43351148257176,
-12.9751490153329));
#361242=CARTESIAN_POINT('Ctrl Pts',(-0.290246273872271,-1.48502724998096,
-12.9643803900853));
#361243=CARTESIAN_POINT('Ctrl Pts',(-0.061166760094827,-1.49906552881572,
-12.95296884465));
#361244=CARTESIAN_POINT('Ctrl Pts',(-0.0305694474716846,-1.5,-12.9514707732272));
#361245=CARTESIAN_POINT('Ctrl Pts',(-1.15591380429657E-13,-1.5,-12.95));
#361246=CARTESIAN_POINT('Ctrl Pts',(-1.83697019872103E-16,-1.5,-12.8875));
#361247=CARTESIAN_POINT('Ctrl Pts',(-0.00807884865481996,-1.5,-12.8878886937871));
#361248=CARTESIAN_POINT('Ctrl Pts',(-0.0161602766706464,-1.49993473226773,
-12.8882793246664));
#361249=CARTESIAN_POINT('Ctrl Pts',(-0.223037962130807,-1.49659066907362,
-12.8983256225932));
#361250=CARTESIAN_POINT('Ctrl Pts',(-0.419188387790651,-1.4538860378266,
-12.9089491541048));
#361251=CARTESIAN_POINT('Ctrl Pts',(-0.780151786748742,-1.29594949218373,
-12.9307031400023));
#361252=CARTESIAN_POINT('Ctrl Pts',(-0.942045516713052,-1.18350295005882,
-12.9416157707759));
#361253=CARTESIAN_POINT('Ctrl Pts',(-1.21031233322143,-0.906324473969546,
-12.9622221661166));
#361254=CARTESIAN_POINT('Ctrl Pts',(-1.31548035152035,-0.745510580599391,
-12.9710827455223));
#361255=CARTESIAN_POINT('Ctrl Pts',(-1.46393442269762,-0.383629870391432,
-12.9911872294227));
#361256=CARTESIAN_POINT('Ctrl Pts',(-1.50206316794945,-0.184567223381819,
-13.0022462653677));
#361257=CARTESIAN_POINT('Ctrl Pts',(-1.49784697651995,0.209023161470686,
-13.0241123978595));
#361258=CARTESIAN_POINT('Ctrl Pts',(-1.4585649562512,0.399800978318997,
-13.0347111654622));
#361259=CARTESIAN_POINT('Ctrl Pts',(-1.30928839502881,0.757346329732696,
-13.0545747960963));
#361260=CARTESIAN_POINT('Ctrl Pts',(-1.20021246007597,0.920492389190269,
-13.0636573174573));
#361261=CARTESIAN_POINT('Ctrl Pts',(-0.923182794605771,1.19875428317566,
-13.0847154105068));
#361262=CARTESIAN_POINT('Ctrl Pts',(-0.75690113054832,1.31010422518364,
-13.0958086947436));
#361263=CARTESIAN_POINT('Ctrl Pts',(-0.397560799802422,1.45887984296568,
-13.117230120517));
#361264=CARTESIAN_POINT('Ctrl Pts',(-0.208979560478688,1.49757686314416,
-13.1273781568515));
#361265=CARTESIAN_POINT('Ctrl Pts',(0.180529207953534,1.50229867163426,
-13.1462495675573));
#361266=CARTESIAN_POINT('Ctrl Pts',(0.377822901886829,1.46519477880051,
-13.1566448245426));
#361267=CARTESIAN_POINT('Ctrl Pts',(0.743702509879271,1.31728437099402,
-13.1783568378287));
#361268=CARTESIAN_POINT('Ctrl Pts',(0.909111631589959,1.20907086766095,
-13.1893210185557));
#361269=CARTESIAN_POINT('Ctrl Pts',(1.18493942771686,0.939180171635513,
-13.2100887533629));
#361270=CARTESIAN_POINT('Ctrl Pts',(1.29428564810427,0.781636310928492,
-13.219075760504));
#361271=CARTESIAN_POINT('Ctrl Pts',(1.45191928137376,0.426021078425527,
-13.2388321623097));
#361272=CARTESIAN_POINT('Ctrl Pts',(1.49554556850097,0.229973772428518,
-13.2497236793096));
#361273=CARTESIAN_POINT('Ctrl Pts',(1.50369690667037,-0.162351848758911,
-13.2715195471533));
#361274=CARTESIAN_POINT('Ctrl Pts',(1.47022567902877,-0.354842241618453,
-13.2822134578677));
#361275=CARTESIAN_POINT('Ctrl Pts',(1.33215624580652,-0.71597793363767,
-13.3022765518688));
#361276=CARTESIAN_POINT('Ctrl Pts',(1.22907824959446,-0.88126846710937,
-13.3111789581204));
#361277=CARTESIAN_POINT('Ctrl Pts',(0.961938307621396,-1.1679948129568,
-13.3319963552892));
#361278=CARTESIAN_POINT('Ctrl Pts',(0.798818223935141,-1.28507501721829,
-13.3430967018709));
#361279=CARTESIAN_POINT('Ctrl Pts',(0.44327680231076,-1.44572266131707,
-13.3646651310528));
#361280=CARTESIAN_POINT('Ctrl Pts',(0.255415543169415,-1.4904339350922,
-13.3749455899245));
#361281=CARTESIAN_POINT('Ctrl Pts',(0.0427931613907333,-1.49954254591616,
-13.3854284060048));
#361282=CARTESIAN_POINT('Ctrl Pts',(0.0213882799085289,-1.5,-13.3864709559031));
#361283=CARTESIAN_POINT('Ctrl Pts',(6.5763550642863E-14,-1.5,-13.3875));
#361284=CARTESIAN_POINT('Origin',(0.,1.30104260698261E-15,-17.7));
#361285=CARTESIAN_POINT('',(6.1641847663942E-14,-1.5,-13.95));
#361286=CARTESIAN_POINT('',(1.23467392347757E-13,-1.5,-13.8875));
#361287=CARTESIAN_POINT('',(-1.83697019872103E-16,-1.5,-17.7));
#361288=CARTESIAN_POINT('Ctrl Pts',(1.23467392347756E-13,-1.5,-13.95));
#361289=CARTESIAN_POINT('Ctrl Pts',(0.0273727606550288,-1.5,-13.9486830274389));
#361290=CARTESIAN_POINT('Ctrl Pts',(0.0547705664019769,-1.4992507445935,
-13.9473440372451));
#361291=CARTESIAN_POINT('Ctrl Pts',(0.27349293350586,-1.48725212293488,
-13.9364874574053));
#361292=CARTESIAN_POINT('Ctrl Pts',(0.461021133040364,-1.44019285401277,
-13.926157800784));
#361293=CARTESIAN_POINT('Ctrl Pts',(0.814973605767246,-1.27493031347283,
-13.9045376283737));
#361294=CARTESIAN_POINT('Ctrl Pts',(0.976806088535854,-1.15563365119737,
-13.8934376632419));
#361295=CARTESIAN_POINT('Ctrl Pts',(1.24005780212886,-0.865642475645971,
-13.8727166488343));
#361296=CARTESIAN_POINT('Ctrl Pts',(1.34081010114396,-0.699504708701909,
-13.8638613727056));
#361297=CARTESIAN_POINT('Ctrl Pts',(1.47445308365235,-0.336977220166086,
-13.8437209566758));
#361298=CARTESIAN_POINT('Ctrl Pts',(1.5056086078487,-0.143858005698238,
-13.8329921114276));
#361299=CARTESIAN_POINT('Ctrl Pts',(1.4925681575455,0.248556174862625,-13.8111913236187));
#361300=CARTESIAN_POINT('Ctrl Pts',(1.44651041138113,0.444035568848532,
-13.8003313572862));
#361301=CARTESIAN_POINT('Ctrl Pts',(1.28451834308037,0.797560797550709,
-13.7806910668027));
#361302=CARTESIAN_POINT('Ctrl Pts',(1.17329856752123,0.953663525102152,
-13.7716263668414));
#361303=CARTESIAN_POINT('Ctrl Pts',(0.894089756253627,1.22025961834643,
-13.7507874796114));
#361304=CARTESIAN_POINT('Ctrl Pts',(0.727136316356959,1.32653649589924,
-13.7398027930016));
#361305=CARTESIAN_POINT('Ctrl Pts',(0.359161671993576,1.46988350906151,
-13.7181167431934));
#361306=CARTESIAN_POINT('Ctrl Pts',(0.161383474980832,1.50448162004382,
-13.7078890555059));
#361307=CARTESIAN_POINT('Ctrl Pts',(-0.228318046516828,1.49478151140755,
-13.6888700848487));
#361308=CARTESIAN_POINT('Ctrl Pts',(-0.416623010527941,1.45358281099932,
-13.6786658496989));
#361309=CARTESIAN_POINT('Ctrl Pts',(-0.774430407259481,1.29985998622534,
-13.6571807548312));
#361310=CARTESIAN_POINT('Ctrl Pts',(-0.939420778107782,1.18611726233594,
-13.6460831318046));
#361311=CARTESIAN_POINT('Ctrl Pts',(-1.21234841839429,0.904315851918118,
-13.6251240776328));
#361312=CARTESIAN_POINT('Ctrl Pts',(-1.31892166504881,0.740281487577644,
-13.6161267493098));
#361313=CARTESIAN_POINT('Ctrl Pts',(-1.46355819493749,0.381238092972433,
-13.596179894054));
#361314=CARTESIAN_POINT('Ctrl Pts',(-1.50044394700116,0.189730464566316,
-13.5855405813648));
#361315=CARTESIAN_POINT('Ctrl Pts',(-1.49953010905219,-0.204397744186537,
-13.5636445697674));
#361316=CARTESIAN_POINT('Ctrl Pts',(-1.45870003340395,-0.403213907571023,
-13.5525992273571));
#361317=CARTESIAN_POINT('Ctrl Pts',(-1.30531953657094,-0.763109642954445,
-13.5326050198358));
#361318=CARTESIAN_POINT('Ctrl Pts',(-1.19812778701953,-0.922330037194102,
-13.5236913378856));
#361319=CARTESIAN_POINT('Ctrl Pts',(-0.926195786334519,-1.19598932968987,
-13.5030063563888));
#361320=CARTESIAN_POINT('Ctrl Pts',(-0.762587572873664,-1.30640090443331,
-13.4920677643612));
#361321=CARTESIAN_POINT('Ctrl Pts',(-0.399276435807626,-1.45947733686857,
-13.4703358260059));
#361322=CARTESIAN_POINT('Ctrl Pts',(-0.202579407806616,-1.49949470960994,
-13.4597606421466));
#361323=CARTESIAN_POINT('Ctrl Pts',(-0.00251767479581147,-1.499998415418,
-13.4501211757012));
#361324=CARTESIAN_POINT('Ctrl Pts',(-0.0012587977324238,-1.50000000001036,
-13.4500605639338));
#361325=CARTESIAN_POINT('Ctrl Pts',(1.23475997724286E-8,-1.5,-13.4499999994059));
#361326=CARTESIAN_POINT('Ctrl Pts',(6.20337115009306E-14,-1.5,-13.3875));
#361327=CARTESIAN_POINT('Ctrl Pts',(-0.178100903696597,-1.5,-13.3960688837243));
#361328=CARTESIAN_POINT('Ctrl Pts',(-0.354967221346645,-1.46828470868815,
-13.4054593487141));
#361329=CARTESIAN_POINT('Ctrl Pts',(-0.70633803961609,-1.33777107321515,
-13.4259900638533));
#361330=CARTESIAN_POINT('Ctrl Pts',(-0.875184458485685,-1.23393656197652,
-13.4369979829477));
#361331=CARTESIAN_POINT('Ctrl Pts',(-1.15859240296114,-0.97146419681889,
-13.457924353066));
#361332=CARTESIAN_POINT('Ctrl Pts',(-1.27214519917268,-0.817134168424963,
-13.4671036573098));
#361333=CARTESIAN_POINT('Ctrl Pts',(-1.4395118380733,-0.466219582375254,
-13.4865989120903));
#361334=CARTESIAN_POINT('Ctrl Pts',(-1.48856622007895,-0.271485424393246,
-13.4974174764227));
#361335=CARTESIAN_POINT('Ctrl Pts',(-1.50765853111819,0.120953412385961,
-13.5192196340215));
#361336=CARTESIAN_POINT('Ctrl Pts',(-1.47938132936033,0.314812388806881,
-13.529989577156));
#361337=CARTESIAN_POINT('Ctrl Pts',(-1.35121242124249,0.679040400354931,
-13.5502244666864));
#361338=CARTESIAN_POINT('Ctrl Pts',(-1.25330353095733,0.846227866481236,
-13.55904006871));
#361339=CARTESIAN_POINT('Ctrl Pts',(-0.994844835122127,1.14019695876635,
-13.5796409766303));
#361340=CARTESIAN_POINT('Ctrl Pts',(-0.834633214314774,1.26219703017889,
-13.5907380527029));
#361341=CARTESIAN_POINT('Ctrl Pts',(-0.482711808255667,1.433106098456,-13.6124173533652));
#361342=CARTESIAN_POINT('Ctrl Pts',(-0.295632313906198,1.48304608128885,
-13.6228054414791));
#361343=CARTESIAN_POINT('Ctrl Pts',(0.0932458580179198,1.51012548968155,
-13.6422675570379));
#361344=CARTESIAN_POINT('Ctrl Pts',(0.291481610423482,1.48466644261322,
-13.6519498476698));
#361345=CARTESIAN_POINT('Ctrl Pts',(0.665692555798307,1.35853927436543,
-13.673457612625));
#361346=CARTESIAN_POINT('Ctrl Pts',(0.838095336951256,1.25951242582141,
-13.6845030910935));
#361347=CARTESIAN_POINT('Ctrl Pts',(1.12957335331216,1.00506872077059,-13.7055947143901));
#361348=CARTESIAN_POINT('Ctrl Pts',(1.24763399480712,0.854095972651749,
-13.7150502237416));
#361349=CARTESIAN_POINT('Ctrl Pts',(1.42521375094207,0.508242002316863,
-13.7342643332047));
#361350=CARTESIAN_POINT('Ctrl Pts',(1.47995176671291,0.31506087755952,-13.7449966179134));
#361351=CARTESIAN_POINT('Ctrl Pts',(1.51060379458671,-0.077164127040108,
-13.7667868959467));
#361352=CARTESIAN_POINT('Ctrl Pts',(1.48786123370151,-0.272317462827342,
-13.7776287479349));
#361353=CARTESIAN_POINT('Ctrl Pts',(1.37014123212598,-0.639731899664652,
-13.7980406610925));
#361354=CARTESIAN_POINT('Ctrl Pts',(1.27756797068767,-0.808926535266669,
-13.8068364972199));
#361355=CARTESIAN_POINT('Ctrl Pts',(1.02820533535891,-1.11031494337791,
-13.8272058628313));
#361356=CARTESIAN_POINT('Ctrl Pts',(0.87116979906505,-1.23735790462876,
-13.8382902097397));
#361357=CARTESIAN_POINT('Ctrl Pts',(0.523318710027666,-1.41885361090174,
-13.8600677504607));
#361358=CARTESIAN_POINT('Ctrl Pts',(0.337204794027228,-1.47421825389061,
-13.8705600671689));
#361359=CARTESIAN_POINT('Ctrl Pts',(0.0971864689633863,-1.49764146682935,
-13.8827585990216));
#361360=CARTESIAN_POINT('Ctrl Pts',(0.0485661678850943,-1.5,-13.8851633591582));
#361361=CARTESIAN_POINT('Ctrl Pts',(2.47118481715386E-13,-1.5,-13.8875));
#361362=CARTESIAN_POINT('Origin',(0.,1.30104260698261E-15,-17.7));
#361363=CARTESIAN_POINT('',(1.15223986389915E-13,-1.5,-14.45));
#361364=CARTESIAN_POINT('',(2.04248178747325E-14,-1.5,-14.3875));
#361365=CARTESIAN_POINT('',(-1.83697019872103E-16,-1.5,-17.7));
#361366=CARTESIAN_POINT('Ctrl Pts',(2.30631669799703E-13,-1.5,-14.45));
#361367=CARTESIAN_POINT('Ctrl Pts',(0.0548934545880663,-1.5,-14.4473589374347));
#361368=CARTESIAN_POINT('Ctrl Pts',(0.109846375959735,-1.49698693850033,
-14.4446313176197));
#361369=CARTESIAN_POINT('Ctrl Pts',(0.356114797475588,-1.46979646143151,
-14.4320274316354));
#361370=CARTESIAN_POINT('Ctrl Pts',(0.541735609813599,-1.41195761642243,
-14.4214901115543));
#361371=CARTESIAN_POINT('Ctrl Pts',(0.887622898574594,-1.22565352496498,
-14.3996734879631));
#361372=CARTESIAN_POINT('Ctrl Pts',(1.04315567077518,-1.09633139380361,
-14.3885981325504));
#361373=CARTESIAN_POINT('Ctrl Pts',(1.28833566498435,-0.791587430127308,
-14.3683367944769));
#361374=CARTESIAN_POINT('Ctrl Pts',(1.3784815054932,-0.621459006709495,
-14.3595255003727));
#361375=CARTESIAN_POINT('Ctrl Pts',(1.4913685586622,-0.252598796378145,
-14.3390332664654));
#361376=CARTESIAN_POINT('Ctrl Pts',(1.51153567546017,-0.0568996909763287,
-14.3281610939431));
#361377=CARTESIAN_POINT('Ctrl Pts',(1.47553879372479,0.335110661665423,
-14.3063827410185));
#361378=CARTESIAN_POINT('Ctrl Pts',(1.41819075254881,0.527516332674454,
-14.2956935370736));
#361379=CARTESIAN_POINT('Ctrl Pts',(1.23590781493958,0.870996745486203,
-14.2766112919174));
#361380=CARTESIAN_POINT('Ctrl Pts',(1.11573602959479,1.02042728393899,-14.2670023390876));
#361381=CARTESIAN_POINT('Ctrl Pts',(0.820502075920879,1.27108579679313,
-14.2458351524004));
#361382=CARTESIAN_POINT('Ctrl Pts',(0.646482477624955,1.36782476586137,
-14.2347754369885));
#361383=CARTESIAN_POINT('Ctrl Pts',(0.271051159733503,1.48841962626682,
-14.2133626320511));
#361384=CARTESIAN_POINT('Ctrl Pts',(0.0733547619086724,1.51111323541884,
-14.2038379836117));
#361385=CARTESIAN_POINT('Ctrl Pts',(-0.314557462546743,1.47917868967553,
-14.1842874772956));
#361386=CARTESIAN_POINT('Ctrl Pts',(-0.501217439520081,1.42677172190501,
-14.1738510458615));
#361387=CARTESIAN_POINT('Ctrl Pts',(-0.851327691872639,1.25104062313835,
-14.1521249390812));
#361388=CARTESIAN_POINT('Ctrl Pts',(-1.01011504827038,1.12673940669524,
-14.1410324672666));
#361389=CARTESIAN_POINT('Ctrl Pts',(-1.26444900369502,0.829385260622806,
-14.12053598174));
#361390=CARTESIAN_POINT('Ctrl Pts',(-1.35992886792741,0.661290561105772,
-14.1117383645058));
#361391=CARTESIAN_POINT('Ctrl Pts',(-1.48336975502415,0.295610939923114,
-14.0914228299957));
#361392=CARTESIAN_POINT('Ctrl Pts',(-1.50914875596412,0.101147022240177,
-14.0806192790133));
#361393=CARTESIAN_POINT('Ctrl Pts',(-1.48482616482199,-0.291237481210953,
-14.0588201399327));
#361394=CARTESIAN_POINT('Ctrl Pts',(-1.43319362671366,-0.485289998468957,
-14.0480394445295));
#361395=CARTESIAN_POINT('Ctrl Pts',(-1.26119818391366,-0.833927043460052,
-14.0286707198077));
#361396=CARTESIAN_POINT('Ctrl Pts',(-1.14561487565883,-0.986733837248934,
-14.0193758148138));
#361397=CARTESIAN_POINT('Ctrl Pts',(-0.858564070758227,-1.24559925824427,
-13.998374370385));
#361398=CARTESIAN_POINT('Ctrl Pts',(-0.68809869252659,-1.34728197701362,
-13.9873483310851));
#361399=CARTESIAN_POINT('Ctrl Pts',(-0.341228236903536,-1.47071578820734,
-13.9672308015301));
#361400=CARTESIAN_POINT('Ctrl Pts',(-0.171142290594654,-1.5,-13.9582340872954));
#361401=CARTESIAN_POINT('Ctrl Pts',(1.24067423001861E-13,-1.5,-13.95));
#361402=CARTESIAN_POINT('Ctrl Pts',(2.47118481715386E-13,-1.5,-13.8875));
#361403=CARTESIAN_POINT('Ctrl Pts',(-0.146901164955814,-1.5,-13.8945677855943));
#361404=CARTESIAN_POINT('Ctrl Pts',(-0.29324926487615,-1.47842590781795,
-13.9022082421731));
#361405=CARTESIAN_POINT('Ctrl Pts',(-0.623428532768038,-1.37853225627447,
-13.9208688232603));
#361406=CARTESIAN_POINT('Ctrl Pts',(-0.799335806249486,-1.28455193913573,
-13.9319427302667));
#361407=CARTESIAN_POINT('Ctrl Pts',(-1.09903141191604,-1.03843192947599,
-13.9531985087522));
#361408=CARTESIAN_POINT('Ctrl Pts',(-1.22172374531855,-0.890818384453344,
-13.9630100897527));
#361409=CARTESIAN_POINT('Ctrl Pts',(-1.40955390799974,-0.550171809059182,
-13.9819348994968));
#361410=CARTESIAN_POINT('Ctrl Pts',(-1.46997231997795,-0.358729462154206,
-13.9925705854359));
#361411=CARTESIAN_POINT('Ctrl Pts',(-1.51228676565712,0.032932669464555,
-14.0143295927481));
#361412=CARTESIAN_POINT('Ctrl Pts',(-1.49517726595293,0.229233814621506,
-14.0252352119235));
#361413=CARTESIAN_POINT('Ctrl Pts',(-1.38800785053078,0.599780881822918,
-14.0458211601013));
#361414=CARTESIAN_POINT('Ctrl Pts',(-1.30070197071466,0.771020319677233,
-14.0546705116916));
#361415=CARTESIAN_POINT('Ctrl Pts',(-1.06044914873033,1.07967342382362,
-14.0748033783162));
#361416=CARTESIAN_POINT('Ctrl Pts',(-0.906719571382535,1.21164763042927,
-14.0858656462383));
#361417=CARTESIAN_POINT('Ctrl Pts',(-0.563218003842742,1.40356600641679,
-14.1077234391118));
#361418=CARTESIAN_POINT('Ctrl Pts',(-0.378216913316017,1.46430207383723,
-14.1183114212137));
#361419=CARTESIAN_POINT('Ctrl Pts',(0.00632781424123031,1.51255890297912,
-14.1381533055208));
#361420=CARTESIAN_POINT('Ctrl Pts',(0.202281576293156,1.49898759168369,
-14.1472603993304));
#361421=CARTESIAN_POINT('Ctrl Pts',(0.581508724714796,1.39681711699902,
-14.1683440427571));
#361422=CARTESIAN_POINT('Ctrl Pts',(0.760705115394362,1.30788860290628,
-14.179435869626));
#361423=CARTESIAN_POINT('Ctrl Pts',(1.06829485686206,1.07009670557278,-14.2008401184439));
#361424=CARTESIAN_POINT('Ctrl Pts',(1.19556689497506,0.925745529551606,
-14.2109732521221));
#361425=CARTESIAN_POINT('Ctrl Pts',(1.39325787996739,0.590186443266003,
-14.2298057498024));
#361426=CARTESIAN_POINT('Ctrl Pts',(1.45914179626626,0.400560887356709,
-14.2402466173691));
#361427=CARTESIAN_POINT('Ctrl Pts',(1.51268440697242,0.00963277955025047,
-14.2619648455806));
#361428=CARTESIAN_POINT('Ctrl Pts',(1.5010363637033,-0.187621421187203,
-14.2729234122882));
#361429=CARTESIAN_POINT('Ctrl Pts',(1.40403520475586,-0.561104485393219,
-14.2936724714108));
#361430=CARTESIAN_POINT('Ctrl Pts',(1.32169950767049,-0.734339156382434,
-14.3026413460211));
#361431=CARTESIAN_POINT('Ctrl Pts',(1.09150246145397,-1.04794409308597,
-14.3224279548129));
#361432=CARTESIAN_POINT('Ctrl Pts',(0.943090741730096,-1.18326898371886,
-14.3333274417471));
#361433=CARTESIAN_POINT('Ctrl Pts',(0.606792062293365,-1.38536725397004,
-14.3551214603459));
#361434=CARTESIAN_POINT('Ctrl Pts',(0.423199204933112,-1.45201782338356,
-14.36580598052));
#361435=CARTESIAN_POINT('Ctrl Pts',(0.155076678190878,-1.49399241577041,
-14.3798719925021));
#361436=CARTESIAN_POINT('Ctrl Pts',(0.0775142586163279,-1.5,-14.3837705934935));
#361437=CARTESIAN_POINT('Ctrl Pts',(4.1033332769337E-14,-1.5,-14.3875));
#361438=CARTESIAN_POINT('Origin',(0.,1.30104260698261E-15,-17.7));
#361439=CARTESIAN_POINT('',(3.9380059590488E-15,-1.5,-14.95));
#361440=CARTESIAN_POINT('',(-4.305399998793E-15,-1.5,-14.8875));
#361441=CARTESIAN_POINT('',(-1.83697019872103E-16,-1.5,-17.7));
#361442=CARTESIAN_POINT('Ctrl Pts',(8.0597089379697E-15,-1.5,-14.95));
#361443=CARTESIAN_POINT('Ctrl Pts',(0.0833426479163508,-1.5,-14.9459901749825));
#361444=CARTESIAN_POINT('Ctrl Pts',(0.166719807561326,-1.49305513625313,
-14.9417857766368));
#361445=CARTESIAN_POINT('Ctrl Pts',(0.440334138154219,-1.44694357835383,
-14.92734062441));
#361446=CARTESIAN_POINT('Ctrl Pts',(0.623337762253202,-1.37803356404355,
-14.9166216913762));
#361447=CARTESIAN_POINT('Ctrl Pts',(0.957346261788502,-1.17176336052225,
-14.8948219720741));
#361448=CARTESIAN_POINT('Ctrl Pts',(1.10410200439716,-1.03465926441528,
-14.8839527360016));
#361449=CARTESIAN_POINT('Ctrl Pts',(1.33041854393489,-0.718392039016014,
-14.8642788757107));
#361450=CARTESIAN_POINT('Ctrl Pts',(1.41062716737482,-0.544282817543551,
-14.8552379343079));
#361451=CARTESIAN_POINT('Ctrl Pts',(1.50321498327612,-0.169551281775696,
-14.8344195156541));
#361452=CARTESIAN_POINT('Ctrl Pts',(1.51248503780511,0.0280695077048375,
-14.8234405829052));
#361453=CARTESIAN_POINT('Ctrl Pts',(1.45408384547968,0.418559633800821,
-14.801746687011));
#361454=CARTESIAN_POINT('Ctrl Pts',(1.38585349562832,0.607383413780491,
-14.7914718125692));
#361455=CARTESIAN_POINT('Ctrl Pts',(1.18387280610371,0.940701591758596,
-14.7724951738364));
#361456=CARTESIAN_POINT('Ctrl Pts',(1.0546254503485,1.0836125085627,-14.7623070098443));
#361457=CARTESIAN_POINT('Ctrl Pts',(0.743605532358566,1.31772476639197,
-14.74083993879));
#361458=CARTESIAN_POINT('Ctrl Pts',(0.563015447126632,1.40441023945795,
-14.7297433644558));
#361459=CARTESIAN_POINT('Ctrl Pts',(0.18279417496058,1.50140926982081,-14.7087555424593));
#361460=CARTESIAN_POINT('Ctrl Pts',(-0.0126886225498201,1.51244081182594,
-14.6997350964691));
#361461=CARTESIAN_POINT('Ctrl Pts',(-0.39624513432888,1.45955748315514,
-14.6798122438401));
#361462=CARTESIAN_POINT('Ctrl Pts',(-0.580705695498423,1.39645389961965,
-14.6691845036325));
#361463=CARTESIAN_POINT('Ctrl Pts',(-0.9221882556015,1.19996076135229,-14.6472967735696));
#361464=CARTESIAN_POINT('Ctrl Pts',(-1.07440923072296,1.0658328764283,-14.6362472639081));
#361465=CARTESIAN_POINT('Ctrl Pts',(-1.31061083652864,0.753999860652955,
-14.6162209806342));
#361466=CARTESIAN_POINT('Ctrl Pts',(-1.39559625713445,0.581837152560039,
-14.6073242862533));
#361467=CARTESIAN_POINT('Ctrl Pts',(-1.49804375618007,0.209916424324193,
-14.5866620235735));
#361468=CARTESIAN_POINT('Ctrl Pts',(-1.51262046441537,0.0131539254397011,
-14.5757307736355));
#361469=CARTESIAN_POINT('Ctrl Pts',(-1.46509565708434,-0.378143856838375,
-14.5539920079534));
#361470=CARTESIAN_POINT('Ctrl Pts',(-1.40215696456351,-0.568753598411832,
-14.5434025778659));
#361471=CARTESIAN_POINT('Ctrl Pts',(-1.20975930776716,-0.907039313885584,
-14.5246089270063));
#361472=CARTESIAN_POINT('Ctrl Pts',(-1.08496567168402,-1.05315762768056,
-14.5146127233373));
#361473=CARTESIAN_POINT('Ctrl Pts',(-0.781571052774216,-1.29547893043548,
-14.4932844956303));
#361474=CARTESIAN_POINT('Ctrl Pts',(-0.604126639955704,-1.38713882161312,
-14.4822010892498));
#361475=CARTESIAN_POINT('Ctrl Pts',(-0.27913311540433,-1.48046544168253,
-14.4639724248964));
#361476=CARTESIAN_POINT('Ctrl Pts',(-0.139785614626517,-1.5,-14.4567254385195));
#361477=CARTESIAN_POINT('Ctrl Pts',(2.31446806164826E-13,-1.5,-14.45));
#361478=CARTESIAN_POINT('Ctrl Pts',(4.10782519111308E-14,-1.5,-14.3875));
#361479=CARTESIAN_POINT('Ctrl Pts',(-0.114802638392122,-1.5,-14.393023444515));
#361480=CARTESIAN_POINT('Ctrl Pts',(-0.229464033139329,-1.48682369573369,
-14.3989061018938));
#361481=CARTESIAN_POINT('Ctrl Pts',(-0.535294746130471,-1.41526322525725,
-14.4156081797797));
#361482=CARTESIAN_POINT('Ctrl Pts',(-0.717909801300955,-1.33195624756892,
-14.4267083334316));
#361483=CARTESIAN_POINT('Ctrl Pts',(-1.03395736808419,-1.10341176165394,
-14.4482626370203));
#361484=CARTESIAN_POINT('Ctrl Pts',(-1.16611604840162,-0.962694650490352,
-14.4585299331351));
#361485=CARTESIAN_POINT('Ctrl Pts',(-1.37511325312879,-0.631742654647489,
-14.4777784268315));
#361486=CARTESIAN_POINT('Ctrl Pts',(-1.44704926475347,-0.442854836839777,
-14.487896953509));
#361487=CARTESIAN_POINT('Ctrl Pts',(-1.51189910921728,-0.0517560135145772,
-14.5096246659159));
#361488=CARTESIAN_POINT('Ctrl Pts',(-1.50569525189539,0.146294635185502,
-14.5206274797326));
#361489=CARTESIAN_POINT('Ctrl Pts',(-1.41878873104838,0.522609896388955,
-14.5415338831328));
#361490=CARTESIAN_POINT('Ctrl Pts',(-1.34129312954439,0.697853135661597,
-14.5506851468736));
#361491=CARTESIAN_POINT('Ctrl Pts',(-1.11994179463028,1.01749033453342,
-14.5702137290199));
#361492=CARTESIAN_POINT('Ctrl Pts',(-0.975330636366259,1.1568341836933,
-14.5810419990925));
#361493=CARTESIAN_POINT('Ctrl Pts',(-0.644319867728664,1.36838967916601,
-14.6028443036649));
#361494=CARTESIAN_POINT('Ctrl Pts',(-0.462107846438292,1.44017602864903,
-14.6136050488901));
#361495=CARTESIAN_POINT('Ctrl Pts',(-0.0823016076968858,1.51001412847041,
-14.6338184322888));
#361496=CARTESIAN_POINT('Ctrl Pts',(0.11155694551423,1.5081352756803,-14.6426413061636));
#361497=CARTESIAN_POINT('Ctrl Pts',(0.495135269222907,1.42988726169609,
-14.6632697828117));
#361498=CARTESIAN_POINT('Ctrl Pts',(0.680550509755873,1.35150894848779,
-14.674367753098));
#361499=CARTESIAN_POINT('Ctrl Pts',(1.00364455605091,1.13113958357526,-14.6960339938958));
#361500=CARTESIAN_POINT('Ctrl Pts',(1.13991781438308,0.993673545026912,
-14.706408945165));
#361501=CARTESIAN_POINT('Ctrl Pts',(1.35681439160581,0.669566740973199,
-14.7258473533814));
#361502=CARTESIAN_POINT('Ctrl Pts',(1.43331430411777,0.484663366150857,
-14.7355742574361));
#361503=CARTESIAN_POINT('Ctrl Pts',(1.5097428860136,0.0970721898109013,
-14.7571071005661));
#361504=CARTESIAN_POINT('Ctrl Pts',(1.50944017341581,-0.101671470041182,
-14.7681484150024));
#361505=CARTESIAN_POINT('Ctrl Pts',(1.43344868231728,-0.480953874011405,
-14.7892196596674));
#361506=CARTESIAN_POINT('Ctrl Pts',(1.36109153695783,-0.658403087718725,
-14.7986367608878));
#361507=CARTESIAN_POINT('Ctrl Pts',(1.14918218367097,-0.98434035303761,
-14.8178860673269));
#361508=CARTESIAN_POINT('Ctrl Pts',(1.0087251700937,-1.12782793490334,-14.8286295747064));
#361509=CARTESIAN_POINT('Ctrl Pts',(0.683617804911299,-1.34926578512871,
-14.8504223615019));
#361510=CARTESIAN_POINT('Ctrl Pts',(0.503025762151212,-1.4264734675165,
-14.8612557580544));
#361511=CARTESIAN_POINT('Ctrl Pts',(0.209684998456008,-1.4890033745908,
-14.8771060639912));
#361512=CARTESIAN_POINT('Ctrl Pts',(0.104876703558311,-1.5,-14.8824541172474));
#361513=CARTESIAN_POINT('Ctrl Pts',(-7.91033905045424E-15,-1.5,-14.8875));
#361514=CARTESIAN_POINT('Origin',(0.,1.30104260698261E-15,-17.7));
#361515=CARTESIAN_POINT('',(-1.25488059566348E-14,-1.5,-15.45));
#361516=CARTESIAN_POINT('',(-9.08611625561304E-14,-1.5,-15.3875));
#361517=CARTESIAN_POINT('',(-1.83697019872103E-16,-1.5,-17.7));
#361518=CARTESIAN_POINT('Ctrl Pts',(-2.42514341941558E-14,-1.5,-15.45));
#361519=CARTESIAN_POINT('Ctrl Pts',(0.111323301433604,-1.5,-15.4446439551625));
#361520=CARTESIAN_POINT('Ctrl Pts',(0.222528418840014,-1.487610191846,-15.438949435119));
#361521=CARTESIAN_POINT('Ctrl Pts',(0.521588263685572,-1.41982534379392,
-15.4226779991793));
#361522=CARTESIAN_POINT('Ctrl Pts',(0.701387188966607,-1.34015125019033,
-15.4118142500866));
#361523=CARTESIAN_POINT('Ctrl Pts',(1.02369796438871,-1.11425235425986,
-15.3900320963425));
#361524=CARTESIAN_POINT('Ctrl Pts',(1.16221616046766,-0.968913692312363,
-15.3793304514723));
#361525=CARTESIAN_POINT('Ctrl Pts',(1.36979060342105,-0.640129619772863,
-15.3602106305254));
#361526=CARTESIAN_POINT('Ctrl Pts',(1.4397950022009,-0.461644714260468,
-15.3506469285699));
#361527=CARTESIAN_POINT('Ctrl Pts',(1.51072425414865,-0.0810206637609527,
-15.3295011479866));
#361528=CARTESIAN_POINT('Ctrl Pts',(1.50828800418927,0.117985125174841,
-15.3184452708235));
#361529=CARTESIAN_POINT('Ctrl Pts',(1.4265462362482,0.503905578853235,-15.2970052456192));
#361530=CARTESIAN_POINT('Ctrl Pts',(1.34795543831095,0.686987858184746,
-15.2874372068696));
#361531=CARTESIAN_POINT('Ctrl Pts',(1.12740342360153,1.00789447542627,-15.2679118204132));
#361532=CARTESIAN_POINT('Ctrl Pts',(0.989235785780901,1.14380179508466,
-15.2574890235153));
#361533=CARTESIAN_POINT('Ctrl Pts',(0.662921772954764,1.36028138369372,
-15.2357759113474));
#361534=CARTESIAN_POINT('Ctrl Pts',(0.476242679886323,1.43632722737674,
-15.2246819247477));
#361535=CARTESIAN_POINT('Ctrl Pts',(0.0918050218253722,1.50941276067965,
-15.2041555055975));
#361536=CARTESIAN_POINT('Ctrl Pts',(-0.101630965929904,1.50878309871131,
-15.195354252836));
#361537=CARTESIAN_POINT('Ctrl Pts',(-0.480357226858617,1.43422493859728,
-15.1750617171081));
#361538=CARTESIAN_POINT('Ctrl Pts',(-0.661868306335575,1.36002328041678,
-15.1642676040534));
#361539=CARTESIAN_POINT('Ctrl Pts',(-0.990290105863839,1.14405209277072,
-15.1424672031994));
#361540=CARTESIAN_POINT('Ctrl Pts',(-1.13306867305426,1.0028494976295,-15.1316754718731));
#361541=CARTESIAN_POINT('Ctrl Pts',(-1.35022747427309,0.680397702134618,
-15.1122704198588));
#361542=CARTESIAN_POINT('Ctrl Pts',(-1.42543857932541,0.504183174466805,
-15.1030101763592));
#361543=CARTESIAN_POINT('Ctrl Pts',(-1.5075168947896,0.126543024855669,
-15.0820301680475));
#361544=CARTESIAN_POINT('Ctrl Pts',(-1.51111163732494,-0.0718357148492454,
-15.0710091269527));
#361545=CARTESIAN_POINT('Ctrl Pts',(-1.44111936884653,-0.461399458746197,
-15.0493666967362));
#361546=CARTESIAN_POINT('Ctrl Pts',(-1.3671547321,-0.648515270510511,-15.0394296163137));
#361547=CARTESIAN_POINT('Ctrl Pts',(-1.15466029410091,-0.976448604471469,
-15.020096713622));
#361548=CARTESIAN_POINT('Ctrl Pts',(-1.02067685168224,-1.11574616139637,
-15.0097810556618));
#361549=CARTESIAN_POINT('Ctrl Pts',(-0.701495530341301,-1.34071034466502,
-14.9881754320879));
#361550=CARTESIAN_POINT('Ctrl Pts',(-0.517629508292398,-1.42185426682779,
-14.9770751761397));
#361551=CARTESIAN_POINT('Ctrl Pts',(-0.216870396831998,-1.4882347989933,
-14.9607609929715));
#361552=CARTESIAN_POINT('Ctrl Pts',(-0.108480333794644,-1.5,-14.9552192624932));
#361553=CARTESIAN_POINT('Ctrl Pts',(8.01442245901285E-15,-1.5,-14.95));
#361554=CARTESIAN_POINT('Ctrl Pts',(-8.4271029777139E-15,-1.5,-14.8875));
#361555=CARTESIAN_POINT('Ctrl Pts',(-0.0855201633304099,-1.5,-14.8916145907767));
#361556=CARTESIAN_POINT('Ctrl Pts',(-0.171066049806968,-1.4926875449768,
-14.8959335429095));
#361557=CARTESIAN_POINT('Ctrl Pts',(-0.4527262879348,-1.44395797271794,
-14.9108385266642));
#361558=CARTESIAN_POINT('Ctrl Pts',(-0.640931643232649,-1.37082770443278,
-14.9219249573841));
#361559=CARTESIAN_POINT('Ctrl Pts',(-0.971170408162794,-1.15922855412728,
-14.943691331545));
#361560=CARTESIAN_POINT('Ctrl Pts',(-1.11165987404137,-1.02528720584264,
-14.9541712271315));
#361561=CARTESIAN_POINT('Ctrl Pts',(-1.3367117285935,-0.708348419626942,
-14.9738028947048));
#361562=CARTESIAN_POINT('Ctrl Pts',(-1.41786008418202,-0.527486975061614,
-14.9831951680522));
#361563=CARTESIAN_POINT('Ctrl Pts',(-1.50610295132645,-0.143662247154666,
-15.0045187640471));
#361564=CARTESIAN_POINT('Ctrl Pts',(-1.51191577587105,0.0556152855864015,
-15.0155897380882));
#361565=CARTESIAN_POINT('Ctrl Pts',(-1.44722790883372,0.437862624097292,
-15.0368257013388));
#361566=CARTESIAN_POINT('Ctrl Pts',(-1.38010005197985,0.61763562974742,
-15.0465897838943));
#361567=CARTESIAN_POINT('Ctrl Pts',(-1.17783126149847,0.949866536949361,
-15.0655500819249));
#361568=CARTESIAN_POINT('Ctrl Pts',(-1.04171156367606,1.09742626632624,
-15.0761980253114));
#361569=CARTESIAN_POINT('Ctrl Pts',(-0.722895001951393,1.32871820587405,
-15.0979618703878));
#361570=CARTESIAN_POINT('Ctrl Pts',(-0.544108190648435,1.41139051879915,
-15.108860207994));
#361571=CARTESIAN_POINT('Ctrl Pts',(-0.16930443437504,1.50255234182842,
-15.1294252349874));
#361572=CARTESIAN_POINT('Ctrl Pts',(0.0227470043379086,1.51188809314083,
-15.1382641909471));
#361573=CARTESIAN_POINT('Ctrl Pts',(0.409971699885314,1.45675699794972,
-15.1584259671089));
#361574=CARTESIAN_POINT('Ctrl Pts',(0.600820985146348,1.38896201249828,
-15.1694914016676));
#361575=CARTESIAN_POINT('Ctrl Pts',(0.93796296179849,1.18634431453642,-15.19134042197));
#361576=CARTESIAN_POINT('Ctrl Pts',(1.08257277860081,1.05604938901551,-15.2019172685116));
#361577=CARTESIAN_POINT('Ctrl Pts',(1.31567390201647,0.746287006525185,
-15.2217368621657));
#361578=CARTESIAN_POINT('Ctrl Pts',(1.40135803625885,0.569337778598538,
-15.2308701234113));
#361579=CARTESIAN_POINT('Ctrl Pts',(1.50112075384638,0.189363321238377,
-15.2519798154869));
#361580=CARTESIAN_POINT('Ctrl Pts',(1.51298098203424,-0.0102601896058358,
-15.2630700105338));
#361581=CARTESIAN_POINT('Ctrl Pts',(1.45950018878855,-0.395215606541005,
-15.2844564225857));
#361582=CARTESIAN_POINT('Ctrl Pts',(1.39751363149503,-0.577335386345449,
-15.2945741881304));
#361583=CARTESIAN_POINT('Ctrl Pts',(1.20464107988243,-0.915599695925714,
-15.3133666497738));
#361584=CARTESIAN_POINT('Ctrl Pts',(1.07285325728569,-1.06701811961393,
-15.3238550491371));
#361585=CARTESIAN_POINT('Ctrl Pts',(0.760308243858021,-1.30775115601977,
-15.3455794068958));
#361586=CARTESIAN_POINT('Ctrl Pts',(0.583422679771014,-1.39567368120654,
-15.3565321099322));
#361587=CARTESIAN_POINT('Ctrl Pts',(0.265773861282844,-1.4822979631247,
-15.3742212258907));
#361588=CARTESIAN_POINT('Ctrl Pts',(0.133067928039146,-1.50000000000002,
-15.3810977663272));
#361589=CARTESIAN_POINT('Ctrl Pts',(-1.81243908770057E-13,-1.5,-15.3875));
#361590=CARTESIAN_POINT('Origin',(0.,1.30104260698261E-15,-17.7));
#361591=CARTESIAN_POINT('',(-9.91045685139722E-14,-1.5,-15.95));
#361592=CARTESIAN_POINT('',(-5.78875387247641E-14,-1.5,-15.8875));
#361593=CARTESIAN_POINT('',(-1.83697019872103E-16,-1.5,-17.7));
#361594=CARTESIAN_POINT('Ctrl Pts',(-1.9824419883463E-13,-1.5,-15.95));
#361595=CARTESIAN_POINT('Ctrl Pts',(0.139005423550127,-1.50000000000002,
-15.9433120984412));
#361596=CARTESIAN_POINT('Ctrl Pts',(0.277560387205389,-1.48068294817197,
-15.9361092848711));
#361597=CARTESIAN_POINT('Ctrl Pts',(0.600085978486933,-1.38862312983871,
-15.9180345479496));
#361598=CARTESIAN_POINT('Ctrl Pts',(0.776112872049263,-1.29846904643623,
-15.9070611699898));
#361599=CARTESIAN_POINT('Ctrl Pts',(1.08587924465258,-1.0537627108278,-15.8853601302278));
#361600=CARTESIAN_POINT('Ctrl Pts',(1.2158160773737,-0.900716948777619,
-15.8750398304875));
#361601=CARTESIAN_POINT('Ctrl Pts',(1.40463721490438,-0.559860276301527,
-15.8561033486833));
#361602=CARTESIAN_POINT('Ctrl Pts',(1.46440645046521,-0.376748429685064,
-15.8459304683157));
#361603=CARTESIAN_POINT('Ctrl Pts',(1.51302063951444,0.00934783112624828,
-15.8244806760484));
#361604=CARTESIAN_POINT('Ctrl Pts',(1.49853823464877,0.209065615577763,
-15.8133852435789));
#361605=CARTESIAN_POINT('Ctrl Pts',(1.39382524437842,0.587332821171853,
-15.7923703988237));
#361606=CARTESIAN_POINT('Ctrl Pts',(1.30618806903924,0.762611041822026,
-15.7833270293886));
#361607=CARTESIAN_POINT('Ctrl Pts',(1.06959752065909,1.06923064121564,-15.7634268502281));
#361608=CARTESIAN_POINT('Ctrl Pts',(0.923216581814794,1.19789325795466,
-15.7528101324482));
#361609=CARTESIAN_POINT('Ctrl Pts',(0.583132675200652,1.39651825520832,
-15.7309304768275));
#361610=CARTESIAN_POINT('Ctrl Pts',(0.39117351318407,1.46195342463353,-15.7198771937437));
#361611=CARTESIAN_POINT('Ctrl Pts',(0.00321980990958416,1.5120275866676,
-15.6998208135468));
#361612=CARTESIAN_POINT('Ctrl Pts',(-0.18847028855034,1.50024098128145,
-15.6909389129386));
#361613=CARTESIAN_POINT('Ctrl Pts',(-0.56211869449964,1.40434869273489,
-15.6702980709437));
#361614=CARTESIAN_POINT('Ctrl Pts',(-0.740055987160223,1.31927374142842,
-15.6593738658672));
#361615=CARTESIAN_POINT('Ctrl Pts',(-1.05599671268407,1.08368405233533,
-15.6376290025927));
#361616=CARTESIAN_POINT('Ctrl Pts',(-1.19016110651751,0.934367809352227,
-15.6270263417686));
#361617=CARTESIAN_POINT('Ctrl Pts',(-1.38814783449007,0.599384255812547,
-15.6081956021682));
#361618=CARTESIAN_POINT('Ctrl Pts',(-1.45295516418789,0.418554810098528,
-15.5982530450054));
#361619=CARTESIAN_POINT('Ctrl Pts',(-1.51256821159738,0.0350132169417762,
-15.5769451787189));
#361620=CARTESIAN_POINT('Ctrl Pts',(-1.50401150674298,-0.164443593428988,
-15.5658642448094));
#361621=CARTESIAN_POINT('Ctrl Pts',(-1.41052302220585,-0.54653655484083,
-15.5446368580643));
#361622=CARTESIAN_POINT('Ctrl Pts',(-1.32731037887536,-0.725612665524742,
-15.5353710096694));
#361623=CARTESIAN_POINT('Ctrl Pts',(-1.09860541639505,-1.0393070754435,
-15.5156537034228));
#361624=CARTESIAN_POINT('Ctrl Pts',(-0.956240325103892,-1.17161411743875,
-15.5051289641634));
#361625=CARTESIAN_POINT('Ctrl Pts',(-0.622849133757918,-1.3791768632517,
-15.4833230411629));
#361626=CARTESIAN_POINT('Ctrl Pts',(-0.433429747115656,-1.44990464399728,
-15.4722449360977));
#361627=CARTESIAN_POINT('Ctrl Pts',(-0.157575290483857,-1.49379678385447,
-15.4577536562577));
#361628=CARTESIAN_POINT('Ctrl Pts',(-0.0787664422449298,-1.5,-15.4537896522194));
#361629=CARTESIAN_POINT('Ctrl Pts',(-2.49139148933975E-14,-1.5,-15.45));
#361630=CARTESIAN_POINT('Ctrl Pts',(-1.81538628092389E-13,-1.5,-15.3875));
#361631=CARTESIAN_POINT('Ctrl Pts',(-0.0563819164787718,-1.49999999999999,
-15.3902126762214));
#361632=CARTESIAN_POINT('Ctrl Pts',(-0.112820272486968,-1.49682133988549,
-15.3930163640053));
#361633=CARTESIAN_POINT('Ctrl Pts',(-0.366693800802395,-1.46802622167381,
-15.4060307242262));
#361634=CARTESIAN_POINT('Ctrl Pts',(-0.557892872152436,-1.4065213599787,
-15.416938262216));
#361635=CARTESIAN_POINT('Ctrl Pts',(-0.900375697723385,-1.21521133216021,
-15.4387301422834));
#361636=CARTESIAN_POINT('Ctrl Pts',(-1.04943199886932,-1.08909227907259,
-15.4494049239462));
#361637=CARTESIAN_POINT('Ctrl Pts',(-1.29133268505232,-0.787292734249682,
-15.4694266968261));
#361638=CARTESIAN_POINT('Ctrl Pts',(-1.38192952606011,-0.614527613446004,
-15.4783595770309));
#361639=CARTESIAN_POINT('Ctrl Pts',(-1.49412509971429,-0.238900033630599,
-15.4992277759095));
#361640=CARTESIAN_POINT('Ctrl Pts',(-1.51259570348729,-0.0391031199996457,
-15.5103276044446));
#361641=CARTESIAN_POINT('Ctrl Pts',(-1.47140529217722,0.348608984033488,
-15.5318671657798));
#361642=CARTESIAN_POINT('Ctrl Pts',(-1.41502953905832,0.533175050865238,
-15.5421208361593));
#361643=CARTESIAN_POINT('Ctrl Pts',(-1.23170628994585,0.879224217244925,
-15.5613457898471));
#361644=CARTESIAN_POINT('Ctrl Pts',(-1.10338153525748,1.03572364197227,
-15.5715169656327));
#361645=CARTESIAN_POINT('Ctrl Pts',(-0.796023642645709,1.28640426416543,
-15.5932680797523));
#361646=CARTESIAN_POINT('Ctrl Pts',(-0.62112711033994,1.37938163956646,
-15.6042654979584));
#361647=CARTESIAN_POINT('Ctrl Pts',(-0.251426690538926,1.49092995580701,
-15.6251512820394));
#361648=CARTESIAN_POINT('Ctrl Pts',(-0.0608274576246367,1.5107522237239,
-15.6342747646995));
#361649=CARTESIAN_POINT('Ctrl Pts',(0.326562741336238,1.47746883594747,
-15.6538376228864));
#361650=CARTESIAN_POINT('Ctrl Pts',(0.519344095745307,1.42120313751349,
-15.6646757561926));
#361651=CARTESIAN_POINT('Ctrl Pts',(0.867345798213808,1.23908164937997,
-15.6864779261351));
#361652=CARTESIAN_POINT('Ctrl Pts',(1.02013094421681,1.11667248839913,-15.6972290593712));
#361653=CARTESIAN_POINT('Ctrl Pts',(1.26952313129237,0.821751391166321,
-15.7174201992672));
#361654=CARTESIAN_POINT('Ctrl Pts',(1.36427593646597,0.652469554342664,
-15.7262516914256));
#361655=CARTESIAN_POINT('Ctrl Pts',(1.48692449351355,0.28064626582611,-15.7469085407876));
#361656=CARTESIAN_POINT('Ctrl Pts',(1.51101166939509,0.0808688019443721,
-15.758007288781));
#361657=CARTESIAN_POINT('Ctrl Pts',(1.48032070916219,-0.30887591067725,
-15.7796597728155));
#361658=CARTESIAN_POINT('Ctrl Pts',(1.42876679947988,-0.4953786169298,-15.790021034274));
#361659=CARTESIAN_POINT('Ctrl Pts',(1.25523973112578,-0.844827663861237,
-15.8094348702146));
#361660=CARTESIAN_POINT('Ctrl Pts',(1.13261743009202,-1.00327631324769,
-15.8192090382999));
#361661=CARTESIAN_POINT('Ctrl Pts',(0.834015518184608,-1.26219443505352,
-15.8407676995351));
#361662=CARTESIAN_POINT('Ctrl Pts',(0.66143190822918,-1.36059728730173,
-15.851804544903));
#361663=CARTESIAN_POINT('Ctrl Pts',(0.321498956392526,-1.47402512943341,
-15.8713103500663));
#361664=CARTESIAN_POINT('Ctrl Pts',(0.161184406212371,-1.50000000000001,
-15.8797450116404));
#361665=CARTESIAN_POINT('Ctrl Pts',(-1.15324416682938E-13,-1.5,-15.8875));
#361666=CARTESIAN_POINT('Origin',(0.,1.30104260698261E-15,-17.7));
#361667=CARTESIAN_POINT('',(-3.52181723406995E-14,-1.5,-16.45));
#361668=CARTESIAN_POINT('',(-3.28061311267145E-9,-1.5,-16.3875000003157));
#361669=CARTESIAN_POINT('',(-1.83697019872103E-16,-1.5,-17.7));
#361670=CARTESIAN_POINT('Ctrl Pts',(-7.03256897160998E-14,-1.5,-16.45));
#361671=CARTESIAN_POINT('Ctrl Pts',(0.168036425573696,-1.50000000000001,
-16.4419153437051));
#361672=CARTESIAN_POINT('Ctrl Pts',(0.335044197307986,-1.4717685684019,
-16.4330959721079));
#361673=CARTESIAN_POINT('Ctrl Pts',(0.680086032609039,-1.35140886275186,
-16.4131518139098));
#361674=CARTESIAN_POINT('Ctrl Pts',(0.851531443639169,-1.2504870512757,
-16.4020997590736));
#361675=CARTESIAN_POINT('Ctrl Pts',(1.14601371920132,-0.987774246726167,
-16.3806338960805));
#361676=CARTESIAN_POINT('Ctrl Pts',(1.26599579666737,-0.82842018359447,
-16.371023343533));
#361677=CARTESIAN_POINT('Ctrl Pts',(1.43490714469483,-0.477395294625578,
-16.3515219608125));
#361678=CARTESIAN_POINT('Ctrl Pts',(1.4841605975908,-0.290020872063163,
-16.3411122706702));
#361679=CARTESIAN_POINT('Ctrl Pts',(1.50986212260163,0.100587505098709,
-16.3194118052723));
#361680=CARTESIAN_POINT('Ctrl Pts',(1.48311557158905,0.300302548213859,
-16.3083165250992));
#361681=CARTESIAN_POINT('Ctrl Pts',(1.35554797880811,0.670289337794323,
-16.2877617034559));
#361682=CARTESIAN_POINT('Ctrl Pts',(1.25882822940715,0.83794366300827,-16.2789558552313));
#361683=CARTESIAN_POINT('Ctrl Pts',(1.00588056946405,1.1295673883459,-16.2586852462309));
#361684=CARTESIAN_POINT('Ctrl Pts',(0.85134626809255,1.25016646854075,-16.2479002367397));
#361685=CARTESIAN_POINT('Ctrl Pts',(0.500796045646876,1.42784262728117,
-16.2260989324447));
#361686=CARTESIAN_POINT('Ctrl Pts',(0.307311031573199,1.48159135488892,
-16.2152968601533));
#361687=CARTESIAN_POINT('Ctrl Pts',(-0.0804273149057107,1.5098304912482,
-16.1958573698059));
#361688=CARTESIAN_POINT('Ctrl Pts',(-0.270721495045628,1.48754355738367,
-16.1866288937016));
#361689=CARTESIAN_POINT('Ctrl Pts',(-0.639161421773415,1.37115465935108,
-16.1656692945166));
#361690=CARTESIAN_POINT('Ctrl Pts',(-0.813047372594786,1.27575252329573,
-16.1546531434721));
#361691=CARTESIAN_POINT('Ctrl Pts',(-1.11651136080784,1.02137886522145,
-16.1329867905853));
#361692=CARTESIAN_POINT('Ctrl Pts',(-1.24228452751426,0.864007809213955,
-16.1230004338451));
#361693=CARTESIAN_POINT('Ctrl Pts',(-1.42125313546844,0.516437942199717,
-16.1036909967887));
#361694=CARTESIAN_POINT('Ctrl Pts',(-1.47549587742737,0.330996665444978,
-16.0933887036357));
#361695=CARTESIAN_POINT('Ctrl Pts',(-1.51203470326867,-0.0576521809014891,
-16.0717971010609));
#361696=CARTESIAN_POINT('Ctrl Pts',(-1.4910723524167,-0.257459318260953,
-16.0606967045409));
#361697=CARTESIAN_POINT('Ctrl Pts',(-1.37422796518395,-0.631411640728053,
-16.039921575515));
#361698=CARTESIAN_POINT('Ctrl Pts',(-1.28178637871755,-0.802623545105735,
-16.031041544091));
#361699=CARTESIAN_POINT('Ctrl Pts',(-1.03656461337122,-1.10138523312758,
-16.0109443706265));
#361700=CARTESIAN_POINT('Ctrl Pts',(-0.885848333753066,-1.22587711713333,
-16.0002349223534));
#361701=CARTESIAN_POINT('Ctrl Pts',(-0.540894576375725,-1.41314385564441,
-15.9784364731159));
#361702=CARTESIAN_POINT('Ctrl Pts',(-0.348977633880678,-1.47233713149717,
-15.9675586072523));
#361703=CARTESIAN_POINT('Ctrl Pts',(-0.100798107708362,-1.49746273757136,
-15.95492013073));
#361704=CARTESIAN_POINT('Ctrl Pts',(-0.0503728797114157,-1.49999999999999,
-15.9524235663051));
#361705=CARTESIAN_POINT('Ctrl Pts',(-1.98025440008072E-13,-1.5,-15.95));
#361706=CARTESIAN_POINT('Ctrl Pts',(-1.15591380429656E-13,-1.5,-15.8875));
#361707=CARTESIAN_POINT('Ctrl Pts',(-0.0282996953382467,-1.5,-15.8888615697268));
#361708=CARTESIAN_POINT('Ctrl Pts',(-0.0566240871054407,-1.49919914153783,
-15.8902465737296));
#361709=CARTESIAN_POINT('Ctrl Pts',(-0.283485129586087,-1.48633215611448,
-15.9015188469868));
#361710=CARTESIAN_POINT('Ctrl Pts',(-0.477791833083697,-1.43570158758071,
-15.9122738372991));
#361711=CARTESIAN_POINT('Ctrl Pts',(-0.831408146007146,-1.26356018264295,
-15.9340689157798));
#361712=CARTESIAN_POINT('Ctrl Pts',(-0.988071982085702,-1.14522831828112,
-15.9448934043398));
#361713=CARTESIAN_POINT('Ctrl Pts',(-1.24539023513224,-0.857683675651588,
-15.9652609857459));
#361714=CARTESIAN_POINT('Ctrl Pts',(-1.34452115083349,-0.692011402109955,
-15.9740549221051));
#361715=CARTESIAN_POINT('Ctrl Pts',(-1.47809729028292,-0.324304246911353,
-15.994483097394));
#361716=CARTESIAN_POINT('Ctrl Pts',(-1.50810420074621,-0.124712286570321,
-16.0055715396351));
#361717=CARTESIAN_POINT('Ctrl Pts',(-1.48853544451949,0.266868562855922,
-16.0273260312699));
#361718=CARTESIAN_POINT('Ctrl Pts',(-1.4421174985353,0.455272106590349,
-16.0377928948107));
#361719=CARTESIAN_POINT('Ctrl Pts',(-1.2788482198455,0.808200849278024,
-16.0574000471822));
#361720=CARTESIAN_POINT('Ctrl Pts',(-1.16205342557626,0.968652795358693,
-16.066831033921));
#361721=CARTESIAN_POINT('Ctrl Pts',(-0.872599471298887,1.23593064859787,
-16.0881817786015));
#361722=CARTESIAN_POINT('Ctrl Pts',(-0.702585751391358,1.33989755061812,
-16.099249537015));
#361723=CARTESIAN_POINT('Ctrl Pts',(-0.338806177850127,1.47356192521677,
-16.1204647892019));
#361724=CARTESIAN_POINT('Ctrl Pts',(-0.149481621918083,1.50458947598212,
-16.1301805766684));
#361725=CARTESIAN_POINT('Ctrl Pts',(0.239299609749548,1.49407842338806,
-16.1491777960815));
#361726=CARTESIAN_POINT('Ctrl Pts',(0.434987759787139,1.44923946858524,
-16.1598383731123));
#361727=CARTESIAN_POINT('Ctrl Pts',(0.794035116108409,1.28745866283198,
-16.1816069583685));
#361728=CARTESIAN_POINT('Ctrl Pts',(0.954546097189385,1.17341011083296,
-16.1924975618797));
#361729=CARTESIAN_POINT('Ctrl Pts',(1.2198857778125,0.893439019887669,-16.2130406979644));
#361730=CARTESIAN_POINT('Ctrl Pts',(1.32343910677365,0.731340871006502,
-16.2218699516109));
#361731=CARTESIAN_POINT('Ctrl Pts',(1.46793947870625,0.367886953782886,
-16.2420618359011));
#361732=CARTESIAN_POINT('Ctrl Pts',(1.50390407689632,0.168652212602878,
-16.2531304326333));
#361733=CARTESIAN_POINT('Ctrl Pts',(1.49558655333712,-0.224460277777845,
-16.2749700154322));
#361734=CARTESIAN_POINT('Ctrl Pts',(1.45439300750538,-0.414631844673234,
-16.285535102482));
#361735=CARTESIAN_POINT('Ctrl Pts',(1.30139496490231,-0.770963910381184,
-16.3053313283546));
#361736=CARTESIAN_POINT('Ctrl Pts',(1.19029155446738,-0.933396272503928,
-16.3144930784542));
#361737=CARTESIAN_POINT('Ctrl Pts',(0.909964975941346,-1.20878284364848,
-16.3356299242282));
#361738=CARTESIAN_POINT('Ctrl Pts',(0.742666467555146,-1.31819339066415,
-16.3467182593274));
#361739=CARTESIAN_POINT('Ctrl Pts',(0.382138693371518,-1.46296970865467,
-16.3680857243389));
#361740=CARTESIAN_POINT('Ctrl Pts',(0.193358648206561,-1.49964906173907,
-16.3781872794157));
#361741=CARTESIAN_POINT('Ctrl Pts',(0.00182787874326844,-1.49999916475107,
-16.3874120329417));
#361742=CARTESIAN_POINT('Ctrl Pts',(0.000913917476143004,-1.500000000004,
-16.387456029125));
#361743=CARTESIAN_POINT('Ctrl Pts',(-6.56122786601575E-9,-1.5,-16.3875000003157));
#361744=CARTESIAN_POINT('Origin',(0.,1.30104260698261E-15,-17.7));
#361745=CARTESIAN_POINT('',(-3.27497425406278E-15,-1.5,-16.95));
#361746=CARTESIAN_POINT('',(7.40069566007051E-14,-1.5,-16.8875));
#361747=CARTESIAN_POINT('',(-1.83697019872103E-16,-1.5,-17.7));
#361748=CARTESIAN_POINT('Ctrl Pts',(-6.36625148825346E-15,-1.5,-16.95));
#361749=CARTESIAN_POINT('Ctrl Pts',(0.00717878911557301,-1.5,-16.9496546103476));
#361750=CARTESIAN_POINT('Ctrl Pts',(0.0143597453507418,-1.49994846502973,
-16.9493076849027));
#361751=CARTESIAN_POINT('Ctrl Pts',(0.212376106994468,-1.49710435039622,
-16.9397016150769));
#361752=CARTESIAN_POINT('Ctrl Pts',(0.400911243289437,-1.45796825101003,
-16.9295436002308));
#361753=CARTESIAN_POINT('Ctrl Pts',(0.759987383851973,-1.3083234108683,
-16.9081107402479));
#361754=CARTESIAN_POINT('Ctrl Pts',(0.926044855054272,-1.1965525530469,
-16.897016550389));
#361755=CARTESIAN_POINT('Ctrl Pts',(1.20235571743438,-0.917667416345093,
-16.8759757284716));
#361756=CARTESIAN_POINT('Ctrl Pts',(1.31099152978271,-0.754365753138052,
-16.8669092085077));
#361757=CARTESIAN_POINT('Ctrl Pts',(1.45945581927049,-0.396556979756925,
-16.8470309433198));
#361758=CARTESIAN_POINT('Ctrl Pts',(1.4983193728066,-0.205649305285253,
-16.8364249614047));
#361759=CARTESIAN_POINT('Ctrl Pts',(1.50163878727677,0.188039890760164,
-16.8145533394022));
#361760=CARTESIAN_POINT('Ctrl Pts',(1.46303737424034,0.387061948217881,
-16.8034965584324));
#361761=CARTESIAN_POINT('Ctrl Pts',(1.31372064674803,0.748597044662741,
-16.7834112752965));
#361762=CARTESIAN_POINT('Ctrl Pts',(1.20819922581391,0.909131369903976,
-16.7745425298575));
#361763=CARTESIAN_POINT('Ctrl Pts',(0.939292039335553,1.18569679716197,
-16.7539223538365));
#361764=CARTESIAN_POINT('Ctrl Pts',(0.777097385352746,1.29779011578116,
-16.7430050566133));
#361765=CARTESIAN_POINT('Ctrl Pts',(0.415719640656572,1.45488122333486,
-16.7212546198885));
#361766=CARTESIAN_POINT('Ctrl Pts',(0.219471117337767,1.49711751151553,
-16.7106393781808));
#361767=CARTESIAN_POINT('Ctrl Pts',(-0.169562171286055,1.50247953702935,
-16.6917730602017));
#361768=CARTESIAN_POINT('Ctrl Pts',(-0.358634652400107,1.46888588907569,
-16.6818809013823));
#361769=CARTESIAN_POINT('Ctrl Pts',(-0.72098912092783,1.33012556726985,
-16.6605926605033));
#361770=CARTESIAN_POINT('Ctrl Pts',(-0.889782806071457,1.22366226856375,
-16.6495142566874));
#361771=CARTESIAN_POINT('Ctrl Pts',(-1.17507366301727,0.952658247764962,
-16.6282603044662));
#361772=CARTESIAN_POINT('Ctrl Pts',(-1.28925790013609,0.791301639710218,
-16.6189612022061));
#361773=CARTESIAN_POINT('Ctrl Pts',(-1.44784764442517,0.436812377816807,
-16.5992673543232));
#361774=CARTESIAN_POINT('Ctrl Pts',(-1.49189503873834,0.247586245339542,
-16.5887547914078));
#361775=CARTESIAN_POINT('Ctrl Pts',(-1.5063509150992,-0.144730905312155,
-16.5669593941493));
#361776=CARTESIAN_POINT('Ctrl Pts',(-1.47363286889394,-0.344181505946763,
-16.5558788052252));
#361777=CARTESIAN_POINT('Ctrl Pts',(-1.33507745593545,-0.709967243911615,
-16.5355573753382));
#361778=CARTESIAN_POINT('Ctrl Pts',(-1.23393748040781,-0.874005706767427,
-16.526756575074));
#361779=CARTESIAN_POINT('Ctrl Pts',(-0.972975121217884,-1.15812390953611,
-16.5063088454143));
#361780=CARTESIAN_POINT('Ctrl Pts',(-0.814553352492015,-1.27452938786755,
-16.4954532890034));
#361781=CARTESIAN_POINT('Ctrl Pts',(-0.458437576191844,-1.44199606386582,
-16.4736678086166));
#361782=CARTESIAN_POINT('Ctrl Pts',(-0.263482699756925,-1.49000622960536,
-16.4629544220358));
#361783=CARTESIAN_POINT('Ctrl Pts',(-0.0432058286522188,-1.49953365893944,
-16.4520916953186));
#361784=CARTESIAN_POINT('Ctrl Pts',(-0.0215950339203933,-1.5,-16.4510389915539));
#361785=CARTESIAN_POINT('Ctrl Pts',(-7.0252647661527E-14,-1.5,-16.45));
#361786=CARTESIAN_POINT('Ctrl Pts',(-6.56122874781451E-9,-1.5,-16.3875000003157));
#361787=CARTESIAN_POINT('Ctrl Pts',(-0.197760835115308,-1.49999999913496,
-16.3970147726398));
#361788=CARTESIAN_POINT('Ctrl Pts',(-0.393674363985098,-1.46088922717867,
-16.4075270770246));
#361789=CARTESIAN_POINT('Ctrl Pts',(-0.756980891744115,-1.30966991596929,
-16.4292072069137));
#361790=CARTESIAN_POINT('Ctrl Pts',(-0.921128318171999,-1.19990983310728,
-16.4401536448406));
#361791=CARTESIAN_POINT('Ctrl Pts',(-1.19422167497537,-0.9273709277071,
-16.460863380246));
#361792=CARTESIAN_POINT('Ctrl Pts',(-1.30205526275989,-0.768652145532881,
-16.4697971030261));
#361793=CARTESIAN_POINT('Ctrl Pts',(-1.45614334856541,-0.411354813164807,
-16.4896469548243));
#361794=CARTESIAN_POINT('Ctrl Pts',(-1.49779139671246,-0.214869528570988,
-16.5005628039684));
#361795=CARTESIAN_POINT('Ctrl Pts',(-1.50197888629897,0.177339198454728,
-16.522352177692));
#361796=CARTESIAN_POINT('Ctrl Pts',(-1.46663648684746,0.36929929400795,
-16.533016627445));
#361797=CARTESIAN_POINT('Ctrl Pts',(-1.32497448529002,0.729294436104746,
-16.5530163575615));
#361798=CARTESIAN_POINT('Ctrl Pts',(-1.21999111521496,0.893897793943286,
-16.5619669777115));
#361799=CARTESIAN_POINT('Ctrl Pts',(-0.949687696780064,1.17794207999332,
-16.5828620760514));
#361800=CARTESIAN_POINT('Ctrl Pts',(-0.785538396757973,1.2932036942435,
-16.593961424438));
#361801=CARTESIAN_POINT('Ctrl Pts',(-0.42874359030238,1.45007444994965,
-16.6154852435592));
#361802=CARTESIAN_POINT('Ctrl Pts',(-0.240632039256655,1.49286834004424,
-16.625724483948));
#361803=CARTESIAN_POINT('Ctrl Pts',(0.150965629028709,1.50580608204866,
-16.6449246172702));
#361804=CARTESIAN_POINT('Ctrl Pts',(0.350813587754195,1.47214577207638,
-16.655152255164));
#361805=CARTESIAN_POINT('Ctrl Pts',(0.721214931117633,1.32977784672249,
-16.6769278626988));
#361806=CARTESIAN_POINT('Ctrl Pts',(0.888712464670945,1.22419508548818,
-16.687919446018));
#361807=CARTESIAN_POINT('Ctrl Pts',(1.16912185117981,0.958774356216467,
-16.708783446952));
#361808=CARTESIAN_POINT('Ctrl Pts',(1.28100791450679,0.803180363582307,
-16.71787886869));
#361809=CARTESIAN_POINT('Ctrl Pts',(1.44454094300695,0.450399892657063,
-16.7374777837414));
#361810=CARTESIAN_POINT('Ctrl Pts',(1.49145811670285,0.2551290911654,-16.7483261616021));
#361811=CARTESIAN_POINT('Ctrl Pts',(1.50623123857247,-0.137301746650813,
-16.7701278748141));
#361812=CARTESIAN_POINT('Ctrl Pts',(1.47589844403143,-0.330637120387082,
-16.7808687289105));
#361813=CARTESIAN_POINT('Ctrl Pts',(1.34382317997907,-0.693653962162479,
-16.8010363312314));
#361814=CARTESIAN_POINT('Ctrl Pts',(1.24388886091701,-0.86009207853055,
-16.809878149235));
#361815=CARTESIAN_POINT('Ctrl Pts',(0.982011607657436,-1.15122916903297,
-16.8305648658598));
#361816=CARTESIAN_POINT('Ctrl Pts',(0.820640162711084,-1.27130434030765,
-16.841664274549));
#361817=CARTESIAN_POINT('Ctrl Pts',(0.467262008540732,-1.4381909115658,
-16.8633019270092));
#361818=CARTESIAN_POINT('Ctrl Pts',(0.279858196352626,-1.4860778314542,
-16.8736485893462));
#361819=CARTESIAN_POINT('Ctrl Pts',(0.0589934646081979,-1.49913079072886,
-16.8846375309088));
#361820=CARTESIAN_POINT('Ctrl Pts',(0.0294826483031038,-1.5,-16.8860815154222));
#361821=CARTESIAN_POINT('Ctrl Pts',(1.48197610221282E-13,-1.5,-16.8875));
#361822=CARTESIAN_POINT('Origin',(0.,0.,0.));
#361823=CARTESIAN_POINT('',(1.,-0.577350269189625,0.));
#361824=CARTESIAN_POINT('',(1.,0.577350269189625,0.));
#361825=CARTESIAN_POINT('Ctrl Pts',(1.,0.577350269189567,-2.89100513080514E-14));
#361826=CARTESIAN_POINT('Ctrl Pts',(1.,0.,-0.288675134594789));
#361827=CARTESIAN_POINT('Ctrl Pts',(1.,-0.577350269189567,-2.89669235401328E-14));
#361828=CARTESIAN_POINT('Origin',(0.,0.,0.));
#361829=CARTESIAN_POINT('Origin',(-9.08513196663917E-30,1.30104260698261E-15,
-2.72083333333333));
#361830=CARTESIAN_POINT('',(1.92031473636372E-14,-2.75,-1.275));
#361831=CARTESIAN_POINT('Origin',(0.,0.,-1.275));
#361832=CARTESIAN_POINT('',(1.48387956900833E-14,-1.5,0.));
#361833=CARTESIAN_POINT('Origin',(0.,0.,0.));
#361834=CARTESIAN_POINT('Origin',(0.,-6.07153216591882E-15,-1.275));
#361835=CARTESIAN_POINT('',(3.5,-6.5001585456204E-15,-1.7));
#361836=CARTESIAN_POINT('Origin',(0.,-6.07153216591882E-15,-1.7));
#361837=CARTESIAN_POINT('',(3.5,-6.5001585456204E-15,-1.275));
#361838=CARTESIAN_POINT('',(3.5,-6.5001585456204E-15,-1.275));
#361839=CARTESIAN_POINT('Origin',(0.,-6.07153216591882E-15,-1.275));
#361840=CARTESIAN_POINT('Origin',(0.,1.30104260698261E-15,-17.7));
#361841=CARTESIAN_POINT('',(-0.190653686693216,-1.15967294634856,-17.6497595264192));
#361842=CARTESIAN_POINT('Origin',(1.61565205658576E-12,-4.96575003339217E-12,
-17.6497595264242));
#361843=CARTESIAN_POINT('',(1.5,1.19400060681869E-14,-17.325));
#361844=CARTESIAN_POINT('Ctrl Pts',(-0.190653686693157,-1.15967294634849,
-17.6497595264193));
#361845=CARTESIAN_POINT('Ctrl Pts',(-0.0284998709946839,-1.21316624422583,
-17.6232802583166));
#361846=CARTESIAN_POINT('Ctrl Pts',(0.132812584998293,-1.22453742267452,
-17.6019314805365));
#361847=CARTESIAN_POINT('Ctrl Pts',(0.43460101025012,-1.20145302480442,
-17.556617792806));
#361848=CARTESIAN_POINT('Ctrl Pts',(0.585964437952993,-1.1617261501811,
-17.5329612724316));
#361849=CARTESIAN_POINT('Ctrl Pts',(0.869448526794397,-1.02932298167968,
-17.4866550394236));
#361850=CARTESIAN_POINT('Ctrl Pts',(0.998920187452606,-0.936988886374714,
-17.4643879452696));
#361851=CARTESIAN_POINT('Ctrl Pts',(1.23902574358817,-0.688927643824148,
-17.4195390704608));
#361852=CARTESIAN_POINT('Ctrl Pts',(1.32213723929246,-0.544619521972593,
-17.4001916451074));
#361853=CARTESIAN_POINT('Ctrl Pts',(1.43760569485959,-0.296763466124491,
-17.364807974774));
#361854=CARTESIAN_POINT('Ctrl Pts',(1.48023624450735,-0.15035662689787,
-17.3447637554926));
#361855=CARTESIAN_POINT('Ctrl Pts',(1.5,-5.5719318048375E-14,-17.325));
#361856=CARTESIAN_POINT('',(1.05094390383305,-1.07028823734362,-17.325));
#361857=CARTESIAN_POINT('Origin',(0.,1.27054942088145E-15,-17.325));
#361858=CARTESIAN_POINT('',(1.21319421105025E-11,1.30188293868178,-17.5231170613182));
#361859=CARTESIAN_POINT('Ctrl Pts',(1.05094390383306,-1.07028823734362,
-17.325));
#361860=CARTESIAN_POINT('Ctrl Pts',(0.935385993427474,-1.17626791798079,
-17.330344050598));
#361861=CARTESIAN_POINT('Ctrl Pts',(0.803785254470359,-1.26328904652287,
-17.3359002371836));
#361862=CARTESIAN_POINT('Ctrl Pts',(0.516934873238126,-1.39355888591543,
-17.3470910935073));
#361863=CARTESIAN_POINT('Ctrl Pts',(0.363306541543587,-1.43555902061286,
-17.3526546969488));
#361864=CARTESIAN_POINT('Ctrl Pts',(0.0426040379259422,-1.47015363976017,
-17.3634241785173));
#361865=CARTESIAN_POINT('Ctrl Pts',(-0.153813269939513,-1.46406932942307,
-17.3692656832653));
#361866=CARTESIAN_POINT('Ctrl Pts',(-0.544498419837906,-1.34782426630485,
-17.3835915070066));
#361867=CARTESIAN_POINT('Ctrl Pts',(-0.712708756400491,-1.25901794320711,
-17.3905532160389));
#361868=CARTESIAN_POINT('Ctrl Pts',(-0.994597414971914,-1.02998098075363,
-17.4038861495252));
#361869=CARTESIAN_POINT('Ctrl Pts',(-1.10896900381996,-0.895834524037364,
-17.4101516283496));
#361870=CARTESIAN_POINT('Ctrl Pts',(-1.31543167012074,-0.538181445013064,
-17.4238015714036));
#361871=CARTESIAN_POINT('Ctrl Pts',(-1.3550125850498,-0.35227324511601,
-17.4305084599621));
#361872=CARTESIAN_POINT('Ctrl Pts',(-1.39356381858887,-0.0519947242753176,
-17.4418520811531));
#361873=CARTESIAN_POINT('Ctrl Pts',(-1.38187430699883,0.12723752056229,
-17.4487219473622));
#361874=CARTESIAN_POINT('Ctrl Pts',(-1.29309014390597,0.463770583356018,
-17.4618139578014));
#361875=CARTESIAN_POINT('Ctrl Pts',(-1.21939859014006,0.619852828413784,
-17.4676355285718));
#361876=CARTESIAN_POINT('Ctrl Pts',(-1.01621515776853,0.898746785102145,
-17.4797586572927));
#361877=CARTESIAN_POINT('Ctrl Pts',(-0.88577741068908,1.01869874939368,
-17.4864917330467));
#361878=CARTESIAN_POINT('Ctrl Pts',(-0.592305977603864,1.19696902839803,
-17.5000787478208));
#361879=CARTESIAN_POINT('Ctrl Pts',(-0.4335679262802,1.25612063590089,-17.5067931009191));
#361880=CARTESIAN_POINT('Ctrl Pts',(-0.19744601600065,1.29605054472226,
-17.5159479725373));
#361881=CARTESIAN_POINT('Ctrl Pts',(-0.106030063883377,1.30560924308118,
-17.5193907569208));
#361882=CARTESIAN_POINT('Ctrl Pts',(2.42640436556823E-11,1.30188293868178,
-17.5231170613182));
#361883=CARTESIAN_POINT('',(-1.37772764904077E-16,1.125,-17.7));
#361884=CARTESIAN_POINT('',(-1.37772764904077E-16,1.125,-17.7));
#361885=CARTESIAN_POINT('Origin',(0.,1.30104260698261E-15,-17.7));
#361886=CARTESIAN_POINT('Ctrl Pts',(2.42640436556823E-11,1.30188293868178,
-17.5231170613182));
#361887=CARTESIAN_POINT('Ctrl Pts',(0.0760719339486668,1.2992094782347,
-17.5257905217639));
#361888=CARTESIAN_POINT('Ctrl Pts',(0.159648962549911,1.28947675310995,
-17.5288785177485));
#361889=CARTESIAN_POINT('Ctrl Pts',(0.40269613660347,1.2320476915949,-17.5385272441259));
#361890=CARTESIAN_POINT('Ctrl Pts',(0.548816268504338,1.16713624115107,
-17.5450297256207));
#361891=CARTESIAN_POINT('Ctrl Pts',(0.818207535128496,0.981215796564792,
-17.5585876105205));
#361892=CARTESIAN_POINT('Ctrl Pts',(0.936716607513114,0.858672224092071,
-17.5655185585548));
#361893=CARTESIAN_POINT('Ctrl Pts',(1.11591095938415,0.579498508975487,
-17.5781734173653));
#361894=CARTESIAN_POINT('Ctrl Pts',(1.17608370721062,0.42793868292318,-17.5841070452516));
#361895=CARTESIAN_POINT('Ctrl Pts',(1.23202197995131,0.11483696308775,-17.5973875990212));
#361896=CARTESIAN_POINT('Ctrl Pts',(1.22996230656325,-0.0417057257492802,
-17.6041323253085));
#361897=CARTESIAN_POINT('Ctrl Pts',(1.16140063641678,-0.374600983755444,
-17.6187180909218));
#361898=CARTESIAN_POINT('Ctrl Pts',(1.08806635420093,-0.523009838130679,
-17.6251950806039));
#361899=CARTESIAN_POINT('Ctrl Pts',(0.926670564829111,-0.759859567065848,
-17.636382069517));
#361900=CARTESIAN_POINT('Ctrl Pts',(0.816778283270273,-0.867993743880628,
-17.6429384269021));
#361901=CARTESIAN_POINT('Ctrl Pts',(0.689217670442692,-0.95192918512462,
-17.6497595264192));
#361902=CARTESIAN_POINT('Origin',(0.,1.30104260698261E-15,-17.7));
#361903=CARTESIAN_POINT('',(0.,1.5,-17.1375));
#361904=CARTESIAN_POINT('Ctrl Pts',(1.48214773787458E-13,-1.5,-16.8875));
#361905=CARTESIAN_POINT('Ctrl Pts',(-0.168700874931512,-1.5,-16.8956166246295));
#361906=CARTESIAN_POINT('Ctrl Pts',(-0.336404258415459,-1.4715456896381,
-16.9044756549396));
#361907=CARTESIAN_POINT('Ctrl Pts',(-0.681664294759072,-1.3505624135401,
-16.9244476327415));
#361908=CARTESIAN_POINT('Ctrl Pts',(-0.852691790631952,-1.24964098115487,
-16.935479570095));
#361909=CARTESIAN_POINT('Ctrl Pts',(-1.14101924136252,-0.992046267738318,
-16.9565071397422));
#361910=CARTESIAN_POINT('Ctrl Pts',(-1.25731577449887,-0.839770223914915,
-16.9658460986716));
#361911=CARTESIAN_POINT('Ctrl Pts',(-1.43092610724364,-0.491934042916581,
-16.9851703309492));
#361912=CARTESIAN_POINT('Ctrl Pts',(-1.48345731807414,-0.298128007144441,
-16.9959373329364));
#361913=CARTESIAN_POINT('Ctrl Pts',(-1.50960821845787,0.0942209676885727,
-17.0177344982049));
#361914=CARTESIAN_POINT('Ctrl Pts',(-1.48470482643099,0.288888827938097,
-17.0285493793299));
#361915=CARTESIAN_POINT('Ctrl Pts',(-1.36291637315436,0.655072135992765,
-17.0488928964441));
#361916=CARTESIAN_POINT('Ctrl Pts',(-1.26827983757057,0.823483999572315,
-17.0576877467413));
#361917=CARTESIAN_POINT('Ctrl Pts',(-1.0153840018506,1.12201042967563,-17.0781476041466));
#361918=CARTESIAN_POINT('Ctrl Pts',(-0.857099532258911,1.24710842449888,
-17.0892380135412));
#361919=CARTESIAN_POINT('Ctrl Pts',(-0.572347677865173,1.39166121246558,
-17.1069534987447));
#361920=CARTESIAN_POINT('Ctrl Pts',(-0.4596082437036,1.4328525882471,-17.1135218821827));
#361921=CARTESIAN_POINT('Ctrl Pts',(-0.23070953814774,1.48664703132354,
-17.1260290663739));
#361922=CARTESIAN_POINT('Ctrl Pts',(-0.115555336796759,1.5,-17.1319403412662));
#361923=CARTESIAN_POINT('Ctrl Pts',(0.,1.5,-17.1375));
#361924=CARTESIAN_POINT('Ctrl Pts',(1.05094390383305,-1.07028823734362,
-17.325));
#361925=CARTESIAN_POINT('Ctrl Pts',(1.19681767290924,-0.927050983124833,
-17.3140028323958));
#361926=CARTESIAN_POINT('Ctrl Pts',(1.29903810567665,-0.749999999999992,
-17.3041666666667));
#361927=CARTESIAN_POINT('Ctrl Pts',(1.73205080756887,5.56731272112934E-15,
-17.2625));
#361928=CARTESIAN_POINT('Ctrl Pts',(1.29903810567665,0.750000000000003,
-17.2208333333333));
#361929=CARTESIAN_POINT('Ctrl Pts',(0.866025403784432,1.50000000000001,
-17.1791666666667));
#361930=CARTESIAN_POINT('Ctrl Pts',(0.,1.5,-17.1375));
#361931=CARTESIAN_POINT('Ctrl Pts',(1.5,-9.16905440462301E-13,-17.325));
#361932=CARTESIAN_POINT('Ctrl Pts',(1.50000000000007,0.113382160049262,
-17.3187009911084));
#361933=CARTESIAN_POINT('Ctrl Pts',(1.48714599278535,0.226394075227564,
-17.3124225513762));
#361934=CARTESIAN_POINT('Ctrl Pts',(1.43685459231838,0.444596795408891,
-17.3003001780328));
#361935=CARTESIAN_POINT('Ctrl Pts',(1.40019786486094,0.549243517321112,
-17.2944864712599));
#361936=CARTESIAN_POINT('Ctrl Pts',(1.27022036812056,0.820121616189383,
-17.2794376879895));
#361937=CARTESIAN_POINT('Ctrl Pts',(1.15630836828071,0.974180856589762,
-17.2702389996247));
#361938=CARTESIAN_POINT('Ctrl Pts',(0.872255139316108,1.23601632287667,
-17.2492992748773));
#361939=CARTESIAN_POINT('Ctrl Pts',(0.703120346224601,1.33947189512315,
-17.2382880074548));
#361940=CARTESIAN_POINT('Ctrl Pts',(0.331429097945265,1.47650377647961,
-17.2165985627852));
#361941=CARTESIAN_POINT('Ctrl Pts',(0.132114621180555,1.50745501208499,
-17.2065634513442));
#361942=CARTESIAN_POINT('Ctrl Pts',(-0.258608395317897,1.48988839341874,
-17.1872768198185));
#361943=CARTESIAN_POINT('Ctrl Pts',(-0.446412994821231,1.44476268630561,
-17.1769875749477));
#361944=CARTESIAN_POINT('Ctrl Pts',(-0.801678290027555,1.28329967090816,
-17.1554097817016));
#361945=CARTESIAN_POINT('Ctrl Pts',(-0.96457328759709,1.16582740490308,
-17.1443093739767));
#361946=CARTESIAN_POINT('Ctrl Pts',(-1.23102809938628,0.878523264761282,
-17.1235088903078));
#361947=CARTESIAN_POINT('Ctrl Pts',(-1.33369501556255,0.713083676857493,
-17.1146157598254));
#361948=CARTESIAN_POINT('Ctrl Pts',(-1.47098536711031,0.351701939382808,
-17.0945389966324));
#361949=CARTESIAN_POINT('Ctrl Pts',(-1.50404981696719,0.159098896944735,
-17.083838827608));
#361950=CARTESIAN_POINT('Ctrl Pts',(-1.49503834317181,-0.233246755242361,
-17.062041846931));
#361951=CARTESIAN_POINT('Ctrl Pts',(-1.45098360774137,-0.429196364751628,
-17.0511557575138));
#361952=CARTESIAN_POINT('Ctrl Pts',(-1.29258205682888,-0.784445130722396,
-17.0314197149599));
#361953=CARTESIAN_POINT('Ctrl Pts',(-1.18290688373643,-0.941734829338834,
-17.022419999831));
#361954=CARTESIAN_POINT('Ctrl Pts',(-0.906484956369989,-1.21104821023222,
-17.0016397164027));
#361955=CARTESIAN_POINT('Ctrl Pts',(-0.740803185746063,-1.31892334248899,
-16.9906718170453));
#361956=CARTESIAN_POINT('Ctrl Pts',(-0.381222093318042,-1.46335566825523,
-16.9693594546205));
#361957=CARTESIAN_POINT('Ctrl Pts',(-0.19142984944887,-1.5,-16.9592101729258));
#361958=CARTESIAN_POINT('Ctrl Pts',(-4.23272528138341E-15,-1.5,-16.95));
#361959=CARTESIAN_POINT('Origin',(-1.04744440165294E-14,-1.5,-17.7));
#361960=CARTESIAN_POINT('Origin',(1.92031473636372E-14,-2.75,-1.7));
#361961=CARTESIAN_POINT('Ctrl Pts',(-0.823407874165082,-0.838564036615827,
-1.7));
#361962=CARTESIAN_POINT('Ctrl Pts',(-0.906490492544621,-0.774359745626708,
-1.7));
#361963=CARTESIAN_POINT('Ctrl Pts',(-0.98024328853839,-0.698926148377459,
-1.7));
#361964=CARTESIAN_POINT('Ctrl Pts',(-1.08660188806759,-0.554873516577794,
-1.7));
#361965=CARTESIAN_POINT('Ctrl Pts',(-1.1486524092587,-0.460342302886378,
-1.7));
#361966=CARTESIAN_POINT('Ctrl Pts',(-1.26101256383043,-0.17907236672097,
-1.7));
#361967=CARTESIAN_POINT('Ctrl Pts',(-1.29189854216959,-0.0173431812158739,
-1.7));
#361968=CARTESIAN_POINT('Ctrl Pts',(-1.29108788069115,0.299928246129644,
-1.7));
#361969=CARTESIAN_POINT('Ctrl Pts',(-1.26280625062506,0.452633561520656,
-1.7));
#361970=CARTESIAN_POINT('Ctrl Pts',(-1.1540332144262,0.739009154469549,
-1.7));
#361971=CARTESIAN_POINT('Ctrl Pts',(-1.06946235041198,0.885676341398372,
-1.70000000000001));
#361972=CARTESIAN_POINT('Ctrl Pts',(-0.838259841587371,1.15024128579277,
-1.70000000000001));
#361973=CARTESIAN_POINT('Ctrl Pts',(-0.700104404477312,1.25940267622837,
-1.7));
#361974=CARTESIAN_POINT('Ctrl Pts',(-0.464671189528445,1.38344546062926,
-1.7));
#361975=CARTESIAN_POINT('Ctrl Pts',(-0.379819280861329,1.41817253578376,
-1.69999999991087));
#361976=CARTESIAN_POINT('Ctrl Pts',(-0.197016232181906,1.47315729177752,
-1.69999999991087));
#361977=CARTESIAN_POINT('Ctrl Pts',(-0.0990761231255047,1.4917436564062,
-1.7));
#361978=CARTESIAN_POINT('Ctrl Pts',(0.,1.49999999999999,-1.7));
#361979=CARTESIAN_POINT('Ctrl Pts',(1.05094390383303,1.07028823734365,-1.7));
#361980=CARTESIAN_POINT('Ctrl Pts',(1.15645058505027,0.945436326977039,
-1.7));
#361981=CARTESIAN_POINT('Ctrl Pts',(1.25865636483395,0.783904299885076,
-1.7));
#361982=CARTESIAN_POINT('Ctrl Pts',(1.37926580863893,0.431617173084607,
-1.7));
#361983=CARTESIAN_POINT('Ctrl Pts',(1.40434751926454,0.262443514736457,
-1.7));
#361984=CARTESIAN_POINT('Ctrl Pts',(1.39184293889025,-0.0842766397941932,
-1.7));
#361985=CARTESIAN_POINT('Ctrl Pts',(1.35147890198672,-0.258564301101902,
-1.69999999999998));
#361986=CARTESIAN_POINT('Ctrl Pts',(1.22264360102688,-0.547784828945173,
-1.69999999999998));
#361987=CARTESIAN_POINT('Ctrl Pts',(1.1307158712709,-0.704303629990696,
-1.69999999996056));
#361988=CARTESIAN_POINT('Ctrl Pts',(0.870778252488567,-0.949211899826218,
-1.69999999996056));
#361989=CARTESIAN_POINT('Ctrl Pts',(0.741392706431225,-1.03250755194956,
-1.7));
#361990=CARTESIAN_POINT('Ctrl Pts',(0.507423555842253,-1.12806524548885,
-1.7));
#361991=CARTESIAN_POINT('Ctrl Pts',(0.410508853202597,-1.15454268439211,
-1.7));
#361992=CARTESIAN_POINT('Ctrl Pts',(0.208302465257298,-1.18420948820834,
-1.7));
#361993=CARTESIAN_POINT('Ctrl Pts',(0.103673587510497,-1.18626732189837,
-1.7));
#361994=CARTESIAN_POINT('Ctrl Pts',(-1.38777878078145E-16,-1.17524047358083,
-1.7));
#361995=CARTESIAN_POINT('Origin',(0.,-6.07153216591882E-15,-1.275));
#361996=CARTESIAN_POINT('Origin',(1.04744440165294E-14,-1.5,0.));
#361997=CARTESIAN_POINT('',(-0.999999999999999,0.577350269189625,0.));
#361998=CARTESIAN_POINT('',(-0.999999999999999,-0.577350269189627,0.));
#361999=CARTESIAN_POINT('Origin',(0.,0.,0.));
#362000=CARTESIAN_POINT('',(3.25260651745651E-16,1.15470053837925,0.));
#362001=CARTESIAN_POINT('Origin',(0.,0.,0.));
#362002=CARTESIAN_POINT('Origin',(0.,0.,0.));
#362003=CARTESIAN_POINT('',(5.42101086242752E-16,-1.15470053837925,0.));
#362004=CARTESIAN_POINT('Origin',(0.,0.,0.));
#362005=CARTESIAN_POINT('Origin',(0.,0.,0.));
#362006=CARTESIAN_POINT('Origin',(0.,0.,0.));
#362007=CARTESIAN_POINT('Ctrl Pts',(0.999999999999951,0.577350269189654,
-2.7791564077117E-14));
#362008=CARTESIAN_POINT('Ctrl Pts',(0.500000000000001,0.866025403784438,
-0.28867513459479));
#362009=CARTESIAN_POINT('Ctrl Pts',(5.09575199449458E-14,1.15470053837922,
-2.90996254149895E-14));
#362010=CARTESIAN_POINT('Origin',(0.,0.,0.));
#362011=CARTESIAN_POINT('Ctrl Pts',(-4.99717345888679E-14,1.15470053837922,
-2.93650291647028E-14));
#362012=CARTESIAN_POINT('Ctrl Pts',(-0.5,0.866025403784438,-0.288675134594791));
#362013=CARTESIAN_POINT('Ctrl Pts',(-0.999999999999949,0.577350269189654,
-2.94219013967842E-14));
#362014=CARTESIAN_POINT('Origin',(0.,0.,0.));
#362015=CARTESIAN_POINT('Ctrl Pts',(-0.999999999999999,0.577350269189567,
-2.99337514855168E-14));
#362016=CARTESIAN_POINT('Ctrl Pts',(-0.999999999999999,-1.33226762955019E-15,
-0.288675134594791));
#362017=CARTESIAN_POINT('Ctrl Pts',(-0.999999999999999,-0.57735026918957,
-2.85119456834816E-14));
#362018=CARTESIAN_POINT('Origin',(0.,0.,0.));
#362019=CARTESIAN_POINT('Ctrl Pts',(-0.999999999999948,-0.577350269189654,
-2.99906237175983E-14));
#362020=CARTESIAN_POINT('Ctrl Pts',(-0.499999999999999,-0.866025403784438,
-0.288675134594791));
#362021=CARTESIAN_POINT('Ctrl Pts',(-4.92134381611157E-14,-1.15470053837922,
-2.91564976470709E-14));
#362022=CARTESIAN_POINT('Origin',(0.,0.,0.));
#362023=CARTESIAN_POINT('Ctrl Pts',(5.0350882802744E-14,-1.15470053837922,
-2.93650291647027E-14));
#362024=CARTESIAN_POINT('Ctrl Pts',(0.5,-0.866025403784437,-0.288675134594791));
#362025=CARTESIAN_POINT('Ctrl Pts',(0.99999999999995,-0.577350269189653,
-2.91944124684585E-14));
#362026=CARTESIAN_POINT('Origin',(1.,-0.577350269189624,-1.19));
#362027=CARTESIAN_POINT('',(1.9352544089507E-16,-1.15470053837925,-1.19));
#362028=CARTESIAN_POINT('',(1.,-0.577350269189624,-1.19));
#362029=CARTESIAN_POINT('',(1.9352544089507E-16,-1.15470053837925,-1.19));
#362030=CARTESIAN_POINT('',(1.,0.577350269189626,-1.19));
#362031=CARTESIAN_POINT('',(1.,-0.577350269189624,-1.19));
#362032=CARTESIAN_POINT('',(3.85779730129493E-16,1.15470053837925,-1.19));
#362033=CARTESIAN_POINT('',(1.,0.577350269189626,-1.19));
#362034=CARTESIAN_POINT('',(-0.999999999999999,0.577350269189625,-1.19));
#362035=CARTESIAN_POINT('',(3.85779730129493E-16,1.15470053837925,-1.19));
#362036=CARTESIAN_POINT('',(-0.999999999999999,-0.577350269189625,-1.19));
#362037=CARTESIAN_POINT('',(-0.999999999999999,0.577350269189625,-1.19));
#362038=CARTESIAN_POINT('',(-0.999999999999999,-0.577350269189625,-1.19));
#362039=CARTESIAN_POINT('Origin',(1.,-0.577350269189624,-1.19));
#362040=CARTESIAN_POINT('',(1.,-0.577350269189624,-1.19));
#362041=CARTESIAN_POINT('',(1.,0.577350269189626,-1.19));
#362042=CARTESIAN_POINT('Origin',(1.,0.577350269189626,-1.19));
#362043=CARTESIAN_POINT('',(3.85779730129493E-16,1.15470053837925,-1.19));
#362044=CARTESIAN_POINT('Origin',(3.85779730129493E-16,1.15470053837925,
-1.19));
#362045=CARTESIAN_POINT('',(-0.999999999999999,0.577350269189625,-1.19));
#362046=CARTESIAN_POINT('Origin',(-0.999999999999999,0.577350269189625,
-1.19));
#362047=CARTESIAN_POINT('',(-0.999999999999999,-0.577350269189625,-1.19));
#362048=CARTESIAN_POINT('Origin',(-0.999999999999999,-0.577350269189625,
-1.19));
#362049=CARTESIAN_POINT('',(1.9352544089507E-16,-1.15470053837925,-1.19));
#362050=CARTESIAN_POINT('Origin',(1.9352544089507E-16,-1.15470053837925,
-1.19));
#362051=CARTESIAN_POINT('Ctrl Pts',(0.,1.17524047358083,-17.95));
#362052=CARTESIAN_POINT('Ctrl Pts',(-0.678525403784434,1.17524047358083,
-17.9083333333333));
#362053=CARTESIAN_POINT('Ctrl Pts',(-1.01778810567665,0.58762023679042,
-17.8666666666667));
#362054=CARTESIAN_POINT('Ctrl Pts',(-1.35705080756887,6.21444700856507E-15,
-17.825));
#362055=CARTESIAN_POINT('Ctrl Pts',(-1.01778810567665,-0.587620236790408,
-17.7833333333333));
#362056=CARTESIAN_POINT('Ctrl Pts',(-0.678525403784435,-1.17524047358082,
-17.7416666666667));
#362057=CARTESIAN_POINT('Ctrl Pts',(-1.43925448419918E-16,-1.17524047358082,
-17.7));
#362058=CARTESIAN_POINT('Ctrl Pts',(0.678525403784434,-1.17524047358082,
-17.6583333333333));
#362059=CARTESIAN_POINT('Ctrl Pts',(1.01778810567665,-0.587620236790409,
-17.6166666666667));
#362060=CARTESIAN_POINT('Ctrl Pts',(1.35705080756887,5.77279150326459E-15,
-17.575));
#362061=CARTESIAN_POINT('Ctrl Pts',(1.01778810567665,0.587620236790419,
-17.5333333333333));
#362062=CARTESIAN_POINT('Ctrl Pts',(0.678525403784435,1.17524047358083,
-17.4916666666667));
#362063=CARTESIAN_POINT('Ctrl Pts',(0.,1.17524047358083,-17.45));
#362064=CARTESIAN_POINT('Ctrl Pts',(-0.678525403784434,1.17524047358083,
-17.4083333333333));
#362065=CARTESIAN_POINT('Ctrl Pts',(-1.01778810567665,0.58762023679042,
-17.3666666666667));
#362066=CARTESIAN_POINT('Ctrl Pts',(-1.35705080756887,5.99589916907193E-15,
-17.325));
#362067=CARTESIAN_POINT('Ctrl Pts',(-1.01778810567665,-0.587620236790408,
-17.2833333333333));
#362068=CARTESIAN_POINT('Ctrl Pts',(-0.678525403784435,-1.17524047358082,
-17.2416666666667));
#362069=CARTESIAN_POINT('Ctrl Pts',(-1.43925448419918E-16,-1.17524047358082,
-17.2));
#362070=CARTESIAN_POINT('Ctrl Pts',(0.678525403784434,-1.17524047358082,
-17.1583333333333));
#362071=CARTESIAN_POINT('Ctrl Pts',(1.01778810567665,-0.587620236790409,
-17.1166666666667));
#362072=CARTESIAN_POINT('Ctrl Pts',(1.35705080756887,5.55424366377145E-15,
-17.075));
#362073=CARTESIAN_POINT('Ctrl Pts',(1.01778810567665,0.587620236790419,
-17.0333333333333));
#362074=CARTESIAN_POINT('Ctrl Pts',(0.678525403784435,1.17524047358083,
-16.9916666666667));
#362075=CARTESIAN_POINT('Ctrl Pts',(0.,1.17524047358083,-16.95));
#362076=CARTESIAN_POINT('Ctrl Pts',(-0.678525403784434,1.17524047358083,
-16.9083333333333));
#362077=CARTESIAN_POINT('Ctrl Pts',(-1.01778810567665,0.58762023679042,
-16.8666666666667));
#362078=CARTESIAN_POINT('Ctrl Pts',(-1.35705080756887,5.77735132957879E-15,
-16.825));
#362079=CARTESIAN_POINT('Ctrl Pts',(-1.01778810567665,-0.587620236790408,
-16.7833333333333));
#362080=CARTESIAN_POINT('Ctrl Pts',(-0.678525403784435,-1.17524047358082,
-16.7416666666667));
#362081=CARTESIAN_POINT('Ctrl Pts',(-1.43925448419918E-16,-1.17524047358082,
-16.7));
#362082=CARTESIAN_POINT('Ctrl Pts',(0.678525403784434,-1.17524047358082,
-16.6583333333333));
#362083=CARTESIAN_POINT('Ctrl Pts',(1.01778810567665,-0.587620236790409,
-16.6166666666667));
#362084=CARTESIAN_POINT('Ctrl Pts',(1.35705080756887,5.33569582427831E-15,
-16.575));
#362085=CARTESIAN_POINT('Ctrl Pts',(1.01778810567665,0.587620236790419,
-16.5333333333333));
#362086=CARTESIAN_POINT('Ctrl Pts',(0.678525403784435,1.17524047358083,
-16.4916666666667));
#362087=CARTESIAN_POINT('Ctrl Pts',(0.,1.17524047358083,-16.45));
#362088=CARTESIAN_POINT('Ctrl Pts',(-0.678525403784434,1.17524047358083,
-16.4083333333333));
#362089=CARTESIAN_POINT('Ctrl Pts',(-1.01778810567665,0.58762023679042,
-16.3666666666667));
#362090=CARTESIAN_POINT('Ctrl Pts',(-1.35705080756887,5.55880349008565E-15,
-16.325));
#362091=CARTESIAN_POINT('Ctrl Pts',(-1.01778810567665,-0.587620236790408,
-16.2833333333333));
#362092=CARTESIAN_POINT('Ctrl Pts',(-0.678525403784435,-1.17524047358082,
-16.2416666666667));
#362093=CARTESIAN_POINT('Ctrl Pts',(-1.43925448419918E-16,-1.17524047358082,
-16.2));
#362094=CARTESIAN_POINT('Ctrl Pts',(0.678525403784434,-1.17524047358082,
-16.1583333333333));
#362095=CARTESIAN_POINT('Ctrl Pts',(1.01778810567665,-0.587620236790409,
-16.1166666666667));
#362096=CARTESIAN_POINT('Ctrl Pts',(1.35705080756887,5.11714798478517E-15,
-16.075));
#362097=CARTESIAN_POINT('Ctrl Pts',(1.01778810567665,0.587620236790419,
-16.0333333333333));
#362098=CARTESIAN_POINT('Ctrl Pts',(0.678525403784435,1.17524047358083,
-15.9916666666667));
#362099=CARTESIAN_POINT('Ctrl Pts',(0.,1.17524047358083,-15.95));
#362100=CARTESIAN_POINT('Ctrl Pts',(-0.678525403784434,1.17524047358083,
-15.9083333333333));
#362101=CARTESIAN_POINT('Ctrl Pts',(-1.01778810567665,0.58762023679042,
-15.8666666666667));
#362102=CARTESIAN_POINT('Ctrl Pts',(-1.35705080756887,5.34025565059251E-15,
-15.825));
#362103=CARTESIAN_POINT('Ctrl Pts',(-1.01778810567665,-0.587620236790409,
-15.7833333333333));
#362104=CARTESIAN_POINT('Ctrl Pts',(-0.678525403784435,-1.17524047358082,
-15.7416666666667));
#362105=CARTESIAN_POINT('Ctrl Pts',(-1.43925448419918E-16,-1.17524047358082,
-15.7));
#362106=CARTESIAN_POINT('Ctrl Pts',(0.678525403784434,-1.17524047358082,
-15.6583333333333));
#362107=CARTESIAN_POINT('Ctrl Pts',(1.01778810567665,-0.587620236790409,
-15.6166666666667));
#362108=CARTESIAN_POINT('Ctrl Pts',(1.35705080756887,4.89860014529203E-15,
-15.575));
#362109=CARTESIAN_POINT('Ctrl Pts',(1.01778810567665,0.587620236790418,
-15.5333333333333));
#362110=CARTESIAN_POINT('Ctrl Pts',(0.678525403784435,1.17524047358083,
-15.4916666666667));
#362111=CARTESIAN_POINT('Ctrl Pts',(0.,1.17524047358083,-15.45));
#362112=CARTESIAN_POINT('Ctrl Pts',(-0.678525403784434,1.17524047358083,
-15.4083333333333));
#362113=CARTESIAN_POINT('Ctrl Pts',(-1.01778810567665,0.587620236790419,
-15.3666666666667));
#362114=CARTESIAN_POINT('Ctrl Pts',(-1.35705080756887,5.12170781109936E-15,
-15.325));
#362115=CARTESIAN_POINT('Ctrl Pts',(-1.01778810567665,-0.587620236790409,
-15.2833333333333));
#362116=CARTESIAN_POINT('Ctrl Pts',(-0.678525403784435,-1.17524047358082,
-15.2416666666667));
#362117=CARTESIAN_POINT('Ctrl Pts',(-1.43925448419918E-16,-1.17524047358082,
-15.2));
#362118=CARTESIAN_POINT('Ctrl Pts',(0.678525403784434,-1.17524047358082,
-15.1583333333333));
#362119=CARTESIAN_POINT('Ctrl Pts',(1.01778810567665,-0.58762023679041,
-15.1166666666667));
#362120=CARTESIAN_POINT('Ctrl Pts',(1.35705080756887,4.68005230579889E-15,
-15.075));
#362121=CARTESIAN_POINT('Ctrl Pts',(1.01778810567665,0.587620236790418,
-15.0333333333333));
#362122=CARTESIAN_POINT('Ctrl Pts',(0.678525403784435,1.17524047358083,
-14.9916666666667));
#362123=CARTESIAN_POINT('Ctrl Pts',(0.,1.17524047358083,-14.95));
#362124=CARTESIAN_POINT('Ctrl Pts',(-0.678525403784434,1.17524047358083,
-14.9083333333333));
#362125=CARTESIAN_POINT('Ctrl Pts',(-1.01778810567665,0.587620236790419,
-14.8666666666667));
#362126=CARTESIAN_POINT('Ctrl Pts',(-1.35705080756887,4.90315997160622E-15,
-14.825));
#362127=CARTESIAN_POINT('Ctrl Pts',(-1.01778810567665,-0.587620236790409,
-14.7833333333333));
#362128=CARTESIAN_POINT('Ctrl Pts',(-0.678525403784435,-1.17524047358082,
-14.7416666666667));
#362129=CARTESIAN_POINT('Ctrl Pts',(-1.43925448419918E-16,-1.17524047358082,
-14.7));
#362130=CARTESIAN_POINT('Ctrl Pts',(0.678525403784434,-1.17524047358082,
-14.6583333333333));
#362131=CARTESIAN_POINT('Ctrl Pts',(1.01778810567665,-0.58762023679041,
-14.6166666666667));
#362132=CARTESIAN_POINT('Ctrl Pts',(1.35705080756887,4.46150446630575E-15,
-14.575));
#362133=CARTESIAN_POINT('Ctrl Pts',(1.01778810567665,0.587620236790418,
-14.5333333333333));
#362134=CARTESIAN_POINT('Ctrl Pts',(0.678525403784435,1.17524047358083,
-14.4916666666667));
#362135=CARTESIAN_POINT('Ctrl Pts',(0.,1.17524047358083,-14.45));
#362136=CARTESIAN_POINT('Ctrl Pts',(-0.678525403784434,1.17524047358083,
-14.4083333333333));
#362137=CARTESIAN_POINT('Ctrl Pts',(-1.01778810567665,0.587620236790419,
-14.3666666666667));
#362138=CARTESIAN_POINT('Ctrl Pts',(-1.35705080756887,4.68461213211308E-15,
-14.325));
#362139=CARTESIAN_POINT('Ctrl Pts',(-1.01778810567665,-0.587620236790409,
-14.2833333333333));
#362140=CARTESIAN_POINT('Ctrl Pts',(-0.678525403784435,-1.17524047358082,
-14.2416666666667));
#362141=CARTESIAN_POINT('Ctrl Pts',(-1.43925448419918E-16,-1.17524047358082,
-14.2));
#362142=CARTESIAN_POINT('Ctrl Pts',(0.678525403784434,-1.17524047358082,
-14.1583333333333));
#362143=CARTESIAN_POINT('Ctrl Pts',(1.01778810567665,-0.58762023679041,
-14.1166666666667));
#362144=CARTESIAN_POINT('Ctrl Pts',(1.35705080756887,4.2429566268126E-15,
-14.075));
#362145=CARTESIAN_POINT('Ctrl Pts',(1.01778810567665,0.587620236790418,
-14.0333333333333));
#362146=CARTESIAN_POINT('Ctrl Pts',(0.678525403784435,1.17524047358083,
-13.9916666666667));
#362147=CARTESIAN_POINT('Ctrl Pts',(0.,1.17524047358083,-13.95));
#362148=CARTESIAN_POINT('Ctrl Pts',(-0.678525403784434,1.17524047358083,
-13.9083333333333));
#362149=CARTESIAN_POINT('Ctrl Pts',(-1.01778810567665,0.587620236790419,
-13.8666666666667));
#362150=CARTESIAN_POINT('Ctrl Pts',(-1.35705080756887,4.46606429261994E-15,
-13.825));
#362151=CARTESIAN_POINT('Ctrl Pts',(-1.01778810567665,-0.58762023679041,
-13.7833333333333));
#362152=CARTESIAN_POINT('Ctrl Pts',(-0.678525403784435,-1.17524047358082,
-13.7416666666667));
#362153=CARTESIAN_POINT('Ctrl Pts',(-1.43925448419918E-16,-1.17524047358082,
-13.7));
#362154=CARTESIAN_POINT('Ctrl Pts',(0.678525403784434,-1.17524047358082,
-13.6583333333333));
#362155=CARTESIAN_POINT('Ctrl Pts',(1.01778810567665,-0.58762023679041,
-13.6166666666667));
#362156=CARTESIAN_POINT('Ctrl Pts',(1.35705080756887,4.02440878731946E-15,
-13.575));
#362157=CARTESIAN_POINT('Ctrl Pts',(1.01778810567665,0.587620236790417,
-13.5333333333333));
#362158=CARTESIAN_POINT('Ctrl Pts',(0.678525403784435,1.17524047358083,
-13.4916666666667));
#362159=CARTESIAN_POINT('Ctrl Pts',(0.,1.17524047358083,-13.45));
#362160=CARTESIAN_POINT('Ctrl Pts',(-0.678525403784434,1.17524047358083,
-13.4083333333333));
#362161=CARTESIAN_POINT('Ctrl Pts',(-1.01778810567665,0.587620236790418,
-13.3666666666667));
#362162=CARTESIAN_POINT('Ctrl Pts',(-1.35705080756887,4.2475164531268E-15,
-13.325));
#362163=CARTESIAN_POINT('Ctrl Pts',(-1.01778810567665,-0.58762023679041,
-13.2833333333333));
#362164=CARTESIAN_POINT('Ctrl Pts',(-0.678525403784435,-1.17524047358082,
-13.2416666666667));
#362165=CARTESIAN_POINT('Ctrl Pts',(-1.43925448419918E-16,-1.17524047358082,
-13.2));
#362166=CARTESIAN_POINT('Ctrl Pts',(0.678525403784434,-1.17524047358082,
-13.1583333333333));
#362167=CARTESIAN_POINT('Ctrl Pts',(1.01778810567665,-0.587620236790411,
-13.1166666666667));
#362168=CARTESIAN_POINT('Ctrl Pts',(1.35705080756887,3.80586094782632E-15,
-13.075));
#362169=CARTESIAN_POINT('Ctrl Pts',(1.01778810567665,0.587620236790417,
-13.0333333333333));
#362170=CARTESIAN_POINT('Ctrl Pts',(0.678525403784435,1.17524047358083,
-12.9916666666667));
#362171=CARTESIAN_POINT('Ctrl Pts',(0.,1.17524047358083,-12.95));
#362172=CARTESIAN_POINT('Ctrl Pts',(-0.678525403784434,1.17524047358083,
-12.9083333333333));
#362173=CARTESIAN_POINT('Ctrl Pts',(-1.01778810567665,0.587620236790418,
-12.8666666666667));
#362174=CARTESIAN_POINT('Ctrl Pts',(-1.35705080756887,4.02896861363366E-15,
-12.825));
#362175=CARTESIAN_POINT('Ctrl Pts',(-1.01778810567665,-0.58762023679041,
-12.7833333333333));
#362176=CARTESIAN_POINT('Ctrl Pts',(-0.678525403784435,-1.17524047358082,
-12.7416666666667));
#362177=CARTESIAN_POINT('Ctrl Pts',(-1.43925448419918E-16,-1.17524047358082,
-12.7));
#362178=CARTESIAN_POINT('Ctrl Pts',(0.678525403784434,-1.17524047358082,
-12.6583333333333));
#362179=CARTESIAN_POINT('Ctrl Pts',(1.01778810567665,-0.587620236790411,
-12.6166666666667));
#362180=CARTESIAN_POINT('Ctrl Pts',(1.35705080756887,3.58731310833318E-15,
-12.575));
#362181=CARTESIAN_POINT('Ctrl Pts',(1.01778810567665,0.587620236790417,
-12.5333333333333));
#362182=CARTESIAN_POINT('Ctrl Pts',(0.678525403784435,1.17524047358083,
-12.4916666666667));
#362183=CARTESIAN_POINT('Ctrl Pts',(0.,1.17524047358083,-12.45));
#362184=CARTESIAN_POINT('Ctrl Pts',(-0.678525403784434,1.17524047358083,
-12.4083333333333));
#362185=CARTESIAN_POINT('Ctrl Pts',(-1.01778810567665,0.587620236790418,
-12.3666666666667));
#362186=CARTESIAN_POINT('Ctrl Pts',(-1.35705080756887,3.81042077414052E-15,
-12.325));
#362187=CARTESIAN_POINT('Ctrl Pts',(-1.01778810567665,-0.58762023679041,
-12.2833333333333));
#362188=CARTESIAN_POINT('Ctrl Pts',(-0.678525403784435,-1.17524047358082,
-12.2416666666667));
#362189=CARTESIAN_POINT('Ctrl Pts',(-1.43925448419918E-16,-1.17524047358082,
-12.2));
#362190=CARTESIAN_POINT('Ctrl Pts',(0.678525403784434,-1.17524047358082,
-12.1583333333333));
#362191=CARTESIAN_POINT('Ctrl Pts',(1.01778810567665,-0.587620236790411,
-12.1166666666667));
#362192=CARTESIAN_POINT('Ctrl Pts',(1.35705080756887,3.36876526884004E-15,
-12.075));
#362193=CARTESIAN_POINT('Ctrl Pts',(1.01778810567665,0.587620236790417,
-12.0333333333333));
#362194=CARTESIAN_POINT('Ctrl Pts',(0.678525403784435,1.17524047358083,
-11.9916666666667));
#362195=CARTESIAN_POINT('Ctrl Pts',(0.,1.17524047358083,-11.95));
#362196=CARTESIAN_POINT('Ctrl Pts',(-0.678525403784434,1.17524047358083,
-11.9083333333333));
#362197=CARTESIAN_POINT('Ctrl Pts',(-1.01778810567665,0.587620236790418,
-11.8666666666667));
#362198=CARTESIAN_POINT('Ctrl Pts',(-1.35705080756887,3.59187293464738E-15,
-11.825));
#362199=CARTESIAN_POINT('Ctrl Pts',(-1.01778810567665,-0.58762023679041,
-11.7833333333333));
#362200=CARTESIAN_POINT('Ctrl Pts',(-0.678525403784435,-1.17524047358082,
-11.7416666666667));
#362201=CARTESIAN_POINT('Ctrl Pts',(-1.43925448419918E-16,-1.17524047358082,
-11.7));
#362202=CARTESIAN_POINT('Ctrl Pts',(0.678525403784434,-1.17524047358083,
-11.6583333333333));
#362203=CARTESIAN_POINT('Ctrl Pts',(1.01778810567665,-0.587620236790411,
-11.6166666666667));
#362204=CARTESIAN_POINT('Ctrl Pts',(1.35705080756887,3.1502174293469E-15,
-11.575));
#362205=CARTESIAN_POINT('Ctrl Pts',(1.01778810567665,0.587620236790417,
-11.5333333333333));
#362206=CARTESIAN_POINT('Ctrl Pts',(0.678525403784435,1.17524047358083,
-11.4916666666667));
#362207=CARTESIAN_POINT('Ctrl Pts',(0.,1.17524047358083,-11.45));
#362208=CARTESIAN_POINT('Ctrl Pts',(-0.678525403784434,1.17524047358083,
-11.4083333333333));
#362209=CARTESIAN_POINT('Ctrl Pts',(-1.01778810567665,0.587620236790417,
-11.3666666666667));
#362210=CARTESIAN_POINT('Ctrl Pts',(-1.35705080756887,3.37332509515423E-15,
-11.325));
#362211=CARTESIAN_POINT('Ctrl Pts',(-1.01778810567665,-0.587620236790411,
-11.2833333333333));
#362212=CARTESIAN_POINT('Ctrl Pts',(-0.678525403784435,-1.17524047358082,
-11.2416666666667));
#362213=CARTESIAN_POINT('Ctrl Pts',(-1.43925448419918E-16,-1.17524047358082,
-11.2));
#362214=CARTESIAN_POINT('Ctrl Pts',(0.678525403784434,-1.17524047358083,
-11.1583333333333));
#362215=CARTESIAN_POINT('Ctrl Pts',(1.01778810567665,-0.587620236790411,
-11.1166666666667));
#362216=CARTESIAN_POINT('Ctrl Pts',(1.35705080756887,2.93166958985376E-15,
-11.075));
#362217=CARTESIAN_POINT('Ctrl Pts',(1.01778810567665,0.587620236790416,
-11.0333333333333));
#362218=CARTESIAN_POINT('Ctrl Pts',(0.678525403784435,1.17524047358083,
-10.9916666666667));
#362219=CARTESIAN_POINT('Ctrl Pts',(0.,1.17524047358083,-10.95));
#362220=CARTESIAN_POINT('Ctrl Pts',(-0.678525403784434,1.17524047358083,
-10.9083333333333));
#362221=CARTESIAN_POINT('Ctrl Pts',(-1.01778810567665,0.587620236790417,
-10.8666666666667));
#362222=CARTESIAN_POINT('Ctrl Pts',(-1.35705080756887,3.15477725566109E-15,
-10.825));
#362223=CARTESIAN_POINT('Ctrl Pts',(-1.01778810567665,-0.587620236790411,
-10.7833333333333));
#362224=CARTESIAN_POINT('Ctrl Pts',(-0.678525403784435,-1.17524047358083,
-10.7416666666667));
#362225=CARTESIAN_POINT('Ctrl Pts',(-1.43925448419918E-16,-1.17524047358083,
-10.7));
#362226=CARTESIAN_POINT('Ctrl Pts',(0.678525403784434,-1.17524047358083,
-10.6583333333333));
#362227=CARTESIAN_POINT('Ctrl Pts',(1.01778810567665,-0.587620236790412,
-10.6166666666667));
#362228=CARTESIAN_POINT('Ctrl Pts',(1.35705080756887,2.71312175036062E-15,
-10.575));
#362229=CARTESIAN_POINT('Ctrl Pts',(1.01778810567665,0.587620236790416,
-10.5333333333333));
#362230=CARTESIAN_POINT('Ctrl Pts',(0.678525403784435,1.17524047358083,
-10.4916666666667));
#362231=CARTESIAN_POINT('Ctrl Pts',(0.,1.17524047358083,-10.45));
#362232=CARTESIAN_POINT('Ctrl Pts',(-0.678525403784434,1.17524047358083,
-10.4083333333333));
#362233=CARTESIAN_POINT('Ctrl Pts',(-1.01778810567665,0.587620236790417,
-10.3666666666667));
#362234=CARTESIAN_POINT('Ctrl Pts',(-1.35705080756887,2.93622941616795E-15,
-10.325));
#362235=CARTESIAN_POINT('Ctrl Pts',(-1.01778810567665,-0.587620236790411,
-10.2833333333333));
#362236=CARTESIAN_POINT('Ctrl Pts',(-0.678525403784435,-1.17524047358083,
-10.2416666666667));
#362237=CARTESIAN_POINT('Ctrl Pts',(-1.43925448419918E-16,-1.17524047358083,
-10.2));
#362238=CARTESIAN_POINT('Ctrl Pts',(0.678525403784434,-1.17524047358083,
-10.1583333333333));
#362239=CARTESIAN_POINT('Ctrl Pts',(1.01778810567665,-0.587620236790412,
-10.1166666666667));
#362240=CARTESIAN_POINT('Ctrl Pts',(1.35705080756887,2.49457391086747E-15,
-10.075));
#362241=CARTESIAN_POINT('Ctrl Pts',(1.01778810567665,0.587620236790416,
-10.0333333333333));
#362242=CARTESIAN_POINT('Ctrl Pts',(0.678525403784435,1.17524047358083,
-9.99166666666667));
#362243=CARTESIAN_POINT('Ctrl Pts',(0.,1.17524047358083,-9.95));
#362244=CARTESIAN_POINT('Ctrl Pts',(-0.678525403784434,1.17524047358083,
-9.90833333333333));
#362245=CARTESIAN_POINT('Ctrl Pts',(-1.01778810567665,0.587620236790417,
-9.86666666666667));
#362246=CARTESIAN_POINT('Ctrl Pts',(-1.35705080756887,2.71768157667481E-15,
-9.825));
#362247=CARTESIAN_POINT('Ctrl Pts',(-1.01778810567665,-0.587620236790411,
-9.78333333333333));
#362248=CARTESIAN_POINT('Ctrl Pts',(-0.678525403784435,-1.17524047358083,
-9.74166666666667));
#362249=CARTESIAN_POINT('Ctrl Pts',(-1.43925448419918E-16,-1.17524047358083,
-9.7));
#362250=CARTESIAN_POINT('Ctrl Pts',(0.678525403784434,-1.17524047358083,
-9.65833333333333));
#362251=CARTESIAN_POINT('Ctrl Pts',(1.01778810567665,-0.587620236790412,
-9.61666666666667));
#362252=CARTESIAN_POINT('Ctrl Pts',(1.35705080756887,2.27602607137433E-15,
-9.575));
#362253=CARTESIAN_POINT('Ctrl Pts',(1.01778810567665,0.587620236790416,
-9.53333333333333));
#362254=CARTESIAN_POINT('Ctrl Pts',(0.678525403784435,1.17524047358083,
-9.49166666666667));
#362255=CARTESIAN_POINT('Ctrl Pts',(0.,1.17524047358083,-9.45));
#362256=CARTESIAN_POINT('Ctrl Pts',(-0.678525403784434,1.17524047358083,
-9.40833333333333));
#362257=CARTESIAN_POINT('Ctrl Pts',(-1.01778810567665,0.587620236790417,
-9.36666666666667));
#362258=CARTESIAN_POINT('Ctrl Pts',(-1.35705080756887,2.49913373718167E-15,
-9.325));
#362259=CARTESIAN_POINT('Ctrl Pts',(-1.01778810567665,-0.587620236790411,
-9.28333333333333));
#362260=CARTESIAN_POINT('Ctrl Pts',(-0.678525403784435,-1.17524047358083,
-9.24166666666667));
#362261=CARTESIAN_POINT('Ctrl Pts',(-1.43925448419918E-16,-1.17524047358083,
-9.2));
#362262=CARTESIAN_POINT('Ctrl Pts',(0.678525403784434,-1.17524047358083,
-9.15833333333333));
#362263=CARTESIAN_POINT('Ctrl Pts',(1.01778810567665,-0.587620236790412,
-9.11666666666667));
#362264=CARTESIAN_POINT('Ctrl Pts',(1.35705080756887,2.05747823188119E-15,
-9.075));
#362265=CARTESIAN_POINT('Ctrl Pts',(1.01778810567665,0.587620236790415,
-9.03333333333333));
#362266=CARTESIAN_POINT('Ctrl Pts',(0.678525403784435,1.17524047358083,
-8.99166666666667));
#362267=CARTESIAN_POINT('Ctrl Pts',(0.,1.17524047358083,-8.95));
#362268=CARTESIAN_POINT('Ctrl Pts',(-0.678525403784434,1.17524047358083,
-8.90833333333333));
#362269=CARTESIAN_POINT('Ctrl Pts',(-1.01778810567665,0.587620236790416,
-8.86666666666667));
#362270=CARTESIAN_POINT('Ctrl Pts',(-1.35705080756887,2.28058589768853E-15,
-8.825));
#362271=CARTESIAN_POINT('Ctrl Pts',(-1.01778810567665,-0.587620236790412,
-8.78333333333333));
#362272=CARTESIAN_POINT('Ctrl Pts',(-0.678525403784435,-1.17524047358083,
-8.74166666666667));
#362273=CARTESIAN_POINT('Ctrl Pts',(-1.43925448419918E-16,-1.17524047358083,
-8.7));
#362274=CARTESIAN_POINT('Ctrl Pts',(0.678525403784434,-1.17524047358083,
-8.65833333333333));
#362275=CARTESIAN_POINT('Ctrl Pts',(1.01778810567665,-0.587620236790413,
-8.61666666666667));
#362276=CARTESIAN_POINT('Ctrl Pts',(1.35705080756887,1.83893039238805E-15,
-8.575));
#362277=CARTESIAN_POINT('Ctrl Pts',(1.01778810567665,0.587620236790415,
-8.53333333333333));
#362278=CARTESIAN_POINT('Ctrl Pts',(0.678525403784435,1.17524047358083,
-8.49166666666667));
#362279=CARTESIAN_POINT('Ctrl Pts',(0.,1.17524047358083,-8.45));
#362280=CARTESIAN_POINT('Ctrl Pts',(-0.678525403784434,1.17524047358083,
-8.40833333333333));
#362281=CARTESIAN_POINT('Ctrl Pts',(-1.01778810567665,0.587620236790416,
-8.36666666666667));
#362282=CARTESIAN_POINT('Ctrl Pts',(-1.35705080756887,2.06203805819539E-15,
-8.325));
#362283=CARTESIAN_POINT('Ctrl Pts',(-1.01778810567665,-0.587620236790412,
-8.28333333333333));
#362284=CARTESIAN_POINT('Ctrl Pts',(-0.678525403784435,-1.17524047358083,
-8.24166666666667));
#362285=CARTESIAN_POINT('Ctrl Pts',(-1.43925448419918E-16,-1.17524047358083,
-8.2));
#362286=CARTESIAN_POINT('Ctrl Pts',(0.678525403784434,-1.17524047358083,
-8.15833333333333));
#362287=CARTESIAN_POINT('Ctrl Pts',(1.01778810567665,-0.587620236790413,
-8.11666666666667));
#362288=CARTESIAN_POINT('Ctrl Pts',(1.35705080756887,1.62038255289491E-15,
-8.075));
#362289=CARTESIAN_POINT('Ctrl Pts',(1.01778810567665,0.587620236790415,
-8.03333333333333));
#362290=CARTESIAN_POINT('Ctrl Pts',(0.678525403784435,1.17524047358083,
-7.99166666666667));
#362291=CARTESIAN_POINT('Ctrl Pts',(0.,1.17524047358083,-7.95));
#362292=CARTESIAN_POINT('Ctrl Pts',(-0.678525403784434,1.17524047358083,
-7.90833333333333));
#362293=CARTESIAN_POINT('Ctrl Pts',(-1.01778810567665,0.587620236790416,
-7.86666666666667));
#362294=CARTESIAN_POINT('Ctrl Pts',(-1.35705080756887,1.84349021870225E-15,
-7.825));
#362295=CARTESIAN_POINT('Ctrl Pts',(-1.01778810567665,-0.587620236790412,
-7.78333333333333));
#362296=CARTESIAN_POINT('Ctrl Pts',(-0.678525403784435,-1.17524047358083,
-7.74166666666667));
#362297=CARTESIAN_POINT('Ctrl Pts',(-1.43925448419918E-16,-1.17524047358083,
-7.7));
#362298=CARTESIAN_POINT('Ctrl Pts',(0.678525403784434,-1.17524047358083,
-7.65833333333334));
#362299=CARTESIAN_POINT('Ctrl Pts',(1.01778810567665,-0.587620236790413,
-7.61666666666667));
#362300=CARTESIAN_POINT('Ctrl Pts',(1.35705080756887,1.40183471340177E-15,
-7.575));
#362301=CARTESIAN_POINT('Ctrl Pts',(1.01778810567665,0.587620236790415,
-7.53333333333333));
#362302=CARTESIAN_POINT('Ctrl Pts',(0.678525403784435,1.17524047358083,
-7.49166666666667));
#362303=CARTESIAN_POINT('Ctrl Pts',(0.,1.17524047358083,-7.45));
#362304=CARTESIAN_POINT('Ctrl Pts',(-0.678525403784434,1.17524047358083,
-7.40833333333333));
#362305=CARTESIAN_POINT('Ctrl Pts',(-1.01778810567665,0.587620236790416,
-7.36666666666667));
#362306=CARTESIAN_POINT('Ctrl Pts',(-1.35705080756887,1.62494237920911E-15,
-7.325));
#362307=CARTESIAN_POINT('Ctrl Pts',(-1.01778810567665,-0.587620236790412,
-7.28333333333333));
#362308=CARTESIAN_POINT('Ctrl Pts',(-0.678525403784435,-1.17524047358083,
-7.24166666666667));
#362309=CARTESIAN_POINT('Ctrl Pts',(-1.43925448419918E-16,-1.17524047358083,
-7.2));
#362310=CARTESIAN_POINT('Ctrl Pts',(0.678525403784434,-1.17524047358083,
-7.15833333333333));
#362311=CARTESIAN_POINT('Ctrl Pts',(1.01778810567665,-0.587620236790413,
-7.11666666666667));
#362312=CARTESIAN_POINT('Ctrl Pts',(1.35705080756887,1.18328687390863E-15,
-7.075));
#362313=CARTESIAN_POINT('Ctrl Pts',(1.01778810567665,0.587620236790415,
-7.03333333333333));
#362314=CARTESIAN_POINT('Ctrl Pts',(0.678525403784435,1.17524047358083,
-6.99166666666667));
#362315=CARTESIAN_POINT('Ctrl Pts',(0.,1.17524047358083,-6.95));
#362316=CARTESIAN_POINT('Ctrl Pts',(-0.678525403784434,1.17524047358083,
-6.90833333333333));
#362317=CARTESIAN_POINT('Ctrl Pts',(-1.01778810567665,0.587620236790415,
-6.86666666666667));
#362318=CARTESIAN_POINT('Ctrl Pts',(-1.35705080756887,1.40639453971596E-15,
-6.825));
#362319=CARTESIAN_POINT('Ctrl Pts',(-1.01778810567665,-0.587620236790413,
-6.78333333333333));
#362320=CARTESIAN_POINT('Ctrl Pts',(-0.678525403784435,-1.17524047358083,
-6.74166666666667));
#362321=CARTESIAN_POINT('Ctrl Pts',(-1.43925448419918E-16,-1.17524047358083,
-6.7));
#362322=CARTESIAN_POINT('Ctrl Pts',(0.678525403784434,-1.17524047358083,
-6.65833333333333));
#362323=CARTESIAN_POINT('Ctrl Pts',(1.01778810567665,-0.587620236790414,
-6.61666666666667));
#362324=CARTESIAN_POINT('Ctrl Pts',(1.35705080756887,9.64739034415485E-16,
-6.575));
#362325=CARTESIAN_POINT('Ctrl Pts',(1.01778810567665,0.587620236790414,
-6.53333333333333));
#362326=CARTESIAN_POINT('Ctrl Pts',(0.678525403784435,1.17524047358083,
-6.49166666666667));
#362327=CARTESIAN_POINT('Ctrl Pts',(0.,1.17524047358083,-6.45));
#362328=CARTESIAN_POINT('Ctrl Pts',(-0.678525403784434,1.17524047358083,
-6.40833333333334));
#362329=CARTESIAN_POINT('Ctrl Pts',(-1.01778810567665,0.587620236790415,
-6.36666666666667));
#362330=CARTESIAN_POINT('Ctrl Pts',(-1.35705080756887,1.18784670022282E-15,
-6.325));
#362331=CARTESIAN_POINT('Ctrl Pts',(-1.01778810567665,-0.587620236790413,
-6.28333333333333));
#362332=CARTESIAN_POINT('Ctrl Pts',(-0.678525403784435,-1.17524047358083,
-6.24166666666667));
#362333=CARTESIAN_POINT('Ctrl Pts',(-1.43925448419918E-16,-1.17524047358083,
-6.2));
#362334=CARTESIAN_POINT('Ctrl Pts',(0.678525403784434,-1.17524047358083,
-6.15833333333333));
#362335=CARTESIAN_POINT('Ctrl Pts',(1.01778810567665,-0.587620236790414,
-6.11666666666667));
#362336=CARTESIAN_POINT('Ctrl Pts',(1.35705080756887,7.46191194922343E-16,
-6.075));
#362337=CARTESIAN_POINT('Ctrl Pts',(1.01778810567665,0.587620236790414,
-6.03333333333333));
#362338=CARTESIAN_POINT('Ctrl Pts',(0.678525403784435,1.17524047358083,
-5.99166666666667));
#362339=CARTESIAN_POINT('Ctrl Pts',(0.,1.17524047358083,-5.95));
#362340=CARTESIAN_POINT('Ctrl Pts',(-0.678525403784434,1.17524047358083,
-5.90833333333333));
#362341=CARTESIAN_POINT('Ctrl Pts',(-1.01778810567665,0.587620236790415,
-5.86666666666667));
#362342=CARTESIAN_POINT('Ctrl Pts',(-1.35705080756887,9.69298860729681E-16,
-5.825));
#362343=CARTESIAN_POINT('Ctrl Pts',(-1.01778810567665,-0.587620236790413,
-5.78333333333333));
#362344=CARTESIAN_POINT('Ctrl Pts',(-0.678525403784435,-1.17524047358083,
-5.74166666666667));
#362345=CARTESIAN_POINT('Ctrl Pts',(-1.43925448419918E-16,-1.17524047358083,
-5.7));
#362346=CARTESIAN_POINT('Ctrl Pts',(0.678525403784434,-1.17524047358083,
-5.65833333333333));
#362347=CARTESIAN_POINT('Ctrl Pts',(1.01778810567665,-0.587620236790414,
-5.61666666666667));
#362348=CARTESIAN_POINT('Ctrl Pts',(1.35705080756887,5.27643355429203E-16,
-5.575));
#362349=CARTESIAN_POINT('Ctrl Pts',(1.01778810567665,0.587620236790414,
-5.53333333333334));
#362350=CARTESIAN_POINT('Ctrl Pts',(0.678525403784435,1.17524047358083,
-5.49166666666667));
#362351=CARTESIAN_POINT('Ctrl Pts',(0.,1.17524047358083,-5.45));
#362352=CARTESIAN_POINT('Ctrl Pts',(-0.678525403784434,1.17524047358083,
-5.40833333333333));
#362353=CARTESIAN_POINT('Ctrl Pts',(-1.01778810567665,0.587620236790415,
-5.36666666666667));
#362354=CARTESIAN_POINT('Ctrl Pts',(-1.35705080756887,7.50751021236542E-16,
-5.325));
#362355=CARTESIAN_POINT('Ctrl Pts',(-1.01778810567665,-0.587620236790413,
-5.28333333333333));
#362356=CARTESIAN_POINT('Ctrl Pts',(-0.678525403784435,-1.17524047358083,
-5.24166666666667));
#362357=CARTESIAN_POINT('Ctrl Pts',(-1.43925448419918E-16,-1.17524047358083,
-5.2));
#362358=CARTESIAN_POINT('Ctrl Pts',(0.678525403784434,-1.17524047358083,
-5.15833333333333));
#362359=CARTESIAN_POINT('Ctrl Pts',(1.01778810567665,-0.587620236790414,
-5.11666666666667));
#362360=CARTESIAN_POINT('Ctrl Pts',(1.35705080756887,3.09095515936061E-16,
-5.075));
#362361=CARTESIAN_POINT('Ctrl Pts',(1.01778810567665,0.587620236790414,
-5.03333333333333));
#362362=CARTESIAN_POINT('Ctrl Pts',(0.678525403784435,1.17524047358083,
-4.99166666666667));
#362363=CARTESIAN_POINT('Ctrl Pts',(0.,1.17524047358083,-4.95));
#362364=CARTESIAN_POINT('Ctrl Pts',(-0.678525403784434,1.17524047358083,
-4.90833333333333));
#362365=CARTESIAN_POINT('Ctrl Pts',(-1.01778810567665,0.587620236790415,
-4.86666666666667));
#362366=CARTESIAN_POINT('Ctrl Pts',(-1.35705080756887,5.322031817434E-16,
-4.825));
#362367=CARTESIAN_POINT('Ctrl Pts',(-1.01778810567665,-0.587620236790414,
-4.78333333333333));
#362368=CARTESIAN_POINT('Ctrl Pts',(-0.678525403784435,-1.17524047358083,
-4.74166666666667));
#362369=CARTESIAN_POINT('Ctrl Pts',(-1.43925448419918E-16,-1.17524047358083,
-4.7));
#362370=CARTESIAN_POINT('Ctrl Pts',(0.678525403784434,-1.17524047358083,
-4.65833333333333));
#362371=CARTESIAN_POINT('Ctrl Pts',(1.01778810567665,-0.587620236790414,
-4.61666666666667));
#362372=CARTESIAN_POINT('Ctrl Pts',(1.35705080756887,9.05476764429197E-17,
-4.575));
#362373=CARTESIAN_POINT('Ctrl Pts',(1.01778810567665,0.587620236790414,
-4.53333333333333));
#362374=CARTESIAN_POINT('Ctrl Pts',(0.678525403784435,1.17524047358083,
-4.49166666666667));
#362375=CARTESIAN_POINT('Ctrl Pts',(0.,1.17524047358083,-4.45));
#362376=CARTESIAN_POINT('Ctrl Pts',(-0.678525403784434,1.17524047358083,
-4.40833333333334));
#362377=CARTESIAN_POINT('Ctrl Pts',(-1.01778810567665,0.587620236790414,
-4.36666666666667));
#362378=CARTESIAN_POINT('Ctrl Pts',(-1.35705080756887,3.13655342250259E-16,
-4.325));
#362379=CARTESIAN_POINT('Ctrl Pts',(-1.01778810567665,-0.587620236790414,
-4.28333333333333));
#362380=CARTESIAN_POINT('Ctrl Pts',(-0.678525403784435,-1.17524047358083,
-4.24166666666667));
#362381=CARTESIAN_POINT('Ctrl Pts',(-1.43925448419918E-16,-1.17524047358083,
-4.2));
#362382=CARTESIAN_POINT('Ctrl Pts',(0.678525403784434,-1.17524047358083,
-4.15833333333334));
#362383=CARTESIAN_POINT('Ctrl Pts',(1.01778810567665,-0.587620236790415,
-4.11666666666667));
#362384=CARTESIAN_POINT('Ctrl Pts',(1.35705080756887,-1.28000163050222E-16,
-4.075));
#362385=CARTESIAN_POINT('Ctrl Pts',(1.01778810567665,0.587620236790413,
-4.03333333333333));
#362386=CARTESIAN_POINT('Ctrl Pts',(0.678525403784435,1.17524047358083,
-3.99166666666667));
#362387=CARTESIAN_POINT('Ctrl Pts',(0.,1.17524047358083,-3.95));
#362388=CARTESIAN_POINT('Ctrl Pts',(-0.678525403784434,1.17524047358083,
-3.90833333333334));
#362389=CARTESIAN_POINT('Ctrl Pts',(-1.01778810567665,0.587620236790414,
-3.86666666666667));
#362390=CARTESIAN_POINT('Ctrl Pts',(-1.35705080756887,9.5107502757118E-17,
-3.825));
#362391=CARTESIAN_POINT('Ctrl Pts',(-1.01778810567665,-0.587620236790414,
-3.78333333333333));
#362392=CARTESIAN_POINT('Ctrl Pts',(-0.678525403784435,-1.17524047358083,
-3.74166666666667));
#362393=CARTESIAN_POINT('Ctrl Pts',(-1.43925448419918E-16,-1.17524047358083,
-3.7));
#362394=CARTESIAN_POINT('Ctrl Pts',(0.678525403784434,-1.17524047358083,
-3.65833333333333));
#362395=CARTESIAN_POINT('Ctrl Pts',(1.01778810567665,-0.587620236790415,
-3.61666666666667));
#362396=CARTESIAN_POINT('Ctrl Pts',(1.35705080756887,-3.46548002543362E-16,
-3.575));
#362397=CARTESIAN_POINT('Ctrl Pts',(1.01778810567665,0.587620236790413,
-3.53333333333333));
#362398=CARTESIAN_POINT('Ctrl Pts',(0.678525403784435,1.17524047358083,
-3.49166666666667));
#362399=CARTESIAN_POINT('Ctrl Pts',(0.,1.17524047358083,-3.45));
#362400=CARTESIAN_POINT('Ctrl Pts',(-0.678525403784434,1.17524047358083,
-3.40833333333333));
#362401=CARTESIAN_POINT('Ctrl Pts',(-1.01778810567665,0.587620236790414,
-3.36666666666667));
#362402=CARTESIAN_POINT('Ctrl Pts',(-1.35705080756887,-1.23440336736023E-16,
-3.325));
#362403=CARTESIAN_POINT('Ctrl Pts',(-1.01778810567665,-0.587620236790414,
-3.28333333333333));
#362404=CARTESIAN_POINT('Ctrl Pts',(-0.678525403784435,-1.17524047358083,
-3.24166666666667));
#362405=CARTESIAN_POINT('Ctrl Pts',(-1.43925448419918E-16,-1.17524047358083,
-3.2));
#362406=CARTESIAN_POINT('Ctrl Pts',(0.678525403784434,-1.17524047358083,
-3.15833333333333));
#362407=CARTESIAN_POINT('Ctrl Pts',(1.01778810567665,-0.587620236790415,
-3.11666666666667));
#362408=CARTESIAN_POINT('Ctrl Pts',(1.35705080756887,-5.65095842036504E-16,
-3.075));
#362409=CARTESIAN_POINT('Ctrl Pts',(1.01778810567665,0.587620236790413,
-3.03333333333333));
#362410=CARTESIAN_POINT('Ctrl Pts',(0.678525403784435,1.17524047358083,
-2.99166666666667));
#362411=CARTESIAN_POINT('Ctrl Pts',(0.,1.17524047358083,-2.95));
#362412=CARTESIAN_POINT('Ctrl Pts',(-0.678525403784434,1.17524047358083,
-2.90833333333333));
#362413=CARTESIAN_POINT('Ctrl Pts',(-1.01778810567665,0.587620236790414,
-2.86666666666667));
#362414=CARTESIAN_POINT('Ctrl Pts',(-1.35705080756887,-3.41988176229165E-16,
-2.825));
#362415=CARTESIAN_POINT('Ctrl Pts',(-1.01778810567665,-0.587620236790414,
-2.78333333333333));
#362416=CARTESIAN_POINT('Ctrl Pts',(-0.678525403784435,-1.17524047358083,
-2.74166666666667));
#362417=CARTESIAN_POINT('Ctrl Pts',(-1.43925448419918E-16,-1.17524047358083,
-2.7));
#362418=CARTESIAN_POINT('Ctrl Pts',(0.678525403784434,-1.17524047358083,
-2.65833333333333));
#362419=CARTESIAN_POINT('Ctrl Pts',(1.01778810567665,-0.587620236790415,
-2.61666666666667));
#362420=CARTESIAN_POINT('Ctrl Pts',(1.35705080756887,-7.83643681529645E-16,
-2.575));
#362421=CARTESIAN_POINT('Ctrl Pts',(1.01778810567665,0.587620236790413,
-2.53333333333334));
#362422=CARTESIAN_POINT('Ctrl Pts',(0.678525403784435,1.17524047358083,
-2.49166666666667));
#362423=CARTESIAN_POINT('Ctrl Pts',(0.,1.17524047358083,-2.45));
#362424=CARTESIAN_POINT('Ctrl Pts',(-0.678525403784434,1.17524047358083,
-2.40833333333334));
#362425=CARTESIAN_POINT('Ctrl Pts',(-1.01778810567665,0.587620236790414,
-2.36666666666667));
#362426=CARTESIAN_POINT('Ctrl Pts',(-1.35705080756887,-5.60536015722306E-16,
-2.325));
#362427=CARTESIAN_POINT('Ctrl Pts',(-1.01778810567665,-0.587620236790415,
-2.28333333333333));
#362428=CARTESIAN_POINT('Ctrl Pts',(-0.678525403784435,-1.17524047358083,
-2.24166666666667));
#362429=CARTESIAN_POINT('Ctrl Pts',(-1.43925448419918E-16,-1.17524047358083,
-2.2));
#362430=CARTESIAN_POINT('Ctrl Pts',(0.678525403784434,-1.17524047358083,
-2.15833333333333));
#362431=CARTESIAN_POINT('Ctrl Pts',(1.01778810567665,-0.587620236790415,
-2.11666666666667));
#362432=CARTESIAN_POINT('Ctrl Pts',(1.35705080756887,-1.00219152102279E-15,
-2.075));
#362433=CARTESIAN_POINT('Ctrl Pts',(1.01778810567665,0.587620236790412,
-2.03333333333333));
#362434=CARTESIAN_POINT('Ctrl Pts',(0.678525403784435,1.17524047358083,
-1.99166666666667));
#362435=CARTESIAN_POINT('Ctrl Pts',(0.,1.17524047358083,-1.95));
#362436=CARTESIAN_POINT('Ctrl Pts',(-0.678525403784434,1.17524047358083,
-1.90833333333333));
#362437=CARTESIAN_POINT('Ctrl Pts',(-1.01778810567665,0.587620236790413,
-1.86666666666667));
#362438=CARTESIAN_POINT('Ctrl Pts',(-1.35705080756887,-7.79083855215448E-16,
-1.825));
#362439=CARTESIAN_POINT('Ctrl Pts',(-1.01778810567665,-0.587620236790415,
-1.78333333333333));
#362440=CARTESIAN_POINT('Ctrl Pts',(-0.678525403784435,-1.17524047358083,
-1.74166666666667));
#362441=CARTESIAN_POINT('Ctrl Pts',(-1.43925448419918E-16,-1.17524047358083,
-1.7));
#362442=CARTESIAN_POINT('Ctrl Pts',(0.678525403784434,-1.17524047358083,
-1.65833333333333));
#362443=CARTESIAN_POINT('Ctrl Pts',(1.01778810567665,-0.587620236790416,
-1.61666666666667));
#362444=CARTESIAN_POINT('Ctrl Pts',(1.35705080756887,-1.22073936051593E-15,
-1.575));
#362445=CARTESIAN_POINT('Ctrl Pts',(1.01778810567665,0.587620236790412,
-1.53333333333333));
#362446=CARTESIAN_POINT('Ctrl Pts',(0.678525403784435,1.17524047358083,
-1.49166666666667));
#362447=CARTESIAN_POINT('Ctrl Pts',(0.,1.17524047358083,-1.45));
#362448=CARTESIAN_POINT('Ctrl Pts',(0.,1.5,-18.1375));
#362449=CARTESIAN_POINT('Ctrl Pts',(-0.866025403784436,1.5,-18.0958333333333));
#362450=CARTESIAN_POINT('Ctrl Pts',(-1.29903810567665,0.750000000000004,
-18.0541666666667));
#362451=CARTESIAN_POINT('Ctrl Pts',(-1.73205080756887,6.31936457585901E-15,
-18.0125));
#362452=CARTESIAN_POINT('Ctrl Pts',(-1.29903810567665,-0.749999999999991,
-17.9708333333333));
#362453=CARTESIAN_POINT('Ctrl Pts',(-0.866025403784437,-1.49999999999999,
-17.9291666666667));
#362454=CARTESIAN_POINT('Ctrl Pts',(-1.83697019872102E-16,-1.49999999999999,
-17.8875));
#362455=CARTESIAN_POINT('Ctrl Pts',(0.866025403784436,-1.49999999999999,
-17.8458333333333));
#362456=CARTESIAN_POINT('Ctrl Pts',(1.29903810567665,-0.749999999999992,
-17.8041666666667));
#362457=CARTESIAN_POINT('Ctrl Pts',(1.73205080756887,5.78586056062248E-15,
-17.7625));
#362458=CARTESIAN_POINT('Ctrl Pts',(1.29903810567665,0.750000000000003,
-17.7208333333333));
#362459=CARTESIAN_POINT('Ctrl Pts',(0.866025403784437,1.5,-17.6791666666667));
#362460=CARTESIAN_POINT('Ctrl Pts',(0.,1.5,-17.6375));
#362461=CARTESIAN_POINT('Ctrl Pts',(-0.866025403784436,1.5,-17.5958333333333));
#362462=CARTESIAN_POINT('Ctrl Pts',(-1.29903810567665,0.750000000000004,
-17.5541666666667));
#362463=CARTESIAN_POINT('Ctrl Pts',(-1.73205080756887,6.10081673636587E-15,
-17.5125));
#362464=CARTESIAN_POINT('Ctrl Pts',(-1.29903810567665,-0.749999999999992,
-17.4708333333333));
#362465=CARTESIAN_POINT('Ctrl Pts',(-0.866025403784437,-1.49999999999999,
-17.4291666666667));
#362466=CARTESIAN_POINT('Ctrl Pts',(-1.83697019872102E-16,-1.49999999999999,
-17.3875));
#362467=CARTESIAN_POINT('Ctrl Pts',(0.866025403784436,-1.49999999999999,
-17.3458333333333));
#362468=CARTESIAN_POINT('Ctrl Pts',(1.29903810567665,-0.749999999999992,
-17.3041666666667));
#362469=CARTESIAN_POINT('Ctrl Pts',(1.73205080756887,5.56731272112934E-15,
-17.2625));
#362470=CARTESIAN_POINT('Ctrl Pts',(1.29903810567665,0.750000000000003,
-17.2208333333333));
#362471=CARTESIAN_POINT('Ctrl Pts',(0.866025403784437,1.5,-17.1791666666667));
#362472=CARTESIAN_POINT('Ctrl Pts',(0.,1.5,-17.1375));
#362473=CARTESIAN_POINT('Ctrl Pts',(-0.866025403784436,1.5,-17.0958333333333));
#362474=CARTESIAN_POINT('Ctrl Pts',(-1.29903810567665,0.750000000000004,
-17.0541666666667));
#362475=CARTESIAN_POINT('Ctrl Pts',(-1.73205080756887,5.88226889687273E-15,
-17.0125));
#362476=CARTESIAN_POINT('Ctrl Pts',(-1.29903810567665,-0.749999999999992,
-16.9708333333333));
#362477=CARTESIAN_POINT('Ctrl Pts',(-0.866025403784437,-1.49999999999999,
-16.9291666666667));
#362478=CARTESIAN_POINT('Ctrl Pts',(-1.83697019872102E-16,-1.49999999999999,
-16.8875));
#362479=CARTESIAN_POINT('Ctrl Pts',(0.866025403784436,-1.49999999999999,
-16.8458333333333));
#362480=CARTESIAN_POINT('Ctrl Pts',(1.29903810567665,-0.749999999999993,
-16.8041666666667));
#362481=CARTESIAN_POINT('Ctrl Pts',(1.73205080756887,5.3487648816362E-15,
-16.7625));
#362482=CARTESIAN_POINT('Ctrl Pts',(1.29903810567665,0.750000000000002,
-16.7208333333333));
#362483=CARTESIAN_POINT('Ctrl Pts',(0.866025403784437,1.5,-16.6791666666667));
#362484=CARTESIAN_POINT('Ctrl Pts',(0.,1.5,-16.6375));
#362485=CARTESIAN_POINT('Ctrl Pts',(-0.866025403784436,1.5,-16.5958333333333));
#362486=CARTESIAN_POINT('Ctrl Pts',(-1.29903810567665,0.750000000000004,
-16.5541666666667));
#362487=CARTESIAN_POINT('Ctrl Pts',(-1.73205080756887,5.66372105737959E-15,
-16.5125));
#362488=CARTESIAN_POINT('Ctrl Pts',(-1.29903810567665,-0.749999999999992,
-16.4708333333333));
#362489=CARTESIAN_POINT('Ctrl Pts',(-0.866025403784437,-1.49999999999999,
-16.4291666666667));
#362490=CARTESIAN_POINT('Ctrl Pts',(-1.83697019872102E-16,-1.49999999999999,
-16.3875));
#362491=CARTESIAN_POINT('Ctrl Pts',(0.866025403784436,-1.49999999999999,
-16.3458333333333));
#362492=CARTESIAN_POINT('Ctrl Pts',(1.29903810567665,-0.749999999999993,
-16.3041666666667));
#362493=CARTESIAN_POINT('Ctrl Pts',(1.73205080756887,5.13021704214306E-15,
-16.2625));
#362494=CARTESIAN_POINT('Ctrl Pts',(1.29903810567665,0.750000000000002,
-16.2208333333333));
#362495=CARTESIAN_POINT('Ctrl Pts',(0.866025403784437,1.5,-16.1791666666667));
#362496=CARTESIAN_POINT('Ctrl Pts',(0.,1.5,-16.1375));
#362497=CARTESIAN_POINT('Ctrl Pts',(-0.866025403784436,1.5,-16.0958333333333));
#362498=CARTESIAN_POINT('Ctrl Pts',(-1.29903810567665,0.750000000000003,
-16.0541666666667));
#362499=CARTESIAN_POINT('Ctrl Pts',(-1.73205080756887,5.44517321788645E-15,
-16.0125));
#362500=CARTESIAN_POINT('Ctrl Pts',(-1.29903810567665,-0.749999999999992,
-15.9708333333333));
#362501=CARTESIAN_POINT('Ctrl Pts',(-0.866025403784437,-1.49999999999999,
-15.9291666666667));
#362502=CARTESIAN_POINT('Ctrl Pts',(-1.83697019872102E-16,-1.49999999999999,
-15.8875));
#362503=CARTESIAN_POINT('Ctrl Pts',(0.866025403784436,-1.49999999999999,
-15.8458333333333));
#362504=CARTESIAN_POINT('Ctrl Pts',(1.29903810567665,-0.749999999999993,
-15.8041666666667));
#362505=CARTESIAN_POINT('Ctrl Pts',(1.73205080756887,4.91166920264992E-15,
-15.7625));
#362506=CARTESIAN_POINT('Ctrl Pts',(1.29903810567665,0.750000000000002,
-15.7208333333333));
#362507=CARTESIAN_POINT('Ctrl Pts',(0.866025403784437,1.5,-15.6791666666667));
#362508=CARTESIAN_POINT('Ctrl Pts',(0.,1.5,-15.6375));
#362509=CARTESIAN_POINT('Ctrl Pts',(-0.866025403784436,1.5,-15.5958333333333));
#362510=CARTESIAN_POINT('Ctrl Pts',(-1.29903810567665,0.750000000000003,
-15.5541666666667));
#362511=CARTESIAN_POINT('Ctrl Pts',(-1.73205080756887,5.22662537839331E-15,
-15.5125));
#362512=CARTESIAN_POINT('Ctrl Pts',(-1.29903810567665,-0.749999999999992,
-15.4708333333333));
#362513=CARTESIAN_POINT('Ctrl Pts',(-0.866025403784437,-1.49999999999999,
-15.4291666666667));
#362514=CARTESIAN_POINT('Ctrl Pts',(-1.83697019872102E-16,-1.49999999999999,
-15.3875));
#362515=CARTESIAN_POINT('Ctrl Pts',(0.866025403784436,-1.49999999999999,
-15.3458333333333));
#362516=CARTESIAN_POINT('Ctrl Pts',(1.29903810567665,-0.749999999999993,
-15.3041666666667));
#362517=CARTESIAN_POINT('Ctrl Pts',(1.73205080756887,4.69312136315677E-15,
-15.2625));
#362518=CARTESIAN_POINT('Ctrl Pts',(1.29903810567665,0.750000000000002,
-15.2208333333333));
#362519=CARTESIAN_POINT('Ctrl Pts',(0.866025403784437,1.5,-15.1791666666667));
#362520=CARTESIAN_POINT('Ctrl Pts',(0.,1.5,-15.1375));
#362521=CARTESIAN_POINT('Ctrl Pts',(-0.866025403784436,1.5,-15.0958333333333));
#362522=CARTESIAN_POINT('Ctrl Pts',(-1.29903810567665,0.750000000000003,
-15.0541666666667));
#362523=CARTESIAN_POINT('Ctrl Pts',(-1.73205080756887,5.00807753890017E-15,
-15.0125));
#362524=CARTESIAN_POINT('Ctrl Pts',(-1.29903810567665,-0.749999999999993,
-14.9708333333333));
#362525=CARTESIAN_POINT('Ctrl Pts',(-0.866025403784437,-1.49999999999999,
-14.9291666666667));
#362526=CARTESIAN_POINT('Ctrl Pts',(-1.83697019872102E-16,-1.49999999999999,
-14.8875));
#362527=CARTESIAN_POINT('Ctrl Pts',(0.866025403784436,-1.49999999999999,
-14.8458333333333));
#362528=CARTESIAN_POINT('Ctrl Pts',(1.29903810567665,-0.749999999999994,
-14.8041666666667));
#362529=CARTESIAN_POINT('Ctrl Pts',(1.73205080756887,4.47457352366363E-15,
-14.7625));
#362530=CARTESIAN_POINT('Ctrl Pts',(1.29903810567665,0.750000000000002,
-14.7208333333333));
#362531=CARTESIAN_POINT('Ctrl Pts',(0.866025403784437,1.5,-14.6791666666667));
#362532=CARTESIAN_POINT('Ctrl Pts',(0.,1.5,-14.6375));
#362533=CARTESIAN_POINT('Ctrl Pts',(-0.866025403784436,1.5,-14.5958333333333));
#362534=CARTESIAN_POINT('Ctrl Pts',(-1.29903810567665,0.750000000000003,
-14.5541666666667));
#362535=CARTESIAN_POINT('Ctrl Pts',(-1.73205080756887,4.78952969940702E-15,
-14.5125));
#362536=CARTESIAN_POINT('Ctrl Pts',(-1.29903810567665,-0.749999999999993,
-14.4708333333333));
#362537=CARTESIAN_POINT('Ctrl Pts',(-0.866025403784437,-1.49999999999999,
-14.4291666666667));
#362538=CARTESIAN_POINT('Ctrl Pts',(-1.83697019872102E-16,-1.49999999999999,
-14.3875));
#362539=CARTESIAN_POINT('Ctrl Pts',(0.866025403784436,-1.49999999999999,
-14.3458333333333));
#362540=CARTESIAN_POINT('Ctrl Pts',(1.29903810567665,-0.749999999999994,
-14.3041666666667));
#362541=CARTESIAN_POINT('Ctrl Pts',(1.73205080756887,4.25602568417049E-15,
-14.2625));
#362542=CARTESIAN_POINT('Ctrl Pts',(1.29903810567665,0.750000000000001,
-14.2208333333333));
#362543=CARTESIAN_POINT('Ctrl Pts',(0.866025403784437,1.5,-14.1791666666667));
#362544=CARTESIAN_POINT('Ctrl Pts',(0.,1.5,-14.1375));
#362545=CARTESIAN_POINT('Ctrl Pts',(-0.866025403784436,1.5,-14.0958333333333));
#362546=CARTESIAN_POINT('Ctrl Pts',(-1.29903810567665,0.750000000000003,
-14.0541666666667));
#362547=CARTESIAN_POINT('Ctrl Pts',(-1.73205080756887,4.57098185991388E-15,
-14.0125));
#362548=CARTESIAN_POINT('Ctrl Pts',(-1.29903810567665,-0.749999999999993,
-13.9708333333333));
#362549=CARTESIAN_POINT('Ctrl Pts',(-0.866025403784437,-1.49999999999999,
-13.9291666666667));
#362550=CARTESIAN_POINT('Ctrl Pts',(-1.83697019872102E-16,-1.49999999999999,
-13.8875));
#362551=CARTESIAN_POINT('Ctrl Pts',(0.866025403784436,-1.49999999999999,
-13.8458333333333));
#362552=CARTESIAN_POINT('Ctrl Pts',(1.29903810567665,-0.749999999999994,
-13.8041666666667));
#362553=CARTESIAN_POINT('Ctrl Pts',(1.73205080756887,4.03747784467735E-15,
-13.7625));
#362554=CARTESIAN_POINT('Ctrl Pts',(1.29903810567665,0.750000000000001,
-13.7208333333333));
#362555=CARTESIAN_POINT('Ctrl Pts',(0.866025403784437,1.5,-13.6791666666667));
#362556=CARTESIAN_POINT('Ctrl Pts',(0.,1.5,-13.6375));
#362557=CARTESIAN_POINT('Ctrl Pts',(-0.866025403784436,1.5,-13.5958333333333));
#362558=CARTESIAN_POINT('Ctrl Pts',(-1.29903810567665,0.750000000000002,
-13.5541666666667));
#362559=CARTESIAN_POINT('Ctrl Pts',(-1.73205080756887,4.35243402042074E-15,
-13.5125));
#362560=CARTESIAN_POINT('Ctrl Pts',(-1.29903810567665,-0.749999999999993,
-13.4708333333333));
#362561=CARTESIAN_POINT('Ctrl Pts',(-0.866025403784437,-1.49999999999999,
-13.4291666666667));
#362562=CARTESIAN_POINT('Ctrl Pts',(-1.83697019872102E-16,-1.49999999999999,
-13.3875));
#362563=CARTESIAN_POINT('Ctrl Pts',(0.866025403784436,-1.49999999999999,
-13.3458333333333));
#362564=CARTESIAN_POINT('Ctrl Pts',(1.29903810567665,-0.749999999999994,
-13.3041666666667));
#362565=CARTESIAN_POINT('Ctrl Pts',(1.73205080756887,3.81893000518421E-15,
-13.2625));
#362566=CARTESIAN_POINT('Ctrl Pts',(1.29903810567665,0.750000000000001,
-13.2208333333333));
#362567=CARTESIAN_POINT('Ctrl Pts',(0.866025403784437,1.5,-13.1791666666667));
#362568=CARTESIAN_POINT('Ctrl Pts',(0.,1.5,-13.1375));
#362569=CARTESIAN_POINT('Ctrl Pts',(-0.866025403784436,1.5,-13.0958333333333));
#362570=CARTESIAN_POINT('Ctrl Pts',(-1.29903810567665,0.750000000000002,
-13.0541666666667));
#362571=CARTESIAN_POINT('Ctrl Pts',(-1.73205080756887,4.1338861809276E-15,
-13.0125));
#362572=CARTESIAN_POINT('Ctrl Pts',(-1.29903810567665,-0.749999999999993,
-12.9708333333333));
#362573=CARTESIAN_POINT('Ctrl Pts',(-0.866025403784437,-1.49999999999999,
-12.9291666666667));
#362574=CARTESIAN_POINT('Ctrl Pts',(-1.83697019872102E-16,-1.49999999999999,
-12.8875));
#362575=CARTESIAN_POINT('Ctrl Pts',(0.866025403784436,-1.49999999999999,
-12.8458333333333));
#362576=CARTESIAN_POINT('Ctrl Pts',(1.29903810567665,-0.749999999999994,
-12.8041666666667));
#362577=CARTESIAN_POINT('Ctrl Pts',(1.73205080756887,3.60038216569107E-15,
-12.7625));
#362578=CARTESIAN_POINT('Ctrl Pts',(1.29903810567665,0.750000000000001,
-12.7208333333333));
#362579=CARTESIAN_POINT('Ctrl Pts',(0.866025403784437,1.5,-12.6791666666667));
#362580=CARTESIAN_POINT('Ctrl Pts',(0.,1.5,-12.6375));
#362581=CARTESIAN_POINT('Ctrl Pts',(-0.866025403784436,1.5,-12.5958333333333));
#362582=CARTESIAN_POINT('Ctrl Pts',(-1.29903810567665,0.750000000000002,
-12.5541666666667));
#362583=CARTESIAN_POINT('Ctrl Pts',(-1.73205080756887,3.91533834143446E-15,
-12.5125));
#362584=CARTESIAN_POINT('Ctrl Pts',(-1.29903810567665,-0.749999999999994,
-12.4708333333333));
#362585=CARTESIAN_POINT('Ctrl Pts',(-0.866025403784437,-1.49999999999999,
-12.4291666666667));
#362586=CARTESIAN_POINT('Ctrl Pts',(-1.83697019872102E-16,-1.49999999999999,
-12.3875));
#362587=CARTESIAN_POINT('Ctrl Pts',(0.866025403784436,-1.49999999999999,
-12.3458333333333));
#362588=CARTESIAN_POINT('Ctrl Pts',(1.29903810567665,-0.749999999999995,
-12.3041666666667));
#362589=CARTESIAN_POINT('Ctrl Pts',(1.73205080756887,3.38183432619793E-15,
-12.2625));
#362590=CARTESIAN_POINT('Ctrl Pts',(1.29903810567665,0.75,-12.2208333333333));
#362591=CARTESIAN_POINT('Ctrl Pts',(0.866025403784437,1.5,-12.1791666666667));
#362592=CARTESIAN_POINT('Ctrl Pts',(0.,1.5,-12.1375));
#362593=CARTESIAN_POINT('Ctrl Pts',(-0.866025403784436,1.5,-12.0958333333333));
#362594=CARTESIAN_POINT('Ctrl Pts',(-1.29903810567665,0.750000000000002,
-12.0541666666667));
#362595=CARTESIAN_POINT('Ctrl Pts',(-1.73205080756887,3.69679050194132E-15,
-12.0125));
#362596=CARTESIAN_POINT('Ctrl Pts',(-1.29903810567665,-0.749999999999994,
-11.9708333333333));
#362597=CARTESIAN_POINT('Ctrl Pts',(-0.866025403784437,-1.49999999999999,
-11.9291666666667));
#362598=CARTESIAN_POINT('Ctrl Pts',(-1.83697019872102E-16,-1.49999999999999,
-11.8875));
#362599=CARTESIAN_POINT('Ctrl Pts',(0.866025403784436,-1.49999999999999,
-11.8458333333333));
#362600=CARTESIAN_POINT('Ctrl Pts',(1.29903810567665,-0.749999999999995,
-11.8041666666667));
#362601=CARTESIAN_POINT('Ctrl Pts',(1.73205080756887,3.16328648670478E-15,
-11.7625));
#362602=CARTESIAN_POINT('Ctrl Pts',(1.29903810567665,0.75,-11.7208333333333));
#362603=CARTESIAN_POINT('Ctrl Pts',(0.866025403784437,1.5,-11.6791666666667));
#362604=CARTESIAN_POINT('Ctrl Pts',(0.,1.5,-11.6375));
#362605=CARTESIAN_POINT('Ctrl Pts',(-0.866025403784436,1.5,-11.5958333333333));
#362606=CARTESIAN_POINT('Ctrl Pts',(-1.29903810567665,0.750000000000001,
-11.5541666666667));
#362607=CARTESIAN_POINT('Ctrl Pts',(-1.73205080756887,3.47824266244818E-15,
-11.5125));
#362608=CARTESIAN_POINT('Ctrl Pts',(-1.29903810567665,-0.749999999999994,
-11.4708333333333));
#362609=CARTESIAN_POINT('Ctrl Pts',(-0.866025403784437,-1.49999999999999,
-11.4291666666667));
#362610=CARTESIAN_POINT('Ctrl Pts',(-1.83697019872102E-16,-1.49999999999999,
-11.3875));
#362611=CARTESIAN_POINT('Ctrl Pts',(0.866025403784436,-1.49999999999999,
-11.3458333333333));
#362612=CARTESIAN_POINT('Ctrl Pts',(1.29903810567665,-0.749999999999995,
-11.3041666666667));
#362613=CARTESIAN_POINT('Ctrl Pts',(1.73205080756887,2.94473864721164E-15,
-11.2625));
#362614=CARTESIAN_POINT('Ctrl Pts',(1.29903810567665,0.75,-11.2208333333333));
#362615=CARTESIAN_POINT('Ctrl Pts',(0.866025403784437,1.5,-11.1791666666667));
#362616=CARTESIAN_POINT('Ctrl Pts',(0.,1.5,-11.1375));
#362617=CARTESIAN_POINT('Ctrl Pts',(-0.866025403784436,1.5,-11.0958333333333));
#362618=CARTESIAN_POINT('Ctrl Pts',(-1.29903810567665,0.750000000000001,
-11.0541666666667));
#362619=CARTESIAN_POINT('Ctrl Pts',(-1.73205080756887,3.25969482295504E-15,
-11.0125));
#362620=CARTESIAN_POINT('Ctrl Pts',(-1.29903810567665,-0.749999999999994,
-10.9708333333333));
#362621=CARTESIAN_POINT('Ctrl Pts',(-0.866025403784437,-1.49999999999999,
-10.9291666666667));
#362622=CARTESIAN_POINT('Ctrl Pts',(-1.83697019872102E-16,-1.49999999999999,
-10.8875));
#362623=CARTESIAN_POINT('Ctrl Pts',(0.866025403784436,-1.49999999999999,
-10.8458333333333));
#362624=CARTESIAN_POINT('Ctrl Pts',(1.29903810567665,-0.749999999999995,
-10.8041666666667));
#362625=CARTESIAN_POINT('Ctrl Pts',(1.73205080756887,2.7261908077185E-15,
-10.7625));
#362626=CARTESIAN_POINT('Ctrl Pts',(1.29903810567665,0.75,-10.7208333333333));
#362627=CARTESIAN_POINT('Ctrl Pts',(0.866025403784437,1.5,-10.6791666666667));
#362628=CARTESIAN_POINT('Ctrl Pts',(0.,1.5,-10.6375));
#362629=CARTESIAN_POINT('Ctrl Pts',(-0.866025403784436,1.5,-10.5958333333333));
#362630=CARTESIAN_POINT('Ctrl Pts',(-1.29903810567665,0.750000000000001,
-10.5541666666667));
#362631=CARTESIAN_POINT('Ctrl Pts',(-1.73205080756887,3.04114698346189E-15,
-10.5125));
#362632=CARTESIAN_POINT('Ctrl Pts',(-1.29903810567665,-0.749999999999994,
-10.4708333333333));
#362633=CARTESIAN_POINT('Ctrl Pts',(-0.866025403784437,-1.49999999999999,
-10.4291666666667));
#362634=CARTESIAN_POINT('Ctrl Pts',(-1.83697019872102E-16,-1.49999999999999,
-10.3875));
#362635=CARTESIAN_POINT('Ctrl Pts',(0.866025403784436,-1.49999999999999,
-10.3458333333333));
#362636=CARTESIAN_POINT('Ctrl Pts',(1.29903810567665,-0.749999999999996,
-10.3041666666667));
#362637=CARTESIAN_POINT('Ctrl Pts',(1.73205080756887,2.50764296822536E-15,
-10.2625));
#362638=CARTESIAN_POINT('Ctrl Pts',(1.29903810567665,0.749999999999999,
-10.2208333333333));
#362639=CARTESIAN_POINT('Ctrl Pts',(0.866025403784437,1.5,-10.1791666666667));
#362640=CARTESIAN_POINT('Ctrl Pts',(0.,1.5,-10.1375));
#362641=CARTESIAN_POINT('Ctrl Pts',(-0.866025403784436,1.5,-10.0958333333333));
#362642=CARTESIAN_POINT('Ctrl Pts',(-1.29903810567665,0.750000000000001,
-10.0541666666667));
#362643=CARTESIAN_POINT('Ctrl Pts',(-1.73205080756887,2.82259914396875E-15,
-10.0125));
#362644=CARTESIAN_POINT('Ctrl Pts',(-1.29903810567665,-0.749999999999995,
-9.97083333333333));
#362645=CARTESIAN_POINT('Ctrl Pts',(-0.866025403784437,-1.49999999999999,
-9.92916666666667));
#362646=CARTESIAN_POINT('Ctrl Pts',(-1.83697019872102E-16,-1.49999999999999,
-9.8875));
#362647=CARTESIAN_POINT('Ctrl Pts',(0.866025403784436,-1.49999999999999,
-9.84583333333333));
#362648=CARTESIAN_POINT('Ctrl Pts',(1.29903810567665,-0.749999999999996,
-9.80416666666667));
#362649=CARTESIAN_POINT('Ctrl Pts',(1.73205080756887,2.28909512873222E-15,
-9.7625));
#362650=CARTESIAN_POINT('Ctrl Pts',(1.29903810567665,0.749999999999999,
-9.72083333333333));
#362651=CARTESIAN_POINT('Ctrl Pts',(0.866025403784437,1.5,-9.67916666666667));
#362652=CARTESIAN_POINT('Ctrl Pts',(0.,1.5,-9.6375));
#362653=CARTESIAN_POINT('Ctrl Pts',(-0.866025403784436,1.5,-9.59583333333333));
#362654=CARTESIAN_POINT('Ctrl Pts',(-1.29903810567665,0.750000000000001,
-9.55416666666667));
#362655=CARTESIAN_POINT('Ctrl Pts',(-1.73205080756887,2.60405130447561E-15,
-9.5125));
#362656=CARTESIAN_POINT('Ctrl Pts',(-1.29903810567665,-0.749999999999995,
-9.47083333333333));
#362657=CARTESIAN_POINT('Ctrl Pts',(-0.866025403784437,-1.49999999999999,
-9.42916666666667));
#362658=CARTESIAN_POINT('Ctrl Pts',(-1.83697019872102E-16,-1.49999999999999,
-9.3875));
#362659=CARTESIAN_POINT('Ctrl Pts',(0.866025403784436,-1.49999999999999,
-9.34583333333333));
#362660=CARTESIAN_POINT('Ctrl Pts',(1.29903810567665,-0.749999999999996,
-9.30416666666667));
#362661=CARTESIAN_POINT('Ctrl Pts',(1.73205080756887,2.07054728923908E-15,
-9.2625));
#362662=CARTESIAN_POINT('Ctrl Pts',(1.29903810567665,0.749999999999999,
-9.22083333333333));
#362663=CARTESIAN_POINT('Ctrl Pts',(0.866025403784437,1.5,-9.17916666666667));
#362664=CARTESIAN_POINT('Ctrl Pts',(0.,1.5,-9.1375));
#362665=CARTESIAN_POINT('Ctrl Pts',(-0.866025403784436,1.5,-9.09583333333333));
#362666=CARTESIAN_POINT('Ctrl Pts',(-1.29903810567665,0.75,-9.05416666666667));
#362667=CARTESIAN_POINT('Ctrl Pts',(-1.73205080756887,2.38550346498247E-15,
-9.0125));
#362668=CARTESIAN_POINT('Ctrl Pts',(-1.29903810567665,-0.749999999999995,
-8.97083333333333));
#362669=CARTESIAN_POINT('Ctrl Pts',(-0.866025403784437,-1.49999999999999,
-8.92916666666667));
#362670=CARTESIAN_POINT('Ctrl Pts',(-1.83697019872102E-16,-1.49999999999999,
-8.8875));
#362671=CARTESIAN_POINT('Ctrl Pts',(0.866025403784436,-1.49999999999999,
-8.84583333333333));
#362672=CARTESIAN_POINT('Ctrl Pts',(1.29903810567665,-0.749999999999996,
-8.80416666666667));
#362673=CARTESIAN_POINT('Ctrl Pts',(1.73205080756887,1.85199944974594E-15,
-8.7625));
#362674=CARTESIAN_POINT('Ctrl Pts',(1.29903810567665,0.749999999999999,
-8.72083333333333));
#362675=CARTESIAN_POINT('Ctrl Pts',(0.866025403784437,1.5,-8.67916666666667));
#362676=CARTESIAN_POINT('Ctrl Pts',(0.,1.5,-8.6375));
#362677=CARTESIAN_POINT('Ctrl Pts',(-0.866025403784436,1.5,-8.59583333333333));
#362678=CARTESIAN_POINT('Ctrl Pts',(-1.29903810567665,0.75,-8.55416666666667));
#362679=CARTESIAN_POINT('Ctrl Pts',(-1.73205080756887,2.16695562548933E-15,
-8.5125));
#362680=CARTESIAN_POINT('Ctrl Pts',(-1.29903810567665,-0.749999999999995,
-8.47083333333333));
#362681=CARTESIAN_POINT('Ctrl Pts',(-0.866025403784437,-1.49999999999999,
-8.42916666666667));
#362682=CARTESIAN_POINT('Ctrl Pts',(-1.83697019872102E-16,-1.49999999999999,
-8.3875));
#362683=CARTESIAN_POINT('Ctrl Pts',(0.866025403784436,-1.49999999999999,
-8.34583333333333));
#362684=CARTESIAN_POINT('Ctrl Pts',(1.29903810567665,-0.749999999999996,
-8.30416666666667));
#362685=CARTESIAN_POINT('Ctrl Pts',(1.73205080756887,1.6334516102528E-15,
-8.2625));
#362686=CARTESIAN_POINT('Ctrl Pts',(1.29903810567665,0.749999999999999,
-8.22083333333333));
#362687=CARTESIAN_POINT('Ctrl Pts',(0.866025403784437,1.5,-8.17916666666667));
#362688=CARTESIAN_POINT('Ctrl Pts',(0.,1.5,-8.1375));
#362689=CARTESIAN_POINT('Ctrl Pts',(-0.866025403784436,1.5,-8.09583333333333));
#362690=CARTESIAN_POINT('Ctrl Pts',(-1.29903810567665,0.75,-8.05416666666667));
#362691=CARTESIAN_POINT('Ctrl Pts',(-1.73205080756887,1.94840778599619E-15,
-8.0125));
#362692=CARTESIAN_POINT('Ctrl Pts',(-1.29903810567665,-0.749999999999996,
-7.97083333333334));
#362693=CARTESIAN_POINT('Ctrl Pts',(-0.866025403784437,-1.49999999999999,
-7.92916666666667));
#362694=CARTESIAN_POINT('Ctrl Pts',(-1.83697019872102E-16,-1.49999999999999,
-7.8875));
#362695=CARTESIAN_POINT('Ctrl Pts',(0.866025403784436,-1.49999999999999,
-7.84583333333333));
#362696=CARTESIAN_POINT('Ctrl Pts',(1.29903810567665,-0.749999999999997,
-7.80416666666667));
#362697=CARTESIAN_POINT('Ctrl Pts',(1.73205080756887,1.41490377075966E-15,
-7.7625));
#362698=CARTESIAN_POINT('Ctrl Pts',(1.29903810567665,0.749999999999998,
-7.72083333333334));
#362699=CARTESIAN_POINT('Ctrl Pts',(0.866025403784437,1.5,-7.67916666666667));
#362700=CARTESIAN_POINT('Ctrl Pts',(0.,1.5,-7.6375));
#362701=CARTESIAN_POINT('Ctrl Pts',(-0.866025403784436,1.5,-7.59583333333333));
#362702=CARTESIAN_POINT('Ctrl Pts',(-1.29903810567665,0.75,-7.55416666666667));
#362703=CARTESIAN_POINT('Ctrl Pts',(-1.73205080756887,1.72985994650305E-15,
-7.5125));
#362704=CARTESIAN_POINT('Ctrl Pts',(-1.29903810567665,-0.749999999999996,
-7.47083333333333));
#362705=CARTESIAN_POINT('Ctrl Pts',(-0.866025403784437,-1.49999999999999,
-7.42916666666667));
#362706=CARTESIAN_POINT('Ctrl Pts',(-1.83697019872102E-16,-1.49999999999999,
-7.3875));
#362707=CARTESIAN_POINT('Ctrl Pts',(0.866025403784436,-1.49999999999999,
-7.34583333333334));
#362708=CARTESIAN_POINT('Ctrl Pts',(1.29903810567665,-0.749999999999997,
-7.30416666666667));
#362709=CARTESIAN_POINT('Ctrl Pts',(1.73205080756887,1.19635593126651E-15,
-7.2625));
#362710=CARTESIAN_POINT('Ctrl Pts',(1.29903810567665,0.749999999999998,
-7.22083333333333));
#362711=CARTESIAN_POINT('Ctrl Pts',(0.866025403784437,1.5,-7.17916666666667));
#362712=CARTESIAN_POINT('Ctrl Pts',(0.,1.5,-7.1375));
#362713=CARTESIAN_POINT('Ctrl Pts',(-0.866025403784436,1.5,-7.09583333333333));
#362714=CARTESIAN_POINT('Ctrl Pts',(-1.29903810567665,0.749999999999999,
-7.05416666666667));
#362715=CARTESIAN_POINT('Ctrl Pts',(-1.73205080756887,1.51131210700991E-15,
-7.0125));
#362716=CARTESIAN_POINT('Ctrl Pts',(-1.29903810567665,-0.749999999999996,
-6.97083333333333));
#362717=CARTESIAN_POINT('Ctrl Pts',(-0.866025403784437,-1.49999999999999,
-6.92916666666667));
#362718=CARTESIAN_POINT('Ctrl Pts',(-1.83697019872102E-16,-1.49999999999999,
-6.8875));
#362719=CARTESIAN_POINT('Ctrl Pts',(0.866025403784436,-1.49999999999999,
-6.84583333333333));
#362720=CARTESIAN_POINT('Ctrl Pts',(1.29903810567665,-0.749999999999997,
-6.80416666666667));
#362721=CARTESIAN_POINT('Ctrl Pts',(1.73205080756887,9.77808091773373E-16,
-6.7625));
#362722=CARTESIAN_POINT('Ctrl Pts',(1.29903810567665,0.749999999999998,
-6.72083333333333));
#362723=CARTESIAN_POINT('Ctrl Pts',(0.866025403784437,1.5,-6.67916666666667));
#362724=CARTESIAN_POINT('Ctrl Pts',(0.,1.5,-6.6375));
#362725=CARTESIAN_POINT('Ctrl Pts',(-0.866025403784436,1.5,-6.59583333333333));
#362726=CARTESIAN_POINT('Ctrl Pts',(-1.29903810567665,0.749999999999999,
-6.55416666666667));
#362727=CARTESIAN_POINT('Ctrl Pts',(-1.73205080756887,1.29276426751676E-15,
-6.5125));
#362728=CARTESIAN_POINT('Ctrl Pts',(-1.29903810567665,-0.749999999999996,
-6.47083333333334));
#362729=CARTESIAN_POINT('Ctrl Pts',(-0.866025403784437,-1.49999999999999,
-6.42916666666667));
#362730=CARTESIAN_POINT('Ctrl Pts',(-1.83697019872102E-16,-1.49999999999999,
-6.3875));
#362731=CARTESIAN_POINT('Ctrl Pts',(0.866025403784436,-1.49999999999999,
-6.34583333333333));
#362732=CARTESIAN_POINT('Ctrl Pts',(1.29903810567665,-0.749999999999997,
-6.30416666666667));
#362733=CARTESIAN_POINT('Ctrl Pts',(1.73205080756887,7.59260252280232E-16,
-6.2625));
#362734=CARTESIAN_POINT('Ctrl Pts',(1.29903810567665,0.749999999999998,
-6.22083333333333));
#362735=CARTESIAN_POINT('Ctrl Pts',(0.866025403784437,1.5,-6.17916666666667));
#362736=CARTESIAN_POINT('Ctrl Pts',(0.,1.5,-6.1375));
#362737=CARTESIAN_POINT('Ctrl Pts',(-0.866025403784436,1.5,-6.09583333333334));
#362738=CARTESIAN_POINT('Ctrl Pts',(-1.29903810567665,0.749999999999999,
-6.05416666666667));
#362739=CARTESIAN_POINT('Ctrl Pts',(-1.73205080756887,1.07421642802362E-15,
-6.0125));
#362740=CARTESIAN_POINT('Ctrl Pts',(-1.29903810567665,-0.749999999999996,
-5.97083333333333));
#362741=CARTESIAN_POINT('Ctrl Pts',(-0.866025403784437,-1.49999999999999,
-5.92916666666667));
#362742=CARTESIAN_POINT('Ctrl Pts',(-1.83697019872102E-16,-1.49999999999999,
-5.8875));
#362743=CARTESIAN_POINT('Ctrl Pts',(0.866025403784436,-1.5,-5.84583333333334));
#362744=CARTESIAN_POINT('Ctrl Pts',(1.29903810567665,-0.749999999999998,
-5.80416666666667));
#362745=CARTESIAN_POINT('Ctrl Pts',(1.73205080756887,5.40712412787091E-16,
-5.7625));
#362746=CARTESIAN_POINT('Ctrl Pts',(1.29903810567665,0.749999999999998,
-5.72083333333333));
#362747=CARTESIAN_POINT('Ctrl Pts',(0.866025403784437,1.5,-5.67916666666667));
#362748=CARTESIAN_POINT('Ctrl Pts',(0.,1.5,-5.6375));
#362749=CARTESIAN_POINT('Ctrl Pts',(-0.866025403784436,1.5,-5.59583333333333));
#362750=CARTESIAN_POINT('Ctrl Pts',(-1.29903810567665,0.749999999999999,
-5.55416666666667));
#362751=CARTESIAN_POINT('Ctrl Pts',(-1.73205080756887,8.55668588530483E-16,
-5.5125));
#362752=CARTESIAN_POINT('Ctrl Pts',(-1.29903810567665,-0.749999999999997,
-5.47083333333333));
#362753=CARTESIAN_POINT('Ctrl Pts',(-0.866025403784437,-1.49999999999999,
-5.42916666666667));
#362754=CARTESIAN_POINT('Ctrl Pts',(-1.83697019872102E-16,-1.49999999999999,
-5.3875));
#362755=CARTESIAN_POINT('Ctrl Pts',(0.866025403784436,-1.5,-5.34583333333333));
#362756=CARTESIAN_POINT('Ctrl Pts',(1.29903810567665,-0.749999999999998,
-5.30416666666667));
#362757=CARTESIAN_POINT('Ctrl Pts',(1.73205080756887,3.2216457329395E-16,
-5.2625));
#362758=CARTESIAN_POINT('Ctrl Pts',(1.29903810567665,0.749999999999997,
-5.22083333333333));
#362759=CARTESIAN_POINT('Ctrl Pts',(0.866025403784437,1.5,-5.17916666666667));
#362760=CARTESIAN_POINT('Ctrl Pts',(0.,1.5,-5.1375));
#362761=CARTESIAN_POINT('Ctrl Pts',(-0.866025403784436,1.5,-5.09583333333333));
#362762=CARTESIAN_POINT('Ctrl Pts',(-1.29903810567665,0.749999999999998,
-5.05416666666667));
#362763=CARTESIAN_POINT('Ctrl Pts',(-1.73205080756887,6.37120749037341E-16,
-5.0125));
#362764=CARTESIAN_POINT('Ctrl Pts',(-1.29903810567665,-0.749999999999997,
-4.97083333333333));
#362765=CARTESIAN_POINT('Ctrl Pts',(-0.866025403784437,-1.49999999999999,
-4.92916666666667));
#362766=CARTESIAN_POINT('Ctrl Pts',(-1.83697019872102E-16,-1.5,-4.8875));
#362767=CARTESIAN_POINT('Ctrl Pts',(0.866025403784436,-1.5,-4.84583333333333));
#362768=CARTESIAN_POINT('Ctrl Pts',(1.29903810567665,-0.749999999999998,
-4.80416666666667));
#362769=CARTESIAN_POINT('Ctrl Pts',(1.73205080756887,1.03616733800808E-16,
-4.7625));
#362770=CARTESIAN_POINT('Ctrl Pts',(1.29903810567665,0.749999999999997,
-4.72083333333333));
#362771=CARTESIAN_POINT('Ctrl Pts',(0.866025403784437,1.5,-4.67916666666667));
#362772=CARTESIAN_POINT('Ctrl Pts',(0.,1.5,-4.6375));
#362773=CARTESIAN_POINT('Ctrl Pts',(-0.866025403784436,1.5,-4.59583333333333));
#362774=CARTESIAN_POINT('Ctrl Pts',(-1.29903810567665,0.749999999999998,
-4.55416666666667));
#362775=CARTESIAN_POINT('Ctrl Pts',(-1.73205080756887,4.185729095442E-16,
-4.5125));
#362776=CARTESIAN_POINT('Ctrl Pts',(-1.29903810567665,-0.749999999999997,
-4.47083333333333));
#362777=CARTESIAN_POINT('Ctrl Pts',(-0.866025403784437,-1.49999999999999,
-4.42916666666667));
#362778=CARTESIAN_POINT('Ctrl Pts',(-1.83697019872102E-16,-1.5,-4.3875));
#362779=CARTESIAN_POINT('Ctrl Pts',(0.866025403784436,-1.5,-4.34583333333333));
#362780=CARTESIAN_POINT('Ctrl Pts',(1.29903810567665,-0.749999999999998,
-4.30416666666667));
#362781=CARTESIAN_POINT('Ctrl Pts',(1.73205080756887,-1.14931105692333E-16,
-4.2625));
#362782=CARTESIAN_POINT('Ctrl Pts',(1.29903810567665,0.749999999999997,
-4.22083333333333));
#362783=CARTESIAN_POINT('Ctrl Pts',(0.866025403784437,1.5,-4.17916666666667));
#362784=CARTESIAN_POINT('Ctrl Pts',(0.,1.5,-4.1375));
#362785=CARTESIAN_POINT('Ctrl Pts',(-0.866025403784436,1.5,-4.09583333333333));
#362786=CARTESIAN_POINT('Ctrl Pts',(-1.29903810567665,0.749999999999998,
-4.05416666666667));
#362787=CARTESIAN_POINT('Ctrl Pts',(-1.73205080756887,2.00025070051059E-16,
-4.0125));
#362788=CARTESIAN_POINT('Ctrl Pts',(-1.29903810567665,-0.749999999999997,
-3.97083333333333));
#362789=CARTESIAN_POINT('Ctrl Pts',(-0.866025403784437,-1.5,-3.92916666666667));
#362790=CARTESIAN_POINT('Ctrl Pts',(-1.83697019872102E-16,-1.5,-3.8875));
#362791=CARTESIAN_POINT('Ctrl Pts',(0.866025403784436,-1.5,-3.84583333333333));
#362792=CARTESIAN_POINT('Ctrl Pts',(1.29903810567665,-0.749999999999998,
-3.80416666666667));
#362793=CARTESIAN_POINT('Ctrl Pts',(1.73205080756887,-3.33478945185474E-16,
-3.7625));
#362794=CARTESIAN_POINT('Ctrl Pts',(1.29903810567665,0.749999999999997,
-3.72083333333333));
#362795=CARTESIAN_POINT('Ctrl Pts',(0.866025403784437,1.5,-3.67916666666667));
#362796=CARTESIAN_POINT('Ctrl Pts',(0.,1.5,-3.6375));
#362797=CARTESIAN_POINT('Ctrl Pts',(-0.866025403784436,1.5,-3.59583333333333));
#362798=CARTESIAN_POINT('Ctrl Pts',(-1.29903810567665,0.749999999999998,
-3.55416666666667));
#362799=CARTESIAN_POINT('Ctrl Pts',(-1.73205080756887,-1.85227694420821E-17,
-3.5125));
#362800=CARTESIAN_POINT('Ctrl Pts',(-1.29903810567665,-0.749999999999998,
-3.47083333333333));
#362801=CARTESIAN_POINT('Ctrl Pts',(-0.866025403784437,-1.5,-3.42916666666667));
#362802=CARTESIAN_POINT('Ctrl Pts',(-1.83697019872102E-16,-1.5,-3.3875));
#362803=CARTESIAN_POINT('Ctrl Pts',(0.866025403784436,-1.5,-3.34583333333333));
#362804=CARTESIAN_POINT('Ctrl Pts',(1.29903810567665,-0.749999999999999,
-3.30416666666667));
#362805=CARTESIAN_POINT('Ctrl Pts',(1.73205080756887,-5.52026784678615E-16,
-3.2625));
#362806=CARTESIAN_POINT('Ctrl Pts',(1.29903810567665,0.749999999999996,
-3.22083333333333));
#362807=CARTESIAN_POINT('Ctrl Pts',(0.866025403784437,1.49999999999999,
-3.17916666666667));
#362808=CARTESIAN_POINT('Ctrl Pts',(0.,1.5,-3.1375));
#362809=CARTESIAN_POINT('Ctrl Pts',(-0.866025403784436,1.5,-3.09583333333333));
#362810=CARTESIAN_POINT('Ctrl Pts',(-1.29903810567665,0.749999999999998,
-3.05416666666667));
#362811=CARTESIAN_POINT('Ctrl Pts',(-1.73205080756887,-2.37070608935224E-16,
-3.0125));
#362812=CARTESIAN_POINT('Ctrl Pts',(-1.29903810567665,-0.749999999999998,
-2.97083333333333));
#362813=CARTESIAN_POINT('Ctrl Pts',(-0.866025403784437,-1.5,-2.92916666666667));
#362814=CARTESIAN_POINT('Ctrl Pts',(-1.83697019872102E-16,-1.5,-2.8875));
#362815=CARTESIAN_POINT('Ctrl Pts',(0.866025403784436,-1.5,-2.84583333333333));
#362816=CARTESIAN_POINT('Ctrl Pts',(1.29903810567665,-0.749999999999999,
-2.80416666666667));
#362817=CARTESIAN_POINT('Ctrl Pts',(1.73205080756887,-7.70574624171757E-16,
-2.7625));
#362818=CARTESIAN_POINT('Ctrl Pts',(1.29903810567665,0.749999999999996,
-2.72083333333334));
#362819=CARTESIAN_POINT('Ctrl Pts',(0.866025403784437,1.49999999999999,
-2.67916666666667));
#362820=CARTESIAN_POINT('Ctrl Pts',(0.,1.5,-2.6375));
#362821=CARTESIAN_POINT('Ctrl Pts',(-0.866025403784436,1.5,-2.59583333333334));
#362822=CARTESIAN_POINT('Ctrl Pts',(-1.29903810567665,0.749999999999997,
-2.55416666666667));
#362823=CARTESIAN_POINT('Ctrl Pts',(-1.73205080756887,-4.55618448428365E-16,
-2.5125));
#362824=CARTESIAN_POINT('Ctrl Pts',(-1.29903810567665,-0.749999999999998,
-2.47083333333334));
#362825=CARTESIAN_POINT('Ctrl Pts',(-0.866025403784437,-1.5,-2.42916666666667));
#362826=CARTESIAN_POINT('Ctrl Pts',(-1.83697019872102E-16,-1.5,-2.3875));
#362827=CARTESIAN_POINT('Ctrl Pts',(0.866025403784436,-1.5,-2.34583333333334));
#362828=CARTESIAN_POINT('Ctrl Pts',(1.29903810567665,-0.749999999999999,
-2.30416666666667));
#362829=CARTESIAN_POINT('Ctrl Pts',(1.73205080756887,-9.89122463664898E-16,
-2.2625));
#362830=CARTESIAN_POINT('Ctrl Pts',(1.29903810567665,0.749999999999996,
-2.22083333333333));
#362831=CARTESIAN_POINT('Ctrl Pts',(0.866025403784437,1.49999999999999,
-2.17916666666667));
#362832=CARTESIAN_POINT('Ctrl Pts',(0.,1.49999999999999,-2.1375));
#362833=CARTESIAN_POINT('Ctrl Pts',(-0.866025403784436,1.49999999999999,
-2.09583333333333));
#362834=CARTESIAN_POINT('Ctrl Pts',(-1.29903810567665,0.749999999999997,
-2.05416666666667));
#362835=CARTESIAN_POINT('Ctrl Pts',(-1.73205080756887,-6.74166287921507E-16,
-2.0125));
#362836=CARTESIAN_POINT('Ctrl Pts',(-1.29903810567665,-0.749999999999998,
-1.97083333333333));
#362837=CARTESIAN_POINT('Ctrl Pts',(-0.866025403784437,-1.5,-1.92916666666667));
#362838=CARTESIAN_POINT('Ctrl Pts',(-1.83697019872102E-16,-1.5,-1.8875));
#362839=CARTESIAN_POINT('Ctrl Pts',(0.866025403784436,-1.5,-1.84583333333334));
#362840=CARTESIAN_POINT('Ctrl Pts',(1.29903810567665,-0.749999999999999,
-1.80416666666667));
#362841=CARTESIAN_POINT('Ctrl Pts',(1.73205080756887,-1.20767030315804E-15,
-1.7625));
#362842=CARTESIAN_POINT('Ctrl Pts',(1.29903810567665,0.749999999999996,
-1.72083333333333));
#362843=CARTESIAN_POINT('Ctrl Pts',(0.866025403784437,1.49999999999999,
-1.67916666666667));
#362844=CARTESIAN_POINT('Ctrl Pts',(0.,1.49999999999999,-1.6375));
#362845=CARTESIAN_POINT('Origin',(-1.38777878078146E-16,-5.55111512312578E-15,
-17.91875));
#362846=CARTESIAN_POINT('Ctrl Pts',(-0.190653686693216,-1.15967294634856,
-17.6497595264192));
#362847=CARTESIAN_POINT('Ctrl Pts',(-0.0959624143348497,-1.17524047358082,
-17.6433928286374));
#362848=CARTESIAN_POINT('Ctrl Pts',(-1.43925448419918E-16,-1.17524047358082,
-17.6375));
#362849=CARTESIAN_POINT('Ctrl Pts',(0.,1.50000395501636,-17.6999977165702));
#362850=CARTESIAN_POINT('Ctrl Pts',(-0.866027687214197,1.50000395501636,
-17.6583310499036));
#362851=CARTESIAN_POINT('Ctrl Pts',(-1.2990415308213,0.750001977508185,
-17.6166643832369));
#362852=CARTESIAN_POINT('Ctrl Pts',(-1.73205537442839,6.12813449786473E-15,
-17.5749977165702));
#362853=CARTESIAN_POINT('Ctrl Pts',(-1.2990415308213,-0.750001977508172,
-17.5333310499036));
#362854=CARTESIAN_POINT('Ctrl Pts',(-0.866027687214197,-1.50000395501635,
-17.4916643832369));
#362855=CARTESIAN_POINT('Ctrl Pts',(-1.83697504221915E-16,-1.50000395501635,
-17.4499977165702));
#362856=CARTESIAN_POINT('Ctrl Pts',(0.866027687214196,-1.50000395501635,
-17.4083310499036));
#362857=CARTESIAN_POINT('Ctrl Pts',(1.29904153082129,-0.750001977508173,
-17.3666643832369));
#362858=CARTESIAN_POINT('Ctrl Pts',(1.73205537442839,5.59462936407022E-15,
-17.3249977165702));
#362859=CARTESIAN_POINT('Ctrl Pts',(1.2990415308213,0.750001977508183,-17.2833310499036));
#362860=CARTESIAN_POINT('Ctrl Pts',(0.866027687214198,1.50000395501636,
-17.2416643832369));
#362861=CARTESIAN_POINT('Ctrl Pts',(0.,1.50000395501636,-17.1999977165702));
#362862=CARTESIAN_POINT('Ctrl Pts',(-0.866027687214197,1.50000395501636,
-17.1583310499036));
#362863=CARTESIAN_POINT('Ctrl Pts',(-1.2990415308213,0.750001977508185,
-17.1166643832369));
#362864=CARTESIAN_POINT('Ctrl Pts',(-1.73205537442839,5.90958665837159E-15,
-17.0749977165702));
#362865=CARTESIAN_POINT('Ctrl Pts',(-1.2990415308213,-0.750001977508172,
-17.0333310499036));
#362866=CARTESIAN_POINT('Ctrl Pts',(-0.866027687214197,-1.50000395501635,
-16.9916643832369));
#362867=CARTESIAN_POINT('Ctrl Pts',(-1.83697504221915E-16,-1.50000395501635,
-16.9499977165702));
#362868=CARTESIAN_POINT('Ctrl Pts',(0.866027687214196,-1.50000395501635,
-16.9083310499036));
#362869=CARTESIAN_POINT('Ctrl Pts',(1.29904153082129,-0.750001977508173,
-16.8666643832369));
#362870=CARTESIAN_POINT('Ctrl Pts',(1.73205537442839,5.37608152457707E-15,
-16.8249977165702));
#362871=CARTESIAN_POINT('Ctrl Pts',(1.2990415308213,0.750001977508183,-16.7833310499036));
#362872=CARTESIAN_POINT('Ctrl Pts',(0.866027687214198,1.50000395501636,
-16.7416643832369));
#362873=CARTESIAN_POINT('Ctrl Pts',(0.,1.50000395501636,-16.6999977165702));
#362874=CARTESIAN_POINT('Ctrl Pts',(-0.866027687214197,1.50000395501636,
-16.6583310499036));
#362875=CARTESIAN_POINT('Ctrl Pts',(-1.2990415308213,0.750001977508184,
-16.6166643832369));
#362876=CARTESIAN_POINT('Ctrl Pts',(-1.73205537442839,5.69103881887844E-15,
-16.5749977165702));
#362877=CARTESIAN_POINT('Ctrl Pts',(-1.2990415308213,-0.750001977508173,
-16.5333310499036));
#362878=CARTESIAN_POINT('Ctrl Pts',(-0.866027687214197,-1.50000395501635,
-16.4916643832369));
#362879=CARTESIAN_POINT('Ctrl Pts',(-1.83697504221915E-16,-1.50000395501635,
-16.4499977165702));
#362880=CARTESIAN_POINT('Ctrl Pts',(0.866027687214196,-1.50000395501635,
-16.4083310499036));
#362881=CARTESIAN_POINT('Ctrl Pts',(1.29904153082129,-0.750001977508174,
-16.3666643832369));
#362882=CARTESIAN_POINT('Ctrl Pts',(1.73205537442839,5.15753368508393E-15,
-16.3249977165702));
#362883=CARTESIAN_POINT('Ctrl Pts',(1.2990415308213,0.750001977508183,-16.2833310499036));
#362884=CARTESIAN_POINT('Ctrl Pts',(0.866027687214198,1.50000395501636,
-16.2416643832369));
#362885=CARTESIAN_POINT('Ctrl Pts',(0.,1.50000395501636,-16.1999977165702));
#362886=CARTESIAN_POINT('Ctrl Pts',(-0.866027687214197,1.50000395501636,
-16.1583310499036));
#362887=CARTESIAN_POINT('Ctrl Pts',(-1.2990415308213,0.750001977508184,
-16.1166643832369));
#362888=CARTESIAN_POINT('Ctrl Pts',(-1.73205537442839,5.4724909793853E-15,
-16.0749977165702));
#362889=CARTESIAN_POINT('Ctrl Pts',(-1.2990415308213,-0.750001977508173,
-16.0333310499036));
#362890=CARTESIAN_POINT('Ctrl Pts',(-0.866027687214197,-1.50000395501635,
-15.9916643832369));
#362891=CARTESIAN_POINT('Ctrl Pts',(-1.83697504221915E-16,-1.50000395501635,
-15.9499977165702));
#362892=CARTESIAN_POINT('Ctrl Pts',(0.866027687214196,-1.50000395501635,
-15.9083310499036));
#362893=CARTESIAN_POINT('Ctrl Pts',(1.29904153082129,-0.750001977508174,
-15.8666643832369));
#362894=CARTESIAN_POINT('Ctrl Pts',(1.73205537442839,4.93898584559079E-15,
-15.8249977165702));
#362895=CARTESIAN_POINT('Ctrl Pts',(1.2990415308213,0.750001977508183,-15.7833310499036));
#362896=CARTESIAN_POINT('Ctrl Pts',(0.866027687214198,1.50000395501636,
-15.7416643832369));
#362897=CARTESIAN_POINT('Ctrl Pts',(0.,1.50000395501636,-15.6999977165702));
#362898=CARTESIAN_POINT('Ctrl Pts',(-0.866027687214197,1.50000395501636,
-15.6583310499036));
#362899=CARTESIAN_POINT('Ctrl Pts',(-1.2990415308213,0.750001977508184,
-15.6166643832369));
#362900=CARTESIAN_POINT('Ctrl Pts',(-1.73205537442839,5.25394313989216E-15,
-15.5749977165702));
#362901=CARTESIAN_POINT('Ctrl Pts',(-1.2990415308213,-0.750001977508173,
-15.5333310499036));
#362902=CARTESIAN_POINT('Ctrl Pts',(-0.866027687214197,-1.50000395501635,
-15.4916643832369));
#362903=CARTESIAN_POINT('Ctrl Pts',(-1.83697504221915E-16,-1.50000395501635,
-15.4499977165702));
#362904=CARTESIAN_POINT('Ctrl Pts',(0.866027687214196,-1.50000395501635,
-15.4083310499036));
#362905=CARTESIAN_POINT('Ctrl Pts',(1.29904153082129,-0.750001977508174,
-15.3666643832369));
#362906=CARTESIAN_POINT('Ctrl Pts',(1.73205537442839,4.72043800609765E-15,
-15.3249977165702));
#362907=CARTESIAN_POINT('Ctrl Pts',(1.2990415308213,0.750001977508182,-15.2833310499036));
#362908=CARTESIAN_POINT('Ctrl Pts',(0.866027687214198,1.50000395501636,
-15.2416643832369));
#362909=CARTESIAN_POINT('Ctrl Pts',(0.,1.50000395501636,-15.1999977165702));
#362910=CARTESIAN_POINT('Ctrl Pts',(-0.866027687214197,1.50000395501636,
-15.1583310499036));
#362911=CARTESIAN_POINT('Ctrl Pts',(-1.2990415308213,0.750001977508184,
-15.1166643832369));
#362912=CARTESIAN_POINT('Ctrl Pts',(-1.73205537442839,5.03539530039902E-15,
-15.0749977165702));
#362913=CARTESIAN_POINT('Ctrl Pts',(-1.2990415308213,-0.750001977508173,
-15.0333310499036));
#362914=CARTESIAN_POINT('Ctrl Pts',(-0.866027687214197,-1.50000395501635,
-14.9916643832369));
#362915=CARTESIAN_POINT('Ctrl Pts',(-1.83697504221915E-16,-1.50000395501635,
-14.9499977165702));
#362916=CARTESIAN_POINT('Ctrl Pts',(0.866027687214196,-1.50000395501635,
-14.9083310499036));
#362917=CARTESIAN_POINT('Ctrl Pts',(1.29904153082129,-0.750001977508174,
-14.8666643832369));
#362918=CARTESIAN_POINT('Ctrl Pts',(1.73205537442839,4.50189016660451E-15,
-14.8249977165702));
#362919=CARTESIAN_POINT('Ctrl Pts',(1.2990415308213,0.750001977508182,-14.7833310499036));
#362920=CARTESIAN_POINT('Ctrl Pts',(0.866027687214198,1.50000395501636,
-14.7416643832369));
#362921=CARTESIAN_POINT('Ctrl Pts',(0.,1.50000395501636,-14.6999977165702));
#362922=CARTESIAN_POINT('Ctrl Pts',(-0.866027687214197,1.50000395501636,
-14.6583310499036));
#362923=CARTESIAN_POINT('Ctrl Pts',(-1.2990415308213,0.750001977508183,
-14.6166643832369));
#362924=CARTESIAN_POINT('Ctrl Pts',(-1.73205537442839,4.81684746090588E-15,
-14.5749977165702));
#362925=CARTESIAN_POINT('Ctrl Pts',(-1.2990415308213,-0.750001977508173,
-14.5333310499036));
#362926=CARTESIAN_POINT('Ctrl Pts',(-0.866027687214197,-1.50000395501635,
-14.4916643832369));
#362927=CARTESIAN_POINT('Ctrl Pts',(-1.83697504221915E-16,-1.50000395501635,
-14.4499977165702));
#362928=CARTESIAN_POINT('Ctrl Pts',(0.866027687214196,-1.50000395501635,
-14.4083310499036));
#362929=CARTESIAN_POINT('Ctrl Pts',(1.29904153082129,-0.750001977508174,
-14.3666643832369));
#362930=CARTESIAN_POINT('Ctrl Pts',(1.73205537442839,4.28334232711137E-15,
-14.3249977165702));
#362931=CARTESIAN_POINT('Ctrl Pts',(1.2990415308213,0.750001977508182,-14.2833310499036));
#362932=CARTESIAN_POINT('Ctrl Pts',(0.866027687214198,1.50000395501636,
-14.2416643832369));
#362933=CARTESIAN_POINT('Ctrl Pts',(0.,1.50000395501636,-14.1999977165702));
#362934=CARTESIAN_POINT('Ctrl Pts',(-0.866027687214197,1.50000395501636,
-14.1583310499036));
#362935=CARTESIAN_POINT('Ctrl Pts',(-1.2990415308213,0.750001977508183,
-14.1166643832369));
#362936=CARTESIAN_POINT('Ctrl Pts',(-1.73205537442839,4.59829962141274E-15,
-14.0749977165702));
#362937=CARTESIAN_POINT('Ctrl Pts',(-1.2990415308213,-0.750001977508174,
-14.0333310499036));
#362938=CARTESIAN_POINT('Ctrl Pts',(-0.866027687214197,-1.50000395501635,
-13.9916643832369));
#362939=CARTESIAN_POINT('Ctrl Pts',(-1.83697504221915E-16,-1.50000395501635,
-13.9499977165702));
#362940=CARTESIAN_POINT('Ctrl Pts',(0.866027687214196,-1.50000395501635,
-13.9083310499036));
#362941=CARTESIAN_POINT('Ctrl Pts',(1.29904153082129,-0.750001977508175,
-13.8666643832369));
#362942=CARTESIAN_POINT('Ctrl Pts',(1.73205537442839,4.06479448761823E-15,
-13.8249977165702));
#362943=CARTESIAN_POINT('Ctrl Pts',(1.2990415308213,0.750001977508182,-13.7833310499036));
#362944=CARTESIAN_POINT('Ctrl Pts',(0.866027687214198,1.50000395501636,
-13.7416643832369));
#362945=CARTESIAN_POINT('Ctrl Pts',(0.,1.50000395501636,-13.6999977165702));
#362946=CARTESIAN_POINT('Ctrl Pts',(-0.866027687214197,1.50000395501636,
-13.6583310499036));
#362947=CARTESIAN_POINT('Ctrl Pts',(-1.2990415308213,0.750001977508183,
-13.6166643832369));
#362948=CARTESIAN_POINT('Ctrl Pts',(-1.73205537442839,4.3797517819196E-15,
-13.5749977165702));
#362949=CARTESIAN_POINT('Ctrl Pts',(-1.2990415308213,-0.750001977508174,
-13.5333310499036));
#362950=CARTESIAN_POINT('Ctrl Pts',(-0.866027687214197,-1.50000395501635,
-13.4916643832369));
#362951=CARTESIAN_POINT('Ctrl Pts',(-1.83697504221915E-16,-1.50000395501635,
-13.4499977165702));
#362952=CARTESIAN_POINT('Ctrl Pts',(0.866027687214196,-1.50000395501635,
-13.4083310499036));
#362953=CARTESIAN_POINT('Ctrl Pts',(1.29904153082129,-0.750001977508175,
-13.3666643832369));
#362954=CARTESIAN_POINT('Ctrl Pts',(1.73205537442839,3.84624664812509E-15,
-13.3249977165702));
#362955=CARTESIAN_POINT('Ctrl Pts',(1.2990415308213,0.750001977508181,-13.2833310499036));
#362956=CARTESIAN_POINT('Ctrl Pts',(0.866027687214198,1.50000395501636,
-13.2416643832369));
#362957=CARTESIAN_POINT('Ctrl Pts',(0.,1.50000395501636,-13.1999977165702));
#362958=CARTESIAN_POINT('Ctrl Pts',(-0.866027687214197,1.50000395501636,
-13.1583310499036));
#362959=CARTESIAN_POINT('Ctrl Pts',(-1.2990415308213,0.750001977508183,
-13.1166643832369));
#362960=CARTESIAN_POINT('Ctrl Pts',(-1.73205537442839,4.16120394242646E-15,
-13.0749977165702));
#362961=CARTESIAN_POINT('Ctrl Pts',(-1.2990415308213,-0.750001977508174,
-13.0333310499036));
#362962=CARTESIAN_POINT('Ctrl Pts',(-0.866027687214197,-1.50000395501635,
-12.9916643832369));
#362963=CARTESIAN_POINT('Ctrl Pts',(-1.83697504221915E-16,-1.50000395501635,
-12.9499977165702));
#362964=CARTESIAN_POINT('Ctrl Pts',(0.866027687214196,-1.50000395501635,
-12.9083310499036));
#362965=CARTESIAN_POINT('Ctrl Pts',(1.29904153082129,-0.750001977508175,
-12.8666643832369));
#362966=CARTESIAN_POINT('Ctrl Pts',(1.73205537442839,3.62769880863194E-15,
-12.8249977165702));
#362967=CARTESIAN_POINT('Ctrl Pts',(1.2990415308213,0.750001977508181,-12.7833310499036));
#362968=CARTESIAN_POINT('Ctrl Pts',(0.866027687214198,1.50000395501636,
-12.7416643832369));
#362969=CARTESIAN_POINT('Ctrl Pts',(0.,1.50000395501636,-12.6999977165702));
#362970=CARTESIAN_POINT('Ctrl Pts',(-0.866027687214197,1.50000395501636,
-12.6583310499036));
#362971=CARTESIAN_POINT('Ctrl Pts',(-1.2990415308213,0.750001977508183,
-12.6166643832369));
#362972=CARTESIAN_POINT('Ctrl Pts',(-1.73205537442839,3.94265610293331E-15,
-12.5749977165702));
#362973=CARTESIAN_POINT('Ctrl Pts',(-1.2990415308213,-0.750001977508174,
-12.5333310499036));
#362974=CARTESIAN_POINT('Ctrl Pts',(-0.866027687214197,-1.50000395501635,
-12.4916643832369));
#362975=CARTESIAN_POINT('Ctrl Pts',(-1.83697504221915E-16,-1.50000395501635,
-12.4499977165702));
#362976=CARTESIAN_POINT('Ctrl Pts',(0.866027687214196,-1.50000395501635,
-12.4083310499036));
#362977=CARTESIAN_POINT('Ctrl Pts',(1.29904153082129,-0.750001977508175,
-12.3666643832369));
#362978=CARTESIAN_POINT('Ctrl Pts',(1.73205537442839,3.4091509691388E-15,
-12.3249977165702));
#362979=CARTESIAN_POINT('Ctrl Pts',(1.2990415308213,0.750001977508181,-12.2833310499036));
#362980=CARTESIAN_POINT('Ctrl Pts',(0.866027687214198,1.50000395501636,
-12.2416643832369));
#362981=CARTESIAN_POINT('Ctrl Pts',(0.,1.50000395501636,-12.1999977165702));
#362982=CARTESIAN_POINT('Ctrl Pts',(-0.866027687214197,1.50000395501636,
-12.1583310499036));
#362983=CARTESIAN_POINT('Ctrl Pts',(-1.2990415308213,0.750001977508182,
-12.1166643832369));
#362984=CARTESIAN_POINT('Ctrl Pts',(-1.73205537442839,3.72410826344017E-15,
-12.0749977165702));
#362985=CARTESIAN_POINT('Ctrl Pts',(-1.2990415308213,-0.750001977508174,
-12.0333310499036));
#362986=CARTESIAN_POINT('Ctrl Pts',(-0.866027687214197,-1.50000395501635,
-11.9916643832369));
#362987=CARTESIAN_POINT('Ctrl Pts',(-1.83697504221915E-16,-1.50000395501635,
-11.9499977165702));
#362988=CARTESIAN_POINT('Ctrl Pts',(0.866027687214196,-1.50000395501635,
-11.9083310499036));
#362989=CARTESIAN_POINT('Ctrl Pts',(1.29904153082129,-0.750001977508176,
-11.8666643832369));
#362990=CARTESIAN_POINT('Ctrl Pts',(1.73205537442839,3.19060312964566E-15,
-11.8249977165702));
#362991=CARTESIAN_POINT('Ctrl Pts',(1.2990415308213,0.750001977508181,-11.7833310499036));
#362992=CARTESIAN_POINT('Ctrl Pts',(0.866027687214198,1.50000395501636,
-11.7416643832369));
#362993=CARTESIAN_POINT('Ctrl Pts',(0.,1.50000395501636,-11.6999977165702));
#362994=CARTESIAN_POINT('Ctrl Pts',(-0.866027687214197,1.50000395501636,
-11.6583310499036));
#362995=CARTESIAN_POINT('Ctrl Pts',(-1.2990415308213,0.750001977508182,
-11.6166643832369));
#362996=CARTESIAN_POINT('Ctrl Pts',(-1.73205537442839,3.50556042394703E-15,
-11.5749977165702));
#362997=CARTESIAN_POINT('Ctrl Pts',(-1.2990415308213,-0.750001977508175,
-11.5333310499036));
#362998=CARTESIAN_POINT('Ctrl Pts',(-0.866027687214197,-1.50000395501635,
-11.4916643832369));
#362999=CARTESIAN_POINT('Ctrl Pts',(-1.83697504221915E-16,-1.50000395501635,
-11.4499977165702));
#363000=CARTESIAN_POINT('Ctrl Pts',(0.866027687214196,-1.50000395501635,
-11.4083310499036));
#363001=CARTESIAN_POINT('Ctrl Pts',(1.29904153082129,-0.750001977508176,
-11.3666643832369));
#363002=CARTESIAN_POINT('Ctrl Pts',(1.73205537442839,2.97205529015252E-15,
-11.3249977165702));
#363003=CARTESIAN_POINT('Ctrl Pts',(1.2990415308213,0.750001977508181,-11.2833310499036));
#363004=CARTESIAN_POINT('Ctrl Pts',(0.866027687214198,1.50000395501636,
-11.2416643832369));
#363005=CARTESIAN_POINT('Ctrl Pts',(0.,1.50000395501636,-11.1999977165702));
#363006=CARTESIAN_POINT('Ctrl Pts',(-0.866027687214197,1.50000395501636,
-11.1583310499036));
#363007=CARTESIAN_POINT('Ctrl Pts',(-1.2990415308213,0.750001977508182,
-11.1166643832369));
#363008=CARTESIAN_POINT('Ctrl Pts',(-1.73205537442839,3.28701258445389E-15,
-11.0749977165702));
#363009=CARTESIAN_POINT('Ctrl Pts',(-1.2990415308213,-0.750001977508175,
-11.0333310499036));
#363010=CARTESIAN_POINT('Ctrl Pts',(-0.866027687214197,-1.50000395501635,
-10.9916643832369));
#363011=CARTESIAN_POINT('Ctrl Pts',(-1.83697504221915E-16,-1.50000395501635,
-10.9499977165702));
#363012=CARTESIAN_POINT('Ctrl Pts',(0.866027687214196,-1.50000395501635,
-10.9083310499036));
#363013=CARTESIAN_POINT('Ctrl Pts',(1.29904153082129,-0.750001977508176,
-10.8666643832369));
#363014=CARTESIAN_POINT('Ctrl Pts',(1.73205537442839,2.75350745065938E-15,
-10.8249977165702));
#363015=CARTESIAN_POINT('Ctrl Pts',(1.2990415308213,0.75000197750818,-10.7833310499036));
#363016=CARTESIAN_POINT('Ctrl Pts',(0.866027687214198,1.50000395501636,
-10.7416643832369));
#363017=CARTESIAN_POINT('Ctrl Pts',(0.,1.50000395501636,-10.6999977165702));
#363018=CARTESIAN_POINT('Ctrl Pts',(-0.866027687214197,1.50000395501636,
-10.6583310499036));
#363019=CARTESIAN_POINT('Ctrl Pts',(-1.2990415308213,0.750001977508182,
-10.6166643832369));
#363020=CARTESIAN_POINT('Ctrl Pts',(-1.73205537442839,3.06846474496075E-15,
-10.5749977165702));
#363021=CARTESIAN_POINT('Ctrl Pts',(-1.2990415308213,-0.750001977508175,
-10.5333310499036));
#363022=CARTESIAN_POINT('Ctrl Pts',(-0.866027687214197,-1.50000395501635,
-10.4916643832369));
#363023=CARTESIAN_POINT('Ctrl Pts',(-1.83697504221915E-16,-1.50000395501635,
-10.4499977165702));
#363024=CARTESIAN_POINT('Ctrl Pts',(0.866027687214196,-1.50000395501635,
-10.4083310499036));
#363025=CARTESIAN_POINT('Ctrl Pts',(1.29904153082129,-0.750001977508176,
-10.3666643832369));
#363026=CARTESIAN_POINT('Ctrl Pts',(1.73205537442839,2.53495961116624E-15,
-10.3249977165702));
#363027=CARTESIAN_POINT('Ctrl Pts',(1.2990415308213,0.75000197750818,-10.2833310499036));
#363028=CARTESIAN_POINT('Ctrl Pts',(0.866027687214198,1.50000395501636,
-10.2416643832369));
#363029=CARTESIAN_POINT('Ctrl Pts',(0.,1.50000395501636,-10.1999977165702));
#363030=CARTESIAN_POINT('Ctrl Pts',(-0.866027687214197,1.50000395501636,
-10.1583310499036));
#363031=CARTESIAN_POINT('Ctrl Pts',(-1.2990415308213,0.750001977508181,
-10.1166643832369));
#363032=CARTESIAN_POINT('Ctrl Pts',(-1.73205537442839,2.84991690546761E-15,
-10.0749977165702));
#363033=CARTESIAN_POINT('Ctrl Pts',(-1.2990415308213,-0.750001977508175,
-10.0333310499036));
#363034=CARTESIAN_POINT('Ctrl Pts',(-0.866027687214197,-1.50000395501635,
-9.99166438323691));
#363035=CARTESIAN_POINT('Ctrl Pts',(-1.83697504221915E-16,-1.50000395501635,
-9.94999771657024));
#363036=CARTESIAN_POINT('Ctrl Pts',(0.866027687214196,-1.50000395501635,
-9.90833104990357));
#363037=CARTESIAN_POINT('Ctrl Pts',(1.29904153082129,-0.750001977508177,
-9.86666438323691));
#363038=CARTESIAN_POINT('Ctrl Pts',(1.73205537442839,2.3164117716731E-15,
-9.82499771657024));
#363039=CARTESIAN_POINT('Ctrl Pts',(1.2990415308213,0.75000197750818,-9.78333104990358));
#363040=CARTESIAN_POINT('Ctrl Pts',(0.866027687214198,1.50000395501636,
-9.74166438323691));
#363041=CARTESIAN_POINT('Ctrl Pts',(0.,1.50000395501636,-9.69999771657024));
#363042=CARTESIAN_POINT('Ctrl Pts',(-0.866027687214197,1.50000395501636,
-9.65833104990358));
#363043=CARTESIAN_POINT('Ctrl Pts',(-1.2990415308213,0.750001977508181,
-9.61666438323691));
#363044=CARTESIAN_POINT('Ctrl Pts',(-1.73205537442839,2.63136906597447E-15,
-9.57499771657024));
#363045=CARTESIAN_POINT('Ctrl Pts',(-1.2990415308213,-0.750001977508176,
-9.53333104990358));
#363046=CARTESIAN_POINT('Ctrl Pts',(-0.866027687214197,-1.50000395501635,
-9.49166438323691));
#363047=CARTESIAN_POINT('Ctrl Pts',(-1.83697504221915E-16,-1.50000395501635,
-9.44999771657024));
#363048=CARTESIAN_POINT('Ctrl Pts',(0.866027687214196,-1.50000395501635,
-9.40833104990358));
#363049=CARTESIAN_POINT('Ctrl Pts',(1.29904153082129,-0.750001977508177,
-9.36666438323691));
#363050=CARTESIAN_POINT('Ctrl Pts',(1.73205537442839,2.09786393217996E-15,
-9.32499771657024));
#363051=CARTESIAN_POINT('Ctrl Pts',(1.2990415308213,0.75000197750818,-9.28333104990358));
#363052=CARTESIAN_POINT('Ctrl Pts',(0.866027687214198,1.50000395501636,
-9.24166438323691));
#363053=CARTESIAN_POINT('Ctrl Pts',(0.,1.50000395501636,-9.19999771657024));
#363054=CARTESIAN_POINT('Ctrl Pts',(-0.866027687214197,1.50000395501636,
-9.15833104990357));
#363055=CARTESIAN_POINT('Ctrl Pts',(-1.2990415308213,0.750001977508181,
-9.11666438323691));
#363056=CARTESIAN_POINT('Ctrl Pts',(-1.73205537442839,2.41282122648133E-15,
-9.07499771657024));
#363057=CARTESIAN_POINT('Ctrl Pts',(-1.2990415308213,-0.750001977508176,
-9.03333104990358));
#363058=CARTESIAN_POINT('Ctrl Pts',(-0.866027687214197,-1.50000395501635,
-8.99166438323691));
#363059=CARTESIAN_POINT('Ctrl Pts',(-1.83697504221915E-16,-1.50000395501635,
-8.94999771657024));
#363060=CARTESIAN_POINT('Ctrl Pts',(0.866027687214196,-1.50000395501635,
-8.90833104990357));
#363061=CARTESIAN_POINT('Ctrl Pts',(1.29904153082129,-0.750001977508177,
-8.86666438323691));
#363062=CARTESIAN_POINT('Ctrl Pts',(1.73205537442839,1.87931609268682E-15,
-8.82499771657024));
#363063=CARTESIAN_POINT('Ctrl Pts',(1.2990415308213,0.750001977508179,-8.78333104990358));
#363064=CARTESIAN_POINT('Ctrl Pts',(0.866027687214198,1.50000395501636,
-8.74166438323691));
#363065=CARTESIAN_POINT('Ctrl Pts',(0.,1.50000395501636,-8.69999771657024));
#363066=CARTESIAN_POINT('Ctrl Pts',(-0.866027687214197,1.50000395501636,
-8.65833104990357));
#363067=CARTESIAN_POINT('Ctrl Pts',(-1.2990415308213,0.750001977508181,
-8.61666438323691));
#363068=CARTESIAN_POINT('Ctrl Pts',(-1.73205537442839,2.19427338698818E-15,
-8.57499771657024));
#363069=CARTESIAN_POINT('Ctrl Pts',(-1.2990415308213,-0.750001977508176,
-8.53333104990357));
#363070=CARTESIAN_POINT('Ctrl Pts',(-0.866027687214197,-1.50000395501635,
-8.49166438323691));
#363071=CARTESIAN_POINT('Ctrl Pts',(-1.83697504221915E-16,-1.50000395501635,
-8.44999771657024));
#363072=CARTESIAN_POINT('Ctrl Pts',(0.866027687214196,-1.50000395501635,
-8.40833104990357));
#363073=CARTESIAN_POINT('Ctrl Pts',(1.29904153082129,-0.750001977508177,
-8.36666438323691));
#363074=CARTESIAN_POINT('Ctrl Pts',(1.73205537442839,1.66076825319367E-15,
-8.32499771657024));
#363075=CARTESIAN_POINT('Ctrl Pts',(1.2990415308213,0.750001977508179,-8.28333104990357));
#363076=CARTESIAN_POINT('Ctrl Pts',(0.866027687214198,1.50000395501636,
-8.24166438323691));
#363077=CARTESIAN_POINT('Ctrl Pts',(0.,1.50000395501636,-8.19999771657024));
#363078=CARTESIAN_POINT('Ctrl Pts',(-0.866027687214197,1.50000395501636,
-8.15833104990357));
#363079=CARTESIAN_POINT('Ctrl Pts',(-1.2990415308213,0.750001977508181,
-8.11666438323691));
#363080=CARTESIAN_POINT('Ctrl Pts',(-1.73205537442839,1.97572554749504E-15,
-8.07499771657024));
#363081=CARTESIAN_POINT('Ctrl Pts',(-1.2990415308213,-0.750001977508176,
-8.03333104990357));
#363082=CARTESIAN_POINT('Ctrl Pts',(-0.866027687214197,-1.50000395501635,
-7.99166438323691));
#363083=CARTESIAN_POINT('Ctrl Pts',(-1.83697504221915E-16,-1.50000395501636,
-7.94999771657024));
#363084=CARTESIAN_POINT('Ctrl Pts',(0.866027687214196,-1.50000395501636,
-7.90833104990357));
#363085=CARTESIAN_POINT('Ctrl Pts',(1.29904153082129,-0.750001977508177,
-7.86666438323691));
#363086=CARTESIAN_POINT('Ctrl Pts',(1.73205537442839,1.44222041370053E-15,
-7.82499771657024));
#363087=CARTESIAN_POINT('Ctrl Pts',(1.2990415308213,0.750001977508179,-7.78333104990358));
#363088=CARTESIAN_POINT('Ctrl Pts',(0.866027687214198,1.50000395501636,
-7.74166438323691));
#363089=CARTESIAN_POINT('Ctrl Pts',(0.,1.50000395501636,-7.69999771657024));
#363090=CARTESIAN_POINT('Ctrl Pts',(-0.866027687214197,1.50000395501636,
-7.65833104990358));
#363091=CARTESIAN_POINT('Ctrl Pts',(-1.2990415308213,0.75000197750818,-7.61666438323691));
#363092=CARTESIAN_POINT('Ctrl Pts',(-1.73205537442839,1.7571777080019E-15,
-7.57499771657024));
#363093=CARTESIAN_POINT('Ctrl Pts',(-1.2990415308213,-0.750001977508177,
-7.53333104990358));
#363094=CARTESIAN_POINT('Ctrl Pts',(-0.866027687214197,-1.50000395501635,
-7.49166438323691));
#363095=CARTESIAN_POINT('Ctrl Pts',(-1.83697504221915E-16,-1.50000395501636,
-7.44999771657024));
#363096=CARTESIAN_POINT('Ctrl Pts',(0.866027687214196,-1.50000395501636,
-7.40833104990358));
#363097=CARTESIAN_POINT('Ctrl Pts',(1.29904153082129,-0.750001977508178,
-7.36666438323691));
#363098=CARTESIAN_POINT('Ctrl Pts',(1.73205537442839,1.22367257420739E-15,
-7.32499771657024));
#363099=CARTESIAN_POINT('Ctrl Pts',(1.2990415308213,0.750001977508179,-7.28333104990358));
#363100=CARTESIAN_POINT('Ctrl Pts',(0.866027687214198,1.50000395501636,
-7.24166438323691));
#363101=CARTESIAN_POINT('Ctrl Pts',(0.,1.50000395501636,-7.19999771657024));
#363102=CARTESIAN_POINT('Ctrl Pts',(-0.866027687214197,1.50000395501636,
-7.15833104990358));
#363103=CARTESIAN_POINT('Ctrl Pts',(-1.2990415308213,0.75000197750818,-7.11666438323691));
#363104=CARTESIAN_POINT('Ctrl Pts',(-1.73205537442839,1.53862986850876E-15,
-7.07499771657024));
#363105=CARTESIAN_POINT('Ctrl Pts',(-1.2990415308213,-0.750001977508177,
-7.03333104990358));
#363106=CARTESIAN_POINT('Ctrl Pts',(-0.866027687214197,-1.50000395501635,
-6.99166438323691));
#363107=CARTESIAN_POINT('Ctrl Pts',(-1.83697504221915E-16,-1.50000395501636,
-6.94999771657024));
#363108=CARTESIAN_POINT('Ctrl Pts',(0.866027687214196,-1.50000395501636,
-6.90833104990358));
#363109=CARTESIAN_POINT('Ctrl Pts',(1.29904153082129,-0.750001977508178,
-6.86666438323691));
#363110=CARTESIAN_POINT('Ctrl Pts',(1.73205537442839,1.00512473471425E-15,
-6.82499771657024));
#363111=CARTESIAN_POINT('Ctrl Pts',(1.2990415308213,0.750001977508179,-6.78333104990358));
#363112=CARTESIAN_POINT('Ctrl Pts',(0.866027687214198,1.50000395501636,
-6.74166438323691));
#363113=CARTESIAN_POINT('Ctrl Pts',(0.,1.50000395501636,-6.69999771657024));
#363114=CARTESIAN_POINT('Ctrl Pts',(-0.866027687214197,1.50000395501636,
-6.65833104990358));
#363115=CARTESIAN_POINT('Ctrl Pts',(-1.2990415308213,0.75000197750818,-6.61666438323691));
#363116=CARTESIAN_POINT('Ctrl Pts',(-1.73205537442839,1.32008202901562E-15,
-6.57499771657024));
#363117=CARTESIAN_POINT('Ctrl Pts',(-1.2990415308213,-0.750001977508177,
-6.53333104990357));
#363118=CARTESIAN_POINT('Ctrl Pts',(-0.866027687214197,-1.50000395501635,
-6.49166438323691));
#363119=CARTESIAN_POINT('Ctrl Pts',(-1.83697504221915E-16,-1.50000395501636,
-6.44999771657024));
#363120=CARTESIAN_POINT('Ctrl Pts',(0.866027687214196,-1.50000395501636,
-6.40833104990358));
#363121=CARTESIAN_POINT('Ctrl Pts',(1.29904153082129,-0.750001977508178,
-6.36666438323691));
#363122=CARTESIAN_POINT('Ctrl Pts',(1.73205537442839,7.86576895221109E-16,
-6.32499771657024));
#363123=CARTESIAN_POINT('Ctrl Pts',(1.2990415308213,0.750001977508178,-6.28333104990357));
#363124=CARTESIAN_POINT('Ctrl Pts',(0.866027687214198,1.50000395501636,
-6.24166438323691));
#363125=CARTESIAN_POINT('Ctrl Pts',(0.,1.50000395501636,-6.19999771657024));
#363126=CARTESIAN_POINT('Ctrl Pts',(-0.866027687214197,1.50000395501636,
-6.15833104990357));
#363127=CARTESIAN_POINT('Ctrl Pts',(-1.2990415308213,0.75000197750818,-6.11666438323691));
#363128=CARTESIAN_POINT('Ctrl Pts',(-1.73205537442839,1.10153418952248E-15,
-6.07499771657024));
#363129=CARTESIAN_POINT('Ctrl Pts',(-1.2990415308213,-0.750001977508177,
-6.03333104990357));
#363130=CARTESIAN_POINT('Ctrl Pts',(-0.866027687214197,-1.50000395501636,
-5.99166438323691));
#363131=CARTESIAN_POINT('Ctrl Pts',(-1.83697504221915E-16,-1.50000395501636,
-5.94999771657024));
#363132=CARTESIAN_POINT('Ctrl Pts',(0.866027687214196,-1.50000395501636,
-5.90833104990358));
#363133=CARTESIAN_POINT('Ctrl Pts',(1.29904153082129,-0.750001977508178,
-5.86666438323691));
#363134=CARTESIAN_POINT('Ctrl Pts',(1.73205537442839,5.68029055727967E-16,
-5.82499771657024));
#363135=CARTESIAN_POINT('Ctrl Pts',(1.2990415308213,0.750001977508178,-5.78333104990358));
#363136=CARTESIAN_POINT('Ctrl Pts',(0.866027687214198,1.50000395501636,
-5.74166438323691));
#363137=CARTESIAN_POINT('Ctrl Pts',(0.,1.50000395501636,-5.69999771657024));
#363138=CARTESIAN_POINT('Ctrl Pts',(-0.866027687214197,1.50000395501636,
-5.65833104990357));
#363139=CARTESIAN_POINT('Ctrl Pts',(-1.2990415308213,0.750001977508179,
-5.61666438323691));
#363140=CARTESIAN_POINT('Ctrl Pts',(-1.73205537442839,8.82986350029337E-16,
-5.57499771657024));
#363141=CARTESIAN_POINT('Ctrl Pts',(-1.2990415308213,-0.750001977508177,
-5.53333104990358));
#363142=CARTESIAN_POINT('Ctrl Pts',(-0.866027687214197,-1.50000395501636,
-5.49166438323691));
#363143=CARTESIAN_POINT('Ctrl Pts',(-1.83697504221915E-16,-1.50000395501636,
-5.44999771657024));
#363144=CARTESIAN_POINT('Ctrl Pts',(0.866027687214196,-1.50000395501636,
-5.40833104990357));
#363145=CARTESIAN_POINT('Ctrl Pts',(1.29904153082129,-0.750001977508178,
-5.36666438323691));
#363146=CARTESIAN_POINT('Ctrl Pts',(1.73205537442839,3.49481216234826E-16,
-5.32499771657024));
#363147=CARTESIAN_POINT('Ctrl Pts',(1.2990415308213,0.750001977508178,-5.28333104990358));
#363148=CARTESIAN_POINT('Ctrl Pts',(0.866027687214198,1.50000395501636,
-5.24166438323691));
#363149=CARTESIAN_POINT('Ctrl Pts',(0.,1.50000395501636,-5.19999771657024));
#363150=CARTESIAN_POINT('Ctrl Pts',(-0.866027687214197,1.50000395501636,
-5.15833104990357));
#363151=CARTESIAN_POINT('Ctrl Pts',(-1.2990415308213,0.750001977508179,
-5.11666438323691));
#363152=CARTESIAN_POINT('Ctrl Pts',(-1.73205537442839,6.64438510536197E-16,
-5.07499771657024));
#363153=CARTESIAN_POINT('Ctrl Pts',(-1.2990415308213,-0.750001977508178,
-5.03333104990357));
#363154=CARTESIAN_POINT('Ctrl Pts',(-0.866027687214197,-1.50000395501636,
-4.99166438323691));
#363155=CARTESIAN_POINT('Ctrl Pts',(-1.83697504221915E-16,-1.50000395501636,
-4.94999771657024));
#363156=CARTESIAN_POINT('Ctrl Pts',(0.866027687214196,-1.50000395501636,
-4.90833104990357));
#363157=CARTESIAN_POINT('Ctrl Pts',(1.29904153082129,-0.750001977508179,
-4.86666438323691));
#363158=CARTESIAN_POINT('Ctrl Pts',(1.73205537442839,1.30933376741685E-16,
-4.82499771657024));
#363159=CARTESIAN_POINT('Ctrl Pts',(1.2990415308213,0.750001977508178,-4.78333104990357));
#363160=CARTESIAN_POINT('Ctrl Pts',(0.866027687214198,1.50000395501636,
-4.74166438323691));
#363161=CARTESIAN_POINT('Ctrl Pts',(0.,1.50000395501636,-4.69999771657024));
#363162=CARTESIAN_POINT('Ctrl Pts',(-0.866027687214197,1.50000395501636,
-4.65833104990357));
#363163=CARTESIAN_POINT('Ctrl Pts',(-1.2990415308213,0.750001977508179,
-4.61666438323691));
#363164=CARTESIAN_POINT('Ctrl Pts',(-1.73205537442839,4.45890671043056E-16,
-4.57499771657024));
#363165=CARTESIAN_POINT('Ctrl Pts',(-1.2990415308213,-0.750001977508178,
-4.53333104990357));
#363166=CARTESIAN_POINT('Ctrl Pts',(-0.866027687214197,-1.50000395501636,
-4.49166438323691));
#363167=CARTESIAN_POINT('Ctrl Pts',(-1.83697504221915E-16,-1.50000395501636,
-4.44999771657024));
#363168=CARTESIAN_POINT('Ctrl Pts',(0.866027687214196,-1.50000395501636,
-4.40833104990357));
#363169=CARTESIAN_POINT('Ctrl Pts',(1.29904153082129,-0.750001977508179,
-4.36666438323691));
#363170=CARTESIAN_POINT('Ctrl Pts',(1.73205537442839,-8.76144627514565E-17,
-4.32499771657024));
#363171=CARTESIAN_POINT('Ctrl Pts',(1.2990415308213,0.750001977508178,-4.28333104990357));
#363172=CARTESIAN_POINT('Ctrl Pts',(0.866027687214198,1.50000395501636,
-4.24166438323691));
#363173=CARTESIAN_POINT('Ctrl Pts',(0.,1.50000395501636,-4.19999771657024));
#363174=CARTESIAN_POINT('Ctrl Pts',(-0.866027687214197,1.50000395501636,
-4.15833104990358));
#363175=CARTESIAN_POINT('Ctrl Pts',(-1.2990415308213,0.750001977508179,
-4.11666438323691));
#363176=CARTESIAN_POINT('Ctrl Pts',(-1.73205537442839,2.27342831549914E-16,
-4.07499771657024));
#363177=CARTESIAN_POINT('Ctrl Pts',(-1.2990415308213,-0.750001977508178,
-4.03333104990358));
#363178=CARTESIAN_POINT('Ctrl Pts',(-0.866027687214197,-1.50000395501636,
-3.99166438323691));
#363179=CARTESIAN_POINT('Ctrl Pts',(-1.83697504221915E-16,-1.50000395501636,
-3.94999771657024));
#363180=CARTESIAN_POINT('Ctrl Pts',(0.866027687214196,-1.50000395501636,
-3.90833104990358));
#363181=CARTESIAN_POINT('Ctrl Pts',(1.29904153082129,-0.750001977508179,
-3.86666438323691));
#363182=CARTESIAN_POINT('Ctrl Pts',(1.73205537442839,-3.06162302244598E-16,
-3.82499771657024));
#363183=CARTESIAN_POINT('Ctrl Pts',(1.2990415308213,0.750001977508177,-3.78333104990357));
#363184=CARTESIAN_POINT('Ctrl Pts',(0.866027687214198,1.50000395501636,
-3.74166438323691));
#363185=CARTESIAN_POINT('Ctrl Pts',(0.,1.50000395501636,-3.69999771657024));
#363186=CARTESIAN_POINT('Ctrl Pts',(-0.866027687214197,1.50000395501636,
-3.65833104990357));
#363187=CARTESIAN_POINT('Ctrl Pts',(-1.2990415308213,0.750001977508179,
-3.61666438323691));
#363188=CARTESIAN_POINT('Ctrl Pts',(-1.73205537442839,8.79499205677354E-18,
-3.57499771657024));
#363189=CARTESIAN_POINT('Ctrl Pts',(-1.2990415308213,-0.750001977508178,
-3.53333104990357));
#363190=CARTESIAN_POINT('Ctrl Pts',(-0.866027687214197,-1.50000395501636,
-3.49166438323691));
#363191=CARTESIAN_POINT('Ctrl Pts',(-1.83697504221915E-16,-1.50000395501636,
-3.44999771657024));
#363192=CARTESIAN_POINT('Ctrl Pts',(0.866027687214196,-1.50000395501636,
-3.40833104990357));
#363193=CARTESIAN_POINT('Ctrl Pts',(1.29904153082129,-0.750001977508179,
-3.36666438323691));
#363194=CARTESIAN_POINT('Ctrl Pts',(1.73205537442839,-5.24710141737739E-16,
-3.32499771657024));
#363195=CARTESIAN_POINT('Ctrl Pts',(1.2990415308213,0.750001977508177,-3.28333104990357));
#363196=CARTESIAN_POINT('Ctrl Pts',(0.866027687214198,1.50000395501636,
-3.24166438323691));
#363197=CARTESIAN_POINT('Ctrl Pts',(0.,1.50000395501636,-3.19999771657024));
#363198=CARTESIAN_POINT('Ctrl Pts',(-0.866027687214197,1.50000395501636,
-3.15833104990357));
#363199=CARTESIAN_POINT('Ctrl Pts',(-1.2990415308213,0.750001977508178,
-3.11666438323691));
#363200=CARTESIAN_POINT('Ctrl Pts',(-1.73205537442839,-2.09752847436368E-16,
-3.07499771657024));
#363201=CARTESIAN_POINT('Ctrl Pts',(-1.2990415308213,-0.750001977508178,
-3.03333104990357));
#363202=CARTESIAN_POINT('Ctrl Pts',(-0.866027687214197,-1.50000395501636,
-2.99166438323691));
#363203=CARTESIAN_POINT('Ctrl Pts',(-1.83697504221915E-16,-1.50000395501636,
-2.94999771657024));
#363204=CARTESIAN_POINT('Ctrl Pts',(0.866027687214196,-1.50000395501636,
-2.90833104990357));
#363205=CARTESIAN_POINT('Ctrl Pts',(1.29904153082129,-0.750001977508179,
-2.86666438323691));
#363206=CARTESIAN_POINT('Ctrl Pts',(1.73205537442839,-7.4325798123088E-16,
-2.82499771657024));
#363207=CARTESIAN_POINT('Ctrl Pts',(1.2990415308213,0.750001977508177,-2.78333104990357));
#363208=CARTESIAN_POINT('Ctrl Pts',(0.866027687214198,1.50000395501636,
-2.74166438323691));
#363209=CARTESIAN_POINT('Ctrl Pts',(0.,1.50000395501636,-2.69999771657024));
#363210=CARTESIAN_POINT('Ctrl Pts',(-0.866027687214197,1.50000395501636,
-2.65833104990357));
#363211=CARTESIAN_POINT('Ctrl Pts',(-1.2990415308213,0.750001977508178,
-2.61666438323691));
#363212=CARTESIAN_POINT('Ctrl Pts',(-1.73205537442839,-4.28300686929509E-16,
-2.57499771657024));
#363213=CARTESIAN_POINT('Ctrl Pts',(-1.2990415308213,-0.750001977508179,
-2.53333104990357));
#363214=CARTESIAN_POINT('Ctrl Pts',(-0.866027687214197,-1.50000395501636,
-2.49166438323691));
#363215=CARTESIAN_POINT('Ctrl Pts',(-1.83697504221915E-16,-1.50000395501636,
-2.44999771657024));
#363216=CARTESIAN_POINT('Ctrl Pts',(0.866027687214196,-1.50000395501636,
-2.40833104990357));
#363217=CARTESIAN_POINT('Ctrl Pts',(1.29904153082129,-0.75000197750818,
-2.36666438323691));
#363218=CARTESIAN_POINT('Ctrl Pts',(1.73205537442839,-9.61805820724022E-16,
-2.32499771657024));
#363219=CARTESIAN_POINT('Ctrl Pts',(1.2990415308213,0.750001977508177,-2.28333104990357));
#363220=CARTESIAN_POINT('Ctrl Pts',(0.866027687214198,1.50000395501636,
-2.24166438323691));
#363221=CARTESIAN_POINT('Ctrl Pts',(0.,1.50000395501636,-2.19999771657024));
#363222=CARTESIAN_POINT('Ctrl Pts',(-0.866027687214197,1.50000395501636,
-2.15833104990357));
#363223=CARTESIAN_POINT('Ctrl Pts',(-1.2990415308213,0.750001977508178,
-2.11666438323691));
#363224=CARTESIAN_POINT('Ctrl Pts',(-1.73205537442839,-6.46848526422651E-16,
-2.07499771657024));
#363225=CARTESIAN_POINT('Ctrl Pts',(-1.2990415308213,-0.750001977508179,
-2.03333104990357));
#363226=CARTESIAN_POINT('Ctrl Pts',(-0.866027687214197,-1.50000395501636,
-1.99166438323691));
#363227=CARTESIAN_POINT('Ctrl Pts',(-1.83697504221915E-16,-1.50000395501636,
-1.94999771657024));
#363228=CARTESIAN_POINT('Ctrl Pts',(0.866027687214196,-1.50000395501636,
-1.90833104990357));
#363229=CARTESIAN_POINT('Ctrl Pts',(1.29904153082129,-0.75000197750818,
-1.86666438323691));
#363230=CARTESIAN_POINT('Ctrl Pts',(1.73205537442839,-1.18035366021716E-15,
-1.82499771657024));
#363231=CARTESIAN_POINT('Ctrl Pts',(1.2990415308213,0.750001977508177,-1.78333104990357));
#363232=CARTESIAN_POINT('Ctrl Pts',(0.866027687214198,1.50000395501636,
-1.74166438323691));
#363233=CARTESIAN_POINT('Ctrl Pts',(0.,1.50000395501636,-1.69999771657024));
#363234=CARTESIAN_POINT('Ctrl Pts',(-0.866027687214197,1.50000395501636,
-1.65833104990357));
#363235=CARTESIAN_POINT('Ctrl Pts',(-1.2990415308213,0.750001977508178,
-1.61666438323691));
#363236=CARTESIAN_POINT('Ctrl Pts',(-1.73205537442839,-8.65396365915792E-16,
-1.57499771657024));
#363237=CARTESIAN_POINT('Ctrl Pts',(-1.2990415308213,-0.750001977508179,
-1.53333104990357));
#363238=CARTESIAN_POINT('Ctrl Pts',(-0.866027687214197,-1.50000395501636,
-1.49166438323691));
#363239=CARTESIAN_POINT('Ctrl Pts',(-1.83697504221915E-16,-1.50000395501636,
-1.44999771657024));
#363240=CARTESIAN_POINT('Ctrl Pts',(0.866027687214196,-1.50000395501636,
-1.40833104990357));
#363241=CARTESIAN_POINT('Ctrl Pts',(1.29904153082129,-0.75000197750818,
-1.36666438323691));
#363242=CARTESIAN_POINT('Ctrl Pts',(1.73205537442839,-1.3989014997103E-15,
-1.32499771657024));
#363243=CARTESIAN_POINT('Ctrl Pts',(1.2990415308213,0.750001977508176,-1.28333104990357));
#363244=CARTESIAN_POINT('Ctrl Pts',(0.866027687214198,1.50000395501635,
-1.24166438323691));
#363245=CARTESIAN_POINT('Ctrl Pts',(0.,1.50000395501636,-1.19999771657024));
#363246=CARTESIAN_POINT('Ctrl Pts',(0.,1.17524047358083,-17.8875));
#363247=CARTESIAN_POINT('Ctrl Pts',(-0.678525403784434,1.17524047358083,
-17.8458333333333));
#363248=CARTESIAN_POINT('Ctrl Pts',(-1.01778810567665,0.58762023679042,
-17.8041666666667));
#363249=CARTESIAN_POINT('Ctrl Pts',(-1.35705080756887,6.18712852862843E-15,
-17.7625));
#363250=CARTESIAN_POINT('Ctrl Pts',(-1.01778810567665,-0.587620236790408,
-17.7208333333333));
#363251=CARTESIAN_POINT('Ctrl Pts',(-0.678525403784435,-1.17524047358082,
-17.6791666666667));
#363252=CARTESIAN_POINT('Ctrl Pts',(-1.43925448419918E-16,-1.17524047358082,
-17.6375));
#363253=CARTESIAN_POINT('Ctrl Pts',(0.678525403784434,-1.17524047358082,
-17.5958333333333));
#363254=CARTESIAN_POINT('Ctrl Pts',(1.01778810567665,-0.587620236790409,
-17.5541666666667));
#363255=CARTESIAN_POINT('Ctrl Pts',(1.35705080756887,5.74547302332795E-15,
-17.5125));
#363256=CARTESIAN_POINT('Ctrl Pts',(1.01778810567665,0.587620236790419,
-17.4708333333333));
#363257=CARTESIAN_POINT('Ctrl Pts',(0.678525403784435,1.17524047358083,
-17.4291666666667));
#363258=CARTESIAN_POINT('Ctrl Pts',(0.,1.17524047358083,-17.3875));
#363259=CARTESIAN_POINT('Ctrl Pts',(-0.678525403784434,1.17524047358083,
-17.3458333333333));
#363260=CARTESIAN_POINT('Ctrl Pts',(-1.01778810567665,0.58762023679042,
-17.3041666666667));
#363261=CARTESIAN_POINT('Ctrl Pts',(-1.35705080756887,5.96858068913529E-15,
-17.2625));
#363262=CARTESIAN_POINT('Ctrl Pts',(-1.01778810567665,-0.587620236790408,
-17.2208333333333));
#363263=CARTESIAN_POINT('Ctrl Pts',(-0.678525403784435,-1.17524047358082,
-17.1791666666667));
#363264=CARTESIAN_POINT('Ctrl Pts',(-1.43925448419918E-16,-1.17524047358082,
-17.1375));
#363265=CARTESIAN_POINT('Ctrl Pts',(0.678525403784434,-1.17524047358082,
-17.0958333333333));
#363266=CARTESIAN_POINT('Ctrl Pts',(1.01778810567665,-0.587620236790409,
-17.0541666666667));
#363267=CARTESIAN_POINT('Ctrl Pts',(1.35705080756887,5.52692518383481E-15,
-17.0125));
#363268=CARTESIAN_POINT('Ctrl Pts',(1.01778810567665,0.587620236790419,
-16.9708333333333));
#363269=CARTESIAN_POINT('Ctrl Pts',(0.678525403784435,1.17524047358083,
-16.9291666666667));
#363270=CARTESIAN_POINT('Ctrl Pts',(0.,1.17524047358083,-16.8875));
#363271=CARTESIAN_POINT('Ctrl Pts',(-0.678525403784434,1.17524047358083,
-16.8458333333333));
#363272=CARTESIAN_POINT('Ctrl Pts',(-1.01778810567665,0.58762023679042,
-16.8041666666667));
#363273=CARTESIAN_POINT('Ctrl Pts',(-1.35705080756887,5.75003284964215E-15,
-16.7625));
#363274=CARTESIAN_POINT('Ctrl Pts',(-1.01778810567665,-0.587620236790408,
-16.7208333333333));
#363275=CARTESIAN_POINT('Ctrl Pts',(-0.678525403784435,-1.17524047358082,
-16.6791666666667));
#363276=CARTESIAN_POINT('Ctrl Pts',(-1.43925448419918E-16,-1.17524047358082,
-16.6375));
#363277=CARTESIAN_POINT('Ctrl Pts',(0.678525403784434,-1.17524047358082,
-16.5958333333333));
#363278=CARTESIAN_POINT('Ctrl Pts',(1.01778810567665,-0.587620236790409,
-16.5541666666667));
#363279=CARTESIAN_POINT('Ctrl Pts',(1.35705080756887,5.30837734434166E-15,
-16.5125));
#363280=CARTESIAN_POINT('Ctrl Pts',(1.01778810567665,0.587620236790419,
-16.4708333333333));
#363281=CARTESIAN_POINT('Ctrl Pts',(0.678525403784435,1.17524047358083,
-16.4291666666667));
#363282=CARTESIAN_POINT('Ctrl Pts',(0.,1.17524047358083,-16.3875));
#363283=CARTESIAN_POINT('Ctrl Pts',(-0.678525403784434,1.17524047358083,
-16.3458333333333));
#363284=CARTESIAN_POINT('Ctrl Pts',(-1.01778810567665,0.58762023679042,
-16.3041666666667));
#363285=CARTESIAN_POINT('Ctrl Pts',(-1.35705080756887,5.53148501014901E-15,
-16.2625));
#363286=CARTESIAN_POINT('Ctrl Pts',(-1.01778810567665,-0.587620236790409,
-16.2208333333333));
#363287=CARTESIAN_POINT('Ctrl Pts',(-0.678525403784435,-1.17524047358082,
-16.1791666666667));
#363288=CARTESIAN_POINT('Ctrl Pts',(-1.43925448419918E-16,-1.17524047358082,
-16.1375));
#363289=CARTESIAN_POINT('Ctrl Pts',(0.678525403784434,-1.17524047358082,
-16.0958333333333));
#363290=CARTESIAN_POINT('Ctrl Pts',(1.01778810567665,-0.587620236790409,
-16.0541666666667));
#363291=CARTESIAN_POINT('Ctrl Pts',(1.35705080756887,5.08982950484852E-15,
-16.0125));
#363292=CARTESIAN_POINT('Ctrl Pts',(1.01778810567665,0.587620236790419,
-15.9708333333333));
#363293=CARTESIAN_POINT('Ctrl Pts',(0.678525403784435,1.17524047358083,
-15.9291666666667));
#363294=CARTESIAN_POINT('Ctrl Pts',(0.,1.17524047358083,-15.8875));
#363295=CARTESIAN_POINT('Ctrl Pts',(-0.678525403784434,1.17524047358083,
-15.8458333333333));
#363296=CARTESIAN_POINT('Ctrl Pts',(-1.01778810567665,0.58762023679042,
-15.8041666666667));
#363297=CARTESIAN_POINT('Ctrl Pts',(-1.35705080756887,5.31293717065586E-15,
-15.7625));
#363298=CARTESIAN_POINT('Ctrl Pts',(-1.01778810567665,-0.587620236790409,
-15.7208333333333));
#363299=CARTESIAN_POINT('Ctrl Pts',(-0.678525403784435,-1.17524047358082,
-15.6791666666667));
#363300=CARTESIAN_POINT('Ctrl Pts',(-1.43925448419918E-16,-1.17524047358082,
-15.6375));
#363301=CARTESIAN_POINT('Ctrl Pts',(0.678525403784434,-1.17524047358082,
-15.5958333333333));
#363302=CARTESIAN_POINT('Ctrl Pts',(1.01778810567665,-0.58762023679041,
-15.5541666666667));
#363303=CARTESIAN_POINT('Ctrl Pts',(1.35705080756887,4.87128166535538E-15,
-15.5125));
#363304=CARTESIAN_POINT('Ctrl Pts',(1.01778810567665,0.587620236790418,
-15.4708333333333));
#363305=CARTESIAN_POINT('Ctrl Pts',(0.678525403784435,1.17524047358083,
-15.4291666666667));
#363306=CARTESIAN_POINT('Ctrl Pts',(0.,1.17524047358083,-15.3875));
#363307=CARTESIAN_POINT('Ctrl Pts',(-0.678525403784434,1.17524047358083,
-15.3458333333333));
#363308=CARTESIAN_POINT('Ctrl Pts',(-1.01778810567665,0.587620236790419,
-15.3041666666667));
#363309=CARTESIAN_POINT('Ctrl Pts',(-1.35705080756887,5.09438933116272E-15,
-15.2625));
#363310=CARTESIAN_POINT('Ctrl Pts',(-1.01778810567665,-0.587620236790409,
-15.2208333333333));
#363311=CARTESIAN_POINT('Ctrl Pts',(-0.678525403784435,-1.17524047358082,
-15.1791666666667));
#363312=CARTESIAN_POINT('Ctrl Pts',(-1.43925448419918E-16,-1.17524047358082,
-15.1375));
#363313=CARTESIAN_POINT('Ctrl Pts',(0.678525403784434,-1.17524047358082,
-15.0958333333333));
#363314=CARTESIAN_POINT('Ctrl Pts',(1.01778810567665,-0.58762023679041,
-15.0541666666667));
#363315=CARTESIAN_POINT('Ctrl Pts',(1.35705080756887,4.65273382586224E-15,
-15.0125));
#363316=CARTESIAN_POINT('Ctrl Pts',(1.01778810567665,0.587620236790418,
-14.9708333333333));
#363317=CARTESIAN_POINT('Ctrl Pts',(0.678525403784435,1.17524047358083,
-14.9291666666667));
#363318=CARTESIAN_POINT('Ctrl Pts',(0.,1.17524047358083,-14.8875));
#363319=CARTESIAN_POINT('Ctrl Pts',(-0.678525403784434,1.17524047358083,
-14.8458333333333));
#363320=CARTESIAN_POINT('Ctrl Pts',(-1.01778810567665,0.587620236790419,
-14.8041666666667));
#363321=CARTESIAN_POINT('Ctrl Pts',(-1.35705080756887,4.87584149166958E-15,
-14.7625));
#363322=CARTESIAN_POINT('Ctrl Pts',(-1.01778810567665,-0.587620236790409,
-14.7208333333333));
#363323=CARTESIAN_POINT('Ctrl Pts',(-0.678525403784435,-1.17524047358082,
-14.6791666666667));
#363324=CARTESIAN_POINT('Ctrl Pts',(-1.43925448419918E-16,-1.17524047358082,
-14.6375));
#363325=CARTESIAN_POINT('Ctrl Pts',(0.678525403784434,-1.17524047358082,
-14.5958333333333));
#363326=CARTESIAN_POINT('Ctrl Pts',(1.01778810567665,-0.58762023679041,
-14.5541666666667));
#363327=CARTESIAN_POINT('Ctrl Pts',(1.35705080756887,4.4341859863691E-15,
-14.5125));
#363328=CARTESIAN_POINT('Ctrl Pts',(1.01778810567665,0.587620236790418,
-14.4708333333333));
#363329=CARTESIAN_POINT('Ctrl Pts',(0.678525403784435,1.17524047358083,
-14.4291666666667));
#363330=CARTESIAN_POINT('Ctrl Pts',(0.,1.17524047358083,-14.3875));
#363331=CARTESIAN_POINT('Ctrl Pts',(-0.678525403784434,1.17524047358083,
-14.3458333333333));
#363332=CARTESIAN_POINT('Ctrl Pts',(-1.01778810567665,0.587620236790419,
-14.3041666666667));
#363333=CARTESIAN_POINT('Ctrl Pts',(-1.35705080756887,4.65729365217644E-15,
-14.2625));
#363334=CARTESIAN_POINT('Ctrl Pts',(-1.01778810567665,-0.587620236790409,
-14.2208333333333));
#363335=CARTESIAN_POINT('Ctrl Pts',(-0.678525403784435,-1.17524047358082,
-14.1791666666667));
#363336=CARTESIAN_POINT('Ctrl Pts',(-1.43925448419918E-16,-1.17524047358082,
-14.1375));
#363337=CARTESIAN_POINT('Ctrl Pts',(0.678525403784434,-1.17524047358082,
-14.0958333333333));
#363338=CARTESIAN_POINT('Ctrl Pts',(1.01778810567665,-0.58762023679041,
-14.0541666666667));
#363339=CARTESIAN_POINT('Ctrl Pts',(1.35705080756887,4.21563814687596E-15,
-14.0125));
#363340=CARTESIAN_POINT('Ctrl Pts',(1.01778810567665,0.587620236790418,
-13.9708333333333));
#363341=CARTESIAN_POINT('Ctrl Pts',(0.678525403784435,1.17524047358083,
-13.9291666666667));
#363342=CARTESIAN_POINT('Ctrl Pts',(0.,1.17524047358083,-13.8875));
#363343=CARTESIAN_POINT('Ctrl Pts',(-0.678525403784434,1.17524047358083,
-13.8458333333333));
#363344=CARTESIAN_POINT('Ctrl Pts',(-1.01778810567665,0.587620236790419,
-13.8041666666667));
#363345=CARTESIAN_POINT('Ctrl Pts',(-1.35705080756887,4.4387458126833E-15,
-13.7625));
#363346=CARTESIAN_POINT('Ctrl Pts',(-1.01778810567665,-0.58762023679041,
-13.7208333333333));
#363347=CARTESIAN_POINT('Ctrl Pts',(-0.678525403784435,-1.17524047358082,
-13.6791666666667));
#363348=CARTESIAN_POINT('Ctrl Pts',(-1.43925448419918E-16,-1.17524047358082,
-13.6375));
#363349=CARTESIAN_POINT('Ctrl Pts',(0.678525403784434,-1.17524047358082,
-13.5958333333333));
#363350=CARTESIAN_POINT('Ctrl Pts',(1.01778810567665,-0.58762023679041,
-13.5541666666667));
#363351=CARTESIAN_POINT('Ctrl Pts',(1.35705080756887,3.99709030738282E-15,
-13.5125));
#363352=CARTESIAN_POINT('Ctrl Pts',(1.01778810567665,0.587620236790418,
-13.4708333333333));
#363353=CARTESIAN_POINT('Ctrl Pts',(0.678525403784435,1.17524047358083,
-13.4291666666667));
#363354=CARTESIAN_POINT('Ctrl Pts',(0.,1.17524047358083,-13.3875));
#363355=CARTESIAN_POINT('Ctrl Pts',(-0.678525403784434,1.17524047358083,
-13.3458333333333));
#363356=CARTESIAN_POINT('Ctrl Pts',(-1.01778810567665,0.587620236790419,
-13.3041666666667));
#363357=CARTESIAN_POINT('Ctrl Pts',(-1.35705080756887,4.22019797319016E-15,
-13.2625));
#363358=CARTESIAN_POINT('Ctrl Pts',(-1.01778810567665,-0.58762023679041,
-13.2208333333333));
#363359=CARTESIAN_POINT('Ctrl Pts',(-0.678525403784435,-1.17524047358082,
-13.1791666666667));
#363360=CARTESIAN_POINT('Ctrl Pts',(-1.43925448419918E-16,-1.17524047358082,
-13.1375));
#363361=CARTESIAN_POINT('Ctrl Pts',(0.678525403784434,-1.17524047358082,
-13.0958333333333));
#363362=CARTESIAN_POINT('Ctrl Pts',(1.01778810567665,-0.587620236790411,
-13.0541666666667));
#363363=CARTESIAN_POINT('Ctrl Pts',(1.35705080756887,3.77854246788968E-15,
-13.0125));
#363364=CARTESIAN_POINT('Ctrl Pts',(1.01778810567665,0.587620236790417,
-12.9708333333333));
#363365=CARTESIAN_POINT('Ctrl Pts',(0.678525403784435,1.17524047358083,
-12.9291666666667));
#363366=CARTESIAN_POINT('Ctrl Pts',(0.,1.17524047358083,-12.8875));
#363367=CARTESIAN_POINT('Ctrl Pts',(-0.678525403784434,1.17524047358083,
-12.8458333333333));
#363368=CARTESIAN_POINT('Ctrl Pts',(-1.01778810567665,0.587620236790418,
-12.8041666666667));
#363369=CARTESIAN_POINT('Ctrl Pts',(-1.35705080756887,4.00165013369702E-15,
-12.7625));
#363370=CARTESIAN_POINT('Ctrl Pts',(-1.01778810567665,-0.58762023679041,
-12.7208333333333));
#363371=CARTESIAN_POINT('Ctrl Pts',(-0.678525403784435,-1.17524047358082,
-12.6791666666667));
#363372=CARTESIAN_POINT('Ctrl Pts',(-1.43925448419918E-16,-1.17524047358082,
-12.6375));
#363373=CARTESIAN_POINT('Ctrl Pts',(0.678525403784434,-1.17524047358083,
-12.5958333333333));
#363374=CARTESIAN_POINT('Ctrl Pts',(1.01778810567665,-0.587620236790411,
-12.5541666666667));
#363375=CARTESIAN_POINT('Ctrl Pts',(1.35705080756887,3.55999462839654E-15,
-12.5125));
#363376=CARTESIAN_POINT('Ctrl Pts',(1.01778810567665,0.587620236790417,
-12.4708333333333));
#363377=CARTESIAN_POINT('Ctrl Pts',(0.678525403784435,1.17524047358083,
-12.4291666666667));
#363378=CARTESIAN_POINT('Ctrl Pts',(0.,1.17524047358083,-12.3875));
#363379=CARTESIAN_POINT('Ctrl Pts',(-0.678525403784434,1.17524047358083,
-12.3458333333333));
#363380=CARTESIAN_POINT('Ctrl Pts',(-1.01778810567665,0.587620236790418,
-12.3041666666667));
#363381=CARTESIAN_POINT('Ctrl Pts',(-1.35705080756887,3.78310229420388E-15,
-12.2625));
#363382=CARTESIAN_POINT('Ctrl Pts',(-1.01778810567665,-0.58762023679041,
-12.2208333333333));
#363383=CARTESIAN_POINT('Ctrl Pts',(-0.678525403784435,-1.17524047358082,
-12.1791666666667));
#363384=CARTESIAN_POINT('Ctrl Pts',(-1.43925448419918E-16,-1.17524047358082,
-12.1375));
#363385=CARTESIAN_POINT('Ctrl Pts',(0.678525403784434,-1.17524047358083,
-12.0958333333333));
#363386=CARTESIAN_POINT('Ctrl Pts',(1.01778810567665,-0.587620236790411,
-12.0541666666667));
#363387=CARTESIAN_POINT('Ctrl Pts',(1.35705080756887,3.34144678890339E-15,
-12.0125));
#363388=CARTESIAN_POINT('Ctrl Pts',(1.01778810567665,0.587620236790417,
-11.9708333333333));
#363389=CARTESIAN_POINT('Ctrl Pts',(0.678525403784435,1.17524047358083,
-11.9291666666667));
#363390=CARTESIAN_POINT('Ctrl Pts',(0.,1.17524047358083,-11.8875));
#363391=CARTESIAN_POINT('Ctrl Pts',(-0.678525403784434,1.17524047358083,
-11.8458333333333));
#363392=CARTESIAN_POINT('Ctrl Pts',(-1.01778810567665,0.587620236790418,
-11.8041666666667));
#363393=CARTESIAN_POINT('Ctrl Pts',(-1.35705080756887,3.56455445471073E-15,
-11.7625));
#363394=CARTESIAN_POINT('Ctrl Pts',(-1.01778810567665,-0.587620236790411,
-11.7208333333333));
#363395=CARTESIAN_POINT('Ctrl Pts',(-0.678525403784435,-1.17524047358083,
-11.6791666666667));
#363396=CARTESIAN_POINT('Ctrl Pts',(-1.43925448419918E-16,-1.17524047358083,
-11.6375));
#363397=CARTESIAN_POINT('Ctrl Pts',(0.678525403784434,-1.17524047358083,
-11.5958333333333));
#363398=CARTESIAN_POINT('Ctrl Pts',(1.01778810567665,-0.587620236790411,
-11.5541666666667));
#363399=CARTESIAN_POINT('Ctrl Pts',(1.35705080756887,3.12289894941025E-15,
-11.5125));
#363400=CARTESIAN_POINT('Ctrl Pts',(1.01778810567665,0.587620236790417,
-11.4708333333333));
#363401=CARTESIAN_POINT('Ctrl Pts',(0.678525403784435,1.17524047358083,
-11.4291666666667));
#363402=CARTESIAN_POINT('Ctrl Pts',(0.,1.17524047358083,-11.3875));
#363403=CARTESIAN_POINT('Ctrl Pts',(-0.678525403784434,1.17524047358083,
-11.3458333333333));
#363404=CARTESIAN_POINT('Ctrl Pts',(-1.01778810567665,0.587620236790418,
-11.3041666666667));
#363405=CARTESIAN_POINT('Ctrl Pts',(-1.35705080756887,3.34600661521759E-15,
-11.2625));
#363406=CARTESIAN_POINT('Ctrl Pts',(-1.01778810567665,-0.587620236790411,
-11.2208333333333));
#363407=CARTESIAN_POINT('Ctrl Pts',(-0.678525403784435,-1.17524047358083,
-11.1791666666667));
#363408=CARTESIAN_POINT('Ctrl Pts',(-1.43925448419918E-16,-1.17524047358083,
-11.1375));
#363409=CARTESIAN_POINT('Ctrl Pts',(0.678525403784434,-1.17524047358083,
-11.0958333333333));
#363410=CARTESIAN_POINT('Ctrl Pts',(1.01778810567665,-0.587620236790412,
-11.0541666666667));
#363411=CARTESIAN_POINT('Ctrl Pts',(1.35705080756887,2.90435110991711E-15,
-11.0125));
#363412=CARTESIAN_POINT('Ctrl Pts',(1.01778810567665,0.587620236790416,
-10.9708333333333));
#363413=CARTESIAN_POINT('Ctrl Pts',(0.678525403784435,1.17524047358083,
-10.9291666666667));
#363414=CARTESIAN_POINT('Ctrl Pts',(0.,1.17524047358083,-10.8875));
#363415=CARTESIAN_POINT('Ctrl Pts',(-0.678525403784434,1.17524047358083,
-10.8458333333333));
#363416=CARTESIAN_POINT('Ctrl Pts',(-1.01778810567665,0.587620236790417,
-10.8041666666667));
#363417=CARTESIAN_POINT('Ctrl Pts',(-1.35705080756887,3.12745877572445E-15,
-10.7625));
#363418=CARTESIAN_POINT('Ctrl Pts',(-1.01778810567665,-0.587620236790411,
-10.7208333333333));
#363419=CARTESIAN_POINT('Ctrl Pts',(-0.678525403784435,-1.17524047358083,
-10.6791666666667));
#363420=CARTESIAN_POINT('Ctrl Pts',(-1.43925448419918E-16,-1.17524047358083,
-10.6375));
#363421=CARTESIAN_POINT('Ctrl Pts',(0.678525403784434,-1.17524047358083,
-10.5958333333333));
#363422=CARTESIAN_POINT('Ctrl Pts',(1.01778810567665,-0.587620236790412,
-10.5541666666667));
#363423=CARTESIAN_POINT('Ctrl Pts',(1.35705080756887,2.68580327042397E-15,
-10.5125));
#363424=CARTESIAN_POINT('Ctrl Pts',(1.01778810567665,0.587620236790416,
-10.4708333333333));
#363425=CARTESIAN_POINT('Ctrl Pts',(0.678525403784435,1.17524047358083,
-10.4291666666667));
#363426=CARTESIAN_POINT('Ctrl Pts',(0.,1.17524047358083,-10.3875));
#363427=CARTESIAN_POINT('Ctrl Pts',(-0.678525403784434,1.17524047358083,
-10.3458333333333));
#363428=CARTESIAN_POINT('Ctrl Pts',(-1.01778810567665,0.587620236790417,
-10.3041666666667));
#363429=CARTESIAN_POINT('Ctrl Pts',(-1.35705080756887,2.90891093623131E-15,
-10.2625));
#363430=CARTESIAN_POINT('Ctrl Pts',(-1.01778810567665,-0.587620236790411,
-10.2208333333333));
#363431=CARTESIAN_POINT('Ctrl Pts',(-0.678525403784435,-1.17524047358083,
-10.1791666666667));
#363432=CARTESIAN_POINT('Ctrl Pts',(-1.43925448419918E-16,-1.17524047358083,
-10.1375));
#363433=CARTESIAN_POINT('Ctrl Pts',(0.678525403784434,-1.17524047358083,
-10.0958333333333));
#363434=CARTESIAN_POINT('Ctrl Pts',(1.01778810567665,-0.587620236790412,
-10.0541666666667));
#363435=CARTESIAN_POINT('Ctrl Pts',(1.35705080756887,2.46725543093083E-15,
-10.0125));
#363436=CARTESIAN_POINT('Ctrl Pts',(1.01778810567665,0.587620236790416,
-9.97083333333333));
#363437=CARTESIAN_POINT('Ctrl Pts',(0.678525403784435,1.17524047358083,
-9.92916666666667));
#363438=CARTESIAN_POINT('Ctrl Pts',(0.,1.17524047358083,-9.8875));
#363439=CARTESIAN_POINT('Ctrl Pts',(-0.678525403784434,1.17524047358083,
-9.84583333333333));
#363440=CARTESIAN_POINT('Ctrl Pts',(-1.01778810567665,0.587620236790417,
-9.80416666666667));
#363441=CARTESIAN_POINT('Ctrl Pts',(-1.35705080756887,2.69036309673817E-15,
-9.7625));
#363442=CARTESIAN_POINT('Ctrl Pts',(-1.01778810567665,-0.587620236790411,
-9.72083333333333));
#363443=CARTESIAN_POINT('Ctrl Pts',(-0.678525403784435,-1.17524047358083,
-9.67916666666667));
#363444=CARTESIAN_POINT('Ctrl Pts',(-1.43925448419918E-16,-1.17524047358083,
-9.6375));
#363445=CARTESIAN_POINT('Ctrl Pts',(0.678525403784434,-1.17524047358083,
-9.59583333333333));
#363446=CARTESIAN_POINT('Ctrl Pts',(1.01778810567665,-0.587620236790412,
-9.55416666666667));
#363447=CARTESIAN_POINT('Ctrl Pts',(1.35705080756887,2.24870759143769E-15,
-9.5125));
#363448=CARTESIAN_POINT('Ctrl Pts',(1.01778810567665,0.587620236790416,
-9.47083333333333));
#363449=CARTESIAN_POINT('Ctrl Pts',(0.678525403784435,1.17524047358083,
-9.42916666666667));
#363450=CARTESIAN_POINT('Ctrl Pts',(0.,1.17524047358083,-9.3875));
#363451=CARTESIAN_POINT('Ctrl Pts',(-0.678525403784434,1.17524047358083,
-9.34583333333333));
#363452=CARTESIAN_POINT('Ctrl Pts',(-1.01778810567665,0.587620236790417,
-9.30416666666667));
#363453=CARTESIAN_POINT('Ctrl Pts',(-1.35705080756887,2.47181525724503E-15,
-9.2625));
#363454=CARTESIAN_POINT('Ctrl Pts',(-1.01778810567665,-0.587620236790412,
-9.22083333333333));
#363455=CARTESIAN_POINT('Ctrl Pts',(-0.678525403784435,-1.17524047358083,
-9.17916666666667));
#363456=CARTESIAN_POINT('Ctrl Pts',(-1.43925448419918E-16,-1.17524047358083,
-9.1375));
#363457=CARTESIAN_POINT('Ctrl Pts',(0.678525403784434,-1.17524047358083,
-9.09583333333333));
#363458=CARTESIAN_POINT('Ctrl Pts',(1.01778810567665,-0.587620236790412,
-9.05416666666667));
#363459=CARTESIAN_POINT('Ctrl Pts',(1.35705080756887,2.03015975194455E-15,
-9.0125));
#363460=CARTESIAN_POINT('Ctrl Pts',(1.01778810567665,0.587620236790416,
-8.97083333333333));
#363461=CARTESIAN_POINT('Ctrl Pts',(0.678525403784435,1.17524047358083,
-8.92916666666667));
#363462=CARTESIAN_POINT('Ctrl Pts',(0.,1.17524047358083,-8.8875));
#363463=CARTESIAN_POINT('Ctrl Pts',(-0.678525403784434,1.17524047358083,
-8.84583333333333));
#363464=CARTESIAN_POINT('Ctrl Pts',(-1.01778810567665,0.587620236790416,
-8.80416666666667));
#363465=CARTESIAN_POINT('Ctrl Pts',(-1.35705080756887,2.25326741775189E-15,
-8.7625));
#363466=CARTESIAN_POINT('Ctrl Pts',(-1.01778810567665,-0.587620236790412,
-8.72083333333333));
#363467=CARTESIAN_POINT('Ctrl Pts',(-0.678525403784435,-1.17524047358083,
-8.67916666666667));
#363468=CARTESIAN_POINT('Ctrl Pts',(-1.43925448419918E-16,-1.17524047358083,
-8.6375));
#363469=CARTESIAN_POINT('Ctrl Pts',(0.678525403784434,-1.17524047358083,
-8.59583333333333));
#363470=CARTESIAN_POINT('Ctrl Pts',(1.01778810567665,-0.587620236790413,
-8.55416666666667));
#363471=CARTESIAN_POINT('Ctrl Pts',(1.35705080756887,1.81161191245141E-15,
-8.5125));
#363472=CARTESIAN_POINT('Ctrl Pts',(1.01778810567665,0.587620236790415,
-8.47083333333333));
#363473=CARTESIAN_POINT('Ctrl Pts',(0.678525403784435,1.17524047358083,
-8.42916666666667));
#363474=CARTESIAN_POINT('Ctrl Pts',(0.,1.17524047358083,-8.3875));
#363475=CARTESIAN_POINT('Ctrl Pts',(-0.678525403784434,1.17524047358083,
-8.34583333333333));
#363476=CARTESIAN_POINT('Ctrl Pts',(-1.01778810567665,0.587620236790416,
-8.30416666666667));
#363477=CARTESIAN_POINT('Ctrl Pts',(-1.35705080756887,2.03471957825875E-15,
-8.2625));
#363478=CARTESIAN_POINT('Ctrl Pts',(-1.01778810567665,-0.587620236790412,
-8.22083333333333));
#363479=CARTESIAN_POINT('Ctrl Pts',(-0.678525403784435,-1.17524047358083,
-8.17916666666667));
#363480=CARTESIAN_POINT('Ctrl Pts',(-1.43925448419918E-16,-1.17524047358083,
-8.1375));
#363481=CARTESIAN_POINT('Ctrl Pts',(0.678525403784434,-1.17524047358083,
-8.09583333333333));
#363482=CARTESIAN_POINT('Ctrl Pts',(1.01778810567665,-0.587620236790413,
-8.05416666666667));
#363483=CARTESIAN_POINT('Ctrl Pts',(1.35705080756887,1.59306407295827E-15,
-8.0125));
#363484=CARTESIAN_POINT('Ctrl Pts',(1.01778810567665,0.587620236790415,
-7.97083333333334));
#363485=CARTESIAN_POINT('Ctrl Pts',(0.678525403784435,1.17524047358083,
-7.92916666666667));
#363486=CARTESIAN_POINT('Ctrl Pts',(0.,1.17524047358083,-7.8875));
#363487=CARTESIAN_POINT('Ctrl Pts',(-0.678525403784434,1.17524047358083,
-7.84583333333333));
#363488=CARTESIAN_POINT('Ctrl Pts',(-1.01778810567665,0.587620236790416,
-7.80416666666667));
#363489=CARTESIAN_POINT('Ctrl Pts',(-1.35705080756887,1.8161717387656E-15,
-7.7625));
#363490=CARTESIAN_POINT('Ctrl Pts',(-1.01778810567665,-0.587620236790412,
-7.72083333333334));
#363491=CARTESIAN_POINT('Ctrl Pts',(-0.678525403784435,-1.17524047358083,
-7.67916666666667));
#363492=CARTESIAN_POINT('Ctrl Pts',(-1.43925448419918E-16,-1.17524047358083,
-7.6375));
#363493=CARTESIAN_POINT('Ctrl Pts',(0.678525403784434,-1.17524047358083,
-7.59583333333333));
#363494=CARTESIAN_POINT('Ctrl Pts',(1.01778810567665,-0.587620236790413,
-7.55416666666667));
#363495=CARTESIAN_POINT('Ctrl Pts',(1.35705080756887,1.37451623346513E-15,
-7.5125));
#363496=CARTESIAN_POINT('Ctrl Pts',(1.01778810567665,0.587620236790415,
-7.47083333333333));
#363497=CARTESIAN_POINT('Ctrl Pts',(0.678525403784435,1.17524047358083,
-7.42916666666667));
#363498=CARTESIAN_POINT('Ctrl Pts',(0.,1.17524047358083,-7.3875));
#363499=CARTESIAN_POINT('Ctrl Pts',(-0.678525403784434,1.17524047358083,
-7.34583333333334));
#363500=CARTESIAN_POINT('Ctrl Pts',(-1.01778810567665,0.587620236790416,
-7.30416666666667));
#363501=CARTESIAN_POINT('Ctrl Pts',(-1.35705080756887,1.59762389927246E-15,
-7.2625));
#363502=CARTESIAN_POINT('Ctrl Pts',(-1.01778810567665,-0.587620236790412,
-7.22083333333333));
#363503=CARTESIAN_POINT('Ctrl Pts',(-0.678525403784435,-1.17524047358083,
-7.17916666666667));
#363504=CARTESIAN_POINT('Ctrl Pts',(-1.43925448419918E-16,-1.17524047358083,
-7.1375));
#363505=CARTESIAN_POINT('Ctrl Pts',(0.678525403784434,-1.17524047358083,
-7.09583333333333));
#363506=CARTESIAN_POINT('Ctrl Pts',(1.01778810567665,-0.587620236790413,
-7.05416666666667));
#363507=CARTESIAN_POINT('Ctrl Pts',(1.35705080756887,1.15596839397198E-15,
-7.0125));
#363508=CARTESIAN_POINT('Ctrl Pts',(1.01778810567665,0.587620236790415,
-6.97083333333333));
#363509=CARTESIAN_POINT('Ctrl Pts',(0.678525403784435,1.17524047358083,
-6.92916666666667));
#363510=CARTESIAN_POINT('Ctrl Pts',(0.,1.17524047358083,-6.8875));
#363511=CARTESIAN_POINT('Ctrl Pts',(-0.678525403784434,1.17524047358083,
-6.84583333333333));
#363512=CARTESIAN_POINT('Ctrl Pts',(-1.01778810567665,0.587620236790416,
-6.80416666666667));
#363513=CARTESIAN_POINT('Ctrl Pts',(-1.35705080756887,1.37907605977932E-15,
-6.7625));
#363514=CARTESIAN_POINT('Ctrl Pts',(-1.01778810567665,-0.587620236790413,
-6.72083333333333));
#363515=CARTESIAN_POINT('Ctrl Pts',(-0.678525403784435,-1.17524047358083,
-6.67916666666667));
#363516=CARTESIAN_POINT('Ctrl Pts',(-1.43925448419918E-16,-1.17524047358083,
-6.6375));
#363517=CARTESIAN_POINT('Ctrl Pts',(0.678525403784434,-1.17524047358083,
-6.59583333333333));
#363518=CARTESIAN_POINT('Ctrl Pts',(1.01778810567665,-0.587620236790414,
-6.55416666666667));
#363519=CARTESIAN_POINT('Ctrl Pts',(1.35705080756887,9.37420554478842E-16,
-6.5125));
#363520=CARTESIAN_POINT('Ctrl Pts',(1.01778810567665,0.587620236790415,
-6.47083333333333));
#363521=CARTESIAN_POINT('Ctrl Pts',(0.678525403784435,1.17524047358083,
-6.42916666666667));
#363522=CARTESIAN_POINT('Ctrl Pts',(0.,1.17524047358083,-6.3875));
#363523=CARTESIAN_POINT('Ctrl Pts',(-0.678525403784434,1.17524047358083,
-6.34583333333333));
#363524=CARTESIAN_POINT('Ctrl Pts',(-1.01778810567665,0.587620236790415,
-6.30416666666667));
#363525=CARTESIAN_POINT('Ctrl Pts',(-1.35705080756887,1.16052822028618E-15,
-6.2625));
#363526=CARTESIAN_POINT('Ctrl Pts',(-1.01778810567665,-0.587620236790413,
-6.22083333333333));
#363527=CARTESIAN_POINT('Ctrl Pts',(-0.678525403784435,-1.17524047358083,
-6.17916666666667));
#363528=CARTESIAN_POINT('Ctrl Pts',(-1.43925448419918E-16,-1.17524047358083,
-6.1375));
#363529=CARTESIAN_POINT('Ctrl Pts',(0.678525403784434,-1.17524047358083,
-6.09583333333334));
#363530=CARTESIAN_POINT('Ctrl Pts',(1.01778810567665,-0.587620236790414,
-6.05416666666667));
#363531=CARTESIAN_POINT('Ctrl Pts',(1.35705080756887,7.18872714985701E-16,
-6.0125));
#363532=CARTESIAN_POINT('Ctrl Pts',(1.01778810567665,0.587620236790414,
-5.97083333333333));
#363533=CARTESIAN_POINT('Ctrl Pts',(0.678525403784435,1.17524047358083,
-5.92916666666667));
#363534=CARTESIAN_POINT('Ctrl Pts',(0.,1.17524047358083,-5.8875));
#363535=CARTESIAN_POINT('Ctrl Pts',(-0.678525403784434,1.17524047358083,
-5.84583333333334));
#363536=CARTESIAN_POINT('Ctrl Pts',(-1.01778810567665,0.587620236790415,
-5.80416666666667));
#363537=CARTESIAN_POINT('Ctrl Pts',(-1.35705080756887,9.41980380793039E-16,
-5.7625));
#363538=CARTESIAN_POINT('Ctrl Pts',(-1.01778810567665,-0.587620236790413,
-5.72083333333333));
#363539=CARTESIAN_POINT('Ctrl Pts',(-0.678525403784435,-1.17524047358083,
-5.67916666666667));
#363540=CARTESIAN_POINT('Ctrl Pts',(-1.43925448419918E-16,-1.17524047358083,
-5.6375));
#363541=CARTESIAN_POINT('Ctrl Pts',(0.678525403784434,-1.17524047358083,
-5.59583333333333));
#363542=CARTESIAN_POINT('Ctrl Pts',(1.01778810567665,-0.587620236790414,
-5.55416666666667));
#363543=CARTESIAN_POINT('Ctrl Pts',(1.35705080756887,5.0032487549256E-16,
-5.5125));
#363544=CARTESIAN_POINT('Ctrl Pts',(1.01778810567665,0.587620236790414,
-5.47083333333333));
#363545=CARTESIAN_POINT('Ctrl Pts',(0.678525403784435,1.17524047358083,
-5.42916666666667));
#363546=CARTESIAN_POINT('Ctrl Pts',(0.,1.17524047358083,-5.3875));
#363547=CARTESIAN_POINT('Ctrl Pts',(-0.678525403784434,1.17524047358083,
-5.34583333333333));
#363548=CARTESIAN_POINT('Ctrl Pts',(-1.01778810567665,0.587620236790415,
-5.30416666666667));
#363549=CARTESIAN_POINT('Ctrl Pts',(-1.35705080756887,7.23432541299899E-16,
-5.2625));
#363550=CARTESIAN_POINT('Ctrl Pts',(-1.01778810567665,-0.587620236790413,
-5.22083333333333));
#363551=CARTESIAN_POINT('Ctrl Pts',(-0.678525403784435,-1.17524047358083,
-5.17916666666667));
#363552=CARTESIAN_POINT('Ctrl Pts',(-1.43925448419918E-16,-1.17524047358083,
-5.1375));
#363553=CARTESIAN_POINT('Ctrl Pts',(0.678525403784434,-1.17524047358083,
-5.09583333333333));
#363554=CARTESIAN_POINT('Ctrl Pts',(1.01778810567665,-0.587620236790414,
-5.05416666666667));
#363555=CARTESIAN_POINT('Ctrl Pts',(1.35705080756887,2.81777035999419E-16,
-5.0125));
#363556=CARTESIAN_POINT('Ctrl Pts',(1.01778810567665,0.587620236790414,
-4.97083333333333));
#363557=CARTESIAN_POINT('Ctrl Pts',(0.678525403784435,1.17524047358083,
-4.92916666666667));
#363558=CARTESIAN_POINT('Ctrl Pts',(0.,1.17524047358083,-4.8875));
#363559=CARTESIAN_POINT('Ctrl Pts',(-0.678525403784434,1.17524047358083,
-4.84583333333333));
#363560=CARTESIAN_POINT('Ctrl Pts',(-1.01778810567665,0.587620236790415,
-4.80416666666667));
#363561=CARTESIAN_POINT('Ctrl Pts',(-1.35705080756887,5.04884701806757E-16,
-4.7625));
#363562=CARTESIAN_POINT('Ctrl Pts',(-1.01778810567665,-0.587620236790414,
-4.72083333333333));
#363563=CARTESIAN_POINT('Ctrl Pts',(-0.678525403784435,-1.17524047358083,
-4.67916666666667));
#363564=CARTESIAN_POINT('Ctrl Pts',(-1.43925448419918E-16,-1.17524047358083,
-4.6375));
#363565=CARTESIAN_POINT('Ctrl Pts',(0.678525403784434,-1.17524047358083,
-4.59583333333333));
#363566=CARTESIAN_POINT('Ctrl Pts',(1.01778810567665,-0.587620236790414,
-4.55416666666667));
#363567=CARTESIAN_POINT('Ctrl Pts',(1.35705080756887,6.32291965062771E-17,
-4.5125));
#363568=CARTESIAN_POINT('Ctrl Pts',(1.01778810567665,0.587620236790414,
-4.47083333333333));
#363569=CARTESIAN_POINT('Ctrl Pts',(0.678525403784435,1.17524047358083,
-4.42916666666667));
#363570=CARTESIAN_POINT('Ctrl Pts',(0.,1.17524047358083,-4.3875));
#363571=CARTESIAN_POINT('Ctrl Pts',(-0.678525403784434,1.17524047358083,
-4.34583333333333));
#363572=CARTESIAN_POINT('Ctrl Pts',(-1.01778810567665,0.587620236790415,
-4.30416666666667));
#363573=CARTESIAN_POINT('Ctrl Pts',(-1.35705080756887,2.86336862313616E-16,
-4.2625));
#363574=CARTESIAN_POINT('Ctrl Pts',(-1.01778810567665,-0.587620236790414,
-4.22083333333333));
#363575=CARTESIAN_POINT('Ctrl Pts',(-0.678525403784435,-1.17524047358083,
-4.17916666666667));
#363576=CARTESIAN_POINT('Ctrl Pts',(-1.43925448419918E-16,-1.17524047358083,
-4.1375));
#363577=CARTESIAN_POINT('Ctrl Pts',(0.678525403784434,-1.17524047358083,
-4.09583333333333));
#363578=CARTESIAN_POINT('Ctrl Pts',(1.01778810567665,-0.587620236790415,
-4.05416666666667));
#363579=CARTESIAN_POINT('Ctrl Pts',(1.35705080756887,-1.55318642986864E-16,
-4.0125));
#363580=CARTESIAN_POINT('Ctrl Pts',(1.01778810567665,0.587620236790414,
-3.97083333333333));
#363581=CARTESIAN_POINT('Ctrl Pts',(0.678525403784435,1.17524047358083,
-3.92916666666667));
#363582=CARTESIAN_POINT('Ctrl Pts',(0.,1.17524047358083,-3.8875));
#363583=CARTESIAN_POINT('Ctrl Pts',(-0.678525403784434,1.17524047358083,
-3.84583333333333));
#363584=CARTESIAN_POINT('Ctrl Pts',(-1.01778810567665,0.587620236790414,
-3.80416666666667));
#363585=CARTESIAN_POINT('Ctrl Pts',(-1.35705080756887,6.77890228204754E-17,
-3.7625));
#363586=CARTESIAN_POINT('Ctrl Pts',(-1.01778810567665,-0.587620236790414,
-3.72083333333333));
#363587=CARTESIAN_POINT('Ctrl Pts',(-0.678525403784435,-1.17524047358083,
-3.67916666666667));
#363588=CARTESIAN_POINT('Ctrl Pts',(-1.43925448419918E-16,-1.17524047358083,
-3.6375));
#363589=CARTESIAN_POINT('Ctrl Pts',(0.678525403784434,-1.17524047358083,
-3.59583333333333));
#363590=CARTESIAN_POINT('Ctrl Pts',(1.01778810567665,-0.587620236790415,
-3.55416666666667));
#363591=CARTESIAN_POINT('Ctrl Pts',(1.35705080756887,-3.73866482480005E-16,
-3.5125));
#363592=CARTESIAN_POINT('Ctrl Pts',(1.01778810567665,0.587620236790413,
-3.47083333333333));
#363593=CARTESIAN_POINT('Ctrl Pts',(0.678525403784435,1.17524047358083,
-3.42916666666667));
#363594=CARTESIAN_POINT('Ctrl Pts',(0.,1.17524047358083,-3.3875));
#363595=CARTESIAN_POINT('Ctrl Pts',(-0.678525403784434,1.17524047358083,
-3.34583333333333));
#363596=CARTESIAN_POINT('Ctrl Pts',(-1.01778810567665,0.587620236790414,
-3.30416666666667));
#363597=CARTESIAN_POINT('Ctrl Pts',(-1.35705080756887,-1.50758816672666E-16,
-3.2625));
#363598=CARTESIAN_POINT('Ctrl Pts',(-1.01778810567665,-0.587620236790414,
-3.22083333333333));
#363599=CARTESIAN_POINT('Ctrl Pts',(-0.678525403784435,-1.17524047358083,
-3.17916666666667));
#363600=CARTESIAN_POINT('Ctrl Pts',(-1.43925448419918E-16,-1.17524047358083,
-3.1375));
#363601=CARTESIAN_POINT('Ctrl Pts',(0.678525403784434,-1.17524047358083,
-3.09583333333333));
#363602=CARTESIAN_POINT('Ctrl Pts',(1.01778810567665,-0.587620236790415,
-3.05416666666667));
#363603=CARTESIAN_POINT('Ctrl Pts',(1.35705080756887,-5.92414321973146E-16,
-3.0125));
#363604=CARTESIAN_POINT('Ctrl Pts',(1.01778810567665,0.587620236790413,
-2.97083333333333));
#363605=CARTESIAN_POINT('Ctrl Pts',(0.678525403784435,1.17524047358083,
-2.92916666666667));
#363606=CARTESIAN_POINT('Ctrl Pts',(0.,1.17524047358083,-2.8875));
#363607=CARTESIAN_POINT('Ctrl Pts',(-0.678525403784434,1.17524047358083,
-2.84583333333333));
#363608=CARTESIAN_POINT('Ctrl Pts',(-1.01778810567665,0.587620236790414,
-2.80416666666667));
#363609=CARTESIAN_POINT('Ctrl Pts',(-1.35705080756887,-3.69306656165808E-16,
-2.7625));
#363610=CARTESIAN_POINT('Ctrl Pts',(-1.01778810567665,-0.587620236790414,
-2.72083333333333));
#363611=CARTESIAN_POINT('Ctrl Pts',(-0.678525403784435,-1.17524047358083,
-2.67916666666667));
#363612=CARTESIAN_POINT('Ctrl Pts',(-1.43925448419918E-16,-1.17524047358083,
-2.6375));
#363613=CARTESIAN_POINT('Ctrl Pts',(0.678525403784434,-1.17524047358083,
-2.59583333333333));
#363614=CARTESIAN_POINT('Ctrl Pts',(1.01778810567665,-0.587620236790415,
-2.55416666666667));
#363615=CARTESIAN_POINT('Ctrl Pts',(1.35705080756887,-8.10962161466288E-16,
-2.5125));
#363616=CARTESIAN_POINT('Ctrl Pts',(1.01778810567665,0.587620236790413,
-2.47083333333334));
#363617=CARTESIAN_POINT('Ctrl Pts',(0.678525403784435,1.17524047358083,
-2.42916666666667));
#363618=CARTESIAN_POINT('Ctrl Pts',(0.,1.17524047358083,-2.3875));
#363619=CARTESIAN_POINT('Ctrl Pts',(-0.678525403784434,1.17524047358083,
-2.34583333333334));
#363620=CARTESIAN_POINT('Ctrl Pts',(-1.01778810567665,0.587620236790414,
-2.30416666666667));
#363621=CARTESIAN_POINT('Ctrl Pts',(-1.35705080756887,-5.87854495658949E-16,
-2.2625));
#363622=CARTESIAN_POINT('Ctrl Pts',(-1.01778810567665,-0.587620236790415,
-2.22083333333333));
#363623=CARTESIAN_POINT('Ctrl Pts',(-0.678525403784435,-1.17524047358083,
-2.17916666666667));
#363624=CARTESIAN_POINT('Ctrl Pts',(-1.43925448419918E-16,-1.17524047358083,
-2.1375));
#363625=CARTESIAN_POINT('Ctrl Pts',(0.678525403784434,-1.17524047358083,
-2.09583333333333));
#363626=CARTESIAN_POINT('Ctrl Pts',(1.01778810567665,-0.587620236790415,
-2.05416666666667));
#363627=CARTESIAN_POINT('Ctrl Pts',(1.35705080756887,-1.02951000095943E-15,
-2.0125));
#363628=CARTESIAN_POINT('Ctrl Pts',(1.01778810567665,0.587620236790413,
-1.97083333333333));
#363629=CARTESIAN_POINT('Ctrl Pts',(0.678525403784435,1.17524047358083,
-1.92916666666667));
#363630=CARTESIAN_POINT('Ctrl Pts',(0.,1.17524047358083,-1.8875));
#363631=CARTESIAN_POINT('Ctrl Pts',(-0.678525403784434,1.17524047358083,
-1.84583333333334));
#363632=CARTESIAN_POINT('Ctrl Pts',(-1.01778810567665,0.587620236790414,
-1.80416666666667));
#363633=CARTESIAN_POINT('Ctrl Pts',(-1.35705080756887,-8.0640233515209E-16,
-1.7625));
#363634=CARTESIAN_POINT('Ctrl Pts',(-1.01778810567665,-0.587620236790415,
-1.72083333333333));
#363635=CARTESIAN_POINT('Ctrl Pts',(-0.678525403784435,-1.17524047358083,
-1.67916666666667));
#363636=CARTESIAN_POINT('Ctrl Pts',(-1.43925448419918E-16,-1.17524047358083,
-1.6375));
#363637=CARTESIAN_POINT('Ctrl Pts',(0.678525403784434,-1.17524047358083,
-1.59583333333333));
#363638=CARTESIAN_POINT('Ctrl Pts',(1.01778810567665,-0.587620236790416,
-1.55416666666667));
#363639=CARTESIAN_POINT('Ctrl Pts',(1.35705080756887,-1.24805784045257E-15,
-1.5125));
#363640=CARTESIAN_POINT('Ctrl Pts',(1.01778810567665,0.587620236790412,
-1.47083333333333));
#363641=CARTESIAN_POINT('Ctrl Pts',(0.678525403784435,1.17524047358083,
-1.42916666666667));
#363642=CARTESIAN_POINT('Ctrl Pts',(0.,1.17524047358083,-1.3875));
#363643=CARTESIAN_POINT('',(0.,0.,0.));
#363644=CARTESIAN_POINT('Ctrl Pts',(2.00016367750204,-0.0349606549171534,
-7.37954989315335));
#363645=CARTESIAN_POINT('Ctrl Pts',(2.00016367750204,-0.165462727384539,
-7.38526442622049));
#363646=CARTESIAN_POINT('Ctrl Pts',(1.96855967425598,-0.409173319918984,
-7.39995586097472));
#363647=CARTESIAN_POINT('Ctrl Pts',(1.85189486927969,-0.792213245836797,
-7.42009815347362));
#363648=CARTESIAN_POINT('Ctrl Pts',(1.6613582879716,-1.13645205609876,-7.44086906835104));
#363649=CARTESIAN_POINT('Ctrl Pts',(1.37992038202068,-1.47263550497672,
-7.46380724865708));
#363650=CARTESIAN_POINT('Ctrl Pts',(0.992206889613594,-1.76297069041634,
-7.48903838801854));
#363651=CARTESIAN_POINT('Ctrl Pts',(0.502190643379444,-1.95990154002328,
-7.51648926813145));
#363652=CARTESIAN_POINT('Ctrl Pts',(-0.0222096198383131,-2.0232383143754,
-7.54405136994835));
#363653=CARTESIAN_POINT('Ctrl Pts',(-0.545023222850085,-1.94828998299833,
-7.57157271170469));
#363654=CARTESIAN_POINT('Ctrl Pts',(-1.0307284358197,-1.74090605654878,
-7.59904290948243));
#363655=CARTESIAN_POINT('Ctrl Pts',(-1.44636321247892,-1.41496070139146,
-7.62658089390187));
#363656=CARTESIAN_POINT('Ctrl Pts',(-1.7630429012686,-0.992255621812916,
-7.65411407831587));
#363657=CARTESIAN_POINT('Ctrl Pts',(-1.95983623864864,-0.502172632985278,
-7.68158430816739));
#363658=CARTESIAN_POINT('Ctrl Pts',(-2.02326404614228,0.0222054813197516,
-7.70911956348259));
#363659=CARTESIAN_POINT('Ctrl Pts',(-1.94828990091774,0.545028935894718,
-7.73665436795491));
#363660=CARTESIAN_POINT('Ctrl Pts',(-1.74090287629493,1.03072354235614,
-7.76412460420479));
#363661=CARTESIAN_POINT('Ctrl Pts',(-1.41496257868532,1.44636639725859,
-7.79165822650409));
#363662=CARTESIAN_POINT('Ctrl Pts',(-0.992256976006747,1.76304240583952,
-7.81919574931953));
#363663=CARTESIAN_POINT('Ctrl Pts',(-0.502167983314945,1.95983220557862,
-7.84666606566923));
#363664=CARTESIAN_POINT('Ctrl Pts',(0.0222021542767409,2.02327125956959,
-7.87418752174917));
#363665=CARTESIAN_POINT('Ctrl Pts',(0.545036582780956,1.94830483935279,
-7.90174989061211));
#363666=CARTESIAN_POINT('Ctrl Pts',(1.03068639649234,1.74088018296961,-7.92919874059292));
#363667=CARTESIAN_POINT('Ctrl Pts',(1.41193217216583,1.44192597876132,-7.95443773023923));
#363668=CARTESIAN_POINT('Ctrl Pts',(1.68594383364152,1.10008635709056,-7.97735256352204));
#363669=CARTESIAN_POINT('Ctrl Pts',(1.86832284879594,0.749865410246654,
-7.99820416287286));
#363670=CARTESIAN_POINT('Ctrl Pts',(1.97885834740452,0.370827498858678,
-8.01808024799317));
#363671=CARTESIAN_POINT('Ctrl Pts',(2.00021510976845,0.108553308485772,
-8.03354455068052));
#363672=CARTESIAN_POINT('Ctrl Pts',(2.00021510976845,-0.0219451194485651,
-8.03925892415782));
#363673=CARTESIAN_POINT('Ctrl Pts',(2.80016361091613,-0.03493223178078,
-7.37981016006517));
#363674=CARTESIAN_POINT('Ctrl Pts',(2.80016361091613,-0.178346676400516,
-7.38609011080151));
#363675=CARTESIAN_POINT('Ctrl Pts',(2.75800714240104,-0.585623740854942,
-7.39993625174015));
#363676=CARTESIAN_POINT('Ctrl Pts',(2.59622001092688,-1.094203255455,-7.42050939398873));
#363677=CARTESIAN_POINT('Ctrl Pts',(2.33073889442298,-1.58539648585596,
-7.44121574714249));
#363678=CARTESIAN_POINT('Ctrl Pts',(1.93774673958377,-2.05527341692013,
-7.46406250879474));
#363679=CARTESIAN_POINT('Ctrl Pts',(1.3977924816811,-2.46335493607239,-7.4892382031805));
#363680=CARTESIAN_POINT('Ctrl Pts',(0.710887177607718,-2.74177962175189,
-7.51690579573811));
#363681=CARTESIAN_POINT('Ctrl Pts',(-0.0222315527777081,-2.83230238724503,
-7.54433060281804));
#363682=CARTESIAN_POINT('Ctrl Pts',(-0.753696284786715,-2.73017360349673,
-7.57179577476958));
#363683=CARTESIAN_POINT('Ctrl Pts',(-1.4359964022639,-2.44137112409355,
-7.59942818098223));
#363684=CARTESIAN_POINT('Ctrl Pts',(-2.01844596000972,-1.98707136838064,
-7.62687978029761));
#363685=CARTESIAN_POINT('Ctrl Pts',(-2.46348770759376,-1.39755415476222,
-7.65433629789662));
#363686=CARTESIAN_POINT('Ctrl Pts',(-2.74170364490091,-0.710913395495067,
-7.6819659616779));
#363687=CARTESIAN_POINT('Ctrl Pts',(-2.83233201369082,0.0221843029796173,
-7.70942122438771));
#363688=CARTESIAN_POINT('Ctrl Pts',(-2.73016814474818,0.753729685089645,
-7.73687603703565));
#363689=CARTESIAN_POINT('Ctrl Pts',(-2.44136831164089,1.43598613500131,
-7.76450570621253));
#363690=CARTESIAN_POINT('Ctrl Pts',(-1.98707527820992,2.01844704832099,
-7.79196266491878));
#363691=CARTESIAN_POINT('Ctrl Pts',(-1.39756088034447,2.46348708795637,
-7.8194137894634));
#363692=CARTESIAN_POINT('Ctrl Pts',(-0.710881081634362,2.74170412714945,
-7.84704636495045));
#363693=CARTESIAN_POINT('Ctrl Pts',(0.0221378788343896,2.83233850612441,
-7.87451146130275));
#363694=CARTESIAN_POINT('Ctrl Pts',(0.753693185451086,2.73018185071023,
-7.90193724347128));
#363695=CARTESIAN_POINT('Ctrl Pts',(1.43623604645724,2.44132953435746,-7.92960016599444));
#363696=CARTESIAN_POINT('Ctrl Pts',(1.96972754709332,2.02444453015913,-7.95479275010049));
#363697=CARTESIAN_POINT('Ctrl Pts',(2.35530318309127,1.54946734602988,-7.97759034640265));
#363698=CARTESIAN_POINT('Ctrl Pts',(2.61262613808022,1.05037578999858,-7.9984674292579));
#363699=CARTESIAN_POINT('Ctrl Pts',(2.76839001336968,0.552800283700582,
-8.01843767560678));
#363700=CARTESIAN_POINT('Ctrl Pts',(2.80021499480674,0.108538122595088,
-8.03388883389828));
#363701=CARTESIAN_POINT('Ctrl Pts',(2.80021499480674,-0.0219216792995908,
-8.0396015159865));
#363702=CARTESIAN_POINT('Ctrl Pts',(2.7998363224979,0.0349606549171637,
-8.01981010684661));
#363703=CARTESIAN_POINT('Ctrl Pts',(2.7998363224979,-0.108453789702572,
-8.02609005758295));
#363704=CARTESIAN_POINT('Ctrl Pts',(2.76770770092932,-0.554475300665122,
-8.04161041709402));
#363705=CARTESIAN_POINT('Ctrl Pts',(2.61230104920345,-1.04994348735895,
-8.06150470700589));
#363706=CARTESIAN_POINT('Ctrl Pts',(2.35499212095577,-1.5493099165356,-8.08239384111292));
#363707=CARTESIAN_POINT('Ctrl Pts',(1.96948131702204,-2.02412699417522,
-8.10518795929102));
#363708=CARTESIAN_POINT('Ctrl Pts',(1.43606137034988,-2.44099583455896,
-8.1303818337545));
#363709=CARTESIAN_POINT('Ctrl Pts',(0.753613249673498,-2.7298044063241,
-8.15804434422187));
#363710=CARTESIAN_POINT('Ctrl Pts',(0.0221607848766011,-2.83195604538419,
-8.18547015377513));
#363711=CARTESIAN_POINT('Ctrl Pts',(-0.710763089306898,-2.74133925166452,
-8.21293536328677));
#363712=CARTESIAN_POINT('Ctrl Pts',(-1.39735180486206,-2.46316525092768,
-8.24056787474674));
#363713=CARTESIAN_POINT('Ctrl Pts',(-1.9867882252217,-2.01819243450698,
-8.26801892009786));
#363714=CARTESIAN_POINT('Ctrl Pts',(-2.44102701245388,-1.43581160139486,
-8.2954760307671));
#363715=CARTESIAN_POINT('Ctrl Pts',(-2.72979268536681,-0.753649988228477,
-8.32310562488017));
#363716=CARTESIAN_POINT('Ctrl Pts',(-2.83194900848818,-0.022207241173352,
-8.35056035976573));
#363717=CARTESIAN_POINT('Ctrl Pts',(-2.74133888936392,0.710795480178799,
-8.37801577635552));
#363718=CARTESIAN_POINT('Ctrl Pts',(-2.4631658691281,1.3973450383548,-8.4056453623318));
#363719=CARTESIAN_POINT('Ctrl Pts',(-2.0181913618354,1.98678420052489,-8.43310180787527));
#363720=CARTESIAN_POINT('Ctrl Pts',(-1.43582178716812,2.44103031792683,
-8.4605535408052));
#363721=CARTESIAN_POINT('Ctrl Pts',(-0.753616702679641,2.7297964193171,
-8.48818595954062));
#363722=CARTESIAN_POINT('Ctrl Pts',(-0.0222544062348159,2.83192570994805,
-8.51565069030184));
#363723=CARTESIAN_POINT('Ctrl Pts',(0.710769507993571,2.74139122758401,
-8.54307702242869));
#363724=CARTESIAN_POINT('Ctrl Pts',(1.39758336815266,2.4631211079265,-8.5707395161615));
#363725=CARTESIAN_POINT('Ctrl Pts',(1.93746427579644,2.05471988808546,-8.59593214237152));
#363726=CARTESIAN_POINT('Ctrl Pts',(2.33041781164643,1.58599477455527,-8.61873057100975));
#363727=CARTESIAN_POINT('Ctrl Pts',(2.59583452983605,1.0910815303924,-8.63960593440206));
#363728=CARTESIAN_POINT('Ctrl Pts',(2.75797391874601,0.595981365328419,
-8.65957756239152));
#363729=CARTESIAN_POINT('Ctrl Pts',(2.79978489023148,0.152404921343189,
-8.67502839375386));
#363730=CARTESIAN_POINT('Ctrl Pts',(2.79978489023148,0.0219451194485099,
-8.68074107584208));
#363731=CARTESIAN_POINT('Ctrl Pts',(1.99983638908381,0.0349322317807904,
-8.0195498399348));
#363732=CARTESIAN_POINT('Ctrl Pts',(1.99983638908381,-0.10202602676277,
-8.02554708183654));
#363733=CARTESIAN_POINT('Ctrl Pts',(1.97826023278427,-0.374998458759011,
-8.04149750289518));
#363734=CARTESIAN_POINT('Ctrl Pts',(1.86797590755627,-0.748764460301907,
-8.06112897846829));
#363735=CARTESIAN_POINT('Ctrl Pts',(1.68561151450438,-1.10015061289253,
-8.08203775324541));
#363736=CARTESIAN_POINT('Ctrl Pts',(1.41165495945895,-1.44156834906321,
-8.10493617015518));
#363737=CARTESIAN_POINT('Ctrl Pts',(1.03047577828238,-1.74058787531436,
-8.13018098020224));
#363738=CARTESIAN_POINT('Ctrl Pts',(0.544916715445223,-1.94793268220013,
-8.15762809500727));
#363739=CARTESIAN_POINT('Ctrl Pts',(0.0221827178159963,-2.02289026809774,
-8.18519084627103));
#363740=CARTESIAN_POINT('Ctrl Pts',(-0.502090027370269,-1.95945608733342,
-8.21271232019691));
#363741=CARTESIAN_POINT('Ctrl Pts',(-0.992083838417867,-1.76270006106949,
-8.24018259789098));
#363742=CARTESIAN_POINT('Ctrl Pts',(-1.4147054776909,-1.44608180030657,
-8.26772003513789));
#363743=CARTESIAN_POINT('Ctrl Pts',(-1.74058220612872,-1.03051305966975,
-8.29525381080208));
#363744=CARTESIAN_POINT('Ctrl Pts',(-1.94792527911454,-0.54490922807225,
-8.32272397147271));
#363745=CARTESIAN_POINT('Ctrl Pts',(-2.02288104093964,-0.0221860622005593,
-8.3502586988329));
#363746=CARTESIAN_POINT('Ctrl Pts',(-1.95946064553349,0.502094730808056,
-8.37779410728247));
#363747=CARTESIAN_POINT('Ctrl Pts',(-1.76270043378214,0.992082445780963,
-8.40526426032094));
#363748=CARTESIAN_POINT('Ctrl Pts',(-1.4460786623108,1.41470354935293,-8.43279736946537));
#363749=CARTESIAN_POINT('Ctrl Pts',(-1.03051788283039,1.74058563617661,
-8.46033550064529));
#363750=CARTESIAN_POINT('Ctrl Pts',(-0.544903604360224,1.94792449639017,
-8.48780566031878));
#363751=CARTESIAN_POINT('Ctrl Pts',(-0.0221901307924648,2.02285846845712,
-8.51532675052651));
#363752=CARTESIAN_POINT('Ctrl Pts',(0.502112905323441,1.95951419733875,
-8.5428896703966));
#363753=CARTESIAN_POINT('Ctrl Pts',(0.992033718187761,1.76267182698944,
-8.57033808767502));
#363754=CARTESIAN_POINT('Ctrl Pts',(1.37966890086895,1.47220110119364,-8.59557713282226));
#363755=CARTESIAN_POINT('Ctrl Pts',(1.66105846219667,1.13661442398405,-8.61849276017575));
#363756=CARTESIAN_POINT('Ctrl Pts',(1.85153124055178,0.790568741290481,
-8.63934277351964));
#363757=CARTESIAN_POINT('Ctrl Pts',(1.96844225278085,0.414017589463527,
-8.65921974028535));
#363758=CARTESIAN_POINT('Ctrl Pts',(1.99978500519319,0.152400794214044,
-8.67468495623063));
#363759=CARTESIAN_POINT('Ctrl Pts',(1.99978500519318,0.0219216792995357,
-8.68039848401339));
#363760=CARTESIAN_POINT('Ctrl Pts',(1.19983645566973,0.0349038086444169,
-8.01928957302298));
#363761=CARTESIAN_POINT('Ctrl Pts',(1.19983645566973,-0.0955982638229683,
-8.02500410609012));
#363762=CARTESIAN_POINT('Ctrl Pts',(1.18881276463922,-0.1955216168529,-8.04138458869635));
#363763=CARTESIAN_POINT('Ctrl Pts',(1.12365076590908,-0.447585433244864,
-8.06075324993069));
#363764=CARTESIAN_POINT('Ctrl Pts',(1.016230908053,-0.650991309249464,-8.0816816653779));
#363765=CARTESIAN_POINT('Ctrl Pts',(0.853828601895857,-0.859009703951189,
-8.10468438101933));
#363766=CARTESIAN_POINT('Ctrl Pts',(0.624890186214873,-1.04017991606976,
-8.12998012664998));
#363767=CARTESIAN_POINT('Ctrl Pts',(0.336220181216949,-1.16606095807615,
-8.15721184579269));
#363768=CARTESIAN_POINT('Ctrl Pts',(0.0222046507553913,-1.21382449081129,
-8.18491153876691));
#363769=CARTESIAN_POINT('Ctrl Pts',(-0.29341696543364,-1.17757292300231,
-8.21248927710705));
#363770=CARTESIAN_POINT('Ctrl Pts',(-0.586815871973671,-1.0622348712113,
-8.23979732103521));
#363771=CARTESIAN_POINT('Ctrl Pts',(-0.842622730160096,-0.873971166106157,
-8.26742115017792));
#363772=CARTESIAN_POINT('Ctrl Pts',(-1.04013739980356,-0.625214517944632,
-8.29503159083705));
#363773=CARTESIAN_POINT('Ctrl Pts',(-1.16605787286226,-0.336168467916023,
-8.32234231806526));
#363774=CARTESIAN_POINT('Ctrl Pts',(-1.2138130733911,-0.0221648832277664,
-8.34995703790007));
#363775=CARTESIAN_POINT('Ctrl Pts',(-1.17758240170305,0.293393981437313,
-8.37757243820942));
#363776=CARTESIAN_POINT('Ctrl Pts',(-1.06223499843619,0.586819853207128,
-8.40488315831008));
#363777=CARTESIAN_POINT('Ctrl Pts',(-0.873965962786202,0.842622898180978,
-8.43249293105548));
#363778=CARTESIAN_POINT('Ctrl Pts',(-0.625213978492663,1.04014095442639,
-8.46011746048537));
#363779=CARTESIAN_POINT('Ctrl Pts',(-0.336190506040807,1.16605257346324,
-8.48742536109694));
#363780=CARTESIAN_POINT('Ctrl Pts',(-0.0221258553501136,1.21379122696619,
-8.51500281075118));
#363781=CARTESIAN_POINT('Ctrl Pts',(0.293456302653311,1.17763716709349,
-8.54270231836451));
#363782=CARTESIAN_POINT('Ctrl Pts',(0.586484068222858,1.06222254605237,
-8.56993665918854));
#363783=CARTESIAN_POINT('Ctrl Pts',(0.821873525941461,0.889682314301827,
-8.59522212327301));
#363784=CARTESIAN_POINT('Ctrl Pts',(0.991699112746911,0.687234073412837,
-8.61825494934175));
#363785=CARTESIAN_POINT('Ctrl Pts',(1.1072279512675,0.490055952188566,-8.63907961263722));
#363786=CARTESIAN_POINT('Ctrl Pts',(1.17891058681569,0.232053813598634,
-8.65886191817918));
#363787=CARTESIAN_POINT('Ctrl Pts',(1.19978512015489,0.152396667084899,
-8.6743415187074));
#363788=CARTESIAN_POINT('Ctrl Pts',(1.19978512015489,0.0218982391505614,
-8.6800558921847));
#363789=CARTESIAN_POINT('Ctrl Pts',(1.20016374408796,-0.0349890780535269,
-7.37928962624154));
#363790=CARTESIAN_POINT('Ctrl Pts',(1.20016374408796,-0.152578778368561,
-7.38443874163948));
#363791=CARTESIAN_POINT('Ctrl Pts',(1.17911220611093,-0.232722898983027,
-7.39997547020929));
#363792=CARTESIAN_POINT('Ctrl Pts',(1.1075697276325,-0.490223236218595,
-7.41968691295851));
#363793=CARTESIAN_POINT('Ctrl Pts',(0.99197768152021,-0.687507626341548,
-7.44052238955959));
#363794=CARTESIAN_POINT('Ctrl Pts',(0.822094024457586,-0.889997593033309,
-7.46355198851942));
#363795=CARTESIAN_POINT('Ctrl Pts',(0.586621297546092,-1.06258644476029,
-7.48883857285657));
#363796=CARTESIAN_POINT('Ctrl Pts',(0.293494109151169,-1.17802345829468,
-7.51607274052479));
#363797=CARTESIAN_POINT('Ctrl Pts',(-0.022187686898918,-1.21417424150576,
-7.54377213707865));
#363798=CARTESIAN_POINT('Ctrl Pts',(-0.336350160913456,-1.16640636249992,
-7.5713496486398));
#363799=CARTESIAN_POINT('Ctrl Pts',(-0.625460469375504,-1.04044098900401,
-7.59865763798262));
#363800=CARTESIAN_POINT('Ctrl Pts',(-0.874280464948115,-0.842850034402287,
-7.62628200750612));
#363801=CARTESIAN_POINT('Ctrl Pts',(-1.06259809494344,-0.586957088863615,
-7.65389185873512));
#363802=CARTESIAN_POINT('Ctrl Pts',(-1.17796883239637,-0.293431870475487,
-7.68120265465688));
#363803=CARTESIAN_POINT('Ctrl Pts',(-1.21419607859374,0.0222266596598858,
-7.70881790257747));
#363804=CARTESIAN_POINT('Ctrl Pts',(-1.16641165708731,0.33632818669979,
-7.73643269887416));
#363805=CARTESIAN_POINT('Ctrl Pts',(-1.04043744094898,0.625460949710965,
-7.76374350219705));
#363806=CARTESIAN_POINT('Ctrl Pts',(-0.842849879160721,0.874285746196179,
-7.7913537880894));
#363807=CARTESIAN_POINT('Ctrl Pts',(-0.58695307166902,1.06259772372267,
-7.81897770917568));
#363808=CARTESIAN_POINT('Ctrl Pts',(-0.293454884995528,1.17796028400778,
-7.846285766388));
#363809=CARTESIAN_POINT('Ctrl Pts',(0.0222664297190919,1.21420401301477,
-7.87386358219558));
#363810=CARTESIAN_POINT('Ctrl Pts',(0.336379980110826,1.16642782799535,
-7.90156253775294));
#363811=CARTESIAN_POINT('Ctrl Pts',(0.625136746527436,1.04043083158176,
-7.9287973151914));
#363812=CARTESIAN_POINT('Ctrl Pts',(0.854136797238339,0.859407427363523,
-7.95408271037797));
#363813=CARTESIAN_POINT('Ctrl Pts',(1.01658448419176,0.650705368151239,
-7.97711478064143));
#363814=CARTESIAN_POINT('Ctrl Pts',(1.12401955951167,0.449355030494726,
-7.99794089648783));
#363815=CARTESIAN_POINT('Ctrl Pts',(1.18932668143936,0.188854714016773,
-8.01772282037956));
#363816=CARTESIAN_POINT('Ctrl Pts',(1.20021522473016,0.108568494376457,
-8.03320026746274));
#363817=CARTESIAN_POINT('Ctrl Pts',(1.20021522473015,-0.0219685595975393,
-8.03891633232913));
#363818=CARTESIAN_POINT('Ctrl Pts',(2.00016367750204,-0.0349606549171534,
-7.37954989315335));
#363819=CARTESIAN_POINT('Ctrl Pts',(2.00016367750204,-0.165462727384539,
-7.38526442622049));
#363820=CARTESIAN_POINT('Ctrl Pts',(1.96855967425598,-0.409173319918984,
-7.39995586097472));
#363821=CARTESIAN_POINT('Ctrl Pts',(1.85189486927969,-0.792213245836797,
-7.42009815347362));
#363822=CARTESIAN_POINT('Ctrl Pts',(1.6613582879716,-1.13645205609876,-7.44086906835104));
#363823=CARTESIAN_POINT('Ctrl Pts',(1.37992038202068,-1.47263550497672,
-7.46380724865708));
#363824=CARTESIAN_POINT('Ctrl Pts',(0.992206889613594,-1.76297069041634,
-7.48903838801854));
#363825=CARTESIAN_POINT('Ctrl Pts',(0.502190643379444,-1.95990154002328,
-7.51648926813145));
#363826=CARTESIAN_POINT('Ctrl Pts',(-0.0222096198383131,-2.0232383143754,
-7.54405136994835));
#363827=CARTESIAN_POINT('Ctrl Pts',(-0.545023222850085,-1.94828998299833,
-7.57157271170469));
#363828=CARTESIAN_POINT('Ctrl Pts',(-1.0307284358197,-1.74090605654878,
-7.59904290948243));
#363829=CARTESIAN_POINT('Ctrl Pts',(-1.44636321247892,-1.41496070139146,
-7.62658089390187));
#363830=CARTESIAN_POINT('Ctrl Pts',(-1.7630429012686,-0.992255621812916,
-7.65411407831587));
#363831=CARTESIAN_POINT('Ctrl Pts',(-1.95983623864864,-0.502172632985278,
-7.68158430816739));
#363832=CARTESIAN_POINT('Ctrl Pts',(-2.02326404614228,0.0222054813197516,
-7.70911956348259));
#363833=CARTESIAN_POINT('Ctrl Pts',(-1.94828990091774,0.545028935894718,
-7.73665436795491));
#363834=CARTESIAN_POINT('Ctrl Pts',(-1.74090287629493,1.03072354235614,
-7.76412460420479));
#363835=CARTESIAN_POINT('Ctrl Pts',(-1.41496257868532,1.44636639725859,
-7.79165822650409));
#363836=CARTESIAN_POINT('Ctrl Pts',(-0.992256976006747,1.76304240583952,
-7.81919574931953));
#363837=CARTESIAN_POINT('Ctrl Pts',(-0.502167983314945,1.95983220557862,
-7.84666606566923));
#363838=CARTESIAN_POINT('Ctrl Pts',(0.0222021542767409,2.02327125956959,
-7.87418752174917));
#363839=CARTESIAN_POINT('Ctrl Pts',(0.545036582780956,1.94830483935279,
-7.90174989061211));
#363840=CARTESIAN_POINT('Ctrl Pts',(1.03068639649234,1.74088018296961,-7.92919874059292));
#363841=CARTESIAN_POINT('Ctrl Pts',(1.41193217216583,1.44192597876132,-7.95443773023923));
#363842=CARTESIAN_POINT('Ctrl Pts',(1.68594383364152,1.10008635709056,-7.97735256352204));
#363843=CARTESIAN_POINT('Ctrl Pts',(1.86832284879594,0.749865410246654,
-7.99820416287286));
#363844=CARTESIAN_POINT('Ctrl Pts',(1.97885834740452,0.370827498858678,
-8.01808024799317));
#363845=CARTESIAN_POINT('Ctrl Pts',(2.00021510976845,0.108553308485772,
-8.03354455068052));
#363846=CARTESIAN_POINT('Ctrl Pts',(2.00021510976845,-0.0219451194485651,
-8.03925892415782));
#363847=CARTESIAN_POINT('',(1.99983638908381,0.0349322317806574,-8.0195498399348));
#363848=CARTESIAN_POINT('',(1.6000000331116,-1.41261775450829E-5,-7.6995506484554));
#363849=CARTESIAN_POINT('Origin',(2.00000003329293,-1.42115683144772E-5,
-7.69954986654408));
#363850=CARTESIAN_POINT('',(1.99978500519318,0.0219216792995357,-8.68039848401339));
#363851=CARTESIAN_POINT('Ctrl Pts',(1.99983638908381,0.0349322317806574,
-8.0195498399348));
#363852=CARTESIAN_POINT('Ctrl Pts',(1.99983638908381,-0.10202602676277,
-8.02554708183654));
#363853=CARTESIAN_POINT('Ctrl Pts',(1.97826023278427,-0.374998458759011,
-8.04149750289518));
#363854=CARTESIAN_POINT('Ctrl Pts',(1.86797590755627,-0.748764460301907,
-8.06112897846829));
#363855=CARTESIAN_POINT('Ctrl Pts',(1.68561151450438,-1.10015061289253,
-8.08203775324541));
#363856=CARTESIAN_POINT('Ctrl Pts',(1.41165495945895,-1.44156834906321,
-8.10493617015518));
#363857=CARTESIAN_POINT('Ctrl Pts',(1.03047577828238,-1.74058787531436,
-8.13018098020224));
#363858=CARTESIAN_POINT('Ctrl Pts',(0.544916715445223,-1.94793268220013,
-8.15762809500727));
#363859=CARTESIAN_POINT('Ctrl Pts',(0.0221827178159963,-2.02289026809774,
-8.18519084627103));
#363860=CARTESIAN_POINT('Ctrl Pts',(-0.502090027370269,-1.95945608733342,
-8.21271232019691));
#363861=CARTESIAN_POINT('Ctrl Pts',(-0.992083838417867,-1.76270006106949,
-8.24018259789098));
#363862=CARTESIAN_POINT('Ctrl Pts',(-1.4147054776909,-1.44608180030657,
-8.26772003513789));
#363863=CARTESIAN_POINT('Ctrl Pts',(-1.74058220612872,-1.03051305966975,
-8.29525381080208));
#363864=CARTESIAN_POINT('Ctrl Pts',(-1.94792527911454,-0.54490922807225,
-8.32272397147271));
#363865=CARTESIAN_POINT('Ctrl Pts',(-2.02288104093964,-0.0221860622005593,
-8.3502586988329));
#363866=CARTESIAN_POINT('Ctrl Pts',(-1.95946064553349,0.502094730808056,
-8.37779410728247));
#363867=CARTESIAN_POINT('Ctrl Pts',(-1.76270043378214,0.992082445780963,
-8.40526426032094));
#363868=CARTESIAN_POINT('Ctrl Pts',(-1.4460786623108,1.41470354935293,-8.43279736946537));
#363869=CARTESIAN_POINT('Ctrl Pts',(-1.03051788283039,1.74058563617661,
-8.46033550064529));
#363870=CARTESIAN_POINT('Ctrl Pts',(-0.544903604360224,1.94792449639017,
-8.48780566031878));
#363871=CARTESIAN_POINT('Ctrl Pts',(-0.0221901307924648,2.02285846845712,
-8.51532675052651));
#363872=CARTESIAN_POINT('Ctrl Pts',(0.502112905323441,1.95951419733875,
-8.5428896703966));
#363873=CARTESIAN_POINT('Ctrl Pts',(0.992033718187761,1.76267182698944,
-8.57033808767502));
#363874=CARTESIAN_POINT('Ctrl Pts',(1.37966890086895,1.47220110119364,-8.59557713282226));
#363875=CARTESIAN_POINT('Ctrl Pts',(1.66105846219667,1.13661442398405,-8.61849276017575));
#363876=CARTESIAN_POINT('Ctrl Pts',(1.85153124055178,0.790568741290481,
-8.63934277351964));
#363877=CARTESIAN_POINT('Ctrl Pts',(1.96844225278085,0.414017589463527,
-8.65921974028535));
#363878=CARTESIAN_POINT('Ctrl Pts',(1.99978500519319,0.152400794214044,
-8.67468495623063));
#363879=CARTESIAN_POINT('Ctrl Pts',(1.99978500519318,0.0219216792995357,
-8.68039848401339));
#363880=CARTESIAN_POINT('',(2.00021510976845,-0.0219451194485651,-8.03925892415782));
#363881=CARTESIAN_POINT('Origin',(2.00000005748082,-1.17200745146546E-5,
-8.35982870408561));
#363882=CARTESIAN_POINT('',(2.00016367750204,-0.0349606549172864,-7.37954989315336));
#363883=CARTESIAN_POINT('Ctrl Pts',(2.00016367750204,-0.0349606549172864,
-7.37954989315336));
#363884=CARTESIAN_POINT('Ctrl Pts',(2.00016367750204,-0.165462727384539,
-7.38526442622049));
#363885=CARTESIAN_POINT('Ctrl Pts',(1.96855967425598,-0.409173319918984,
-7.39995586097472));
#363886=CARTESIAN_POINT('Ctrl Pts',(1.85189486927969,-0.792213245836797,
-7.42009815347362));
#363887=CARTESIAN_POINT('Ctrl Pts',(1.6613582879716,-1.13645205609876,-7.44086906835104));
#363888=CARTESIAN_POINT('Ctrl Pts',(1.37992038202068,-1.47263550497672,
-7.46380724865708));
#363889=CARTESIAN_POINT('Ctrl Pts',(0.992206889613594,-1.76297069041634,
-7.48903838801854));
#363890=CARTESIAN_POINT('Ctrl Pts',(0.502190643379444,-1.95990154002328,
-7.51648926813145));
#363891=CARTESIAN_POINT('Ctrl Pts',(-0.0222096198383131,-2.0232383143754,
-7.54405136994835));
#363892=CARTESIAN_POINT('Ctrl Pts',(-0.545023222850085,-1.94828998299833,
-7.57157271170469));
#363893=CARTESIAN_POINT('Ctrl Pts',(-1.0307284358197,-1.74090605654878,
-7.59904290948243));
#363894=CARTESIAN_POINT('Ctrl Pts',(-1.44636321247892,-1.41496070139146,
-7.62658089390187));
#363895=CARTESIAN_POINT('Ctrl Pts',(-1.7630429012686,-0.992255621812916,
-7.65411407831587));
#363896=CARTESIAN_POINT('Ctrl Pts',(-1.95983623864864,-0.502172632985277,
-7.68158430816739));
#363897=CARTESIAN_POINT('Ctrl Pts',(-2.02326404614228,0.0222054813197516,
-7.70911956348259));
#363898=CARTESIAN_POINT('Ctrl Pts',(-1.94828990091774,0.545028935894718,
-7.73665436795491));
#363899=CARTESIAN_POINT('Ctrl Pts',(-1.74090287629493,1.03072354235614,
-7.76412460420479));
#363900=CARTESIAN_POINT('Ctrl Pts',(-1.41496257868532,1.44636639725859,
-7.79165822650409));
#363901=CARTESIAN_POINT('Ctrl Pts',(-0.992256976006747,1.76304240583952,
-7.81919574931953));
#363902=CARTESIAN_POINT('Ctrl Pts',(-0.502167983314945,1.95983220557862,
-7.84666606566923));
#363903=CARTESIAN_POINT('Ctrl Pts',(0.0222021542767409,2.02327125956959,
-7.87418752174917));
#363904=CARTESIAN_POINT('Ctrl Pts',(0.545036582780956,1.94830483935279,
-7.90174989061211));
#363905=CARTESIAN_POINT('Ctrl Pts',(1.03068639649234,1.74088018296961,-7.92919874059292));
#363906=CARTESIAN_POINT('Ctrl Pts',(1.41193217216583,1.44192597876132,-7.95443773023923));
#363907=CARTESIAN_POINT('Ctrl Pts',(1.68594383364152,1.10008635709056,-7.97735256352204));
#363908=CARTESIAN_POINT('Ctrl Pts',(1.86832284879594,0.749865410246654,
-7.99820416287286));
#363909=CARTESIAN_POINT('Ctrl Pts',(1.97885834740452,0.370827498858678,
-8.01808024799317));
#363910=CARTESIAN_POINT('Ctrl Pts',(2.00021510976845,0.108553308485772,
-8.03354455068052));
#363911=CARTESIAN_POINT('Ctrl Pts',(2.00021510976845,-0.0219451194485651,
-8.03925892415782));
#363912=CARTESIAN_POINT('Origin',(2.00000003329293,-1.42115683144772E-5,
-7.69954986654408));
#363913=CARTESIAN_POINT('Ctrl Pts',(2.00005141137773,-0.0349509159166537,
-1.58027907189674));
#363914=CARTESIAN_POINT('Ctrl Pts',(2.00005141137773,-0.209477500702,-1.59705901785001));
#363915=CARTESIAN_POINT('Ctrl Pts',(1.93937485936534,-0.574981221086946,
-1.64398167301615));
#363916=CARTESIAN_POINT('Ctrl Pts',(1.72866575619624,-1.05218683017129,
-1.70157781695483));
#363917=CARTESIAN_POINT('Ctrl Pts',(1.39603065320521,-1.46514475575449,
-1.76296158741006));
#363918=CARTESIAN_POINT('Ctrl Pts',(0.969522180315677,-1.77589106055163,
-1.82311912419573));
#363919=CARTESIAN_POINT('Ctrl Pts',(0.476783238604109,-1.96670288995313,
-1.88346520364747));
#363920=CARTESIAN_POINT('Ctrl Pts',(-0.0484603850821368,-2.02312932285366,
-1.94396055370022));
#363921=CARTESIAN_POINT('Ctrl Pts',(-0.570338856925993,-1.94138942628423,
-2.00439291407465));
#363922=CARTESIAN_POINT('Ctrl Pts',(-1.05344948325284,-1.72773686772633,
-2.06470891120488));
#363923=CARTESIAN_POINT('Ctrl Pts',(-1.46487312544728,-1.39632835696345,
-2.1251726344757));
#363924=CARTESIAN_POINT('Ctrl Pts',(-1.77606001340043,-0.969474639293403,
-2.18562457894241));
#363925=CARTESIAN_POINT('Ctrl Pts',(-1.9665886161183,-0.476795144252666,
-2.2459421237894));
#363926=CARTESIAN_POINT('Ctrl Pts',(-2.0231790616074,0.0484698229690482,
-2.30639998925771));
#363927=CARTESIAN_POINT('Ctrl Pts',(-1.94138573006516,0.570342005097921,
-2.36685494461854));
#363928=CARTESIAN_POINT('Ctrl Pts',(-1.72773301625381,1.05344259449438,
-2.42717237256682));
#363929=CARTESIAN_POINT('Ctrl Pts',(-1.39633042998923,1.46487729238585,
-2.48762977035772));
#363930=CARTESIAN_POINT('Ctrl Pts',(-0.969474291036093,1.77605966206198,
-2.54808497616048));
#363931=CARTESIAN_POINT('Ctrl Pts',(-0.476795343347378,1.96658811640277,
-2.6084023881129));
#363932=CARTESIAN_POINT('Ctrl Pts',(0.0484699602192744,2.02317939996145,
-2.66885975673847));
#363933=CARTESIAN_POINT('Ctrl Pts',(0.570341982836039,1.94138567238666,
-2.72931497821885));
#363934=CARTESIAN_POINT('Ctrl Pts',(1.05344257210098,1.72773301387229,-2.78963238875962));
#363935=CARTESIAN_POINT('Ctrl Pts',(1.46487731147791,1.39633043581364,-2.85008975616076));
#363936=CARTESIAN_POINT('Ctrl Pts',(1.7760596572503,0.96947429019414,-2.91054497830833));
#363937=CARTESIAN_POINT('Ctrl Pts',(1.96658811657123,0.47679534386094,-2.97086238877306));
#363938=CARTESIAN_POINT('Ctrl Pts',(2.02317940049204,-0.0484699606166185,
-3.03131975614836));
#363939=CARTESIAN_POINT('Ctrl Pts',(1.94138567221384,-0.570341982644115,
-3.09177497831011));
#363940=CARTESIAN_POINT('Ctrl Pts',(1.72773301391076,-1.05344257214956,
-3.15209238877301));
#363941=CARTESIAN_POINT('Ctrl Pts',(1.39633043580907,-1.46487731147983,
-3.21254975614839));
#363942=CARTESIAN_POINT('Ctrl Pts',(0.969474290197969,-1.77605965724421,
-3.27300497831004));
#363943=CARTESIAN_POINT('Ctrl Pts',(0.476795343858464,-1.96658811657341,
-3.33332238877311));
#363944=CARTESIAN_POINT('Ctrl Pts',(-0.0484699606159255,-2.0231794004916,
-3.39377975614832));
#363945=CARTESIAN_POINT('Ctrl Pts',(-0.570341982644268,-1.94138567221424,
-3.45423497831005));
#363946=CARTESIAN_POINT('Ctrl Pts',(-1.05344257214943,-1.72773301391041,
-3.51455238877311));
#363947=CARTESIAN_POINT('Ctrl Pts',(-1.46487731147993,-1.39633043580919,
-3.57500975614831));
#363948=CARTESIAN_POINT('Ctrl Pts',(-1.77605965724425,-0.969474290197954,
-3.63546497831004));
#363949=CARTESIAN_POINT('Ctrl Pts',(-1.96658811657337,-0.476795343858458,
-3.69578238877312));
#363950=CARTESIAN_POINT('Ctrl Pts',(-2.02317940049162,0.0484699606159343,
-3.75623975614831));
#363951=CARTESIAN_POINT('Ctrl Pts',(-1.94138567221425,0.570341982644281,
-3.81669497831005));
#363952=CARTESIAN_POINT('Ctrl Pts',(-1.7277330139104,1.05344257214943,-3.87701238877311));
#363953=CARTESIAN_POINT('Ctrl Pts',(-1.39633043580919,1.46487731147993,
-3.93746975614831));
#363954=CARTESIAN_POINT('Ctrl Pts',(-0.969474290197942,1.77605965724426,
-3.99792497831004));
#363955=CARTESIAN_POINT('Ctrl Pts',(-0.476795343858452,1.96658811657335,
-4.05824238877313));
#363956=CARTESIAN_POINT('Ctrl Pts',(0.0484699606159434,2.02317940049163,
-4.11869975614831));
#363957=CARTESIAN_POINT('Ctrl Pts',(0.570341982644284,1.94138567221424,
-4.17915497831005));
#363958=CARTESIAN_POINT('Ctrl Pts',(1.05344257214943,1.72773301391039,-4.23947238877311));
#363959=CARTESIAN_POINT('Ctrl Pts',(1.46487731147993,1.39633043580918,-4.29992975614832));
#363960=CARTESIAN_POINT('Ctrl Pts',(1.77605965724427,0.969474290197945,
-4.36038497831003));
#363961=CARTESIAN_POINT('Ctrl Pts',(1.96658811657337,0.476795343858441,
-4.42070238877312));
#363962=CARTESIAN_POINT('Ctrl Pts',(2.02317940049162,-0.0484699606159445,
-4.48115975614831));
#363963=CARTESIAN_POINT('Ctrl Pts',(1.94138567221424,-0.570341982644292,
-4.54161497831005));
#363964=CARTESIAN_POINT('Ctrl Pts',(1.72773301391038,-1.05344257214943,
-4.60193238877312));
#363965=CARTESIAN_POINT('Ctrl Pts',(1.39633043580918,-1.46487731147994,
-4.66238975614831));
#363966=CARTESIAN_POINT('Ctrl Pts',(0.969474290197935,-1.77605965724426,
-4.72284497831004));
#363967=CARTESIAN_POINT('Ctrl Pts',(0.476795343858439,-1.96658811657337,
-4.78316238877312));
#363968=CARTESIAN_POINT('Ctrl Pts',(-0.0484699606159579,-2.02317940049164,
-4.8436197561483));
#363969=CARTESIAN_POINT('Ctrl Pts',(-0.570341982644288,-1.94138567221422,
-4.90407497831006));
#363970=CARTESIAN_POINT('Ctrl Pts',(-1.05344257214943,-1.72773301391037,
-4.96439238877312));
#363971=CARTESIAN_POINT('Ctrl Pts',(-1.46487731147995,-1.39633043580918,
-5.02484975614831));
#363972=CARTESIAN_POINT('Ctrl Pts',(-1.77605965724426,-0.969474290197928,
-5.08530497831004));
#363973=CARTESIAN_POINT('Ctrl Pts',(-1.96658811657335,-0.476795343858433,
-5.14562238877313));
#363974=CARTESIAN_POINT('Ctrl Pts',(-2.02317940049163,0.0484699606159606,
-5.2060797561483));
#363975=CARTESIAN_POINT('Ctrl Pts',(-1.94138567221425,0.570341982644311,
-5.26653497831003));
#363976=CARTESIAN_POINT('Ctrl Pts',(-1.72773301391036,1.05344257214944,
-5.32685238877313));
#363977=CARTESIAN_POINT('Ctrl Pts',(-1.39633043580918,1.46487731147996,
-5.3873097561483));
#363978=CARTESIAN_POINT('Ctrl Pts',(-0.969474290197916,1.77605965724424,
-5.44776497831006));
#363979=CARTESIAN_POINT('Ctrl Pts',(-0.476795343858422,1.96658811657339,
-5.5080823887731));
#363980=CARTESIAN_POINT('Ctrl Pts',(0.0484699606159706,2.02317940049163,
-5.56853975614829));
#363981=CARTESIAN_POINT('Ctrl Pts',(0.570341982644291,1.94138567221422,
-5.62899497831007));
#363982=CARTESIAN_POINT('Ctrl Pts',(1.05344257214944,1.72773301391032,-5.68931238877313));
#363983=CARTESIAN_POINT('Ctrl Pts',(1.46487731147996,1.3963304358092,-5.74976975614823));
#363984=CARTESIAN_POINT('Ctrl Pts',(1.77605965724441,0.969474290197947,
-5.81022497831013));
#363985=CARTESIAN_POINT('Ctrl Pts',(1.96658811657315,0.476795343858267,
-5.87054238877304));
#363986=CARTESIAN_POINT('Ctrl Pts',(2.02317940049197,-0.0484699606151168,
-5.93099975614826));
#363987=CARTESIAN_POINT('Ctrl Pts',(1.94138567221262,-0.570341982647331,
-5.99145497831012));
#363988=CARTESIAN_POINT('Ctrl Pts',(1.72773301391079,-1.05344257214282,
-6.05177238877488));
#363989=CARTESIAN_POINT('Ctrl Pts',(1.39633043583791,-1.46487731150212,
-6.1122297561358));
#363990=CARTESIAN_POINT('Ctrl Pts',(0.969474290103704,-1.77605965719443,
-6.17268497832268));
#363991=CARTESIAN_POINT('Ctrl Pts',(0.476795344014053,-1.96658811647506,
-6.23300238886911));
#363992=CARTESIAN_POINT('Ctrl Pts',(-0.0484699607888847,-2.02317940162764,
-6.293459755551));
#363993=CARTESIAN_POINT('Ctrl Pts',(-0.570341982515374,-1.94138566986718,
-6.35391497894857));
#363994=CARTESIAN_POINT('Ctrl Pts',(-1.0534425689941,-1.72773301427299,
-6.41423239105532));
#363995=CARTESIAN_POINT('Ctrl Pts',(-1.46487733129139,-1.39633044764682,
-6.47468974174144));
#363996=CARTESIAN_POINT('Ctrl Pts',(-1.77605962440754,-0.969474272408487,
-6.53514499410053));
#363997=CARTESIAN_POINT('Ctrl Pts',(-1.96658808441403,-0.4767953693466,
-6.59546242507117));
#363998=CARTESIAN_POINT('Ctrl Pts',(-2.02317971788315,0.0484700612956726,
-6.65591951867769));
#363999=CARTESIAN_POINT('Ctrl Pts',(-1.94138529374751,0.57034175258804,
-6.71637524065362));
#364000=CARTESIAN_POINT('Ctrl Pts',(-1.7277327906675,1.05344225923825,-6.77669281345839));
#364001=CARTESIAN_POINT('Ctrl Pts',(-1.39633190064527,1.46488023063332,
-6.83714685373563));
#364002=CARTESIAN_POINT('Ctrl Pts',(-0.969474795144666,1.77605674551469,
-6.89760831895014));
#364003=CARTESIAN_POINT('Ctrl Pts',(-0.476792483974202,1.96658170561334,
-6.95792512927773));
#364004=CARTESIAN_POINT('Ctrl Pts',(0.0484734593030573,2.0232081210323,
-7.01835708981697));
#364005=CARTESIAN_POINT('Ctrl Pts',(0.570336624689882,1.94136175768686,
-7.07885725203471));
#364006=CARTESIAN_POINT('Ctrl Pts',(1.05340619968671,1.72778052727257,-7.13918044053492));
#364007=CARTESIAN_POINT('Ctrl Pts',(1.46503146071072,1.39600002911185,-7.19942807213429));
#364008=CARTESIAN_POINT('Ctrl Pts',(1.77572739170825,0.970967789756964,
-7.26046972816476));
#364009=CARTESIAN_POINT('Ctrl Pts',(1.9679960876878,0.471734127632586,-7.31921124624962));
#364010=CARTESIAN_POINT('Ctrl Pts',(2.00016367750205,0.139563645186354,
-7.36277016686196));
#364011=CARTESIAN_POINT('Ctrl Pts',(2.00016367750204,-0.0349606549172864,
-7.37954989315336));
#364012=CARTESIAN_POINT('Ctrl Pts',(1.20005141796495,-0.0349598558146385,
-1.58019721042982));
#364013=CARTESIAN_POINT('Ctrl Pts',(1.20005141796495,-0.196639509400045,
-1.59574198174499));
#364014=CARTESIAN_POINT('Ctrl Pts',(1.15732797686238,-0.340816716447164,
-1.6447382432052));
#364015=CARTESIAN_POINT('Ctrl Pts',(1.02794595474197,-0.654182454634222,
-1.70085757593186));
#364016=CARTESIAN_POINT('Ctrl Pts',(0.824371570064879,-0.890750973398493,
-1.76298366242172));
#364017=CARTESIAN_POINT('Ctrl Pts',(0.563969291479731,-1.07614468532721,
-1.82314153495176));
#364018=CARTESIAN_POINT('Ctrl Pts',(0.268053015090469,-1.18466145511491,
-1.88305373693166));
#364019=CARTESIAN_POINT('Ctrl Pts',(-0.0484395870237313,-1.21410753423567,
-1.9438363016732));
#364020=CARTESIAN_POINT('Ctrl Pts',(-0.361651032204537,-1.15949959431507,
-2.00439370017114));
#364021=CARTESIAN_POINT('Ctrl Pts',(-0.648204859882796,-1.02726348852071,
-2.06435695179187));
#364022=CARTESIAN_POINT('Ctrl Pts',(-0.892791267502041,-0.824210832808723,
-2.12500826054469));
#364023=CARTESIAN_POINT('Ctrl Pts',(-1.07560894612736,-0.564190577762509,
-2.18562659547641));
#364024=CARTESIAN_POINT('Ctrl Pts',(-1.1847293912525,-0.268030428045687,
-2.24559800960236));
#364025=CARTESIAN_POINT('Ctrl Pts',(-1.21410751416084,0.0484963826130714,
-2.30623010797513));
#364026=CARTESIAN_POINT('Ctrl Pts',(-1.1595132046369,0.36162639690026,-2.36685750692005));
#364027=CARTESIAN_POINT('Ctrl Pts',(-1.02725604518277,0.648203827608334,
-2.42682890216184));
#364028=CARTESIAN_POINT('Ctrl Pts',(-0.824211659423609,0.892796064601774,
-2.48745940373019));
#364029=CARTESIAN_POINT('Ctrl Pts',(-0.564191142051916,1.07560808882016,
-2.54808760329284));
#364030=CARTESIAN_POINT('Ctrl Pts',(-0.268030403610479,1.18472901687534,
-2.60805895542665));
#364031=CARTESIAN_POINT('Ctrl Pts',(0.0484964956129267,1.21410782343574,
-2.66868935921047));
#364032=CARTESIAN_POINT('Ctrl Pts',(0.361626396132377,1.15951315047799,
-2.72931761037603));
#364033=CARTESIAN_POINT('Ctrl Pts',(0.648203803824844,1.0272560382112,-2.78928895746987));
#364034=CARTESIAN_POINT('Ctrl Pts',(0.892796076188025,0.824211675103123,
-2.84991935728737));
#364035=CARTESIAN_POINT('Ctrl Pts',(1.07560808862158,0.56419113400383,-2.91054761072926));
#364036=CARTESIAN_POINT('Ctrl Pts',(1.18472901588199,0.26803040550146,-2.97051895749492));
#364037=CARTESIAN_POINT('Ctrl Pts',(1.21410782431058,-0.0484964950668307,
-3.03114935724649));
#364038=CARTESIAN_POINT('Ctrl Pts',(1.15951315008857,-0.361626396645578,
-3.09177761073831));
#364039=CARTESIAN_POINT('Ctrl Pts',(1.02725603829716,-0.6482038036989,-3.15174895749339));
#364040=CARTESIAN_POINT('Ctrl Pts',(0.824211675135244,-0.892796076188428,
-3.21237935724692));
#364041=CARTESIAN_POINT('Ctrl Pts',(0.564191133978922,-1.07560808862653,
-3.27300761073802));
#364042=CARTESIAN_POINT('Ctrl Pts',(0.268030405508416,-1.18472901588096,
-3.33297895749366));
#364043=CARTESIAN_POINT('Ctrl Pts',(-0.0484964950686988,-1.21410782431092,
-3.39360935724675));
#364044=CARTESIAN_POINT('Ctrl Pts',(-0.361626396644909,-1.15951315008879,
-3.45423761073805));
#364045=CARTESIAN_POINT('Ctrl Pts',(-0.648203803698724,-1.02725603829705,
-3.51420895749367));
#364046=CARTESIAN_POINT('Ctrl Pts',(-0.89279607618879,-0.824211675135025,
-3.57483935724674));
#364047=CARTESIAN_POINT('Ctrl Pts',(-1.07560808862643,-0.564191133979103,
-3.63546761073801));
#364048=CARTESIAN_POINT('Ctrl Pts',(-1.18472901588094,-0.26803040550839,
-3.6954389574937));
#364049=CARTESIAN_POINT('Ctrl Pts',(-1.21410782431094,0.0484964950687397,
-3.75606935724672));
#364050=CARTESIAN_POINT('Ctrl Pts',(-1.1595131500888,0.361626396644898,
-3.81669761073803));
#364051=CARTESIAN_POINT('Ctrl Pts',(-1.02725603829704,0.648203803698727,
-3.87666895749368));
#364052=CARTESIAN_POINT('Ctrl Pts',(-0.824211675135021,0.892796076188792,
-3.93729935724673));
#364053=CARTESIAN_POINT('Ctrl Pts',(-0.564191133979095,1.07560808862643,
-3.99792761073801));
#364054=CARTESIAN_POINT('Ctrl Pts',(-0.268030405508389,1.18472901588092,
-4.05789895749373));
#364055=CARTESIAN_POINT('Ctrl Pts',(0.0484964950687464,1.21410782431094,
-4.11852935724671));
#364056=CARTESIAN_POINT('Ctrl Pts',(0.3616263966449,1.15951315008879,-4.17915761073805));
#364057=CARTESIAN_POINT('Ctrl Pts',(0.648203803698728,1.02725603829704,
-4.23912895749368));
#364058=CARTESIAN_POINT('Ctrl Pts',(0.892796076188791,0.824211675135014,
-4.29975935724674));
#364059=CARTESIAN_POINT('Ctrl Pts',(1.07560808862644,0.564191133979099,
-4.36038761073799));
#364060=CARTESIAN_POINT('Ctrl Pts',(1.18472901588094,0.268030405508375,
-4.42035895749369));
#364061=CARTESIAN_POINT('Ctrl Pts',(1.21410782431093,-0.0484964950687469,
-4.48098935724673));
#364062=CARTESIAN_POINT('Ctrl Pts',(1.15951315008879,-0.361626396644902,
-4.54161761073803));
#364063=CARTESIAN_POINT('Ctrl Pts',(1.02725603829703,-0.648203803698725,
-4.6015889574937));
#364064=CARTESIAN_POINT('Ctrl Pts',(0.824211675135013,-0.892796076188798,
-4.66221935724673));
#364065=CARTESIAN_POINT('Ctrl Pts',(0.564191133979094,-1.07560808862644,
-4.722847610738));
#364066=CARTESIAN_POINT('Ctrl Pts',(0.268030405508374,-1.18472901588094,
-4.7828189574937));
#364067=CARTESIAN_POINT('Ctrl Pts',(-0.04849649506876,-1.21410782431095,
-4.84344935724668));
#364068=CARTESIAN_POINT('Ctrl Pts',(-0.361626396644897,-1.15951315008877,
-4.90407761073806));
#364069=CARTESIAN_POINT('Ctrl Pts',(-0.648203803698715,-1.02725603829702,
-4.96404895749372));
#364070=CARTESIAN_POINT('Ctrl Pts',(-0.892796076188803,-0.824211675135015,
-5.02467935724671));
#364071=CARTESIAN_POINT('Ctrl Pts',(-1.07560808862644,-0.564191133979088,
-5.085307610738));
#364072=CARTESIAN_POINT('Ctrl Pts',(-1.18472901588092,-0.268030405508372,
-5.14527895749374));
#364073=CARTESIAN_POINT('Ctrl Pts',(-1.21410782431095,0.0484964950687572,
-5.20590935724669));
#364074=CARTESIAN_POINT('Ctrl Pts',(-1.1595131500888,0.361626396644921,
-5.26653761073799));
#364075=CARTESIAN_POINT('Ctrl Pts',(-1.02725603829702,0.64820380369872,
-5.32650895749373));
#364076=CARTESIAN_POINT('Ctrl Pts',(-0.824211675135014,0.892796076188816,
-5.38713935724669));
#364077=CARTESIAN_POINT('Ctrl Pts',(-0.564191133979076,1.07560808862641,
-5.44776761073806));
#364078=CARTESIAN_POINT('Ctrl Pts',(-0.268030405508379,1.18472901588095,
-5.50773895749365));
#364079=CARTESIAN_POINT('Ctrl Pts',(0.0484964950687955,1.21410782431095,
-5.56836935724668));
#364080=CARTESIAN_POINT('Ctrl Pts',(0.361626396644923,1.15951315008874,
-5.62899761073811));
#364081=CARTESIAN_POINT('Ctrl Pts',(0.648203803698529,1.02725603829711,
-5.68896895749371));
#364082=CARTESIAN_POINT('Ctrl Pts',(0.892796076189156,0.824211675134774,
-5.74959935724652));
#364083=CARTESIAN_POINT('Ctrl Pts',(1.07560808862635,0.564191133979143,
-5.81022761073827));
#364084=CARTESIAN_POINT('Ctrl Pts',(1.18472901588091,0.268030405509044,
-5.87019895749336));
#364085=CARTESIAN_POINT('Ctrl Pts',(1.2141078243105,-0.0484964950705043,
-5.93082935724695));
#364086=CARTESIAN_POINT('Ctrl Pts',(1.15951315009036,-0.361626396638523,
-5.99145761073686));
#364087=CARTESIAN_POINT('Ctrl Pts',(1.02725603828656,-0.648203803720622,
-6.05142895750248));
#364088=CARTESIAN_POINT('Ctrl Pts',(0.824211675164934,-0.892796076174764,
-6.11205935720599));
#364089=CARTESIAN_POINT('Ctrl Pts',(0.564191134059871,-1.07560808852829,
-6.17268761076101));
#364090=CARTESIAN_POINT('Ctrl Pts',(0.268030404959908,-1.18472901600022,
-6.23265895786053));
#364091=CARTESIAN_POINT('Ctrl Pts',(-0.048496494303855,-1.21410782509991,
-6.29328935527559));
#364092=CARTESIAN_POINT('Ctrl Pts',(-0.361626395111129,-1.15951314891753,
-6.35391761278417));
#364093=CARTESIAN_POINT('Ctrl Pts',(-0.648203807785757,-1.02725603400328,
-6.41388896506857));
#364094=CARTESIAN_POINT('Ctrl Pts',(-0.892796086148053,-0.82421169457497,
-6.47451931057689));
#364095=CARTESIAN_POINT('Ctrl Pts',(-1.0756080601232,-0.564191117561312,
-6.53514766561185));
#364096=CARTESIAN_POINT('Ctrl Pts',(-1.18472898053544,-0.268030410347432,
-6.59511906407632));
#364097=CARTESIAN_POINT('Ctrl Pts',(-1.21410817056974,0.0484965775982433,
-6.65574860156863));
#364098=CARTESIAN_POINT('Ctrl Pts',(-1.15951264802113,0.361626359829526,
-6.71637855817043));
#364099=CARTESIAN_POINT('Ctrl Pts',(-1.02725631549215,0.648202679709777,
-6.77634998994504));
#364100=CARTESIAN_POINT('Ctrl Pts',(-0.824212514048729,0.89279989750689,
-6.83697046026166));
#364101=CARTESIAN_POINT('Ctrl Pts',(-0.564185827571163,1.07561000588125,
-6.89761936594616));
#364102=CARTESIAN_POINT('Ctrl Pts',(-0.268055236457238,1.1847006164406,
-6.95758396792716));
#364103=CARTESIAN_POINT('Ctrl Pts',(0.0485472352404887,1.2142038916925,
-7.01813896161907));
#364104=CARTESIAN_POINT('Ctrl Pts',(0.361655804485534,1.15924149264237,
-7.07893382111904));
#364105=CARTESIAN_POINT('Ctrl Pts',(0.6478968782727,1.02825270748,-7.1387952204064));
#364106=CARTESIAN_POINT('Ctrl Pts',(0.893414088159582,0.820656810820771,
-7.19914743650299));
#364107=CARTESIAN_POINT('Ctrl Pts',(1.07501647976632,0.576321349623175,
-7.26054245691513));
#364108=CARTESIAN_POINT('Ctrl Pts',(1.18621324528802,0.224452404214759,
-7.3192609169548));
#364109=CARTESIAN_POINT('Ctrl Pts',(1.20016374408797,0.152327073866745,
-7.36128002094695));
#364110=CARTESIAN_POINT('Ctrl Pts',(1.20016374408796,-0.0349890780536599,
-7.37928962624155));
#364111=CARTESIAN_POINT('Ctrl Pts',(1.19994860179671,0.0349330361207006,
-2.22019720516939));
#364112=CARTESIAN_POINT('Ctrl Pts',(1.19994860179671,-0.126746617464705,
-2.23574197648456));
#364113=CARTESIAN_POINT('Ctrl Pts',(1.18628451104366,-0.235287042882826,
-2.2810964912132));
#364114=CARTESIAN_POINT('Ctrl Pts',(1.07477771342961,-0.573169099315595,
-2.33867755519319));
#364115=CARTESIAN_POINT('Ctrl Pts',(0.893209191596192,-0.821391071780957,
-2.40041325450729));
#364116=CARTESIAN_POINT('Ctrl Pts',(0.647719578695754,-1.02788019949386,
-2.46067439994995));
#364117=CARTESIAN_POINT('Ctrl Pts',(0.361523604188232,-1.15911171219588,
-2.52056034931245));
#364118=CARTESIAN_POINT('Ctrl Pts',(0.0484713603287608,-1.21397018964645,
-2.58134810525369));
#364119=CARTESIAN_POINT('Ctrl Pts',(-0.26807499252822,-1.18447453220047,
-2.64190541780525));
#364120=CARTESIAN_POINT('Ctrl Pts',(-0.564145022724671,-1.07538119354467,
-2.70186948165707));
#364121=CARTESIAN_POINT('Ctrl Pts',(-0.82411227040745,-0.892592747940269,
-2.76251800818134));
#364122=CARTESIAN_POINT('Ctrl Pts',(-1.02710741719481,-0.648025648702113,
-2.82313903087394));
#364123=CARTESIAN_POINT('Ctrl Pts',(-1.15932278442025,-0.361494315792975,
-2.88311038111178));
#364124=CARTESIAN_POINT('Ctrl Pts',(-1.21389060301799,-0.0484207535259056,
-2.94373983918878));
#364125=CARTESIAN_POINT('Ctrl Pts',(-1.18449856839689,0.268050248144059,
-3.00436996521972));
#364126=CARTESIAN_POINT('Ctrl Pts',(-1.0753804241319,0.564150242879215,
-3.06434127064474));
#364127=CARTESIAN_POINT('Ctrl Pts',(-0.892588631186338,0.824111463629319,
-3.12496913072614));
#364128=CARTESIAN_POINT('Ctrl Pts',(-0.648026852820059,1.02710713661446,
-3.18560006416148));
#364129=CARTESIAN_POINT('Ctrl Pts',(-0.361494335707408,1.15932328272349,
-3.24557132342766));
#364130=CARTESIAN_POINT('Ctrl Pts',(-0.0484206753242147,1.21389025844596,
-3.30619908602272));
#364131=CARTESIAN_POINT('Ctrl Pts',(0.268050244650624,1.18449860355023,
-3.36683007137514));
#364132=CARTESIAN_POINT('Ctrl Pts',(0.564150258467979,1.07538045277468,
-3.42680132544561));
#364133=CARTESIAN_POINT('Ctrl Pts',(0.824111444426381,0.892588621200653,
-3.48742908409296));
#364134=CARTESIAN_POINT('Ctrl Pts',(1.02710714086036,0.648026848734914,
-3.54806007173318));
#364135=CARTESIAN_POINT('Ctrl Pts',(1.15932328389686,0.361494337262554,
-3.60803132546964));
#364136=CARTESIAN_POINT('Ctrl Pts',(1.21389025765669,0.0484206760863054,
-3.66865908405205));
#364137=CARTESIAN_POINT('Ctrl Pts',(1.18449860343075,-0.268050245199621,
-3.72929007174227));
#364138=CARTESIAN_POINT('Ctrl Pts',(1.07538045287309,-0.564150258386447,
-3.78926132546809));
#364139=CARTESIAN_POINT('Ctrl Pts',(0.892588621215019,-0.824111444396376,
-3.84988908405249));
#364140=CARTESIAN_POINT('Ctrl Pts',(0.648026848712835,-1.02710714087089,
-3.91052007174198));
#364141=CARTESIAN_POINT('Ctrl Pts',(0.361494337268959,-1.15932328389524,
-3.97049132546837));
#364142=CARTESIAN_POINT('Ctrl Pts',(0.0484206760845926,-1.21389025765713,
-4.03111908405232));
#364143=CARTESIAN_POINT('Ctrl Pts',(-0.268050245198952,-1.18449860343081,
-4.09175007174202));
#364144=CARTESIAN_POINT('Ctrl Pts',(-0.564150258386389,-1.07538045287319,
-4.15172132546838));
#364145=CARTESIAN_POINT('Ctrl Pts',(-0.82411144439661,-0.892588621214665,
-4.2123490840523));
#364146=CARTESIAN_POINT('Ctrl Pts',(-1.0271071408708,-0.648026848713027,
-4.27298007174198));
#364147=CARTESIAN_POINT('Ctrl Pts',(-1.15932328389526,-0.361494337268938,
-4.33295132546841));
#364148=CARTESIAN_POINT('Ctrl Pts',(-1.21389025765712,-0.0484206760845532,
-4.39357908405229));
#364149=CARTESIAN_POINT('Ctrl Pts',(-1.1844986034308,0.268050245198939,
-4.45421007174199));
#364150=CARTESIAN_POINT('Ctrl Pts',(-1.07538045287319,0.564150258386394,
-4.51418132546839));
#364151=CARTESIAN_POINT('Ctrl Pts',(-0.892588621214658,0.82411144439661,
-4.5748090840523));
#364152=CARTESIAN_POINT('Ctrl Pts',(-0.648026848713022,1.0271071408708,
-4.63544007174198));
#364153=CARTESIAN_POINT('Ctrl Pts',(-0.361494337268941,1.15932328389527,
-4.69541132546844));
#364154=CARTESIAN_POINT('Ctrl Pts',(-0.0484206760845442,1.21389025765711,
-4.75603908405227));
#364155=CARTESIAN_POINT('Ctrl Pts',(0.268050245198942,1.18449860343081,
-4.81667007174201));
#364156=CARTESIAN_POINT('Ctrl Pts',(0.564150258386395,1.07538045287318,
-4.87664132546839));
#364157=CARTESIAN_POINT('Ctrl Pts',(0.824111444396615,0.892588621214655,
-4.9372690840523));
#364158=CARTESIAN_POINT('Ctrl Pts',(1.02710714087079,0.648026848713006,
-4.99790007174195));
#364159=CARTESIAN_POINT('Ctrl Pts',(1.15932328389525,0.361494337268927,
-5.0578713254684));
#364160=CARTESIAN_POINT('Ctrl Pts',(1.21389025765711,0.0484206760845428,
-5.11849908405229));
#364161=CARTESIAN_POINT('Ctrl Pts',(1.1844986034308,-0.268050245198941,
-5.179130071742));
#364162=CARTESIAN_POINT('Ctrl Pts',(1.07538045287319,-0.5641502583864,-5.2391013254684));
#364163=CARTESIAN_POINT('Ctrl Pts',(0.892588621214648,-0.824111444396615,
-5.29972908405229));
#364164=CARTESIAN_POINT('Ctrl Pts',(0.648026848713012,-1.0271071408708,
-5.36036007174197));
#364165=CARTESIAN_POINT('Ctrl Pts',(0.361494337268925,-1.15932328389526,
-5.42033132546841));
#364166=CARTESIAN_POINT('Ctrl Pts',(0.0484206760845338,-1.21389025765709,
-5.48095908405224));
#364167=CARTESIAN_POINT('Ctrl Pts',(-0.268050245198938,-1.18449860343081,
-5.54159007174203));
#364168=CARTESIAN_POINT('Ctrl Pts',(-0.564150258386406,-1.0753804528732,
-5.60156132546843));
#364169=CARTESIAN_POINT('Ctrl Pts',(-0.824111444396613,-0.89258862121464,
-5.66218908405228));
#364170=CARTESIAN_POINT('Ctrl Pts',(-1.02710714087079,-0.648026848713008,
-5.72282007174197));
#364171=CARTESIAN_POINT('Ctrl Pts',(-1.15932328389528,-0.36149433726893,
-5.78279132546845));
#364172=CARTESIAN_POINT('Ctrl Pts',(-1.2138902576571,-0.0484206760845329,
-5.84341908405225));
#364173=CARTESIAN_POINT('Ctrl Pts',(-1.18449860343078,0.268050245198954,
-5.90405007174196));
#364174=CARTESIAN_POINT('Ctrl Pts',(-1.07538045287319,0.564150258386408,
-5.96402132546844));
#364175=CARTESIAN_POINT('Ctrl Pts',(-0.892588621214629,0.824111444396606,
-6.02464908405225));
#364176=CARTESIAN_POINT('Ctrl Pts',(-0.64802684871302,1.02710714087081,
-6.08528007174203));
#364177=CARTESIAN_POINT('Ctrl Pts',(-0.361494337268917,1.15932328389523,
-6.14525132546836));
#364178=CARTESIAN_POINT('Ctrl Pts',(-0.048420676084498,1.21389025765709,
-6.20587908405224));
#364179=CARTESIAN_POINT('Ctrl Pts',(0.268050245198975,1.18449860343083,
-6.26651007174208));
#364180=CARTESIAN_POINT('Ctrl Pts',(0.564150258386226,1.07538045287327,
-6.32648132546841));
#364181=CARTESIAN_POINT('Ctrl Pts',(0.824111444396827,0.892588621214275,
-6.38710908405208));
#364182=CARTESIAN_POINT('Ctrl Pts',(1.0271071408709,0.648026848713156,-6.44774007174223));
#364183=CARTESIAN_POINT('Ctrl Pts',(1.159323283895,0.361494337269589,-6.50771132546807));
#364184=CARTESIAN_POINT('Ctrl Pts',(1.21389025765673,0.0484206760826282,
-6.56833908405251));
#364185=CARTESIAN_POINT('Ctrl Pts',(1.18449860343187,-0.268050245192022,
-6.62897007174084));
#364186=CARTESIAN_POINT('Ctrl Pts',(1.07538045286828,-0.564150258411146,
-6.68894132547714));
#364187=CARTESIAN_POINT('Ctrl Pts',(0.892588621213993,-0.824111444364615,
-6.74956908401155));
#364188=CARTESIAN_POINT('Ctrl Pts',(0.648026848838496,-1.0271071407854,
-6.81020007176602));
#364189=CARTESIAN_POINT('Ctrl Pts',(0.361494336755823,-1.1593232842844,
-6.87017132583052));
#364190=CARTESIAN_POINT('Ctrl Pts',(0.0484206766338695,-1.2138902567815,
-6.93079908208711));
#364191=CARTESIAN_POINT('Ctrl Pts',(-0.268050243328471,-1.18449860442843,
-6.99143007381518));
#364192=CARTESIAN_POINT('Ctrl Pts',(-0.564150266443273,-1.07538045302616,
-7.05140133291083));
#364193=CARTESIAN_POINT('Ctrl Pts',(-0.824111428662813,-0.892588609834598,
-7.11202903755537));
#364194=CARTESIAN_POINT('Ctrl Pts',(-1.02710714802879,-0.648026871740004,
-7.17266012714546));
#364195=CARTESIAN_POINT('Ctrl Pts',(-1.15932333812035,-0.361494339370128,
-7.23263142938285));
#364196=CARTESIAN_POINT('Ctrl Pts',(-1.21388994830272,-0.048420558641127,
-7.29325833250989));
#364197=CARTESIAN_POINT('Ctrl Pts',(-1.18449897688191,0.268050252868152,
-7.3538910230542));
#364198=CARTESIAN_POINT('Ctrl Pts',(-1.07538131032931,0.564149776786355,
-7.41386233272661));
#364199=CARTESIAN_POINT('Ctrl Pts',(-0.89258382755218,0.824110299740277,
-7.47448020435212));
#364200=CARTESIAN_POINT('Ctrl Pts',(-0.648027824318076,1.02711576339274,
-7.53513199456933));
#364201=CARTESIAN_POINT('Ctrl Pts',(-0.361519103800307,1.1593054263198,
-7.59509558925458));
#364202=CARTESIAN_POINT('Ctrl Pts',(-0.048363558710048,1.21390597518738,
-7.65565075634608));
#364203=CARTESIAN_POINT('Ctrl Pts',(0.268072537684821,1.18437146807072,
-7.71644050362745));
#364204=CARTESIAN_POINT('Ctrl Pts',(0.563930411939142,1.07613883654808,
-7.77632820376135));
#364205=CARTESIAN_POINT('Ctrl Pts',(0.82426225220675,0.889715887308659,
-7.83657609568004));
#364206=CARTESIAN_POINT('Ctrl Pts',(1.02783344969258,0.657090690457504,
-7.89836582380498));
#364207=CARTESIAN_POINT('Ctrl Pts',(1.15670010462145,0.329911052415485,
-7.95561053869555));
#364208=CARTESIAN_POINT('Ctrl Pts',(1.19983645566974,0.222219960564689,
-8.00127996772839));
#364209=CARTESIAN_POINT('Ctrl Pts',(1.19983645566973,0.0349038086442839,
-8.01928957302298));
#364210=CARTESIAN_POINT('Ctrl Pts',(1.99994859520949,0.0349419760186855,
-2.22027906663631));
#364211=CARTESIAN_POINT('Ctrl Pts',(1.99994859520949,-0.133161143166691,
-2.23644142527053));
#364212=CARTESIAN_POINT('Ctrl Pts',(1.96833139354662,-0.472425718114294,
-2.28062587414611));
#364213=CARTESIAN_POINT('Ctrl Pts',(1.77549751488388,-0.970378153502274,
-2.33932132964638));
#364214=CARTESIAN_POINT('Ctrl Pts',(1.46486827473653,-1.39599810161593,
-2.40041168228136));
#364215=CARTESIAN_POINT('Ctrl Pts',(1.0532724675317,-1.72756949816,-2.46064650153962));
#364216=CARTESIAN_POINT('Ctrl Pts',(0.570253827701872,-1.94116844962337,
-2.52097328730337));
#364217=CARTESIAN_POINT('Ctrl Pts',(0.0484505622703552,-2.02298787581022,
-2.58147196284819));
#364218=CARTESIAN_POINT('Ctrl Pts',(-0.476762817249676,-1.96636546213765,
-2.64190473727344));
#364219=CARTESIAN_POINT('Ctrl Pts',(-0.969389646094711,-1.7758542783469,
-2.70222141276452));
#364220=CARTESIAN_POINT('Ctrl Pts',(-1.39619412835269,-1.46471035101601,
-2.76268238970025));
#364221=CARTESIAN_POINT('Ctrl Pts',(-1.72755848446788,-1.05330968911041,
-2.8231370123091));
#364222=CARTESIAN_POINT('Ctrl Pts',(-1.94118200928605,-0.570259037663673,
-2.88345449584336));
#364223=CARTESIAN_POINT('Ctrl Pts',(-2.02296215046454,-0.0484473116516587,
-2.94390972032538));
#364224=CARTESIAN_POINT('Ctrl Pts',(-1.96637109382515,0.476765855935366,
-3.00436740295728));
#364225=CARTESIAN_POINT('Ctrl Pts',(-1.77585739520295,0.969389009874219,
-3.06468474103924));
#364226=CARTESIAN_POINT('Ctrl Pts',(-1.46470740175196,1.39619269138418,
-3.12513949735647));
#364227=CARTESIAN_POINT('Ctrl Pts',(-1.05331000180424,1.72755870986409,
-3.18559743702838));
#364228=CARTESIAN_POINT('Ctrl Pts',(-0.570259275444307,1.94118238224882,
-3.2459147561141));
#364229=CARTESIAN_POINT('Ctrl Pts',(-0.0484472107178668,2.02296183497224,
-3.30636948355066));
#364230=CARTESIAN_POINT('Ctrl Pts',(0.476765831354286,1.96637112545875,
-3.36682743921798));
#364231=CARTESIAN_POINT('Ctrl Pts',(0.969389026744113,1.77585742843582,
-3.42714475673536));
#364232=CARTESIAN_POINT('Ctrl Pts',(1.39619267971627,1.46470738191116,-3.48759948296635));
#364233=CARTESIAN_POINT('Ctrl Pts',(1.72755870948907,1.05331000492523,-3.54805743931225));
#364234=CARTESIAN_POINT('Ctrl Pts',(1.9411823845861,0.570259275622033,-3.60837475674778));
#364235=CARTESIAN_POINT('Ctrl Pts',(2.02296183383815,0.0484472105365179,
-3.66882948295392));
#364236=CARTESIAN_POINT('Ctrl Pts',(1.96637112555601,-0.476765831198158,
-3.72928743931407));
#364237=CARTESIAN_POINT('Ctrl Pts',(1.77585742848668,-0.969389026837108,
-3.78960475674772));
#364238=CARTESIAN_POINT('Ctrl Pts',(1.46470738188885,-1.39619267968778,
-3.85005948295395));
#364239=CARTESIAN_POINT('Ctrl Pts',(1.05331000493188,-1.72755870948857,
-3.910517439314));
#364240=CARTESIAN_POINT('Ctrl Pts',(0.570259275619007,-1.9411823845877,
-3.97083475674782));
#364241=CARTESIAN_POINT('Ctrl Pts',(0.0484472105373659,-2.02296183383781,
-4.03128948295388));
#364242=CARTESIAN_POINT('Ctrl Pts',(-0.476765831198311,-1.96637112555626,
-4.09174743931402));
#364243=CARTESIAN_POINT('Ctrl Pts',(-0.969389026837092,-1.77585742848654,
-4.15206475674782));
#364244=CARTESIAN_POINT('Ctrl Pts',(-1.39619267968775,-1.46470738188883,
-4.21251948295388));
#364245=CARTESIAN_POINT('Ctrl Pts',(-1.72755870948862,-1.05331000493188,
-4.27297743931401));
#364246=CARTESIAN_POINT('Ctrl Pts',(-1.94118238458768,-0.570259275619005,
-4.33329475674783));
#364247=CARTESIAN_POINT('Ctrl Pts',(-2.0229618338378,-0.0484472105373586,
-4.39374948295387));
#364248=CARTESIAN_POINT('Ctrl Pts',(-1.96637112555625,0.476765831198322,
-4.45420743931402));
#364249=CARTESIAN_POINT('Ctrl Pts',(-1.77585742848654,0.969389026837096,
-4.51452475674782));
#364250=CARTESIAN_POINT('Ctrl Pts',(-1.46470738188882,1.39619267968775,
-4.57497948295388));
#364251=CARTESIAN_POINT('Ctrl Pts',(-1.05331000493187,1.72755870948862,
-4.63543743931401));
#364252=CARTESIAN_POINT('Ctrl Pts',(-0.570259275619004,1.9411823845877,
-4.69575475674784));
#364253=CARTESIAN_POINT('Ctrl Pts',(-0.0484472105373471,2.0229618338378,
-4.75620948295387));
#364254=CARTESIAN_POINT('Ctrl Pts',(0.476765831198326,1.96637112555626,
-4.81666743931402));
#364255=CARTESIAN_POINT('Ctrl Pts',(0.969389026837101,1.77585742848653,
-4.87698475674782));
#364256=CARTESIAN_POINT('Ctrl Pts',(1.39619267968776,1.46470738188882,-4.93743948295388));
#364257=CARTESIAN_POINT('Ctrl Pts',(1.72755870948861,1.05331000493185,-4.997897439314));
#364258=CARTESIAN_POINT('Ctrl Pts',(1.94118238458768,0.570259275618993,
-5.05821475674782));
#364259=CARTESIAN_POINT('Ctrl Pts',(2.0229618338378,0.0484472105373451,
-5.11866948295387));
#364260=CARTESIAN_POINT('Ctrl Pts',(1.96637112555625,-0.476765831198331,
-5.17912743931402));
#364261=CARTESIAN_POINT('Ctrl Pts',(1.77585742848654,-0.969389026837107,
-5.23944475674783));
#364262=CARTESIAN_POINT('Ctrl Pts',(1.46470738188881,-1.39619267968776,
-5.29989948295387));
#364263=CARTESIAN_POINT('Ctrl Pts',(1.05331000493185,-1.72755870948862,
-5.36035743931401));
#364264=CARTESIAN_POINT('Ctrl Pts',(0.57025927561899,-1.94118238458768,
-5.42067475674783));
#364265=CARTESIAN_POINT('Ctrl Pts',(0.0484472105373359,-2.02296183383778,
-5.48112948295386));
#364266=CARTESIAN_POINT('Ctrl Pts',(-0.476765831198329,-1.96637112555626,
-5.54158743931402));
#364267=CARTESIAN_POINT('Ctrl Pts',(-0.96938902683712,-1.77585742848655,
-5.60190475674783));
#364268=CARTESIAN_POINT('Ctrl Pts',(-1.39619267968776,-1.4647073818888,
-5.66235948295387));
#364269=CARTESIAN_POINT('Ctrl Pts',(-1.72755870948862,-1.05331000493185,
-5.722817439314));
#364270=CARTESIAN_POINT('Ctrl Pts',(-1.9411823845877,-0.570259275618991,
-5.78313475674784));
#364271=CARTESIAN_POINT('Ctrl Pts',(-2.02296183383779,-0.0484472105373294,
-5.84358948295386));
#364272=CARTESIAN_POINT('Ctrl Pts',(-1.96637112555623,0.476765831198343,
-5.904047439314));
#364273=CARTESIAN_POINT('Ctrl Pts',(-1.77585742848654,0.969389026837124,
-5.96436475674784));
#364274=CARTESIAN_POINT('Ctrl Pts',(-1.46470738188879,1.39619267968775,
-6.02481948295386));
#364275=CARTESIAN_POINT('Ctrl Pts',(-1.05331000493186,1.72755870948864,
-6.08527743931403));
#364276=CARTESIAN_POINT('Ctrl Pts',(-0.57025927561896,1.94118238458767,
-6.14559475674781));
#364277=CARTESIAN_POINT('Ctrl Pts',(-0.0484472105373227,2.02296183383776,
-6.20604948295386));
#364278=CARTESIAN_POINT('Ctrl Pts',(0.476765831198343,1.96637112555631,
-6.26650743931404));
#364279=CARTESIAN_POINT('Ctrl Pts',(0.969389026837138,1.77585742848649,
-6.32682475674784));
#364280=CARTESIAN_POINT('Ctrl Pts',(1.39619267968763,1.4647073818887,-6.3872794829538));
#364281=CARTESIAN_POINT('Ctrl Pts',(1.72755870948896,1.05331000493196,-6.4477374393141));
#364282=CARTESIAN_POINT('Ctrl Pts',(1.94118238458724,0.570259275618813,
-6.50805475674775));
#364283=CARTESIAN_POINT('Ctrl Pts',(2.0229618338382,0.0484472105380158,
-6.56850948295382));
#364284=CARTESIAN_POINT('Ctrl Pts',(1.96637112555413,-0.47676583120083,
-6.62896743931409));
#364285=CARTESIAN_POINT('Ctrl Pts',(1.77585742849251,-0.969389026833344,
-6.68928475674954));
#364286=CARTESIAN_POINT('Ctrl Pts',(1.46470738188697,-1.39619267969199,
-6.74973948294137));
#364287=CARTESIAN_POINT('Ctrl Pts',(1.05331000488233,-1.72755870945149,
-6.81019743932769));
#364288=CARTESIAN_POINT('Ctrl Pts',(0.570259275809968,-1.94118238475938,
-6.87051475683913));
#364289=CARTESIAN_POINT('Ctrl Pts',(0.0484472101488399,-2.02296183330866,
-6.93096948236246));
#364290=CARTESIAN_POINT('Ctrl Pts',(-0.476765830732716,-1.96637112538019,
-6.99142743997978));
#364291=CARTESIAN_POINT('Ctrl Pts',(-0.969389027651612,-1.775857433288,
-7.05174475889683));
#364292=CARTESIAN_POINT('Ctrl Pts',(-1.39619267380615,-1.46470736293583,
-7.11219946872276));
#364293=CARTESIAN_POINT('Ctrl Pts',(-1.72755871231312,-1.05331002647757,
-7.1726574556236));
#364294=CARTESIAN_POINT('Ctrl Pts',(-1.94118244199894,-0.570259298778077,
-7.23297479041701));
#364295=CARTESIAN_POINT('Ctrl Pts',(-2.02296149561613,-0.0484470734163606,
-7.29342924947211));
#364296=CARTESIAN_POINT('Ctrl Pts',(-1.96637162260829,0.47676563992917,
-7.35388770608518));
#364297=CARTESIAN_POINT('Ctrl Pts',(-1.77585778550465,0.969389377563547,
-7.41420515419699));
#364298=CARTESIAN_POINT('Ctrl Pts',(-1.46470321414872,1.39619055347437,
-7.4746566054593));
#364299=CARTESIAN_POINT('Ctrl Pts',(-1.05331679189158,1.72756279918536,
-7.53512091909894));
#364300=CARTESIAN_POINT('Ctrl Pts',(-0.570256351317271,1.94118541096824,
-7.5954368568002));
#364301=CARTESIAN_POINT('Ctrl Pts',(-0.0484373346474795,2.02291433148142,
-7.65586848775589));
#364302=CARTESIAN_POINT('Ctrl Pts',(0.476753357889169,1.96647633924905,
-7.7163654145941));
#364303=CARTESIAN_POINT('Ctrl Pts',(0.969439733353148,1.77572407380791,
-7.7767079034587));
#364304=CARTESIAN_POINT('Ctrl Pts',(1.39587962475789,1.46484458461224,-7.83687735653918));
#364305=CARTESIAN_POINT('Ctrl Pts',(1.72854436163452,1.05253719801599,-7.89821617217114));
#364306=CARTESIAN_POINT('Ctrl Pts',(1.93848294702123,0.574209674581668,
-7.95584767975511));
#364307=CARTESIAN_POINT('Ctrl Pts',(1.99983638908382,0.21585245779268,-8.0021551741418));
#364308=CARTESIAN_POINT('Ctrl Pts',(1.99983638908381,0.0349322317806574,
-8.0195498399348));
#364309=CARTESIAN_POINT('Ctrl Pts',(2.79994858862227,0.0349509159166703,
-2.22036092810323));
#364310=CARTESIAN_POINT('Ctrl Pts',(2.79994858862227,-0.139575668868676,
-2.2371408740565));
#364311=CARTESIAN_POINT('Ctrl Pts',(2.75037827604958,-0.709564393345761,
-2.28015525707901));
#364312=CARTESIAN_POINT('Ctrl Pts',(2.47621731633814,-1.36758720768895,
-2.33996510409957));
#364313=CARTESIAN_POINT('Ctrl Pts',(2.03652735787686,-1.97060513145091,
-2.40041011005543));
#364314=CARTESIAN_POINT('Ctrl Pts',(1.45882535636765,-2.42725879682614,
-2.46061860312929));
#364315=CARTESIAN_POINT('Ctrl Pts',(0.778984051215511,-2.72322518705085,
-2.52138622529428));
#364316=CARTESIAN_POINT('Ctrl Pts',(0.0484297642119496,-2.83200556197398,
-2.58159582044269));
#364317=CARTESIAN_POINT('Ctrl Pts',(-0.685450641971131,-2.74825639207482,
-2.64190405674164));
#364318=CARTESIAN_POINT('Ctrl Pts',(-1.37463426946475,-2.47632736314912,
-2.70257334387197));
#364319=CARTESIAN_POINT('Ctrl Pts',(-1.96827598629794,-2.03682795409175,
-2.76284677121916));
#364320=CARTESIAN_POINT('Ctrl Pts',(-2.42800955174095,-1.45859372951871,
-2.82313499374427));
#364321=CARTESIAN_POINT('Ctrl Pts',(-2.72304123415184,-0.779023759534372,
-2.88379861057494));
#364322=CARTESIAN_POINT('Ctrl Pts',(-2.8320336979111,-0.048473869777412,
-2.94407960146198));
#364323=CARTESIAN_POINT('Ctrl Pts',(-2.74824361925341,0.685481463726674,
-3.00436484069483));
#364324=CARTESIAN_POINT('Ctrl Pts',(-2.47633436627399,1.37462777686922,
-3.06502821143375));
#364325=CARTESIAN_POINT('Ctrl Pts',(-2.03682617231757,1.96827391913905,
-3.1253098639868));
#364326=CARTESIAN_POINT('Ctrl Pts',(-1.45859315078841,2.42801028311372,
-3.18559480989526));
#364327=CARTESIAN_POINT('Ctrl Pts',(-0.779024215181206,2.72304148177415,
-3.24625818880055));
#364328=CARTESIAN_POINT('Ctrl Pts',(-0.048473746111519,2.83203341149851,
-3.30653988107861));
#364329=CARTESIAN_POINT('Ctrl Pts',(0.685481418057947,2.74824364736727,
-3.36682480706082));
#364330=CARTESIAN_POINT('Ctrl Pts',(1.37462779502025,2.47633440409695,-3.42748818802511));
#364331=CARTESIAN_POINT('Ctrl Pts',(1.96827391500616,2.03682614262167,-3.48776988183974));
#364332=CARTESIAN_POINT('Ctrl Pts',(2.42801027811778,1.45859316111554,-3.54805480689131));
#364333=CARTESIAN_POINT('Ctrl Pts',(2.72304148527533,0.779024213981512,
-3.60871818802593));
#364334=CARTESIAN_POINT('Ctrl Pts',(2.83203341001962,0.0484737449867304,
-3.66899988185579));
#364335=CARTESIAN_POINT('Ctrl Pts',(2.74824364768127,-0.685481417196696,
-3.72928480688587));
#364336=CARTESIAN_POINT('Ctrl Pts',(2.47633440410028,-1.37462779528777,
-3.78994818802735));
#364337=CARTESIAN_POINT('Ctrl Pts',(2.03682614256268,-1.96827391497919,
-3.85022988185542));
#364338=CARTESIAN_POINT('Ctrl Pts',(1.45859316115093,-2.42801027810626,
-3.91051480688602));
#364339=CARTESIAN_POINT('Ctrl Pts',(0.779024213969054,-2.72304148528015,
-3.97117818802726));
#364340=CARTESIAN_POINT('Ctrl Pts',(0.0484737449901392,-2.83203341001849,
-4.03145988185545));
#364341=CARTESIAN_POINT('Ctrl Pts',(-0.685481417197671,-2.74824364768172,
-4.09174480688602));
#364342=CARTESIAN_POINT('Ctrl Pts',(-1.3746277952878,-2.4763344040999,-4.15240818802725));
#364343=CARTESIAN_POINT('Ctrl Pts',(-1.96827391497889,-2.03682614256299,
-4.21268988185546));
#364344=CARTESIAN_POINT('Ctrl Pts',(-2.42801027810644,-1.45859316115073,
-4.27297480688604));
#364345=CARTESIAN_POINT('Ctrl Pts',(-2.72304148528011,-0.779024213969072,
-4.33363818802725));
#364346=CARTESIAN_POINT('Ctrl Pts',(-2.83203341001849,-0.0484737449901639,
-4.39391988185546));
#364347=CARTESIAN_POINT('Ctrl Pts',(-2.7482436476817,0.685481417197704,
-4.45420480688603));
#364348=CARTESIAN_POINT('Ctrl Pts',(-2.4763344040999,1.3746277952878,-4.51486818802725));
#364349=CARTESIAN_POINT('Ctrl Pts',(-2.03682614256298,1.96827391497889,
-4.57514988185546));
#364350=CARTESIAN_POINT('Ctrl Pts',(-1.45859316115072,2.42801027810644,
-4.63543480688604));
#364351=CARTESIAN_POINT('Ctrl Pts',(-0.779024213969067,2.72304148528013,
-4.69609818802723));
#364352=CARTESIAN_POINT('Ctrl Pts',(-0.04847374499015,2.83203341001848,
-4.75637988185547));
#364353=CARTESIAN_POINT('Ctrl Pts',(0.685481417197709,2.7482436476817,-4.81666480688603));
#364354=CARTESIAN_POINT('Ctrl Pts',(1.37462779528781,2.47633440409989,-4.87732818802725));
#364355=CARTESIAN_POINT('Ctrl Pts',(1.9682739149789,2.03682614256298,-4.93760988185546));
#364356=CARTESIAN_POINT('Ctrl Pts',(2.42801027810644,1.4585931611507,-4.99789480688605));
#364357=CARTESIAN_POINT('Ctrl Pts',(2.7230414852801,0.779024213969058,-5.05855818802725));
#364358=CARTESIAN_POINT('Ctrl Pts',(2.83203341001848,0.0484737449901475,
-5.11883988185546));
#364359=CARTESIAN_POINT('Ctrl Pts',(2.74824364768169,-0.685481417197721,
-5.17912480688604));
#364360=CARTESIAN_POINT('Ctrl Pts',(2.47633440409989,-1.37462779528781,
-5.23978818802725));
#364361=CARTESIAN_POINT('Ctrl Pts',(2.03682614256297,-1.9682739149789,-5.30006988185546));
#364362=CARTESIAN_POINT('Ctrl Pts',(1.45859316115069,-2.42801027810645,
-5.36035480688604));
#364363=CARTESIAN_POINT('Ctrl Pts',(0.779024213969056,-2.72304148528011,
-5.42101818802724));
#364364=CARTESIAN_POINT('Ctrl Pts',(0.0484737449901378,-2.83203341001847,
-5.48129988185548));
#364365=CARTESIAN_POINT('Ctrl Pts',(-0.685481417197721,-2.7482436476817,
-5.54158480688602));
#364366=CARTESIAN_POINT('Ctrl Pts',(-1.37462779528784,-2.4763344040999,
-5.60224818802724));
#364367=CARTESIAN_POINT('Ctrl Pts',(-1.9682739149789,-2.03682614256296,
-5.66252988185546));
#364368=CARTESIAN_POINT('Ctrl Pts',(-2.42801027810645,-1.45859316115069,
-5.72281480688604));
#364369=CARTESIAN_POINT('Ctrl Pts',(-2.72304148528013,-0.779024213969052,
-5.78347818802723));
#364370=CARTESIAN_POINT('Ctrl Pts',(-2.83203341001847,-0.0484737449901258,
-5.84375988185547));
#364371=CARTESIAN_POINT('Ctrl Pts',(-2.74824364768167,0.685481417197731,
-5.90404480688604));
#364372=CARTESIAN_POINT('Ctrl Pts',(-2.47633440409989,1.37462779528784,
-5.96470818802724));
#364373=CARTESIAN_POINT('Ctrl Pts',(-2.03682614256295,1.96827391497889,
-6.02498988185547));
#364374=CARTESIAN_POINT('Ctrl Pts',(-1.4585931611507,2.42801027810647,-6.08527480688602));
#364375=CARTESIAN_POINT('Ctrl Pts',(-0.779024213969003,2.7230414852801,
-6.14593818802726));
#364376=CARTESIAN_POINT('Ctrl Pts',(-0.0484737449901475,2.83203341001844,
-6.20621988185547));
#364377=CARTESIAN_POINT('Ctrl Pts',(0.685481417197711,2.74824364768178,
-6.266504806886));
#364378=CARTESIAN_POINT('Ctrl Pts',(1.37462779528805,2.4763344040997,-6.32716818802727));
#364379=CARTESIAN_POINT('Ctrl Pts',(1.96827391497844,2.03682614256313,-6.3874498818555));
#364380=CARTESIAN_POINT('Ctrl Pts',(2.42801027810703,1.45859316115076,-6.44773480688596));
#364381=CARTESIAN_POINT('Ctrl Pts',(2.72304148527948,0.779024213968036,
-6.50839818802743));
#364382=CARTESIAN_POINT('Ctrl Pts',(2.83203341001966,0.0484737449934034,
-6.56867988185514));
#364383=CARTESIAN_POINT('Ctrl Pts',(2.74824364767639,-0.685481417209638,
-6.62896480688735));
#364384=CARTESIAN_POINT('Ctrl Pts',(2.47633440411674,-1.37462779525554,
-6.68962818802195));
#364385=CARTESIAN_POINT('Ctrl Pts',(2.03682614255995,-1.96827391501936,
-6.74990988187118));
#364386=CARTESIAN_POINT('Ctrl Pts',(1.45859316092616,-2.42801027811759,
-6.81019480688936));
#364387=CARTESIAN_POINT('Ctrl Pts',(0.779024214864112,-2.72304148523437,
-6.87085818784773));
#364388=CARTESIAN_POINT('Ctrl Pts',(0.0484737436638102,-2.83203340983582,
-6.93113988263782));
#364389=CARTESIAN_POINT('Ctrl Pts',(-0.685481418136962,-2.74824364633194,
-6.99142480614438));
#364390=CARTESIAN_POINT('Ctrl Pts',(-1.37462778885995,-2.47633441354984,
-7.05208818488281));
#364391=CARTESIAN_POINT('Ctrl Pts',(-1.96827391894949,-2.03682611603706,
-7.11236989989014));
#364392=CARTESIAN_POINT('Ctrl Pts',(-2.42801027659746,-1.45859318121514,
-7.17265478410175));
#364393=CARTESIAN_POINT('Ctrl Pts',(-2.72304154587753,-0.779024258186026,
-7.23331815145116));
#364394=CARTESIAN_POINT('Ctrl Pts',(-2.83203304292954,-0.0484735881915938,
-7.29360016643431));
#364395=CARTESIAN_POINT('Ctrl Pts',(-2.74824426833468,0.685481026990187,
-7.35388438911616));
#364396=CARTESIAN_POINT('Ctrl Pts',(-2.47633426068,1.37462897834074,-7.41454797566736));
#364397=CARTESIAN_POINT('Ctrl Pts',(-2.03682260074525,1.96827080720847,
-7.47483300656648));
#364398=CARTESIAN_POINT('Ctrl Pts',(-1.45860575946508,2.42800983497797,
-7.53510984362855));
#364399=CARTESIAN_POINT('Ctrl Pts',(-0.778993598834234,2.72306539561668,
-7.59577812434582));
#364400=CARTESIAN_POINT('Ctrl Pts',(-0.0485111105849109,2.83192268777547,
-7.65608621916571));
#364401=CARTESIAN_POINT('Ctrl Pts',(0.685434178093518,2.74858121042738,
-7.71629032556075));
#364402=CARTESIAN_POINT('Ctrl Pts',(1.37494905476715,2.47530931106774,-7.77708760315606));
#364403=CARTESIAN_POINT('Ctrl Pts',(1.96749699730902,2.03997328191583,-7.83717861739831));
#364404=CARTESIAN_POINT('Ctrl Pts',(2.42925527357646,1.44798370557448,-7.89806652053729));
#364405=CARTESIAN_POINT('Ctrl Pts',(2.72026578942101,0.81850829674785,-7.95608482081467));
#364406=CARTESIAN_POINT('Ctrl Pts',(2.7998363224979,0.209484955020671,-8.00303038055522));
#364407=CARTESIAN_POINT('Ctrl Pts',(2.7998363224979,0.0349606549170308,
-8.01981010684662));
#364408=CARTESIAN_POINT('Ctrl Pts',(2.80005140479051,-0.0349419760186688,
-1.58036093336367));
#364409=CARTESIAN_POINT('Ctrl Pts',(2.80005140479051,-0.222315492003956,
-1.59837605395503));
#364410=CARTESIAN_POINT('Ctrl Pts',(2.7214217418683,-0.809145725726729,
-1.6432251028271));
#364411=CARTESIAN_POINT('Ctrl Pts',(2.4293855576505,-1.45019120570836,-1.70229805797781));
#364412=CARTESIAN_POINT('Ctrl Pts',(1.96768973634555,-2.03953853811049,
-1.7629395123984));
#364413=CARTESIAN_POINT('Ctrl Pts',(1.37507506915162,-2.47563743577604,
-1.8230967134397));
#364414=CARTESIAN_POINT('Ctrl Pts',(0.685513462117749,-2.74874432479135,
-1.88387667036327));
#364415=CARTESIAN_POINT('Ctrl Pts',(-0.0484811831405424,-2.83215111147164,
-1.94408480572724));
#364416=CARTESIAN_POINT('Ctrl Pts',(-0.779026681647449,-2.72327925825339,
-2.00439212797816));
#364417=CARTESIAN_POINT('Ctrl Pts',(-1.45869410662288,-2.42821024693195,
-2.0650608706179));
#364418=CARTESIAN_POINT('Ctrl Pts',(-2.03695498339253,-1.96844588111817,
-2.12533700840671));
#364419=CARTESIAN_POINT('Ctrl Pts',(-2.4765110806735,-1.3747587008243,-2.18562256240842));
#364420=CARTESIAN_POINT('Ctrl Pts',(-2.7484478409841,-0.685559860459645,
-2.24628623797644));
#364421=CARTESIAN_POINT('Ctrl Pts',(-2.83225060905395,0.048443263325025,
-2.30656987054029));
#364422=CARTESIAN_POINT('Ctrl Pts',(-2.72325825549342,0.779057613295582,
-2.36685238231703));
#364423=CARTESIAN_POINT('Ctrl Pts',(-2.42820998732486,1.45868136138043,
-2.4275158429718));
#364424=CARTESIAN_POINT('Ctrl Pts',(-1.96844920055485,2.03695852016992,
-2.48780013698524));
#364425=CARTESIAN_POINT('Ctrl Pts',(-1.37475744002027,2.4765112353038,-2.54808234902813));
#364426=CARTESIAN_POINT('Ctrl Pts',(-0.685560283084277,2.74844721593019,
-2.60874582079915));
#364427=CARTESIAN_POINT('Ctrl Pts',(0.0484434248256224,2.83225097648717,
-2.66903015426646));
#364428=CARTESIAN_POINT('Ctrl Pts',(0.7790575695397,2.72325819429533,-2.72931234606168));
#364429=CARTESIAN_POINT('Ctrl Pts',(1.45868134037711,2.42820998953338,-2.78997582004938));
#364430=CARTESIAN_POINT('Ctrl Pts',(2.0369585467678,1.96844919652417,-2.85026015503416));
#364431=CARTESIAN_POINT('Ctrl Pts',(2.47651122587901,1.37475744638445,-2.91054234588739));
#364432=CARTESIAN_POINT('Ctrl Pts',(2.74844721726047,0.68556028222042,-2.97120582005121));
#364433=CARTESIAN_POINT('Ctrl Pts',(2.8322509766735,-0.0484434261664062,
-3.03149015505023));
#364434=CARTESIAN_POINT('Ctrl Pts',(2.7232581943391,-0.779057568642653,
-3.09177234588191));
#364435=CARTESIAN_POINT('Ctrl Pts',(2.42820998952435,-1.45868134060022,
-3.15243582005264));
#364436=CARTESIAN_POINT('Ctrl Pts',(1.9684491964829,-2.03695854677124,-3.21272015504985));
#364437=CARTESIAN_POINT('Ctrl Pts',(1.37475744641701,-2.4765112258619,-3.27300234588205));
#364438=CARTESIAN_POINT('Ctrl Pts',(0.685560282208511,-2.74844721726587,
-3.33366582005255));
#364439=CARTESIAN_POINT('Ctrl Pts',(-0.0484434261631521,-2.83225097667228,
-3.39395015504989));
#364440=CARTESIAN_POINT('Ctrl Pts',(-0.779057568643627,-2.7232581943397,
-3.45423234588206));
#364441=CARTESIAN_POINT('Ctrl Pts',(-1.45868134060013,-2.42820998952376,
-3.51489582005254));
#364442=CARTESIAN_POINT('Ctrl Pts',(-2.03695854677107,-1.96844919648335,
-3.57518015504989));
#364443=CARTESIAN_POINT('Ctrl Pts',(-2.47651122586207,-1.3747574464168,
-3.63546234588207));
#364444=CARTESIAN_POINT('Ctrl Pts',(-2.74844721726579,-0.685560282208525,
-3.69612582005254));
#364445=CARTESIAN_POINT('Ctrl Pts',(-2.83225097667231,0.0484434261631291,
-3.7564101550499));
#364446=CARTESIAN_POINT('Ctrl Pts',(-2.7232581943397,0.779057568643663,
-3.81669234588207));
#364447=CARTESIAN_POINT('Ctrl Pts',(-2.42820998952376,1.45868134060013,
-3.87735582005254));
#364448=CARTESIAN_POINT('Ctrl Pts',(-1.96844919648335,2.03695854677107,
-3.9376401550499));
#364449=CARTESIAN_POINT('Ctrl Pts',(-1.37475744641679,2.47651122586208,
-3.99792234588207));
#364450=CARTESIAN_POINT('Ctrl Pts',(-0.685560282208515,2.74844721726578,
-4.05858582005252));
#364451=CARTESIAN_POINT('Ctrl Pts',(0.0484434261631405,2.83225097667232,
-4.1188701550499));
#364452=CARTESIAN_POINT('Ctrl Pts',(0.779057568643667,2.72325819433969,
-4.17915234588206));
#364453=CARTESIAN_POINT('Ctrl Pts',(1.45868134060014,2.42820998952375,-4.23981582005254));
#364454=CARTESIAN_POINT('Ctrl Pts',(2.03695854677108,1.96844919648334,-4.30010015504989));
#364455=CARTESIAN_POINT('Ctrl Pts',(2.47651122586209,1.37475744641679,-4.36038234588208));
#364456=CARTESIAN_POINT('Ctrl Pts',(2.74844721726579,0.685560282208506,
-4.42104582005254));
#364457=CARTESIAN_POINT('Ctrl Pts',(2.8322509766723,-0.0484434261631421,
-4.4813301550499));
#364458=CARTESIAN_POINT('Ctrl Pts',(2.72325819433969,-0.779057568643682,
-4.54161234588207));
#364459=CARTESIAN_POINT('Ctrl Pts',(2.42820998952373,-1.45868134060014,
-4.60227582005254));
#364460=CARTESIAN_POINT('Ctrl Pts',(1.96844919648334,-2.03695854677108,
-4.6625601550499));
#364461=CARTESIAN_POINT('Ctrl Pts',(1.37475744641678,-2.47651122586209,
-4.72284234588207));
#364462=CARTESIAN_POINT('Ctrl Pts',(0.685560282208503,-2.74844721726579,
-4.78350582005254));
#364463=CARTESIAN_POINT('Ctrl Pts',(-0.0484434261631558,-2.83225097667233,
-4.84379015504992));
#364464=CARTESIAN_POINT('Ctrl Pts',(-0.77905756864368,-2.72325819433967,
-4.90407234588205));
#364465=CARTESIAN_POINT('Ctrl Pts',(-1.45868134060014,-2.42820998952372,
-4.96473582005253));
#364466=CARTESIAN_POINT('Ctrl Pts',(-2.03695854677109,-1.96844919648334,
-5.0250201550499));
#364467=CARTESIAN_POINT('Ctrl Pts',(-2.47651122586209,-1.37475744641677,
-5.08530234588207));
#364468=CARTESIAN_POINT('Ctrl Pts',(-2.74844721726577,-0.685560282208494,
-5.14596582005252));
#364469=CARTESIAN_POINT('Ctrl Pts',(-2.83225097667232,0.0484434261631642,
-5.20625015504991));
#364470=CARTESIAN_POINT('Ctrl Pts',(-2.72325819433969,0.779057568643699,
-5.26653234588207));
#364471=CARTESIAN_POINT('Ctrl Pts',(-2.42820998952371,1.45868134060015,
-5.32719582005253));
#364472=CARTESIAN_POINT('Ctrl Pts',(-1.96844919648334,2.0369585467711,-5.38748015504991));
#364473=CARTESIAN_POINT('Ctrl Pts',(-1.37475744641676,2.47651122586207,
-5.44776234588206));
#364474=CARTESIAN_POINT('Ctrl Pts',(-0.685560282208465,2.74844721726582,
-5.50842582005256));
#364475=CARTESIAN_POINT('Ctrl Pts',(0.0484434261631459,2.8322509766723,
-5.56871015504991));
#364476=CARTESIAN_POINT('Ctrl Pts',(0.77905756864366,2.7232581943397,-5.62899234588203));
#364477=CARTESIAN_POINT('Ctrl Pts',(1.45868134060035,2.42820998952354,-5.68965582005256));
#364478=CARTESIAN_POINT('Ctrl Pts',(2.03695854677077,1.96844919648363,-5.74994015504994));
#364479=CARTESIAN_POINT('Ctrl Pts',(2.47651122586247,1.37475744641675,-5.81022234588199));
#364480=CARTESIAN_POINT('Ctrl Pts',(2.74844721726539,0.68556028220749,-5.87088582005272));
#364481=CARTESIAN_POINT('Ctrl Pts',(2.83225097667343,-0.0484434261597295,
-5.93117015504957));
#364482=CARTESIAN_POINT('Ctrl Pts',(2.72325819433488,-0.779057568656138,
-5.99145234588337));
#364483=CARTESIAN_POINT('Ctrl Pts',(2.42820998953502,-1.45868134056502,
-6.05211582004729));
#364484=CARTESIAN_POINT('Ctrl Pts',(1.96844919651089,-2.03695854682948,
-6.11240015506561));
#364485=CARTESIAN_POINT('Ctrl Pts',(1.37475744614754,-2.47651122586056,
-6.17268234588436));
#364486=CARTESIAN_POINT('Ctrl Pts',(0.685560283068197,-2.7484472169499,
-6.2333458198777));
#364487=CARTESIAN_POINT('Ctrl Pts',(-0.0484434272739145,-2.83225097815536,
-6.29363015582641));
#364488=CARTESIAN_POINT('Ctrl Pts',(-0.779057569919619,-2.72325819081683,
-6.35391234511296));
#364489=CARTESIAN_POINT('Ctrl Pts',(-1.45868133020244,-2.42820999454269,
-6.41457581704206));
#364490=CARTESIAN_POINT('Ctrl Pts',(-2.03695857643473,-1.96844920071866,
-6.47486017290601));
#364491=CARTESIAN_POINT('Ctrl Pts',(-2.47651118869187,-1.37475742725566,
-6.53514232258922));
#364492=CARTESIAN_POINT('Ctrl Pts',(-2.74844718829262,-0.685560328345768,
-6.59580578606602));
#364493=CARTESIAN_POINT('Ctrl Pts',(-2.83225126519656,0.0484435449931018,
-6.65609043578674));
#364494=CARTESIAN_POINT('Ctrl Pts',(-2.72325793947389,0.779057145346554,
-6.71637192313681));
#364495=CARTESIAN_POINT('Ctrl Pts',(-2.42820926584284,1.45868183876673,
-6.77703563697173));
#364496=CARTESIAN_POINT('Ctrl Pts',(-1.9684512872418,2.03696056375976,-6.83732324720959));
#364497=CARTESIAN_POINT('Ctrl Pts',(-1.37476376271817,2.47650348514813,
-6.89759727195412));
#364498=CARTESIAN_POINT('Ctrl Pts',(-0.685529731491166,2.74846279478609,
-6.95826629062831));
#364499=CARTESIAN_POINT('Ctrl Pts',(0.0483996833656258,2.8322123503721,
-7.01857521801487));
#364500=CARTESIAN_POINT('Ctrl Pts',(0.779017444894231,2.72348202273134,
-7.07878068295039));
#364501=CARTESIAN_POINT('Ctrl Pts',(1.45891552110071,2.42730834706515,-7.13956566066343));
#364502=CARTESIAN_POINT('Ctrl Pts',(2.03664883326185,1.97134324740292,-7.19970870776557));
#364503=CARTESIAN_POINT('Ctrl Pts',(2.47643830365019,1.36561422989075,-7.2603969994144));
#364504=CARTESIAN_POINT('Ctrl Pts',(2.74977893008757,0.719015851050413,
-7.31916157554443));
#364505=CARTESIAN_POINT('Ctrl Pts',(2.80016361091614,0.126800216505963,
-7.36426031277698));
#364506=CARTESIAN_POINT('Ctrl Pts',(2.80016361091613,-0.0349322317809129,
-7.37981016006518));
#364507=CARTESIAN_POINT('Ctrl Pts',(2.00005141137773,-0.0349509159166537,
-1.58027907189674));
#364508=CARTESIAN_POINT('Ctrl Pts',(2.00005141137773,-0.209477500702,-1.59705901785001));
#364509=CARTESIAN_POINT('Ctrl Pts',(1.93937485936534,-0.574981221086946,
-1.64398167301615));
#364510=CARTESIAN_POINT('Ctrl Pts',(1.72866575619624,-1.05218683017129,
-1.70157781695483));
#364511=CARTESIAN_POINT('Ctrl Pts',(1.39603065320521,-1.46514475575449,
-1.76296158741006));
#364512=CARTESIAN_POINT('Ctrl Pts',(0.969522180315677,-1.77589106055163,
-1.82311912419573));
#364513=CARTESIAN_POINT('Ctrl Pts',(0.476783238604109,-1.96670288995313,
-1.88346520364747));
#364514=CARTESIAN_POINT('Ctrl Pts',(-0.0484603850821368,-2.02312932285366,
-1.94396055370022));
#364515=CARTESIAN_POINT('Ctrl Pts',(-0.570338856925993,-1.94138942628423,
-2.00439291407465));
#364516=CARTESIAN_POINT('Ctrl Pts',(-1.05344948325284,-1.72773686772633,
-2.06470891120488));
#364517=CARTESIAN_POINT('Ctrl Pts',(-1.46487312544728,-1.39632835696345,
-2.1251726344757));
#364518=CARTESIAN_POINT('Ctrl Pts',(-1.77606001340043,-0.969474639293403,
-2.18562457894241));
#364519=CARTESIAN_POINT('Ctrl Pts',(-1.9665886161183,-0.476795144252666,
-2.2459421237894));
#364520=CARTESIAN_POINT('Ctrl Pts',(-2.0231790616074,0.0484698229690482,
-2.30639998925771));
#364521=CARTESIAN_POINT('Ctrl Pts',(-1.94138573006516,0.570342005097921,
-2.36685494461854));
#364522=CARTESIAN_POINT('Ctrl Pts',(-1.72773301625381,1.05344259449438,
-2.42717237256682));
#364523=CARTESIAN_POINT('Ctrl Pts',(-1.39633042998923,1.46487729238585,
-2.48762977035772));
#364524=CARTESIAN_POINT('Ctrl Pts',(-0.969474291036093,1.77605966206198,
-2.54808497616048));
#364525=CARTESIAN_POINT('Ctrl Pts',(-0.476795343347378,1.96658811640277,
-2.6084023881129));
#364526=CARTESIAN_POINT('Ctrl Pts',(0.0484699602192744,2.02317939996145,
-2.66885975673847));
#364527=CARTESIAN_POINT('Ctrl Pts',(0.570341982836039,1.94138567238666,
-2.72931497821885));
#364528=CARTESIAN_POINT('Ctrl Pts',(1.05344257210098,1.72773301387229,-2.78963238875962));
#364529=CARTESIAN_POINT('Ctrl Pts',(1.46487731147791,1.39633043581364,-2.85008975616076));
#364530=CARTESIAN_POINT('Ctrl Pts',(1.7760596572503,0.96947429019414,-2.91054497830833));
#364531=CARTESIAN_POINT('Ctrl Pts',(1.96658811657123,0.47679534386094,-2.97086238877306));
#364532=CARTESIAN_POINT('Ctrl Pts',(2.02317940049204,-0.0484699606166185,
-3.03131975614836));
#364533=CARTESIAN_POINT('Ctrl Pts',(1.94138567221384,-0.570341982644115,
-3.09177497831011));
#364534=CARTESIAN_POINT('Ctrl Pts',(1.72773301391076,-1.05344257214956,
-3.15209238877301));
#364535=CARTESIAN_POINT('Ctrl Pts',(1.39633043580907,-1.46487731147983,
-3.21254975614839));
#364536=CARTESIAN_POINT('Ctrl Pts',(0.969474290197969,-1.77605965724421,
-3.27300497831004));
#364537=CARTESIAN_POINT('Ctrl Pts',(0.476795343858464,-1.96658811657341,
-3.33332238877311));
#364538=CARTESIAN_POINT('Ctrl Pts',(-0.0484699606159255,-2.0231794004916,
-3.39377975614832));
#364539=CARTESIAN_POINT('Ctrl Pts',(-0.570341982644268,-1.94138567221424,
-3.45423497831005));
#364540=CARTESIAN_POINT('Ctrl Pts',(-1.05344257214943,-1.72773301391041,
-3.51455238877311));
#364541=CARTESIAN_POINT('Ctrl Pts',(-1.46487731147993,-1.39633043580919,
-3.57500975614831));
#364542=CARTESIAN_POINT('Ctrl Pts',(-1.77605965724425,-0.969474290197954,
-3.63546497831004));
#364543=CARTESIAN_POINT('Ctrl Pts',(-1.96658811657337,-0.476795343858458,
-3.69578238877312));
#364544=CARTESIAN_POINT('Ctrl Pts',(-2.02317940049162,0.0484699606159343,
-3.75623975614831));
#364545=CARTESIAN_POINT('Ctrl Pts',(-1.94138567221425,0.570341982644281,
-3.81669497831005));
#364546=CARTESIAN_POINT('Ctrl Pts',(-1.7277330139104,1.05344257214943,-3.87701238877311));
#364547=CARTESIAN_POINT('Ctrl Pts',(-1.39633043580919,1.46487731147993,
-3.93746975614831));
#364548=CARTESIAN_POINT('Ctrl Pts',(-0.969474290197942,1.77605965724426,
-3.99792497831004));
#364549=CARTESIAN_POINT('Ctrl Pts',(-0.476795343858452,1.96658811657335,
-4.05824238877313));
#364550=CARTESIAN_POINT('Ctrl Pts',(0.0484699606159434,2.02317940049163,
-4.11869975614831));
#364551=CARTESIAN_POINT('Ctrl Pts',(0.570341982644284,1.94138567221424,
-4.17915497831005));
#364552=CARTESIAN_POINT('Ctrl Pts',(1.05344257214943,1.72773301391039,-4.23947238877311));
#364553=CARTESIAN_POINT('Ctrl Pts',(1.46487731147993,1.39633043580918,-4.29992975614832));
#364554=CARTESIAN_POINT('Ctrl Pts',(1.77605965724427,0.969474290197945,
-4.36038497831003));
#364555=CARTESIAN_POINT('Ctrl Pts',(1.96658811657337,0.476795343858441,
-4.42070238877312));
#364556=CARTESIAN_POINT('Ctrl Pts',(2.02317940049162,-0.0484699606159445,
-4.48115975614831));
#364557=CARTESIAN_POINT('Ctrl Pts',(1.94138567221424,-0.570341982644292,
-4.54161497831005));
#364558=CARTESIAN_POINT('Ctrl Pts',(1.72773301391038,-1.05344257214943,
-4.60193238877312));
#364559=CARTESIAN_POINT('Ctrl Pts',(1.39633043580918,-1.46487731147994,
-4.66238975614831));
#364560=CARTESIAN_POINT('Ctrl Pts',(0.969474290197935,-1.77605965724426,
-4.72284497831004));
#364561=CARTESIAN_POINT('Ctrl Pts',(0.476795343858439,-1.96658811657337,
-4.78316238877312));
#364562=CARTESIAN_POINT('Ctrl Pts',(-0.0484699606159579,-2.02317940049164,
-4.8436197561483));
#364563=CARTESIAN_POINT('Ctrl Pts',(-0.570341982644288,-1.94138567221422,
-4.90407497831006));
#364564=CARTESIAN_POINT('Ctrl Pts',(-1.05344257214943,-1.72773301391037,
-4.96439238877312));
#364565=CARTESIAN_POINT('Ctrl Pts',(-1.46487731147995,-1.39633043580918,
-5.02484975614831));
#364566=CARTESIAN_POINT('Ctrl Pts',(-1.77605965724426,-0.969474290197928,
-5.08530497831004));
#364567=CARTESIAN_POINT('Ctrl Pts',(-1.96658811657335,-0.476795343858433,
-5.14562238877313));
#364568=CARTESIAN_POINT('Ctrl Pts',(-2.02317940049163,0.0484699606159606,
-5.2060797561483));
#364569=CARTESIAN_POINT('Ctrl Pts',(-1.94138567221425,0.570341982644311,
-5.26653497831003));
#364570=CARTESIAN_POINT('Ctrl Pts',(-1.72773301391036,1.05344257214944,
-5.32685238877313));
#364571=CARTESIAN_POINT('Ctrl Pts',(-1.39633043580918,1.46487731147996,
-5.3873097561483));
#364572=CARTESIAN_POINT('Ctrl Pts',(-0.969474290197916,1.77605965724424,
-5.44776497831006));
#364573=CARTESIAN_POINT('Ctrl Pts',(-0.476795343858422,1.96658811657339,
-5.5080823887731));
#364574=CARTESIAN_POINT('Ctrl Pts',(0.0484699606159706,2.02317940049163,
-5.56853975614829));
#364575=CARTESIAN_POINT('Ctrl Pts',(0.570341982644291,1.94138567221422,
-5.62899497831007));
#364576=CARTESIAN_POINT('Ctrl Pts',(1.05344257214944,1.72773301391032,-5.68931238877313));
#364577=CARTESIAN_POINT('Ctrl Pts',(1.46487731147996,1.3963304358092,-5.74976975614823));
#364578=CARTESIAN_POINT('Ctrl Pts',(1.77605965724441,0.969474290197947,
-5.81022497831013));
#364579=CARTESIAN_POINT('Ctrl Pts',(1.96658811657315,0.476795343858267,
-5.87054238877304));
#364580=CARTESIAN_POINT('Ctrl Pts',(2.02317940049197,-0.0484699606151168,
-5.93099975614826));
#364581=CARTESIAN_POINT('Ctrl Pts',(1.94138567221262,-0.570341982647331,
-5.99145497831012));
#364582=CARTESIAN_POINT('Ctrl Pts',(1.72773301391079,-1.05344257214282,
-6.05177238877488));
#364583=CARTESIAN_POINT('Ctrl Pts',(1.39633043583791,-1.46487731150212,
-6.1122297561358));
#364584=CARTESIAN_POINT('Ctrl Pts',(0.969474290103704,-1.77605965719443,
-6.17268497832268));
#364585=CARTESIAN_POINT('Ctrl Pts',(0.476795344014053,-1.96658811647506,
-6.23300238886911));
#364586=CARTESIAN_POINT('Ctrl Pts',(-0.0484699607888847,-2.02317940162764,
-6.293459755551));
#364587=CARTESIAN_POINT('Ctrl Pts',(-0.570341982515374,-1.94138566986718,
-6.35391497894857));
#364588=CARTESIAN_POINT('Ctrl Pts',(-1.0534425689941,-1.72773301427299,
-6.41423239105532));
#364589=CARTESIAN_POINT('Ctrl Pts',(-1.46487733129139,-1.39633044764682,
-6.47468974174144));
#364590=CARTESIAN_POINT('Ctrl Pts',(-1.77605962440754,-0.969474272408487,
-6.53514499410053));
#364591=CARTESIAN_POINT('Ctrl Pts',(-1.96658808441403,-0.4767953693466,
-6.59546242507117));
#364592=CARTESIAN_POINT('Ctrl Pts',(-2.02317971788315,0.0484700612956726,
-6.65591951867769));
#364593=CARTESIAN_POINT('Ctrl Pts',(-1.94138529374751,0.57034175258804,
-6.71637524065362));
#364594=CARTESIAN_POINT('Ctrl Pts',(-1.7277327906675,1.05344225923825,-6.77669281345839));
#364595=CARTESIAN_POINT('Ctrl Pts',(-1.39633190064527,1.46488023063332,
-6.83714685373563));
#364596=CARTESIAN_POINT('Ctrl Pts',(-0.969474795144666,1.77605674551469,
-6.89760831895014));
#364597=CARTESIAN_POINT('Ctrl Pts',(-0.476792483974202,1.96658170561334,
-6.95792512927773));
#364598=CARTESIAN_POINT('Ctrl Pts',(0.0484734593030573,2.0232081210323,
-7.01835708981697));
#364599=CARTESIAN_POINT('Ctrl Pts',(0.570336624689882,1.94136175768686,
-7.07885725203471));
#364600=CARTESIAN_POINT('Ctrl Pts',(1.05340619968671,1.72778052727257,-7.13918044053492));
#364601=CARTESIAN_POINT('Ctrl Pts',(1.46503146071072,1.39600002911185,-7.19942807213429));
#364602=CARTESIAN_POINT('Ctrl Pts',(1.77572739170825,0.970967789756964,
-7.26046972816476));
#364603=CARTESIAN_POINT('Ctrl Pts',(1.9679960876878,0.471734127632586,-7.31921124624962));
#364604=CARTESIAN_POINT('Ctrl Pts',(2.00016367750205,0.139563645186354,
-7.36277016686196));
#364605=CARTESIAN_POINT('Ctrl Pts',(2.00016367750204,-0.0349606549172864,
-7.37954989315336));
#364606=CARTESIAN_POINT('',(2.00005141137773,-0.0349509159166537,-1.58027907189674));
#364607=CARTESIAN_POINT('',(1.7237531792885,-0.0252784459846846,-1.66884860356395));
#364608=CARTESIAN_POINT('Origin',(2.00000000329361,-4.46994898412652E-6,
-1.90027906926653));
#364609=CARTESIAN_POINT('',(1.99994859520949,0.0349419760186854,-2.22027906663631));
#364610=CARTESIAN_POINT('Origin',(2.00000000329361,-4.46994898412652E-6,
-1.90027906926653));
#364611=CARTESIAN_POINT('Ctrl Pts',(1.99994859520949,0.0349419760186854,
-2.22027906663631));
#364612=CARTESIAN_POINT('Ctrl Pts',(1.99994859520949,-0.133161143166691,
-2.23644142527053));
#364613=CARTESIAN_POINT('Ctrl Pts',(1.96833139354662,-0.472425718114294,
-2.28062587414611));
#364614=CARTESIAN_POINT('Ctrl Pts',(1.77549751488388,-0.970378153502274,
-2.33932132964638));
#364615=CARTESIAN_POINT('Ctrl Pts',(1.46486827473653,-1.39599810161593,
-2.40041168228136));
#364616=CARTESIAN_POINT('Ctrl Pts',(1.0532724675317,-1.72756949816,-2.46064650153962));
#364617=CARTESIAN_POINT('Ctrl Pts',(0.570253827701872,-1.94116844962337,
-2.52097328730337));
#364618=CARTESIAN_POINT('Ctrl Pts',(0.0484505622703552,-2.02298787581022,
-2.58147196284819));
#364619=CARTESIAN_POINT('Ctrl Pts',(-0.476762817249676,-1.96636546213765,
-2.64190473727344));
#364620=CARTESIAN_POINT('Ctrl Pts',(-0.969389646094711,-1.7758542783469,
-2.70222141276452));
#364621=CARTESIAN_POINT('Ctrl Pts',(-1.39619412835269,-1.46471035101601,
-2.76268238970025));
#364622=CARTESIAN_POINT('Ctrl Pts',(-1.72755848446788,-1.05330968911041,
-2.8231370123091));
#364623=CARTESIAN_POINT('Ctrl Pts',(-1.94118200928605,-0.570259037663673,
-2.88345449584336));
#364624=CARTESIAN_POINT('Ctrl Pts',(-2.02296215046454,-0.0484473116516587,
-2.94390972032538));
#364625=CARTESIAN_POINT('Ctrl Pts',(-1.96637109382515,0.476765855935366,
-3.00436740295728));
#364626=CARTESIAN_POINT('Ctrl Pts',(-1.77585739520295,0.969389009874219,
-3.06468474103924));
#364627=CARTESIAN_POINT('Ctrl Pts',(-1.46470740175196,1.39619269138418,
-3.12513949735647));
#364628=CARTESIAN_POINT('Ctrl Pts',(-1.05331000180424,1.72755870986409,
-3.18559743702838));
#364629=CARTESIAN_POINT('Ctrl Pts',(-0.570259275444307,1.94118238224882,
-3.2459147561141));
#364630=CARTESIAN_POINT('Ctrl Pts',(-0.0484472107178668,2.02296183497224,
-3.30636948355066));
#364631=CARTESIAN_POINT('Ctrl Pts',(0.476765831354286,1.96637112545875,
-3.36682743921798));
#364632=CARTESIAN_POINT('Ctrl Pts',(0.969389026744113,1.77585742843582,
-3.42714475673536));
#364633=CARTESIAN_POINT('Ctrl Pts',(1.39619267971627,1.46470738191116,-3.48759948296635));
#364634=CARTESIAN_POINT('Ctrl Pts',(1.72755870948907,1.05331000492523,-3.54805743931225));
#364635=CARTESIAN_POINT('Ctrl Pts',(1.9411823845861,0.570259275622033,-3.60837475674778));
#364636=CARTESIAN_POINT('Ctrl Pts',(2.02296183383815,0.0484472105365179,
-3.66882948295392));
#364637=CARTESIAN_POINT('Ctrl Pts',(1.96637112555601,-0.476765831198158,
-3.72928743931407));
#364638=CARTESIAN_POINT('Ctrl Pts',(1.77585742848668,-0.969389026837108,
-3.78960475674772));
#364639=CARTESIAN_POINT('Ctrl Pts',(1.46470738188885,-1.39619267968778,
-3.85005948295395));
#364640=CARTESIAN_POINT('Ctrl Pts',(1.05331000493188,-1.72755870948857,
-3.910517439314));
#364641=CARTESIAN_POINT('Ctrl Pts',(0.570259275619007,-1.9411823845877,
-3.97083475674782));
#364642=CARTESIAN_POINT('Ctrl Pts',(0.0484472105373659,-2.02296183383781,
-4.03128948295388));
#364643=CARTESIAN_POINT('Ctrl Pts',(-0.476765831198311,-1.96637112555626,
-4.09174743931402));
#364644=CARTESIAN_POINT('Ctrl Pts',(-0.969389026837092,-1.77585742848654,
-4.15206475674782));
#364645=CARTESIAN_POINT('Ctrl Pts',(-1.39619267968775,-1.46470738188883,
-4.21251948295388));
#364646=CARTESIAN_POINT('Ctrl Pts',(-1.72755870948862,-1.05331000493188,
-4.27297743931401));
#364647=CARTESIAN_POINT('Ctrl Pts',(-1.94118238458768,-0.570259275619005,
-4.33329475674783));
#364648=CARTESIAN_POINT('Ctrl Pts',(-2.0229618338378,-0.0484472105373586,
-4.39374948295387));
#364649=CARTESIAN_POINT('Ctrl Pts',(-1.96637112555625,0.476765831198322,
-4.45420743931402));
#364650=CARTESIAN_POINT('Ctrl Pts',(-1.77585742848654,0.969389026837096,
-4.51452475674782));
#364651=CARTESIAN_POINT('Ctrl Pts',(-1.46470738188882,1.39619267968775,
-4.57497948295388));
#364652=CARTESIAN_POINT('Ctrl Pts',(-1.05331000493187,1.72755870948862,
-4.63543743931401));
#364653=CARTESIAN_POINT('Ctrl Pts',(-0.570259275619004,1.9411823845877,
-4.69575475674784));
#364654=CARTESIAN_POINT('Ctrl Pts',(-0.0484472105373471,2.0229618338378,
-4.75620948295387));
#364655=CARTESIAN_POINT('Ctrl Pts',(0.476765831198326,1.96637112555626,
-4.81666743931402));
#364656=CARTESIAN_POINT('Ctrl Pts',(0.969389026837101,1.77585742848653,
-4.87698475674782));
#364657=CARTESIAN_POINT('Ctrl Pts',(1.39619267968776,1.46470738188882,-4.93743948295388));
#364658=CARTESIAN_POINT('Ctrl Pts',(1.72755870948861,1.05331000493185,-4.997897439314));
#364659=CARTESIAN_POINT('Ctrl Pts',(1.94118238458768,0.570259275618993,
-5.05821475674782));
#364660=CARTESIAN_POINT('Ctrl Pts',(2.0229618338378,0.0484472105373451,
-5.11866948295387));
#364661=CARTESIAN_POINT('Ctrl Pts',(1.96637112555625,-0.476765831198331,
-5.17912743931402));
#364662=CARTESIAN_POINT('Ctrl Pts',(1.77585742848654,-0.969389026837107,
-5.23944475674783));
#364663=CARTESIAN_POINT('Ctrl Pts',(1.46470738188881,-1.39619267968776,
-5.29989948295387));
#364664=CARTESIAN_POINT('Ctrl Pts',(1.05331000493185,-1.72755870948862,
-5.36035743931401));
#364665=CARTESIAN_POINT('Ctrl Pts',(0.57025927561899,-1.94118238458768,
-5.42067475674783));
#364666=CARTESIAN_POINT('Ctrl Pts',(0.0484472105373359,-2.02296183383778,
-5.48112948295386));
#364667=CARTESIAN_POINT('Ctrl Pts',(-0.476765831198329,-1.96637112555626,
-5.54158743931402));
#364668=CARTESIAN_POINT('Ctrl Pts',(-0.96938902683712,-1.77585742848655,
-5.60190475674783));
#364669=CARTESIAN_POINT('Ctrl Pts',(-1.39619267968776,-1.4647073818888,
-5.66235948295387));
#364670=CARTESIAN_POINT('Ctrl Pts',(-1.72755870948862,-1.05331000493185,
-5.722817439314));
#364671=CARTESIAN_POINT('Ctrl Pts',(-1.9411823845877,-0.570259275618991,
-5.78313475674784));
#364672=CARTESIAN_POINT('Ctrl Pts',(-2.02296183383779,-0.0484472105373294,
-5.84358948295386));
#364673=CARTESIAN_POINT('Ctrl Pts',(-1.96637112555623,0.476765831198343,
-5.904047439314));
#364674=CARTESIAN_POINT('Ctrl Pts',(-1.77585742848654,0.969389026837124,
-5.96436475674784));
#364675=CARTESIAN_POINT('Ctrl Pts',(-1.46470738188879,1.39619267968775,
-6.02481948295386));
#364676=CARTESIAN_POINT('Ctrl Pts',(-1.05331000493186,1.72755870948864,
-6.08527743931403));
#364677=CARTESIAN_POINT('Ctrl Pts',(-0.57025927561896,1.94118238458767,
-6.14559475674781));
#364678=CARTESIAN_POINT('Ctrl Pts',(-0.0484472105373227,2.02296183383776,
-6.20604948295386));
#364679=CARTESIAN_POINT('Ctrl Pts',(0.476765831198343,1.96637112555631,
-6.26650743931404));
#364680=CARTESIAN_POINT('Ctrl Pts',(0.969389026837138,1.77585742848649,
-6.32682475674784));
#364681=CARTESIAN_POINT('Ctrl Pts',(1.39619267968763,1.4647073818887,-6.3872794829538));
#364682=CARTESIAN_POINT('Ctrl Pts',(1.72755870948896,1.05331000493196,-6.4477374393141));
#364683=CARTESIAN_POINT('Ctrl Pts',(1.94118238458724,0.570259275618813,
-6.50805475674775));
#364684=CARTESIAN_POINT('Ctrl Pts',(2.0229618338382,0.0484472105380158,
-6.56850948295382));
#364685=CARTESIAN_POINT('Ctrl Pts',(1.96637112555413,-0.47676583120083,
-6.62896743931409));
#364686=CARTESIAN_POINT('Ctrl Pts',(1.77585742849251,-0.969389026833344,
-6.68928475674954));
#364687=CARTESIAN_POINT('Ctrl Pts',(1.46470738188697,-1.39619267969199,
-6.74973948294137));
#364688=CARTESIAN_POINT('Ctrl Pts',(1.05331000488233,-1.72755870945149,
-6.81019743932769));
#364689=CARTESIAN_POINT('Ctrl Pts',(0.570259275809968,-1.94118238475938,
-6.87051475683913));
#364690=CARTESIAN_POINT('Ctrl Pts',(0.0484472101488399,-2.02296183330866,
-6.93096948236246));
#364691=CARTESIAN_POINT('Ctrl Pts',(-0.476765830732716,-1.96637112538019,
-6.99142743997978));
#364692=CARTESIAN_POINT('Ctrl Pts',(-0.969389027651612,-1.775857433288,
-7.05174475889683));
#364693=CARTESIAN_POINT('Ctrl Pts',(-1.39619267380615,-1.46470736293583,
-7.11219946872276));
#364694=CARTESIAN_POINT('Ctrl Pts',(-1.72755871231312,-1.05331002647757,
-7.1726574556236));
#364695=CARTESIAN_POINT('Ctrl Pts',(-1.94118244199894,-0.570259298778077,
-7.23297479041701));
#364696=CARTESIAN_POINT('Ctrl Pts',(-2.02296149561613,-0.0484470734163606,
-7.29342924947211));
#364697=CARTESIAN_POINT('Ctrl Pts',(-1.96637162260829,0.47676563992917,
-7.35388770608518));
#364698=CARTESIAN_POINT('Ctrl Pts',(-1.77585778550465,0.969389377563547,
-7.41420515419699));
#364699=CARTESIAN_POINT('Ctrl Pts',(-1.46470321414872,1.39619055347437,
-7.4746566054593));
#364700=CARTESIAN_POINT('Ctrl Pts',(-1.05331679189158,1.72756279918536,
-7.53512091909894));
#364701=CARTESIAN_POINT('Ctrl Pts',(-0.570256351317271,1.94118541096824,
-7.5954368568002));
#364702=CARTESIAN_POINT('Ctrl Pts',(-0.0484373346474795,2.02291433148142,
-7.65586848775589));
#364703=CARTESIAN_POINT('Ctrl Pts',(0.476753357889169,1.96647633924905,
-7.7163654145941));
#364704=CARTESIAN_POINT('Ctrl Pts',(0.969439733353148,1.77572407380791,
-7.7767079034587));
#364705=CARTESIAN_POINT('Ctrl Pts',(1.39587962475789,1.46484458461224,-7.83687735653918));
#364706=CARTESIAN_POINT('Ctrl Pts',(1.72854436163452,1.05253719801599,-7.89821617217114));
#364707=CARTESIAN_POINT('Ctrl Pts',(1.93848294702123,0.574209674581668,
-7.95584767975511));
#364708=CARTESIAN_POINT('Ctrl Pts',(1.99983638908382,0.21585245779268,-8.0021551741418));
#364709=CARTESIAN_POINT('Ctrl Pts',(1.99983638908381,0.0349322317806574,
-8.0195498399348));
#364710=CARTESIAN_POINT('Ctrl Pts',(2.00005141137773,-0.0349509159166537,
-1.58027907189674));
#364711=CARTESIAN_POINT('Ctrl Pts',(2.00005141137773,-0.209477500702,-1.59705901785001));
#364712=CARTESIAN_POINT('Ctrl Pts',(1.93937485936534,-0.574981221086946,
-1.64398167301615));
#364713=CARTESIAN_POINT('Ctrl Pts',(1.72866575619624,-1.05218683017129,
-1.70157781695483));
#364714=CARTESIAN_POINT('Ctrl Pts',(1.39603065320521,-1.46514475575449,
-1.76296158741006));
#364715=CARTESIAN_POINT('Ctrl Pts',(0.969522180315677,-1.77589106055163,
-1.82311912419573));
#364716=CARTESIAN_POINT('Ctrl Pts',(0.476783238604109,-1.96670288995313,
-1.88346520364747));
#364717=CARTESIAN_POINT('Ctrl Pts',(-0.0484603850821368,-2.02312932285366,
-1.94396055370022));
#364718=CARTESIAN_POINT('Ctrl Pts',(-0.570338856925993,-1.94138942628423,
-2.00439291407465));
#364719=CARTESIAN_POINT('Ctrl Pts',(-1.05344948325284,-1.72773686772633,
-2.06470891120488));
#364720=CARTESIAN_POINT('Ctrl Pts',(-1.46487312544728,-1.39632835696345,
-2.1251726344757));
#364721=CARTESIAN_POINT('Ctrl Pts',(-1.77606001340043,-0.969474639293403,
-2.18562457894241));
#364722=CARTESIAN_POINT('Ctrl Pts',(-1.9665886161183,-0.476795144252666,
-2.2459421237894));
#364723=CARTESIAN_POINT('Ctrl Pts',(-2.0231790616074,0.0484698229690482,
-2.30639998925771));
#364724=CARTESIAN_POINT('Ctrl Pts',(-1.94138573006516,0.570342005097921,
-2.36685494461854));
#364725=CARTESIAN_POINT('Ctrl Pts',(-1.72773301625381,1.05344259449438,
-2.42717237256682));
#364726=CARTESIAN_POINT('Ctrl Pts',(-1.39633042998923,1.46487729238585,
-2.48762977035772));
#364727=CARTESIAN_POINT('Ctrl Pts',(-0.969474291036093,1.77605966206198,
-2.54808497616048));
#364728=CARTESIAN_POINT('Ctrl Pts',(-0.476795343347378,1.96658811640277,
-2.6084023881129));
#364729=CARTESIAN_POINT('Ctrl Pts',(0.0484699602192744,2.02317939996145,
-2.66885975673847));
#364730=CARTESIAN_POINT('Ctrl Pts',(0.570341982836039,1.94138567238666,
-2.72931497821885));
#364731=CARTESIAN_POINT('Ctrl Pts',(1.05344257210098,1.72773301387229,-2.78963238875962));
#364732=CARTESIAN_POINT('Ctrl Pts',(1.46487731147791,1.39633043581364,-2.85008975616076));
#364733=CARTESIAN_POINT('Ctrl Pts',(1.7760596572503,0.96947429019414,-2.91054497830833));
#364734=CARTESIAN_POINT('Ctrl Pts',(1.96658811657123,0.47679534386094,-2.97086238877306));
#364735=CARTESIAN_POINT('Ctrl Pts',(2.02317940049204,-0.0484699606166185,
-3.03131975614836));
#364736=CARTESIAN_POINT('Ctrl Pts',(1.94138567221384,-0.570341982644115,
-3.09177497831011));
#364737=CARTESIAN_POINT('Ctrl Pts',(1.72773301391076,-1.05344257214956,
-3.15209238877301));
#364738=CARTESIAN_POINT('Ctrl Pts',(1.39633043580907,-1.46487731147983,
-3.21254975614839));
#364739=CARTESIAN_POINT('Ctrl Pts',(0.969474290197968,-1.77605965724421,
-3.27300497831004));
#364740=CARTESIAN_POINT('Ctrl Pts',(0.476795343858464,-1.96658811657341,
-3.33332238877311));
#364741=CARTESIAN_POINT('Ctrl Pts',(-0.0484699606159255,-2.0231794004916,
-3.39377975614832));
#364742=CARTESIAN_POINT('Ctrl Pts',(-0.570341982644268,-1.94138567221424,
-3.45423497831005));
#364743=CARTESIAN_POINT('Ctrl Pts',(-1.05344257214943,-1.72773301391041,
-3.51455238877311));
#364744=CARTESIAN_POINT('Ctrl Pts',(-1.46487731147993,-1.39633043580919,
-3.57500975614831));
#364745=CARTESIAN_POINT('Ctrl Pts',(-1.77605965724425,-0.969474290197954,
-3.63546497831004));
#364746=CARTESIAN_POINT('Ctrl Pts',(-1.96658811657337,-0.476795343858458,
-3.69578238877312));
#364747=CARTESIAN_POINT('Ctrl Pts',(-2.02317940049162,0.0484699606159343,
-3.75623975614831));
#364748=CARTESIAN_POINT('Ctrl Pts',(-1.94138567221425,0.570341982644281,
-3.81669497831005));
#364749=CARTESIAN_POINT('Ctrl Pts',(-1.7277330139104,1.05344257214943,-3.87701238877311));
#364750=CARTESIAN_POINT('Ctrl Pts',(-1.39633043580919,1.46487731147993,
-3.93746975614831));
#364751=CARTESIAN_POINT('Ctrl Pts',(-0.969474290197942,1.77605965724426,
-3.99792497831004));
#364752=CARTESIAN_POINT('Ctrl Pts',(-0.476795343858452,1.96658811657335,
-4.05824238877313));
#364753=CARTESIAN_POINT('Ctrl Pts',(0.0484699606159434,2.02317940049163,
-4.11869975614831));
#364754=CARTESIAN_POINT('Ctrl Pts',(0.570341982644284,1.94138567221424,
-4.17915497831005));
#364755=CARTESIAN_POINT('Ctrl Pts',(1.05344257214943,1.72773301391039,-4.23947238877311));
#364756=CARTESIAN_POINT('Ctrl Pts',(1.46487731147993,1.39633043580918,-4.29992975614832));
#364757=CARTESIAN_POINT('Ctrl Pts',(1.77605965724427,0.969474290197945,
-4.36038497831003));
#364758=CARTESIAN_POINT('Ctrl Pts',(1.96658811657337,0.476795343858441,
-4.42070238877312));
#364759=CARTESIAN_POINT('Ctrl Pts',(2.02317940049162,-0.0484699606159445,
-4.48115975614831));
#364760=CARTESIAN_POINT('Ctrl Pts',(1.94138567221424,-0.570341982644292,
-4.54161497831005));
#364761=CARTESIAN_POINT('Ctrl Pts',(1.72773301391038,-1.05344257214943,
-4.60193238877312));
#364762=CARTESIAN_POINT('Ctrl Pts',(1.39633043580918,-1.46487731147994,
-4.66238975614831));
#364763=CARTESIAN_POINT('Ctrl Pts',(0.969474290197935,-1.77605965724426,
-4.72284497831004));
#364764=CARTESIAN_POINT('Ctrl Pts',(0.476795343858439,-1.96658811657337,
-4.78316238877312));
#364765=CARTESIAN_POINT('Ctrl Pts',(-0.0484699606159579,-2.02317940049164,
-4.8436197561483));
#364766=CARTESIAN_POINT('Ctrl Pts',(-0.570341982644288,-1.94138567221422,
-4.90407497831006));
#364767=CARTESIAN_POINT('Ctrl Pts',(-1.05344257214943,-1.72773301391037,
-4.96439238877312));
#364768=CARTESIAN_POINT('Ctrl Pts',(-1.46487731147995,-1.39633043580918,
-5.02484975614831));
#364769=CARTESIAN_POINT('Ctrl Pts',(-1.77605965724426,-0.969474290197928,
-5.08530497831004));
#364770=CARTESIAN_POINT('Ctrl Pts',(-1.96658811657335,-0.476795343858433,
-5.14562238877313));
#364771=CARTESIAN_POINT('Ctrl Pts',(-2.02317940049163,0.0484699606159606,
-5.2060797561483));
#364772=CARTESIAN_POINT('Ctrl Pts',(-1.94138567221425,0.570341982644311,
-5.26653497831003));
#364773=CARTESIAN_POINT('Ctrl Pts',(-1.72773301391036,1.05344257214944,
-5.32685238877313));
#364774=CARTESIAN_POINT('Ctrl Pts',(-1.39633043580918,1.46487731147996,
-5.3873097561483));
#364775=CARTESIAN_POINT('Ctrl Pts',(-0.969474290197916,1.77605965724424,
-5.44776497831006));
#364776=CARTESIAN_POINT('Ctrl Pts',(-0.476795343858422,1.96658811657339,
-5.5080823887731));
#364777=CARTESIAN_POINT('Ctrl Pts',(0.0484699606159706,2.02317940049163,
-5.56853975614829));
#364778=CARTESIAN_POINT('Ctrl Pts',(0.570341982644291,1.94138567221422,
-5.62899497831007));
#364779=CARTESIAN_POINT('Ctrl Pts',(1.05344257214944,1.72773301391032,-5.68931238877313));
#364780=CARTESIAN_POINT('Ctrl Pts',(1.46487731147996,1.3963304358092,-5.74976975614823));
#364781=CARTESIAN_POINT('Ctrl Pts',(1.77605965724441,0.969474290197947,
-5.81022497831013));
#364782=CARTESIAN_POINT('Ctrl Pts',(1.96658811657315,0.476795343858267,
-5.87054238877304));
#364783=CARTESIAN_POINT('Ctrl Pts',(2.02317940049197,-0.0484699606151168,
-5.93099975614826));
#364784=CARTESIAN_POINT('Ctrl Pts',(1.94138567221262,-0.570341982647331,
-5.99145497831012));
#364785=CARTESIAN_POINT('Ctrl Pts',(1.72773301391079,-1.05344257214282,
-6.05177238877488));
#364786=CARTESIAN_POINT('Ctrl Pts',(1.39633043583791,-1.46487731150212,
-6.1122297561358));
#364787=CARTESIAN_POINT('Ctrl Pts',(0.969474290103703,-1.77605965719442,
-6.17268497832268));
#364788=CARTESIAN_POINT('Ctrl Pts',(0.476795344014053,-1.96658811647506,
-6.23300238886911));
#364789=CARTESIAN_POINT('Ctrl Pts',(-0.0484699607888847,-2.02317940162764,
-6.293459755551));
#364790=CARTESIAN_POINT('Ctrl Pts',(-0.570341982515374,-1.94138566986718,
-6.35391497894857));
#364791=CARTESIAN_POINT('Ctrl Pts',(-1.0534425689941,-1.72773301427299,
-6.41423239105532));
#364792=CARTESIAN_POINT('Ctrl Pts',(-1.46487733129139,-1.39633044764682,
-6.47468974174144));
#364793=CARTESIAN_POINT('Ctrl Pts',(-1.77605962440754,-0.969474272408487,
-6.53514499410053));
#364794=CARTESIAN_POINT('Ctrl Pts',(-1.96658808441403,-0.4767953693466,
-6.59546242507117));
#364795=CARTESIAN_POINT('Ctrl Pts',(-2.02317971788315,0.0484700612956726,
-6.65591951867769));
#364796=CARTESIAN_POINT('Ctrl Pts',(-1.94138529374751,0.57034175258804,
-6.71637524065362));
#364797=CARTESIAN_POINT('Ctrl Pts',(-1.7277327906675,1.05344225923825,-6.77669281345839));
#364798=CARTESIAN_POINT('Ctrl Pts',(-1.39633190064527,1.46488023063332,
-6.83714685373563));
#364799=CARTESIAN_POINT('Ctrl Pts',(-0.969474795144666,1.77605674551469,
-6.89760831895014));
#364800=CARTESIAN_POINT('Ctrl Pts',(-0.476792483974202,1.96658170561334,
-6.95792512927773));
#364801=CARTESIAN_POINT('Ctrl Pts',(0.0484734593030573,2.0232081210323,
-7.01835708981697));
#364802=CARTESIAN_POINT('Ctrl Pts',(0.570336624689882,1.94136175768686,
-7.07885725203471));
#364803=CARTESIAN_POINT('Ctrl Pts',(1.05340619968671,1.72778052727257,-7.13918044053492));
#364804=CARTESIAN_POINT('Ctrl Pts',(1.46503146071072,1.39600002911185,-7.19942807213429));
#364805=CARTESIAN_POINT('Ctrl Pts',(1.77572739170825,0.970967789756964,
-7.26046972816476));
#364806=CARTESIAN_POINT('Ctrl Pts',(1.9679960876878,0.471734127632586,-7.31921124624962));
#364807=CARTESIAN_POINT('Ctrl Pts',(2.00016367750205,0.139563645186354,
-7.36277016686196));
#364808=CARTESIAN_POINT('Ctrl Pts',(2.00016367750204,-0.0349606549172864,
-7.37954989315336));
#364809=CARTESIAN_POINT('Ctrl Pts',(2.,0.,-0.919999999999993));
#364810=CARTESIAN_POINT('Ctrl Pts',(1.9924061401935,-0.1305836429736,-0.926868907781472));
#364811=CARTESIAN_POINT('Ctrl Pts',(1.97718154739341,-0.392384998448425,
-0.940640076412341));
#364812=CARTESIAN_POINT('Ctrl Pts',(1.85901893075151,-0.770264472745852,
-0.961199190461979));
#364813=CARTESIAN_POINT('Ctrl Pts',(1.67380212461465,-1.11839049672256,
-0.981867932445977));
#364814=CARTESIAN_POINT('Ctrl Pts',(1.39568858766182,-1.45707298411786,
-1.00483530662099));
#364815=CARTESIAN_POINT('Ctrl Pts',(1.01136330582357,-1.75174676674517,
-1.03005611602139));
#364816=CARTESIAN_POINT('Ctrl Pts',(0.523585702942253,-1.95400607364428,
-1.05751009591307));
#364817=CARTESIAN_POINT('Ctrl Pts',(-1.62435722739463E-5,-2.02307699179836,
-1.08507117314344));
#364818=CARTESIAN_POINT('Ctrl Pts',(-0.523536317885363,-1.95385305544458,
-1.11259298299813));
#364819=CARTESIAN_POINT('Ctrl Pts',(-1.01143313765049,-1.75187888421358,
-1.14006309809451));
#364820=CARTESIAN_POINT('Ctrl Pts',(-1.43055439145378,-1.43053532023484,
-1.16760081034308));
#364821=CARTESIAN_POINT('Ctrl Pts',(-1.7517838724523,-1.01138424804627,
-1.19513433615883));
#364822=CARTESIAN_POINT('Ctrl Pts',(-1.95395118967044,-0.52357502362932,
-1.22260450625386));
#364823=CARTESIAN_POINT('Ctrl Pts',(-2.02309840874517,1.39140831439291E-5,
-1.25013947035447));
#364824=CARTESIAN_POINT('Ctrl Pts',(-1.95385456936267,0.52354165019408,
-1.27767463061609));
#364825=CARTESIAN_POINT('Ctrl Pts',(-1.75187530264009,1.01142844098439,
-1.30514480045556));
#364826=CARTESIAN_POINT('Ctrl Pts',(-1.43053726663428,1.4305573555692,-1.33267812946709));
#364827=CARTESIAN_POINT('Ctrl Pts',(-1.01138541561949,1.75178358667915,
-1.36021604426028));
#364828=CARTESIAN_POINT('Ctrl Pts',(-0.523570999948669,1.95394672745918,
-1.38768613982889));
#364829=CARTESIAN_POINT('Ctrl Pts',(1.24423377236111E-5,2.02310883807685,
-1.41520780852107));
#364830=CARTESIAN_POINT('Ctrl Pts',(0.523542096174336,1.95385181633148,
-1.44276890960603));
#364831=CARTESIAN_POINT('Ctrl Pts',(1.0114195685531,1.75192189566403,-1.47022354238125));
#364832=CARTESIAN_POINT('Ctrl Pts',(1.39574727856968,1.45690129136922,-1.49544185654267));
#364833=CARTESIAN_POINT('Ctrl Pts',(1.67373453408061,1.11891073119414,-1.51841614397666));
#364834=CARTESIAN_POINT('Ctrl Pts',(1.85897590932335,0.768114988005871,
-1.53906122201719));
#364835=CARTESIAN_POINT('Ctrl Pts',(1.97776901413901,0.398755552237307,
-1.55979576815126));
#364836=CARTESIAN_POINT('Ctrl Pts',(1.99260464990788,0.109993480400852,
-1.57343356620573));
#364837=CARTESIAN_POINT('Ctrl Pts',(2.00005141137773,-0.0349509159166537,
-1.58027907189674));
#364838=CARTESIAN_POINT('Ctrl Pts',(2.8,0.,-0.919999999999993));
#364839=CARTESIAN_POINT('Ctrl Pts',(2.78939199277986,-0.182993728026944,
-0.926864406801388));
#364840=CARTESIAN_POINT('Ctrl Pts',(2.76812446948309,-0.54986973906403,
-0.940626551616868));
#364841=CARTESIAN_POINT('Ctrl Pts',(2.60295543055419,-1.07729524714901,
-0.961278164543689));
#364842=CARTESIAN_POINT('Ctrl Pts',(2.3432740748819,-1.56601868287461,-0.981972834586931));
#364843=CARTESIAN_POINT('Ctrl Pts',(1.9534645938062,-2.04021452969416,-1.00482284429261));
#364844=CARTESIAN_POINT('Ctrl Pts',(1.41694431361456,-2.45199325498274,
-1.02999729271682));
#364845=CARTESIAN_POINT('Ctrl Pts',(0.732261973497512,-2.73592828705718,
-1.05766533228683));
#364846=CARTESIAN_POINT('Ctrl Pts',(-5.53107937837186E-5,-2.83213060052566,
-1.08508982617781));
#364847=CARTESIAN_POINT('Ctrl Pts',(-0.732227236330921,-2.73573484730789,
-1.11255527546237));
#364848=CARTESIAN_POINT('Ctrl Pts',(-1.41671668511953,-2.4523342703758,
-1.14018764997613));
#364849=CARTESIAN_POINT('Ctrl Pts',(-2.00264985801735,-2.00263363186375,
-1.16763896370469));
#364850=CARTESIAN_POINT('Ctrl Pts',(-2.4522378702943,-1.41666694884076,
-1.19509582612308));
#364851=CARTESIAN_POINT('Ctrl Pts',(-2.73582334389193,-0.732298418914319,
-1.22272542915656));
#364852=CARTESIAN_POINT('Ctrl Pts',(-2.83216647994848,1.05873370328634E-5,
-1.25018040117675));
#364853=CARTESIAN_POINT('Ctrl Pts',(-2.73572815948738,0.732260080199856,
-1.27763556928937));
#364854=CARTESIAN_POINT('Ctrl Pts',(-2.4523317981686,1.41670660974565,-1.30526517206592));
#364855=CARTESIAN_POINT('Ctrl Pts',(-2.0026374388973,2.0026509689249,-1.33272183775651));
#364856=CARTESIAN_POINT('Ctrl Pts',(-1.41667347271186,2.45223646417305,
-1.3601733539516));
#364857=CARTESIAN_POINT('Ctrl Pts',(-0.73226691430792,2.73582715423785,
-1.38780570894782));
#364858=CARTESIAN_POINT('Ctrl Pts',(-3.32541419378344E-5,2.83216215152901,
-1.41527101711875));
#364859=CARTESIAN_POINT('Ctrl Pts',(0.732213474069494,2.73577655753039,
-1.44269553505523));
#364860=CARTESIAN_POINT('Ctrl Pts',(1.41699596320263,2.45216677851596,-1.47036422641732));
#364861=CARTESIAN_POINT('Ctrl Pts',(1.95351849625047,2.04006124129144,-1.49553618329511));
#364862=CARTESIAN_POINT('Ctrl Pts',(2.34320434404536,1.56650518466477,-1.51839309578454));
#364863=CARTESIAN_POINT('Ctrl Pts',(2.60290758877066,1.07529461519169,-1.5390641373972));
#364864=CARTESIAN_POINT('Ctrl Pts',(2.7689186260588,0.55507555381449,-1.55989143937075));
#364865=CARTESIAN_POINT('Ctrl Pts',(2.78964685205658,0.162241467065363,
-1.57352004288224));
#364866=CARTESIAN_POINT('Ctrl Pts',(2.80005140479051,-0.0349419760186688,
-1.58036093336367));
#364867=CARTESIAN_POINT('Ctrl Pts',(2.8,0.,-1.55999999999999));
#364868=CARTESIAN_POINT('Ctrl Pts',(2.78939649751634,-0.182997808095028,
-1.56686440711942));
#364869=CARTESIAN_POINT('Ctrl Pts',(2.76813800556597,-0.549881999079696,
-1.58062655257252));
#364870=CARTESIAN_POINT('Ctrl Pts',(2.60287048343998,-1.07724179710562,
-1.6012781606252));
#364871=CARTESIAN_POINT('Ctrl Pts',(2.34315963754124,-1.56595368435367,
-1.62197282719421));
#364872=CARTESIAN_POINT('Ctrl Pts',(1.95348731824777,-2.04021286575323,
-1.64482284638796));
#364873=CARTESIAN_POINT('Ctrl Pts',(1.41697144358507,-2.45206379948272,
-1.66999729490308));
#364874=CARTESIAN_POINT('Ctrl Pts',(0.732200851511023,-2.73574151657536,
-1.69766532043691));
#364875=CARTESIAN_POINT('Ctrl Pts',(-2.70481749242659E-5,-2.83210623547185,
-1.72508982747625));
#364876=CARTESIAN_POINT('Ctrl Pts',(-0.732252487208887,-2.73577889971119,
-1.75255527725563));
#364877=CARTESIAN_POINT('Ctrl Pts',(-1.41664649586044,-2.45219160028545,
-1.78018764150562));
#364878=CARTESIAN_POINT('Ctrl Pts',(-2.00259639972156,-2.00261890380741,
-1.80763896342095));
#364879=CARTESIAN_POINT('Ctrl Pts',(-2.45228673495991,-1.41668180042844,
-1.83509582821663));
#364880=CARTESIAN_POINT('Ctrl Pts',(-2.73567754904204,-0.732247710943258,
-1.86272542106748));
#364881=CARTESIAN_POINT('Ctrl Pts',(-2.83211473644778,-1.68757765071671E-5,
-1.89018040067487));
#364882=CARTESIAN_POINT('Ctrl Pts',(-2.73577394601168,0.732284104217307,
-1.91763557143196));
#364883=CARTESIAN_POINT('Ctrl Pts',(-2.45219333916896,1.41663986613312,
-1.94526516399832));
#364884=CARTESIAN_POINT('Ctrl Pts',(-2.00261772079364,2.00259272042701,
-1.9727218371175));
#364885=CARTESIAN_POINT('Ctrl Pts',(-1.41669182241623,2.4522887952019,-2.00017335617694));
#364886=CARTESIAN_POINT('Ctrl Pts',(-0.732214969721451,2.73568587053461,
-2.02780570068256));
#364887=CARTESIAN_POINT('Ctrl Pts',(-6.15112143014144E-5,2.83207265142351,
-2.05527101556769));
#364888=CARTESIAN_POINT('Ctrl Pts',(0.732247904310314,2.73590203116,-2.08269553782593));
#364889=CARTESIAN_POINT('Ctrl Pts',(1.41691695808072,2.45186224921218,-2.11036421584428));
#364890=CARTESIAN_POINT('Ctrl Pts',(1.95342442139249,2.04047105442842,-2.13553617856065));
#364891=CARTESIAN_POINT('Ctrl Pts',(2.34323316729515,1.56520434188013,-2.15839309657528));
#364892=CARTESIAN_POINT('Ctrl Pts',(2.60289731690865,1.08024771508786,-2.17906413834116));
#364893=CARTESIAN_POINT('Ctrl Pts',(2.76880371833477,0.536476428508159,
-2.19989143334533));
#364894=CARTESIAN_POINT('Ctrl Pts',(2.7895399948989,0.202560389138996,-2.21352003736615));
#364895=CARTESIAN_POINT('Ctrl Pts',(2.79994858862227,0.0349509159166703,
-2.22036092810323));
#364896=CARTESIAN_POINT('Ctrl Pts',(2.,0.,-1.55999999999999));
#364897=CARTESIAN_POINT('Ctrl Pts',(1.99241064492998,-0.130587723041684,
-1.56686890809951));
#364898=CARTESIAN_POINT('Ctrl Pts',(1.97719508347629,-0.392397258464091,
-1.58064007736799));
#364899=CARTESIAN_POINT('Ctrl Pts',(1.85893398363731,-0.77021102270246,
-1.60119918654349));
#364900=CARTESIAN_POINT('Ctrl Pts',(1.67368768727399,-1.11832549820161,
-1.62186792505326));
#364901=CARTESIAN_POINT('Ctrl Pts',(1.39571131210339,-1.45707132017693,
-1.64483530871634));
#364902=CARTESIAN_POINT('Ctrl Pts',(1.01139043579407,-1.75181731124514,
-1.67005611820765));
#364903=CARTESIAN_POINT('Ctrl Pts',(0.523524580955764,-1.95381930316246,
-1.69751008406315));
#364904=CARTESIAN_POINT('Ctrl Pts',(1.20190465855827E-5,-2.02305262674455,
-1.72507117444189));
#364905=CARTESIAN_POINT('Ctrl Pts',(-0.523561568763329,-1.95389710784788,
-1.75259298479139));
#364906=CARTESIAN_POINT('Ctrl Pts',(-1.0113629483914,-1.75173621412323,
-1.780063089624));
#364907=CARTESIAN_POINT('Ctrl Pts',(-1.43050093315799,-1.4305205921785,
-1.80760081005934));
#364908=CARTESIAN_POINT('Ctrl Pts',(-1.75183273711791,-1.01139909963394,
-1.83513433825238));
#364909=CARTESIAN_POINT('Ctrl Pts',(-1.95380539482055,-0.523524315658259,
-1.86260449816478));
#364910=CARTESIAN_POINT('Ctrl Pts',(-2.02304666524447,-1.35490303961885E-5,
-1.89013946985259));
#364911=CARTESIAN_POINT('Ctrl Pts',(-1.95390035588696,0.523565674211531,
-1.91767463275868));
#364912=CARTESIAN_POINT('Ctrl Pts',(-1.75173684364045,1.01136169737186,
-1.94514479238796));
#364913=CARTESIAN_POINT('Ctrl Pts',(-1.43051754853062,1.43049910707131,
-1.97267812882809));
#364914=CARTESIAN_POINT('Ctrl Pts',(-1.01140376532386,1.751835917708,-2.00021604648563));
#364915=CARTESIAN_POINT('Ctrl Pts',(-0.523519055362199,1.95380544375593,
-2.02768613156363));
#364916=CARTESIAN_POINT('Ctrl Pts',(-1.58147346400669E-5,2.02301933797135,
-2.05520780697));
#364917=CARTESIAN_POINT('Ctrl Pts',(0.523576526415156,1.95397728996109,
-2.08276891237674));
#364918=CARTESIAN_POINT('Ctrl Pts',(1.01134056343118,1.75161736636026,-2.11022353180821));
#364919=CARTESIAN_POINT('Ctrl Pts',(1.3956532037117,1.4573111045062,-2.13544185180822));
#364920=CARTESIAN_POINT('Ctrl Pts',(1.67376335733039,1.1176098884095,-2.1584161447674));
#364921=CARTESIAN_POINT('Ctrl Pts',(1.85896563746134,0.773068087902041,
-2.17906122296115));
#364922=CARTESIAN_POINT('Ctrl Pts',(1.97765410641497,0.380156426930975,
-2.19979576212585));
#364923=CARTESIAN_POINT('Ctrl Pts',(1.9924977927502,0.150312402474485,-2.21343356068965));
#364924=CARTESIAN_POINT('Ctrl Pts',(1.99994859520949,0.0349419760186854,
-2.22027906663631));
#364925=CARTESIAN_POINT('Ctrl Pts',(1.2,0.,-1.55999999999999));
#364926=CARTESIAN_POINT('Ctrl Pts',(1.19542479234362,-0.0781776379883396,
-1.56687340907959));
#364927=CARTESIAN_POINT('Ctrl Pts',(1.18625216138661,-0.234912517848486,
-1.58065360216347));
#364928=CARTESIAN_POINT('Ctrl Pts',(1.11499748383463,-0.4631802482993,-1.60112021246178));
#364929=CARTESIAN_POINT('Ctrl Pts',(1.00421573700674,-0.670697312049558,
-1.62176302291231));
#364930=CARTESIAN_POINT('Ctrl Pts',(0.837935305959016,-0.873929774600632,
-1.64484777104472));
#364931=CARTESIAN_POINT('Ctrl Pts',(0.60580942800308,-1.05157082300757,
-1.67011494151222));
#364932=CARTESIAN_POINT('Ctrl Pts',(0.314848310400505,-1.17189708974956,
-1.6973548476894));
#364933=CARTESIAN_POINT('Ctrl Pts',(5.10862680953333E-5,-1.21399901801725,
-1.72505252140752));
#364934=CARTESIAN_POINT('Ctrl Pts',(-0.31487065031777,-1.17201531598458,
-1.75263069232715));
#364935=CARTESIAN_POINT('Ctrl Pts',(-0.606079400922359,-1.05128082796102,
-1.77993853774237));
#364936=CARTESIAN_POINT('Ctrl Pts',(-0.858405466594417,-0.858422280549586,
-1.80756265669772));
#364937=CARTESIAN_POINT('Ctrl Pts',(-1.0513787392759,-0.606116398839451,
-1.83517284828813));
#364938=CARTESIAN_POINT('Ctrl Pts',(-1.17193324059906,-0.31480092037326,
-1.86248357526207));
#364939=CARTESIAN_POINT('Ctrl Pts',(-1.21397859404116,-1.02222842850628E-5,
-1.89009853903031));
#364940=CARTESIAN_POINT('Ctrl Pts',(-1.17202676576225,0.314847244205754,
-1.9177136940854));
#364941=CARTESIAN_POINT('Ctrl Pts',(-1.05128034811194,0.606083528610609,
-1.9450244207776));
#364942=CARTESIAN_POINT('Ctrl Pts',(-0.858417376267602,0.858405493715605,
-1.97263442053868));
#364943=CARTESIAN_POINT('Ctrl Pts',(-0.606115708231486,1.05138304021409,
-2.00025873679431));
#364944=CARTESIAN_POINT('Ctrl Pts',(-0.314823141002948,1.17192501697726,
-2.0275665624447));
#364945=CARTESIAN_POINT('Ctrl Pts',(2.98817450213404E-5,1.21396602451919,
-2.05514459837232));
#364946=CARTESIAN_POINT('Ctrl Pts',(0.314905148519997,1.17205254876217,
-2.08284228692754));
#364947=CARTESIAN_POINT('Ctrl Pts',(0.605764168781643,1.05137248350833,
-2.11008284777213));
#364948=CARTESIAN_POINT('Ctrl Pts',(0.837881986030918,0.874151154583981,
-2.13534752505579));
#364949=CARTESIAN_POINT('Ctrl Pts',(1.00429354736563,0.670015434938871,
-2.15843919295953));
#364950=CARTESIAN_POINT('Ctrl Pts',(1.11503395801403,0.465888460716222,
-2.17905830758114));
#364951=CARTESIAN_POINT('Ctrl Pts',(1.18650449449518,0.223836425353792,
-2.19970009090637));
#364952=CARTESIAN_POINT('Ctrl Pts',(1.1954555906015,0.0980644158099734,
-2.21334708401314));
#364953=CARTESIAN_POINT('Ctrl Pts',(1.19994860179671,0.0349330361207006,
-2.22019720516939));
#364954=CARTESIAN_POINT('Ctrl Pts',(1.2,0.,-0.919999999999993));
#364955=CARTESIAN_POINT('Ctrl Pts',(1.19542028760714,-0.0781735579202564,
-0.926873408761556));
#364956=CARTESIAN_POINT('Ctrl Pts',(1.18623862530372,-0.23490025783282,
-0.940653601207814));
#364957=CARTESIAN_POINT('Ctrl Pts',(1.11508243094883,-0.463233698342691,
-0.961120216380269));
#364958=CARTESIAN_POINT('Ctrl Pts',(1.0043301743474,-0.670762310570501,
-0.981763030305022));
#364959=CARTESIAN_POINT('Ctrl Pts',(0.837912581517445,-0.873931438541563,
-1.00484776894937));
#364960=CARTESIAN_POINT('Ctrl Pts',(0.605782298032579,-1.0515002785076,
-1.03011493932597));
#364961=CARTESIAN_POINT('Ctrl Pts',(0.314909432386994,-1.17208386023138,
-1.05735485953932));
#364962=CARTESIAN_POINT('Ctrl Pts',(2.28236492357989E-5,-1.21402338307106,
-1.08505252010907));
#364963=CARTESIAN_POINT('Ctrl Pts',(-0.314845399439805,-1.17197126358128,
-1.11263069053389));
#364964=CARTESIAN_POINT('Ctrl Pts',(-0.606149590181453,-1.05142349805137,
-1.13993854621288));
#364965=CARTESIAN_POINT('Ctrl Pts',(-0.858458924890206,-0.858437008605928,
-1.16756265698147));
#364966=CARTESIAN_POINT('Ctrl Pts',(-1.05132987461029,-0.606101547251777,
-1.19517284619458));
#364967=CARTESIAN_POINT('Ctrl Pts',(-1.17207903544895,-0.314851628344321,
-1.22248358335115));
#364968=CARTESIAN_POINT('Ctrl Pts',(-1.21403033754186,1.72408292549676E-5,
-1.25009853953219));
#364969=CARTESIAN_POINT('Ctrl Pts',(-1.17198097923795,0.314823220188304,
-1.27771369194281));
#364970=CARTESIAN_POINT('Ctrl Pts',(-1.05141880711158,0.60615027222314,
-1.3050244288452));
#364971=CARTESIAN_POINT('Ctrl Pts',(-0.858437094371262,0.858463742213499,
-1.33263442117768));
#364972=CARTESIAN_POINT('Ctrl Pts',(-0.606097358527115,1.05133070918524,
-1.36025873456897));
#364973=CARTESIAN_POINT('Ctrl Pts',(-0.314875085589417,1.1720663006805,
-1.38756657070996));
#364974=CARTESIAN_POINT('Ctrl Pts',(5.81388173850348E-5,1.21405552462469,
-1.41514459992339));
#364975=CARTESIAN_POINT('Ctrl Pts',(0.314870718279177,1.17192707513256,
-1.44284228415683));
#364976=CARTESIAN_POINT('Ctrl Pts',(0.60584317390356,1.05167701281211,-1.47008285834517));
#364977=CARTESIAN_POINT('Ctrl Pts',(0.837976060888895,0.873741341447001,
-1.49534752979024));
#364978=CARTESIAN_POINT('Ctrl Pts',(1.00426472411585,0.671316277723509,
-1.51843919216879));
#364979=CARTESIAN_POINT('Ctrl Pts',(1.11504422987604,0.460935360820052,
-1.53905830663718));
#364980=CARTESIAN_POINT('Ctrl Pts',(1.18661940221922,0.242435550660123,
-1.55970009693178));
#364981=CARTESIAN_POINT('Ctrl Pts',(1.19556244775918,0.0577454937363405,
-1.57334708952923));
#364982=CARTESIAN_POINT('Ctrl Pts',(1.20005141796495,-0.0349598558146385,
-1.58019721042982));
#364983=CARTESIAN_POINT('Ctrl Pts',(2.,0.,-0.919999999999993));
#364984=CARTESIAN_POINT('Ctrl Pts',(1.9924061401935,-0.1305836429736,-0.926868907781472));
#364985=CARTESIAN_POINT('Ctrl Pts',(1.97718154739341,-0.392384998448425,
-0.940640076412341));
#364986=CARTESIAN_POINT('Ctrl Pts',(1.85901893075151,-0.770264472745852,
-0.961199190461979));
#364987=CARTESIAN_POINT('Ctrl Pts',(1.67380212461465,-1.11839049672256,
-0.981867932445977));
#364988=CARTESIAN_POINT('Ctrl Pts',(1.39568858766182,-1.45707298411786,
-1.00483530662099));
#364989=CARTESIAN_POINT('Ctrl Pts',(1.01136330582357,-1.75174676674517,
-1.03005611602139));
#364990=CARTESIAN_POINT('Ctrl Pts',(0.523585702942253,-1.95400607364428,
-1.05751009591307));
#364991=CARTESIAN_POINT('Ctrl Pts',(-1.62435722739463E-5,-2.02307699179836,
-1.08507117314344));
#364992=CARTESIAN_POINT('Ctrl Pts',(-0.523536317885363,-1.95385305544458,
-1.11259298299813));
#364993=CARTESIAN_POINT('Ctrl Pts',(-1.01143313765049,-1.75187888421358,
-1.14006309809451));
#364994=CARTESIAN_POINT('Ctrl Pts',(-1.43055439145378,-1.43053532023484,
-1.16760081034308));
#364995=CARTESIAN_POINT('Ctrl Pts',(-1.7517838724523,-1.01138424804627,
-1.19513433615883));
#364996=CARTESIAN_POINT('Ctrl Pts',(-1.95395118967044,-0.52357502362932,
-1.22260450625386));
#364997=CARTESIAN_POINT('Ctrl Pts',(-2.02309840874517,1.39140831439291E-5,
-1.25013947035447));
#364998=CARTESIAN_POINT('Ctrl Pts',(-1.95385456936267,0.52354165019408,
-1.27767463061609));
#364999=CARTESIAN_POINT('Ctrl Pts',(-1.75187530264009,1.01142844098439,
-1.30514480045556));
#365000=CARTESIAN_POINT('Ctrl Pts',(-1.43053726663428,1.4305573555692,-1.33267812946709));
#365001=CARTESIAN_POINT('Ctrl Pts',(-1.01138541561949,1.75178358667915,
-1.36021604426028));
#365002=CARTESIAN_POINT('Ctrl Pts',(-0.523570999948669,1.95394672745918,
-1.38768613982889));
#365003=CARTESIAN_POINT('Ctrl Pts',(1.24423377236111E-5,2.02310883807685,
-1.41520780852107));
#365004=CARTESIAN_POINT('Ctrl Pts',(0.523542096174336,1.95385181633148,
-1.44276890960603));
#365005=CARTESIAN_POINT('Ctrl Pts',(1.0114195685531,1.75192189566403,-1.47022354238125));
#365006=CARTESIAN_POINT('Ctrl Pts',(1.39574727856968,1.45690129136922,-1.49544185654267));
#365007=CARTESIAN_POINT('Ctrl Pts',(1.67373453408061,1.11891073119414,-1.51841614397666));
#365008=CARTESIAN_POINT('Ctrl Pts',(1.85897590932335,0.768114988005871,
-1.53906122201719));
#365009=CARTESIAN_POINT('Ctrl Pts',(1.97776901413901,0.398755552237307,
-1.55979576815126));
#365010=CARTESIAN_POINT('Ctrl Pts',(1.99260464990788,0.109993480400852,
-1.57343356620573));
#365011=CARTESIAN_POINT('Ctrl Pts',(2.00005141137773,-0.0349509159166537,
-1.58027907189674));
#365012=CARTESIAN_POINT('',(2.,0.,-1.55999999999999));
#365013=CARTESIAN_POINT('',(2.,0.,-0.919999999999993));
#365014=CARTESIAN_POINT('Origin',(2.,0.,-1.23999999999999));
#365015=CARTESIAN_POINT('Ctrl Pts',(2.,0.,-1.55999999999999));
#365016=CARTESIAN_POINT('Ctrl Pts',(1.99241064492998,-0.130587723041684,
-1.56686890809951));
#365017=CARTESIAN_POINT('Ctrl Pts',(1.97719508347629,-0.392397258464091,
-1.58064007736799));
#365018=CARTESIAN_POINT('Ctrl Pts',(1.85893398363731,-0.77021102270246,
-1.60119918654349));
#365019=CARTESIAN_POINT('Ctrl Pts',(1.67368768727399,-1.11832549820161,
-1.62186792505326));
#365020=CARTESIAN_POINT('Ctrl Pts',(1.39571131210339,-1.45707132017693,
-1.64483530871634));
#365021=CARTESIAN_POINT('Ctrl Pts',(1.01139043579407,-1.75181731124514,
-1.67005611820765));
#365022=CARTESIAN_POINT('Ctrl Pts',(0.523524580955764,-1.95381930316246,
-1.69751008406315));
#365023=CARTESIAN_POINT('Ctrl Pts',(1.20190465855827E-5,-2.02305262674455,
-1.72507117444189));
#365024=CARTESIAN_POINT('Ctrl Pts',(-0.523561568763329,-1.95389710784788,
-1.75259298479139));
#365025=CARTESIAN_POINT('Ctrl Pts',(-1.0113629483914,-1.75173621412323,
-1.780063089624));
#365026=CARTESIAN_POINT('Ctrl Pts',(-1.43050093315799,-1.4305205921785,
-1.80760081005934));
#365027=CARTESIAN_POINT('Ctrl Pts',(-1.75183273711791,-1.01139909963394,
-1.83513433825238));
#365028=CARTESIAN_POINT('Ctrl Pts',(-1.95380539482055,-0.523524315658259,
-1.86260449816478));
#365029=CARTESIAN_POINT('Ctrl Pts',(-2.02304666524447,-1.35490303961885E-5,
-1.89013946985259));
#365030=CARTESIAN_POINT('Ctrl Pts',(-1.95390035588696,0.523565674211531,
-1.91767463275868));
#365031=CARTESIAN_POINT('Ctrl Pts',(-1.75173684364045,1.01136169737186,
-1.94514479238796));
#365032=CARTESIAN_POINT('Ctrl Pts',(-1.43051754853062,1.43049910707131,
-1.97267812882809));
#365033=CARTESIAN_POINT('Ctrl Pts',(-1.01140376532386,1.751835917708,-2.00021604648563));
#365034=CARTESIAN_POINT('Ctrl Pts',(-0.523519055362199,1.95380544375593,
-2.02768613156363));
#365035=CARTESIAN_POINT('Ctrl Pts',(-1.58147346400669E-5,2.02301933797135,
-2.05520780697));
#365036=CARTESIAN_POINT('Ctrl Pts',(0.523576526415156,1.95397728996109,
-2.08276891237674));
#365037=CARTESIAN_POINT('Ctrl Pts',(1.01134056343118,1.75161736636026,-2.11022353180821));
#365038=CARTESIAN_POINT('Ctrl Pts',(1.3956532037117,1.4573111045062,-2.13544185180822));
#365039=CARTESIAN_POINT('Ctrl Pts',(1.67376335733039,1.1176098884095,-2.1584161447674));
#365040=CARTESIAN_POINT('Ctrl Pts',(1.85896563746134,0.773068087902041,
-2.17906122296115));
#365041=CARTESIAN_POINT('Ctrl Pts',(1.97765410641497,0.380156426930975,
-2.19979576212585));
#365042=CARTESIAN_POINT('Ctrl Pts',(1.9924977927502,0.150312402474485,-2.21343356068965));
#365043=CARTESIAN_POINT('Ctrl Pts',(1.99994859520949,0.0349419760186854,
-2.22027906663631));
#365044=CARTESIAN_POINT('Ctrl Pts',(2.,0.,-0.919999999999993));
#365045=CARTESIAN_POINT('Ctrl Pts',(1.9924061401935,-0.1305836429736,-0.926868907781472));
#365046=CARTESIAN_POINT('Ctrl Pts',(1.97718154739341,-0.392384998448425,
-0.940640076412341));
#365047=CARTESIAN_POINT('Ctrl Pts',(1.85901893075151,-0.770264472745852,
-0.961199190461979));
#365048=CARTESIAN_POINT('Ctrl Pts',(1.67380212461465,-1.11839049672256,
-0.981867932445977));
#365049=CARTESIAN_POINT('Ctrl Pts',(1.39568858766182,-1.45707298411786,
-1.00483530662099));
#365050=CARTESIAN_POINT('Ctrl Pts',(1.01136330582357,-1.75174676674517,
-1.03005611602139));
#365051=CARTESIAN_POINT('Ctrl Pts',(0.523585702942253,-1.95400607364428,
-1.05751009591307));
#365052=CARTESIAN_POINT('Ctrl Pts',(-1.62435722739463E-5,-2.02307699179836,
-1.08507117314344));
#365053=CARTESIAN_POINT('Ctrl Pts',(-0.523536317885363,-1.95385305544458,
-1.11259298299813));
#365054=CARTESIAN_POINT('Ctrl Pts',(-1.01143313765049,-1.75187888421358,
-1.14006309809451));
#365055=CARTESIAN_POINT('Ctrl Pts',(-1.43055439145378,-1.43053532023484,
-1.16760081034308));
#365056=CARTESIAN_POINT('Ctrl Pts',(-1.7517838724523,-1.01138424804627,
-1.19513433615883));
#365057=CARTESIAN_POINT('Ctrl Pts',(-1.95395118967044,-0.52357502362932,
-1.22260450625386));
#365058=CARTESIAN_POINT('Ctrl Pts',(-2.02309840874517,1.39140831439291E-5,
-1.25013947035447));
#365059=CARTESIAN_POINT('Ctrl Pts',(-1.95385456936267,0.52354165019408,
-1.27767463061609));
#365060=CARTESIAN_POINT('Ctrl Pts',(-1.75187530264009,1.01142844098439,
-1.30514480045556));
#365061=CARTESIAN_POINT('Ctrl Pts',(-1.43053726663428,1.4305573555692,-1.33267812946709));
#365062=CARTESIAN_POINT('Ctrl Pts',(-1.01138541561949,1.75178358667915,
-1.36021604426028));
#365063=CARTESIAN_POINT('Ctrl Pts',(-0.523570999948669,1.95394672745918,
-1.38768613982889));
#365064=CARTESIAN_POINT('Ctrl Pts',(1.24423377236111E-5,2.02310883807685,
-1.41520780852107));
#365065=CARTESIAN_POINT('Ctrl Pts',(0.523542096174336,1.95385181633148,
-1.44276890960603));
#365066=CARTESIAN_POINT('Ctrl Pts',(1.0114195685531,1.75192189566403,-1.47022354238125));
#365067=CARTESIAN_POINT('Ctrl Pts',(1.39574727856968,1.45690129136922,-1.49544185654267));
#365068=CARTESIAN_POINT('Ctrl Pts',(1.67373453408061,1.11891073119414,-1.51841614397666));
#365069=CARTESIAN_POINT('Ctrl Pts',(1.85897590932335,0.768114988005871,
-1.53906122201719));
#365070=CARTESIAN_POINT('Ctrl Pts',(1.97776901413901,0.398755552237307,
-1.55979576815126));
#365071=CARTESIAN_POINT('Ctrl Pts',(1.99260464990788,0.109993480400852,
-1.57343356620573));
#365072=CARTESIAN_POINT('Ctrl Pts',(2.00005141137773,-0.0349509159166537,
-1.58027907189674));
#365073=CARTESIAN_POINT('Ctrl Pts',(2.,0.,-0.919999999999993));
#365074=CARTESIAN_POINT('Ctrl Pts',(1.9924061401935,-0.1305836429736,-0.926868907781472));
#365075=CARTESIAN_POINT('Ctrl Pts',(1.97718154739341,-0.392384998448425,
-0.940640076412341));
#365076=CARTESIAN_POINT('Ctrl Pts',(1.85901893075151,-0.770264472745852,
-0.961199190461979));
#365077=CARTESIAN_POINT('Ctrl Pts',(1.67380212461465,-1.11839049672256,
-0.981867932445977));
#365078=CARTESIAN_POINT('Ctrl Pts',(1.39568858766182,-1.45707298411786,
-1.00483530662099));
#365079=CARTESIAN_POINT('Ctrl Pts',(1.01136330582357,-1.75174676674517,
-1.03005611602139));
#365080=CARTESIAN_POINT('Ctrl Pts',(0.523585702942253,-1.95400607364428,
-1.05751009591307));
#365081=CARTESIAN_POINT('Ctrl Pts',(-1.62435722739463E-5,-2.02307699179836,
-1.08507117314344));
#365082=CARTESIAN_POINT('Ctrl Pts',(-0.523536317885363,-1.95385305544458,
-1.11259298299813));
#365083=CARTESIAN_POINT('Ctrl Pts',(-1.01143313765049,-1.75187888421358,
-1.14006309809451));
#365084=CARTESIAN_POINT('Ctrl Pts',(-1.43055439145378,-1.43053532023484,
-1.16760081034308));
#365085=CARTESIAN_POINT('Ctrl Pts',(-1.7517838724523,-1.01138424804627,
-1.19513433615883));
#365086=CARTESIAN_POINT('Ctrl Pts',(-1.95395118967044,-0.52357502362932,
-1.22260450625386));
#365087=CARTESIAN_POINT('Ctrl Pts',(-2.02309840874517,1.39140831439291E-5,
-1.25013947035447));
#365088=CARTESIAN_POINT('Ctrl Pts',(-1.95385456936267,0.52354165019408,
-1.27767463061609));
#365089=CARTESIAN_POINT('Ctrl Pts',(-1.75187530264009,1.01142844098439,
-1.30514480045556));
#365090=CARTESIAN_POINT('Ctrl Pts',(-1.43053726663428,1.4305573555692,-1.33267812946709));
#365091=CARTESIAN_POINT('Ctrl Pts',(-1.01138541561949,1.75178358667915,
-1.36021604426028));
#365092=CARTESIAN_POINT('Ctrl Pts',(-0.523570999948669,1.95394672745918,
-1.38768613982889));
#365093=CARTESIAN_POINT('Ctrl Pts',(1.24423377236111E-5,2.02310883807685,
-1.41520780852107));
#365094=CARTESIAN_POINT('Ctrl Pts',(0.523542096174336,1.95385181633148,
-1.44276890960603));
#365095=CARTESIAN_POINT('Ctrl Pts',(1.0114195685531,1.75192189566403,-1.47022354238125));
#365096=CARTESIAN_POINT('Ctrl Pts',(1.39574727856968,1.45690129136922,-1.49544185654267));
#365097=CARTESIAN_POINT('Ctrl Pts',(1.67373453408061,1.11891073119414,-1.51841614397666));
#365098=CARTESIAN_POINT('Ctrl Pts',(1.85897590932335,0.768114988005871,
-1.53906122201719));
#365099=CARTESIAN_POINT('Ctrl Pts',(1.97776901413901,0.398755552237307,
-1.55979576815126));
#365100=CARTESIAN_POINT('Ctrl Pts',(1.99260464990788,0.109993480400852,
-1.57343356620573));
#365101=CARTESIAN_POINT('Ctrl Pts',(2.00005141137773,-0.0349509159166537,
-1.58027907189674));
#365102=CARTESIAN_POINT('Ctrl Pts',(2.8,0.,-0.919999999999993));
#365103=CARTESIAN_POINT('Ctrl Pts',(2.78939199277986,-0.182993728026944,
-0.926864406801388));
#365104=CARTESIAN_POINT('Ctrl Pts',(2.76812446948309,-0.54986973906403,
-0.940626551616868));
#365105=CARTESIAN_POINT('Ctrl Pts',(2.60295543055419,-1.07729524714901,
-0.961278164543689));
#365106=CARTESIAN_POINT('Ctrl Pts',(2.3432740748819,-1.56601868287461,-0.981972834586931));
#365107=CARTESIAN_POINT('Ctrl Pts',(1.9534645938062,-2.04021452969416,-1.00482284429261));
#365108=CARTESIAN_POINT('Ctrl Pts',(1.41694431361456,-2.45199325498274,
-1.02999729271682));
#365109=CARTESIAN_POINT('Ctrl Pts',(0.732261973497512,-2.73592828705718,
-1.05766533228683));
#365110=CARTESIAN_POINT('Ctrl Pts',(-5.53107937837186E-5,-2.83213060052566,
-1.08508982617781));
#365111=CARTESIAN_POINT('Ctrl Pts',(-0.732227236330921,-2.73573484730789,
-1.11255527546237));
#365112=CARTESIAN_POINT('Ctrl Pts',(-1.41671668511953,-2.4523342703758,
-1.14018764997613));
#365113=CARTESIAN_POINT('Ctrl Pts',(-2.00264985801735,-2.00263363186375,
-1.16763896370469));
#365114=CARTESIAN_POINT('Ctrl Pts',(-2.4522378702943,-1.41666694884076,
-1.19509582612308));
#365115=CARTESIAN_POINT('Ctrl Pts',(-2.73582334389193,-0.732298418914319,
-1.22272542915656));
#365116=CARTESIAN_POINT('Ctrl Pts',(-2.83216647994848,1.05873370328634E-5,
-1.25018040117675));
#365117=CARTESIAN_POINT('Ctrl Pts',(-2.73572815948738,0.732260080199856,
-1.27763556928937));
#365118=CARTESIAN_POINT('Ctrl Pts',(-2.4523317981686,1.41670660974565,-1.30526517206592));
#365119=CARTESIAN_POINT('Ctrl Pts',(-2.0026374388973,2.0026509689249,-1.33272183775651));
#365120=CARTESIAN_POINT('Ctrl Pts',(-1.41667347271186,2.45223646417305,
-1.3601733539516));
#365121=CARTESIAN_POINT('Ctrl Pts',(-0.73226691430792,2.73582715423785,
-1.38780570894782));
#365122=CARTESIAN_POINT('Ctrl Pts',(-3.32541419378344E-5,2.83216215152901,
-1.41527101711875));
#365123=CARTESIAN_POINT('Ctrl Pts',(0.732213474069494,2.73577655753039,
-1.44269553505523));
#365124=CARTESIAN_POINT('Ctrl Pts',(1.41699596320263,2.45216677851596,-1.47036422641732));
#365125=CARTESIAN_POINT('Ctrl Pts',(1.95351849625047,2.04006124129144,-1.49553618329511));
#365126=CARTESIAN_POINT('Ctrl Pts',(2.34320434404536,1.56650518466477,-1.51839309578454));
#365127=CARTESIAN_POINT('Ctrl Pts',(2.60290758877066,1.07529461519169,-1.5390641373972));
#365128=CARTESIAN_POINT('Ctrl Pts',(2.7689186260588,0.55507555381449,-1.55989143937075));
#365129=CARTESIAN_POINT('Ctrl Pts',(2.78964685205658,0.162241467065363,
-1.57352004288224));
#365130=CARTESIAN_POINT('Ctrl Pts',(2.80005140479051,-0.0349419760186688,
-1.58036093336367));
#365131=CARTESIAN_POINT('Ctrl Pts',(2.8,0.,-1.55999999999999));
#365132=CARTESIAN_POINT('Ctrl Pts',(2.78939649751634,-0.182997808095028,
-1.56686440711942));
#365133=CARTESIAN_POINT('Ctrl Pts',(2.76813800556597,-0.549881999079696,
-1.58062655257252));
#365134=CARTESIAN_POINT('Ctrl Pts',(2.60287048343998,-1.07724179710562,
-1.6012781606252));
#365135=CARTESIAN_POINT('Ctrl Pts',(2.34315963754124,-1.56595368435367,
-1.62197282719421));
#365136=CARTESIAN_POINT('Ctrl Pts',(1.95348731824777,-2.04021286575323,
-1.64482284638796));
#365137=CARTESIAN_POINT('Ctrl Pts',(1.41697144358507,-2.45206379948272,
-1.66999729490308));
#365138=CARTESIAN_POINT('Ctrl Pts',(0.732200851511023,-2.73574151657536,
-1.69766532043691));
#365139=CARTESIAN_POINT('Ctrl Pts',(-2.70481749242659E-5,-2.83210623547185,
-1.72508982747625));
#365140=CARTESIAN_POINT('Ctrl Pts',(-0.732252487208887,-2.73577889971119,
-1.75255527725563));
#365141=CARTESIAN_POINT('Ctrl Pts',(-1.41664649586044,-2.45219160028545,
-1.78018764150562));
#365142=CARTESIAN_POINT('Ctrl Pts',(-2.00259639972156,-2.00261890380741,
-1.80763896342095));
#365143=CARTESIAN_POINT('Ctrl Pts',(-2.45228673495991,-1.41668180042844,
-1.83509582821663));
#365144=CARTESIAN_POINT('Ctrl Pts',(-2.73567754904204,-0.732247710943258,
-1.86272542106748));
#365145=CARTESIAN_POINT('Ctrl Pts',(-2.83211473644778,-1.68757765071671E-5,
-1.89018040067487));
#365146=CARTESIAN_POINT('Ctrl Pts',(-2.73577394601168,0.732284104217307,
-1.91763557143196));
#365147=CARTESIAN_POINT('Ctrl Pts',(-2.45219333916896,1.41663986613312,
-1.94526516399832));
#365148=CARTESIAN_POINT('Ctrl Pts',(-2.00261772079364,2.00259272042701,
-1.9727218371175));
#365149=CARTESIAN_POINT('Ctrl Pts',(-1.41669182241623,2.4522887952019,-2.00017335617694));
#365150=CARTESIAN_POINT('Ctrl Pts',(-0.732214969721451,2.73568587053461,
-2.02780570068256));
#365151=CARTESIAN_POINT('Ctrl Pts',(-6.15112143014144E-5,2.83207265142351,
-2.05527101556769));
#365152=CARTESIAN_POINT('Ctrl Pts',(0.732247904310314,2.73590203116,-2.08269553782593));
#365153=CARTESIAN_POINT('Ctrl Pts',(1.41691695808072,2.45186224921218,-2.11036421584428));
#365154=CARTESIAN_POINT('Ctrl Pts',(1.95342442139249,2.04047105442842,-2.13553617856065));
#365155=CARTESIAN_POINT('Ctrl Pts',(2.34323316729515,1.56520434188013,-2.15839309657528));
#365156=CARTESIAN_POINT('Ctrl Pts',(2.60289731690865,1.08024771508786,-2.17906413834116));
#365157=CARTESIAN_POINT('Ctrl Pts',(2.76880371833477,0.536476428508159,
-2.19989143334533));
#365158=CARTESIAN_POINT('Ctrl Pts',(2.7895399948989,0.202560389138996,-2.21352003736615));
#365159=CARTESIAN_POINT('Ctrl Pts',(2.79994858862227,0.0349509159166703,
-2.22036092810323));
#365160=CARTESIAN_POINT('Ctrl Pts',(2.,0.,-1.55999999999999));
#365161=CARTESIAN_POINT('Ctrl Pts',(1.99241064492998,-0.130587723041684,
-1.56686890809951));
#365162=CARTESIAN_POINT('Ctrl Pts',(1.97719508347629,-0.392397258464091,
-1.58064007736799));
#365163=CARTESIAN_POINT('Ctrl Pts',(1.85893398363731,-0.77021102270246,
-1.60119918654349));
#365164=CARTESIAN_POINT('Ctrl Pts',(1.67368768727399,-1.11832549820161,
-1.62186792505326));
#365165=CARTESIAN_POINT('Ctrl Pts',(1.39571131210339,-1.45707132017693,
-1.64483530871634));
#365166=CARTESIAN_POINT('Ctrl Pts',(1.01139043579407,-1.75181731124514,
-1.67005611820765));
#365167=CARTESIAN_POINT('Ctrl Pts',(0.523524580955764,-1.95381930316246,
-1.69751008406315));
#365168=CARTESIAN_POINT('Ctrl Pts',(1.20190465855827E-5,-2.02305262674455,
-1.72507117444189));
#365169=CARTESIAN_POINT('Ctrl Pts',(-0.523561568763329,-1.95389710784788,
-1.75259298479139));
#365170=CARTESIAN_POINT('Ctrl Pts',(-1.0113629483914,-1.75173621412323,
-1.780063089624));
#365171=CARTESIAN_POINT('Ctrl Pts',(-1.43050093315799,-1.4305205921785,
-1.80760081005934));
#365172=CARTESIAN_POINT('Ctrl Pts',(-1.75183273711791,-1.01139909963394,
-1.83513433825238));
#365173=CARTESIAN_POINT('Ctrl Pts',(-1.95380539482055,-0.523524315658259,
-1.86260449816478));
#365174=CARTESIAN_POINT('Ctrl Pts',(-2.02304666524447,-1.35490303961885E-5,
-1.89013946985259));
#365175=CARTESIAN_POINT('Ctrl Pts',(-1.95390035588696,0.523565674211531,
-1.91767463275868));
#365176=CARTESIAN_POINT('Ctrl Pts',(-1.75173684364045,1.01136169737186,
-1.94514479238796));
#365177=CARTESIAN_POINT('Ctrl Pts',(-1.43051754853062,1.43049910707131,
-1.97267812882809));
#365178=CARTESIAN_POINT('Ctrl Pts',(-1.01140376532386,1.751835917708,-2.00021604648563));
#365179=CARTESIAN_POINT('Ctrl Pts',(-0.523519055362199,1.95380544375593,
-2.02768613156363));
#365180=CARTESIAN_POINT('Ctrl Pts',(-1.58147346400669E-5,2.02301933797135,
-2.05520780697));
#365181=CARTESIAN_POINT('Ctrl Pts',(0.523576526415156,1.95397728996109,
-2.08276891237674));
#365182=CARTESIAN_POINT('Ctrl Pts',(1.01134056343118,1.75161736636026,-2.11022353180821));
#365183=CARTESIAN_POINT('Ctrl Pts',(1.3956532037117,1.4573111045062,-2.13544185180822));
#365184=CARTESIAN_POINT('Ctrl Pts',(1.67376335733039,1.1176098884095,-2.1584161447674));
#365185=CARTESIAN_POINT('Ctrl Pts',(1.85896563746134,0.773068087902041,
-2.17906122296115));
#365186=CARTESIAN_POINT('Ctrl Pts',(1.97765410641497,0.380156426930975,
-2.19979576212585));
#365187=CARTESIAN_POINT('Ctrl Pts',(1.9924977927502,0.150312402474485,-2.21343356068965));
#365188=CARTESIAN_POINT('Ctrl Pts',(1.99994859520949,0.0349419760186854,
-2.22027906663631));
#365189=CARTESIAN_POINT('Ctrl Pts',(1.2,0.,-1.55999999999999));
#365190=CARTESIAN_POINT('Ctrl Pts',(1.19542479234362,-0.0781776379883396,
-1.56687340907959));
#365191=CARTESIAN_POINT('Ctrl Pts',(1.18625216138661,-0.234912517848486,
-1.58065360216347));
#365192=CARTESIAN_POINT('Ctrl Pts',(1.11499748383463,-0.4631802482993,-1.60112021246178));
#365193=CARTESIAN_POINT('Ctrl Pts',(1.00421573700674,-0.670697312049558,
-1.62176302291231));
#365194=CARTESIAN_POINT('Ctrl Pts',(0.837935305959016,-0.873929774600632,
-1.64484777104472));
#365195=CARTESIAN_POINT('Ctrl Pts',(0.60580942800308,-1.05157082300757,
-1.67011494151222));
#365196=CARTESIAN_POINT('Ctrl Pts',(0.314848310400505,-1.17189708974956,
-1.6973548476894));
#365197=CARTESIAN_POINT('Ctrl Pts',(5.10862680953333E-5,-1.21399901801725,
-1.72505252140752));
#365198=CARTESIAN_POINT('Ctrl Pts',(-0.31487065031777,-1.17201531598458,
-1.75263069232715));
#365199=CARTESIAN_POINT('Ctrl Pts',(-0.606079400922359,-1.05128082796102,
-1.77993853774237));
#365200=CARTESIAN_POINT('Ctrl Pts',(-0.858405466594417,-0.858422280549586,
-1.80756265669772));
#365201=CARTESIAN_POINT('Ctrl Pts',(-1.0513787392759,-0.606116398839451,
-1.83517284828813));
#365202=CARTESIAN_POINT('Ctrl Pts',(-1.17193324059906,-0.31480092037326,
-1.86248357526207));
#365203=CARTESIAN_POINT('Ctrl Pts',(-1.21397859404116,-1.02222842850628E-5,
-1.89009853903031));
#365204=CARTESIAN_POINT('Ctrl Pts',(-1.17202676576225,0.314847244205754,
-1.9177136940854));
#365205=CARTESIAN_POINT('Ctrl Pts',(-1.05128034811194,0.606083528610609,
-1.9450244207776));
#365206=CARTESIAN_POINT('Ctrl Pts',(-0.858417376267602,0.858405493715605,
-1.97263442053868));
#365207=CARTESIAN_POINT('Ctrl Pts',(-0.606115708231486,1.05138304021409,
-2.00025873679431));
#365208=CARTESIAN_POINT('Ctrl Pts',(-0.314823141002948,1.17192501697726,
-2.0275665624447));
#365209=CARTESIAN_POINT('Ctrl Pts',(2.98817450213404E-5,1.21396602451919,
-2.05514459837232));
#365210=CARTESIAN_POINT('Ctrl Pts',(0.314905148519997,1.17205254876217,
-2.08284228692754));
#365211=CARTESIAN_POINT('Ctrl Pts',(0.605764168781643,1.05137248350833,
-2.11008284777213));
#365212=CARTESIAN_POINT('Ctrl Pts',(0.837881986030918,0.874151154583981,
-2.13534752505579));
#365213=CARTESIAN_POINT('Ctrl Pts',(1.00429354736563,0.670015434938871,
-2.15843919295953));
#365214=CARTESIAN_POINT('Ctrl Pts',(1.11503395801403,0.465888460716222,
-2.17905830758114));
#365215=CARTESIAN_POINT('Ctrl Pts',(1.18650449449518,0.223836425353792,
-2.19970009090637));
#365216=CARTESIAN_POINT('Ctrl Pts',(1.1954555906015,0.0980644158099734,
-2.21334708401314));
#365217=CARTESIAN_POINT('Ctrl Pts',(1.19994860179671,0.0349330361207006,
-2.22019720516939));
#365218=CARTESIAN_POINT('Ctrl Pts',(1.2,0.,-0.919999999999993));
#365219=CARTESIAN_POINT('Ctrl Pts',(1.19542028760714,-0.0781735579202564,
-0.926873408761556));
#365220=CARTESIAN_POINT('Ctrl Pts',(1.18623862530372,-0.23490025783282,
-0.940653601207814));
#365221=CARTESIAN_POINT('Ctrl Pts',(1.11508243094883,-0.463233698342691,
-0.961120216380269));
#365222=CARTESIAN_POINT('Ctrl Pts',(1.0043301743474,-0.670762310570501,
-0.981763030305022));
#365223=CARTESIAN_POINT('Ctrl Pts',(0.837912581517445,-0.873931438541563,
-1.00484776894937));
#365224=CARTESIAN_POINT('Ctrl Pts',(0.605782298032579,-1.0515002785076,
-1.03011493932597));
#365225=CARTESIAN_POINT('Ctrl Pts',(0.314909432386994,-1.17208386023138,
-1.05735485953932));
#365226=CARTESIAN_POINT('Ctrl Pts',(2.28236492357989E-5,-1.21402338307106,
-1.08505252010907));
#365227=CARTESIAN_POINT('Ctrl Pts',(-0.314845399439805,-1.17197126358128,
-1.11263069053389));
#365228=CARTESIAN_POINT('Ctrl Pts',(-0.606149590181453,-1.05142349805137,
-1.13993854621288));
#365229=CARTESIAN_POINT('Ctrl Pts',(-0.858458924890206,-0.858437008605928,
-1.16756265698147));
#365230=CARTESIAN_POINT('Ctrl Pts',(-1.05132987461029,-0.606101547251777,
-1.19517284619458));
#365231=CARTESIAN_POINT('Ctrl Pts',(-1.17207903544895,-0.314851628344321,
-1.22248358335115));
#365232=CARTESIAN_POINT('Ctrl Pts',(-1.21403033754186,1.72408292549676E-5,
-1.25009853953219));
#365233=CARTESIAN_POINT('Ctrl Pts',(-1.17198097923795,0.314823220188304,
-1.27771369194281));
#365234=CARTESIAN_POINT('Ctrl Pts',(-1.05141880711158,0.60615027222314,
-1.3050244288452));
#365235=CARTESIAN_POINT('Ctrl Pts',(-0.858437094371262,0.858463742213499,
-1.33263442117768));
#365236=CARTESIAN_POINT('Ctrl Pts',(-0.606097358527115,1.05133070918524,
-1.36025873456897));
#365237=CARTESIAN_POINT('Ctrl Pts',(-0.314875085589417,1.1720663006805,
-1.38756657070996));
#365238=CARTESIAN_POINT('Ctrl Pts',(5.81388173850348E-5,1.21405552462469,
-1.41514459992339));
#365239=CARTESIAN_POINT('Ctrl Pts',(0.314870718279177,1.17192707513256,
-1.44284228415683));
#365240=CARTESIAN_POINT('Ctrl Pts',(0.60584317390356,1.05167701281211,-1.47008285834517));
#365241=CARTESIAN_POINT('Ctrl Pts',(0.837976060888895,0.873741341447001,
-1.49534752979024));
#365242=CARTESIAN_POINT('Ctrl Pts',(1.00426472411585,0.671316277723509,
-1.51843919216879));
#365243=CARTESIAN_POINT('Ctrl Pts',(1.11504422987604,0.460935360820052,
-1.53905830663718));
#365244=CARTESIAN_POINT('Ctrl Pts',(1.18661940221922,0.242435550660123,
-1.55970009693178));
#365245=CARTESIAN_POINT('Ctrl Pts',(1.19556244775918,0.0577454937363405,
-1.57334708952923));
#365246=CARTESIAN_POINT('Ctrl Pts',(1.20005141796495,-0.0349598558146385,
-1.58019721042982));
#365247=CARTESIAN_POINT('Ctrl Pts',(2.,0.,-0.919999999999993));
#365248=CARTESIAN_POINT('Ctrl Pts',(1.9924061401935,-0.1305836429736,-0.926868907781472));
#365249=CARTESIAN_POINT('Ctrl Pts',(1.97718154739341,-0.392384998448425,
-0.940640076412341));
#365250=CARTESIAN_POINT('Ctrl Pts',(1.85901893075151,-0.770264472745852,
-0.961199190461979));
#365251=CARTESIAN_POINT('Ctrl Pts',(1.67380212461465,-1.11839049672256,
-0.981867932445977));
#365252=CARTESIAN_POINT('Ctrl Pts',(1.39568858766182,-1.45707298411786,
-1.00483530662099));
#365253=CARTESIAN_POINT('Ctrl Pts',(1.01136330582357,-1.75174676674517,
-1.03005611602139));
#365254=CARTESIAN_POINT('Ctrl Pts',(0.523585702942253,-1.95400607364428,
-1.05751009591307));
#365255=CARTESIAN_POINT('Ctrl Pts',(-1.62435722739463E-5,-2.02307699179836,
-1.08507117314344));
#365256=CARTESIAN_POINT('Ctrl Pts',(-0.523536317885363,-1.95385305544458,
-1.11259298299813));
#365257=CARTESIAN_POINT('Ctrl Pts',(-1.01143313765049,-1.75187888421358,
-1.14006309809451));
#365258=CARTESIAN_POINT('Ctrl Pts',(-1.43055439145378,-1.43053532023484,
-1.16760081034308));
#365259=CARTESIAN_POINT('Ctrl Pts',(-1.7517838724523,-1.01138424804627,
-1.19513433615883));
#365260=CARTESIAN_POINT('Ctrl Pts',(-1.95395118967044,-0.52357502362932,
-1.22260450625386));
#365261=CARTESIAN_POINT('Ctrl Pts',(-2.02309840874517,1.39140831439291E-5,
-1.25013947035447));
#365262=CARTESIAN_POINT('Ctrl Pts',(-1.95385456936267,0.52354165019408,
-1.27767463061609));
#365263=CARTESIAN_POINT('Ctrl Pts',(-1.75187530264009,1.01142844098439,
-1.30514480045556));
#365264=CARTESIAN_POINT('Ctrl Pts',(-1.43053726663428,1.4305573555692,-1.33267812946709));
#365265=CARTESIAN_POINT('Ctrl Pts',(-1.01138541561949,1.75178358667915,
-1.36021604426028));
#365266=CARTESIAN_POINT('Ctrl Pts',(-0.523570999948669,1.95394672745918,
-1.38768613982889));
#365267=CARTESIAN_POINT('Ctrl Pts',(1.24423377236111E-5,2.02310883807685,
-1.41520780852107));
#365268=CARTESIAN_POINT('Ctrl Pts',(0.523542096174336,1.95385181633148,
-1.44276890960603));
#365269=CARTESIAN_POINT('Ctrl Pts',(1.0114195685531,1.75192189566403,-1.47022354238125));
#365270=CARTESIAN_POINT('Ctrl Pts',(1.39574727856968,1.45690129136922,-1.49544185654267));
#365271=CARTESIAN_POINT('Ctrl Pts',(1.67373453408061,1.11891073119414,-1.51841614397666));
#365272=CARTESIAN_POINT('Ctrl Pts',(1.85897590932335,0.768114988005871,
-1.53906122201719));
#365273=CARTESIAN_POINT('Ctrl Pts',(1.97776901413901,0.398755552237307,
-1.55979576815126));
#365274=CARTESIAN_POINT('Ctrl Pts',(1.99260464990788,0.109993480400852,
-1.57343356620573));
#365275=CARTESIAN_POINT('Ctrl Pts',(2.00005141137773,-0.0349509159166537,
-1.58027907189674));
#365276=CARTESIAN_POINT('Origin',(2.,0.,-1.23999999999999));
#365277=CARTESIAN_POINT('',(2.27188945184575,0.0256276272719289,-2.13498880343698));
#365278=CARTESIAN_POINT('Origin',(2.00000000329361,-4.46994898409183E-6,
-1.90027906926653));
#365279=CARTESIAN_POINT('Origin',(2.00000000329361,-4.46994898409183E-6,
-1.90027906926653));
#365280=CARTESIAN_POINT('Origin',(2.,0.,-1.23999999999999));
#365281=CARTESIAN_POINT('Ctrl Pts',(2.00005141137773,-0.0349509159166537,
-1.58027907189674));
#365282=CARTESIAN_POINT('Ctrl Pts',(2.00005141137773,-0.209477500702,-1.59705901785001));
#365283=CARTESIAN_POINT('Ctrl Pts',(1.93937485936534,-0.574981221086946,
-1.64398167301615));
#365284=CARTESIAN_POINT('Ctrl Pts',(1.72866575619624,-1.05218683017129,
-1.70157781695483));
#365285=CARTESIAN_POINT('Ctrl Pts',(1.39603065320521,-1.46514475575449,
-1.76296158741006));
#365286=CARTESIAN_POINT('Ctrl Pts',(0.969522180315677,-1.77589106055163,
-1.82311912419573));
#365287=CARTESIAN_POINT('Ctrl Pts',(0.476783238604109,-1.96670288995313,
-1.88346520364747));
#365288=CARTESIAN_POINT('Ctrl Pts',(-0.0484603850821368,-2.02312932285366,
-1.94396055370022));
#365289=CARTESIAN_POINT('Ctrl Pts',(-0.570338856925993,-1.94138942628423,
-2.00439291407465));
#365290=CARTESIAN_POINT('Ctrl Pts',(-1.05344948325284,-1.72773686772633,
-2.06470891120488));
#365291=CARTESIAN_POINT('Ctrl Pts',(-1.46487312544728,-1.39632835696345,
-2.1251726344757));
#365292=CARTESIAN_POINT('Ctrl Pts',(-1.77606001340043,-0.969474639293403,
-2.18562457894241));
#365293=CARTESIAN_POINT('Ctrl Pts',(-1.9665886161183,-0.476795144252666,
-2.2459421237894));
#365294=CARTESIAN_POINT('Ctrl Pts',(-2.0231790616074,0.0484698229690482,
-2.30639998925771));
#365295=CARTESIAN_POINT('Ctrl Pts',(-1.94138573006516,0.570342005097921,
-2.36685494461854));
#365296=CARTESIAN_POINT('Ctrl Pts',(-1.72773301625381,1.05344259449438,
-2.42717237256682));
#365297=CARTESIAN_POINT('Ctrl Pts',(-1.39633042998923,1.46487729238585,
-2.48762977035772));
#365298=CARTESIAN_POINT('Ctrl Pts',(-0.969474291036093,1.77605966206198,
-2.54808497616048));
#365299=CARTESIAN_POINT('Ctrl Pts',(-0.476795343347378,1.96658811640277,
-2.6084023881129));
#365300=CARTESIAN_POINT('Ctrl Pts',(0.0484699602192744,2.02317939996145,
-2.66885975673847));
#365301=CARTESIAN_POINT('Ctrl Pts',(0.570341982836039,1.94138567238666,
-2.72931497821885));
#365302=CARTESIAN_POINT('Ctrl Pts',(1.05344257210098,1.72773301387229,-2.78963238875962));
#365303=CARTESIAN_POINT('Ctrl Pts',(1.46487731147791,1.39633043581364,-2.85008975616076));
#365304=CARTESIAN_POINT('Ctrl Pts',(1.7760596572503,0.96947429019414,-2.91054497830833));
#365305=CARTESIAN_POINT('Ctrl Pts',(1.96658811657123,0.47679534386094,-2.97086238877306));
#365306=CARTESIAN_POINT('Ctrl Pts',(2.02317940049204,-0.0484699606166185,
-3.03131975614836));
#365307=CARTESIAN_POINT('Ctrl Pts',(1.94138567221384,-0.570341982644115,
-3.09177497831011));
#365308=CARTESIAN_POINT('Ctrl Pts',(1.72773301391076,-1.05344257214956,
-3.15209238877301));
#365309=CARTESIAN_POINT('Ctrl Pts',(1.39633043580907,-1.46487731147983,
-3.21254975614839));
#365310=CARTESIAN_POINT('Ctrl Pts',(0.969474290197969,-1.77605965724421,
-3.27300497831004));
#365311=CARTESIAN_POINT('Ctrl Pts',(0.476795343858464,-1.96658811657341,
-3.33332238877311));
#365312=CARTESIAN_POINT('Ctrl Pts',(-0.0484699606159255,-2.0231794004916,
-3.39377975614832));
#365313=CARTESIAN_POINT('Ctrl Pts',(-0.570341982644268,-1.94138567221424,
-3.45423497831005));
#365314=CARTESIAN_POINT('Ctrl Pts',(-1.05344257214943,-1.72773301391041,
-3.51455238877311));
#365315=CARTESIAN_POINT('Ctrl Pts',(-1.46487731147993,-1.39633043580919,
-3.57500975614831));
#365316=CARTESIAN_POINT('Ctrl Pts',(-1.77605965724425,-0.969474290197954,
-3.63546497831004));
#365317=CARTESIAN_POINT('Ctrl Pts',(-1.96658811657337,-0.476795343858458,
-3.69578238877312));
#365318=CARTESIAN_POINT('Ctrl Pts',(-2.02317940049162,0.0484699606159343,
-3.75623975614831));
#365319=CARTESIAN_POINT('Ctrl Pts',(-1.94138567221425,0.570341982644281,
-3.81669497831005));
#365320=CARTESIAN_POINT('Ctrl Pts',(-1.7277330139104,1.05344257214943,-3.87701238877311));
#365321=CARTESIAN_POINT('Ctrl Pts',(-1.39633043580919,1.46487731147993,
-3.93746975614831));
#365322=CARTESIAN_POINT('Ctrl Pts',(-0.969474290197942,1.77605965724426,
-3.99792497831004));
#365323=CARTESIAN_POINT('Ctrl Pts',(-0.476795343858452,1.96658811657335,
-4.05824238877313));
#365324=CARTESIAN_POINT('Ctrl Pts',(0.0484699606159434,2.02317940049163,
-4.11869975614831));
#365325=CARTESIAN_POINT('Ctrl Pts',(0.570341982644284,1.94138567221424,
-4.17915497831005));
#365326=CARTESIAN_POINT('Ctrl Pts',(1.05344257214943,1.72773301391039,-4.23947238877311));
#365327=CARTESIAN_POINT('Ctrl Pts',(1.46487731147993,1.39633043580918,-4.29992975614832));
#365328=CARTESIAN_POINT('Ctrl Pts',(1.77605965724427,0.969474290197945,
-4.36038497831003));
#365329=CARTESIAN_POINT('Ctrl Pts',(1.96658811657337,0.476795343858441,
-4.42070238877312));
#365330=CARTESIAN_POINT('Ctrl Pts',(2.02317940049162,-0.0484699606159445,
-4.48115975614831));
#365331=CARTESIAN_POINT('Ctrl Pts',(1.94138567221424,-0.570341982644292,
-4.54161497831005));
#365332=CARTESIAN_POINT('Ctrl Pts',(1.72773301391038,-1.05344257214943,
-4.60193238877312));
#365333=CARTESIAN_POINT('Ctrl Pts',(1.39633043580918,-1.46487731147994,
-4.66238975614831));
#365334=CARTESIAN_POINT('Ctrl Pts',(0.969474290197935,-1.77605965724426,
-4.72284497831004));
#365335=CARTESIAN_POINT('Ctrl Pts',(0.476795343858439,-1.96658811657337,
-4.78316238877312));
#365336=CARTESIAN_POINT('Ctrl Pts',(-0.0484699606159579,-2.02317940049164,
-4.8436197561483));
#365337=CARTESIAN_POINT('Ctrl Pts',(-0.570341982644288,-1.94138567221422,
-4.90407497831006));
#365338=CARTESIAN_POINT('Ctrl Pts',(-1.05344257214943,-1.72773301391037,
-4.96439238877312));
#365339=CARTESIAN_POINT('Ctrl Pts',(-1.46487731147995,-1.39633043580918,
-5.02484975614831));
#365340=CARTESIAN_POINT('Ctrl Pts',(-1.77605965724426,-0.969474290197928,
-5.08530497831004));
#365341=CARTESIAN_POINT('Ctrl Pts',(-1.96658811657335,-0.476795343858433,
-5.14562238877313));
#365342=CARTESIAN_POINT('Ctrl Pts',(-2.02317940049163,0.0484699606159606,
-5.2060797561483));
#365343=CARTESIAN_POINT('Ctrl Pts',(-1.94138567221425,0.570341982644311,
-5.26653497831003));
#365344=CARTESIAN_POINT('Ctrl Pts',(-1.72773301391036,1.05344257214944,
-5.32685238877313));
#365345=CARTESIAN_POINT('Ctrl Pts',(-1.39633043580918,1.46487731147996,
-5.3873097561483));
#365346=CARTESIAN_POINT('Ctrl Pts',(-0.969474290197916,1.77605965724424,
-5.44776497831006));
#365347=CARTESIAN_POINT('Ctrl Pts',(-0.476795343858422,1.96658811657339,
-5.5080823887731));
#365348=CARTESIAN_POINT('Ctrl Pts',(0.0484699606159706,2.02317940049163,
-5.56853975614829));
#365349=CARTESIAN_POINT('Ctrl Pts',(0.570341982644291,1.94138567221422,
-5.62899497831007));
#365350=CARTESIAN_POINT('Ctrl Pts',(1.05344257214944,1.72773301391032,-5.68931238877313));
#365351=CARTESIAN_POINT('Ctrl Pts',(1.46487731147996,1.3963304358092,-5.74976975614823));
#365352=CARTESIAN_POINT('Ctrl Pts',(1.77605965724441,0.969474290197947,
-5.81022497831013));
#365353=CARTESIAN_POINT('Ctrl Pts',(1.96658811657315,0.476795343858267,
-5.87054238877304));
#365354=CARTESIAN_POINT('Ctrl Pts',(2.02317940049197,-0.0484699606151168,
-5.93099975614826));
#365355=CARTESIAN_POINT('Ctrl Pts',(1.94138567221262,-0.570341982647331,
-5.99145497831012));
#365356=CARTESIAN_POINT('Ctrl Pts',(1.72773301391079,-1.05344257214282,
-6.05177238877488));
#365357=CARTESIAN_POINT('Ctrl Pts',(1.39633043583791,-1.46487731150212,
-6.1122297561358));
#365358=CARTESIAN_POINT('Ctrl Pts',(0.969474290103704,-1.77605965719443,
-6.17268497832268));
#365359=CARTESIAN_POINT('Ctrl Pts',(0.476795344014053,-1.96658811647506,
-6.23300238886911));
#365360=CARTESIAN_POINT('Ctrl Pts',(-0.0484699607888847,-2.02317940162764,
-6.293459755551));
#365361=CARTESIAN_POINT('Ctrl Pts',(-0.570341982515374,-1.94138566986718,
-6.35391497894857));
#365362=CARTESIAN_POINT('Ctrl Pts',(-1.0534425689941,-1.72773301427299,
-6.41423239105532));
#365363=CARTESIAN_POINT('Ctrl Pts',(-1.46487733129139,-1.39633044764682,
-6.47468974174144));
#365364=CARTESIAN_POINT('Ctrl Pts',(-1.77605962440754,-0.969474272408487,
-6.53514499410053));
#365365=CARTESIAN_POINT('Ctrl Pts',(-1.96658808441403,-0.4767953693466,
-6.59546242507117));
#365366=CARTESIAN_POINT('Ctrl Pts',(-2.02317971788315,0.0484700612956726,
-6.65591951867769));
#365367=CARTESIAN_POINT('Ctrl Pts',(-1.94138529374751,0.57034175258804,
-6.71637524065362));
#365368=CARTESIAN_POINT('Ctrl Pts',(-1.7277327906675,1.05344225923825,-6.77669281345839));
#365369=CARTESIAN_POINT('Ctrl Pts',(-1.39633190064527,1.46488023063332,
-6.83714685373563));
#365370=CARTESIAN_POINT('Ctrl Pts',(-0.969474795144666,1.77605674551469,
-6.89760831895014));
#365371=CARTESIAN_POINT('Ctrl Pts',(-0.476792483974202,1.96658170561334,
-6.95792512927773));
#365372=CARTESIAN_POINT('Ctrl Pts',(0.0484734593030573,2.0232081210323,
-7.01835708981697));
#365373=CARTESIAN_POINT('Ctrl Pts',(0.570336624689882,1.94136175768686,
-7.07885725203471));
#365374=CARTESIAN_POINT('Ctrl Pts',(1.05340619968671,1.72778052727257,-7.13918044053492));
#365375=CARTESIAN_POINT('Ctrl Pts',(1.46503146071072,1.39600002911185,-7.19942807213429));
#365376=CARTESIAN_POINT('Ctrl Pts',(1.77572739170825,0.970967789756964,
-7.26046972816476));
#365377=CARTESIAN_POINT('Ctrl Pts',(1.9679960876878,0.471734127632586,-7.31921124624962));
#365378=CARTESIAN_POINT('Ctrl Pts',(2.00016367750205,0.139563645186354,
-7.36277016686196));
#365379=CARTESIAN_POINT('Ctrl Pts',(2.00016367750204,-0.0349606549172864,
-7.37954989315336));
#365380=CARTESIAN_POINT('Ctrl Pts',(1.20005141796495,-0.0349598558146385,
-1.58019721042982));
#365381=CARTESIAN_POINT('Ctrl Pts',(1.20005141796495,-0.196639509400045,
-1.59574198174499));
#365382=CARTESIAN_POINT('Ctrl Pts',(1.15732797686238,-0.340816716447164,
-1.6447382432052));
#365383=CARTESIAN_POINT('Ctrl Pts',(1.02794595474197,-0.654182454634222,
-1.70085757593186));
#365384=CARTESIAN_POINT('Ctrl Pts',(0.824371570064879,-0.890750973398493,
-1.76298366242172));
#365385=CARTESIAN_POINT('Ctrl Pts',(0.563969291479731,-1.07614468532721,
-1.82314153495176));
#365386=CARTESIAN_POINT('Ctrl Pts',(0.268053015090469,-1.18466145511491,
-1.88305373693166));
#365387=CARTESIAN_POINT('Ctrl Pts',(-0.0484395870237313,-1.21410753423567,
-1.9438363016732));
#365388=CARTESIAN_POINT('Ctrl Pts',(-0.361651032204537,-1.15949959431507,
-2.00439370017114));
#365389=CARTESIAN_POINT('Ctrl Pts',(-0.648204859882796,-1.02726348852071,
-2.06435695179187));
#365390=CARTESIAN_POINT('Ctrl Pts',(-0.892791267502041,-0.824210832808723,
-2.12500826054469));
#365391=CARTESIAN_POINT('Ctrl Pts',(-1.07560894612736,-0.564190577762509,
-2.18562659547641));
#365392=CARTESIAN_POINT('Ctrl Pts',(-1.1847293912525,-0.268030428045687,
-2.24559800960236));
#365393=CARTESIAN_POINT('Ctrl Pts',(-1.21410751416084,0.0484963826130714,
-2.30623010797513));
#365394=CARTESIAN_POINT('Ctrl Pts',(-1.1595132046369,0.36162639690026,-2.36685750692005));
#365395=CARTESIAN_POINT('Ctrl Pts',(-1.02725604518277,0.648203827608334,
-2.42682890216184));
#365396=CARTESIAN_POINT('Ctrl Pts',(-0.824211659423609,0.892796064601774,
-2.48745940373019));
#365397=CARTESIAN_POINT('Ctrl Pts',(-0.564191142051916,1.07560808882016,
-2.54808760329284));
#365398=CARTESIAN_POINT('Ctrl Pts',(-0.268030403610479,1.18472901687534,
-2.60805895542665));
#365399=CARTESIAN_POINT('Ctrl Pts',(0.0484964956129267,1.21410782343574,
-2.66868935921047));
#365400=CARTESIAN_POINT('Ctrl Pts',(0.361626396132377,1.15951315047799,
-2.72931761037603));
#365401=CARTESIAN_POINT('Ctrl Pts',(0.648203803824844,1.0272560382112,-2.78928895746987));
#365402=CARTESIAN_POINT('Ctrl Pts',(0.892796076188025,0.824211675103123,
-2.84991935728737));
#365403=CARTESIAN_POINT('Ctrl Pts',(1.07560808862158,0.56419113400383,-2.91054761072926));
#365404=CARTESIAN_POINT('Ctrl Pts',(1.18472901588199,0.26803040550146,-2.97051895749492));
#365405=CARTESIAN_POINT('Ctrl Pts',(1.21410782431058,-0.0484964950668307,
-3.03114935724649));
#365406=CARTESIAN_POINT('Ctrl Pts',(1.15951315008857,-0.361626396645578,
-3.09177761073831));
#365407=CARTESIAN_POINT('Ctrl Pts',(1.02725603829716,-0.6482038036989,-3.15174895749339));
#365408=CARTESIAN_POINT('Ctrl Pts',(0.824211675135244,-0.892796076188428,
-3.21237935724692));
#365409=CARTESIAN_POINT('Ctrl Pts',(0.564191133978922,-1.07560808862653,
-3.27300761073802));
#365410=CARTESIAN_POINT('Ctrl Pts',(0.268030405508416,-1.18472901588096,
-3.33297895749366));
#365411=CARTESIAN_POINT('Ctrl Pts',(-0.0484964950686988,-1.21410782431092,
-3.39360935724675));
#365412=CARTESIAN_POINT('Ctrl Pts',(-0.361626396644909,-1.15951315008879,
-3.45423761073805));
#365413=CARTESIAN_POINT('Ctrl Pts',(-0.648203803698724,-1.02725603829705,
-3.51420895749367));
#365414=CARTESIAN_POINT('Ctrl Pts',(-0.89279607618879,-0.824211675135025,
-3.57483935724674));
#365415=CARTESIAN_POINT('Ctrl Pts',(-1.07560808862643,-0.564191133979103,
-3.63546761073801));
#365416=CARTESIAN_POINT('Ctrl Pts',(-1.18472901588094,-0.26803040550839,
-3.6954389574937));
#365417=CARTESIAN_POINT('Ctrl Pts',(-1.21410782431094,0.0484964950687397,
-3.75606935724672));
#365418=CARTESIAN_POINT('Ctrl Pts',(-1.1595131500888,0.361626396644898,
-3.81669761073803));
#365419=CARTESIAN_POINT('Ctrl Pts',(-1.02725603829704,0.648203803698727,
-3.87666895749368));
#365420=CARTESIAN_POINT('Ctrl Pts',(-0.824211675135021,0.892796076188792,
-3.93729935724673));
#365421=CARTESIAN_POINT('Ctrl Pts',(-0.564191133979095,1.07560808862643,
-3.99792761073801));
#365422=CARTESIAN_POINT('Ctrl Pts',(-0.268030405508389,1.18472901588092,
-4.05789895749373));
#365423=CARTESIAN_POINT('Ctrl Pts',(0.0484964950687464,1.21410782431094,
-4.11852935724671));
#365424=CARTESIAN_POINT('Ctrl Pts',(0.3616263966449,1.15951315008879,-4.17915761073805));
#365425=CARTESIAN_POINT('Ctrl Pts',(0.648203803698728,1.02725603829704,
-4.23912895749368));
#365426=CARTESIAN_POINT('Ctrl Pts',(0.892796076188791,0.824211675135014,
-4.29975935724674));
#365427=CARTESIAN_POINT('Ctrl Pts',(1.07560808862644,0.564191133979099,
-4.36038761073799));
#365428=CARTESIAN_POINT('Ctrl Pts',(1.18472901588094,0.268030405508375,
-4.42035895749369));
#365429=CARTESIAN_POINT('Ctrl Pts',(1.21410782431093,-0.0484964950687469,
-4.48098935724673));
#365430=CARTESIAN_POINT('Ctrl Pts',(1.15951315008879,-0.361626396644902,
-4.54161761073803));
#365431=CARTESIAN_POINT('Ctrl Pts',(1.02725603829703,-0.648203803698725,
-4.6015889574937));
#365432=CARTESIAN_POINT('Ctrl Pts',(0.824211675135013,-0.892796076188798,
-4.66221935724673));
#365433=CARTESIAN_POINT('Ctrl Pts',(0.564191133979094,-1.07560808862644,
-4.722847610738));
#365434=CARTESIAN_POINT('Ctrl Pts',(0.268030405508374,-1.18472901588094,
-4.7828189574937));
#365435=CARTESIAN_POINT('Ctrl Pts',(-0.04849649506876,-1.21410782431095,
-4.84344935724668));
#365436=CARTESIAN_POINT('Ctrl Pts',(-0.361626396644897,-1.15951315008877,
-4.90407761073806));
#365437=CARTESIAN_POINT('Ctrl Pts',(-0.648203803698715,-1.02725603829702,
-4.96404895749372));
#365438=CARTESIAN_POINT('Ctrl Pts',(-0.892796076188803,-0.824211675135015,
-5.02467935724671));
#365439=CARTESIAN_POINT('Ctrl Pts',(-1.07560808862644,-0.564191133979088,
-5.085307610738));
#365440=CARTESIAN_POINT('Ctrl Pts',(-1.18472901588092,-0.268030405508372,
-5.14527895749374));
#365441=CARTESIAN_POINT('Ctrl Pts',(-1.21410782431095,0.0484964950687572,
-5.20590935724669));
#365442=CARTESIAN_POINT('Ctrl Pts',(-1.1595131500888,0.361626396644921,
-5.26653761073799));
#365443=CARTESIAN_POINT('Ctrl Pts',(-1.02725603829702,0.64820380369872,
-5.32650895749373));
#365444=CARTESIAN_POINT('Ctrl Pts',(-0.824211675135014,0.892796076188816,
-5.38713935724669));
#365445=CARTESIAN_POINT('Ctrl Pts',(-0.564191133979076,1.07560808862641,
-5.44776761073806));
#365446=CARTESIAN_POINT('Ctrl Pts',(-0.268030405508379,1.18472901588095,
-5.50773895749365));
#365447=CARTESIAN_POINT('Ctrl Pts',(0.0484964950687955,1.21410782431095,
-5.56836935724668));
#365448=CARTESIAN_POINT('Ctrl Pts',(0.361626396644923,1.15951315008874,
-5.62899761073811));
#365449=CARTESIAN_POINT('Ctrl Pts',(0.648203803698529,1.02725603829711,
-5.68896895749371));
#365450=CARTESIAN_POINT('Ctrl Pts',(0.892796076189156,0.824211675134774,
-5.74959935724652));
#365451=CARTESIAN_POINT('Ctrl Pts',(1.07560808862635,0.564191133979143,
-5.81022761073827));
#365452=CARTESIAN_POINT('Ctrl Pts',(1.18472901588091,0.268030405509044,
-5.87019895749336));
#365453=CARTESIAN_POINT('Ctrl Pts',(1.2141078243105,-0.0484964950705043,
-5.93082935724695));
#365454=CARTESIAN_POINT('Ctrl Pts',(1.15951315009036,-0.361626396638523,
-5.99145761073686));
#365455=CARTESIAN_POINT('Ctrl Pts',(1.02725603828656,-0.648203803720622,
-6.05142895750248));
#365456=CARTESIAN_POINT('Ctrl Pts',(0.824211675164934,-0.892796076174764,
-6.11205935720599));
#365457=CARTESIAN_POINT('Ctrl Pts',(0.564191134059871,-1.07560808852829,
-6.17268761076101));
#365458=CARTESIAN_POINT('Ctrl Pts',(0.268030404959908,-1.18472901600022,
-6.23265895786053));
#365459=CARTESIAN_POINT('Ctrl Pts',(-0.048496494303855,-1.21410782509991,
-6.29328935527559));
#365460=CARTESIAN_POINT('Ctrl Pts',(-0.361626395111129,-1.15951314891753,
-6.35391761278417));
#365461=CARTESIAN_POINT('Ctrl Pts',(-0.648203807785757,-1.02725603400328,
-6.41388896506857));
#365462=CARTESIAN_POINT('Ctrl Pts',(-0.892796086148053,-0.82421169457497,
-6.47451931057689));
#365463=CARTESIAN_POINT('Ctrl Pts',(-1.0756080601232,-0.564191117561312,
-6.53514766561185));
#365464=CARTESIAN_POINT('Ctrl Pts',(-1.18472898053544,-0.268030410347432,
-6.59511906407632));
#365465=CARTESIAN_POINT('Ctrl Pts',(-1.21410817056974,0.0484965775982433,
-6.65574860156863));
#365466=CARTESIAN_POINT('Ctrl Pts',(-1.15951264802113,0.361626359829526,
-6.71637855817043));
#365467=CARTESIAN_POINT('Ctrl Pts',(-1.02725631549215,0.648202679709777,
-6.77634998994504));
#365468=CARTESIAN_POINT('Ctrl Pts',(-0.824212514048729,0.89279989750689,
-6.83697046026166));
#365469=CARTESIAN_POINT('Ctrl Pts',(-0.564185827571163,1.07561000588125,
-6.89761936594616));
#365470=CARTESIAN_POINT('Ctrl Pts',(-0.268055236457238,1.1847006164406,
-6.95758396792716));
#365471=CARTESIAN_POINT('Ctrl Pts',(0.0485472352404887,1.2142038916925,
-7.01813896161907));
#365472=CARTESIAN_POINT('Ctrl Pts',(0.361655804485534,1.15924149264237,
-7.07893382111904));
#365473=CARTESIAN_POINT('Ctrl Pts',(0.6478968782727,1.02825270748,-7.1387952204064));
#365474=CARTESIAN_POINT('Ctrl Pts',(0.893414088159582,0.820656810820771,
-7.19914743650299));
#365475=CARTESIAN_POINT('Ctrl Pts',(1.07501647976632,0.576321349623175,
-7.26054245691513));
#365476=CARTESIAN_POINT('Ctrl Pts',(1.18621324528802,0.224452404214759,
-7.3192609169548));
#365477=CARTESIAN_POINT('Ctrl Pts',(1.20016374408797,0.152327073866745,
-7.36128002094695));
#365478=CARTESIAN_POINT('Ctrl Pts',(1.20016374408796,-0.0349890780536599,
-7.37928962624155));
#365479=CARTESIAN_POINT('Ctrl Pts',(1.19994860179671,0.0349330361207006,
-2.22019720516939));
#365480=CARTESIAN_POINT('Ctrl Pts',(1.19994860179671,-0.126746617464705,
-2.23574197648456));
#365481=CARTESIAN_POINT('Ctrl Pts',(1.18628451104366,-0.235287042882826,
-2.2810964912132));
#365482=CARTESIAN_POINT('Ctrl Pts',(1.07477771342961,-0.573169099315595,
-2.33867755519319));
#365483=CARTESIAN_POINT('Ctrl Pts',(0.893209191596192,-0.821391071780957,
-2.40041325450729));
#365484=CARTESIAN_POINT('Ctrl Pts',(0.647719578695754,-1.02788019949386,
-2.46067439994995));
#365485=CARTESIAN_POINT('Ctrl Pts',(0.361523604188232,-1.15911171219588,
-2.52056034931245));
#365486=CARTESIAN_POINT('Ctrl Pts',(0.0484713603287608,-1.21397018964645,
-2.58134810525369));
#365487=CARTESIAN_POINT('Ctrl Pts',(-0.26807499252822,-1.18447453220047,
-2.64190541780525));
#365488=CARTESIAN_POINT('Ctrl Pts',(-0.564145022724671,-1.07538119354467,
-2.70186948165707));
#365489=CARTESIAN_POINT('Ctrl Pts',(-0.82411227040745,-0.892592747940269,
-2.76251800818134));
#365490=CARTESIAN_POINT('Ctrl Pts',(-1.02710741719481,-0.648025648702113,
-2.82313903087394));
#365491=CARTESIAN_POINT('Ctrl Pts',(-1.15932278442025,-0.361494315792975,
-2.88311038111178));
#365492=CARTESIAN_POINT('Ctrl Pts',(-1.21389060301799,-0.0484207535259056,
-2.94373983918878));
#365493=CARTESIAN_POINT('Ctrl Pts',(-1.18449856839689,0.268050248144059,
-3.00436996521972));
#365494=CARTESIAN_POINT('Ctrl Pts',(-1.0753804241319,0.564150242879215,
-3.06434127064474));
#365495=CARTESIAN_POINT('Ctrl Pts',(-0.892588631186338,0.824111463629319,
-3.12496913072614));
#365496=CARTESIAN_POINT('Ctrl Pts',(-0.648026852820059,1.02710713661446,
-3.18560006416148));
#365497=CARTESIAN_POINT('Ctrl Pts',(-0.361494335707408,1.15932328272349,
-3.24557132342766));
#365498=CARTESIAN_POINT('Ctrl Pts',(-0.0484206753242147,1.21389025844596,
-3.30619908602272));
#365499=CARTESIAN_POINT('Ctrl Pts',(0.268050244650624,1.18449860355023,
-3.36683007137514));
#365500=CARTESIAN_POINT('Ctrl Pts',(0.564150258467979,1.07538045277468,
-3.42680132544561));
#365501=CARTESIAN_POINT('Ctrl Pts',(0.824111444426381,0.892588621200653,
-3.48742908409296));
#365502=CARTESIAN_POINT('Ctrl Pts',(1.02710714086036,0.648026848734914,
-3.54806007173318));
#365503=CARTESIAN_POINT('Ctrl Pts',(1.15932328389686,0.361494337262554,
-3.60803132546964));
#365504=CARTESIAN_POINT('Ctrl Pts',(1.21389025765669,0.0484206760863054,
-3.66865908405205));
#365505=CARTESIAN_POINT('Ctrl Pts',(1.18449860343075,-0.268050245199621,
-3.72929007174227));
#365506=CARTESIAN_POINT('Ctrl Pts',(1.07538045287309,-0.564150258386447,
-3.78926132546809));
#365507=CARTESIAN_POINT('Ctrl Pts',(0.892588621215019,-0.824111444396376,
-3.84988908405249));
#365508=CARTESIAN_POINT('Ctrl Pts',(0.648026848712835,-1.02710714087089,
-3.91052007174198));
#365509=CARTESIAN_POINT('Ctrl Pts',(0.361494337268959,-1.15932328389524,
-3.97049132546837));
#365510=CARTESIAN_POINT('Ctrl Pts',(0.0484206760845926,-1.21389025765713,
-4.03111908405232));
#365511=CARTESIAN_POINT('Ctrl Pts',(-0.268050245198952,-1.18449860343081,
-4.09175007174202));
#365512=CARTESIAN_POINT('Ctrl Pts',(-0.564150258386389,-1.07538045287319,
-4.15172132546838));
#365513=CARTESIAN_POINT('Ctrl Pts',(-0.82411144439661,-0.892588621214665,
-4.2123490840523));
#365514=CARTESIAN_POINT('Ctrl Pts',(-1.0271071408708,-0.648026848713027,
-4.27298007174198));
#365515=CARTESIAN_POINT('Ctrl Pts',(-1.15932328389526,-0.361494337268938,
-4.33295132546841));
#365516=CARTESIAN_POINT('Ctrl Pts',(-1.21389025765712,-0.0484206760845532,
-4.39357908405229));
#365517=CARTESIAN_POINT('Ctrl Pts',(-1.1844986034308,0.268050245198939,
-4.45421007174199));
#365518=CARTESIAN_POINT('Ctrl Pts',(-1.07538045287319,0.564150258386394,
-4.51418132546839));
#365519=CARTESIAN_POINT('Ctrl Pts',(-0.892588621214658,0.82411144439661,
-4.5748090840523));
#365520=CARTESIAN_POINT('Ctrl Pts',(-0.648026848713022,1.0271071408708,
-4.63544007174198));
#365521=CARTESIAN_POINT('Ctrl Pts',(-0.361494337268941,1.15932328389527,
-4.69541132546844));
#365522=CARTESIAN_POINT('Ctrl Pts',(-0.0484206760845442,1.21389025765711,
-4.75603908405227));
#365523=CARTESIAN_POINT('Ctrl Pts',(0.268050245198942,1.18449860343081,
-4.81667007174201));
#365524=CARTESIAN_POINT('Ctrl Pts',(0.564150258386395,1.07538045287318,
-4.87664132546839));
#365525=CARTESIAN_POINT('Ctrl Pts',(0.824111444396615,0.892588621214655,
-4.9372690840523));
#365526=CARTESIAN_POINT('Ctrl Pts',(1.02710714087079,0.648026848713006,
-4.99790007174195));
#365527=CARTESIAN_POINT('Ctrl Pts',(1.15932328389525,0.361494337268927,
-5.0578713254684));
#365528=CARTESIAN_POINT('Ctrl Pts',(1.21389025765711,0.0484206760845428,
-5.11849908405229));
#365529=CARTESIAN_POINT('Ctrl Pts',(1.1844986034308,-0.268050245198941,
-5.179130071742));
#365530=CARTESIAN_POINT('Ctrl Pts',(1.07538045287319,-0.5641502583864,-5.2391013254684));
#365531=CARTESIAN_POINT('Ctrl Pts',(0.892588621214648,-0.824111444396615,
-5.29972908405229));
#365532=CARTESIAN_POINT('Ctrl Pts',(0.648026848713012,-1.0271071408708,
-5.36036007174197));
#365533=CARTESIAN_POINT('Ctrl Pts',(0.361494337268925,-1.15932328389526,
-5.42033132546841));
#365534=CARTESIAN_POINT('Ctrl Pts',(0.0484206760845338,-1.21389025765709,
-5.48095908405224));
#365535=CARTESIAN_POINT('Ctrl Pts',(-0.268050245198938,-1.18449860343081,
-5.54159007174203));
#365536=CARTESIAN_POINT('Ctrl Pts',(-0.564150258386406,-1.0753804528732,
-5.60156132546843));
#365537=CARTESIAN_POINT('Ctrl Pts',(-0.824111444396613,-0.89258862121464,
-5.66218908405228));
#365538=CARTESIAN_POINT('Ctrl Pts',(-1.02710714087079,-0.648026848713008,
-5.72282007174197));
#365539=CARTESIAN_POINT('Ctrl Pts',(-1.15932328389528,-0.36149433726893,
-5.78279132546845));
#365540=CARTESIAN_POINT('Ctrl Pts',(-1.2138902576571,-0.0484206760845329,
-5.84341908405225));
#365541=CARTESIAN_POINT('Ctrl Pts',(-1.18449860343078,0.268050245198954,
-5.90405007174196));
#365542=CARTESIAN_POINT('Ctrl Pts',(-1.07538045287319,0.564150258386408,
-5.96402132546844));
#365543=CARTESIAN_POINT('Ctrl Pts',(-0.892588621214629,0.824111444396606,
-6.02464908405225));
#365544=CARTESIAN_POINT('Ctrl Pts',(-0.64802684871302,1.02710714087081,
-6.08528007174203));
#365545=CARTESIAN_POINT('Ctrl Pts',(-0.361494337268917,1.15932328389523,
-6.14525132546836));
#365546=CARTESIAN_POINT('Ctrl Pts',(-0.048420676084498,1.21389025765709,
-6.20587908405224));
#365547=CARTESIAN_POINT('Ctrl Pts',(0.268050245198975,1.18449860343083,
-6.26651007174208));
#365548=CARTESIAN_POINT('Ctrl Pts',(0.564150258386226,1.07538045287327,
-6.32648132546841));
#365549=CARTESIAN_POINT('Ctrl Pts',(0.824111444396827,0.892588621214275,
-6.38710908405208));
#365550=CARTESIAN_POINT('Ctrl Pts',(1.0271071408709,0.648026848713156,-6.44774007174223));
#365551=CARTESIAN_POINT('Ctrl Pts',(1.159323283895,0.361494337269589,-6.50771132546807));
#365552=CARTESIAN_POINT('Ctrl Pts',(1.21389025765673,0.0484206760826282,
-6.56833908405251));
#365553=CARTESIAN_POINT('Ctrl Pts',(1.18449860343187,-0.268050245192022,
-6.62897007174084));
#365554=CARTESIAN_POINT('Ctrl Pts',(1.07538045286828,-0.564150258411146,
-6.68894132547714));
#365555=CARTESIAN_POINT('Ctrl Pts',(0.892588621213993,-0.824111444364615,
-6.74956908401155));
#365556=CARTESIAN_POINT('Ctrl Pts',(0.648026848838496,-1.0271071407854,
-6.81020007176602));
#365557=CARTESIAN_POINT('Ctrl Pts',(0.361494336755823,-1.1593232842844,
-6.87017132583052));
#365558=CARTESIAN_POINT('Ctrl Pts',(0.0484206766338695,-1.2138902567815,
-6.93079908208711));
#365559=CARTESIAN_POINT('Ctrl Pts',(-0.268050243328471,-1.18449860442843,
-6.99143007381518));
#365560=CARTESIAN_POINT('Ctrl Pts',(-0.564150266443273,-1.07538045302616,
-7.05140133291083));
#365561=CARTESIAN_POINT('Ctrl Pts',(-0.824111428662813,-0.892588609834598,
-7.11202903755537));
#365562=CARTESIAN_POINT('Ctrl Pts',(-1.02710714802879,-0.648026871740004,
-7.17266012714546));
#365563=CARTESIAN_POINT('Ctrl Pts',(-1.15932333812035,-0.361494339370128,
-7.23263142938285));
#365564=CARTESIAN_POINT('Ctrl Pts',(-1.21388994830272,-0.048420558641127,
-7.29325833250989));
#365565=CARTESIAN_POINT('Ctrl Pts',(-1.18449897688191,0.268050252868152,
-7.3538910230542));
#365566=CARTESIAN_POINT('Ctrl Pts',(-1.07538131032931,0.564149776786355,
-7.41386233272661));
#365567=CARTESIAN_POINT('Ctrl Pts',(-0.89258382755218,0.824110299740277,
-7.47448020435212));
#365568=CARTESIAN_POINT('Ctrl Pts',(-0.648027824318076,1.02711576339274,
-7.53513199456933));
#365569=CARTESIAN_POINT('Ctrl Pts',(-0.361519103800307,1.1593054263198,
-7.59509558925458));
#365570=CARTESIAN_POINT('Ctrl Pts',(-0.048363558710048,1.21390597518738,
-7.65565075634608));
#365571=CARTESIAN_POINT('Ctrl Pts',(0.268072537684821,1.18437146807072,
-7.71644050362745));
#365572=CARTESIAN_POINT('Ctrl Pts',(0.563930411939142,1.07613883654808,
-7.77632820376135));
#365573=CARTESIAN_POINT('Ctrl Pts',(0.82426225220675,0.889715887308659,
-7.83657609568004));
#365574=CARTESIAN_POINT('Ctrl Pts',(1.02783344969258,0.657090690457504,
-7.89836582380498));
#365575=CARTESIAN_POINT('Ctrl Pts',(1.15670010462145,0.329911052415485,
-7.95561053869555));
#365576=CARTESIAN_POINT('Ctrl Pts',(1.19983645566974,0.222219960564689,
-8.00127996772839));
#365577=CARTESIAN_POINT('Ctrl Pts',(1.19983645566973,0.0349038086442839,
-8.01928957302298));
#365578=CARTESIAN_POINT('Ctrl Pts',(1.99994859520949,0.0349419760186855,
-2.22027906663631));
#365579=CARTESIAN_POINT('Ctrl Pts',(1.99994859520949,-0.133161143166691,
-2.23644142527053));
#365580=CARTESIAN_POINT('Ctrl Pts',(1.96833139354662,-0.472425718114294,
-2.28062587414611));
#365581=CARTESIAN_POINT('Ctrl Pts',(1.77549751488388,-0.970378153502274,
-2.33932132964638));
#365582=CARTESIAN_POINT('Ctrl Pts',(1.46486827473653,-1.39599810161593,
-2.40041168228136));
#365583=CARTESIAN_POINT('Ctrl Pts',(1.0532724675317,-1.72756949816,-2.46064650153962));
#365584=CARTESIAN_POINT('Ctrl Pts',(0.570253827701872,-1.94116844962337,
-2.52097328730337));
#365585=CARTESIAN_POINT('Ctrl Pts',(0.0484505622703552,-2.02298787581022,
-2.58147196284819));
#365586=CARTESIAN_POINT('Ctrl Pts',(-0.476762817249676,-1.96636546213765,
-2.64190473727344));
#365587=CARTESIAN_POINT('Ctrl Pts',(-0.969389646094711,-1.7758542783469,
-2.70222141276452));
#365588=CARTESIAN_POINT('Ctrl Pts',(-1.39619412835269,-1.46471035101601,
-2.76268238970025));
#365589=CARTESIAN_POINT('Ctrl Pts',(-1.72755848446788,-1.05330968911041,
-2.8231370123091));
#365590=CARTESIAN_POINT('Ctrl Pts',(-1.94118200928605,-0.570259037663673,
-2.88345449584336));
#365591=CARTESIAN_POINT('Ctrl Pts',(-2.02296215046454,-0.0484473116516587,
-2.94390972032538));
#365592=CARTESIAN_POINT('Ctrl Pts',(-1.96637109382515,0.476765855935366,
-3.00436740295728));
#365593=CARTESIAN_POINT('Ctrl Pts',(-1.77585739520295,0.969389009874219,
-3.06468474103924));
#365594=CARTESIAN_POINT('Ctrl Pts',(-1.46470740175196,1.39619269138418,
-3.12513949735647));
#365595=CARTESIAN_POINT('Ctrl Pts',(-1.05331000180424,1.72755870986409,
-3.18559743702838));
#365596=CARTESIAN_POINT('Ctrl Pts',(-0.570259275444307,1.94118238224882,
-3.2459147561141));
#365597=CARTESIAN_POINT('Ctrl Pts',(-0.0484472107178668,2.02296183497224,
-3.30636948355066));
#365598=CARTESIAN_POINT('Ctrl Pts',(0.476765831354286,1.96637112545875,
-3.36682743921798));
#365599=CARTESIAN_POINT('Ctrl Pts',(0.969389026744113,1.77585742843582,
-3.42714475673536));
#365600=CARTESIAN_POINT('Ctrl Pts',(1.39619267971627,1.46470738191116,-3.48759948296635));
#365601=CARTESIAN_POINT('Ctrl Pts',(1.72755870948907,1.05331000492523,-3.54805743931225));
#365602=CARTESIAN_POINT('Ctrl Pts',(1.9411823845861,0.570259275622033,-3.60837475674778));
#365603=CARTESIAN_POINT('Ctrl Pts',(2.02296183383815,0.0484472105365179,
-3.66882948295392));
#365604=CARTESIAN_POINT('Ctrl Pts',(1.96637112555601,-0.476765831198158,
-3.72928743931407));
#365605=CARTESIAN_POINT('Ctrl Pts',(1.77585742848668,-0.969389026837108,
-3.78960475674772));
#365606=CARTESIAN_POINT('Ctrl Pts',(1.46470738188885,-1.39619267968778,
-3.85005948295395));
#365607=CARTESIAN_POINT('Ctrl Pts',(1.05331000493188,-1.72755870948857,
-3.910517439314));
#365608=CARTESIAN_POINT('Ctrl Pts',(0.570259275619007,-1.9411823845877,
-3.97083475674782));
#365609=CARTESIAN_POINT('Ctrl Pts',(0.0484472105373659,-2.02296183383781,
-4.03128948295388));
#365610=CARTESIAN_POINT('Ctrl Pts',(-0.476765831198311,-1.96637112555626,
-4.09174743931402));
#365611=CARTESIAN_POINT('Ctrl Pts',(-0.969389026837092,-1.77585742848654,
-4.15206475674782));
#365612=CARTESIAN_POINT('Ctrl Pts',(-1.39619267968775,-1.46470738188883,
-4.21251948295388));
#365613=CARTESIAN_POINT('Ctrl Pts',(-1.72755870948862,-1.05331000493188,
-4.27297743931401));
#365614=CARTESIAN_POINT('Ctrl Pts',(-1.94118238458768,-0.570259275619005,
-4.33329475674783));
#365615=CARTESIAN_POINT('Ctrl Pts',(-2.0229618338378,-0.0484472105373586,
-4.39374948295387));
#365616=CARTESIAN_POINT('Ctrl Pts',(-1.96637112555625,0.476765831198322,
-4.45420743931402));
#365617=CARTESIAN_POINT('Ctrl Pts',(-1.77585742848654,0.969389026837096,
-4.51452475674782));
#365618=CARTESIAN_POINT('Ctrl Pts',(-1.46470738188882,1.39619267968775,
-4.57497948295388));
#365619=CARTESIAN_POINT('Ctrl Pts',(-1.05331000493187,1.72755870948862,
-4.63543743931401));
#365620=CARTESIAN_POINT('Ctrl Pts',(-0.570259275619004,1.9411823845877,
-4.69575475674784));
#365621=CARTESIAN_POINT('Ctrl Pts',(-0.0484472105373471,2.0229618338378,
-4.75620948295387));
#365622=CARTESIAN_POINT('Ctrl Pts',(0.476765831198326,1.96637112555626,
-4.81666743931402));
#365623=CARTESIAN_POINT('Ctrl Pts',(0.969389026837101,1.77585742848653,
-4.87698475674782));
#365624=CARTESIAN_POINT('Ctrl Pts',(1.39619267968776,1.46470738188882,-4.93743948295388));
#365625=CARTESIAN_POINT('Ctrl Pts',(1.72755870948861,1.05331000493185,-4.997897439314));
#365626=CARTESIAN_POINT('Ctrl Pts',(1.94118238458768,0.570259275618993,
-5.05821475674782));
#365627=CARTESIAN_POINT('Ctrl Pts',(2.0229618338378,0.0484472105373451,
-5.11866948295387));
#365628=CARTESIAN_POINT('Ctrl Pts',(1.96637112555625,-0.476765831198331,
-5.17912743931402));
#365629=CARTESIAN_POINT('Ctrl Pts',(1.77585742848654,-0.969389026837107,
-5.23944475674783));
#365630=CARTESIAN_POINT('Ctrl Pts',(1.46470738188881,-1.39619267968776,
-5.29989948295387));
#365631=CARTESIAN_POINT('Ctrl Pts',(1.05331000493185,-1.72755870948862,
-5.36035743931401));
#365632=CARTESIAN_POINT('Ctrl Pts',(0.57025927561899,-1.94118238458768,
-5.42067475674783));
#365633=CARTESIAN_POINT('Ctrl Pts',(0.0484472105373359,-2.02296183383778,
-5.48112948295386));
#365634=CARTESIAN_POINT('Ctrl Pts',(-0.476765831198329,-1.96637112555626,
-5.54158743931402));
#365635=CARTESIAN_POINT('Ctrl Pts',(-0.96938902683712,-1.77585742848655,
-5.60190475674783));
#365636=CARTESIAN_POINT('Ctrl Pts',(-1.39619267968776,-1.4647073818888,
-5.66235948295387));
#365637=CARTESIAN_POINT('Ctrl Pts',(-1.72755870948862,-1.05331000493185,
-5.722817439314));
#365638=CARTESIAN_POINT('Ctrl Pts',(-1.9411823845877,-0.570259275618991,
-5.78313475674784));
#365639=CARTESIAN_POINT('Ctrl Pts',(-2.02296183383779,-0.0484472105373294,
-5.84358948295386));
#365640=CARTESIAN_POINT('Ctrl Pts',(-1.96637112555623,0.476765831198343,
-5.904047439314));
#365641=CARTESIAN_POINT('Ctrl Pts',(-1.77585742848654,0.969389026837124,
-5.96436475674784));
#365642=CARTESIAN_POINT('Ctrl Pts',(-1.46470738188879,1.39619267968775,
-6.02481948295386));
#365643=CARTESIAN_POINT('Ctrl Pts',(-1.05331000493186,1.72755870948864,
-6.08527743931403));
#365644=CARTESIAN_POINT('Ctrl Pts',(-0.57025927561896,1.94118238458767,
-6.14559475674781));
#365645=CARTESIAN_POINT('Ctrl Pts',(-0.0484472105373227,2.02296183383776,
-6.20604948295386));
#365646=CARTESIAN_POINT('Ctrl Pts',(0.476765831198343,1.96637112555631,
-6.26650743931404));
#365647=CARTESIAN_POINT('Ctrl Pts',(0.969389026837138,1.77585742848649,
-6.32682475674784));
#365648=CARTESIAN_POINT('Ctrl Pts',(1.39619267968763,1.4647073818887,-6.3872794829538));
#365649=CARTESIAN_POINT('Ctrl Pts',(1.72755870948896,1.05331000493196,-6.4477374393141));
#365650=CARTESIAN_POINT('Ctrl Pts',(1.94118238458724,0.570259275618813,
-6.50805475674775));
#365651=CARTESIAN_POINT('Ctrl Pts',(2.0229618338382,0.0484472105380158,
-6.56850948295382));
#365652=CARTESIAN_POINT('Ctrl Pts',(1.96637112555413,-0.47676583120083,
-6.62896743931409));
#365653=CARTESIAN_POINT('Ctrl Pts',(1.77585742849251,-0.969389026833344,
-6.68928475674954));
#365654=CARTESIAN_POINT('Ctrl Pts',(1.46470738188697,-1.39619267969199,
-6.74973948294137));
#365655=CARTESIAN_POINT('Ctrl Pts',(1.05331000488233,-1.72755870945149,
-6.81019743932769));
#365656=CARTESIAN_POINT('Ctrl Pts',(0.570259275809968,-1.94118238475938,
-6.87051475683913));
#365657=CARTESIAN_POINT('Ctrl Pts',(0.0484472101488399,-2.02296183330866,
-6.93096948236246));
#365658=CARTESIAN_POINT('Ctrl Pts',(-0.476765830732716,-1.96637112538019,
-6.99142743997978));
#365659=CARTESIAN_POINT('Ctrl Pts',(-0.969389027651612,-1.775857433288,
-7.05174475889683));
#365660=CARTESIAN_POINT('Ctrl Pts',(-1.39619267380615,-1.46470736293583,
-7.11219946872276));
#365661=CARTESIAN_POINT('Ctrl Pts',(-1.72755871231312,-1.05331002647757,
-7.1726574556236));
#365662=CARTESIAN_POINT('Ctrl Pts',(-1.94118244199894,-0.570259298778077,
-7.23297479041701));
#365663=CARTESIAN_POINT('Ctrl Pts',(-2.02296149561613,-0.0484470734163606,
-7.29342924947211));
#365664=CARTESIAN_POINT('Ctrl Pts',(-1.96637162260829,0.47676563992917,
-7.35388770608518));
#365665=CARTESIAN_POINT('Ctrl Pts',(-1.77585778550465,0.969389377563547,
-7.41420515419699));
#365666=CARTESIAN_POINT('Ctrl Pts',(-1.46470321414872,1.39619055347437,
-7.4746566054593));
#365667=CARTESIAN_POINT('Ctrl Pts',(-1.05331679189158,1.72756279918536,
-7.53512091909894));
#365668=CARTESIAN_POINT('Ctrl Pts',(-0.570256351317271,1.94118541096824,
-7.5954368568002));
#365669=CARTESIAN_POINT('Ctrl Pts',(-0.0484373346474795,2.02291433148142,
-7.65586848775589));
#365670=CARTESIAN_POINT('Ctrl Pts',(0.476753357889169,1.96647633924905,
-7.7163654145941));
#365671=CARTESIAN_POINT('Ctrl Pts',(0.969439733353148,1.77572407380791,
-7.7767079034587));
#365672=CARTESIAN_POINT('Ctrl Pts',(1.39587962475789,1.46484458461224,-7.83687735653918));
#365673=CARTESIAN_POINT('Ctrl Pts',(1.72854436163452,1.05253719801599,-7.89821617217114));
#365674=CARTESIAN_POINT('Ctrl Pts',(1.93848294702123,0.574209674581668,
-7.95584767975511));
#365675=CARTESIAN_POINT('Ctrl Pts',(1.99983638908382,0.21585245779268,-8.0021551741418));
#365676=CARTESIAN_POINT('Ctrl Pts',(1.99983638908381,0.0349322317806574,
-8.0195498399348));
#365677=CARTESIAN_POINT('Ctrl Pts',(2.79994858862227,0.0349509159166703,
-2.22036092810323));
#365678=CARTESIAN_POINT('Ctrl Pts',(2.79994858862227,-0.139575668868676,
-2.2371408740565));
#365679=CARTESIAN_POINT('Ctrl Pts',(2.75037827604958,-0.709564393345761,
-2.28015525707901));
#365680=CARTESIAN_POINT('Ctrl Pts',(2.47621731633814,-1.36758720768895,
-2.33996510409957));
#365681=CARTESIAN_POINT('Ctrl Pts',(2.03652735787686,-1.97060513145091,
-2.40041011005543));
#365682=CARTESIAN_POINT('Ctrl Pts',(1.45882535636765,-2.42725879682614,
-2.46061860312929));
#365683=CARTESIAN_POINT('Ctrl Pts',(0.778984051215511,-2.72322518705085,
-2.52138622529428));
#365684=CARTESIAN_POINT('Ctrl Pts',(0.0484297642119496,-2.83200556197398,
-2.58159582044269));
#365685=CARTESIAN_POINT('Ctrl Pts',(-0.685450641971131,-2.74825639207482,
-2.64190405674164));
#365686=CARTESIAN_POINT('Ctrl Pts',(-1.37463426946475,-2.47632736314912,
-2.70257334387197));
#365687=CARTESIAN_POINT('Ctrl Pts',(-1.96827598629794,-2.03682795409175,
-2.76284677121916));
#365688=CARTESIAN_POINT('Ctrl Pts',(-2.42800955174095,-1.45859372951871,
-2.82313499374427));
#365689=CARTESIAN_POINT('Ctrl Pts',(-2.72304123415184,-0.779023759534372,
-2.88379861057494));
#365690=CARTESIAN_POINT('Ctrl Pts',(-2.8320336979111,-0.048473869777412,
-2.94407960146198));
#365691=CARTESIAN_POINT('Ctrl Pts',(-2.74824361925341,0.685481463726674,
-3.00436484069483));
#365692=CARTESIAN_POINT('Ctrl Pts',(-2.47633436627399,1.37462777686922,
-3.06502821143375));
#365693=CARTESIAN_POINT('Ctrl Pts',(-2.03682617231757,1.96827391913905,
-3.1253098639868));
#365694=CARTESIAN_POINT('Ctrl Pts',(-1.45859315078841,2.42801028311372,
-3.18559480989526));
#365695=CARTESIAN_POINT('Ctrl Pts',(-0.779024215181206,2.72304148177415,
-3.24625818880055));
#365696=CARTESIAN_POINT('Ctrl Pts',(-0.048473746111519,2.83203341149851,
-3.30653988107861));
#365697=CARTESIAN_POINT('Ctrl Pts',(0.685481418057947,2.74824364736727,
-3.36682480706082));
#365698=CARTESIAN_POINT('Ctrl Pts',(1.37462779502025,2.47633440409695,-3.42748818802511));
#365699=CARTESIAN_POINT('Ctrl Pts',(1.96827391500616,2.03682614262167,-3.48776988183974));
#365700=CARTESIAN_POINT('Ctrl Pts',(2.42801027811778,1.45859316111554,-3.54805480689131));
#365701=CARTESIAN_POINT('Ctrl Pts',(2.72304148527533,0.779024213981512,
-3.60871818802593));
#365702=CARTESIAN_POINT('Ctrl Pts',(2.83203341001962,0.0484737449867304,
-3.66899988185579));
#365703=CARTESIAN_POINT('Ctrl Pts',(2.74824364768127,-0.685481417196696,
-3.72928480688587));
#365704=CARTESIAN_POINT('Ctrl Pts',(2.47633440410028,-1.37462779528777,
-3.78994818802735));
#365705=CARTESIAN_POINT('Ctrl Pts',(2.03682614256268,-1.96827391497919,
-3.85022988185542));
#365706=CARTESIAN_POINT('Ctrl Pts',(1.45859316115093,-2.42801027810626,
-3.91051480688602));
#365707=CARTESIAN_POINT('Ctrl Pts',(0.779024213969054,-2.72304148528015,
-3.97117818802726));
#365708=CARTESIAN_POINT('Ctrl Pts',(0.0484737449901392,-2.83203341001849,
-4.03145988185545));
#365709=CARTESIAN_POINT('Ctrl Pts',(-0.685481417197671,-2.74824364768172,
-4.09174480688602));
#365710=CARTESIAN_POINT('Ctrl Pts',(-1.3746277952878,-2.4763344040999,-4.15240818802725));
#365711=CARTESIAN_POINT('Ctrl Pts',(-1.96827391497889,-2.03682614256299,
-4.21268988185546));
#365712=CARTESIAN_POINT('Ctrl Pts',(-2.42801027810644,-1.45859316115073,
-4.27297480688604));
#365713=CARTESIAN_POINT('Ctrl Pts',(-2.72304148528011,-0.779024213969072,
-4.33363818802725));
#365714=CARTESIAN_POINT('Ctrl Pts',(-2.83203341001849,-0.0484737449901639,
-4.39391988185546));
#365715=CARTESIAN_POINT('Ctrl Pts',(-2.7482436476817,0.685481417197704,
-4.45420480688603));
#365716=CARTESIAN_POINT('Ctrl Pts',(-2.4763344040999,1.3746277952878,-4.51486818802725));
#365717=CARTESIAN_POINT('Ctrl Pts',(-2.03682614256298,1.96827391497889,
-4.57514988185546));
#365718=CARTESIAN_POINT('Ctrl Pts',(-1.45859316115072,2.42801027810644,
-4.63543480688604));
#365719=CARTESIAN_POINT('Ctrl Pts',(-0.779024213969067,2.72304148528013,
-4.69609818802723));
#365720=CARTESIAN_POINT('Ctrl Pts',(-0.04847374499015,2.83203341001848,
-4.75637988185547));
#365721=CARTESIAN_POINT('Ctrl Pts',(0.685481417197709,2.7482436476817,-4.81666480688603));
#365722=CARTESIAN_POINT('Ctrl Pts',(1.37462779528781,2.47633440409989,-4.87732818802725));
#365723=CARTESIAN_POINT('Ctrl Pts',(1.9682739149789,2.03682614256298,-4.93760988185546));
#365724=CARTESIAN_POINT('Ctrl Pts',(2.42801027810644,1.4585931611507,-4.99789480688605));
#365725=CARTESIAN_POINT('Ctrl Pts',(2.7230414852801,0.779024213969058,-5.05855818802725));
#365726=CARTESIAN_POINT('Ctrl Pts',(2.83203341001848,0.0484737449901475,
-5.11883988185546));
#365727=CARTESIAN_POINT('Ctrl Pts',(2.74824364768169,-0.685481417197721,
-5.17912480688604));
#365728=CARTESIAN_POINT('Ctrl Pts',(2.47633440409989,-1.37462779528781,
-5.23978818802725));
#365729=CARTESIAN_POINT('Ctrl Pts',(2.03682614256297,-1.9682739149789,-5.30006988185546));
#365730=CARTESIAN_POINT('Ctrl Pts',(1.45859316115069,-2.42801027810645,
-5.36035480688604));
#365731=CARTESIAN_POINT('Ctrl Pts',(0.779024213969056,-2.72304148528011,
-5.42101818802724));
#365732=CARTESIAN_POINT('Ctrl Pts',(0.0484737449901378,-2.83203341001847,
-5.48129988185548));
#365733=CARTESIAN_POINT('Ctrl Pts',(-0.685481417197721,-2.7482436476817,
-5.54158480688602));
#365734=CARTESIAN_POINT('Ctrl Pts',(-1.37462779528784,-2.4763344040999,
-5.60224818802724));
#365735=CARTESIAN_POINT('Ctrl Pts',(-1.9682739149789,-2.03682614256296,
-5.66252988185546));
#365736=CARTESIAN_POINT('Ctrl Pts',(-2.42801027810645,-1.45859316115069,
-5.72281480688604));
#365737=CARTESIAN_POINT('Ctrl Pts',(-2.72304148528013,-0.779024213969052,
-5.78347818802723));
#365738=CARTESIAN_POINT('Ctrl Pts',(-2.83203341001847,-0.0484737449901258,
-5.84375988185547));
#365739=CARTESIAN_POINT('Ctrl Pts',(-2.74824364768167,0.685481417197731,
-5.90404480688604));
#365740=CARTESIAN_POINT('Ctrl Pts',(-2.47633440409989,1.37462779528784,
-5.96470818802724));
#365741=CARTESIAN_POINT('Ctrl Pts',(-2.03682614256295,1.96827391497889,
-6.02498988185547));
#365742=CARTESIAN_POINT('Ctrl Pts',(-1.4585931611507,2.42801027810647,-6.08527480688602));
#365743=CARTESIAN_POINT('Ctrl Pts',(-0.779024213969003,2.7230414852801,
-6.14593818802726));
#365744=CARTESIAN_POINT('Ctrl Pts',(-0.0484737449901475,2.83203341001844,
-6.20621988185547));
#365745=CARTESIAN_POINT('Ctrl Pts',(0.685481417197711,2.74824364768178,
-6.266504806886));
#365746=CARTESIAN_POINT('Ctrl Pts',(1.37462779528805,2.4763344040997,-6.32716818802727));
#365747=CARTESIAN_POINT('Ctrl Pts',(1.96827391497844,2.03682614256313,-6.3874498818555));
#365748=CARTESIAN_POINT('Ctrl Pts',(2.42801027810703,1.45859316115076,-6.44773480688596));
#365749=CARTESIAN_POINT('Ctrl Pts',(2.72304148527948,0.779024213968036,
-6.50839818802743));
#365750=CARTESIAN_POINT('Ctrl Pts',(2.83203341001966,0.0484737449934034,
-6.56867988185514));
#365751=CARTESIAN_POINT('Ctrl Pts',(2.74824364767639,-0.685481417209638,
-6.62896480688735));
#365752=CARTESIAN_POINT('Ctrl Pts',(2.47633440411674,-1.37462779525554,
-6.68962818802195));
#365753=CARTESIAN_POINT('Ctrl Pts',(2.03682614255995,-1.96827391501936,
-6.74990988187118));
#365754=CARTESIAN_POINT('Ctrl Pts',(1.45859316092616,-2.42801027811759,
-6.81019480688936));
#365755=CARTESIAN_POINT('Ctrl Pts',(0.779024214864112,-2.72304148523437,
-6.87085818784773));
#365756=CARTESIAN_POINT('Ctrl Pts',(0.0484737436638102,-2.83203340983582,
-6.93113988263782));
#365757=CARTESIAN_POINT('Ctrl Pts',(-0.685481418136962,-2.74824364633194,
-6.99142480614438));
#365758=CARTESIAN_POINT('Ctrl Pts',(-1.37462778885995,-2.47633441354984,
-7.05208818488281));
#365759=CARTESIAN_POINT('Ctrl Pts',(-1.96827391894949,-2.03682611603706,
-7.11236989989014));
#365760=CARTESIAN_POINT('Ctrl Pts',(-2.42801027659746,-1.45859318121514,
-7.17265478410175));
#365761=CARTESIAN_POINT('Ctrl Pts',(-2.72304154587753,-0.779024258186026,
-7.23331815145116));
#365762=CARTESIAN_POINT('Ctrl Pts',(-2.83203304292954,-0.0484735881915938,
-7.29360016643431));
#365763=CARTESIAN_POINT('Ctrl Pts',(-2.74824426833468,0.685481026990187,
-7.35388438911616));
#365764=CARTESIAN_POINT('Ctrl Pts',(-2.47633426068,1.37462897834074,-7.41454797566736));
#365765=CARTESIAN_POINT('Ctrl Pts',(-2.03682260074525,1.96827080720847,
-7.47483300656648));
#365766=CARTESIAN_POINT('Ctrl Pts',(-1.45860575946508,2.42800983497797,
-7.53510984362855));
#365767=CARTESIAN_POINT('Ctrl Pts',(-0.778993598834234,2.72306539561668,
-7.59577812434582));
#365768=CARTESIAN_POINT('Ctrl Pts',(-0.0485111105849109,2.83192268777547,
-7.65608621916571));
#365769=CARTESIAN_POINT('Ctrl Pts',(0.685434178093518,2.74858121042738,
-7.71629032556075));
#365770=CARTESIAN_POINT('Ctrl Pts',(1.37494905476715,2.47530931106774,-7.77708760315606));
#365771=CARTESIAN_POINT('Ctrl Pts',(1.96749699730902,2.03997328191583,-7.83717861739831));
#365772=CARTESIAN_POINT('Ctrl Pts',(2.42925527357646,1.44798370557448,-7.89806652053729));
#365773=CARTESIAN_POINT('Ctrl Pts',(2.72026578942101,0.81850829674785,-7.95608482081467));
#365774=CARTESIAN_POINT('Ctrl Pts',(2.7998363224979,0.209484955020671,-8.00303038055522));
#365775=CARTESIAN_POINT('Ctrl Pts',(2.7998363224979,0.0349606549170308,
-8.01981010684662));
#365776=CARTESIAN_POINT('Ctrl Pts',(2.80005140479051,-0.0349419760186688,
-1.58036093336367));
#365777=CARTESIAN_POINT('Ctrl Pts',(2.80005140479051,-0.222315492003956,
-1.59837605395503));
#365778=CARTESIAN_POINT('Ctrl Pts',(2.7214217418683,-0.809145725726729,
-1.6432251028271));
#365779=CARTESIAN_POINT('Ctrl Pts',(2.4293855576505,-1.45019120570836,-1.70229805797781));
#365780=CARTESIAN_POINT('Ctrl Pts',(1.96768973634555,-2.03953853811049,
-1.7629395123984));
#365781=CARTESIAN_POINT('Ctrl Pts',(1.37507506915162,-2.47563743577604,
-1.8230967134397));
#365782=CARTESIAN_POINT('Ctrl Pts',(0.685513462117749,-2.74874432479135,
-1.88387667036327));
#365783=CARTESIAN_POINT('Ctrl Pts',(-0.0484811831405424,-2.83215111147164,
-1.94408480572724));
#365784=CARTESIAN_POINT('Ctrl Pts',(-0.779026681647449,-2.72327925825339,
-2.00439212797816));
#365785=CARTESIAN_POINT('Ctrl Pts',(-1.45869410662288,-2.42821024693195,
-2.0650608706179));
#365786=CARTESIAN_POINT('Ctrl Pts',(-2.03695498339253,-1.96844588111817,
-2.12533700840671));
#365787=CARTESIAN_POINT('Ctrl Pts',(-2.4765110806735,-1.3747587008243,-2.18562256240842));
#365788=CARTESIAN_POINT('Ctrl Pts',(-2.7484478409841,-0.685559860459645,
-2.24628623797644));
#365789=CARTESIAN_POINT('Ctrl Pts',(-2.83225060905395,0.048443263325025,
-2.30656987054029));
#365790=CARTESIAN_POINT('Ctrl Pts',(-2.72325825549342,0.779057613295582,
-2.36685238231703));
#365791=CARTESIAN_POINT('Ctrl Pts',(-2.42820998732486,1.45868136138043,
-2.4275158429718));
#365792=CARTESIAN_POINT('Ctrl Pts',(-1.96844920055485,2.03695852016992,
-2.48780013698524));
#365793=CARTESIAN_POINT('Ctrl Pts',(-1.37475744002027,2.4765112353038,-2.54808234902813));
#365794=CARTESIAN_POINT('Ctrl Pts',(-0.685560283084277,2.74844721593019,
-2.60874582079915));
#365795=CARTESIAN_POINT('Ctrl Pts',(0.0484434248256224,2.83225097648717,
-2.66903015426646));
#365796=CARTESIAN_POINT('Ctrl Pts',(0.7790575695397,2.72325819429533,-2.72931234606168));
#365797=CARTESIAN_POINT('Ctrl Pts',(1.45868134037711,2.42820998953338,-2.78997582004938));
#365798=CARTESIAN_POINT('Ctrl Pts',(2.0369585467678,1.96844919652417,-2.85026015503416));
#365799=CARTESIAN_POINT('Ctrl Pts',(2.47651122587901,1.37475744638445,-2.91054234588739));
#365800=CARTESIAN_POINT('Ctrl Pts',(2.74844721726047,0.68556028222042,-2.97120582005121));
#365801=CARTESIAN_POINT('Ctrl Pts',(2.8322509766735,-0.0484434261664062,
-3.03149015505023));
#365802=CARTESIAN_POINT('Ctrl Pts',(2.7232581943391,-0.779057568642653,
-3.09177234588191));
#365803=CARTESIAN_POINT('Ctrl Pts',(2.42820998952435,-1.45868134060022,
-3.15243582005264));
#365804=CARTESIAN_POINT('Ctrl Pts',(1.9684491964829,-2.03695854677124,-3.21272015504985));
#365805=CARTESIAN_POINT('Ctrl Pts',(1.37475744641701,-2.4765112258619,-3.27300234588205));
#365806=CARTESIAN_POINT('Ctrl Pts',(0.685560282208511,-2.74844721726587,
-3.33366582005255));
#365807=CARTESIAN_POINT('Ctrl Pts',(-0.0484434261631521,-2.83225097667228,
-3.39395015504989));
#365808=CARTESIAN_POINT('Ctrl Pts',(-0.779057568643627,-2.7232581943397,
-3.45423234588206));
#365809=CARTESIAN_POINT('Ctrl Pts',(-1.45868134060013,-2.42820998952376,
-3.51489582005254));
#365810=CARTESIAN_POINT('Ctrl Pts',(-2.03695854677107,-1.96844919648335,
-3.57518015504989));
#365811=CARTESIAN_POINT('Ctrl Pts',(-2.47651122586207,-1.3747574464168,
-3.63546234588207));
#365812=CARTESIAN_POINT('Ctrl Pts',(-2.74844721726579,-0.685560282208525,
-3.69612582005254));
#365813=CARTESIAN_POINT('Ctrl Pts',(-2.83225097667231,0.0484434261631291,
-3.7564101550499));
#365814=CARTESIAN_POINT('Ctrl Pts',(-2.7232581943397,0.779057568643663,
-3.81669234588207));
#365815=CARTESIAN_POINT('Ctrl Pts',(-2.42820998952376,1.45868134060013,
-3.87735582005254));
#365816=CARTESIAN_POINT('Ctrl Pts',(-1.96844919648335,2.03695854677107,
-3.9376401550499));
#365817=CARTESIAN_POINT('Ctrl Pts',(-1.37475744641679,2.47651122586208,
-3.99792234588207));
#365818=CARTESIAN_POINT('Ctrl Pts',(-0.685560282208515,2.74844721726578,
-4.05858582005252));
#365819=CARTESIAN_POINT('Ctrl Pts',(0.0484434261631405,2.83225097667232,
-4.1188701550499));
#365820=CARTESIAN_POINT('Ctrl Pts',(0.779057568643667,2.72325819433969,
-4.17915234588206));
#365821=CARTESIAN_POINT('Ctrl Pts',(1.45868134060014,2.42820998952375,-4.23981582005254));
#365822=CARTESIAN_POINT('Ctrl Pts',(2.03695854677108,1.96844919648334,-4.30010015504989));
#365823=CARTESIAN_POINT('Ctrl Pts',(2.47651122586209,1.37475744641679,-4.36038234588208));
#365824=CARTESIAN_POINT('Ctrl Pts',(2.74844721726579,0.685560282208506,
-4.42104582005254));
#365825=CARTESIAN_POINT('Ctrl Pts',(2.8322509766723,-0.0484434261631421,
-4.4813301550499));
#365826=CARTESIAN_POINT('Ctrl Pts',(2.72325819433969,-0.779057568643682,
-4.54161234588207));
#365827=CARTESIAN_POINT('Ctrl Pts',(2.42820998952373,-1.45868134060014,
-4.60227582005254));
#365828=CARTESIAN_POINT('Ctrl Pts',(1.96844919648334,-2.03695854677108,
-4.6625601550499));
#365829=CARTESIAN_POINT('Ctrl Pts',(1.37475744641678,-2.47651122586209,
-4.72284234588207));
#365830=CARTESIAN_POINT('Ctrl Pts',(0.685560282208503,-2.74844721726579,
-4.78350582005254));
#365831=CARTESIAN_POINT('Ctrl Pts',(-0.0484434261631558,-2.83225097667233,
-4.84379015504992));
#365832=CARTESIAN_POINT('Ctrl Pts',(-0.77905756864368,-2.72325819433967,
-4.90407234588205));
#365833=CARTESIAN_POINT('Ctrl Pts',(-1.45868134060014,-2.42820998952372,
-4.96473582005253));
#365834=CARTESIAN_POINT('Ctrl Pts',(-2.03695854677109,-1.96844919648334,
-5.0250201550499));
#365835=CARTESIAN_POINT('Ctrl Pts',(-2.47651122586209,-1.37475744641677,
-5.08530234588207));
#365836=CARTESIAN_POINT('Ctrl Pts',(-2.74844721726577,-0.685560282208494,
-5.14596582005252));
#365837=CARTESIAN_POINT('Ctrl Pts',(-2.83225097667232,0.0484434261631642,
-5.20625015504991));
#365838=CARTESIAN_POINT('Ctrl Pts',(-2.72325819433969,0.779057568643699,
-5.26653234588207));
#365839=CARTESIAN_POINT('Ctrl Pts',(-2.42820998952371,1.45868134060015,
-5.32719582005253));
#365840=CARTESIAN_POINT('Ctrl Pts',(-1.96844919648334,2.0369585467711,-5.38748015504991));
#365841=CARTESIAN_POINT('Ctrl Pts',(-1.37475744641676,2.47651122586207,
-5.44776234588206));
#365842=CARTESIAN_POINT('Ctrl Pts',(-0.685560282208465,2.74844721726582,
-5.50842582005256));
#365843=CARTESIAN_POINT('Ctrl Pts',(0.0484434261631459,2.8322509766723,
-5.56871015504991));
#365844=CARTESIAN_POINT('Ctrl Pts',(0.77905756864366,2.7232581943397,-5.62899234588203));
#365845=CARTESIAN_POINT('Ctrl Pts',(1.45868134060035,2.42820998952354,-5.68965582005256));
#365846=CARTESIAN_POINT('Ctrl Pts',(2.03695854677077,1.96844919648363,-5.74994015504994));
#365847=CARTESIAN_POINT('Ctrl Pts',(2.47651122586247,1.37475744641675,-5.81022234588199));
#365848=CARTESIAN_POINT('Ctrl Pts',(2.74844721726539,0.68556028220749,-5.87088582005272));
#365849=CARTESIAN_POINT('Ctrl Pts',(2.83225097667343,-0.0484434261597295,
-5.93117015504957));
#365850=CARTESIAN_POINT('Ctrl Pts',(2.72325819433488,-0.779057568656138,
-5.99145234588337));
#365851=CARTESIAN_POINT('Ctrl Pts',(2.42820998953502,-1.45868134056502,
-6.05211582004729));
#365852=CARTESIAN_POINT('Ctrl Pts',(1.96844919651089,-2.03695854682948,
-6.11240015506561));
#365853=CARTESIAN_POINT('Ctrl Pts',(1.37475744614754,-2.47651122586056,
-6.17268234588436));
#365854=CARTESIAN_POINT('Ctrl Pts',(0.685560283068197,-2.7484472169499,
-6.2333458198777));
#365855=CARTESIAN_POINT('Ctrl Pts',(-0.0484434272739145,-2.83225097815536,
-6.29363015582641));
#365856=CARTESIAN_POINT('Ctrl Pts',(-0.779057569919619,-2.72325819081683,
-6.35391234511296));
#365857=CARTESIAN_POINT('Ctrl Pts',(-1.45868133020244,-2.42820999454269,
-6.41457581704206));
#365858=CARTESIAN_POINT('Ctrl Pts',(-2.03695857643473,-1.96844920071866,
-6.47486017290601));
#365859=CARTESIAN_POINT('Ctrl Pts',(-2.47651118869187,-1.37475742725566,
-6.53514232258922));
#365860=CARTESIAN_POINT('Ctrl Pts',(-2.74844718829262,-0.685560328345768,
-6.59580578606602));
#365861=CARTESIAN_POINT('Ctrl Pts',(-2.83225126519656,0.0484435449931018,
-6.65609043578674));
#365862=CARTESIAN_POINT('Ctrl Pts',(-2.72325793947389,0.779057145346554,
-6.71637192313681));
#365863=CARTESIAN_POINT('Ctrl Pts',(-2.42820926584284,1.45868183876673,
-6.77703563697173));
#365864=CARTESIAN_POINT('Ctrl Pts',(-1.9684512872418,2.03696056375976,-6.83732324720959));
#365865=CARTESIAN_POINT('Ctrl Pts',(-1.37476376271817,2.47650348514813,
-6.89759727195412));
#365866=CARTESIAN_POINT('Ctrl Pts',(-0.685529731491166,2.74846279478609,
-6.95826629062831));
#365867=CARTESIAN_POINT('Ctrl Pts',(0.0483996833656258,2.8322123503721,
-7.01857521801487));
#365868=CARTESIAN_POINT('Ctrl Pts',(0.779017444894231,2.72348202273134,
-7.07878068295039));
#365869=CARTESIAN_POINT('Ctrl Pts',(1.45891552110071,2.42730834706515,-7.13956566066343));
#365870=CARTESIAN_POINT('Ctrl Pts',(2.03664883326185,1.97134324740292,-7.19970870776557));
#365871=CARTESIAN_POINT('Ctrl Pts',(2.47643830365019,1.36561422989075,-7.2603969994144));
#365872=CARTESIAN_POINT('Ctrl Pts',(2.74977893008757,0.719015851050413,
-7.31916157554443));
#365873=CARTESIAN_POINT('Ctrl Pts',(2.80016361091614,0.126800216505963,
-7.36426031277698));
#365874=CARTESIAN_POINT('Ctrl Pts',(2.80016361091613,-0.0349322317809129,
-7.37981016006518));
#365875=CARTESIAN_POINT('Ctrl Pts',(2.00005141137773,-0.0349509159166537,
-1.58027907189674));
#365876=CARTESIAN_POINT('Ctrl Pts',(2.00005141137773,-0.209477500702,-1.59705901785001));
#365877=CARTESIAN_POINT('Ctrl Pts',(1.93937485936534,-0.574981221086946,
-1.64398167301615));
#365878=CARTESIAN_POINT('Ctrl Pts',(1.72866575619624,-1.05218683017129,
-1.70157781695483));
#365879=CARTESIAN_POINT('Ctrl Pts',(1.39603065320521,-1.46514475575449,
-1.76296158741006));
#365880=CARTESIAN_POINT('Ctrl Pts',(0.969522180315677,-1.77589106055163,
-1.82311912419573));
#365881=CARTESIAN_POINT('Ctrl Pts',(0.476783238604109,-1.96670288995313,
-1.88346520364747));
#365882=CARTESIAN_POINT('Ctrl Pts',(-0.0484603850821368,-2.02312932285366,
-1.94396055370022));
#365883=CARTESIAN_POINT('Ctrl Pts',(-0.570338856925993,-1.94138942628423,
-2.00439291407465));
#365884=CARTESIAN_POINT('Ctrl Pts',(-1.05344948325284,-1.72773686772633,
-2.06470891120488));
#365885=CARTESIAN_POINT('Ctrl Pts',(-1.46487312544728,-1.39632835696345,
-2.1251726344757));
#365886=CARTESIAN_POINT('Ctrl Pts',(-1.77606001340043,-0.969474639293403,
-2.18562457894241));
#365887=CARTESIAN_POINT('Ctrl Pts',(-1.9665886161183,-0.476795144252666,
-2.2459421237894));
#365888=CARTESIAN_POINT('Ctrl Pts',(-2.0231790616074,0.0484698229690482,
-2.30639998925771));
#365889=CARTESIAN_POINT('Ctrl Pts',(-1.94138573006516,0.570342005097921,
-2.36685494461854));
#365890=CARTESIAN_POINT('Ctrl Pts',(-1.72773301625381,1.05344259449438,
-2.42717237256682));
#365891=CARTESIAN_POINT('Ctrl Pts',(-1.39633042998923,1.46487729238585,
-2.48762977035772));
#365892=CARTESIAN_POINT('Ctrl Pts',(-0.969474291036093,1.77605966206198,
-2.54808497616048));
#365893=CARTESIAN_POINT('Ctrl Pts',(-0.476795343347378,1.96658811640277,
-2.6084023881129));
#365894=CARTESIAN_POINT('Ctrl Pts',(0.0484699602192744,2.02317939996145,
-2.66885975673847));
#365895=CARTESIAN_POINT('Ctrl Pts',(0.570341982836039,1.94138567238666,
-2.72931497821885));
#365896=CARTESIAN_POINT('Ctrl Pts',(1.05344257210098,1.72773301387229,-2.78963238875962));
#365897=CARTESIAN_POINT('Ctrl Pts',(1.46487731147791,1.39633043581364,-2.85008975616076));
#365898=CARTESIAN_POINT('Ctrl Pts',(1.7760596572503,0.96947429019414,-2.91054497830833));
#365899=CARTESIAN_POINT('Ctrl Pts',(1.96658811657123,0.47679534386094,-2.97086238877306));
#365900=CARTESIAN_POINT('Ctrl Pts',(2.02317940049204,-0.0484699606166185,
-3.03131975614836));
#365901=CARTESIAN_POINT('Ctrl Pts',(1.94138567221384,-0.570341982644115,
-3.09177497831011));
#365902=CARTESIAN_POINT('Ctrl Pts',(1.72773301391076,-1.05344257214956,
-3.15209238877301));
#365903=CARTESIAN_POINT('Ctrl Pts',(1.39633043580907,-1.46487731147983,
-3.21254975614839));
#365904=CARTESIAN_POINT('Ctrl Pts',(0.969474290197969,-1.77605965724421,
-3.27300497831004));
#365905=CARTESIAN_POINT('Ctrl Pts',(0.476795343858464,-1.96658811657341,
-3.33332238877311));
#365906=CARTESIAN_POINT('Ctrl Pts',(-0.0484699606159255,-2.0231794004916,
-3.39377975614832));
#365907=CARTESIAN_POINT('Ctrl Pts',(-0.570341982644268,-1.94138567221424,
-3.45423497831005));
#365908=CARTESIAN_POINT('Ctrl Pts',(-1.05344257214943,-1.72773301391041,
-3.51455238877311));
#365909=CARTESIAN_POINT('Ctrl Pts',(-1.46487731147993,-1.39633043580919,
-3.57500975614831));
#365910=CARTESIAN_POINT('Ctrl Pts',(-1.77605965724425,-0.969474290197954,
-3.63546497831004));
#365911=CARTESIAN_POINT('Ctrl Pts',(-1.96658811657337,-0.476795343858458,
-3.69578238877312));
#365912=CARTESIAN_POINT('Ctrl Pts',(-2.02317940049162,0.0484699606159343,
-3.75623975614831));
#365913=CARTESIAN_POINT('Ctrl Pts',(-1.94138567221425,0.570341982644281,
-3.81669497831005));
#365914=CARTESIAN_POINT('Ctrl Pts',(-1.7277330139104,1.05344257214943,-3.87701238877311));
#365915=CARTESIAN_POINT('Ctrl Pts',(-1.39633043580919,1.46487731147993,
-3.93746975614831));
#365916=CARTESIAN_POINT('Ctrl Pts',(-0.969474290197942,1.77605965724426,
-3.99792497831004));
#365917=CARTESIAN_POINT('Ctrl Pts',(-0.476795343858452,1.96658811657335,
-4.05824238877313));
#365918=CARTESIAN_POINT('Ctrl Pts',(0.0484699606159434,2.02317940049163,
-4.11869975614831));
#365919=CARTESIAN_POINT('Ctrl Pts',(0.570341982644284,1.94138567221424,
-4.17915497831005));
#365920=CARTESIAN_POINT('Ctrl Pts',(1.05344257214943,1.72773301391039,-4.23947238877311));
#365921=CARTESIAN_POINT('Ctrl Pts',(1.46487731147993,1.39633043580918,-4.29992975614832));
#365922=CARTESIAN_POINT('Ctrl Pts',(1.77605965724427,0.969474290197945,
-4.36038497831003));
#365923=CARTESIAN_POINT('Ctrl Pts',(1.96658811657337,0.476795343858441,
-4.42070238877312));
#365924=CARTESIAN_POINT('Ctrl Pts',(2.02317940049162,-0.0484699606159445,
-4.48115975614831));
#365925=CARTESIAN_POINT('Ctrl Pts',(1.94138567221424,-0.570341982644292,
-4.54161497831005));
#365926=CARTESIAN_POINT('Ctrl Pts',(1.72773301391038,-1.05344257214943,
-4.60193238877312));
#365927=CARTESIAN_POINT('Ctrl Pts',(1.39633043580918,-1.46487731147994,
-4.66238975614831));
#365928=CARTESIAN_POINT('Ctrl Pts',(0.969474290197935,-1.77605965724426,
-4.72284497831004));
#365929=CARTESIAN_POINT('Ctrl Pts',(0.476795343858439,-1.96658811657337,
-4.78316238877312));
#365930=CARTESIAN_POINT('Ctrl Pts',(-0.0484699606159579,-2.02317940049164,
-4.8436197561483));
#365931=CARTESIAN_POINT('Ctrl Pts',(-0.570341982644288,-1.94138567221422,
-4.90407497831006));
#365932=CARTESIAN_POINT('Ctrl Pts',(-1.05344257214943,-1.72773301391037,
-4.96439238877312));
#365933=CARTESIAN_POINT('Ctrl Pts',(-1.46487731147995,-1.39633043580918,
-5.02484975614831));
#365934=CARTESIAN_POINT('Ctrl Pts',(-1.77605965724426,-0.969474290197928,
-5.08530497831004));
#365935=CARTESIAN_POINT('Ctrl Pts',(-1.96658811657335,-0.476795343858433,
-5.14562238877313));
#365936=CARTESIAN_POINT('Ctrl Pts',(-2.02317940049163,0.0484699606159606,
-5.2060797561483));
#365937=CARTESIAN_POINT('Ctrl Pts',(-1.94138567221425,0.570341982644311,
-5.26653497831003));
#365938=CARTESIAN_POINT('Ctrl Pts',(-1.72773301391036,1.05344257214944,
-5.32685238877313));
#365939=CARTESIAN_POINT('Ctrl Pts',(-1.39633043580918,1.46487731147996,
-5.3873097561483));
#365940=CARTESIAN_POINT('Ctrl Pts',(-0.969474290197916,1.77605965724424,
-5.44776497831006));
#365941=CARTESIAN_POINT('Ctrl Pts',(-0.476795343858422,1.96658811657339,
-5.5080823887731));
#365942=CARTESIAN_POINT('Ctrl Pts',(0.0484699606159706,2.02317940049163,
-5.56853975614829));
#365943=CARTESIAN_POINT('Ctrl Pts',(0.570341982644291,1.94138567221422,
-5.62899497831007));
#365944=CARTESIAN_POINT('Ctrl Pts',(1.05344257214944,1.72773301391032,-5.68931238877313));
#365945=CARTESIAN_POINT('Ctrl Pts',(1.46487731147996,1.3963304358092,-5.74976975614823));
#365946=CARTESIAN_POINT('Ctrl Pts',(1.77605965724441,0.969474290197947,
-5.81022497831013));
#365947=CARTESIAN_POINT('Ctrl Pts',(1.96658811657315,0.476795343858267,
-5.87054238877304));
#365948=CARTESIAN_POINT('Ctrl Pts',(2.02317940049197,-0.0484699606151168,
-5.93099975614826));
#365949=CARTESIAN_POINT('Ctrl Pts',(1.94138567221262,-0.570341982647331,
-5.99145497831012));
#365950=CARTESIAN_POINT('Ctrl Pts',(1.72773301391079,-1.05344257214282,
-6.05177238877488));
#365951=CARTESIAN_POINT('Ctrl Pts',(1.39633043583791,-1.46487731150212,
-6.1122297561358));
#365952=CARTESIAN_POINT('Ctrl Pts',(0.969474290103704,-1.77605965719443,
-6.17268497832268));
#365953=CARTESIAN_POINT('Ctrl Pts',(0.476795344014053,-1.96658811647506,
-6.23300238886911));
#365954=CARTESIAN_POINT('Ctrl Pts',(-0.0484699607888847,-2.02317940162764,
-6.293459755551));
#365955=CARTESIAN_POINT('Ctrl Pts',(-0.570341982515374,-1.94138566986718,
-6.35391497894857));
#365956=CARTESIAN_POINT('Ctrl Pts',(-1.0534425689941,-1.72773301427299,
-6.41423239105532));
#365957=CARTESIAN_POINT('Ctrl Pts',(-1.46487733129139,-1.39633044764682,
-6.47468974174144));
#365958=CARTESIAN_POINT('Ctrl Pts',(-1.77605962440754,-0.969474272408487,
-6.53514499410053));
#365959=CARTESIAN_POINT('Ctrl Pts',(-1.96658808441403,-0.4767953693466,
-6.59546242507117));
#365960=CARTESIAN_POINT('Ctrl Pts',(-2.02317971788315,0.0484700612956726,
-6.65591951867769));
#365961=CARTESIAN_POINT('Ctrl Pts',(-1.94138529374751,0.57034175258804,
-6.71637524065362));
#365962=CARTESIAN_POINT('Ctrl Pts',(-1.7277327906675,1.05344225923825,-6.77669281345839));
#365963=CARTESIAN_POINT('Ctrl Pts',(-1.39633190064527,1.46488023063332,
-6.83714685373563));
#365964=CARTESIAN_POINT('Ctrl Pts',(-0.969474795144666,1.77605674551469,
-6.89760831895014));
#365965=CARTESIAN_POINT('Ctrl Pts',(-0.476792483974202,1.96658170561334,
-6.95792512927773));
#365966=CARTESIAN_POINT('Ctrl Pts',(0.0484734593030573,2.0232081210323,
-7.01835708981697));
#365967=CARTESIAN_POINT('Ctrl Pts',(0.570336624689882,1.94136175768686,
-7.07885725203471));
#365968=CARTESIAN_POINT('Ctrl Pts',(1.05340619968671,1.72778052727257,-7.13918044053492));
#365969=CARTESIAN_POINT('Ctrl Pts',(1.46503146071072,1.39600002911185,-7.19942807213429));
#365970=CARTESIAN_POINT('Ctrl Pts',(1.77572739170825,0.970967789756964,
-7.26046972816476));
#365971=CARTESIAN_POINT('Ctrl Pts',(1.9679960876878,0.471734127632586,-7.31921124624962));
#365972=CARTESIAN_POINT('Ctrl Pts',(2.00016367750205,0.139563645186354,
-7.36277016686196));
#365973=CARTESIAN_POINT('Ctrl Pts',(2.00016367750204,-0.0349606549172864,
-7.37954989315336));
#365974=CARTESIAN_POINT('',(2.40000003347425,-1.4296958965801E-5,-7.69954908463262));
#365975=CARTESIAN_POINT('Origin',(2.00000003329294,-1.42115683144641E-5,
-7.69954986654408));
#365976=CARTESIAN_POINT('Origin',(2.00000003329294,-1.42115683144641E-5,
-7.69954986654408));
#365977=CARTESIAN_POINT('Origin',(1.99978500519318,0.0219216792995357,-8.68039848401339));
#365978=CARTESIAN_POINT('Origin',(2.00000005748081,-1.17200745147024E-5,
-8.35982870408561));
#365979=CARTESIAN_POINT('Ctrl Pts',(2.00016367750204,-0.0349606549171534,
-7.37954989315335));
#365980=CARTESIAN_POINT('Ctrl Pts',(2.00016367750204,-0.165462727384539,
-7.38526442622049));
#365981=CARTESIAN_POINT('Ctrl Pts',(1.96855967425598,-0.409173319918984,
-7.39995586097472));
#365982=CARTESIAN_POINT('Ctrl Pts',(1.85189486927969,-0.792213245836797,
-7.42009815347362));
#365983=CARTESIAN_POINT('Ctrl Pts',(1.6613582879716,-1.13645205609876,-7.44086906835104));
#365984=CARTESIAN_POINT('Ctrl Pts',(1.37992038202068,-1.47263550497672,
-7.46380724865708));
#365985=CARTESIAN_POINT('Ctrl Pts',(0.992206889613594,-1.76297069041634,
-7.48903838801854));
#365986=CARTESIAN_POINT('Ctrl Pts',(0.502190643379444,-1.95990154002328,
-7.51648926813145));
#365987=CARTESIAN_POINT('Ctrl Pts',(-0.0222096198383131,-2.0232383143754,
-7.54405136994835));
#365988=CARTESIAN_POINT('Ctrl Pts',(-0.545023222850085,-1.94828998299833,
-7.57157271170469));
#365989=CARTESIAN_POINT('Ctrl Pts',(-1.0307284358197,-1.74090605654878,
-7.59904290948243));
#365990=CARTESIAN_POINT('Ctrl Pts',(-1.44636321247892,-1.41496070139146,
-7.62658089390187));
#365991=CARTESIAN_POINT('Ctrl Pts',(-1.7630429012686,-0.992255621812916,
-7.65411407831587));
#365992=CARTESIAN_POINT('Ctrl Pts',(-1.95983623864864,-0.502172632985278,
-7.68158430816739));
#365993=CARTESIAN_POINT('Ctrl Pts',(-2.02326404614228,0.0222054813197516,
-7.70911956348259));
#365994=CARTESIAN_POINT('Ctrl Pts',(-1.94828990091774,0.545028935894718,
-7.73665436795491));
#365995=CARTESIAN_POINT('Ctrl Pts',(-1.74090287629493,1.03072354235614,
-7.76412460420479));
#365996=CARTESIAN_POINT('Ctrl Pts',(-1.41496257868532,1.44636639725859,
-7.79165822650409));
#365997=CARTESIAN_POINT('Ctrl Pts',(-0.992256976006747,1.76304240583952,
-7.81919574931953));
#365998=CARTESIAN_POINT('Ctrl Pts',(-0.502167983314945,1.95983220557862,
-7.84666606566923));
#365999=CARTESIAN_POINT('Ctrl Pts',(0.0222021542767409,2.02327125956959,
-7.87418752174917));
#366000=CARTESIAN_POINT('Ctrl Pts',(0.545036582780956,1.94830483935279,
-7.90174989061211));
#366001=CARTESIAN_POINT('Ctrl Pts',(1.03068639649234,1.74088018296961,-7.92919874059292));
#366002=CARTESIAN_POINT('Ctrl Pts',(1.41193217216583,1.44192597876132,-7.95443773023923));
#366003=CARTESIAN_POINT('Ctrl Pts',(1.68594383364152,1.10008635709056,-7.97735256352204));
#366004=CARTESIAN_POINT('Ctrl Pts',(1.86832284879594,0.749865410246654,
-7.99820416287286));
#366005=CARTESIAN_POINT('Ctrl Pts',(1.97885834740452,0.370827498858678,
-8.01808024799317));
#366006=CARTESIAN_POINT('Ctrl Pts',(2.00021510976845,0.108553308485772,
-8.03354455068052));
#366007=CARTESIAN_POINT('Ctrl Pts',(2.00021510976845,-0.0219451194485651,
-8.03925892415782));
#366008=CARTESIAN_POINT('Ctrl Pts',(2.80016361091613,-0.03493223178078,
-7.37981016006517));
#366009=CARTESIAN_POINT('Ctrl Pts',(2.80016361091613,-0.178346676400516,
-7.38609011080151));
#366010=CARTESIAN_POINT('Ctrl Pts',(2.75800714240104,-0.585623740854942,
-7.39993625174015));
#366011=CARTESIAN_POINT('Ctrl Pts',(2.59622001092688,-1.094203255455,-7.42050939398873));
#366012=CARTESIAN_POINT('Ctrl Pts',(2.33073889442298,-1.58539648585596,
-7.44121574714249));
#366013=CARTESIAN_POINT('Ctrl Pts',(1.93774673958377,-2.05527341692013,
-7.46406250879474));
#366014=CARTESIAN_POINT('Ctrl Pts',(1.3977924816811,-2.46335493607239,-7.4892382031805));
#366015=CARTESIAN_POINT('Ctrl Pts',(0.710887177607718,-2.74177962175189,
-7.51690579573811));
#366016=CARTESIAN_POINT('Ctrl Pts',(-0.0222315527777081,-2.83230238724503,
-7.54433060281804));
#366017=CARTESIAN_POINT('Ctrl Pts',(-0.753696284786715,-2.73017360349673,
-7.57179577476958));
#366018=CARTESIAN_POINT('Ctrl Pts',(-1.4359964022639,-2.44137112409355,
-7.59942818098223));
#366019=CARTESIAN_POINT('Ctrl Pts',(-2.01844596000972,-1.98707136838064,
-7.62687978029761));
#366020=CARTESIAN_POINT('Ctrl Pts',(-2.46348770759376,-1.39755415476222,
-7.65433629789662));
#366021=CARTESIAN_POINT('Ctrl Pts',(-2.74170364490091,-0.710913395495067,
-7.6819659616779));
#366022=CARTESIAN_POINT('Ctrl Pts',(-2.83233201369082,0.0221843029796173,
-7.70942122438771));
#366023=CARTESIAN_POINT('Ctrl Pts',(-2.73016814474818,0.753729685089645,
-7.73687603703565));
#366024=CARTESIAN_POINT('Ctrl Pts',(-2.44136831164089,1.43598613500131,
-7.76450570621253));
#366025=CARTESIAN_POINT('Ctrl Pts',(-1.98707527820992,2.01844704832099,
-7.79196266491878));
#366026=CARTESIAN_POINT('Ctrl Pts',(-1.39756088034447,2.46348708795637,
-7.8194137894634));
#366027=CARTESIAN_POINT('Ctrl Pts',(-0.710881081634362,2.74170412714945,
-7.84704636495045));
#366028=CARTESIAN_POINT('Ctrl Pts',(0.0221378788343896,2.83233850612441,
-7.87451146130275));
#366029=CARTESIAN_POINT('Ctrl Pts',(0.753693185451086,2.73018185071023,
-7.90193724347128));
#366030=CARTESIAN_POINT('Ctrl Pts',(1.43623604645724,2.44132953435746,-7.92960016599444));
#366031=CARTESIAN_POINT('Ctrl Pts',(1.96972754709332,2.02444453015913,-7.95479275010049));
#366032=CARTESIAN_POINT('Ctrl Pts',(2.35530318309127,1.54946734602988,-7.97759034640265));
#366033=CARTESIAN_POINT('Ctrl Pts',(2.61262613808022,1.05037578999858,-7.9984674292579));
#366034=CARTESIAN_POINT('Ctrl Pts',(2.76839001336968,0.552800283700582,
-8.01843767560678));
#366035=CARTESIAN_POINT('Ctrl Pts',(2.80021499480674,0.108538122595088,
-8.03388883389828));
#366036=CARTESIAN_POINT('Ctrl Pts',(2.80021499480674,-0.0219216792995908,
-8.0396015159865));
#366037=CARTESIAN_POINT('Ctrl Pts',(2.7998363224979,0.0349606549171637,
-8.01981010684661));
#366038=CARTESIAN_POINT('Ctrl Pts',(2.7998363224979,-0.108453789702572,
-8.02609005758295));
#366039=CARTESIAN_POINT('Ctrl Pts',(2.76770770092932,-0.554475300665122,
-8.04161041709402));
#366040=CARTESIAN_POINT('Ctrl Pts',(2.61230104920345,-1.04994348735895,
-8.06150470700589));
#366041=CARTESIAN_POINT('Ctrl Pts',(2.35499212095577,-1.5493099165356,-8.08239384111292));
#366042=CARTESIAN_POINT('Ctrl Pts',(1.96948131702204,-2.02412699417522,
-8.10518795929102));
#366043=CARTESIAN_POINT('Ctrl Pts',(1.43606137034988,-2.44099583455896,
-8.1303818337545));
#366044=CARTESIAN_POINT('Ctrl Pts',(0.753613249673498,-2.7298044063241,
-8.15804434422187));
#366045=CARTESIAN_POINT('Ctrl Pts',(0.0221607848766011,-2.83195604538419,
-8.18547015377513));
#366046=CARTESIAN_POINT('Ctrl Pts',(-0.710763089306898,-2.74133925166452,
-8.21293536328677));
#366047=CARTESIAN_POINT('Ctrl Pts',(-1.39735180486206,-2.46316525092768,
-8.24056787474674));
#366048=CARTESIAN_POINT('Ctrl Pts',(-1.9867882252217,-2.01819243450698,
-8.26801892009786));
#366049=CARTESIAN_POINT('Ctrl Pts',(-2.44102701245388,-1.43581160139486,
-8.2954760307671));
#366050=CARTESIAN_POINT('Ctrl Pts',(-2.72979268536681,-0.753649988228477,
-8.32310562488017));
#366051=CARTESIAN_POINT('Ctrl Pts',(-2.83194900848818,-0.022207241173352,
-8.35056035976573));
#366052=CARTESIAN_POINT('Ctrl Pts',(-2.74133888936392,0.710795480178799,
-8.37801577635552));
#366053=CARTESIAN_POINT('Ctrl Pts',(-2.4631658691281,1.3973450383548,-8.4056453623318));
#366054=CARTESIAN_POINT('Ctrl Pts',(-2.0181913618354,1.98678420052489,-8.43310180787527));
#366055=CARTESIAN_POINT('Ctrl Pts',(-1.43582178716812,2.44103031792683,
-8.4605535408052));
#366056=CARTESIAN_POINT('Ctrl Pts',(-0.753616702679641,2.7297964193171,
-8.48818595954062));
#366057=CARTESIAN_POINT('Ctrl Pts',(-0.0222544062348159,2.83192570994805,
-8.51565069030184));
#366058=CARTESIAN_POINT('Ctrl Pts',(0.710769507993571,2.74139122758401,
-8.54307702242869));
#366059=CARTESIAN_POINT('Ctrl Pts',(1.39758336815266,2.4631211079265,-8.5707395161615));
#366060=CARTESIAN_POINT('Ctrl Pts',(1.93746427579644,2.05471988808546,-8.59593214237152));
#366061=CARTESIAN_POINT('Ctrl Pts',(2.33041781164643,1.58599477455527,-8.61873057100975));
#366062=CARTESIAN_POINT('Ctrl Pts',(2.59583452983605,1.0910815303924,-8.63960593440206));
#366063=CARTESIAN_POINT('Ctrl Pts',(2.75797391874601,0.595981365328419,
-8.65957756239152));
#366064=CARTESIAN_POINT('Ctrl Pts',(2.79978489023148,0.152404921343189,
-8.67502839375386));
#366065=CARTESIAN_POINT('Ctrl Pts',(2.79978489023148,0.0219451194485099,
-8.68074107584208));
#366066=CARTESIAN_POINT('Ctrl Pts',(1.99983638908381,0.0349322317807904,
-8.0195498399348));
#366067=CARTESIAN_POINT('Ctrl Pts',(1.99983638908381,-0.10202602676277,
-8.02554708183654));
#366068=CARTESIAN_POINT('Ctrl Pts',(1.97826023278427,-0.374998458759011,
-8.04149750289518));
#366069=CARTESIAN_POINT('Ctrl Pts',(1.86797590755627,-0.748764460301907,
-8.06112897846829));
#366070=CARTESIAN_POINT('Ctrl Pts',(1.68561151450438,-1.10015061289253,
-8.08203775324541));
#366071=CARTESIAN_POINT('Ctrl Pts',(1.41165495945895,-1.44156834906321,
-8.10493617015518));
#366072=CARTESIAN_POINT('Ctrl Pts',(1.03047577828238,-1.74058787531436,
-8.13018098020224));
#366073=CARTESIAN_POINT('Ctrl Pts',(0.544916715445223,-1.94793268220013,
-8.15762809500727));
#366074=CARTESIAN_POINT('Ctrl Pts',(0.0221827178159963,-2.02289026809774,
-8.18519084627103));
#366075=CARTESIAN_POINT('Ctrl Pts',(-0.502090027370269,-1.95945608733342,
-8.21271232019691));
#366076=CARTESIAN_POINT('Ctrl Pts',(-0.992083838417867,-1.76270006106949,
-8.24018259789098));
#366077=CARTESIAN_POINT('Ctrl Pts',(-1.4147054776909,-1.44608180030657,
-8.26772003513789));
#366078=CARTESIAN_POINT('Ctrl Pts',(-1.74058220612872,-1.03051305966975,
-8.29525381080208));
#366079=CARTESIAN_POINT('Ctrl Pts',(-1.94792527911454,-0.54490922807225,
-8.32272397147271));
#366080=CARTESIAN_POINT('Ctrl Pts',(-2.02288104093964,-0.0221860622005593,
-8.3502586988329));
#366081=CARTESIAN_POINT('Ctrl Pts',(-1.95946064553349,0.502094730808056,
-8.37779410728247));
#366082=CARTESIAN_POINT('Ctrl Pts',(-1.76270043378214,0.992082445780963,
-8.40526426032094));
#366083=CARTESIAN_POINT('Ctrl Pts',(-1.4460786623108,1.41470354935293,-8.43279736946537));
#366084=CARTESIAN_POINT('Ctrl Pts',(-1.03051788283039,1.74058563617661,
-8.46033550064529));
#366085=CARTESIAN_POINT('Ctrl Pts',(-0.544903604360224,1.94792449639017,
-8.48780566031878));
#366086=CARTESIAN_POINT('Ctrl Pts',(-0.0221901307924648,2.02285846845712,
-8.51532675052651));
#366087=CARTESIAN_POINT('Ctrl Pts',(0.502112905323441,1.95951419733875,
-8.5428896703966));
#366088=CARTESIAN_POINT('Ctrl Pts',(0.992033718187761,1.76267182698944,
-8.57033808767502));
#366089=CARTESIAN_POINT('Ctrl Pts',(1.37966890086895,1.47220110119364,-8.59557713282226));
#366090=CARTESIAN_POINT('Ctrl Pts',(1.66105846219667,1.13661442398405,-8.61849276017575));
#366091=CARTESIAN_POINT('Ctrl Pts',(1.85153124055178,0.790568741290481,
-8.63934277351964));
#366092=CARTESIAN_POINT('Ctrl Pts',(1.96844225278085,0.414017589463527,
-8.65921974028535));
#366093=CARTESIAN_POINT('Ctrl Pts',(1.99978500519319,0.152400794214044,
-8.67468495623063));
#366094=CARTESIAN_POINT('Ctrl Pts',(1.99978500519318,0.0219216792995357,
-8.68039848401339));
#366095=CARTESIAN_POINT('Ctrl Pts',(1.19983645566973,0.0349038086444169,
-8.01928957302298));
#366096=CARTESIAN_POINT('Ctrl Pts',(1.19983645566973,-0.0955982638229683,
-8.02500410609012));
#366097=CARTESIAN_POINT('Ctrl Pts',(1.18881276463922,-0.1955216168529,-8.04138458869635));
#366098=CARTESIAN_POINT('Ctrl Pts',(1.12365076590908,-0.447585433244864,
-8.06075324993069));
#366099=CARTESIAN_POINT('Ctrl Pts',(1.016230908053,-0.650991309249464,-8.0816816653779));
#366100=CARTESIAN_POINT('Ctrl Pts',(0.853828601895857,-0.859009703951189,
-8.10468438101933));
#366101=CARTESIAN_POINT('Ctrl Pts',(0.624890186214873,-1.04017991606976,
-8.12998012664998));
#366102=CARTESIAN_POINT('Ctrl Pts',(0.336220181216949,-1.16606095807615,
-8.15721184579269));
#366103=CARTESIAN_POINT('Ctrl Pts',(0.0222046507553913,-1.21382449081129,
-8.18491153876691));
#366104=CARTESIAN_POINT('Ctrl Pts',(-0.29341696543364,-1.17757292300231,
-8.21248927710705));
#366105=CARTESIAN_POINT('Ctrl Pts',(-0.586815871973671,-1.0622348712113,
-8.23979732103521));
#366106=CARTESIAN_POINT('Ctrl Pts',(-0.842622730160096,-0.873971166106157,
-8.26742115017792));
#366107=CARTESIAN_POINT('Ctrl Pts',(-1.04013739980356,-0.625214517944632,
-8.29503159083705));
#366108=CARTESIAN_POINT('Ctrl Pts',(-1.16605787286226,-0.336168467916023,
-8.32234231806526));
#366109=CARTESIAN_POINT('Ctrl Pts',(-1.2138130733911,-0.0221648832277664,
-8.34995703790007));
#366110=CARTESIAN_POINT('Ctrl Pts',(-1.17758240170305,0.293393981437313,
-8.37757243820942));
#366111=CARTESIAN_POINT('Ctrl Pts',(-1.06223499843619,0.586819853207128,
-8.40488315831008));
#366112=CARTESIAN_POINT('Ctrl Pts',(-0.873965962786202,0.842622898180978,
-8.43249293105548));
#366113=CARTESIAN_POINT('Ctrl Pts',(-0.625213978492663,1.04014095442639,
-8.46011746048537));
#366114=CARTESIAN_POINT('Ctrl Pts',(-0.336190506040807,1.16605257346324,
-8.48742536109694));
#366115=CARTESIAN_POINT('Ctrl Pts',(-0.0221258553501136,1.21379122696619,
-8.51500281075118));
#366116=CARTESIAN_POINT('Ctrl Pts',(0.293456302653311,1.17763716709349,
-8.54270231836451));
#366117=CARTESIAN_POINT('Ctrl Pts',(0.586484068222858,1.06222254605237,
-8.56993665918854));
#366118=CARTESIAN_POINT('Ctrl Pts',(0.821873525941461,0.889682314301827,
-8.59522212327301));
#366119=CARTESIAN_POINT('Ctrl Pts',(0.991699112746911,0.687234073412837,
-8.61825494934175));
#366120=CARTESIAN_POINT('Ctrl Pts',(1.1072279512675,0.490055952188566,-8.63907961263722));
#366121=CARTESIAN_POINT('Ctrl Pts',(1.17891058681569,0.232053813598634,
-8.65886191817918));
#366122=CARTESIAN_POINT('Ctrl Pts',(1.19978512015489,0.152396667084899,
-8.6743415187074));
#366123=CARTESIAN_POINT('Ctrl Pts',(1.19978512015489,0.0218982391505614,
-8.6800558921847));
#366124=CARTESIAN_POINT('Ctrl Pts',(1.20016374408796,-0.0349890780535269,
-7.37928962624154));
#366125=CARTESIAN_POINT('Ctrl Pts',(1.20016374408796,-0.152578778368561,
-7.38443874163948));
#366126=CARTESIAN_POINT('Ctrl Pts',(1.17911220611093,-0.232722898983027,
-7.39997547020929));
#366127=CARTESIAN_POINT('Ctrl Pts',(1.1075697276325,-0.490223236218595,
-7.41968691295851));
#366128=CARTESIAN_POINT('Ctrl Pts',(0.99197768152021,-0.687507626341548,
-7.44052238955959));
#366129=CARTESIAN_POINT('Ctrl Pts',(0.822094024457586,-0.889997593033309,
-7.46355198851942));
#366130=CARTESIAN_POINT('Ctrl Pts',(0.586621297546092,-1.06258644476029,
-7.48883857285657));
#366131=CARTESIAN_POINT('Ctrl Pts',(0.293494109151169,-1.17802345829468,
-7.51607274052479));
#366132=CARTESIAN_POINT('Ctrl Pts',(-0.022187686898918,-1.21417424150576,
-7.54377213707865));
#366133=CARTESIAN_POINT('Ctrl Pts',(-0.336350160913456,-1.16640636249992,
-7.5713496486398));
#366134=CARTESIAN_POINT('Ctrl Pts',(-0.625460469375504,-1.04044098900401,
-7.59865763798262));
#366135=CARTESIAN_POINT('Ctrl Pts',(-0.874280464948115,-0.842850034402287,
-7.62628200750612));
#366136=CARTESIAN_POINT('Ctrl Pts',(-1.06259809494344,-0.586957088863615,
-7.65389185873512));
#366137=CARTESIAN_POINT('Ctrl Pts',(-1.17796883239637,-0.293431870475487,
-7.68120265465688));
#366138=CARTESIAN_POINT('Ctrl Pts',(-1.21419607859374,0.0222266596598858,
-7.70881790257747));
#366139=CARTESIAN_POINT('Ctrl Pts',(-1.16641165708731,0.33632818669979,
-7.73643269887416));
#366140=CARTESIAN_POINT('Ctrl Pts',(-1.04043744094898,0.625460949710965,
-7.76374350219705));
#366141=CARTESIAN_POINT('Ctrl Pts',(-0.842849879160721,0.874285746196179,
-7.7913537880894));
#366142=CARTESIAN_POINT('Ctrl Pts',(-0.58695307166902,1.06259772372267,
-7.81897770917568));
#366143=CARTESIAN_POINT('Ctrl Pts',(-0.293454884995528,1.17796028400778,
-7.846285766388));
#366144=CARTESIAN_POINT('Ctrl Pts',(0.0222664297190919,1.21420401301477,
-7.87386358219558));
#366145=CARTESIAN_POINT('Ctrl Pts',(0.336379980110826,1.16642782799535,
-7.90156253775294));
#366146=CARTESIAN_POINT('Ctrl Pts',(0.625136746527436,1.04043083158176,
-7.9287973151914));
#366147=CARTESIAN_POINT('Ctrl Pts',(0.854136797238339,0.859407427363523,
-7.95408271037797));
#366148=CARTESIAN_POINT('Ctrl Pts',(1.01658448419176,0.650705368151239,
-7.97711478064143));
#366149=CARTESIAN_POINT('Ctrl Pts',(1.12401955951167,0.449355030494726,
-7.99794089648783));
#366150=CARTESIAN_POINT('Ctrl Pts',(1.18932668143936,0.188854714016773,
-8.01772282037956));
#366151=CARTESIAN_POINT('Ctrl Pts',(1.20021522473016,0.108568494376457,
-8.03320026746274));
#366152=CARTESIAN_POINT('Ctrl Pts',(1.20021522473015,-0.0219685595975393,
-8.03891633232913));
#366153=CARTESIAN_POINT('Ctrl Pts',(2.00016367750204,-0.0349606549171534,
-7.37954989315335));
#366154=CARTESIAN_POINT('Ctrl Pts',(2.00016367750204,-0.165462727384539,
-7.38526442622049));
#366155=CARTESIAN_POINT('Ctrl Pts',(1.96855967425598,-0.409173319918984,
-7.39995586097472));
#366156=CARTESIAN_POINT('Ctrl Pts',(1.85189486927969,-0.792213245836797,
-7.42009815347362));
#366157=CARTESIAN_POINT('Ctrl Pts',(1.6613582879716,-1.13645205609876,-7.44086906835104));
#366158=CARTESIAN_POINT('Ctrl Pts',(1.37992038202068,-1.47263550497672,
-7.46380724865708));
#366159=CARTESIAN_POINT('Ctrl Pts',(0.992206889613594,-1.76297069041634,
-7.48903838801854));
#366160=CARTESIAN_POINT('Ctrl Pts',(0.502190643379444,-1.95990154002328,
-7.51648926813145));
#366161=CARTESIAN_POINT('Ctrl Pts',(-0.0222096198383131,-2.0232383143754,
-7.54405136994835));
#366162=CARTESIAN_POINT('Ctrl Pts',(-0.545023222850085,-1.94828998299833,
-7.57157271170469));
#366163=CARTESIAN_POINT('Ctrl Pts',(-1.0307284358197,-1.74090605654878,
-7.59904290948243));
#366164=CARTESIAN_POINT('Ctrl Pts',(-1.44636321247892,-1.41496070139146,
-7.62658089390187));
#366165=CARTESIAN_POINT('Ctrl Pts',(-1.7630429012686,-0.992255621812916,
-7.65411407831587));
#366166=CARTESIAN_POINT('Ctrl Pts',(-1.95983623864864,-0.502172632985278,
-7.68158430816739));
#366167=CARTESIAN_POINT('Ctrl Pts',(-2.02326404614228,0.0222054813197516,
-7.70911956348259));
#366168=CARTESIAN_POINT('Ctrl Pts',(-1.94828990091774,0.545028935894718,
-7.73665436795491));
#366169=CARTESIAN_POINT('Ctrl Pts',(-1.74090287629493,1.03072354235614,
-7.76412460420479));
#366170=CARTESIAN_POINT('Ctrl Pts',(-1.41496257868532,1.44636639725859,
-7.79165822650409));
#366171=CARTESIAN_POINT('Ctrl Pts',(-0.992256976006747,1.76304240583952,
-7.81919574931953));
#366172=CARTESIAN_POINT('Ctrl Pts',(-0.502167983314945,1.95983220557862,
-7.84666606566923));
#366173=CARTESIAN_POINT('Ctrl Pts',(0.0222021542767409,2.02327125956959,
-7.87418752174917));
#366174=CARTESIAN_POINT('Ctrl Pts',(0.545036582780956,1.94830483935279,
-7.90174989061211));
#366175=CARTESIAN_POINT('Ctrl Pts',(1.03068639649234,1.74088018296961,-7.92919874059292));
#366176=CARTESIAN_POINT('Ctrl Pts',(1.41193217216583,1.44192597876132,-7.95443773023923));
#366177=CARTESIAN_POINT('Ctrl Pts',(1.68594383364152,1.10008635709056,-7.97735256352204));
#366178=CARTESIAN_POINT('Ctrl Pts',(1.86832284879594,0.749865410246654,
-7.99820416287286));
#366179=CARTESIAN_POINT('Ctrl Pts',(1.97885834740452,0.370827498858678,
-8.01808024799317));
#366180=CARTESIAN_POINT('Ctrl Pts',(2.00021510976845,0.108553308485772,
-8.03354455068052));
#366181=CARTESIAN_POINT('Ctrl Pts',(2.00021510976845,-0.0219451194485651,
-8.03925892415782));
#366182=CARTESIAN_POINT('',(1.50000000000003,-2.79999999999998,-0.100000000000142));
#366183=CARTESIAN_POINT('',(1.50000000003703,-13.1999999999996,-0.100000000000131));
#366184=CARTESIAN_POINT('',(0.,0.,0.));
#366185=CARTESIAN_POINT('Origin',(0.,0.,1.25));
#366186=CARTESIAN_POINT('',(-2.40384615384615,-2.94386249795037E-16,0.555555555555555));
#366187=CARTESIAN_POINT('Origin',(0.,0.,0.555555555555555));
#366188=CARTESIAN_POINT('',(-2.40384615384615,-2.94386249795037E-16,1.25));
#366189=CARTESIAN_POINT('',(-2.40384615384615,-2.94386249795037E-16,1.25));
#366190=CARTESIAN_POINT('Origin',(0.,0.,1.25));
#366191=CARTESIAN_POINT('Origin',(0.,0.,-3.36777869765522E-16));
#366192=CARTESIAN_POINT('',(-2.40384615384615,-2.94386249795037E-16,-0.555555555555556));
#366193=CARTESIAN_POINT('Origin',(0.,0.,-0.555555555555556));
#366194=CARTESIAN_POINT('Origin',(-2.25,-2.75545529808155E-16,-3.36777869765522E-16));
#366195=CARTESIAN_POINT('Origin',(0.,0.,1.25));
#366196=CARTESIAN_POINT('',(-2.40384615384615,-2.94386249795037E-16,-1.25));
#366197=CARTESIAN_POINT('Origin',(0.,0.,-1.25));
#366198=CARTESIAN_POINT('',(-2.40384615384615,-2.94386249795037E-16,1.25));
#366199=CARTESIAN_POINT('Origin',(0.,0.,-1.25));
#366200=CARTESIAN_POINT('',(-3.,-3.67394039744206E-16,-1.125));
#366201=CARTESIAN_POINT('Origin',(0.,0.,-1.125));
#366202=CARTESIAN_POINT('',(-2.875,-3.52085954754864E-16,-1.25));
#366203=CARTESIAN_POINT('',(-2.875,-3.52085954754864E-16,-1.25));
#366204=CARTESIAN_POINT('Origin',(0.,0.,-1.25));
#366205=CARTESIAN_POINT('Origin',(0.,0.,1.25));
#366206=CARTESIAN_POINT('',(3.,3.67394039744206E-16,1.125));
#366207=CARTESIAN_POINT('',(-3.,-3.67394039744206E-16,1.125));
#366208=CARTESIAN_POINT('Origin',(0.,0.,1.125));
#366209=CARTESIAN_POINT('Origin',(0.,0.,1.125));
#366210=CARTESIAN_POINT('',(-3.,-3.67394039744206E-16,1.25));
#366211=CARTESIAN_POINT('Origin',(0.,0.,1.125));
#366212=CARTESIAN_POINT('',(2.875,-3.52085954754864E-16,1.25));
#366213=CARTESIAN_POINT('',(3.,-3.67394039744206E-16,1.125));
#366214=CARTESIAN_POINT('Origin',(0.,0.,1.25));
#366215=CARTESIAN_POINT('Origin',(0.,2.875,-1.25));
#366216=CARTESIAN_POINT('Origin',(0.,2.875,1.25));
#366217=CARTESIAN_POINT('Origin',(0.,0.,-9.75781955236954E-16));
#366218=CARTESIAN_POINT('',(-2.09615384615385,2.56704809821272E-16,0.555555555555555));
#366219=CARTESIAN_POINT('Origin',(0.,0.,0.555555555555555));
#366220=CARTESIAN_POINT('',(-2.09615384615385,-2.56704809821272E-16,-0.555555555555556));
#366221=CARTESIAN_POINT('Origin',(-2.25,-2.75545529808154E-16,-9.75781955236954E-16));
#366222=CARTESIAN_POINT('Origin',(0.,0.,-0.555555555555556));
#366223=CARTESIAN_POINT('Origin',(0.,0.,1.25));
#366224=CARTESIAN_POINT('',(-1.5,-1.83697019872103E-16,1.125));
#366225=CARTESIAN_POINT('Origin',(0.,0.,1.125));
#366226=CARTESIAN_POINT('',(-1.625,-1.99005104861445E-16,1.25));
#366227=CARTESIAN_POINT('',(-1.625,-1.99005104861445E-16,1.25));
#366228=CARTESIAN_POINT('Origin',(0.,0.,1.25));
#366229=CARTESIAN_POINT('Origin',(0.,0.,1.25));
#366230=CARTESIAN_POINT('',(1.5,1.91351062366774E-16,-1.125));
#366231=CARTESIAN_POINT('',(-1.5,-1.83697019872103E-16,-1.125));
#366232=CARTESIAN_POINT('Origin',(0.,0.,-1.125));
#366233=CARTESIAN_POINT('Origin',(0.,0.,-1.125));
#366234=CARTESIAN_POINT('',(-1.5,-1.83697019872103E-16,1.25));
#366235=CARTESIAN_POINT('Origin',(0.,0.,-1.125));
#366236=CARTESIAN_POINT('',(1.625,-1.99005104861445E-16,-1.25));
#366237=CARTESIAN_POINT('',(1.5,-1.83697019872103E-16,-1.125));
#366238=CARTESIAN_POINT('Origin',(0.,0.,-1.25));
#366239=CARTESIAN_POINT('Origin',(0.,0.,1.25));
#366240=CARTESIAN_POINT('',(-2.09615384615385,-2.56704809821272E-16,-1.25));
#366241=CARTESIAN_POINT('',(-2.09615384615385,-2.56704809821272E-16,1.25));
#366242=CARTESIAN_POINT('Origin',(0.,0.,-1.25));
#366243=CARTESIAN_POINT('Origin',(0.,0.,1.25));
#366244=CARTESIAN_POINT('',(-2.09615384615385,-2.56704809821272E-16,1.25));
#366245=CARTESIAN_POINT('Origin',(0.,0.,1.25));
#366246=CARTESIAN_POINT('',(-2.09615384615385,-2.56704809821272E-16,1.25));
#366247=CARTESIAN_POINT('Origin',(0.,2.09615384615385,1.25));
#366248=CARTESIAN_POINT('Origin',(0.,1.625,-1.25));
#366249=CARTESIAN_POINT('Origin',(0.,2.25,-3.36777869765522E-16));
#366250=CARTESIAN_POINT('',(-0.576463888168111,2.25,-3.36777869765522E-16));
#366251=CARTESIAN_POINT('',(0.576463888168111,2.25,-3.36777869765522E-16));
#366252=CARTESIAN_POINT('Origin',(0.,2.25,-3.36777869765522E-16));
#366253=CARTESIAN_POINT('Origin',(1.125,1.94855715851499,-3.36777869765522E-16));
#366254=CARTESIAN_POINT('',(0.625767628482067,2.23678910259904,-3.36777869765522E-16));
#366255=CARTESIAN_POINT('',(1.62423237151794,1.66032521443093,-3.36777869765522E-16));
#366256=CARTESIAN_POINT('Origin',(1.125,1.94855715851499,-3.36777869765522E-16));
#366257=CARTESIAN_POINT('Origin',(1.94855715851499,1.125,-3.36777869765522E-16));
#366258=CARTESIAN_POINT('',(1.66032521443094,1.62423237151793,-3.36777869765522E-16));
#366259=CARTESIAN_POINT('',(2.23678910259904,0.625767628482059,-3.36777869765522E-16));
#366260=CARTESIAN_POINT('Origin',(1.94855715851499,1.125,-3.36777869765522E-16));
#366261=CARTESIAN_POINT('Origin',(2.25,-7.85583301239705E-15,-3.36777869765522E-16));
#366262=CARTESIAN_POINT('',(2.25,0.576463888168103,-3.36777869765522E-16));
#366263=CARTESIAN_POINT('',(2.25,-0.576463888168119,-3.36777869765522E-16));
#366264=CARTESIAN_POINT('Origin',(2.25,-7.85583301239705E-15,-3.36777869765522E-16));
#366265=CARTESIAN_POINT('Origin',(1.94855715851498,-1.12500000000001,-3.36777869765522E-16));
#366266=CARTESIAN_POINT('',(2.23678910259904,-0.625767628482075,-3.36777869765522E-16));
#366267=CARTESIAN_POINT('',(1.66032521443092,-1.62423237151794,-3.36777869765522E-16));
#366268=CARTESIAN_POINT('Origin',(1.94855715851498,-1.12500000000001,-3.36777869765522E-16));
#366269=CARTESIAN_POINT('Origin',(1.12499999999999,-1.94855715851499,-3.36777869765522E-16));
#366270=CARTESIAN_POINT('',(1.62423237151793,-1.66032521443094,-3.36777869765522E-16));
#366271=CARTESIAN_POINT('',(0.625767628482051,-2.23678910259905,-3.36777869765522E-16));
#366272=CARTESIAN_POINT('Origin',(1.12499999999999,-1.94855715851499,-3.36777869765522E-16));
#366273=CARTESIAN_POINT('Origin',(-1.57116660247941E-14,-2.25,-3.36777869765522E-16));
#366274=CARTESIAN_POINT('',(0.576463888168095,-2.25,-3.36777869765522E-16));
#366275=CARTESIAN_POINT('',(-0.576463888168127,-2.25,-3.36777869765522E-16));
#366276=CARTESIAN_POINT('Origin',(-1.57116660247941E-14,-2.25,-3.36777869765522E-16));
#366277=CARTESIAN_POINT('Origin',(-1.12500000000002,-1.94855715851498,-3.36777869765522E-16));
#366278=CARTESIAN_POINT('',(-0.625767628482083,-2.23678910259904,-3.36777869765522E-16));
#366279=CARTESIAN_POINT('',(-1.62423237151795,-1.66032521443092,-3.36777869765522E-16));
#366280=CARTESIAN_POINT('Origin',(-1.12500000000002,-1.94855715851498,-3.36777869765522E-16));
#366281=CARTESIAN_POINT('Origin',(-1.948557158515,-1.12499999999998,-3.36777869765522E-16));
#366282=CARTESIAN_POINT('',(-1.66032521443095,-1.62423237151792,-3.36777869765522E-16));
#366283=CARTESIAN_POINT('',(-2.23678910259905,-0.625767628482044,-3.36777869765522E-16));
#366284=CARTESIAN_POINT('Origin',(-1.948557158515,-1.12499999999998,-3.36777869765522E-16));
#366285=CARTESIAN_POINT('Origin',(-2.25,2.35674990371912E-14,-3.36777869765522E-16));
#366286=CARTESIAN_POINT('',(-2.25000000000001,-0.576463888168087,-3.36777869765522E-16));
#366287=CARTESIAN_POINT('',(-2.24999999999999,0.576463888168134,-3.36777869765522E-16));
#366288=CARTESIAN_POINT('Origin',(-2.25,2.35674990371912E-14,-3.36777869765522E-16));
#366289=CARTESIAN_POINT('Origin',(-1.94855715851497,1.12500000000002,-3.36777869765522E-16));
#366290=CARTESIAN_POINT('',(-2.23678910259904,0.62576762848209,-3.36777869765522E-16));
#366291=CARTESIAN_POINT('',(-1.66032521443091,1.62423237151796,-3.36777869765522E-16));
#366292=CARTESIAN_POINT('Origin',(-1.94855715851497,1.12500000000002,-3.36777869765522E-16));
#366293=CARTESIAN_POINT('Origin',(-1.12499999999998,1.948557158515,-3.36777869765522E-16));
#366294=CARTESIAN_POINT('',(-1.62423237151791,1.66032521443095,-3.36777869765522E-16));
#366295=CARTESIAN_POINT('',(-0.625767628482036,2.23678910259905,-3.36777869765522E-16));
#366296=CARTESIAN_POINT('Origin',(-1.12499999999998,1.948557158515,-3.36777869765522E-16));
#366297=CARTESIAN_POINT('Origin',(0.,0.,1.25));
#366298=CARTESIAN_POINT('',(-2.40384615384615,-2.94386249795037E-16,1.1875));
#366299=CARTESIAN_POINT('Origin',(0.,0.,1.1875));
#366300=CARTESIAN_POINT('',(-2.40384615384615,-2.94386249795037E-16,0.576463888168111));
#366301=CARTESIAN_POINT('',(-2.40384615384615,-2.94386249795037E-16,1.25));
#366302=CARTESIAN_POINT('Origin',(0.,0.,0.576463888168111));
#366303=CARTESIAN_POINT('Origin',(0.,0.,1.25));
#366304=CARTESIAN_POINT('',(-2.09615384615385,-2.56704809821272E-16,0.576463888168111));
#366305=CARTESIAN_POINT('Origin',(0.,0.,0.576463888168111));
#366306=CARTESIAN_POINT('',(-2.09615384615385,-2.56704809821272E-16,1.1875));
#366307=CARTESIAN_POINT('',(-2.09615384615385,-2.56704809821272E-16,1.25));
#366308=CARTESIAN_POINT('Origin',(0.,0.,1.1875));
#366309=CARTESIAN_POINT('Origin',(0.,2.40384615384615,1.1875));
#366310=CARTESIAN_POINT('Origin',(0.,2.40384615384615,0.576463888168111));
#366311=CARTESIAN_POINT('Origin',(0.,0.,1.25));
#366312=CARTESIAN_POINT('',(-2.40384615384615,-2.94386249795037E-16,-0.576463888168111));
#366313=CARTESIAN_POINT('Origin',(0.,0.,-0.576463888168111));
#366314=CARTESIAN_POINT('',(-2.40384615384615,-2.94386249795037E-16,-1.1875));
#366315=CARTESIAN_POINT('',(-2.40384615384615,-2.94386249795037E-16,1.25));
#366316=CARTESIAN_POINT('Origin',(0.,0.,-1.1875));
#366317=CARTESIAN_POINT('Origin',(0.,0.,1.25));
#366318=CARTESIAN_POINT('',(-2.09615384615385,-2.56704809821272E-16,-1.1875));
#366319=CARTESIAN_POINT('Origin',(0.,0.,-1.1875));
#366320=CARTESIAN_POINT('',(-2.09615384615385,-2.56704809821272E-16,-0.576463888168111));
#366321=CARTESIAN_POINT('',(-2.09615384615385,-2.56704809821272E-16,1.25));
#366322=CARTESIAN_POINT('Origin',(0.,0.,-0.576463888168111));
#366323=CARTESIAN_POINT('Origin',(0.,2.40384615384615,-1.1875));
#366324=CARTESIAN_POINT('Origin',(0.,2.40384615384615,-0.576463888168111));
#366325=CARTESIAN_POINT('',(0.,0.,0.));
#366326=CARTESIAN_POINT('Origin',(0.,-7.56339435525888E-14,-9.91875));
#366327=CARTESIAN_POINT('',(-4.89956577852113E-30,-1.17524047358082,-9.6375));
#366328=CARTESIAN_POINT('',(1.43925448419928E-16,-1.17524047358099,-9.64975952641922));
#366329=CARTESIAN_POINT('',(1.43925448419928E-16,-1.17524047358099,-9.91875));
#366330=CARTESIAN_POINT('',(-0.190653686693206,-1.15967294634857,-9.64975952641922));
#366331=CARTESIAN_POINT('Ctrl Pts',(-0.190653686693206,-1.15967294634857,
-9.64975952641922));
#366332=CARTESIAN_POINT('Ctrl Pts',(-0.0959624143348448,-1.17524047358082,
-9.64339282863739));
#366333=CARTESIAN_POINT('Ctrl Pts',(-1.43925448419918E-16,-1.17524047358082,
-9.6375));
#366334=CARTESIAN_POINT('Origin',(-1.87350135405495E-14,6.89726054048379E-14,
-9.6497595264191));
#366335=CARTESIAN_POINT('Origin',(0.,-7.56339435525888E-14,-9.91875));
#366336=CARTESIAN_POINT('',(-4.86875089941093E-30,-1.17524047358082,-9.1375));
#366337=CARTESIAN_POINT('',(-4.86875089941093E-30,-1.17524047358082,-9.2));
#366338=CARTESIAN_POINT('',(1.43925448419928E-16,-1.17524047358099,-9.91875));
#366339=CARTESIAN_POINT('Ctrl Pts',(-1.43925448419918E-16,-1.17524047358082,
-9.6375));
#366340=CARTESIAN_POINT('Ctrl Pts',(0.678525403784435,-1.17524047358082,
-9.59583333333333));
#366341=CARTESIAN_POINT('Ctrl Pts',(1.01778810567665,-0.58762023679041,
-9.55416666666667));
#366342=CARTESIAN_POINT('Ctrl Pts',(1.35705080756887,4.56911366618117E-15,
-9.5125));
#366343=CARTESIAN_POINT('Ctrl Pts',(1.01778810567665,0.587620236790419,
-9.47083333333333));
#366344=CARTESIAN_POINT('Ctrl Pts',(0.678525403784436,1.17524047358083,
-9.42916666666667));
#366345=CARTESIAN_POINT('Ctrl Pts',(0.,1.17524047358083,-9.3875));
#366346=CARTESIAN_POINT('Ctrl Pts',(-0.678525403784435,1.17524047358083,
-9.34583333333333));
#366347=CARTESIAN_POINT('Ctrl Pts',(-1.01778810567665,0.58762023679042,
-9.30416666666667));
#366348=CARTESIAN_POINT('Ctrl Pts',(-1.35705080756887,4.79222133198851E-15,
-9.2625));
#366349=CARTESIAN_POINT('Ctrl Pts',(-1.01778810567665,-0.58762023679041,
-9.22083333333333));
#366350=CARTESIAN_POINT('Ctrl Pts',(-0.678525403784435,-1.17524047358082,
-9.17916666666667));
#366351=CARTESIAN_POINT('Ctrl Pts',(-1.43925448419918E-16,-1.17524047358082,
-9.1375));
#366352=CARTESIAN_POINT('',(0.689217670442765,-0.951929185124572,-9.64975952641917));
#366353=CARTESIAN_POINT('Origin',(-1.87350135405495E-14,6.89726054048379E-14,
-9.6497595264191));
#366354=CARTESIAN_POINT('Ctrl Pts',(0.689217670442765,-0.951929185124572,
-9.64975952641917));
#366355=CARTESIAN_POINT('Ctrl Pts',(0.892378271989736,-0.804836440504912,
-9.63206891898562));
#366356=CARTESIAN_POINT('Ctrl Pts',(1.01778810567665,-0.58762023679041,
-9.61666666666667));
#366357=CARTESIAN_POINT('Ctrl Pts',(1.35705080756887,4.59643214611782E-15,
-9.575));
#366358=CARTESIAN_POINT('Ctrl Pts',(1.01778810567665,0.587620236790419,
-9.53333333333333));
#366359=CARTESIAN_POINT('Ctrl Pts',(0.678525403784436,1.17524047358083,
-9.49166666666667));
#366360=CARTESIAN_POINT('Ctrl Pts',(0.,1.17524047358083,-9.45));
#366361=CARTESIAN_POINT('Ctrl Pts',(-0.678525403784435,1.17524047358083,
-9.40833333333333));
#366362=CARTESIAN_POINT('Ctrl Pts',(-1.01778810567665,0.58762023679042,
-9.36666666666667));
#366363=CARTESIAN_POINT('Ctrl Pts',(-1.35705080756887,4.81953981192516E-15,
-9.325));
#366364=CARTESIAN_POINT('Ctrl Pts',(-1.01778810567665,-0.58762023679041,
-9.28333333333333));
#366365=CARTESIAN_POINT('Ctrl Pts',(-0.678525403784435,-1.17524047358082,
-9.24166666666667));
#366366=CARTESIAN_POINT('Ctrl Pts',(-1.43925448419918E-16,-1.17524047358082,
-9.2));
#366367=CARTESIAN_POINT('Origin',(0.,-7.56339435525888E-14,-9.91875));
#366368=CARTESIAN_POINT('',(-4.86875089941093E-30,-1.17524047358082,-8.6375));
#366369=CARTESIAN_POINT('',(-4.86875089941093E-30,-1.17524047358082,-8.7));
#366370=CARTESIAN_POINT('',(1.43925448419928E-16,-1.17524047358099,-9.91875));
#366371=CARTESIAN_POINT('Ctrl Pts',(-1.43925448419918E-16,-1.17524047358082,
-9.1375));
#366372=CARTESIAN_POINT('Ctrl Pts',(0.678525403784435,-1.17524047358083,
-9.09583333333333));
#366373=CARTESIAN_POINT('Ctrl Pts',(1.01778810567665,-0.587620236790411,
-9.05416666666667));
#366374=CARTESIAN_POINT('Ctrl Pts',(1.35705080756887,4.35056582668803E-15,
-9.0125));
#366375=CARTESIAN_POINT('Ctrl Pts',(1.01778810567665,0.587620236790418,
-8.97083333333333));
#366376=CARTESIAN_POINT('Ctrl Pts',(0.678525403784436,1.17524047358083,
-8.92916666666667));
#366377=CARTESIAN_POINT('Ctrl Pts',(0.,1.17524047358083,-8.8875));
#366378=CARTESIAN_POINT('Ctrl Pts',(-0.678525403784435,1.17524047358083,
-8.84583333333333));
#366379=CARTESIAN_POINT('Ctrl Pts',(-1.01778810567665,0.587620236790419,
-8.80416666666667));
#366380=CARTESIAN_POINT('Ctrl Pts',(-1.35705080756887,4.57367349249537E-15,
-8.7625));
#366381=CARTESIAN_POINT('Ctrl Pts',(-1.01778810567665,-0.58762023679041,
-8.72083333333333));
#366382=CARTESIAN_POINT('Ctrl Pts',(-0.678525403784435,-1.17524047358082,
-8.67916666666667));
#366383=CARTESIAN_POINT('Ctrl Pts',(-1.43925448419918E-16,-1.17524047358082,
-8.6375));
#366384=CARTESIAN_POINT('Ctrl Pts',(-1.43925448419918E-16,-1.17524047358082,
-9.2));
#366385=CARTESIAN_POINT('Ctrl Pts',(0.678525403784435,-1.17524047358083,
-9.15833333333333));
#366386=CARTESIAN_POINT('Ctrl Pts',(1.01778810567665,-0.587620236790411,
-9.11666666666667));
#366387=CARTESIAN_POINT('Ctrl Pts',(1.35705080756887,4.37788430662468E-15,
-9.075));
#366388=CARTESIAN_POINT('Ctrl Pts',(1.01778810567665,0.587620236790418,
-9.03333333333333));
#366389=CARTESIAN_POINT('Ctrl Pts',(0.678525403784436,1.17524047358083,
-8.99166666666667));
#366390=CARTESIAN_POINT('Ctrl Pts',(0.,1.17524047358083,-8.95));
#366391=CARTESIAN_POINT('Ctrl Pts',(-0.678525403784435,1.17524047358083,
-8.90833333333333));
#366392=CARTESIAN_POINT('Ctrl Pts',(-1.01778810567665,0.587620236790419,
-8.86666666666667));
#366393=CARTESIAN_POINT('Ctrl Pts',(-1.35705080756887,4.60099197243202E-15,
-8.825));
#366394=CARTESIAN_POINT('Ctrl Pts',(-1.01778810567665,-0.58762023679041,
-8.78333333333333));
#366395=CARTESIAN_POINT('Ctrl Pts',(-0.678525403784435,-1.17524047358082,
-8.74166666666667));
#366396=CARTESIAN_POINT('Ctrl Pts',(-1.43925448419918E-16,-1.17524047358082,
-8.7));
#366397=CARTESIAN_POINT('Origin',(0.,-7.56339435525888E-14,-9.91875));
#366398=CARTESIAN_POINT('',(-4.86875089941093E-30,-1.17524047358083,-8.1375));
#366399=CARTESIAN_POINT('',(-4.86875089941093E-30,-1.17524047358083,-8.2));
#366400=CARTESIAN_POINT('',(1.43925448419928E-16,-1.17524047358099,-9.91875));
#366401=CARTESIAN_POINT('Ctrl Pts',(-1.43925448419918E-16,-1.17524047358082,
-8.6375));
#366402=CARTESIAN_POINT('Ctrl Pts',(0.678525403784435,-1.17524047358083,
-8.59583333333333));
#366403=CARTESIAN_POINT('Ctrl Pts',(1.01778810567665,-0.587620236790411,
-8.55416666666667));
#366404=CARTESIAN_POINT('Ctrl Pts',(1.35705080756887,4.13201798719489E-15,
-8.5125));
#366405=CARTESIAN_POINT('Ctrl Pts',(1.01778810567665,0.587620236790418,
-8.47083333333333));
#366406=CARTESIAN_POINT('Ctrl Pts',(0.678525403784436,1.17524047358083,
-8.42916666666667));
#366407=CARTESIAN_POINT('Ctrl Pts',(0.,1.17524047358083,-8.3875));
#366408=CARTESIAN_POINT('Ctrl Pts',(-0.678525403784435,1.17524047358083,
-8.34583333333333));
#366409=CARTESIAN_POINT('Ctrl Pts',(-1.01778810567665,0.587620236790419,
-8.30416666666667));
#366410=CARTESIAN_POINT('Ctrl Pts',(-1.35705080756887,4.35512565300223E-15,
-8.2625));
#366411=CARTESIAN_POINT('Ctrl Pts',(-1.01778810567665,-0.58762023679041,
-8.22083333333333));
#366412=CARTESIAN_POINT('Ctrl Pts',(-0.678525403784435,-1.17524047358082,
-8.17916666666667));
#366413=CARTESIAN_POINT('Ctrl Pts',(-1.43925448419918E-16,-1.17524047358083,
-8.1375));
#366414=CARTESIAN_POINT('Ctrl Pts',(-1.43925448419918E-16,-1.17524047358082,
-8.7));
#366415=CARTESIAN_POINT('Ctrl Pts',(0.678525403784435,-1.17524047358083,
-8.65833333333333));
#366416=CARTESIAN_POINT('Ctrl Pts',(1.01778810567665,-0.587620236790411,
-8.61666666666667));
#366417=CARTESIAN_POINT('Ctrl Pts',(1.35705080756887,4.15933646713154E-15,
-8.575));
#366418=CARTESIAN_POINT('Ctrl Pts',(1.01778810567665,0.587620236790418,
-8.53333333333333));
#366419=CARTESIAN_POINT('Ctrl Pts',(0.678525403784436,1.17524047358083,
-8.49166666666667));
#366420=CARTESIAN_POINT('Ctrl Pts',(0.,1.17524047358083,-8.45));
#366421=CARTESIAN_POINT('Ctrl Pts',(-0.678525403784435,1.17524047358083,
-8.40833333333333));
#366422=CARTESIAN_POINT('Ctrl Pts',(-1.01778810567665,0.587620236790419,
-8.36666666666667));
#366423=CARTESIAN_POINT('Ctrl Pts',(-1.35705080756887,4.38244413293887E-15,
-8.325));
#366424=CARTESIAN_POINT('Ctrl Pts',(-1.01778810567665,-0.58762023679041,
-8.28333333333333));
#366425=CARTESIAN_POINT('Ctrl Pts',(-0.678525403784435,-1.17524047358082,
-8.24166666666667));
#366426=CARTESIAN_POINT('Ctrl Pts',(-1.43925448419918E-16,-1.17524047358083,
-8.2));
#366427=CARTESIAN_POINT('Origin',(0.,-7.56339435525888E-14,-9.91875));
#366428=CARTESIAN_POINT('',(-4.83793602030074E-30,-1.17524047358083,-7.6375));
#366429=CARTESIAN_POINT('',(-4.83793602030074E-30,-1.17524047358083,-7.7));
#366430=CARTESIAN_POINT('',(1.43925448419928E-16,-1.17524047358099,-9.91875));
#366431=CARTESIAN_POINT('Ctrl Pts',(-1.43925448419918E-16,-1.17524047358083,
-8.1375));
#366432=CARTESIAN_POINT('Ctrl Pts',(0.678525403784435,-1.17524047358083,
-8.09583333333333));
#366433=CARTESIAN_POINT('Ctrl Pts',(1.01778810567665,-0.587620236790411,
-8.05416666666667));
#366434=CARTESIAN_POINT('Ctrl Pts',(1.35705080756887,3.91347014770175E-15,
-8.0125));
#366435=CARTESIAN_POINT('Ctrl Pts',(1.01778810567665,0.587620236790418,
-7.97083333333333));
#366436=CARTESIAN_POINT('Ctrl Pts',(0.678525403784436,1.17524047358083,
-7.92916666666667));
#366437=CARTESIAN_POINT('Ctrl Pts',(0.,1.17524047358083,-7.8875));
#366438=CARTESIAN_POINT('Ctrl Pts',(-0.678525403784435,1.17524047358083,
-7.84583333333333));
#366439=CARTESIAN_POINT('Ctrl Pts',(-1.01778810567665,0.587620236790419,
-7.80416666666667));
#366440=CARTESIAN_POINT('Ctrl Pts',(-1.35705080756887,4.13657781350909E-15,
-7.7625));
#366441=CARTESIAN_POINT('Ctrl Pts',(-1.01778810567665,-0.58762023679041,
-7.72083333333333));
#366442=CARTESIAN_POINT('Ctrl Pts',(-0.678525403784435,-1.17524047358083,
-7.67916666666667));
#366443=CARTESIAN_POINT('Ctrl Pts',(-1.43925448419918E-16,-1.17524047358083,
-7.6375));
#366444=CARTESIAN_POINT('Ctrl Pts',(-1.43925448419918E-16,-1.17524047358083,
-8.2));
#366445=CARTESIAN_POINT('Ctrl Pts',(0.678525403784435,-1.17524047358083,
-8.15833333333333));
#366446=CARTESIAN_POINT('Ctrl Pts',(1.01778810567665,-0.587620236790411,
-8.11666666666667));
#366447=CARTESIAN_POINT('Ctrl Pts',(1.35705080756887,3.94078862763839E-15,
-8.075));
#366448=CARTESIAN_POINT('Ctrl Pts',(1.01778810567665,0.587620236790418,
-8.03333333333333));
#366449=CARTESIAN_POINT('Ctrl Pts',(0.678525403784436,1.17524047358083,
-7.99166666666667));
#366450=CARTESIAN_POINT('Ctrl Pts',(0.,1.17524047358083,-7.95));
#366451=CARTESIAN_POINT('Ctrl Pts',(-0.678525403784435,1.17524047358083,
-7.90833333333333));
#366452=CARTESIAN_POINT('Ctrl Pts',(-1.01778810567665,0.587620236790419,
-7.86666666666667));
#366453=CARTESIAN_POINT('Ctrl Pts',(-1.35705080756887,4.16389629344573E-15,
-7.825));
#366454=CARTESIAN_POINT('Ctrl Pts',(-1.01778810567665,-0.58762023679041,
-7.78333333333333));
#366455=CARTESIAN_POINT('Ctrl Pts',(-0.678525403784435,-1.17524047358083,
-7.74166666666667));
#366456=CARTESIAN_POINT('Ctrl Pts',(-1.43925448419918E-16,-1.17524047358083,
-7.7));
#366457=CARTESIAN_POINT('Origin',(0.,-7.56339435525888E-14,-9.91875));
#366458=CARTESIAN_POINT('',(-4.83793602030074E-30,-1.17524047358083,-7.1375));
#366459=CARTESIAN_POINT('',(-4.83793602030074E-30,-1.17524047358083,-7.2));
#366460=CARTESIAN_POINT('',(1.43925448419928E-16,-1.17524047358099,-9.91875));
#366461=CARTESIAN_POINT('Ctrl Pts',(-1.43925448419918E-16,-1.17524047358083,
-7.6375));
#366462=CARTESIAN_POINT('Ctrl Pts',(0.678525403784435,-1.17524047358083,
-7.59583333333333));
#366463=CARTESIAN_POINT('Ctrl Pts',(1.01778810567665,-0.587620236790411,
-7.55416666666667));
#366464=CARTESIAN_POINT('Ctrl Pts',(1.35705080756887,3.69492230820861E-15,
-7.5125));
#366465=CARTESIAN_POINT('Ctrl Pts',(1.01778810567665,0.587620236790418,
-7.47083333333333));
#366466=CARTESIAN_POINT('Ctrl Pts',(0.678525403784436,1.17524047358083,
-7.42916666666667));
#366467=CARTESIAN_POINT('Ctrl Pts',(0.,1.17524047358083,-7.3875));
#366468=CARTESIAN_POINT('Ctrl Pts',(-0.678525403784435,1.17524047358083,
-7.34583333333333));
#366469=CARTESIAN_POINT('Ctrl Pts',(-1.01778810567665,0.587620236790419,
-7.30416666666667));
#366470=CARTESIAN_POINT('Ctrl Pts',(-1.35705080756887,3.91802997401595E-15,
-7.2625));
#366471=CARTESIAN_POINT('Ctrl Pts',(-1.01778810567665,-0.587620236790411,
-7.22083333333333));
#366472=CARTESIAN_POINT('Ctrl Pts',(-0.678525403784435,-1.17524047358083,
-7.17916666666667));
#366473=CARTESIAN_POINT('Ctrl Pts',(-1.43925448419918E-16,-1.17524047358083,
-7.1375));
#366474=CARTESIAN_POINT('Ctrl Pts',(-1.43925448419918E-16,-1.17524047358083,
-7.7));
#366475=CARTESIAN_POINT('Ctrl Pts',(0.678525403784435,-1.17524047358083,
-7.65833333333333));
#366476=CARTESIAN_POINT('Ctrl Pts',(1.01778810567665,-0.587620236790411,
-7.61666666666667));
#366477=CARTESIAN_POINT('Ctrl Pts',(1.35705080756887,3.72224078814525E-15,
-7.575));
#366478=CARTESIAN_POINT('Ctrl Pts',(1.01778810567665,0.587620236790418,
-7.53333333333333));
#366479=CARTESIAN_POINT('Ctrl Pts',(0.678525403784436,1.17524047358083,
-7.49166666666667));
#366480=CARTESIAN_POINT('Ctrl Pts',(0.,1.17524047358083,-7.45));
#366481=CARTESIAN_POINT('Ctrl Pts',(-0.678525403784435,1.17524047358083,
-7.40833333333333));
#366482=CARTESIAN_POINT('Ctrl Pts',(-1.01778810567665,0.587620236790419,
-7.36666666666667));
#366483=CARTESIAN_POINT('Ctrl Pts',(-1.35705080756887,3.94534845395259E-15,
-7.325));
#366484=CARTESIAN_POINT('Ctrl Pts',(-1.01778810567665,-0.587620236790411,
-7.28333333333333));
#366485=CARTESIAN_POINT('Ctrl Pts',(-0.678525403784435,-1.17524047358083,
-7.24166666666667));
#366486=CARTESIAN_POINT('Ctrl Pts',(-1.43925448419918E-16,-1.17524047358083,
-7.2));
#366487=CARTESIAN_POINT('Origin',(0.,-7.56339435525888E-14,-9.91875));
#366488=CARTESIAN_POINT('',(-4.80712114119054E-30,-1.17524047358083,-6.6375));
#366489=CARTESIAN_POINT('',(-4.80712114119054E-30,-1.17524047358083,-6.7));
#366490=CARTESIAN_POINT('',(1.43925448419928E-16,-1.17524047358099,-9.91875));
#366491=CARTESIAN_POINT('Ctrl Pts',(-1.43925448419918E-16,-1.17524047358083,
-7.1375));
#366492=CARTESIAN_POINT('Ctrl Pts',(0.678525403784435,-1.17524047358083,
-7.09583333333333));
#366493=CARTESIAN_POINT('Ctrl Pts',(1.01778810567665,-0.587620236790411,
-7.05416666666667));
#366494=CARTESIAN_POINT('Ctrl Pts',(1.35705080756887,3.47637446871547E-15,
-7.0125));
#366495=CARTESIAN_POINT('Ctrl Pts',(1.01778810567665,0.587620236790417,
-6.97083333333333));
#366496=CARTESIAN_POINT('Ctrl Pts',(0.678525403784436,1.17524047358083,
-6.92916666666667));
#366497=CARTESIAN_POINT('Ctrl Pts',(0.,1.17524047358083,-6.8875));
#366498=CARTESIAN_POINT('Ctrl Pts',(-0.678525403784435,1.17524047358083,
-6.84583333333333));
#366499=CARTESIAN_POINT('Ctrl Pts',(-1.01778810567665,0.587620236790418,
-6.80416666666667));
#366500=CARTESIAN_POINT('Ctrl Pts',(-1.35705080756887,3.69948213452281E-15,
-6.7625));
#366501=CARTESIAN_POINT('Ctrl Pts',(-1.01778810567665,-0.587620236790411,
-6.72083333333333));
#366502=CARTESIAN_POINT('Ctrl Pts',(-0.678525403784435,-1.17524047358083,
-6.67916666666667));
#366503=CARTESIAN_POINT('Ctrl Pts',(-1.43925448419918E-16,-1.17524047358083,
-6.6375));
#366504=CARTESIAN_POINT('Ctrl Pts',(-1.43925448419918E-16,-1.17524047358083,
-7.2));
#366505=CARTESIAN_POINT('Ctrl Pts',(0.678525403784435,-1.17524047358083,
-7.15833333333333));
#366506=CARTESIAN_POINT('Ctrl Pts',(1.01778810567665,-0.587620236790411,
-7.11666666666667));
#366507=CARTESIAN_POINT('Ctrl Pts',(1.35705080756887,3.50369294865211E-15,
-7.075));
#366508=CARTESIAN_POINT('Ctrl Pts',(1.01778810567665,0.587620236790417,
-7.03333333333333));
#366509=CARTESIAN_POINT('Ctrl Pts',(0.678525403784436,1.17524047358083,
-6.99166666666667));
#366510=CARTESIAN_POINT('Ctrl Pts',(0.,1.17524047358083,-6.95));
#366511=CARTESIAN_POINT('Ctrl Pts',(-0.678525403784435,1.17524047358083,
-6.90833333333333));
#366512=CARTESIAN_POINT('Ctrl Pts',(-1.01778810567665,0.587620236790418,
-6.86666666666667));
#366513=CARTESIAN_POINT('Ctrl Pts',(-1.35705080756887,3.72680061445945E-15,
-6.825));
#366514=CARTESIAN_POINT('Ctrl Pts',(-1.01778810567665,-0.587620236790411,
-6.78333333333333));
#366515=CARTESIAN_POINT('Ctrl Pts',(-0.678525403784435,-1.17524047358083,
-6.74166666666667));
#366516=CARTESIAN_POINT('Ctrl Pts',(-1.43925448419918E-16,-1.17524047358083,
-6.7));
#366517=CARTESIAN_POINT('Origin',(0.,-7.56339435525888E-14,-9.91875));
#366518=CARTESIAN_POINT('',(-4.80712114119054E-30,-1.17524047358083,-6.1375));
#366519=CARTESIAN_POINT('',(-4.80712114119054E-30,-1.17524047358083,-6.2));
#366520=CARTESIAN_POINT('',(1.43925448419928E-16,-1.17524047358099,-9.91875));
#366521=CARTESIAN_POINT('Ctrl Pts',(-1.43925448419918E-16,-1.17524047358083,
-6.6375));
#366522=CARTESIAN_POINT('Ctrl Pts',(0.678525403784435,-1.17524047358083,
-6.59583333333333));
#366523=CARTESIAN_POINT('Ctrl Pts',(1.01778810567665,-0.587620236790412,
-6.55416666666667));
#366524=CARTESIAN_POINT('Ctrl Pts',(1.35705080756887,3.25782662922233E-15,
-6.5125));
#366525=CARTESIAN_POINT('Ctrl Pts',(1.01778810567665,0.587620236790417,
-6.47083333333333));
#366526=CARTESIAN_POINT('Ctrl Pts',(0.678525403784436,1.17524047358083,
-6.42916666666667));
#366527=CARTESIAN_POINT('Ctrl Pts',(0.,1.17524047358083,-6.3875));
#366528=CARTESIAN_POINT('Ctrl Pts',(-0.678525403784435,1.17524047358083,
-6.34583333333333));
#366529=CARTESIAN_POINT('Ctrl Pts',(-1.01778810567665,0.587620236790418,
-6.30416666666667));
#366530=CARTESIAN_POINT('Ctrl Pts',(-1.35705080756887,3.48093429502967E-15,
-6.2625));
#366531=CARTESIAN_POINT('Ctrl Pts',(-1.01778810567665,-0.587620236790411,
-6.22083333333333));
#366532=CARTESIAN_POINT('Ctrl Pts',(-0.678525403784435,-1.17524047358083,
-6.17916666666667));
#366533=CARTESIAN_POINT('Ctrl Pts',(-1.43925448419918E-16,-1.17524047358083,
-6.1375));
#366534=CARTESIAN_POINT('Ctrl Pts',(-1.43925448419918E-16,-1.17524047358083,
-6.7));
#366535=CARTESIAN_POINT('Ctrl Pts',(0.678525403784435,-1.17524047358083,
-6.65833333333333));
#366536=CARTESIAN_POINT('Ctrl Pts',(1.01778810567665,-0.587620236790412,
-6.61666666666667));
#366537=CARTESIAN_POINT('Ctrl Pts',(1.35705080756887,3.28514510915897E-15,
-6.575));
#366538=CARTESIAN_POINT('Ctrl Pts',(1.01778810567665,0.587620236790417,
-6.53333333333333));
#366539=CARTESIAN_POINT('Ctrl Pts',(0.678525403784436,1.17524047358083,
-6.49166666666667));
#366540=CARTESIAN_POINT('Ctrl Pts',(0.,1.17524047358083,-6.45));
#366541=CARTESIAN_POINT('Ctrl Pts',(-0.678525403784435,1.17524047358083,
-6.40833333333334));
#366542=CARTESIAN_POINT('Ctrl Pts',(-1.01778810567665,0.587620236790418,
-6.36666666666667));
#366543=CARTESIAN_POINT('Ctrl Pts',(-1.35705080756887,3.50825277496631E-15,
-6.325));
#366544=CARTESIAN_POINT('Ctrl Pts',(-1.01778810567665,-0.587620236790411,
-6.28333333333333));
#366545=CARTESIAN_POINT('Ctrl Pts',(-0.678525403784435,-1.17524047358083,
-6.24166666666667));
#366546=CARTESIAN_POINT('Ctrl Pts',(-1.43925448419918E-16,-1.17524047358083,
-6.2));
#366547=CARTESIAN_POINT('Origin',(0.,-7.56339435525888E-14,-9.91875));
#366548=CARTESIAN_POINT('',(-4.77630626208034E-30,-1.17524047358083,-5.6375));
#366549=CARTESIAN_POINT('',(-4.77630626208034E-30,-1.17524047358083,-5.7));
#366550=CARTESIAN_POINT('',(1.43925448419928E-16,-1.17524047358099,-9.91875));
#366551=CARTESIAN_POINT('Ctrl Pts',(-1.43925448419918E-16,-1.17524047358083,
-6.1375));
#366552=CARTESIAN_POINT('Ctrl Pts',(0.678525403784435,-1.17524047358083,
-6.09583333333333));
#366553=CARTESIAN_POINT('Ctrl Pts',(1.01778810567665,-0.587620236790412,
-6.05416666666667));
#366554=CARTESIAN_POINT('Ctrl Pts',(1.35705080756887,3.03927878972919E-15,
-6.0125));
#366555=CARTESIAN_POINT('Ctrl Pts',(1.01778810567665,0.587620236790417,
-5.97083333333333));
#366556=CARTESIAN_POINT('Ctrl Pts',(0.678525403784436,1.17524047358083,
-5.92916666666667));
#366557=CARTESIAN_POINT('Ctrl Pts',(0.,1.17524047358083,-5.8875));
#366558=CARTESIAN_POINT('Ctrl Pts',(-0.678525403784435,1.17524047358083,
-5.84583333333333));
#366559=CARTESIAN_POINT('Ctrl Pts',(-1.01778810567665,0.587620236790418,
-5.80416666666667));
#366560=CARTESIAN_POINT('Ctrl Pts',(-1.35705080756887,3.26238645553653E-15,
-5.7625));
#366561=CARTESIAN_POINT('Ctrl Pts',(-1.01778810567665,-0.587620236790411,
-5.72083333333333));
#366562=CARTESIAN_POINT('Ctrl Pts',(-0.678525403784435,-1.17524047358083,
-5.67916666666667));
#366563=CARTESIAN_POINT('Ctrl Pts',(-1.43925448419918E-16,-1.17524047358083,
-5.6375));
#366564=CARTESIAN_POINT('Ctrl Pts',(-1.43925448419918E-16,-1.17524047358083,
-6.2));
#366565=CARTESIAN_POINT('Ctrl Pts',(0.678525403784435,-1.17524047358083,
-6.15833333333333));
#366566=CARTESIAN_POINT('Ctrl Pts',(1.01778810567665,-0.587620236790412,
-6.11666666666667));
#366567=CARTESIAN_POINT('Ctrl Pts',(1.35705080756887,3.06659726966583E-15,
-6.075));
#366568=CARTESIAN_POINT('Ctrl Pts',(1.01778810567665,0.587620236790417,
-6.03333333333333));
#366569=CARTESIAN_POINT('Ctrl Pts',(0.678525403784436,1.17524047358083,
-5.99166666666667));
#366570=CARTESIAN_POINT('Ctrl Pts',(0.,1.17524047358083,-5.95));
#366571=CARTESIAN_POINT('Ctrl Pts',(-0.678525403784435,1.17524047358083,
-5.90833333333333));
#366572=CARTESIAN_POINT('Ctrl Pts',(-1.01778810567665,0.587620236790418,
-5.86666666666667));
#366573=CARTESIAN_POINT('Ctrl Pts',(-1.35705080756887,3.28970493547317E-15,
-5.825));
#366574=CARTESIAN_POINT('Ctrl Pts',(-1.01778810567665,-0.587620236790411,
-5.78333333333333));
#366575=CARTESIAN_POINT('Ctrl Pts',(-0.678525403784435,-1.17524047358083,
-5.74166666666667));
#366576=CARTESIAN_POINT('Ctrl Pts',(-1.43925448419918E-16,-1.17524047358083,
-5.7));
#366577=CARTESIAN_POINT('Origin',(0.,-7.56339435525888E-14,-9.91875));
#366578=CARTESIAN_POINT('',(-4.77630626208034E-30,-1.17524047358083,-5.1375));
#366579=CARTESIAN_POINT('',(-4.77630626208034E-30,-1.17524047358083,-5.2));
#366580=CARTESIAN_POINT('',(1.43925448419928E-16,-1.17524047358099,-9.91875));
#366581=CARTESIAN_POINT('Ctrl Pts',(-1.43925448419918E-16,-1.17524047358083,
-5.6375));
#366582=CARTESIAN_POINT('Ctrl Pts',(0.678525403784435,-1.17524047358083,
-5.59583333333333));
#366583=CARTESIAN_POINT('Ctrl Pts',(1.01778810567665,-0.587620236790412,
-5.55416666666667));
#366584=CARTESIAN_POINT('Ctrl Pts',(1.35705080756887,2.82073095023605E-15,
-5.5125));
#366585=CARTESIAN_POINT('Ctrl Pts',(1.01778810567665,0.587620236790417,
-5.47083333333333));
#366586=CARTESIAN_POINT('Ctrl Pts',(0.678525403784436,1.17524047358083,
-5.42916666666667));
#366587=CARTESIAN_POINT('Ctrl Pts',(0.,1.17524047358083,-5.3875));
#366588=CARTESIAN_POINT('Ctrl Pts',(-0.678525403784435,1.17524047358083,
-5.34583333333333));
#366589=CARTESIAN_POINT('Ctrl Pts',(-1.01778810567665,0.587620236790418,
-5.30416666666667));
#366590=CARTESIAN_POINT('Ctrl Pts',(-1.35705080756887,3.04383861604338E-15,
-5.2625));
#366591=CARTESIAN_POINT('Ctrl Pts',(-1.01778810567665,-0.587620236790411,
-5.22083333333333));
#366592=CARTESIAN_POINT('Ctrl Pts',(-0.678525403784435,-1.17524047358083,
-5.17916666666667));
#366593=CARTESIAN_POINT('Ctrl Pts',(-1.43925448419918E-16,-1.17524047358083,
-5.1375));
#366594=CARTESIAN_POINT('Ctrl Pts',(-1.43925448419918E-16,-1.17524047358083,
-5.7));
#366595=CARTESIAN_POINT('Ctrl Pts',(0.678525403784435,-1.17524047358083,
-5.65833333333333));
#366596=CARTESIAN_POINT('Ctrl Pts',(1.01778810567665,-0.587620236790412,
-5.61666666666667));
#366597=CARTESIAN_POINT('Ctrl Pts',(1.35705080756887,2.84804943017269E-15,
-5.575));
#366598=CARTESIAN_POINT('Ctrl Pts',(1.01778810567665,0.587620236790417,
-5.53333333333333));
#366599=CARTESIAN_POINT('Ctrl Pts',(0.678525403784436,1.17524047358083,
-5.49166666666667));
#366600=CARTESIAN_POINT('Ctrl Pts',(0.,1.17524047358083,-5.45));
#366601=CARTESIAN_POINT('Ctrl Pts',(-0.678525403784435,1.17524047358083,
-5.40833333333333));
#366602=CARTESIAN_POINT('Ctrl Pts',(-1.01778810567665,0.587620236790418,
-5.36666666666667));
#366603=CARTESIAN_POINT('Ctrl Pts',(-1.35705080756887,3.07115709598003E-15,
-5.325));
#366604=CARTESIAN_POINT('Ctrl Pts',(-1.01778810567665,-0.587620236790411,
-5.28333333333333));
#366605=CARTESIAN_POINT('Ctrl Pts',(-0.678525403784435,-1.17524047358083,
-5.24166666666667));
#366606=CARTESIAN_POINT('Ctrl Pts',(-1.43925448419918E-16,-1.17524047358083,
-5.2));
#366607=CARTESIAN_POINT('Origin',(0.,-7.56339435525888E-14,-9.91875));
#366608=CARTESIAN_POINT('',(-4.74549138297015E-30,-1.17524047358083,-4.6375));
#366609=CARTESIAN_POINT('',(-4.74549138297015E-30,-1.17524047358083,-4.7));
#366610=CARTESIAN_POINT('',(1.43925448419928E-16,-1.17524047358099,-9.91875));
#366611=CARTESIAN_POINT('Ctrl Pts',(-1.43925448419918E-16,-1.17524047358083,
-5.1375));
#366612=CARTESIAN_POINT('Ctrl Pts',(0.678525403784435,-1.17524047358083,
-5.09583333333333));
#366613=CARTESIAN_POINT('Ctrl Pts',(1.01778810567665,-0.587620236790412,
-5.05416666666667));
#366614=CARTESIAN_POINT('Ctrl Pts',(1.35705080756887,2.6021831107429E-15,
-5.0125));
#366615=CARTESIAN_POINT('Ctrl Pts',(1.01778810567665,0.587620236790417,
-4.97083333333333));
#366616=CARTESIAN_POINT('Ctrl Pts',(0.678525403784436,1.17524047358083,
-4.92916666666667));
#366617=CARTESIAN_POINT('Ctrl Pts',(0.,1.17524047358083,-4.8875));
#366618=CARTESIAN_POINT('Ctrl Pts',(-0.678525403784435,1.17524047358083,
-4.84583333333333));
#366619=CARTESIAN_POINT('Ctrl Pts',(-1.01778810567665,0.587620236790418,
-4.80416666666667));
#366620=CARTESIAN_POINT('Ctrl Pts',(-1.35705080756887,2.82529077655024E-15,
-4.7625));
#366621=CARTESIAN_POINT('Ctrl Pts',(-1.01778810567665,-0.587620236790412,
-4.72083333333333));
#366622=CARTESIAN_POINT('Ctrl Pts',(-0.678525403784435,-1.17524047358083,
-4.67916666666667));
#366623=CARTESIAN_POINT('Ctrl Pts',(-1.43925448419918E-16,-1.17524047358083,
-4.6375));
#366624=CARTESIAN_POINT('Ctrl Pts',(-1.43925448419918E-16,-1.17524047358083,
-5.2));
#366625=CARTESIAN_POINT('Ctrl Pts',(0.678525403784435,-1.17524047358083,
-5.15833333333333));
#366626=CARTESIAN_POINT('Ctrl Pts',(1.01778810567665,-0.587620236790412,
-5.11666666666667));
#366627=CARTESIAN_POINT('Ctrl Pts',(1.35705080756887,2.62950159067955E-15,
-5.075));
#366628=CARTESIAN_POINT('Ctrl Pts',(1.01778810567665,0.587620236790417,
-5.03333333333333));
#366629=CARTESIAN_POINT('Ctrl Pts',(0.678525403784436,1.17524047358083,
-4.99166666666667));
#366630=CARTESIAN_POINT('Ctrl Pts',(0.,1.17524047358083,-4.95));
#366631=CARTESIAN_POINT('Ctrl Pts',(-0.678525403784435,1.17524047358083,
-4.90833333333333));
#366632=CARTESIAN_POINT('Ctrl Pts',(-1.01778810567665,0.587620236790418,
-4.86666666666667));
#366633=CARTESIAN_POINT('Ctrl Pts',(-1.35705080756887,2.85260925648689E-15,
-4.825));
#366634=CARTESIAN_POINT('Ctrl Pts',(-1.01778810567665,-0.587620236790412,
-4.78333333333333));
#366635=CARTESIAN_POINT('Ctrl Pts',(-0.678525403784435,-1.17524047358083,
-4.74166666666667));
#366636=CARTESIAN_POINT('Ctrl Pts',(-1.43925448419918E-16,-1.17524047358083,
-4.7));
#366637=CARTESIAN_POINT('Origin',(0.,-7.56339435525888E-14,-9.91875));
#366638=CARTESIAN_POINT('',(-4.74549138297015E-30,-1.17524047358083,-4.1375));
#366639=CARTESIAN_POINT('',(-4.74549138297015E-30,-1.17524047358083,-4.2));
#366640=CARTESIAN_POINT('',(1.43925448419928E-16,-1.17524047358099,-9.91875));
#366641=CARTESIAN_POINT('Ctrl Pts',(-1.43925448419918E-16,-1.17524047358083,
-4.6375));
#366642=CARTESIAN_POINT('Ctrl Pts',(0.678525403784435,-1.17524047358083,
-4.59583333333333));
#366643=CARTESIAN_POINT('Ctrl Pts',(1.01778810567665,-0.587620236790413,
-4.55416666666667));
#366644=CARTESIAN_POINT('Ctrl Pts',(1.35705080756887,2.38363527124976E-15,
-4.5125));
#366645=CARTESIAN_POINT('Ctrl Pts',(1.01778810567665,0.587620236790416,
-4.47083333333333));
#366646=CARTESIAN_POINT('Ctrl Pts',(0.678525403784436,1.17524047358083,
-4.42916666666667));
#366647=CARTESIAN_POINT('Ctrl Pts',(0.,1.17524047358083,-4.3875));
#366648=CARTESIAN_POINT('Ctrl Pts',(-0.678525403784435,1.17524047358083,
-4.34583333333333));
#366649=CARTESIAN_POINT('Ctrl Pts',(-1.01778810567665,0.587620236790417,
-4.30416666666667));
#366650=CARTESIAN_POINT('Ctrl Pts',(-1.35705080756887,2.6067429370571E-15,
-4.2625));
#366651=CARTESIAN_POINT('Ctrl Pts',(-1.01778810567665,-0.587620236790412,
-4.22083333333333));
#366652=CARTESIAN_POINT('Ctrl Pts',(-0.678525403784435,-1.17524047358083,
-4.17916666666667));
#366653=CARTESIAN_POINT('Ctrl Pts',(-1.43925448419918E-16,-1.17524047358083,
-4.1375));
#366654=CARTESIAN_POINT('Ctrl Pts',(-1.43925448419918E-16,-1.17524047358083,
-4.7));
#366655=CARTESIAN_POINT('Ctrl Pts',(0.678525403784435,-1.17524047358083,
-4.65833333333333));
#366656=CARTESIAN_POINT('Ctrl Pts',(1.01778810567665,-0.587620236790413,
-4.61666666666667));
#366657=CARTESIAN_POINT('Ctrl Pts',(1.35705080756887,2.41095375118641E-15,
-4.575));
#366658=CARTESIAN_POINT('Ctrl Pts',(1.01778810567665,0.587620236790416,
-4.53333333333333));
#366659=CARTESIAN_POINT('Ctrl Pts',(0.678525403784436,1.17524047358083,
-4.49166666666667));
#366660=CARTESIAN_POINT('Ctrl Pts',(0.,1.17524047358083,-4.45));
#366661=CARTESIAN_POINT('Ctrl Pts',(-0.678525403784435,1.17524047358083,
-4.40833333333333));
#366662=CARTESIAN_POINT('Ctrl Pts',(-1.01778810567665,0.587620236790417,
-4.36666666666667));
#366663=CARTESIAN_POINT('Ctrl Pts',(-1.35705080756887,2.63406141699374E-15,
-4.325));
#366664=CARTESIAN_POINT('Ctrl Pts',(-1.01778810567665,-0.587620236790412,
-4.28333333333333));
#366665=CARTESIAN_POINT('Ctrl Pts',(-0.678525403784435,-1.17524047358083,
-4.24166666666667));
#366666=CARTESIAN_POINT('Ctrl Pts',(-1.43925448419918E-16,-1.17524047358083,
-4.2));
#366667=CARTESIAN_POINT('Origin',(0.,-7.56339435525888E-14,-9.91875));
#366668=CARTESIAN_POINT('',(-4.74549138297015E-30,-1.17524047358083,-3.6375));
#366669=CARTESIAN_POINT('',(-4.74549138297015E-30,-1.17524047358083,-3.7));
#366670=CARTESIAN_POINT('',(1.43925448419928E-16,-1.17524047358099,-9.91875));
#366671=CARTESIAN_POINT('Ctrl Pts',(-1.43925448419918E-16,-1.17524047358083,
-4.1375));
#366672=CARTESIAN_POINT('Ctrl Pts',(0.678525403784435,-1.17524047358083,
-4.09583333333333));
#366673=CARTESIAN_POINT('Ctrl Pts',(1.01778810567665,-0.587620236790413,
-4.05416666666667));
#366674=CARTESIAN_POINT('Ctrl Pts',(1.35705080756887,2.16508743175662E-15,
-4.0125));
#366675=CARTESIAN_POINT('Ctrl Pts',(1.01778810567665,0.587620236790416,
-3.97083333333333));
#366676=CARTESIAN_POINT('Ctrl Pts',(0.678525403784436,1.17524047358083,
-3.92916666666667));
#366677=CARTESIAN_POINT('Ctrl Pts',(0.,1.17524047358083,-3.8875));
#366678=CARTESIAN_POINT('Ctrl Pts',(-0.678525403784435,1.17524047358083,
-3.84583333333333));
#366679=CARTESIAN_POINT('Ctrl Pts',(-1.01778810567665,0.587620236790417,
-3.80416666666667));
#366680=CARTESIAN_POINT('Ctrl Pts',(-1.35705080756887,2.38819509756396E-15,
-3.7625));
#366681=CARTESIAN_POINT('Ctrl Pts',(-1.01778810567665,-0.587620236790412,
-3.72083333333333));
#366682=CARTESIAN_POINT('Ctrl Pts',(-0.678525403784435,-1.17524047358083,
-3.67916666666667));
#366683=CARTESIAN_POINT('Ctrl Pts',(-1.43925448419918E-16,-1.17524047358083,
-3.6375));
#366684=CARTESIAN_POINT('Ctrl Pts',(-1.43925448419918E-16,-1.17524047358083,
-4.2));
#366685=CARTESIAN_POINT('Ctrl Pts',(0.678525403784435,-1.17524047358083,
-4.15833333333333));
#366686=CARTESIAN_POINT('Ctrl Pts',(1.01778810567665,-0.587620236790413,
-4.11666666666667));
#366687=CARTESIAN_POINT('Ctrl Pts',(1.35705080756887,2.19240591169326E-15,
-4.075));
#366688=CARTESIAN_POINT('Ctrl Pts',(1.01778810567665,0.587620236790416,
-4.03333333333333));
#366689=CARTESIAN_POINT('Ctrl Pts',(0.678525403784436,1.17524047358083,
-3.99166666666667));
#366690=CARTESIAN_POINT('Ctrl Pts',(0.,1.17524047358083,-3.95));
#366691=CARTESIAN_POINT('Ctrl Pts',(-0.678525403784435,1.17524047358083,
-3.90833333333333));
#366692=CARTESIAN_POINT('Ctrl Pts',(-1.01778810567665,0.587620236790417,
-3.86666666666667));
#366693=CARTESIAN_POINT('Ctrl Pts',(-1.35705080756887,2.4155135775006E-15,
-3.825));
#366694=CARTESIAN_POINT('Ctrl Pts',(-1.01778810567665,-0.587620236790412,
-3.78333333333333));
#366695=CARTESIAN_POINT('Ctrl Pts',(-0.678525403784435,-1.17524047358083,
-3.74166666666667));
#366696=CARTESIAN_POINT('Ctrl Pts',(-1.43925448419918E-16,-1.17524047358083,
-3.7));
#366697=CARTESIAN_POINT('Origin',(0.,-7.56339435525888E-14,-9.91875));
#366698=CARTESIAN_POINT('',(-4.71467650385995E-30,-1.17524047358083,-3.1375));
#366699=CARTESIAN_POINT('',(-4.71467650385995E-30,-1.17524047358083,-3.2));
#366700=CARTESIAN_POINT('',(1.43925448419928E-16,-1.17524047358099,-9.91875));
#366701=CARTESIAN_POINT('Ctrl Pts',(-1.43925448419918E-16,-1.17524047358083,
-3.6375));
#366702=CARTESIAN_POINT('Ctrl Pts',(0.678525403784435,-1.17524047358083,
-3.59583333333333));
#366703=CARTESIAN_POINT('Ctrl Pts',(1.01778810567665,-0.587620236790413,
-3.55416666666667));
#366704=CARTESIAN_POINT('Ctrl Pts',(1.35705080756887,1.94653959226348E-15,
-3.5125));
#366705=CARTESIAN_POINT('Ctrl Pts',(1.01778810567665,0.587620236790416,
-3.47083333333333));
#366706=CARTESIAN_POINT('Ctrl Pts',(0.678525403784436,1.17524047358083,
-3.42916666666667));
#366707=CARTESIAN_POINT('Ctrl Pts',(0.,1.17524047358083,-3.3875));
#366708=CARTESIAN_POINT('Ctrl Pts',(-0.678525403784435,1.17524047358083,
-3.34583333333333));
#366709=CARTESIAN_POINT('Ctrl Pts',(-1.01778810567665,0.587620236790417,
-3.30416666666667));
#366710=CARTESIAN_POINT('Ctrl Pts',(-1.35705080756887,2.16964725807082E-15,
-3.2625));
#366711=CARTESIAN_POINT('Ctrl Pts',(-1.01778810567665,-0.587620236790412,
-3.22083333333333));
#366712=CARTESIAN_POINT('Ctrl Pts',(-0.678525403784435,-1.17524047358083,
-3.17916666666667));
#366713=CARTESIAN_POINT('Ctrl Pts',(-1.43925448419918E-16,-1.17524047358083,
-3.1375));
#366714=CARTESIAN_POINT('Ctrl Pts',(-1.43925448419918E-16,-1.17524047358083,
-3.7));
#366715=CARTESIAN_POINT('Ctrl Pts',(0.678525403784435,-1.17524047358083,
-3.65833333333333));
#366716=CARTESIAN_POINT('Ctrl Pts',(1.01778810567665,-0.587620236790413,
-3.61666666666667));
#366717=CARTESIAN_POINT('Ctrl Pts',(1.35705080756887,1.97385807220012E-15,
-3.575));
#366718=CARTESIAN_POINT('Ctrl Pts',(1.01778810567665,0.587620236790416,
-3.53333333333333));
#366719=CARTESIAN_POINT('Ctrl Pts',(0.678525403784436,1.17524047358083,
-3.49166666666667));
#366720=CARTESIAN_POINT('Ctrl Pts',(0.,1.17524047358083,-3.45));
#366721=CARTESIAN_POINT('Ctrl Pts',(-0.678525403784435,1.17524047358083,
-3.40833333333333));
#366722=CARTESIAN_POINT('Ctrl Pts',(-1.01778810567665,0.587620236790417,
-3.36666666666667));
#366723=CARTESIAN_POINT('Ctrl Pts',(-1.35705080756887,2.19696573800746E-15,
-3.325));
#366724=CARTESIAN_POINT('Ctrl Pts',(-1.01778810567665,-0.587620236790412,
-3.28333333333333));
#366725=CARTESIAN_POINT('Ctrl Pts',(-0.678525403784435,-1.17524047358083,
-3.24166666666667));
#366726=CARTESIAN_POINT('Ctrl Pts',(-1.43925448419918E-16,-1.17524047358083,
-3.2));
#366727=CARTESIAN_POINT('Origin',(0.,-7.56339435525888E-14,-9.91875));
#366728=CARTESIAN_POINT('',(-4.71467650385995E-30,-1.17524047358083,-2.6375));
#366729=CARTESIAN_POINT('',(-4.71467650385995E-30,-1.17524047358083,-2.7));
#366730=CARTESIAN_POINT('',(1.43925448419928E-16,-1.17524047358099,-9.91875));
#366731=CARTESIAN_POINT('Ctrl Pts',(-1.43925448419918E-16,-1.17524047358083,
-3.1375));
#366732=CARTESIAN_POINT('Ctrl Pts',(0.678525403784435,-1.17524047358083,
-3.09583333333333));
#366733=CARTESIAN_POINT('Ctrl Pts',(1.01778810567665,-0.587620236790413,
-3.05416666666667));
#366734=CARTESIAN_POINT('Ctrl Pts',(1.35705080756887,1.72799175277034E-15,
-3.0125));
#366735=CARTESIAN_POINT('Ctrl Pts',(1.01778810567665,0.587620236790416,
-2.97083333333333));
#366736=CARTESIAN_POINT('Ctrl Pts',(0.678525403784436,1.17524047358083,
-2.92916666666667));
#366737=CARTESIAN_POINT('Ctrl Pts',(0.,1.17524047358083,-2.8875));
#366738=CARTESIAN_POINT('Ctrl Pts',(-0.678525403784435,1.17524047358083,
-2.84583333333333));
#366739=CARTESIAN_POINT('Ctrl Pts',(-1.01778810567665,0.587620236790417,
-2.80416666666667));
#366740=CARTESIAN_POINT('Ctrl Pts',(-1.35705080756887,1.95109941857768E-15,
-2.7625));
#366741=CARTESIAN_POINT('Ctrl Pts',(-1.01778810567665,-0.587620236790413,
-2.72083333333333));
#366742=CARTESIAN_POINT('Ctrl Pts',(-0.678525403784435,-1.17524047358083,
-2.67916666666667));
#366743=CARTESIAN_POINT('Ctrl Pts',(-1.43925448419918E-16,-1.17524047358083,
-2.6375));
#366744=CARTESIAN_POINT('Ctrl Pts',(-1.43925448419918E-16,-1.17524047358083,
-3.2));
#366745=CARTESIAN_POINT('Ctrl Pts',(0.678525403784435,-1.17524047358083,
-3.15833333333333));
#366746=CARTESIAN_POINT('Ctrl Pts',(1.01778810567665,-0.587620236790413,
-3.11666666666667));
#366747=CARTESIAN_POINT('Ctrl Pts',(1.35705080756887,1.75531023270698E-15,
-3.075));
#366748=CARTESIAN_POINT('Ctrl Pts',(1.01778810567665,0.587620236790416,
-3.03333333333333));
#366749=CARTESIAN_POINT('Ctrl Pts',(0.678525403784436,1.17524047358083,
-2.99166666666667));
#366750=CARTESIAN_POINT('Ctrl Pts',(0.,1.17524047358083,-2.95));
#366751=CARTESIAN_POINT('Ctrl Pts',(-0.678525403784435,1.17524047358083,
-2.90833333333333));
#366752=CARTESIAN_POINT('Ctrl Pts',(-1.01778810567665,0.587620236790417,
-2.86666666666667));
#366753=CARTESIAN_POINT('Ctrl Pts',(-1.35705080756887,1.97841789851432E-15,
-2.825));
#366754=CARTESIAN_POINT('Ctrl Pts',(-1.01778810567665,-0.587620236790413,
-2.78333333333333));
#366755=CARTESIAN_POINT('Ctrl Pts',(-0.678525403784435,-1.17524047358083,
-2.74166666666667));
#366756=CARTESIAN_POINT('Ctrl Pts',(-1.43925448419918E-16,-1.17524047358083,
-2.7));
#366757=CARTESIAN_POINT('Origin',(0.,-7.56339435525888E-14,-9.91875));
#366758=CARTESIAN_POINT('',(-4.68386162474976E-30,-1.17524047358083,-2.1375));
#366759=CARTESIAN_POINT('',(-4.68386162474976E-30,-1.17524047358083,-2.2));
#366760=CARTESIAN_POINT('',(1.43925448419928E-16,-1.17524047358099,-9.91875));
#366761=CARTESIAN_POINT('Ctrl Pts',(-1.43925448419918E-16,-1.17524047358083,
-2.6375));
#366762=CARTESIAN_POINT('Ctrl Pts',(0.678525403784435,-1.17524047358083,
-2.59583333333333));
#366763=CARTESIAN_POINT('Ctrl Pts',(1.01778810567665,-0.587620236790414,
-2.55416666666667));
#366764=CARTESIAN_POINT('Ctrl Pts',(1.35705080756887,1.5094439132772E-15,
-2.5125));
#366765=CARTESIAN_POINT('Ctrl Pts',(1.01778810567665,0.587620236790415,
-2.47083333333333));
#366766=CARTESIAN_POINT('Ctrl Pts',(0.678525403784436,1.17524047358083,
-2.42916666666667));
#366767=CARTESIAN_POINT('Ctrl Pts',(0.,1.17524047358083,-2.3875));
#366768=CARTESIAN_POINT('Ctrl Pts',(-0.678525403784435,1.17524047358083,
-2.34583333333333));
#366769=CARTESIAN_POINT('Ctrl Pts',(-1.01778810567665,0.587620236790416,
-2.30416666666667));
#366770=CARTESIAN_POINT('Ctrl Pts',(-1.35705080756887,1.73255157908454E-15,
-2.2625));
#366771=CARTESIAN_POINT('Ctrl Pts',(-1.01778810567665,-0.587620236790413,
-2.22083333333333));
#366772=CARTESIAN_POINT('Ctrl Pts',(-0.678525403784435,-1.17524047358083,
-2.17916666666667));
#366773=CARTESIAN_POINT('Ctrl Pts',(-1.43925448419918E-16,-1.17524047358083,
-2.1375));
#366774=CARTESIAN_POINT('Ctrl Pts',(-1.43925448419918E-16,-1.17524047358083,
-2.7));
#366775=CARTESIAN_POINT('Ctrl Pts',(0.678525403784435,-1.17524047358083,
-2.65833333333333));
#366776=CARTESIAN_POINT('Ctrl Pts',(1.01778810567665,-0.587620236790414,
-2.61666666666667));
#366777=CARTESIAN_POINT('Ctrl Pts',(1.35705080756887,1.53676239321384E-15,
-2.575));
#366778=CARTESIAN_POINT('Ctrl Pts',(1.01778810567665,0.587620236790415,
-2.53333333333333));
#366779=CARTESIAN_POINT('Ctrl Pts',(0.678525403784436,1.17524047358083,
-2.49166666666667));
#366780=CARTESIAN_POINT('Ctrl Pts',(0.,1.17524047358083,-2.45));
#366781=CARTESIAN_POINT('Ctrl Pts',(-0.678525403784435,1.17524047358083,
-2.40833333333333));
#366782=CARTESIAN_POINT('Ctrl Pts',(-1.01778810567665,0.587620236790416,
-2.36666666666667));
#366783=CARTESIAN_POINT('Ctrl Pts',(-1.35705080756887,1.75987005902118E-15,
-2.325));
#366784=CARTESIAN_POINT('Ctrl Pts',(-1.01778810567665,-0.587620236790413,
-2.28333333333333));
#366785=CARTESIAN_POINT('Ctrl Pts',(-0.678525403784435,-1.17524047358083,
-2.24166666666667));
#366786=CARTESIAN_POINT('Ctrl Pts',(-1.43925448419918E-16,-1.17524047358083,
-2.2));
#366787=CARTESIAN_POINT('Origin',(0.,2.16840434497101E-16,-9.7));
#366788=CARTESIAN_POINT('',(8.37355900338938E-15,-1.5,-1.95));
#366789=CARTESIAN_POINT('',(-1.10524344990624E-13,-1.5,-1.88750000000001));
#366790=CARTESIAN_POINT('',(-1.83697019872103E-16,-1.5,-9.7));
#366791=CARTESIAN_POINT('',(3.31235039396818E-12,1.5,-1.70000000000016));
#366792=CARTESIAN_POINT('Ctrl Pts',(1.69308150266509E-14,-1.5,-1.95));
#366793=CARTESIAN_POINT('Ctrl Pts',(0.01548927559932,-1.5,-1.94925477188026));
#366794=CARTESIAN_POINT('Ctrl Pts',(0.0309872899763081,-1.49976008338734,
-1.94850245896548));
#366795=CARTESIAN_POINT('Ctrl Pts',(0.245230706998799,-1.49311698268964,
-1.93801013718304));
#366796=CARTESIAN_POINT('Ctrl Pts',(0.440744097796248,-1.44749995108539,
-1.92733635501567));
#366797=CARTESIAN_POINT('Ctrl Pts',(0.799081574720929,-1.28432119946332,
-1.90556309201812));
#366798=CARTESIAN_POINT('Ctrl Pts',(0.959083807576905,-1.16969177102424,
-1.89468083021062));
#366799=CARTESIAN_POINT('Ctrl Pts',(1.22335267335872,-0.888702989669011,
-1.87416094455096));
#366800=CARTESIAN_POINT('Ctrl Pts',(1.32631553511077,-0.726132398087802,
-1.8653406887826));
#366801=CARTESIAN_POINT('Ctrl Pts',(1.46936522121737,-0.362105715195533,
-1.84511698417747));
#366802=CARTESIAN_POINT('Ctrl Pts',(1.50453671316576,-0.16281355519964,
-1.83404519751103));
#366803=CARTESIAN_POINT('Ctrl Pts',(1.49471805803775,0.230113327460341,
-1.81221592625215));
#366804=CARTESIAN_POINT('Ctrl Pts',(1.45282581838479,0.420057916318203,
-1.80166344909338));
#366805=CARTESIAN_POINT('Ctrl Pts',(1.29846283502885,0.775942345695251,
-1.78189209190576));
#366806=CARTESIAN_POINT('Ctrl Pts',(1.18661123088408,0.938112544720388,
-1.77269884433335));
#366807=CARTESIAN_POINT('Ctrl Pts',(0.906165332737575,1.21137288812808,
-1.75161531967302));
#366808=CARTESIAN_POINT('Ctrl Pts',(0.739976898836962,1.31946560344659,
-1.74061699949345));
#366809=CARTESIAN_POINT('Ctrl Pts',(0.38027303752142,1.4635305198243,-1.71930893616415));
#366810=CARTESIAN_POINT('Ctrl Pts',(0.190972331354127,1.49999999999957,
-1.70918816057627));
#366811=CARTESIAN_POINT('Ctrl Pts',(3.42524619778573E-12,1.5,-1.70000000000016));
#366812=CARTESIAN_POINT('',(1.05094390383305,1.07028823734364,-1.7));
#366813=CARTESIAN_POINT('Origin',(0.,0.,-1.7));
#366814=CARTESIAN_POINT('Ctrl Pts',(1.05094390383305,1.07028823734364,-1.7));
#366815=CARTESIAN_POINT('Ctrl Pts',(1.13868622596693,0.984131765341644,
-1.70661473977534));
#366816=CARTESIAN_POINT('Ctrl Pts',(1.21551289992726,0.887500782972839,
-1.71299525880436));
#366817=CARTESIAN_POINT('Ctrl Pts',(1.34320212457071,0.678698115085337,
-1.72493878359739));
#366818=CARTESIAN_POINT('Ctrl Pts',(1.39385259493898,0.567464160994353,
-1.7309742132781));
#366819=CARTESIAN_POINT('Ctrl Pts',(1.48909100396381,0.265573903134679,
-1.74774589427031));
#366820=CARTESIAN_POINT('Ctrl Pts',(1.51095330790636,0.0702300270822034,
-1.75859833182878));
#366821=CARTESIAN_POINT('Ctrl Pts',(1.47847203925917,-0.321929757940045,
-1.78038498655224));
#366822=CARTESIAN_POINT('Ctrl Pts',(1.42283948268589,-0.514849569711096,
-1.79110275387285));
#366823=CARTESIAN_POINT('Ctrl Pts',(1.24364892170843,-0.859893643390216,
-1.81027186907725));
#366824=CARTESIAN_POINT('Ctrl Pts',(1.12486783254292,-1.01033797780081,
-1.81977804833436));
#366825=CARTESIAN_POINT('Ctrl Pts',(0.832106228736892,-1.26349166477242,
-1.84089559442517));
#366826=CARTESIAN_POINT('Ctrl Pts',(0.659148099511349,-1.36174019513924,
-1.85194617214093));
#366827=CARTESIAN_POINT('Ctrl Pts',(0.319613523634357,-1.47433868038769,
-1.87140977274076));
#366828=CARTESIAN_POINT('Ctrl Pts',(0.160210430373053,-1.50000000000003,
-1.87979187207477));
#366829=CARTESIAN_POINT('Ctrl Pts',(-2.2062213167473E-13,-1.5,-1.88750000000001));
#366830=CARTESIAN_POINT('Origin',(0.,2.16840434497101E-16,-9.7));
#366831=CARTESIAN_POINT('',(1.10235999999511E-13,-1.5,-2.44999999999999));
#366832=CARTESIAN_POINT('',(-1.78584683734892E-16,-1.5,-2.3875));
#366833=CARTESIAN_POINT('',(-1.83697019872103E-16,-1.5,-9.7));
#366834=CARTESIAN_POINT('Ctrl Pts',(2.20655697018894E-13,-1.5,-2.44999999999999));
#366835=CARTESIAN_POINT('Ctrl Pts',(0.0446866432717563,-1.5,-2.44785001287315));
#366836=CARTESIAN_POINT('Ctrl Pts',(0.0894198514888752,-1.498003204062,
-2.44564231883545));
#366837=CARTESIAN_POINT('Ctrl Pts',(0.3321653732503,-1.47621975128952,-2.43335812356398));
#366838=CARTESIAN_POINT('Ctrl Pts',(0.524735235130775,-1.41922200076027,
-2.4225098309164));
#366839=CARTESIAN_POINT('Ctrl Pts',(0.871983263480545,-1.23581136686393,
-2.40070811253234));
#366840=CARTESIAN_POINT('Ctrl Pts',(1.02425456323397,-1.11287912297099,
-2.38996717165455));
#366841=CARTESIAN_POINT('Ctrl Pts',(1.27260752980148,-0.816998279750627,
-2.36979937166772));
#366842=CARTESIAN_POINT('Ctrl Pts',(1.3667848766936,-0.647237619333921,
-2.3609576455185));
#366843=CARTESIAN_POINT('Ctrl Pts',(1.48799058251274,-0.274881222866593,
-2.34027117904809));
#366844=CARTESIAN_POINT('Ctrl Pts',(1.51129959338589,-0.0750919538647505,
-2.32917177521466));
#366845=CARTESIAN_POINT('Ctrl Pts',(1.47915085768955,0.314388053469471,
-2.30753399702943));
#366846=CARTESIAN_POINT('Ctrl Pts',(1.42692591478426,0.500630191029841,
-2.29718721160941));
#366847=CARTESIAN_POINT('Ctrl Pts',(1.25204566055684,0.849614101653204,
-2.27779921657477));
#366848=CARTESIAN_POINT('Ctrl Pts',(1.1286436947597,1.00779587912277,-2.26797423177337));
#366849=CARTESIAN_POINT('Ctrl Pts',(0.828833174688191,1.2655911178986,-2.24638861254606));
#366850=CARTESIAN_POINT('Ctrl Pts',(0.655921667069359,1.36325085762577,
-2.23535663320894));
#366851=CARTESIAN_POINT('Ctrl Pts',(0.288677744379025,1.48416505168848,
-2.21432887412746));
#366852=CARTESIAN_POINT('Ctrl Pts',(0.0986552973958269,1.50874919684857,
-2.20498958845478));
#366853=CARTESIAN_POINT('Ctrl Pts',(-0.289385654160681,1.48519512435956,
-2.18566567967694));
#366854=CARTESIAN_POINT('Ctrl Pts',(-0.483493906473983,1.43379201778904,
-2.17489877796179));
#366855=CARTESIAN_POINT('Ctrl Pts',(-0.836359921965577,1.26027651369972,
-2.1531016287622));
#366856=CARTESIAN_POINT('Ctrl Pts',(-0.992499988597624,1.14138038910413,
-2.1422866661761));
#366857=CARTESIAN_POINT('Ctrl Pts',(-1.2487389672651,0.852825405147202,
-2.12194294634587));
#366858=CARTESIAN_POINT('Ctrl Pts',(-1.34727470246183,0.686665969635683,
-2.11314810942415));
#366859=CARTESIAN_POINT('Ctrl Pts',(-1.47937082574391,0.318393327600033,
-2.09268851819995));
#366860=CARTESIAN_POINT('Ctrl Pts',(-1.50857345947938,0.118766243301032,
-2.08159812462778));
#366861=CARTESIAN_POINT('Ctrl Pts',(-1.48749023769102,-0.272583545355803,
-2.0598564697024));
#366862=CARTESIAN_POINT('Ctrl Pts',(-1.44037126809873,-0.460737270908912,
-2.04940348494945));
#366863=CARTESIAN_POINT('Ctrl Pts',(-1.27571175718277,-0.813199170429424,
-2.02982226830943));
#366864=CARTESIAN_POINT('Ctrl Pts',(-1.15813565951456,-0.973381389779296,
-2.02034912262653));
#366865=CARTESIAN_POINT('Ctrl Pts',(-0.86744354656846,-1.23954180631063,
-1.99896984691782));
#366866=CARTESIAN_POINT('Ctrl Pts',(-0.697073007651896,-1.34276191574104,
-1.98790566528041));
#366867=CARTESIAN_POINT('Ctrl Pts',(-0.347459626841339,-1.46961511417048,
-1.9675611836971));
#366868=CARTESIAN_POINT('Ctrl Pts',(-0.174323197795173,-1.5,-1.95838712876442));
#366869=CARTESIAN_POINT('Ctrl Pts',(1.5855372570428E-14,-1.5,-1.95));
#366870=CARTESIAN_POINT('Ctrl Pts',(-2.20864992961377E-13,-1.5,-1.88750000000001));
#366871=CARTESIAN_POINT('Ctrl Pts',(-0.0368623918547273,-1.5,-1.88927354265503));
#366872=CARTESIAN_POINT('Ctrl Pts',(-0.0737639135159791,-1.49864120837783,
-1.89108671215548));
#366873=CARTESIAN_POINT('Ctrl Pts',(-0.302085379330646,-1.48175565959102,
-1.90254087682316));
#366874=CARTESIAN_POINT('Ctrl Pts',(-0.489025568623064,-1.43097495551993,
-1.91294561598711));
#366875=CARTESIAN_POINT('Ctrl Pts',(-0.840337210031122,-1.25842118658735,
-1.93464126546327));
#366876=CARTESIAN_POINT('Ctrl Pts',(-1.00006721705373,-1.13563545664226,
-1.94573699372998));
#366877=CARTESIAN_POINT('Ctrl Pts',(-1.25712218842694,-0.840510858843861,
-1.96630246230095));
#366878=CARTESIAN_POINT('Ctrl Pts',(-1.35420304308014,-0.673014628741669,
-1.97511029840325));
#366879=CARTESIAN_POINT('Ctrl Pts',(-1.48076488748363,-0.308291742248993,
-1.99537268098618));
#366880=CARTESIAN_POINT('Ctrl Pts',(-1.50819421076492,-0.114223606293866,
-2.0061542440948));
#366881=CARTESIAN_POINT('Ctrl Pts',(-1.48732444675329,0.278204630505327,
-2.02795581280586));
#366882=CARTESIAN_POINT('Ctrl Pts',(-1.43739269292505,0.472711044720166,
-2.03876172470669));
#366883=CARTESIAN_POINT('Ctrl Pts',(-1.26845143123851,0.822853866465687,
-2.05821410369255));
#366884=CARTESIAN_POINT('Ctrl Pts',(-1.15421015875391,0.976665383468958,
-2.06743096516376));
#366885=CARTESIAN_POINT('Ctrl Pts',(-0.869565726160317,1.23791656925302,
-2.08838290419509));
#366886=CARTESIAN_POINT('Ctrl Pts',(-0.700167326634511,1.34102411927311,
-2.09939718710397));
#366887=CARTESIAN_POINT('Ctrl Pts',(-0.328270138095944,1.47718926068047,
-2.12107246396919));
#366888=CARTESIAN_POINT('Ctrl Pts',(-0.129042021872983,1.50770184074051,
-2.13107752280734));
#366889=CARTESIAN_POINT('Ctrl Pts',(0.261537194048148,1.48938177747693,
-2.15037816474122));
#366890=CARTESIAN_POINT('Ctrl Pts',(0.449289004131965,1.44387580850969,
-2.16067543260915));
#366891=CARTESIAN_POINT('Ctrl Pts',(0.804299308327845,1.28166496038003,
-2.18226173072602));
#366892=CARTESIAN_POINT('Ctrl Pts',(0.966986956683662,1.16383327810383,
-2.19336214614247));
#366893=CARTESIAN_POINT('Ctrl Pts',(1.2328126962066,0.875999571507584,-2.21414707373718));
#366894=CARTESIAN_POINT('Ctrl Pts',(1.33510265331455,0.710423042788745,
-2.22303205317841));
#366895=CARTESIAN_POINT('Ctrl Pts',(1.47167733932044,0.348815694246995,
-2.24312135031962));
#366896=CARTESIAN_POINT('Ctrl Pts',(1.50436781701598,0.156109912924603,
-2.25382722705976));
#366897=CARTESIAN_POINT('Ctrl Pts',(1.49456606947089,-0.236252467601609,
-2.27562513708899));
#366898=CARTESIAN_POINT('Ctrl Pts',(1.45011794280952,-0.432111481359206,
-2.28650619340886));
#366899=CARTESIAN_POINT('Ctrl Pts',(1.29101128548853,-0.787023085734208,
-2.30622350476302));
#366900=CARTESIAN_POINT('Ctrl Pts',(1.18103363775905,-0.944079505943259,
-2.31523525666381));
#366901=CARTESIAN_POINT('Ctrl Pts',(0.9040655830077,-1.21286160675192,-2.33602705787802));
#366902=CARTESIAN_POINT('Ctrl Pts',(0.738133667625035,-1.32042497463635,
-2.34699833220925));
#366903=CARTESIAN_POINT('Ctrl Pts',(0.379175592598109,-1.46375304244289,
-2.36825004586315));
#366904=CARTESIAN_POINT('Ctrl Pts',(0.190390033540378,-1.5,-2.37833985524037));
#366905=CARTESIAN_POINT('Ctrl Pts',(9.36750677027476E-16,-1.5,-2.3875));
#366906=CARTESIAN_POINT('Origin',(0.,2.16840434497101E-16,-9.7));
#366907=CARTESIAN_POINT('',(2.53043732100507E-14,-1.5,-2.94999999999999));
#366908=CARTESIAN_POINT('',(2.5321850413124E-14,-1.5,-2.8875));
#366909=CARTESIAN_POINT('',(-1.83697019872103E-16,-1.5,-9.7));
#366910=CARTESIAN_POINT('Ctrl Pts',(5.07924434399736E-14,-1.5,-2.94999999999999));
#366911=CARTESIAN_POINT('Ctrl Pts',(0.0744213382181849,-1.5,-2.94641940169552));
#366912=CARTESIAN_POINT('Ctrl Pts',(0.148892353057916,-1.4944622271461,
-2.94268258629972));
#366913=CARTESIAN_POINT('Ctrl Pts',(0.420969831647567,-1.45359546756537,
-2.92845706474157));
#366914=CARTESIAN_POINT('Ctrl Pts',(0.611154960021442,-1.3844238016528,
-2.91738534332213));
#366915=CARTESIAN_POINT('Ctrl Pts',(0.946549473523585,-1.17948246468226,
-2.89555585235168));
#366916=CARTESIAN_POINT('Ctrl Pts',(1.09011167306719,-1.04824072625686,
-2.88500310896054));
#366917=CARTESIAN_POINT('Ctrl Pts',(1.3211576247791,-0.736636363828259,
-2.86523122869174));
#366918=CARTESIAN_POINT('Ctrl Pts',(1.40568797429451,-0.55869580933379,
-2.85603865607406));
#366919=CARTESIAN_POINT('Ctrl Pts',(1.50252275599202,-0.177726380825034,
-2.83487368782357));
#366920=CARTESIAN_POINT('Ctrl Pts',(1.51283851044406,0.0218258598492461,
-2.82378745223056));
#366921=CARTESIAN_POINT('Ctrl Pts',(1.4564811902691,0.406185454812701,-2.80243414139925));
#366922=CARTESIAN_POINT('Ctrl Pts',(1.39315447369828,0.587696925737235,
-2.79236992793051));
#366923=CARTESIAN_POINT('Ctrl Pts',(1.19789975854395,0.924423411128237,
-2.77362221758452));
#366924=CARTESIAN_POINT('Ctrl Pts',(1.06499159643924,1.0748433825963,-2.76304933811302));
#366925=CARTESIAN_POINT('Ctrl Pts',(0.750911055879611,1.31314905744491,
-2.74131852898062));
#366926=CARTESIAN_POINT('Ctrl Pts',(0.573530775952319,1.39974863451254,
-2.73037877247611));
#366927=CARTESIAN_POINT('Ctrl Pts',(0.200625988877396,1.49864904366988,
-2.70969014895509));
#366928=CARTESIAN_POINT('Ctrl Pts',(0.00915798051034495,1.51198819321672,
-2.70077361890983));
#366929=CARTESIAN_POINT('Ctrl Pts',(-0.377196203055984,1.46536349575517,
-2.68089001410107));
#366930=CARTESIAN_POINT('Ctrl Pts',(-0.567955146829013,1.40248926947439,
-2.66996561385402));
#366931=CARTESIAN_POINT('Ctrl Pts',(-0.908947172797603,1.20879214084764,
-2.64817915156013));
#366932=CARTESIAN_POINT('Ctrl Pts',(-1.05700900098552,1.08171642547661,
-2.63752564254751));
#366933=CARTESIAN_POINT('Ctrl Pts',(-1.29692998600533,0.778114569031601,
-2.61754905387248));
#366934=CARTESIAN_POINT('Ctrl Pts',(-1.38642500099297,0.604416767699619,
-2.6085787093166));
#366935=CARTESIAN_POINT('Ctrl Pts',(-1.49583808741873,0.227799377384436,
-2.58765552096576));
#366936=CARTESIAN_POINT('Ctrl Pts',(-1.51282229632946,0.0280229106174455,
-2.57655682836759));
#366937=CARTESIAN_POINT('Ctrl Pts',(-1.46886197321051,-0.359103764703532,
-2.55504979084976));
#366938=CARTESIAN_POINT('Ctrl Pts',(-1.41121851423137,-0.543135540070848,
-2.54482580332935));
#366939=CARTESIAN_POINT('Ctrl Pts',(-1.2262879171076,-0.886416245393696,
-2.52575465303364));
#366940=CARTESIAN_POINT('Ctrl Pts',(-1.0981320239873,-1.0409918706452,-2.51558412745327));
#366941=CARTESIAN_POINT('Ctrl Pts',(-0.791055940191536,-1.28945370009369,
-2.49390820499849));
#366942=CARTESIAN_POINT('Ctrl Pts',(-0.615872233743788,-1.38172540247317,
-2.48291657214834));
#366943=CARTESIAN_POINT('Ctrl Pts',(-0.288782841940459,-1.47907824222109,
-2.46447523089923));
#366944=CARTESIAN_POINT('Ctrl Pts',(-0.144663401257926,-1.5,-2.45696012113819));
#366945=CARTESIAN_POINT('Ctrl Pts',(2.20655697018894E-13,-1.5,-2.44999999999999));
#366946=CARTESIAN_POINT('Ctrl Pts',(-1.73472347597681E-16,-1.5,-2.3875));
#366947=CARTESIAN_POINT('Ctrl Pts',(-0.00820824151007254,-1.5,-2.38789491920379));
#366948=CARTESIAN_POINT('Ctrl Pts',(-0.0164192878007734,-1.49993262484668,
-2.38829184488469));
#366949=CARTESIAN_POINT('Ctrl Pts',(-0.215498919763185,-1.49666298850653,
-2.397960891375));
#366950=CARTESIAN_POINT('Ctrl Pts',(-0.403990759766078,-1.4571230805755,
-2.40812804003134));
#366951=CARTESIAN_POINT('Ctrl Pts',(-0.762822106339094,-1.30667918707593,
-2.42957131828446));
#366952=CARTESIAN_POINT('Ctrl Pts',(-0.928672474770597,-1.19452158185493,
-2.44066628688997));
#366953=CARTESIAN_POINT('Ctrl Pts',(-1.20432184412241,-0.915064031477631,
-2.46169118308911));
#366954=CARTESIAN_POINT('Ctrl Pts',(-1.31255322090007,-0.751619157500383,
-2.47074338013888));
#366955=CARTESIAN_POINT('Ctrl Pts',(-1.46026970433536,-0.393568310786017,
-2.49063509384523));
#366956=CARTESIAN_POINT('Ctrl Pts',(-1.49874761594601,-0.202541870011464,
-2.50124767388826));
#366957=CARTESIAN_POINT('Ctrl Pts',(-1.5012409378723,0.191236548850281,
-2.52312425271391));
#366958=CARTESIAN_POINT('Ctrl Pts',(-1.46220428198257,0.390220278258254,
-2.53417890434769));
#366959=CARTESIAN_POINT('Ctrl Pts',(-1.31209345675809,0.751436486119095,
-2.55424647145107));
#366960=CARTESIAN_POINT('Ctrl Pts',(-1.20624636216264,0.911713663222863,
-2.56312315770868));
#366961=CARTESIAN_POINT('Ctrl Pts',(-0.936749160411386,1.18771357230621,
-2.58375601201463));
#366962=CARTESIAN_POINT('Ctrl Pts',(-0.774277755585629,1.29948057143874,
-2.59467755998873));
#366963=CARTESIAN_POINT('Ctrl Pts',(-0.412519795634319,1.45579132507715,
-2.61642461333086));
#366964=CARTESIAN_POINT('Ctrl Pts',(-0.216181858431131,1.49759565573891,
-2.62703215814616));
#366965=CARTESIAN_POINT('Ctrl Pts',(0.172891068474,1.50210410915275,-2.6458766728868));
#366966=CARTESIAN_POINT('Ctrl Pts',(0.361923021625222,1.46808371059299,
-2.65579959309142));
#366967=CARTESIAN_POINT('Ctrl Pts',(0.724037963046113,1.32847515826504,
-2.67709987167611));
#366968=CARTESIAN_POINT('Ctrl Pts',(0.892625190355791,1.22159778381432,
-2.68817984438883));
#366969=CARTESIAN_POINT('Ctrl Pts',(1.17722185853026,0.949977003646278,
-2.70941752964192));
#366970=CARTESIAN_POINT('Ctrl Pts',(1.29097321174977,0.788469814882173,
-2.71869612139544));
#366971=CARTESIAN_POINT('Ctrl Pts',(1.44878182832975,0.433721693734626,
-2.73840435034808));
#366972=CARTESIAN_POINT('Ctrl Pts',(1.49243191904509,0.244361021410866,
-2.7489243876994));
#366973=CARTESIAN_POINT('Ctrl Pts',(1.50603213313662,-0.148072780988375,
-2.77072626561047));
#366974=CARTESIAN_POINT('Ctrl Pts',(1.47286098589617,-0.347496303598292,
-2.78180535019991));
#366975=CARTESIAN_POINT('Ctrl Pts',(1.33347477910016,-0.712958631639371,
-2.80210881286886));
#366976=CARTESIAN_POINT('Ctrl Pts',(1.23199853818993,-0.876725265436446,
-2.81091225562337));
#366977=CARTESIAN_POINT('Ctrl Pts',(0.970426193171564,-1.16026762329887,
-2.83137333754807));
#366978=CARTESIAN_POINT('Ctrl Pts',(0.81171179415968,-1.27634746178067,
-2.84223392758871));
#366979=CARTESIAN_POINT('Ctrl Pts',(0.455182813765921,-1.4430263855456,
-2.86401740626031));
#366980=CARTESIAN_POINT('Ctrl Pts',(0.260122768660399,-1.49059615477631,
-2.87472361953476));
#366981=CARTESIAN_POINT('Ctrl Pts',(0.0409548134732333,-1.49958097346455,
-2.88551792099208));
#366982=CARTESIAN_POINT('Ctrl Pts',(0.0204702234117732,-1.5,-2.88651512591691));
#366983=CARTESIAN_POINT('Ctrl Pts',(5.08273978461202E-14,-1.5,-2.8875));
#366984=CARTESIAN_POINT('Origin',(0.,2.16840434497101E-16,-9.7));
#366985=CARTESIAN_POINT('',(-2.58985031534265E-15,-1.5,-3.45));
#366986=CARTESIAN_POINT('',(1.01771113999419E-13,-1.5,-3.38749999999999));
#366987=CARTESIAN_POINT('',(-1.83697019872103E-16,-1.5,-9.7));
#366988=CARTESIAN_POINT('Ctrl Pts',(-1.12757025938492E-15,-1.5,-3.45));
#366989=CARTESIAN_POINT('Ctrl Pts',(0.104274349025483,-1.5,-3.44498309804338));
#366990=CARTESIAN_POINT('Ctrl Pts',(0.20848744942163,-1.48912928790673,
-3.43966717868797));
#366991=CARTESIAN_POINT('Ctrl Pts',(0.505825920466392,-1.42611936646804,
-3.42361119923427));
#366992=CARTESIAN_POINT('Ctrl Pts',(0.69051093996075,-1.34642509850937,
-3.41251180742539));
#366993=CARTESIAN_POINT('Ctrl Pts',(1.01175618937721,-1.12386701912129,
-3.39087371928463));
#366994=CARTESIAN_POINT('Ctrl Pts',(1.14694586773164,-0.985527209922369,
-3.38052663037441));
#366995=CARTESIAN_POINT('Ctrl Pts',(1.36175721992224,-0.659604114449861,
-3.36113809505471));
#366996=CARTESIAN_POINT('Ctrl Pts',(1.43705865734217,-0.473655318003814,
-3.35131418433351));
#366997=CARTESIAN_POINT('Ctrl Pts',(1.51044358412492,-0.0851242809337696,
-3.32972912671851));
#366998=CARTESIAN_POINT('Ctrl Pts',(1.50858050856705,0.113453209714267,
-3.31869704390473));
#366999=CARTESIAN_POINT('Ctrl Pts',(1.42970448816059,0.491961281274415,
-3.29766881770694));
#367000=CARTESIAN_POINT('Ctrl Pts',(1.35599837329553,0.668823945725757,
-3.28832872588338));
#367001=CARTESIAN_POINT('Ctrl Pts',(1.1416063557085,0.993118075303684,-3.26900561486183));
#367002=CARTESIAN_POINT('Ctrl Pts',(1.00004772648413,1.13553089559032,-3.25823896046313));
#367003=CARTESIAN_POINT('Ctrl Pts',(0.673362868540264,1.35439206440055,
-3.23644185099557));
#367004=CARTESIAN_POINT('Ctrl Pts',(0.492330483354827,1.43018065835238,
-3.22562668758144));
#367005=CARTESIAN_POINT('Ctrl Pts',(0.114322046291612,1.50784274836868,
-3.20528246789535));
#367006=CARTESIAN_POINT('Ctrl Pts',(-0.0788414997936811,1.51011337096137,
-3.19648766354368));
#367007=CARTESIAN_POINT('Ctrl Pts',(-0.463828289110963,1.44040839658907,
-3.17602872871833));
#367008=CARTESIAN_POINT('Ctrl Pts',(-0.651319540490476,1.36590000784234,
-3.16493837421526));
#367009=CARTESIAN_POINT('Ctrl Pts',(-0.97971687249228,1.15199150335434,
-3.14319644731011));
#367010=CARTESIAN_POINT('Ctrl Pts',(-1.11911517725929,1.01711848626125,
-3.13274317054793));
#367011=CARTESIAN_POINT('Ctrl Pts',(-1.34204941391269,0.698308531425868,
-3.11316141000722));
#367012=CARTESIAN_POINT('Ctrl Pts',(-1.42199632483557,0.516404899013764,
-3.10368916105629));
#367013=CARTESIAN_POINT('Ctrl Pts',(-1.50718522169627,0.131588669849777,
-3.08231048165829));
#367014=CARTESIAN_POINT('Ctrl Pts',(-1.51140847386047,-0.0675679828713596,
-3.07124622317378));
#367015=CARTESIAN_POINT('Ctrl Pts',(-1.44378208131313,-0.449055345529514,
-3.05005248080388));
#367016=CARTESIAN_POINT('Ctrl Pts',(-1.3753031265635,-0.628220357727625,
-3.04038540370243));
#367017=CARTESIAN_POINT('Ctrl Pts',(-1.17054174751803,-0.958837005905384,
-3.02135002147708));
#367018=CARTESIAN_POINT('Ctrl Pts',(-1.03329182319454,-1.10535941348711,
-3.01067651453694));
#367019=CARTESIAN_POINT('Ctrl Pts',(-0.712824034722463,-1.33412698629862,
-2.98890334607488));
#367020=CARTESIAN_POINT('Ctrl Pts',(-0.533556107643747,-1.41539361172663,
-2.97802090764999));
#367021=CARTESIAN_POINT('Ctrl Pts',(-0.230841399415094,-1.48666354507819,
-2.96147681908883));
#367022=CARTESIAN_POINT('Ctrl Pts',(-0.115498535002616,-1.5,-2.95555692585623));
#367023=CARTESIAN_POINT('Ctrl Pts',(5.20763987488237E-14,-1.5,-2.94999999999999));
#367024=CARTESIAN_POINT('Ctrl Pts',(5.19029264012261E-14,-1.5,-2.8875));
#367025=CARTESIAN_POINT('Ctrl Pts',(-0.169191228008341,-1.5,-2.89564021675293));
#367026=CARTESIAN_POINT('Ctrl Pts',(-0.337325653434019,-1.47137896582402,
-2.90452461679501));
#367027=CARTESIAN_POINT('Ctrl Pts',(-0.683215605809903,-1.34983600112939,
-2.9245424483516));
#367028=CARTESIAN_POINT('Ctrl Pts',(-0.854465761761834,-1.24849108906284,
-2.93559686176769));
#367029=CARTESIAN_POINT('Ctrl Pts',(-1.14825257380326,-0.985142589364441,
-2.95704692245513));
#367030=CARTESIAN_POINT('Ctrl Pts',(-1.26779153793086,-0.825636253928343,
-2.96663131922621));
#367031=CARTESIAN_POINT('Ctrl Pts',(-1.43592311619488,-0.474346778137693,
-2.98614740121458));
#367032=CARTESIAN_POINT('Ctrl Pts',(-1.48478620139945,-0.286827721696611,
-2.99656512657242));
#367033=CARTESIAN_POINT('Ctrl Pts',(-1.5096423051372,0.103920533796697,
-3.01827336298871));
#367034=CARTESIAN_POINT('Ctrl Pts',(-1.48244575409252,0.303621637952862,
-3.02936786877517));
#367035=CARTESIAN_POINT('Ctrl Pts',(-1.35404742260803,0.673295757271683,
-3.04990531984843));
#367036=CARTESIAN_POINT('Ctrl Pts',(-1.25699504700908,0.84067543846082,
-3.05870822644941));
#367037=CARTESIAN_POINT('Ctrl Pts',(-1.00344486967301,1.13173871654929,
-3.07899225610226));
#367038=CARTESIAN_POINT('Ctrl Pts',(-0.848615659840483,1.25202804359538,
-3.08978285012926));
#367039=CARTESIAN_POINT('Ctrl Pts',(-0.497638394565766,1.42894587829609,
-3.11158363597532));
#367040=CARTESIAN_POINT('Ctrl Pts',(-0.304037264242564,1.4822663644638,
-3.12237939931671));
#367041=CARTESIAN_POINT('Ctrl Pts',(0.0837578803978027,1.5096490567957,
-3.14179783225498));
#367042=CARTESIAN_POINT('Ctrl Pts',(0.274001552302664,1.48694279115938,
-3.15104560607727));
#367043=CARTESIAN_POINT('Ctrl Pts',(0.642224686814734,1.36972878103256,
-3.17201769462238));
#367044=CARTESIAN_POINT('Ctrl Pts',(0.815935095358566,1.27391432361466,
-3.18303685325625));
#367045=CARTESIAN_POINT('Ctrl Pts',(1.11873386344195,1.01891457967269,-3.2046885919988));
#367046=CARTESIAN_POINT('Ctrl Pts',(1.24407365753746,0.861395430350653,
-3.21464469831386));
#367047=CARTESIAN_POINT('Ctrl Pts',(1.4222980773209,0.513567189131623,-3.23396848949269));
#367048=CARTESIAN_POINT('Ctrl Pts',(1.47617461089027,0.327978621958125,
-3.24427896544678));
#367049=CARTESIAN_POINT('Ctrl Pts',(1.51191594848997,-0.0608250166043019,
-3.26587916758913));
#367050=CARTESIAN_POINT('Ctrl Pts',(1.49052695146521,-0.260630887484796,
-3.27697949374916));
#367051=CARTESIAN_POINT('Ctrl Pts',(1.37288845797995,-0.634294366679431,
-3.29773857592664));
#367052=CARTESIAN_POINT('Ctrl Pts',(1.28013121590112,-0.805241597497524,
-3.3066108136445));
#367053=CARTESIAN_POINT('Ctrl Pts',(1.03434044541333,-1.10348098533582,
-3.32672085504324));
#367054=CARTESIAN_POINT('Ctrl Pts',(0.883340843740472,-1.22769128682558,
-3.33743611291852));
#367055=CARTESIAN_POINT('Ctrl Pts',(0.537967582982333,-1.41426044671337,
-3.35923536833787));
#367056=CARTESIAN_POINT('Ctrl Pts',(0.345930252409157,-1.47305589754972,
-3.37010797568062));
#367057=CARTESIAN_POINT('Ctrl Pts',(0.0987335442719462,-1.49756561069993,
-3.38268205821138));
#367058=CARTESIAN_POINT('Ctrl Pts',(0.0493410623683693,-1.5,-3.38512607702997));
#367059=CARTESIAN_POINT('Ctrl Pts',(2.0372592501871E-13,-1.5,-3.38749999999999));
#367060=CARTESIAN_POINT('Origin',(0.,2.16840434497101E-16,-9.7));
#367061=CARTESIAN_POINT('',(-9.36276598708176E-14,-1.5,-3.95000000000001));
#367062=CARTESIAN_POINT('',(1.68390526155976E-14,-1.5,-3.8875));
#367063=CARTESIAN_POINT('',(-1.83697019872103E-16,-1.5,-9.7));
#367064=CARTESIAN_POINT('Ctrl Pts',(-1.88182802673964E-13,-1.5,-3.95000000000001));
#367065=CARTESIAN_POINT('Ctrl Pts',(0.135231780044054,-1.50000000000002,
-3.94349365794904));
#367066=CARTESIAN_POINT('Ctrl Pts',(0.270091652890841,-1.48171749714704,
-3.93649736198997));
#367067=CARTESIAN_POINT('Ctrl Pts',(0.591701203054428,-1.39250952169454,
-3.91854591597511));
#367068=CARTESIAN_POINT('Ctrl Pts',(0.770114601928998,-1.30234851268668,
-3.90745752484706));
#367069=CARTESIAN_POINT('Ctrl Pts',(1.07578737076159,-1.06254064857899,
-3.88608950734106));
#367070=CARTESIAN_POINT('Ctrl Pts',(1.20195921834089,-0.917403757532496,
-3.87598748118721));
#367071=CARTESIAN_POINT('Ctrl Pts',(1.39726514048798,-0.580627582297759,
-3.85723592687019));
#367072=CARTESIAN_POINT('Ctrl Pts',(1.46184639615906,-0.39057002758959,
-3.84669833486606));
#367073=CARTESIAN_POINT('Ctrl Pts',(1.51269818200308,0.000576252643117829,
-3.82496798596425));
#367074=CARTESIAN_POINT('Ctrl Pts',(1.49973660386404,0.197615433066233,
-3.81402136482963));
#367075=CARTESIAN_POINT('Ctrl Pts',(1.40029435044894,0.570401185793709,
-3.79331104523366));
#367076=CARTESIAN_POINT('Ctrl Pts',(1.31677448459466,0.743154425879645,
-3.78437683009855));
#367077=CARTESIAN_POINT('Ctrl Pts',(1.0844223927983,1.05526976744912,-3.76452791427061));
#367078=CARTESIAN_POINT('Ctrl Pts',(0.935098847945181,1.18959576866844,
-3.75361230405752));
#367079=CARTESIAN_POINT('Ctrl Pts',(0.597548595218118,1.38936178618908,
-3.73182285390887));
#367080=CARTESIAN_POINT('Ctrl Pts',(0.413639769565851,1.45475338707051,
-3.72115810305133));
#367081=CARTESIAN_POINT('Ctrl Pts',(0.0310519172398163,1.51210510409059,
-3.70115773317334));
#367082=CARTESIAN_POINT('Ctrl Pts',(-0.163986821645253,1.50350863135109,
-3.69220764234691));
#367083=CARTESIAN_POINT('Ctrl Pts',(-0.545135657673647,1.41148227548547,
-3.67131332276045));
#367084=CARTESIAN_POINT('Ctrl Pts',(-0.727040565581374,1.32697370289724,
-3.66021395844849));
#367085=CARTESIAN_POINT('Ctrl Pts',(-1.04131881414212,1.09644554015147,
-3.63868967908831));
#367086=CARTESIAN_POINT('Ctrl Pts',(-1.17245071122195,0.954944868213632,
-3.62845001852794));
#367087=CARTESIAN_POINT('Ctrl Pts',(-1.37948364167474,0.622305661029978,
-3.60924916403995));
#367088=CARTESIAN_POINT('Ctrl Pts',(-1.45027427968896,0.432417245938569,
-3.59902318032989));
#367089=CARTESIAN_POINT('Ctrl Pts',(-1.5122245890554,0.0404690730220717,
-3.57724828183453));
#367090=CARTESIAN_POINT('Ctrl Pts',(-1.50455808839533,-0.157382516188904,
-3.56625652687837));
#367091=CARTESIAN_POINT('Ctrl Pts',(-1.41494260791851,-0.532945936441863,
-3.54539189241987));
#367092=CARTESIAN_POINT('Ctrl Pts',(-1.33615682591316,-0.70764727509372,
-3.53629567317408));
#367093=CARTESIAN_POINT('Ctrl Pts',(-1.11244224847975,-1.02568553090108,
-3.51669780455419));
#367094=CARTESIAN_POINT('Ctrl Pts',(-0.96680680985833,-1.16396852008114,
-3.50584972210266));
#367095=CARTESIAN_POINT('Ctrl Pts',(-0.634359896426993,-1.37301589271101,
-3.48404799106065));
#367096=CARTESIAN_POINT('Ctrl Pts',(-0.451765861327982,-1.44343532132478,
-3.47330683621165));
#367097=CARTESIAN_POINT('Ctrl Pts',(-0.174510362890852,-1.49238980262838,
-3.45860752812069));
#367098=CARTESIAN_POINT('Ctrl Pts',(-0.0872440292034471,-1.5,-3.45419753031215));
#367099=CARTESIAN_POINT('Ctrl Pts',(8.19989359106401E-22,-1.5,-3.45));
#367100=CARTESIAN_POINT('Ctrl Pts',(2.05807593189888E-13,-1.5,-3.3875));
#367101=CARTESIAN_POINT('Ctrl Pts',(-0.140029260838789,-1.5,-3.3942371609533));
#367102=CARTESIAN_POINT('Ctrl Pts',(-0.279591813351883,-1.48039732319827,
-3.40149638619188));
#367103=CARTESIAN_POINT('Ctrl Pts',(-0.602949332181216,-1.38738786328683,
-3.41963752817892));
#367104=CARTESIAN_POINT('Ctrl Pts',(-0.778825446680177,-1.29684993574237,
-3.43061431411487));
#367105=CARTESIAN_POINT('Ctrl Pts',(-1.08810807736369,-1.05146177325118,
-3.45231101946858));
#367106=CARTESIAN_POINT('Ctrl Pts',(-1.21772387864441,-0.898137641636366,
-3.46260346435354));
#367107=CARTESIAN_POINT('Ctrl Pts',(-1.40584314148586,-0.556838944498058,
-3.48156450308345));
#367108=CARTESIAN_POINT('Ctrl Pts',(-1.46522861883794,-0.373558785243038,
-3.49174673415317));
#367109=CARTESIAN_POINT('Ctrl Pts',(-1.51300181436644,0.0127280448211617,
-3.51320711360118));
#367110=CARTESIAN_POINT('Ctrl Pts',(-1.49806689799126,0.212458701953946,
-3.52430326121967));
#367111=CARTESIAN_POINT('Ctrl Pts',(-1.39250216908306,0.590429007327594,
-3.5453016115182));
#367112=CARTESIAN_POINT('Ctrl Pts',(-1.30452860073399,0.7654203759335,-3.55433084887599));
#367113=CARTESIAN_POINT('Ctrl Pts',(-1.06733578123864,1.07149557017,-3.57424488245357));
#367114=CARTESIAN_POINT('Ctrl Pts',(-0.920650162759634,1.19987330666118,
-3.58486834579903));
#367115=CARTESIAN_POINT('Ctrl Pts',(-0.580061762350196,1.39780315213869,
-3.60675296411723));
#367116=CARTESIAN_POINT('Ctrl Pts',(-0.387913345294798,1.46282819114682,
-3.61780396022673));
#367117=CARTESIAN_POINT('Ctrl Pts',(0.000164181943814248,1.51202666694766,
-3.63784197328934));
#367118=CARTESIAN_POINT('Ctrl Pts',(0.191793026215588,1.49981555817854,
-3.64673276966012));
#367119=CARTESIAN_POINT('Ctrl Pts',(0.565239014991216,1.40310163880413,
-3.6673866959328));
#367120=CARTESIAN_POINT('Ctrl Pts',(0.743025460494158,1.31760999323215,
-3.67831521821281));
#367121=CARTESIAN_POINT('Ctrl Pts',(1.05846051210802,1.08127713162049,-3.700056395921));
#367122=CARTESIAN_POINT('Ctrl Pts',(1.19228276290732,0.931658386013542,
-3.71065099823141));
#367123=CARTESIAN_POINT('Ctrl Pts',(1.38952397062882,0.596198198774931,
-3.72945910879692));
#367124=CARTESIAN_POINT('Ctrl Pts',(1.45392729091196,0.415183262171618,
-3.73943426321269));
#367125=CARTESIAN_POINT('Ctrl Pts',(1.51265330275542,0.0314178396428978,
-3.76075456446429));
#367126=CARTESIAN_POINT('Ctrl Pts',(1.50361722287959,-0.168066484823331,
-3.77183702693463));
#367127=CARTESIAN_POINT('Ctrl Pts',(1.40921555701814,-0.549854287798661,
-3.79304746043326));
#367128=CARTESIAN_POINT('Ctrl Pts',(1.32564340431154,-0.728620246368115,
-3.80229273659395));
#367129=CARTESIAN_POINT('Ctrl Pts',(1.0963004264774,-1.04174588564233,-3.82202494018401));
#367130=CARTESIAN_POINT('Ctrl Pts',(0.953608685826855,-1.17376398194826,
-3.83255736909882));
#367131=CARTESIAN_POINT('Ctrl Pts',(0.619670176697447,-1.38061497341427,
-3.85436985398443));
#367132=CARTESIAN_POINT('Ctrl Pts',(0.430041132846712,-1.45091992434412,
-3.86544630091415));
#367133=CARTESIAN_POINT('Ctrl Pts',(0.155211736207756,-1.4939816801484,
-3.87986519630849));
#367134=CARTESIAN_POINT('Ctrl Pts',(0.0775835479173541,-1.5,-3.88376725981044));
#367135=CARTESIAN_POINT('Ctrl Pts',(3.38618022510672E-14,-1.5,-3.8875));
#367136=CARTESIAN_POINT('Origin',(0.,2.16840434497101E-16,-9.7));
#367137=CARTESIAN_POINT('',(-8.50234748894081E-14,-1.5,-4.45000000000001));
#367138=CARTESIAN_POINT('',(-8.67872971602131E-15,-1.5,-4.38750000000001));
#367139=CARTESIAN_POINT('',(-1.83697019872103E-16,-1.5,-9.7));
#367140=CARTESIAN_POINT('Ctrl Pts',(-1.71841707530263E-13,-1.5,-4.45));
#367141=CARTESIAN_POINT('Ctrl Pts',(0.166531914299599,-1.50000000000002,
-4.44198772953754));
#367142=CARTESIAN_POINT('Ctrl Pts',(0.332117043998036,-1.47227294080272,
-4.43325081518161));
#367143=CARTESIAN_POINT('Ctrl Pts',(0.675932825307817,-1.35345201347111,
-4.41340838937594));
#367144=CARTESIAN_POINT('Ctrl Pts',(0.847457115836254,-1.25320965332295,
-4.40237141309606));
#367145=CARTESIAN_POINT('Ctrl Pts',(1.13691812902165,-0.996746171624119,
-4.38132072800311));
#367146=CARTESIAN_POINT('Ctrl Pts',(1.25384871279216,-0.844940101725643,
-4.37194111676252));
#367147=CARTESIAN_POINT('Ctrl Pts',(1.42888981888619,-0.497816171315387,
-4.35265645396195));
#367148=CARTESIAN_POINT('Ctrl Pts',(1.48221684129832,-0.304232262081196,
-4.34190179233783));
#367149=CARTESIAN_POINT('Ctrl Pts',(1.5099890379016,0.088078041336461,-4.32010677548129));
#367150=CARTESIAN_POINT('Ctrl Pts',(1.48586312548998,0.28292349174859,-4.30928202823617));
#367151=CARTESIAN_POINT('Ctrl Pts',(1.36554003428657,0.649551699860725,
-4.28891379445217));
#367152=CARTESIAN_POINT('Ctrl Pts',(1.27164877018827,0.818245178988515,
-4.28011986389887));
#367153=CARTESIAN_POINT('Ctrl Pts',(1.02002676734894,1.117806391016,-4.25969254986422));
#367154=CARTESIAN_POINT('Ctrl Pts',(0.862190388629051,1.24360767462841,
-4.24860416345206));
#367155=CARTESIAN_POINT('Ctrl Pts',(0.513302369906706,1.42249008150699,
-4.22684932507823));
#367156=CARTESIAN_POINT('Ctrl Pts',(0.326934852408628,1.47651275693882,
-4.21638208383882));
#367157=CARTESIAN_POINT('Ctrl Pts',(-0.0603370709084466,1.51162109260476,
-4.19677422319448));
#367158=CARTESIAN_POINT('Ctrl Pts',(-0.257685646017792,1.4907219683773,
-4.1873443704748));
#367159=CARTESIAN_POINT('Ctrl Pts',(-0.633891516278368,1.37373098968563,
-4.16599440769455));
#367160=CARTESIAN_POINT('Ctrl Pts',(-0.808949118249591,1.27849692188573,
-4.15492655412052));
#367161=CARTESIAN_POINT('Ctrl Pts',(-1.10662584179872,1.03031748334567,
-4.13371070278836));
#367162=CARTESIAN_POINT('Ctrl Pts',(-1.22817582784007,0.881883674541403,
-4.1239935374745));
#367163=CARTESIAN_POINT('Ctrl Pts',(-1.41350113107434,0.539952906895013,
-4.10499738371637));
#367164=CARTESIAN_POINT('Ctrl Pts',(-1.4725343002586,0.3480690531609,-4.09433716962003));
#367165=CARTESIAN_POINT('Ctrl Pts',(-1.51199443291843,-0.0437630945133086,
-4.07256871697146));
#367166=CARTESIAN_POINT('Ctrl Pts',(-1.49350167119399,-0.239798016752632,
-4.06167788795817));
#367167=CARTESIAN_POINT('Ctrl Pts',(-1.3837481189278,-0.609585871565706,
-4.04113411824633));
#367168=CARTESIAN_POINT('Ctrl Pts',(-1.29516287259196,-0.780322278400673,
-4.03230460058346));
#367169=CARTESIAN_POINT('Ctrl Pts',(-1.05268606270819,-1.08721665840631,
-4.01211358573953));
#367170=CARTESIAN_POINT('Ctrl Pts',(-0.89813822328151,-1.21799821368605,
-4.00104507836823));
#367171=CARTESIAN_POINT('Ctrl Pts',(-0.553550220567405,-1.40738923330208,
-3.97920521870169));
#367172=CARTESIAN_POINT('Ctrl Pts',(-0.368264244678165,-1.46681995203088,
-3.96863978973227));
#367173=CARTESIAN_POINT('Ctrl Pts',(-0.117999612449124,-1.49652294866404,
-3.95577384376029));
#367174=CARTESIAN_POINT('Ctrl Pts',(-0.0589691261687392,-1.49999999999999,
-3.95283715340561));
#367175=CARTESIAN_POINT('Ctrl Pts',(-1.87071622721763E-13,-1.5,-3.95));
#367176=CARTESIAN_POINT('Ctrl Pts',(3.4104663537704E-14,-1.5,-3.8875));
#367177=CARTESIAN_POINT('Ctrl Pts',(-0.112457791852702,-1.5,-3.89291062803322));
#367178=CARTESIAN_POINT('Ctrl Pts',(-0.224787631218977,-1.48735641864598,
-3.89866631054274));
#367179=CARTESIAN_POINT('Ctrl Pts',(-0.524844452862437,-1.41863092322023,
-3.91501184264468));
#367180=CARTESIAN_POINT('Ctrl Pts',(-0.704500440241314,-1.33852372035449,
-3.92588074544717));
#367181=CARTESIAN_POINT('Ctrl Pts',(-1.02631289747861,-1.11184373287966,
-3.9476606208338));
#367182=CARTESIAN_POINT('Ctrl Pts',(-1.164487448864,-0.96618224120435,-3.95835469958346));
#367183=CARTESIAN_POINT('Ctrl Pts',(-1.37129796079268,-0.63689936401491,
-3.97745162156649));
#367184=CARTESIAN_POINT('Ctrl Pts',(-1.44088801771752,-0.45823039515529,
-3.98704275582471));
#367185=CARTESIAN_POINT('Ctrl Pts',(-1.51092172795299,-0.0773713183246262,
-4.00820159342641));
#367186=CARTESIAN_POINT('Ctrl Pts',(-1.50800092734712,0.121676946614712,
-4.01925983036749));
#367187=CARTESIAN_POINT('Ctrl Pts',(-1.42532298188988,0.507299084571875,
-4.04068328247622));
#367188=CARTESIAN_POINT('Ctrl Pts',(-1.34636387258557,0.690061032852196,
-4.05022473333497));
#367189=CARTESIAN_POINT('Ctrl Pts',(-1.12516572374012,1.01039983755458,
-4.06976543436394));
#367190=CARTESIAN_POINT('Ctrl Pts',(-0.986663972320751,1.14602806404199,
-4.0801965537218));
#367191=CARTESIAN_POINT('Ctrl Pts',(-0.65978368952105,1.36181310646325,
-4.10191761761688));
#367192=CARTESIAN_POINT('Ctrl Pts',(-0.472883402989013,1.43744329523372,
-4.11301070042224));
#367193=CARTESIAN_POINT('Ctrl Pts',(-0.088295867177473,1.50961319637537,
-4.13351889634238));
#367194=CARTESIAN_POINT('Ctrl Pts',(0.105065807819668,1.50853894991074,
-4.14231778798253));
#367195=CARTESIAN_POINT('Ctrl Pts',(0.483598568783563,1.43314108124307,
-4.1626243391766));
#367196=CARTESIAN_POINT('Ctrl Pts',(0.664981538209517,1.35850999407786,
-4.17342421711657));
#367197=CARTESIAN_POINT('Ctrl Pts',(0.992936135736941,1.14175588414345,
-4.19522388754512));
#367198=CARTESIAN_POINT('Ctrl Pts',(1.13538582934671,1.00022493250985,-4.20600891694757));
#367199=CARTESIAN_POINT('Ctrl Pts',(1.35179690425842,0.677274072965561,
-4.22539185685346));
#367200=CARTESIAN_POINT('Ctrl Pts',(1.4266010967402,0.500884954451108,-4.23467305808605));
#367201=CARTESIAN_POINT('Ctrl Pts',(1.50781525845693,0.123009737984317,
-4.25566612566754));
#367202=CARTESIAN_POINT('Ctrl Pts',(1.51094277891903,-0.0754241163179732,
-4.26669022868434));
#367203=CARTESIAN_POINT('Ctrl Pts',(1.4400335667351,-0.464710305168755,
-4.28831723917605));
#367204=CARTESIAN_POINT('Ctrl Pts',(1.36570752133438,-0.651510534190223,
-4.29822321441556));
#367205=CARTESIAN_POINT('Ctrl Pts',(1.15258764832469,-0.978902033192879,
-4.31757115739218));
#367206=CARTESIAN_POINT('Ctrl Pts',(1.01827836840078,-1.11794241172047,
-4.32789534837228));
#367207=CARTESIAN_POINT('Ctrl Pts',(0.698538920278946,-1.34225976346303,
-4.34950985729099));
#367208=CARTESIAN_POINT('Ctrl Pts',(0.51445103527626,-1.42301366315333,
-4.36060995358802));
#367209=CARTESIAN_POINT('Ctrl Pts',(0.214614486740088,-1.48847859698552,
-4.37685431663842));
#367210=CARTESIAN_POINT('Ctrl Pts',(0.107350430474416,-1.5,-4.38233510000567));
#367211=CARTESIAN_POINT('Ctrl Pts',(-1.85615411929518E-14,-1.5,-4.38750000000001));
#367212=CARTESIAN_POINT('Origin',(0.,2.16840434497101E-16,-9.7));
#367213=CARTESIAN_POINT('',(2.85080663018025E-8,-1.5,-4.94999999725681));
#367214=CARTESIAN_POINT('',(-9.36107910998493E-14,-1.5,-4.88750000000001));
#367215=CARTESIAN_POINT('',(-1.83697019872103E-16,-1.5,-9.7));
#367216=CARTESIAN_POINT('Ctrl Pts',(2.85743037217734E-8,-1.5,-4.94999999862521));
#367217=CARTESIAN_POINT('Ctrl Pts',(0.195910416521886,-1.499999996268,-4.94057425558667));
#367218=CARTESIAN_POINT('Ctrl Pts',(0.390036215857167,-1.46161847367431,
-4.93016822030604));
#367219=CARTESIAN_POINT('Ctrl Pts',(0.752265960510316,-1.31239413191948,
-4.9085953129864));
#367220=CARTESIAN_POINT('Ctrl Pts',(0.916863851397284,-1.20318262903278,
-4.8976424404108));
#367221=CARTESIAN_POINT('Ctrl Pts',(1.19093071414502,-0.931584875463727,
-4.87691201028527));
#367222=CARTESIAN_POINT('Ctrl Pts',(1.29930258487063,-0.773285365167594,
-4.86796029806485));
#367223=CARTESIAN_POINT('Ctrl Pts',(1.4546550758443,-0.416586025147008,
-4.84814366806371));
#367224=CARTESIAN_POINT('Ctrl Pts',(1.49700859427159,-0.220254463497417,
-4.83723635908318));
#367225=CARTESIAN_POINT('Ctrl Pts',(1.5026082262154,0.172000542307146,-4.81544441431626));
#367226=CARTESIAN_POINT('Ctrl Pts',(1.46793179708167,0.36415166339195,-4.80476935203377));
#367227=CARTESIAN_POINT('Ctrl Pts',(1.32755011756857,0.724554399049284,
-4.78474697783058));
#367228=CARTESIAN_POINT('Ctrl Pts',(1.22324763612743,0.889402637915464,
-4.77581456716931));
#367229=CARTESIAN_POINT('Ctrl Pts',(0.954072389203067,1.17440610602936,
-4.75494710406024));
#367230=CARTESIAN_POINT('Ctrl Pts',(0.790288222939562,1.29031783605482,
-4.74384726440832));
#367231=CARTESIAN_POINT('Ctrl Pts',(0.433936319256726,1.44853778172871,
-4.72230727695758));
#367232=CARTESIAN_POINT('Ctrl Pts',(0.245911886995276,1.49201616816243,
-4.71205321428606));
#367233=CARTESIAN_POINT('Ctrl Pts',(-0.145430304789549,1.50631428890775,
-4.69282758428434));
#367234=CARTESIAN_POINT('Ctrl Pts',(-0.34512098777978,1.47345268809556,
-4.68265793340284));
#367235=CARTESIAN_POINT('Ctrl Pts',(-0.71590585867546,1.33265493519117,
-4.66090748929246));
#367236=CARTESIAN_POINT('Ctrl Pts',(-0.883887722705555,1.22769535459211,
-4.64990991418554));
#367237=CARTESIAN_POINT('Ctrl Pts',(-1.165370081398,0.963327528173154,-4.62902353715474));
#367238=CARTESIAN_POINT('Ctrl Pts',(-1.27785210651291,0.808186899595166,
-4.61989927219972));
#367239=CARTESIAN_POINT('Ctrl Pts',(-1.44275937897357,0.456073158691434,
-4.60033739770507));
#367240=CARTESIAN_POINT('Ctrl Pts',(-1.49044284487975,0.260991823984585,
-4.58949954577691));
#367241=CARTESIAN_POINT('Ctrl Pts',(-1.50676289141006,-0.131447377579266,
-4.56769736791225));
#367242=CARTESIAN_POINT('Ctrl Pts',(-1.47716553931379,-0.324972780132217,
-4.55694595665931));
#367243=CARTESIAN_POINT('Ctrl Pts',(-1.3464895819,-0.688424820958513,-4.5367541766134));
#367244=CARTESIAN_POINT('Ctrl Pts',(-1.2472828805662,-0.855131192483876,
-4.52792294800186));
#367245=CARTESIAN_POINT('Ctrl Pts',(-0.986631235378525,-1.14728655357929,
-4.50726691317862));
#367246=CARTESIAN_POINT('Ctrl Pts',(-0.825673461623653,-1.26805370866375,
-4.49616818548137));
#367247=CARTESIAN_POINT('Ctrl Pts',(-0.472812948553632,-1.43638517702935,
-4.47451530200948));
#367248=CARTESIAN_POINT('Ctrl Pts',(-0.285522965064557,-1.48500905798133,
-4.46415364511771));
#367249=CARTESIAN_POINT('Ctrl Pts',(-0.0627541717646307,-1.4990164725753,
-4.45304658170298));
#367250=CARTESIAN_POINT('Ctrl Pts',(-0.0313615984996725,-1.5,-4.45150888561133));
#367251=CARTESIAN_POINT('Ctrl Pts',(-1.69863252758944E-13,-1.5,-4.45000000000001));
#367252=CARTESIAN_POINT('Ctrl Pts',(-1.71737624121705E-14,-1.5,-4.38750000000001));
#367253=CARTESIAN_POINT('Ctrl Pts',(-0.0829221129230426,-1.5,-4.39148959201816));
#367254=CARTESIAN_POINT('Ctrl Pts',(-0.165877183164973,-1.49312504344208,
-4.39567174071156));
#367255=CARTESIAN_POINT('Ctrl Pts',(-0.445313583363476,-1.44627570677349,
-4.41041750124758));
#367256=CARTESIAN_POINT('Ctrl Pts',(-0.633989368825423,-1.37406727321907,
-4.42150095902903));
#367257=CARTESIAN_POINT('Ctrl Pts',(-0.965446337687612,-1.16401532744184,
-4.4432829661504));
#367258=CARTESIAN_POINT('Ctrl Pts',(-1.10665945088798,-1.03069955306717,
-4.45378030118187));
#367259=CARTESIAN_POINT('Ctrl Pts',(-1.33311870096298,-0.715008228143621,
-4.47344503040124));
#367260=CARTESIAN_POINT('Ctrl Pts',(-1.41506355227756,-0.534836499656983,
-4.48278686113017));
#367261=CARTESIAN_POINT('Ctrl Pts',(-1.50533076614708,-0.151675795448859,
-4.50407356691951));
#367262=CARTESIAN_POINT('Ctrl Pts',(-1.51220048320158,0.0476751903314799,
-4.51514862168509));
#367263=CARTESIAN_POINT('Ctrl Pts',(-1.44946690860152,0.430423689729183,
-4.53641242720718));
#367264=CARTESIAN_POINT('Ctrl Pts',(-1.38323455609893,0.610602562238479,
-4.54624361200806));
#367265=CARTESIAN_POINT('Ctrl Pts',(-1.18261816761641,0.943898733305205,
-4.56515399947332));
#367266=CARTESIAN_POINT('Ctrl Pts',(-1.04725098352344,1.09214011438375,
-4.57578467229569));
#367267=CARTESIAN_POINT('Ctrl Pts',(-0.729538359551367,1.32509637034778,
-4.59754163515374));
#367268=CARTESIAN_POINT('Ctrl Pts',(-0.551075941165947,1.40869768735186,
-4.60845017106733));
#367269=CARTESIAN_POINT('Ctrl Pts',(-0.176716557605994,1.5016872279536,
-4.62904458810115));
#367270=CARTESIAN_POINT('Ctrl Pts',(0.0151935172421368,1.51197132588372,
-4.63789846160904));
#367271=CARTESIAN_POINT('Ctrl Pts',(0.402703160445184,1.45879716567031,
-4.65801958801637));
#367272=CARTESIAN_POINT('Ctrl Pts',(0.593985367226513,1.39191361876467,
-4.66908053378401));
#367273=CARTESIAN_POINT('Ctrl Pts',(0.932271564999293,1.19083659572109,
-4.69094180892527));
#367274=CARTESIAN_POINT('Ctrl Pts',(1.07756911177044,1.06117073233087,-4.70153426994229));
#367275=CARTESIAN_POINT('Ctrl Pts',(1.31202288914959,0.752624332817159,
-4.72138516588565));
#367276=CARTESIAN_POINT('Ctrl Pts',(1.39846495836364,0.576324684903343,
-4.73048196194982));
#367277=CARTESIAN_POINT('Ctrl Pts',(1.5001497547969,0.197009390524566,-4.75155503385975));
#367278=CARTESIAN_POINT('Ctrl Pts',(1.51302651117266,-0.0026546548410443,
-4.76264748082451));
#367279=CARTESIAN_POINT('Ctrl Pts',(1.46143097252156,-0.388059744347202,
-4.78405887468596));
#367280=CARTESIAN_POINT('Ctrl Pts',(1.40030268792451,-0.570567507184692,
-4.7941981948436));
#367281=CARTESIAN_POINT('Ctrl Pts',(1.20899755076974,-0.909843039816958,
-4.81304683554539));
#367282=CARTESIAN_POINT('Ctrl Pts',(1.07792543005673,-1.06189520343739,
-4.82346871088358));
#367283=CARTESIAN_POINT('Ctrl Pts',(0.766452670177431,-1.30417307550099,
-4.84518439192103));
#367284=CARTESIAN_POINT('Ctrl Pts',(0.589896936198974,-1.39296218739351,
-4.85614529785189));
#367285=CARTESIAN_POINT('Ctrl Pts',(0.270346234866123,-1.48167998739823,
-4.87398407147154));
#367286=CARTESIAN_POINT('Ctrl Pts',(0.135370689680846,-1.50000000000002,
-4.88098697465604));
#367287=CARTESIAN_POINT('Ctrl Pts',(-1.88703219716757E-13,-1.5,-4.88750000000001));
#367288=CARTESIAN_POINT('Origin',(0.,2.16840434497101E-16,-9.7));
#367289=CARTESIAN_POINT('',(5.08393723981206E-14,-1.5,-5.44999999999999));
#367290=CARTESIAN_POINT('',(-5.10233297646163E-14,-1.5,-5.38750000000001));
#367291=CARTESIAN_POINT('',(-1.83697019872103E-16,-1.5,-9.7));
#367292=CARTESIAN_POINT('Ctrl Pts',(1.01862441816113E-13,-1.5,-5.44999999999999));
#367293=CARTESIAN_POINT('Ctrl Pts',(0.0263651739551401,-1.5,-5.44873150497664));
#367294=CARTESIAN_POINT('Ctrl Pts',(0.0527523821946788,-1.49930488812725,
-5.44744264116515));
#367295=CARTESIAN_POINT('Ctrl Pts',(0.277718326846129,-1.4874199513975,
-5.43628882497519));
#367296=CARTESIAN_POINT('Ctrl Pts',(0.472215788715003,-1.43754461477542,
-5.42554563546068));
#367297=CARTESIAN_POINT('Ctrl Pts',(0.826559672875883,-1.26674832897375,
-5.40375291611291));
#367298=CARTESIAN_POINT('Ctrl Pts',(0.983733117419562,-1.14896970203481,
-5.39291927671044));
#367299=CARTESIAN_POINT('Ctrl Pts',(1.24210426384262,-0.862412663408363,
-5.37252847139263));
#367300=CARTESIAN_POINT('Ctrl Pts',(1.34181572159714,-0.697214195621655,
-5.36373412197897));
#367301=CARTESIAN_POINT('Ctrl Pts',(1.47683335814032,-0.330060296931495,
-5.34333668316285));
#367302=CARTESIAN_POINT('Ctrl Pts',(1.50762432316895,-0.130505577948834,
-5.33225030988604));
#367303=CARTESIAN_POINT('Ctrl Pts',(1.48953296953489,0.261294957627765,
-5.31048361346512));
#367304=CARTESIAN_POINT('Ctrl Pts',(1.44379939786353,0.449939486882149,
-5.30000336183987));
#367305=CARTESIAN_POINT('Ctrl Pts',(1.28188447478999,0.803321599497433,
-5.28037102225013));
#367306=CARTESIAN_POINT('Ctrl Pts',(1.16584828536497,0.964035863125838,
-5.27097979447342));
#367307=CARTESIAN_POINT('Ctrl Pts',(0.877599962231806,1.2323976979204,-5.24965694514959));
#367308=CARTESIAN_POINT('Ctrl Pts',(0.707936356116261,1.33708986900095,
-5.23858588523104));
#367309=CARTESIAN_POINT('Ctrl Pts',(0.344567510283842,1.47223165337793,
-5.21734935502975));
#367310=CARTESIAN_POINT('Ctrl Pts',(0.155317568062389,1.50400359956028,
-5.20758393107645));
#367311=CARTESIAN_POINT('Ctrl Pts',(-0.233539223820948,1.49498906414918,
-5.18862464619252));
#367312=CARTESIAN_POINT('Ctrl Pts',(-0.429393951225143,1.45090598297018,
-5.17797705119403));
#367313=CARTESIAN_POINT('Ctrl Pts',(-0.789125099850543,1.29048502131858,
-5.15621334041248));
#367314=CARTESIAN_POINT('Ctrl Pts',(-0.95012792291364,1.17700237915228,
-5.14531479286043));
#367315=CARTESIAN_POINT('Ctrl Pts',(-1.21650593922147,0.898020105215934,
-5.12474916696596));
#367316=CARTESIAN_POINT('Ctrl Pts',(-1.320631925763,0.736378716832192,-5.11590992871289));
#367317=CARTESIAN_POINT('Ctrl Pts',(-1.46653676135899,0.373481609252619,
-5.0957489782918));
#367318=CARTESIAN_POINT('Ctrl Pts',(-1.50326970020796,0.174305383486191,
-5.08468363241589));
#367319=CARTESIAN_POINT('Ctrl Pts',(-1.49640740843039,-0.218981562746956,
-5.06283435762516));
#367320=CARTESIAN_POINT('Ctrl Pts',(-1.45589167669697,-0.409370563639839,
-5.05225719090889));
#367321=CARTESIAN_POINT('Ctrl Pts',(-1.30421536216214,-0.766134745524016,
-5.03243695858199));
#367322=CARTESIAN_POINT('Ctrl Pts',(-1.19383411420971,-0.928820751969231,
-5.02330446082362));
#367323=CARTESIAN_POINT('Ctrl Pts',(-0.914679147103492,-1.20523228366345,
-5.00219551310397));
#367324=CARTESIAN_POINT('Ctrl Pts',(-0.747739827958748,-1.31533367575935,
-4.9911052693641));
#367325=CARTESIAN_POINT('Ctrl Pts',(-0.387629444244665,-1.46153354298933,
-4.96971834302643));
#367326=CARTESIAN_POINT('Ctrl Pts',(-0.198917662169693,-1.49893060653779,
-4.95960013585729));
#367327=CARTESIAN_POINT('Ctrl Pts',(-0.00548928539186333,-1.49999246786982,
-4.95026431259238));
#367328=CARTESIAN_POINT('Ctrl Pts',(-0.00274446328429652,-1.50000000005228,
-4.95013204305278));
#367329=CARTESIAN_POINT('Ctrl Pts',(2.85743048114312E-8,-1.5,-4.94999999862521));
#367330=CARTESIAN_POINT('Ctrl Pts',(-1.87037885179826E-13,-1.5,-4.88750000000001));
#367331=CARTESIAN_POINT('Ctrl Pts',(-0.0540462695308795,-1.49999999999999,
-4.8901003023552));
#367332=CARTESIAN_POINT('Ctrl Pts',(-0.108147676289032,-1.49707922019035,
-4.89278439027397));
#367333=CARTESIAN_POINT('Ctrl Pts',(-0.359814125721349,-1.46972714332125,
-4.90565247788081));
#367334=CARTESIAN_POINT('Ctrl Pts',(-0.551295619407549,-1.40911968988848,
-4.91654867591433));
#367335=CARTESIAN_POINT('Ctrl Pts',(-0.894744498290115,-1.21937731862514,
-4.93834348922795));
#367336=CARTESIAN_POINT('Ctrl Pts',(-1.04444802750409,-1.09388814473448,
-4.94903191402133));
#367337=CARTESIAN_POINT('Ctrl Pts',(-1.28764107828231,-0.793268603442221,
-4.96908308794599));
#367338=CARTESIAN_POINT('Ctrl Pts',(-1.37895629232874,-0.621109605663026,
-4.9779939107965));
#367339=CARTESIAN_POINT('Ctrl Pts',(-1.4929637296001,-0.246131760036213,
-4.99882601333133));
#367340=CARTESIAN_POINT('Ctrl Pts',(-1.5124042662344,-0.046327287996343,
-5.00992626177799));
#367341=CARTESIAN_POINT('Ctrl Pts',(-1.47302330444493,0.341756093908819,
-5.0314864496616));
#367342=CARTESIAN_POINT('Ctrl Pts',(-1.41747667306572,0.52666588745438,
-5.04175921596969));
#367343=CARTESIAN_POINT('Ctrl Pts',(-1.23585023889997,0.873309400994758,
-5.06101718894416));
#367344=CARTESIAN_POINT('Ctrl Pts',(-1.10852292020812,1.03014952423744,
-5.07111476403007));
#367345=CARTESIAN_POINT('Ctrl Pts',(-0.802682556237449,1.28227517515059,
-5.09283300570551));
#367346=CARTESIAN_POINT('Ctrl Pts',(-0.628176408674604,1.37619980171365,
-5.10383795404925));
#367347=CARTESIAN_POINT('Ctrl Pts',(-0.258965513662954,1.48963680612895,
-5.12475264941824));
#367348=CARTESIAN_POINT('Ctrl Pts',(-0.0684870903143073,1.51042170292824,
-5.13391542158291));
#367349=CARTESIAN_POINT('Ctrl Pts',(0.319042014244513,1.47911051435621,
-5.15343017955735));
#367350=CARTESIAN_POINT('Ctrl Pts',(0.512102500769454,1.42382780144004,
-5.16425443746044));
#367351=CARTESIAN_POINT('Ctrl Pts',(0.861107381613573,1.24344002427904,
-5.1860567142069));
#367352=CARTESIAN_POINT('Ctrl Pts',(1.01457887995497,1.12173564265987,-5.19682129238079));
#367353=CARTESIAN_POINT('Ctrl Pts',(1.2653628380366,0.828102729138014,-5.21704361100975));
#367354=CARTESIAN_POINT('Ctrl Pts',(1.36088590783901,0.65945994173573,-5.22586333657024));
#367355=CARTESIAN_POINT('Ctrl Pts',(1.48546319186562,0.288353241746187,
-5.24648037545855));
#367356=CARTESIAN_POINT('Ctrl Pts',(1.51059193401268,0.0885961576228984,
-5.25757799124318));
#367357=CARTESIAN_POINT('Ctrl Pts',(1.48185374683415,-0.301494364037364,
-5.27924968689097));
#367358=CARTESIAN_POINT('Ctrl Pts',(1.43119950302677,-0.488341944754652,
-5.28963010804193));
#367359=CARTESIAN_POINT('Ctrl Pts',(1.2594817962717,-0.838410696396134,
-5.30907837202201));
#367360=CARTESIAN_POINT('Ctrl Pts',(1.13789799615601,-0.997215134410307,
-5.31878661086771));
#367361=CARTESIAN_POINT('Ctrl Pts',(0.840911554960286,-1.25762727854883,
-5.34030904835239));
#367362=CARTESIAN_POINT('Ctrl Pts',(0.668770495030703,-1.35702049989082,
-5.35135211177486));
#367363=CARTESIAN_POINT('Ctrl Pts',(0.326816869742832,-1.47315072340218,
-5.37103020278437));
#367364=CARTESIAN_POINT('Ctrl Pts',(0.163873689066774,-1.50000000000001,
-5.37961562345869));
#367365=CARTESIAN_POINT('Ctrl Pts',(-1.03146657881581E-13,-1.5,-5.38750000000001));
#367366=CARTESIAN_POINT('Origin',(0.,2.16840434497101E-16,-9.7));
#367367=CARTESIAN_POINT('',(9.74881735715278E-14,-1.5,-5.94999999999999));
#367368=CARTESIAN_POINT('',(-4.32989591281128E-8,-1.5,-5.88750000416645));
#367369=CARTESIAN_POINT('',(-1.83697019872103E-16,-1.5,-9.7));
#367370=CARTESIAN_POINT('Ctrl Pts',(1.95160044162928E-13,-1.5,-5.94999999999999));
#367371=CARTESIAN_POINT('Ctrl Pts',(0.0546724918751179,-1.5,-5.94736956850821));
#367372=CARTESIAN_POINT('Ctrl Pts',(0.109400508428987,-1.49701114857146,
-5.94465344193329));
#367373=CARTESIAN_POINT('Ctrl Pts',(0.361659483794658,-1.46927425572993,
-5.93174615707662));
#367374=CARTESIAN_POINT('Ctrl Pts',(0.553065678554439,-1.40842605692642,
-5.92084689449298));
#367375=CARTESIAN_POINT('Ctrl Pts',(0.896256244038983,-1.21826288033519,
-5.89905282025163));
#367376=CARTESIAN_POINT('Ctrl Pts',(1.04578649131481,-1.09260450286954,
-5.88836803239008));
#367377=CARTESIAN_POINT('Ctrl Pts',(1.28863322740306,-0.791668488711237,
-5.86832472962576));
#367378=CARTESIAN_POINT('Ctrl Pts',(1.37975600578144,-0.619347280917291,
-5.85940818227318));
#367379=CARTESIAN_POINT('Ctrl Pts',(1.49327827165981,-0.244195051917849,
-5.83856639177321));
#367380=CARTESIAN_POINT('Ctrl Pts',(1.51245892969766,-0.0443921573901792,
-5.82746623096612));
#367381=CARTESIAN_POINT('Ctrl Pts',(1.47259300132903,0.343592577334264,
-5.80591152348143));
#367382=CARTESIAN_POINT('Ctrl Pts',(1.41682407311496,0.528410655372149,
-5.79564385247932));
#367383=CARTESIAN_POINT('Ctrl Pts',(1.23474322506663,0.874895225824404,
-5.77639470967642));
#367384=CARTESIAN_POINT('Ctrl Pts',(1.10714918922497,1.03164424545367,-5.7662776222734));
#367385=CARTESIAN_POINT('Ctrl Pts',(0.800902451810381,1.28338366753864,
-5.74455055752509));
#367386=CARTESIAN_POINT('Ctrl Pts',(0.626291330195158,1.37705491791357,
-5.73354759684234));
#367387=CARTESIAN_POINT('Ctrl Pts',(0.256949134406888,1.4899864401885,-5.71264062543236));
#367388=CARTESIAN_POINT('Ctrl Pts',(0.0664386026299455,1.5105138274722,
-5.70348857952253));
#367389=CARTESIAN_POINT('Ctrl Pts',(-0.32105371365814,1.47867531398939,
-5.68396094361041));
#367390=CARTESIAN_POINT('Ctrl Pts',(-0.51404007021658,1.42312963011403,
-5.67313294753812));
#367391=CARTESIAN_POINT('Ctrl Pts',(-0.86277756894227,1.24227774632932,
-5.65133064336918));
#367392=CARTESIAN_POINT('Ctrl Pts',(-1.0160658593181,1.12038455171356,-5.64056963498718));
#367393=CARTESIAN_POINT('Ctrl Pts',(-1.26647789513751,0.826407077074905,
-5.62035563933427));
#367394=CARTESIAN_POINT('Ctrl Pts',(-1.36179517096147,0.657593764873694,
-5.61153298693742));
#367395=CARTESIAN_POINT('Ctrl Pts',(-1.48585744571148,0.286295279048441,
-5.59090529328046));
#367396=CARTESIAN_POINT('Ctrl Pts',(-1.5107079190491,0.086532237250619,
-5.57980734651392));
#367397=CARTESIAN_POINT('Ctrl Pts',(-1.48144784744948,-0.303466848535801,
-5.55814073063689));
#367398=CARTESIAN_POINT('Ctrl Pts',(-1.4305530780986,-0.490222727524862,
-5.54776540402639));
#367399=CARTESIAN_POINT('Ctrl Pts',(-1.25835217976544,-0.84012623627136,
-5.52832632020714));
#367400=CARTESIAN_POINT('Ctrl Pts',(-1.13649149405738,-0.998835774444738,
-5.51860070098978));
#367401=CARTESIAN_POINT('Ctrl Pts',(-0.839073707596556,-1.25884976420935,
-5.49706857024008));
#367402=CARTESIAN_POINT('Ctrl Pts',(-0.666814006000366,-1.35797887345876,
-5.48602713511478));
#367403=CARTESIAN_POINT('Ctrl Pts',(-0.325397739255144,-1.47338552249901,
-5.46639499707107));
#367404=CARTESIAN_POINT('Ctrl Pts',(-0.16315592440875,-1.5,-5.45784984307311));
#367405=CARTESIAN_POINT('Ctrl Pts',(1.01377239936085E-13,-1.5,-5.44999999999999));
#367406=CARTESIAN_POINT('Ctrl Pts',(-1.0186296250936E-13,-1.5,-5.38750000000001));
#367407=CARTESIAN_POINT('Ctrl Pts',(-0.0256619673057862,-1.5,-5.38873466197767));
#367408=CARTESIAN_POINT('Ctrl Pts',(-0.0513450144281305,-1.49934147279655,
-5.3899886305808));
#367409=CARTESIAN_POINT('Ctrl Pts',(-0.275621128406905,-1.48780980469279,
-5.40109944425966));
#367410=CARTESIAN_POINT('Ctrl Pts',(-0.47018718093381,-1.43820917050335,
-5.41183830322061));
#367411=CARTESIAN_POINT('Ctrl Pts',(-0.824794258445663,-1.26790258960189,
-5.43363008255048));
#367412=CARTESIAN_POINT('Ctrl Pts',(-0.982152470284429,-1.15032558928547,
-5.44446701083407));
#367413=CARTESIAN_POINT('Ctrl Pts',(-1.24090605577986,-0.864127755771773,
-5.46486623834053));
#367414=CARTESIAN_POINT('Ctrl Pts',(-1.34082836484502,-0.699101034024753,
-5.4736610536653));
#367415=CARTESIAN_POINT('Ctrl Pts',(-1.47636902037079,-0.332148478379624,
-5.49404730675669));
#367416=CARTESIAN_POINT('Ctrl Pts',(-1.50744463298203,-0.132608012550994,
-5.50513288819162));
#367417=CARTESIAN_POINT('Ctrl Pts',(-1.48988989187833,0.259270920023298,
-5.5269039400013));
#367418=CARTESIAN_POINT('Ctrl Pts',(-1.44440501779414,0.448002314883359,
-5.53738901749352));
#367419=CARTESIAN_POINT('Ctrl Pts',(-1.28298157039537,0.801548601297589,
-5.55703047784987));
#367420=CARTESIAN_POINT('Ctrl Pts',(-1.16722005041924,0.962357952463247,
-5.56640759782012));
#367421=CARTESIAN_POINT('Ctrl Pts',(-0.879409087628147,1.23111202588909,
-5.58772030015221));
#367422=CARTESIAN_POINT('Ctrl Pts',(-0.70987313894258,1.33606683349401,
-5.59879251360881));
#367423=CARTESIAN_POINT('Ctrl Pts',(-0.346653687238665,1.4717442380186,
-5.62003673441918));
#367424=CARTESIAN_POINT('Ctrl Pts',(-0.157430484209326,1.50378596490384,
-5.62982045660516));
#367425=CARTESIAN_POINT('Ctrl Pts',(0.231453196392725,1.4953132249182,-5.64876598530023));
#367426=CARTESIAN_POINT('Ctrl Pts',(0.427367482033715,1.45150391708622,
-5.65940884098053));
#367427=CARTESIAN_POINT('Ctrl Pts',(0.787344881840087,1.29157591836,-5.68117070611296));
#367428=CARTESIAN_POINT('Ctrl Pts',(0.94852526786724,1.17829863658823,-5.69207209221169));
#367429=CARTESIAN_POINT('Ctrl Pts',(1.21527890331185,0.899674554409161,
-5.71264584031927));
#367430=CARTESIAN_POINT('Ctrl Pts',(1.31961207830169,0.73819807357228,-5.72148899591266));
#367431=CARTESIAN_POINT('Ctrl Pts',(1.46602444349983,0.375502732956456,
-5.74163873705798));
#367432=CARTESIAN_POINT('Ctrl Pts',(1.5030351545464,0.176348361746048,-5.75270286879189));
#367433=CARTESIAN_POINT('Ctrl Pts',(1.49669919734387,-0.217000356834536,
-5.7745555753797));
#367434=CARTESIAN_POINT('Ctrl Pts',(1.45642873751693,-0.407467369946189,
-5.78513707610813));
#367435=CARTESIAN_POINT('Ctrl Pts',(1.30523012125535,-0.76438740080986,
-5.80496596671167));
#367436=CARTESIAN_POINT('Ctrl Pts',(1.19510931166096,-0.927165031214452,
-5.8140881939672));
#367437=CARTESIAN_POINT('Ctrl Pts',(0.916377607621684,-1.2039459831623,
-5.83518703910676));
#367438=CARTESIAN_POINT('Ctrl Pts',(0.749568638977346,-1.31429650733405,
-5.84627793169071));
#367439=CARTESIAN_POINT('Ctrl Pts',(0.389610289995854,-1.46101002328375,
-5.86767181127388));
#367440=CARTESIAN_POINT('Ctrl Pts',(0.200923816790519,-1.49866618236168,
-5.8777959978675));
#367441=CARTESIAN_POINT('Ctrl Pts',(0.00681097685229299,-1.49998840442069,
-5.88717198462399));
#367442=CARTESIAN_POINT('Ctrl Pts',(0.00340521405330191,-1.50000000009853,
-5.88733616655974));
#367443=CARTESIAN_POINT('Ctrl Pts',(-4.33996891097767E-8,-1.5,-5.88750000208807));
#367444=CARTESIAN_POINT('Origin',(0.,2.16840434497101E-16,-9.7));
#367445=CARTESIAN_POINT('',(4.06290604931913E-15,-1.5,-6.45));
#367446=CARTESIAN_POINT('',(8.47483643639537E-14,-1.5,-6.3875));
#367447=CARTESIAN_POINT('',(-1.83697019872103E-16,-1.5,-9.7));
#367448=CARTESIAN_POINT('Ctrl Pts',(8.30950911851036E-15,-1.5,-6.45));
#367449=CARTESIAN_POINT('Ctrl Pts',(0.0836220240189683,-1.5,-6.44597673349354));
#367450=CARTESIAN_POINT('Ctrl Pts',(0.167275159716708,-1.4930085099386,
-6.44175776206847));
#367451=CARTESIAN_POINT('Ctrl Pts',(0.447311848965298,-1.44565501504088,
-6.42696911571681));
#367452=CARTESIAN_POINT('Ctrl Pts',(0.635861319637451,-1.37319794769801,
-6.41588482876439));
#367453=CARTESIAN_POINT('Ctrl Pts',(0.966990781533922,-1.16272850281152,
-6.39410698163178));
#367454=CARTESIAN_POINT('Ctrl Pts',(1.10800920467463,-1.02924381484293,
-6.3836143215859));
#367455=CARTESIAN_POINT('Ctrl Pts',(1.334089564726,-0.713216352739631,-6.36395848457741));
#367456=CARTESIAN_POINT('Ctrl Pts',(1.4158201412557,-0.532859175839884,
-6.35460328754666));
#367457=CARTESIAN_POINT('Ctrl Pts',(1.50554279496689,-0.149519314526434,
-6.3333066285848));
#367458=CARTESIAN_POINT('Ctrl Pts',(1.51212795197166,0.0498124374358952,
-6.32223264236467));
#367459=CARTESIAN_POINT('Ctrl Pts',(1.44886815250877,0.432426328348405,
-6.30097631509175));
#367460=CARTESIAN_POINT('Ctrl Pts',(1.38239490638562,0.61249579567037,-6.29116340050872));
#367461=CARTESIAN_POINT('Ctrl Pts',(1.18133400021063,0.945505775759388,
-6.27223957592539));
#367462=CARTESIAN_POINT('Ctrl Pts',(1.0457641280893,1.09356425628846,-6.26160423184153));
#367463=CARTESIAN_POINT('Ctrl Pts',(0.727753807144858,1.32607351058838,
-6.23984536274412));
#367464=CARTESIAN_POINT('Ctrl Pts',(0.549203697674222,1.40942514019646,
-6.22893954355222));
#367465=CARTESIAN_POINT('Ctrl Pts',(0.17472459156813,1.50192328426092,-6.20835301626852));
#367466=CARTESIAN_POINT('Ctrl Pts',(-0.0172232732627098,1.51195258899534,
-6.19950336123977));
#367467=CARTESIAN_POINT('Ctrl Pts',(-0.404656715019742,1.45825267216852,
-6.17937129672584));
#367468=CARTESIAN_POINT('Ctrl Pts',(-0.595823034910048,1.39112403379354,
-6.16830911847248));
#367469=CARTESIAN_POINT('Ctrl Pts',(-0.933802532933181,1.18963253496017,
-6.14645108621343));
#367470=CARTESIAN_POINT('Ctrl Pts',(-1.07891560035492,1.05979734012534,
-6.135862797312));
#367471=CARTESIAN_POINT('Ctrl Pts',(-1.31300625698492,0.75092422433093,
-6.11602029657159));
#367472=CARTESIAN_POINT('Ctrl Pts',(-1.39924496724479,0.574450422168306,
-6.10691391234268));
#367473=CARTESIAN_POINT('Ctrl Pts',(-1.50041417045913,0.194957843525356,
-6.08583099130696));
#367474=CARTESIAN_POINT('Ctrl Pts',(-1.51301804316835,-0.00469581672682119,
-6.07473912129295));
#367475=CARTESIAN_POINT('Ctrl Pts',(-1.46091624463761,-0.389981114792215,
-6.05333438251154));
#367476=CARTESIAN_POINT('Ctrl Pts',(-1.399557396858,-0.572385147039804,
-6.04320082516445));
#367477=CARTESIAN_POINT('Ctrl Pts',(-1.20783109806283,-0.911389995950663,
-6.02436722244718));
#367478=CARTESIAN_POINT('Ctrl Pts',(-1.07656661998166,-1.06327239050781,
-6.0139276581398));
#367479=CARTESIAN_POINT('Ctrl Pts',(-0.764805407702597,-1.30513611986922,
-5.99220960289375));
#367480=CARTESIAN_POINT('Ctrl Pts',(-0.588160753060915,-1.39369278579797,
-5.98125087559781));
#367481=CARTESIAN_POINT('Ctrl Pts',(-0.269119198949494,-1.48184688845222,
-5.96345225659501));
#367482=CARTESIAN_POINT('Ctrl Pts',(-0.134752651461745,-1.5,-5.95648328996629));
#367483=CARTESIAN_POINT('Ctrl Pts',(1.96006405550619E-13,-1.5,-5.94999999999999));
#367484=CARTESIAN_POINT('Ctrl Pts',(-4.33996887733157E-8,-1.5,-5.88750000208807));
#367485=CARTESIAN_POINT('Ctrl Pts',(-0.195242606810165,-1.49999999435102,
-5.89689361445685));
#367486=CARTESIAN_POINT('Ctrl Pts',(-0.388722924848865,-1.46187996269871,
-5.90726133036685));
#367487=CARTESIAN_POINT('Ctrl Pts',(-0.750561595655201,-1.31337333001173,
-5.92879548577426));
#367488=CARTESIAN_POINT('Ctrl Pts',(-0.915321653672233,-1.20436028788468,
-5.93975064782067));
#367489=CARTESIAN_POINT('Ctrl Pts',(-1.18973972539303,-0.93310251861447,
-5.96048853148749));
#367490=CARTESIAN_POINT('Ctrl Pts',(-1.29830585366695,-0.774954000507073,
-5.96944699997184));
#367491=CARTESIAN_POINT('Ctrl Pts',(-1.45411392074071,-0.41847063235772,
-5.98925163153569));
#367492=CARTESIAN_POINT('Ctrl Pts',(-1.49672162993495,-0.22219512861367,
-6.00015582618814));
#367493=CARTESIAN_POINT('Ctrl Pts',(-1.50283046342648,0.17007530608529,
-6.02194862811586));
#367494=CARTESIAN_POINT('Ctrl Pts',(-1.46839435017176,0.362294737240242,
-6.03262748540224));
#367495=CARTESIAN_POINT('Ctrl Pts',(-1.32847421282326,0.722844100909313,
-6.05265800560608));
#367496=CARTESIAN_POINT('Ctrl Pts',(-1.22441668040302,0.887780618452159,
-6.06158413106555));
#367497=CARTESIAN_POINT('Ctrl Pts',(-0.955647919996864,1.17312894984812,
-6.08244161661851));
#367498=CARTESIAN_POINT('Ctrl Pts',(-0.791995833525539,1.28927449625884,
-6.09354159647806));
#367499=CARTESIAN_POINT('Ctrl Pts',(-0.435804622016396,1.44797995007156,
-6.11508733896017));
#367500=CARTESIAN_POINT('Ctrl Pts',(-0.247812161776026,1.49170477213654,
-6.12534670881131));
#367501=CARTESIAN_POINT('Ctrl Pts',(0.143437792981978,1.50649233312871,
-6.14458149661943));
#367502=CARTESIAN_POINT('Ctrl Pts',(0.343071986735211,1.47391757420866,
-6.1547305704853));
#367503=CARTESIAN_POINT('Ctrl Pts',(0.71399393589645,1.33368434453721,-6.17647192857588));
#367504=CARTESIAN_POINT('Ctrl Pts',(0.882149412527287,1.22894938002697,
-6.18747161728716));
#367505=CARTESIAN_POINT('Ctrl Pts',(1.16401738391211,0.964960525296338,
-6.20836602012592));
#367506=CARTESIAN_POINT('Ctrl Pts',(1.27671370824356,0.80998253382708,-6.21750097034295));
#367507=CARTESIAN_POINT('Ctrl Pts',(1.44211419342194,0.458108664485862,
-6.23704951863969));
#367508=CARTESIAN_POINT('Ctrl Pts',(1.49007263878478,0.263096120522399,
-6.24788354885988));
#367509=CARTESIAN_POINT('Ctrl Pts',(1.5069482561287,-0.129344586869214,
-6.26968581038164));
#367510=CARTESIAN_POINT('Ctrl Pts',(1.47761524480886,-0.322937556506277,
-6.28044097536147));
#367511=CARTESIAN_POINT('Ctrl Pts',(1.34744177127719,-0.686545509678991,
-6.3006414172044));
#367512=CARTESIAN_POINT('Ctrl Pts',(1.24849578411744,-0.853348254296545,
-6.30946917008806));
#367513=CARTESIAN_POINT('Ctrl Pts',(0.988283968217334,-1.14586823009435,
-6.33011417180102));
#367514=CARTESIAN_POINT('Ctrl Pts',(0.827475233263472,-1.26688320437232,
-6.3412126127321));
#367515=CARTESIAN_POINT('Ctrl Pts',(0.474801747978033,-1.43573244565706,
-6.36287088040659));
#367516=CARTESIAN_POINT('Ctrl Pts',(0.28755328116884,-1.48462055179668,
-6.37323787941471));
#367517=CARTESIAN_POINT('Ctrl Pts',(0.0641026458976871,-1.49897376207815,
-6.38438735340234));
#367518=CARTESIAN_POINT('Ctrl Pts',(0.0320353314952041,-1.5,-6.38595869939481));
#367519=CARTESIAN_POINT('Ctrl Pts',(1.6968042574778E-13,-1.5,-6.3875));
#367520=CARTESIAN_POINT('Origin',(0.,2.16840434497101E-16,-9.7));
#367521=CARTESIAN_POINT('',(-2.14167123658283E-14,-1.5,-6.95));
#367522=CARTESIAN_POINT('',(9.32415705023364E-14,-1.5,-6.8875));
#367523=CARTESIAN_POINT('',(-1.83697019872103E-16,-1.5,-9.7));
#367524=CARTESIAN_POINT('Ctrl Pts',(-4.29864477347053E-14,-1.5,-6.95));
#367525=CARTESIAN_POINT('Ctrl Pts',(0.11291155950509,-1.5,-6.94456754006042));
#367526=CARTESIAN_POINT('Ctrl Pts',(0.225691172814987,-1.48725419527285,
-6.93878737825382));
#367527=CARTESIAN_POINT('Ctrl Pts',(0.526145953213928,-1.41815114243535,
-6.92241221164644));
#367528=CARTESIAN_POINT('Ctrl Pts',(0.705744487927115,-1.33787078720479,
-6.9115412632487));
#367529=CARTESIAN_POINT('Ctrl Pts',(1.02735711636434,-1.11087871951942,
-6.88976233323497));
#367530=CARTESIAN_POINT('Ctrl Pts',(1.16539401547416,-0.965088350881621,
-6.87907129736788));
#367531=CARTESIAN_POINT('Ctrl Pts',(1.37189888429361,-0.63560614470349,
-6.85998354372944));
#367532=CARTESIAN_POINT('Ctrl Pts',(1.44132318505672,-0.456863402306125,
-6.85038130012812));
#367533=CARTESIAN_POINT('Ctrl Pts',(1.51099830419892,-0.0759104136947216,
-6.82921724520526));
#367534=CARTESIAN_POINT('Ctrl Pts',(1.50788348376108,0.1231545316006,-6.81815808157774));
#367535=CARTESIAN_POINT('Ctrl Pts',(1.42483099268254,0.508656990753634,
-6.79674127829146));
#367536=CARTESIAN_POINT('Ctrl Pts',(1.34572453403093,0.691290828855329,
-6.78721034547439));
#367537=CARTESIAN_POINT('Ctrl Pts',(1.1242677063703,1.01140212949755,-6.76766351831235));
#367538=CARTESIAN_POINT('Ctrl Pts',(0.985632258322067,1.14691832046349,
-6.75722907857026));
#367539=CARTESIAN_POINT('Ctrl Pts',(0.658525520100797,1.3624247149364,-6.73550485955441));
#367540=CARTESIAN_POINT('Ctrl Pts',(0.471536868009192,1.43788821446901,
-6.72441215551569));
#367541=CARTESIAN_POINT('Ctrl Pts',(0.0868895231586778,1.50969127631196,
-6.70391127201234));
#367542=CARTESIAN_POINT('Ctrl Pts',(-0.106442488420188,1.50843893766231,
-6.69511319859553));
#367543=CARTESIAN_POINT('Ctrl Pts',(-0.489874426699714,1.43170848958283,
-6.67453391950496));
#367544=CARTESIAN_POINT('Ctrl Pts',(-0.675645000454847,1.35397879398435,
-6.66343687014768));
#367545=CARTESIAN_POINT('Ctrl Pts',(-0.999641720894044,1.13468977939164,
-6.64175720915104));
#367546=CARTESIAN_POINT('Ctrl Pts',(-1.136445113522,0.997655916834551,-6.63136875667225));
#367547=CARTESIAN_POINT('Ctrl Pts',(-1.35436332559314,0.674441434527717,
-6.61190598174145));
#367548=CARTESIAN_POINT('Ctrl Pts',(-1.43144886866969,0.490048524005243,
-6.60222491800029));
#367549=CARTESIAN_POINT('Ctrl Pts',(-1.50936527731721,0.102921352358107,
-6.58071785290878));
#367550=CARTESIAN_POINT('Ctrl Pts',(-1.50982762747414,-0.0958993071838165,
-6.56967226071201));
#367551=CARTESIAN_POINT('Ctrl Pts',(-1.4352502306905,-0.475558716944506,
-6.54858007128086));
#367552=CARTESIAN_POINT('Ctrl Pts',(-1.36355215107595,-0.653296429370576,
-6.53912347708507));
#367553=CARTESIAN_POINT('Ctrl Pts',(-1.15285655631797,-0.980033616011744,
-6.5199103475936));
#367554=CARTESIAN_POINT('Ctrl Pts',(-1.01294046321328,-1.12404277400895,
-6.50917837703663));
#367555=CARTESIAN_POINT('Ctrl Pts',(-0.688610762681138,-1.34673460120227,
-6.48738817295556));
#367556=CARTESIAN_POINT('Ctrl Pts',(-0.508237694368947,-1.42463435001778,
-6.47654608774863));
#367557=CARTESIAN_POINT('Ctrl Pts',(-0.213285115742221,-1.4886213369331,
-6.46057775888974));
#367558=CARTESIAN_POINT('Ctrl Pts',(-0.106683253673148,-1.5,-6.45513280043552));
#367559=CARTESIAN_POINT('Ctrl Pts',(8.01442245901285E-15,-1.5,-6.45));
#367560=CARTESIAN_POINT('Ctrl Pts',(1.6968042574778E-13,-1.5,-6.3875));
#367561=CARTESIAN_POINT('Ctrl Pts',(-0.165755393035949,-1.5,-6.39547491006574));
#367562=CARTESIAN_POINT('Ctrl Pts',(-0.330581797108966,-1.47253101276845,
-6.40416815155229));
#367563=CARTESIAN_POINT('Ctrl Pts',(-0.673877430137846,-1.3544808574772,
-6.42396414137767));
#367564=CARTESIAN_POINT('Ctrl Pts',(-0.845578985174142,-1.25448224127724,
-6.43500287563493));
#367565=CARTESIAN_POINT('Ctrl Pts',(-1.13544569244925,-0.998424297400548,
-6.45606181475437));
#367566=CARTESIAN_POINT('Ctrl Pts',(-1.25260337840686,-0.846786137732792,
-6.46545632568153));
#367567=CARTESIAN_POINT('Ctrl Pts',(-1.42815583912755,-0.499917375911177,
-6.4847268124494));
#367568=CARTESIAN_POINT('Ctrl Pts',(-1.48176718453481,-0.306413707829004,
-6.49547701623174));
#367569=CARTESIAN_POINT('Ctrl Pts',(-1.51011914362045,0.0858811320265719,
-6.51727117400149));
#367570=CARTESIAN_POINT('Ctrl Pts',(-1.48627148300686,0.28078934314199,
-6.52809940795235));
#367571=CARTESIAN_POINT('Ctrl Pts',(-1.3664724106079,0.647576246047647,
-6.54847645811377));
#367572=CARTESIAN_POINT('Ctrl Pts',(-1.27284707380272,0.81637051742483,
-6.55727040875927));
#367573=CARTESIAN_POINT('Ctrl Pts',(-1.02168025717648,1.11630068461384,
-6.57768607139152));
#367574=CARTESIAN_POINT('Ctrl Pts',(-0.864004598244528,1.24235271466741,
-6.5887736903482));
#367575=CARTESIAN_POINT('Ctrl Pts',(-0.515324127038387,1.42176250249477,
-6.6105331925583));
#367576=CARTESIAN_POINT('Ctrl Pts',(-0.329006976753908,1.47605584177366,
-6.62100552894422));
#367577=CARTESIAN_POINT('Ctrl Pts',(0.0581570840512136,1.51169543180713,
-6.64062295711679));
#367578=CARTESIAN_POINT('Ctrl Pts',(0.255447828508453,1.49109567670693,
-6.65003758169315));
#367579=CARTESIAN_POINT('Ctrl Pts',(0.631781586702912,1.37470695816143,
-6.67137696803598));
#367580=CARTESIAN_POINT('Ctrl Pts',(0.80701146867335,1.27972548506312,-6.68244609391585));
#367581=CARTESIAN_POINT('Ctrl Pts',(1.10509610966416,1.0319613805034,-6.70367003413006));
#367582=CARTESIAN_POINT('Ctrl Pts',(1.22687666158932,0.883693556645477,
-6.71340591351972));
#367583=CARTESIAN_POINT('Ctrl Pts',(1.41270876705042,0.54202201144847,-6.73238766603066));
#367584=CARTESIAN_POINT('Ctrl Pts',(1.4720223737034,0.350226621709424,-6.74304296546061));
#367585=CARTESIAN_POINT('Ctrl Pts',(1.5120598119248,-0.0415728267988367,
-6.76480960148885));
#367586=CARTESIAN_POINT('Ctrl Pts',(1.4938465836399,-0.237662363874076,
-6.77570346465969));
#367587=CARTESIAN_POINT('Ctrl Pts',(1.38461556434909,-0.607604161078553,
-6.79625578672661));
#367588=CARTESIAN_POINT('Ctrl Pts',(1.29628956641475,-0.778442162188688,
-6.80508896588438));
#367589=CARTESIAN_POINT('Ctrl Pts',(1.05426285246871,-1.08569323481702,
-6.82526823360582));
#367590=CARTESIAN_POINT('Ctrl Pts',(0.899880040821621,-1.21671675064297,
-6.83633552220066));
#367591=CARTESIAN_POINT('Ctrl Pts',(0.555510646549586,-1.40662016700689,
-6.85817909730662));
#367592=CARTESIAN_POINT('Ctrl Pts',(0.370281643719095,-1.46631538374509,
-6.8687491323254));
#367593=CARTESIAN_POINT('Ctrl Pts',(0.119354979579826,-1.49644258950569,
-6.88165871390939));
#367594=CARTESIAN_POINT('Ctrl Pts',(0.0596467206442825,-1.5,-6.88463024581499));
#367595=CARTESIAN_POINT('Ctrl Pts',(1.86666838024545E-13,-1.5,-6.8875));
#367596=CARTESIAN_POINT('Origin',(0.,2.16840434497101E-16,-9.7));
#367597=CARTESIAN_POINT('',(-1.0210217068046E-13,-1.5,-7.45000000000001));
#367598=CARTESIAN_POINT('',(-1.83697019872103E-16,-1.5,-7.38750000000001));
#367599=CARTESIAN_POINT('',(-1.83697019872103E-16,-1.5,-9.7));
#367600=CARTESIAN_POINT('Ctrl Pts',(-2.049402314519E-13,-1.5,-7.45000000000001));
#367601=CARTESIAN_POINT('Ctrl Pts',(0.140437042333261,-1.50000000000002,
-7.44324321965039));
#367602=CARTESIAN_POINT('Ctrl Pts',(0.280400822634887,-1.48028297751634,
-7.4359615140619));
#367603=CARTESIAN_POINT('Ctrl Pts',(0.604088942930021,-1.38689428063388,
-7.41779393164412));
#367604=CARTESIAN_POINT('Ctrl Pts',(0.779904782302742,-1.29620355229113,
-7.40681580122991));
#367605=CARTESIAN_POINT('Ctrl Pts',(1.08899436646274,-1.05054410181683,
-7.38512084805408));
#367606=CARTESIAN_POINT('Ctrl Pts',(1.21848215277776,-0.897109286002776,
-7.37483940477793));
#367607=CARTESIAN_POINT('Ctrl Pts',(1.406321603195,-0.555634949767438,-7.35586860832041));
#367608=CARTESIAN_POINT('Ctrl Pts',(1.46555412110688,-0.37228798043576,
-7.34568266557976));
#367609=CARTESIAN_POINT('Ctrl Pts',(1.51299221578371,0.0140742457643191,
-7.32421809745754));
#367610=CARTESIAN_POINT('Ctrl Pts',(1.49787704346723,0.213809752656271,
-7.31312168040798));
#367611=CARTESIAN_POINT('Ctrl Pts',(1.39197323008777,0.591661603187691,
-7.29212991093402));
#367612=CARTESIAN_POINT('Ctrl Pts',(1.3038657083438,0.766538828644638,-7.28310618956815));
#367613=CARTESIAN_POINT('Ctrl Pts',(1.06643296464032,1.07239698873722,-7.26318664135795));
#367614=CARTESIAN_POINT('Ctrl Pts',(0.919626058030341,1.20066098112188,
-7.25256050209308));
#367615=CARTESIAN_POINT('Ctrl Pts',(0.578836958715456,1.39831341033431,
-7.23067393365165));
#367616=CARTESIAN_POINT('Ctrl Pts',(0.386613340744211,1.46317483680862,
-7.21962386422901));
#367617=CARTESIAN_POINT('Ctrl Pts',(-0.00151335003668148,1.51202423354,
-7.19959318242519));
#367618=CARTESIAN_POINT('Ctrl Pts',(-0.193117885335683,1.49964389128048,
-7.1906987195008));
#367619=CARTESIAN_POINT('Ctrl Pts',(-0.566482987975544,1.40260223596492,
-7.17003958108799));
#367620=CARTESIAN_POINT('Ctrl Pts',(-0.74420899135005,1.31694443138796,
-7.15910935130334));
#367621=CARTESIAN_POINT('Ctrl Pts',(-1.05944183060186,1.08031540776268,
-7.13736967581935));
#367622=CARTESIAN_POINT('Ctrl Pts',(-1.1931273993454,0.930576214328794,
-7.12677830385444));
#367623=CARTESIAN_POINT('Ctrl Pts',(-1.39007108458186,0.594926025763823,
-7.10797923003154));
#367624=CARTESIAN_POINT('Ctrl Pts',(-1.45431316870517,0.413836933241608,
-7.09799094073564));
#367625=CARTESIAN_POINT('Ctrl Pts',(-1.5126848900854,0.0299823118952904,
-7.07666568399418));
#367626=CARTESIAN_POINT('Ctrl Pts',(-1.503457366199,-0.169512684862048,
-7.06558262861877));
#367627=CARTESIAN_POINT('Ctrl Pts',(-1.40869127483083,-0.551178404032966,
-7.04437897755372));
#367628=CARTESIAN_POINT('Ctrl Pts',(-1.32497563560172,-0.729820644777665,
-7.03514179096876));
#367629=CARTESIAN_POINT('Ctrl Pts',(-1.09537787108247,-1.04271897136768,
-7.01540364318983));
#367630=CARTESIAN_POINT('Ctrl Pts',(-0.952555765747528,-1.17462138761499,
-7.00486815543617));
#367631=CARTESIAN_POINT('Ctrl Pts',(-0.618398965905427,-1.38118758222441,
-6.98305307905755));
#367632=CARTESIAN_POINT('Ctrl Pts',(-0.428686397280591,-1.4513234117932,
-6.97197731135584));
#367633=CARTESIAN_POINT('Ctrl Pts',(-0.154267259301207,-1.49405477840375,
-6.95758733201806));
#367634=CARTESIAN_POINT('Ctrl Pts',(-0.0771108902263344,-1.5,-6.9537099994358));
#367635=CARTESIAN_POINT('Ctrl Pts',(-4.26497277117844E-14,-1.5,-6.95));
#367636=CARTESIAN_POINT('Ctrl Pts',(1.87055232414579E-13,-1.5,-6.8875));
#367637=CARTESIAN_POINT('Ctrl Pts',(-0.134476935078994,-1.5,-6.89397002455563));
#367638=CARTESIAN_POINT('Ctrl Pts',(-0.268592394842974,-1.48192102679756,
-6.90092485132217));
#367639=CARTESIAN_POINT('Ctrl Pts',(-0.589636184084624,-1.39338934895648,
-6.91883029110723));
#367640=CARTESIAN_POINT('Ctrl Pts',(-0.768209078573734,-1.30347783016702,
-6.92991942568776));
#367641=CARTESIAN_POINT('Ctrl Pts',(-1.07427176036584,-1.06407770958817,
-6.95129487668064));
#367642=CARTESIAN_POINT('Ctrl Pts',(-1.20066717458189,-0.919099539462454,
-6.96140325027485));
#367643=CARTESIAN_POINT('Ctrl Pts',(-1.39645751585126,-0.582568918544948,
-6.9801712902645));
#367644=CARTESIAN_POINT('Ctrl Pts',(-1.46130323893525,-0.392598325701134,
-6.99068898190552));
#367645=CARTESIAN_POINT('Ctrl Pts',(-1.51270095576477,-0.0014949167896889,
-7.01241694906727));
#367646=CARTESIAN_POINT('Ctrl Pts',(-1.50000567634135,0.195588578785192,
-7.02336603215476));
#367647=CARTESIAN_POINT('Ctrl Pts',(-1.40105852305377,0.568516146700469,
-7.04408423037227));
#367648=CARTESIAN_POINT('Ctrl Pts',(-1.31777927839766,0.741366900979518,
-7.05302517326762));
#367649=CARTESIAN_POINT('Ctrl Pts',(-1.08586476580297,1.05378535214069,
-7.07286145576728));
#367650=CARTESIAN_POINT('Ctrl Pts',(-0.936725907773699,1.18831479822963,
-7.08377383147779));
#367651=CARTESIAN_POINT('Ctrl Pts',(-0.599428604164675,1.38855525628651,
-7.10556429051011));
#367652=CARTESIAN_POINT('Ctrl Pts',(-0.415583281557217,1.45420272592114,
-7.11623309354135));
#367653=CARTESIAN_POINT('Ctrl Pts',(-0.0331046029529278,1.51205403693844,
-7.13624208840723));
#367654=CARTESIAN_POINT('Ctrl Pts',(0.161885171787989,1.50372875951478,
-7.14518512730597));
#367655=CARTESIAN_POINT('Ctrl Pts',(0.543135763622651,1.41225702056906,
-7.16606893659539));
#367656=CARTESIAN_POINT('Ctrl Pts',(0.725185762635119,1.32799244163293,
-7.17716850400493));
#367657=CARTESIAN_POINT('Ctrl Pts',(1.0398249511182,1.09786677591472,-7.19869896862224));
#367658=CARTESIAN_POINT('Ctrl Pts',(1.17116611133969,0.956524919258439,
-7.2089442858246));
#367659=CARTESIAN_POINT('Ctrl Pts',(1.3785991781178,0.624228926299006,-7.22815485815207));
#367660=CARTESIAN_POINT('Ctrl Pts',(1.44962349447218,0.434544642446531,
-7.23835863097522));
#367661=CARTESIAN_POINT('Ctrl Pts',(1.51216510990107,0.0427687254564257,
-7.26012395969689));
#367662=CARTESIAN_POINT('Ctrl Pts',(1.50479638433807,-0.15512427430675,
-7.27111801523929));
#367663=CARTESIAN_POINT('Ctrl Pts',(1.41573257018693,-0.530841294492776,
-7.2919911830274));
#367664=CARTESIAN_POINT('Ctrl Pts',(1.33721003007483,-0.705652812938672,
-7.30109825279054));
#367665=CARTESIAN_POINT('Ctrl Pts',(1.11397734882578,-1.02401785086592,
-7.32068201345055));
#367666=CARTESIAN_POINT('Ctrl Pts',(0.968550256288191,-1.16251792797778,
-7.33152610206678));
#367667=CARTESIAN_POINT('Ctrl Pts',(0.636394820737358,-1.372077846342,-7.35332804675424));
#367668=CARTESIAN_POINT('Ctrl Pts',(0.453877912632891,-1.44277632123166,
-7.36407324211443));
#367669=CARTESIAN_POINT('Ctrl Pts',(0.175951754616519,-1.49226334300853,
-7.37881961012036));
#367670=CARTESIAN_POINT('Ctrl Pts',(0.0879659976243163,-1.5,-7.38326773396601));
#367671=CARTESIAN_POINT('Ctrl Pts',(-1.83697019872104E-16,-1.5,-7.38750000000001));
#367672=CARTESIAN_POINT('Origin',(0.,2.16840434497101E-16,-9.7));
#367673=CARTESIAN_POINT('',(-2.56633154350194E-14,-1.5,-7.95));
#367674=CARTESIAN_POINT('',(-2.56633154350194E-14,-1.5,-7.88750000000001));
#367675=CARTESIAN_POINT('',(-1.83697019872103E-16,-1.5,-9.7));
#367676=CARTESIAN_POINT('Ctrl Pts',(-5.15212872365112E-14,-1.5,-7.95));
#367677=CARTESIAN_POINT('Ctrl Pts',(0.169649030212483,-1.50000000000001,
-7.94183775722825));
#367678=CARTESIAN_POINT('Ctrl Pts',(0.338229987551259,-1.47122377203185,
-7.93292756247082));
#367679=CARTESIAN_POINT('Ctrl Pts',(0.684455122501634,-1.34921053430319,
-7.91288054129526));
#367680=CARTESIAN_POINT('Ctrl Pts',(0.855627600158956,-1.24769800639786,
-7.90182520918234));
#367681=CARTESIAN_POINT('Ctrl Pts',(1.1491386146339,-0.984097798600795,
-7.88038142591987));
#367682=CARTESIAN_POINT('Ctrl Pts',(1.26850206005723,-0.82453111852428,
-7.87080728436246));
#367683=CARTESIAN_POINT('Ctrl Pts',(1.43632435921431,-0.473136830219077,
-7.85128537945661));
#367684=CARTESIAN_POINT('Ctrl Pts',(1.48503247678298,-0.28556062007432,
-7.84086447889301));
#367685=CARTESIAN_POINT('Ctrl Pts',(1.50955306563698,0.105242630406832,
-7.81915318719962));
#367686=CARTESIAN_POINT('Ctrl Pts',(1.48217797589332,0.304937933588397,
-7.80805900368953));
#367687=CARTESIAN_POINT('Ctrl Pts',(1.35345017162957,0.674487844230075,
-7.78752845309833));
#367688=CARTESIAN_POINT('Ctrl Pts',(1.25626583476381,0.841758623162788,
-7.77872660084614));
#367689=CARTESIAN_POINT('Ctrl Pts',(1.00247653346502,1.13259933499009,-7.75843724873241));
#367690=CARTESIAN_POINT('Ctrl Pts',(0.847530404712385,1.25276548683173,
-7.74764445097471));
#367691=CARTESIAN_POINT('Ctrl Pts',(0.496384048790409,1.42938196077102,
-7.72584390088335));
#367692=CARTESIAN_POINT('Ctrl Pts',(0.302737087598003,1.48253235258537,
-7.71505065734638));
#367693=CARTESIAN_POINT('Ctrl Pts',(-0.0850804230589879,1.50957501010104,
-7.6956405937342));
#367694=CARTESIAN_POINT('Ctrl Pts',(-0.275304145189383,1.48670218358323,
-7.68638503934947));
#367695=CARTESIAN_POINT('Ctrl Pts',(-0.643440979793326,1.36916031540728,
-7.66540799574259));
#367696=CARTESIAN_POINT('Ctrl Pts',(-0.817081372258155,1.27318210552497,
-7.65438765707932));
#367697=CARTESIAN_POINT('Ctrl Pts',(-1.11961569878932,1.01793386183373,
-7.63274173851608));
#367698=CARTESIAN_POINT('Ctrl Pts',(-1.2447834190928,0.860355903267692,
-7.62279755018153));
#367699=CARTESIAN_POINT('Ctrl Pts',(-1.42271198097539,0.512425064932855,
-7.60346805916293));
#367700=CARTESIAN_POINT('Ctrl Pts',(-1.47644279044892,0.32677812751696,
-7.59315434041761));
#367701=CARTESIAN_POINT('Ctrl Pts',(-1.5118668771993,-0.0620866185101912,
-7.5715507434161));
#367702=CARTESIAN_POINT('Ctrl Pts',(-1.49030819952901,-0.261891740745748,
-7.56045045884746));
#367703=CARTESIAN_POINT('Ctrl Pts',(-1.37235403146986,-0.635440182437178,
-7.53969776764238));
#367704=CARTESIAN_POINT('Ctrl Pts',(-1.27947126280045,-0.806282252778367,
-7.53082852725601));
#367705=CARTESIAN_POINT('Ctrl Pts',(-1.03345416187703,-1.10431373891751,
-7.5107133715763));
#367706=CARTESIAN_POINT('Ctrl Pts',(-0.882341954946408,-1.22841180962396,
-7.4999958134998));
#367707=CARTESIAN_POINT('Ctrl Pts',(-0.536802147266234,-1.41470310596347,
-7.47819626351982));
#367708=CARTESIAN_POINT('Ctrl Pts',(-0.344717144208225,-1.47334017307293,
-7.46732576208155));
#367709=CARTESIAN_POINT('Ctrl Pts',(-0.097911947230068,-1.49760595641594,
-7.45477729196818));
#367710=CARTESIAN_POINT('Ctrl Pts',(-0.0489304567307137,-1.49999999999999,
-7.45235416769708));
#367711=CARTESIAN_POINT('Ctrl Pts',(-2.04020644341047E-13,-1.5,-7.45000000000001));
#367712=CARTESIAN_POINT('Ctrl Pts',(-4.33680868994202E-16,-1.5,-7.38750000000001));
#367713=CARTESIAN_POINT('Ctrl Pts',(-0.103498290049447,-1.5,-7.39247956380173));
#367714=CARTESIAN_POINT('Ctrl Pts',(-0.206940275664367,-1.48929046845617,
-7.39775390564245));
#367715=CARTESIAN_POINT('Ctrl Pts',(-0.503643604568591,-1.42689583247804,
-7.41376223554287));
#367716=CARTESIAN_POINT('Ctrl Pts',(-0.688478575587678,-1.34746996432422,
-7.42486138634771));
#367717=CARTESIAN_POINT('Ctrl Pts',(-1.0101028052577,-1.12535794412252,
-7.44650531765147));
#367718=CARTESIAN_POINT('Ctrl Pts',(-1.14551436471142,-0.987196013291791,
-7.45685814075527));
#367719=CARTESIAN_POINT('Ctrl Pts',(-1.36075238870163,-0.661644015737823,
-7.47625689605598));
#367720=CARTESIAN_POINT('Ctrl Pts',(-1.43629940598586,-0.475909511502501,
-7.48606058269434));
#367721=CARTESIAN_POINT('Ctrl Pts',(-1.51030786796259,-0.0875699896681622,
-7.50763500057403));
#367722=CARTESIAN_POINT('Ctrl Pts',(-1.50876393250556,0.111042482143407,
-7.51866902678578));
#367723=CARTESIAN_POINT('Ctrl Pts',(-1.43047794526851,0.489709522131853,
-7.53970608456291));
#367724=CARTESIAN_POINT('Ctrl Pts',(-1.35704827088219,0.666691954518031,
-7.54906153891744));
#367725=CARTESIAN_POINT('Ctrl Pts',(-1.14316482437444,0.991323444194374,
-7.56836955241538));
#367726=CARTESIAN_POINT('Ctrl Pts',(-1.00183132950032,1.13395729188269,
-7.57913151468264));
#367727=CARTESIAN_POINT('Ctrl Pts',(-0.675468170279157,1.3533475707223,
-7.60092784391401));
#367728=CARTESIAN_POINT('Ctrl Pts',(-0.494525159301831,1.42942724371325,
-7.61174679283841));
#367729=CARTESIAN_POINT('Ctrl Pts',(-0.116649211979274,1.50765892423412,
-7.63210046006734));
#367730=CARTESIAN_POINT('Ctrl Pts',(0.076465011572568,1.51022996233389,
-7.64089475896424));
#367731=CARTESIAN_POINT('Ctrl Pts',(0.461551125383072,1.44114414373383,
-7.66134127377004));
#367732=CARTESIAN_POINT('Ctrl Pts',(0.649189784601783,1.36691817947591,
-7.6724308753114));
#367733=CARTESIAN_POINT('Ctrl Pts',(0.977966479177636,1.15348257980608,
-7.69417791806195));
#367734=CARTESIAN_POINT('Ctrl Pts',(1.11758931678336,1.01880014504509,-7.7046367037117));
#367735=CARTESIAN_POINT('Ctrl Pts',(1.34095887333867,0.700374278604906,
-7.72422873946887));
#367736=CARTESIAN_POINT('Ctrl Pts',(1.42115306908879,0.518685318835995,
-7.7336841489536));
#367737=CARTESIAN_POINT('Ctrl Pts',(1.50697056267944,0.134072157882677,
-7.75505154678434));
#367738=CARTESIAN_POINT('Ctrl Pts',(1.51152051034369,-0.0651103607297328,
-7.76611724226281));
#367739=CARTESIAN_POINT('Ctrl Pts',(1.44449799810243,-0.446754527862136,
-7.78731969599238));
#367740=CARTESIAN_POINT('Ctrl Pts',(1.3762971592515,-0.626044261873528,
-7.79700632377052));
#367741=CARTESIAN_POINT('Ctrl Pts',(1.17204880129264,-0.956993882235811,
-7.81602627248468));
#367742=CARTESIAN_POINT('Ctrl Pts',(1.03503100953311,-1.10373068000132,
-7.82669456622451));
#367743=CARTESIAN_POINT('Ctrl Pts',(0.714901685733098,-1.33301916458055,
-7.84846592006877));
#367744=CARTESIAN_POINT('Ctrl Pts',(0.535731969675832,-1.41457552668073,
-7.85935168155458));
#367745=CARTESIAN_POINT('Ctrl Pts',(0.232355588865252,-1.48648730918881,
-7.87594543399592));
#367746=CARTESIAN_POINT('Ctrl Pts',(0.11625927429028,-1.5,-7.88190647305773));
#367747=CARTESIAN_POINT('Ctrl Pts',(-5.09314812546791E-14,-1.5,-7.88750000000001));
#367748=CARTESIAN_POINT('Origin',(0.,2.16840434497101E-16,-9.7));
#367749=CARTESIAN_POINT('',(6.18620758391476E-15,-1.5,-8.45));
#367750=CARTESIAN_POINT('',(-1.06348773749651E-13,-1.5,-8.38750000000002));
#367751=CARTESIAN_POINT('',(-1.83697019872103E-16,-1.5,-9.7));
#367752=CARTESIAN_POINT('Ctrl Pts',(1.25561121877016E-14,-1.5,-8.45));
#367753=CARTESIAN_POINT('Ctrl Pts',(0.00861429778850655,-1.5,-8.44958554440441));
#367754=CARTESIAN_POINT('Ctrl Pts',(0.0172316723228776,-1.49992579396597,
-8.44916887950008));
#367755=CARTESIAN_POINT('Ctrl Pts',(0.216730498483306,-1.49648709693699,
-8.43947496838927));
#367756=CARTESIAN_POINT('Ctrl Pts',(0.405205023619677,-1.45678790405548,
-8.42930422821288));
#367757=CARTESIAN_POINT('Ctrl Pts',(0.763939328292724,-1.30602890974033,
-8.40785686608991));
#367758=CARTESIAN_POINT('Ctrl Pts',(0.929707761400483,-1.19371884349497,
-8.39676160457105));
#367759=CARTESIAN_POINT('Ctrl Pts',(1.20509608623561,-0.914035700736181,
-8.37574300142704));
#367760=CARTESIAN_POINT('Ctrl Pts',(1.31316801726847,-0.750534306911873,
-8.36669635038398));
#367761=CARTESIAN_POINT('Ctrl Pts',(1.46058931529617,-0.392388022013749,
-8.34679933455631));
#367762=CARTESIAN_POINT('Ctrl Pts',(1.49891489916418,-0.201314907576628,
-8.33618416153202));
#367763=CARTESIAN_POINT('Ctrl Pts',(1.50108200612855,0.19249826939769,-8.31430565170012));
#367764=CARTESIAN_POINT('Ctrl Pts',(1.46187352216226,0.391466615992827,
-8.30325185466706));
#367765=CARTESIAN_POINT('Ctrl Pts',(1.31144926331368,0.752556761797094,
-8.28319129101127));
#367766=CARTESIAN_POINT('Ctrl Pts',(1.20547352871805,0.912732494481734,
-8.27431135845658));
#367767=CARTESIAN_POINT('Ctrl Pts',(0.935743303605986,1.18850887613864,
-8.25367350190414));
#367768=CARTESIAN_POINT('Ctrl Pts',(0.77316273312452,1.30014676725224,-8.24275028802884));
#367769=CARTESIAN_POINT('Ctrl Pts',(0.411255019791086,1.45614895662291,
-8.22100460090341));
#367770=CARTESIAN_POINT('Ctrl Pts',(0.214882025841304,1.49778257196538,
-8.21040011151181));
#367771=CARTESIAN_POINT('Ctrl Pts',(-0.174206396355913,1.50195375454829,
-8.19156421988777));
#367772=CARTESIAN_POINT('Ctrl Pts',(-0.363222433697757,1.467764624521,-8.1816290254141));
#367773=CARTESIAN_POINT('Ctrl Pts',(-0.725242470020206,1.32782064009227,
-8.16032399539473));
#367774=CARTESIAN_POINT('Ctrl Pts',(-0.893747788845163,1.22077963681101,
-8.14924341826052));
#367775=CARTESIAN_POINT('Ctrl Pts',(-1.17806984563516,0.948915230794823,
-8.12801217786916));
#367776=CARTESIAN_POINT('Ctrl Pts',(-1.2916501441798,0.787348491302205,
-8.11874158285011));
#367777=CARTESIAN_POINT('Ctrl Pts',(-1.4491496887938,0.432498074699068,
-8.09902767081661));
#367778=CARTESIAN_POINT('Ctrl Pts',(-1.49264245272113,0.243084388697504,
-8.08850468826097));
#367779=CARTESIAN_POINT('Ctrl Pts',(-1.50590393515616,-0.149395073754563,
-8.0667002736803));
#367780=CARTESIAN_POINT('Ctrl Pts',(-1.47255346733907,-0.348807606776928,
-8.0556217996235));
#367781=CARTESIAN_POINT('Ctrl Pts',(-1.33283856573897,-0.714141759724103,
-8.0353254577931));
#367782=CARTESIAN_POINT('Ctrl Pts',(-1.23122919841274,-0.877800908019311,
-8.02652085053871));
#367783=CARTESIAN_POINT('Ctrl Pts',(-0.969415363518022,-1.16111510898422,
-8.00605448761852));
#367784=CARTESIAN_POINT('Ctrl Pts',(-0.810585245633811,-1.27706577719137,
-7.99519191811422));
#367785=CARTESIAN_POINT('Ctrl Pts',(-0.453893095493189,-1.44343242172073,
-7.97340926335772));
#367786=CARTESIAN_POINT('Ctrl Pts',(-0.25879168041917,-1.49082770289231,
-7.96270590656026));
#367787=CARTESIAN_POINT('Ctrl Pts',(-0.0400632634351528,-1.4995990138221,
-7.95193868316567));
#367788=CARTESIAN_POINT('Ctrl Pts',(-0.0200247189458719,-1.5,-7.95096343973948));
#367789=CARTESIAN_POINT('Ctrl Pts',(-5.11429338501666E-14,-1.5,-7.95));
#367790=CARTESIAN_POINT('Ctrl Pts',(-5.11429338501666E-14,-1.5,-7.88750000000001));
#367791=CARTESIAN_POINT('Ctrl Pts',(-0.0736320868157455,-1.5,-7.89104262542868));
#367792=CARTESIAN_POINT('Ctrl Pts',(-0.147314902069754,-1.49457904917319,
-7.89473827349793));
#367793=CARTESIAN_POINT('Ctrl Pts',(-0.418702927434066,-1.45425447866906,
-7.90891556291462));
#367794=CARTESIAN_POINT('Ctrl Pts',(-0.609025848846148,-1.38536633060707,
-7.91998603840886));
#367795=CARTESIAN_POINT('Ctrl Pts',(-0.944782138143701,-1.18090318746338,
-7.94181965216352));
#367796=CARTESIAN_POINT('Ctrl Pts',(-1.08856096172562,-1.04985610672164,
-7.95237741072569));
#367797=CARTESIAN_POINT('Ctrl Pts',(-1.32003136507659,-0.738631619722692,
-7.97215916033823));
#367798=CARTESIAN_POINT('Ctrl Pts',(-1.40480022985449,-0.560896232853786,
-7.98133909817484));
#367799=CARTESIAN_POINT('Ctrl Pts',(-1.50224046510422,-0.180131641157084,
-8.00249268660243));
#367800=CARTESIAN_POINT('Ctrl Pts',(-1.51287518985252,0.0194362765722913,
-8.01357979314295));
#367801=CARTESIAN_POINT('Ctrl Pts',(-1.45710848051361,0.403943219053963,
-8.03494128994749));
#367802=CARTESIAN_POINT('Ctrl Pts',(-1.3940497063946,0.585578769316464,
-8.04502816248795));
#367803=CARTESIAN_POINT('Ctrl Pts',(-1.19928932849217,0.922619535335456,
-8.06376081903927));
#367804=CARTESIAN_POINT('Ctrl Pts',(-1.06660917766218,1.07323780149619,
-8.07432823649911));
#367805=CARTESIAN_POINT('Ctrl Pts',(-0.752867300763901,1.31203272481169,
-8.0960563419037));
#367806=CARTESIAN_POINT('Ctrl Pts',(-0.575589044828377,1.39890746718006,
-8.10699883325719));
#367807=CARTESIAN_POINT('Ctrl Pts',(-0.202819353943747,1.49835135182648,
-8.12769605350109));
#367808=CARTESIAN_POINT('Ctrl Pts',(-0.0113908336243939,1.51197052822358,
-8.1366194435889));
#367809=CARTESIAN_POINT('Ctrl Pts',(0.375011792040734,1.46592391911218,
-8.15648932105949));
#367810=CARTESIAN_POINT('Ctrl Pts',(0.565863175268461,1.40333444856677,
-8.16741025892034));
#367811=CARTESIAN_POINT('Ctrl Pts',(0.907166874920003,1.21013321233666,
-8.1891979418325));
#367812=CARTESIAN_POINT('Ctrl Pts',(1.05543618606226,1.08325598596651,-8.19985591979005));
#367813=CARTESIAN_POINT('Ctrl Pts',(1.29576961923913,0.780029096600294,
-8.21984193663411));
#367814=CARTESIAN_POINT('Ctrl Pts',(1.38549433300877,0.606526026137088,
-8.2288041096591));
#367815=CARTESIAN_POINT('Ctrl Pts',(1.49548781765011,0.230114298782428,
-8.24971587228992));
#367816=CARTESIAN_POINT('Ctrl Pts',(1.51278175429125,0.030332685950176,
-8.2608148507806));
#367817=CARTESIAN_POINT('Ctrl Pts',(1.46939831026169,-0.356917622094825,
-8.2823287567831));
#367818=CARTESIAN_POINT('Ctrl Pts',(1.41201871989969,-0.541061483730698,
-8.29255897131843));
#367819=CARTESIAN_POINT('Ctrl Pts',(1.22663389120196,-0.886385431748862,
-8.31174363509721));
#367820=CARTESIAN_POINT('Ctrl Pts',(1.09709178138546,-1.04246898246255,
-8.32200695212607));
#367821=CARTESIAN_POINT('Ctrl Pts',(0.78788982081973,-1.29138352291927,
-8.34379773118042));
#367822=CARTESIAN_POINT('Ctrl Pts',(0.612524884090505,-1.38320591296693,
-8.35478560257844));
#367823=CARTESIAN_POINT('Ctrl Pts',(0.286398521866563,-1.47942465534937,
-8.37314910734072));
#367824=CARTESIAN_POINT('Ctrl Pts',(0.14346092522985,-1.50000000000002,
-8.3805977330167));
#367825=CARTESIAN_POINT('Ctrl Pts',(-2.12746487093796E-13,-1.5,-8.38750000000002));
#367826=CARTESIAN_POINT('Origin',(0.,2.16840434497101E-16,-9.7));
#367827=CARTESIAN_POINT('',(1.03858078175315E-13,-1.5,-8.94999999999999));
#367828=CARTESIAN_POINT('',(-1.50468077620414E-14,-1.5,-8.88750000000001));
#367829=CARTESIAN_POINT('',(-1.83697019872103E-16,-1.5,-9.7));
#367830=CARTESIAN_POINT('Ctrl Pts',(2.07899853370503E-13,-1.5,-8.94999999999999));
#367831=CARTESIAN_POINT('Ctrl Pts',(0.0372649113391745,-1.5,-8.94820709111724));
#367832=CARTESIAN_POINT('Ctrl Pts',(0.0745695358632018,-1.49861137275991,
-8.9463736985541));
#367833=CARTESIAN_POINT('Ctrl Pts',(0.30329600300598,-1.48151031632727,
-8.93489406192744));
#367834=CARTESIAN_POINT('Ctrl Pts',(0.490209627590489,-1.43057183543788,
-8.9244862181692));
#367835=CARTESIAN_POINT('Ctrl Pts',(0.841405977044156,-1.25770957002068,
-8.90278754633298));
#367836=CARTESIAN_POINT('Ctrl Pts',(1.00104516758194,-1.13477656415575,
-8.89169209647867));
#367837=CARTESIAN_POINT('Ctrl Pts',(1.25783645012521,-0.839435377793257,
-8.87113329829344));
#367838=CARTESIAN_POINT('Ctrl Pts',(1.35476199033148,-0.671881071606827,
-8.86232672620036));
#367839=CARTESIAN_POINT('Ctrl Pts',(1.48102174625321,-0.307065382477598,
-8.84205918791541));
#367840=CARTESIAN_POINT('Ctrl Pts',(1.50829154998946,-0.112958337924697,
-8.83127546321802));
#367841=CARTESIAN_POINT('Ctrl Pts',(1.48708764335021,0.279467001944457,
-8.80947405544752));
#367842=CARTESIAN_POINT('Ctrl Pts',(1.43699109229512,0.473930153689053,
-8.79867054701726));
#367843=CARTESIAN_POINT('Ctrl Pts',(1.26775400370753,0.823927635892113,
-8.77922624245043));
#367844=CARTESIAN_POINT('Ctrl Pts',(1.15338312850122,0.977641779435656,
-8.77000212221447));
#367845=CARTESIAN_POINT('Ctrl Pts',(0.868506079734434,1.23866287308289,
-8.74904538288054));
#367846=CARTESIAN_POINT('Ctrl Pts',(0.699004118880926,1.34163326918927,
-8.73802992720589));
#367847=CARTESIAN_POINT('Ctrl Pts',(0.327026154934649,1.47745730690498,
-8.71636023913459));
#367848=CARTESIAN_POINT('Ctrl Pts',(0.127832000440199,1.50779735873836,
-8.70636691328704));
#367849=CARTESIAN_POINT('Ctrl Pts',(-0.262690489890152,1.48918065627799,
-8.68706076058674));
#367850=CARTESIAN_POINT('Ctrl Pts',(-0.450421298277766,1.44352492164979,
-8.67676034300615));
#367851=CARTESIAN_POINT('Ctrl Pts',(-0.805330745648177,1.28101962154612,
-8.65517071814405));
#367852=CARTESIAN_POINT('Ctrl Pts',(-0.967936513681968,1.16304646733895,
-8.64407031242057));
#367853=CARTESIAN_POINT('Ctrl Pts',(-1.23351437923819,0.875004344501689,
-8.62329152132761));
#367854=CARTESIAN_POINT('Ctrl Pts',(-1.33565592983522,0.709373834332001,
-8.61440965746288));
#367855=CARTESIAN_POINT('Ctrl Pts',(-1.47194853413449,0.347677667547077,
-8.59431542597483));
#367856=CARTESIAN_POINT('Ctrl Pts',(-1.50449152991188,0.154931586657638,
-8.58360731036986));
#367857=CARTESIAN_POINT('Ctrl Pts',(-1.49437825522114,-0.237436947311771,
-8.56180905848267));
#367858=CARTESIAN_POINT('Ctrl Pts',(-1.4497751209325,-0.433260028587922,
-8.55092999841177));
#367859=CARTESIAN_POINT('Ctrl Pts',(-1.29039062376177,-0.788038602079775,
-8.53122007766222));
#367860=CARTESIAN_POINT('Ctrl Pts',(-1.18029367557154,-0.945003126011328,
-8.52220348577584));
#367861=CARTESIAN_POINT('Ctrl Pts',(-0.903110269139051,-1.21357556860263,
-8.50140714728842));
#367862=CARTESIAN_POINT('Ctrl Pts',(-0.737079841084386,-1.321015807329,
-8.49043455351843));
#367863=CARTESIAN_POINT('Ctrl Pts',(-0.378368345440081,-1.46390916922604,
-8.46920677858477));
#367864=CARTESIAN_POINT('Ctrl Pts',(-0.189979927018365,-1.5,-8.45914041350039));
#367865=CARTESIAN_POINT('Ctrl Pts',(1.30798150088651E-14,-1.5,-8.45));
#367866=CARTESIAN_POINT('Ctrl Pts',(-2.12513850479429E-13,-1.5,-8.38750000000002));
#367867=CARTESIAN_POINT('Ctrl Pts',(-0.0458918994678753,-1.49999999999999,
-8.38970797504262));
#367868=CARTESIAN_POINT('Ctrl Pts',(-0.0918317158667109,-1.49789404547631,
-8.39197675422648));
#367869=CARTESIAN_POINT('Ctrl Pts',(-0.335732616452112,-1.47541280668582,
-8.40433592063249));
#367870=CARTESIAN_POINT('Ctrl Pts',(-0.528166235830199,-1.41794905611572,
-8.41519060275519));
#367871=CARTESIAN_POINT('Ctrl Pts',(-0.874931563379712,-1.23371868116764,
-8.43699186777094));
#367872=CARTESIAN_POINT('Ctrl Pts',(-1.02687455944189,-1.1104542542655,
-8.44772624043583));
#367873=CARTESIAN_POINT('Ctrl Pts',(-1.27456475548438,-0.813962270949951,
-8.46787912897466));
#367874=CARTESIAN_POINT('Ctrl Pts',(-1.36837494747328,-0.64389549964342,
-8.47672802779765));
#367875=CARTESIAN_POINT('Ctrl Pts',(-1.48865925982964,-0.271199995133596,
-8.49743333360375));
#367876=CARTESIAN_POINT('Ctrl Pts',(-1.51147180590034,-0.0714047240208655,
-8.50853307088779));
#367877=CARTESIAN_POINT('Ctrl Pts',(-1.47839353742528,0.317903564515033,
-8.53016130913978));
#367878=CARTESIAN_POINT('Ctrl Pts',(-1.42574097855776,0.503978159891549,
-8.5404987866607));
#367879=CARTESIAN_POINT('Ctrl Pts',(-1.2499967564876,0.852664344843762,
-8.55987024138027));
#367880=CARTESIAN_POINT('Ctrl Pts',(-1.12609565658542,1.01067536499336,
-8.56972834648909));
#367881=CARTESIAN_POINT('Ctrl Pts',(-0.825513299539681,1.26775118754061,
-8.59133111695601));
#367882=CARTESIAN_POINT('Ctrl Pts',(-0.652393827643045,1.3649353924963,
-8.6023598926799));
#367883=CARTESIAN_POINT('Ctrl Pts',(-0.284896137119151,1.48489483651446,
-8.62337334033739));
#367884=CARTESIAN_POINT('Ctrl Pts',(-0.0948174301912979,1.50899482999332,
-8.63268823787429));
#367885=CARTESIAN_POINT('Ctrl Pts',(0.293161477204924,1.48445475357866,
-8.65203655054902));
#367886=CARTESIAN_POINT('Ctrl Pts',(0.487140999572001,1.43255739996276,
-8.66281098782634));
#367887=CARTESIAN_POINT('Ctrl Pts',(0.839523777297171,1.25816376717198,
-8.68460927970198));
#367888=CARTESIAN_POINT('Ctrl Pts',(0.995327430827507,1.13890752447603,
-8.69541805988573));
#367889=CARTESIAN_POINT('Ctrl Pts',(1.25087470635368,0.849706080390263,
-8.71574645735887));
#367890=CARTESIAN_POINT('Ctrl Pts',(1.34902893073365,0.68323363120199,-8.7245425760444));
#367891=CARTESIAN_POINT('Ctrl Pts',(1.48017523509372,0.314599449042532,
-8.74502225283104));
#367892=CARTESIAN_POINT('Ctrl Pts',(1.508862114537,0.11495148166446,-8.75611380657427));
#367893=CARTESIAN_POINT('Ctrl Pts',(1.48680827499995,-0.276247092765537,
-8.77784706070926));
#367894=CARTESIAN_POINT('Ctrl Pts',(1.43924029795828,-0.464239223595349,
-8.78829106797759));
#367895=CARTESIAN_POINT('Ctrl Pts',(1.27368875643019,-0.81640079493658,
-8.80785559971877));
#367896=CARTESIAN_POINT('Ctrl Pts',(1.15560994852043,-0.976409685917739,
-8.81735651503753));
#367897=CARTESIAN_POINT('Ctrl Pts',(0.864123079281189,-1.24185056708233,
-8.8387540413827));
#367898=CARTESIAN_POINT('Ctrl Pts',(0.693524972739318,-1.34459027887538,
-8.84981582749377));
#367899=CARTESIAN_POINT('Ctrl Pts',(0.3448599190496,-1.47007278833151,-8.8700766079735));
#367900=CARTESIAN_POINT('Ctrl Pts',(0.173006288184303,-1.5,-8.87917623107878));
#367901=CARTESIAN_POINT('Ctrl Pts',(-3.00454106039183E-14,-1.5,-8.88750000000001));
#367902=CARTESIAN_POINT('Origin',(0.,0.,0.));
#367903=CARTESIAN_POINT('',(1.,-0.577350269189625,0.));
#367904=CARTESIAN_POINT('',(1.,0.577350269189625,0.));
#367905=CARTESIAN_POINT('Ctrl Pts',(1.,0.577350269189567,-2.89100513080514E-14));
#367906=CARTESIAN_POINT('Ctrl Pts',(1.,0.,-0.288675134594789));
#367907=CARTESIAN_POINT('Ctrl Pts',(1.,-0.577350269189567,-2.89669235401328E-14));
#367908=CARTESIAN_POINT('Origin',(0.,0.,0.));
#367909=CARTESIAN_POINT('Origin',(-9.08513196663917E-30,1.30104260698261E-15,
-2.72083333333333));
#367910=CARTESIAN_POINT('',(1.92031473636372E-14,-2.75,-1.275));
#367911=CARTESIAN_POINT('Origin',(0.,0.,-1.275));
#367912=CARTESIAN_POINT('',(1.48387956900833E-14,-1.5,0.));
#367913=CARTESIAN_POINT('Origin',(0.,0.,0.));
#367914=CARTESIAN_POINT('Origin',(0.,-6.07153216591882E-15,-1.275));
#367915=CARTESIAN_POINT('',(3.5,-6.5001585456204E-15,-1.7));
#367916=CARTESIAN_POINT('Origin',(0.,-6.07153216591882E-15,-1.7));
#367917=CARTESIAN_POINT('',(3.5,-6.5001585456204E-15,-1.275));
#367918=CARTESIAN_POINT('',(3.5,-6.5001585456204E-15,-1.275));
#367919=CARTESIAN_POINT('Origin',(0.,-6.07153216591882E-15,-1.275));
#367920=CARTESIAN_POINT('Origin',(0.,2.16840434497101E-16,-9.7));
#367921=CARTESIAN_POINT('',(1.5,1.26953349192158E-14,-9.325));
#367922=CARTESIAN_POINT('Ctrl Pts',(-0.190653686693144,-1.15967294634849,
-9.64975952641927));
#367923=CARTESIAN_POINT('Ctrl Pts',(-0.0285031007229647,-1.21316517876327,
-9.62328078572229));
#367924=CARTESIAN_POINT('Ctrl Pts',(0.132806008053662,-1.22453687890282,
-9.60193243194212));
#367925=CARTESIAN_POINT('Ctrl Pts',(0.434592435142101,-1.20145478370504,
-9.55661911842553));
#367926=CARTESIAN_POINT('Ctrl Pts',(0.585956558405005,-1.16172879077905,
-9.53296252240899));
#367927=CARTESIAN_POINT('Ctrl Pts',(0.869444002206283,-1.02932614938086,
-9.48665581615357));
#367928=CARTESIAN_POINT('Ctrl Pts',(0.998917957166605,-0.936991063680698,
-9.46438835594032));
#367929=CARTESIAN_POINT('Ctrl Pts',(1.23902375947727,-0.688929844127107,
-9.41953944808946));
#367930=CARTESIAN_POINT('Ctrl Pts',(1.32213455554229,-0.544623881037455,
-9.40019228876427));
#367931=CARTESIAN_POINT('Ctrl Pts',(1.43760433325456,-0.296768134705317,
-9.36480861464899));
#367932=CARTESIAN_POINT('Ctrl Pts',(1.48023592847381,-0.150359031185724,
-9.34476407152631));
#367933=CARTESIAN_POINT('Ctrl Pts',(1.50000000000017,1.24646820642837E-12,
-9.32499999999983));
#367934=CARTESIAN_POINT('',(1.05094390383308,-1.0702882373436,-9.325));
#367935=CARTESIAN_POINT('Origin',(0.,2.06676039130049E-16,-9.325));
#367936=CARTESIAN_POINT('',(1.21964286610306E-11,1.30188293868178,-9.52311706131822));
#367937=CARTESIAN_POINT('Ctrl Pts',(1.05094390383308,-1.0702882373436,-9.325));
#367938=CARTESIAN_POINT('Ctrl Pts',(0.968016858591267,-1.14634172204288,
-9.32883501505143));
#367939=CARTESIAN_POINT('Ctrl Pts',(0.876722528496159,-1.21272862092496,
-9.33278379259671));
#367940=CARTESIAN_POINT('Ctrl Pts',(0.682284006851511,-1.32283847967238,
-9.3407082862428));
#367941=CARTESIAN_POINT('Ctrl Pts',(0.579933643683517,-1.36652156451929,
-9.34465804140652));
#367942=CARTESIAN_POINT('Ctrl Pts',(0.280932987527152,-1.4562425328007,
-9.35560555159769));
#367943=CARTESIAN_POINT('Ctrl Pts',(0.0977811463329117,-1.46852820111501,
-9.3614595719435));
#367944=CARTESIAN_POINT('Ctrl Pts',(-0.246256444951042,-1.44391378849632,
-9.37251106997738));
#367945=CARTESIAN_POINT('Ctrl Pts',(-0.430540842049319,-1.39313332243859,
-9.37917748919023));
#367946=CARTESIAN_POINT('Ctrl Pts',(-0.762425243253192,-1.22606064184007,
-9.39275094465158));
#367947=CARTESIAN_POINT('Ctrl Pts',(-0.908108296131221,-1.11378854845243,
-9.39951694367669));
#367948=CARTESIAN_POINT('Ctrl Pts',(-1.13479032378965,-0.857402666085909,
-9.41172780093104));
#367949=CARTESIAN_POINT('Ctrl Pts',(-1.23935650826235,-0.698870792205104,
-9.41759745728602));
#367950=CARTESIAN_POINT('Ctrl Pts',(-1.3666521923041,-0.328284329478432,
-9.43139532516328));
#367951=CARTESIAN_POINT('Ctrl Pts',(-1.39110799634833,-0.145328529779098,
-9.43829819428533));
#367952=CARTESIAN_POINT('Ctrl Pts',(-1.36804302987891,0.208327411726666,
-9.45185416355787));
#367953=CARTESIAN_POINT('Ctrl Pts',(-1.32502441327286,0.376015034876667,
-9.45837881792392));
#367954=CARTESIAN_POINT('Ctrl Pts',(-1.21566879613637,0.610056988684251,
-9.46760725983284));
#367955=CARTESIAN_POINT('Ctrl Pts',(-1.17108914819411,0.686181342639889,
-9.47051827587565));
#367956=CARTESIAN_POINT('Ctrl Pts',(-1.01610091220513,0.89886764355412,
-9.47976483332994));
#367957=CARTESIAN_POINT('Ctrl Pts',(-0.885644382509459,1.01880653830682,
-9.48649835405591));
#367958=CARTESIAN_POINT('Ctrl Pts',(-0.592130096913835,1.19705002479627,
-9.50008644802564));
#367959=CARTESIAN_POINT('Ctrl Pts',(-0.433365879600623,1.25618399199256,
-9.50680144369053));
#367960=CARTESIAN_POINT('Ctrl Pts',(-0.197295674427518,1.2960635134121,
-9.51595358432894));
#367961=CARTESIAN_POINT('Ctrl Pts',(-0.105956107225097,1.30560664395967,
-9.51939335604232));
#367962=CARTESIAN_POINT('Ctrl Pts',(2.43930167567386E-11,1.30188293868178,
-9.52311706131822));
#367963=CARTESIAN_POINT('',(-1.37772764904077E-16,1.125,-9.7));
#367964=CARTESIAN_POINT('',(-1.37772764904077E-16,1.125,-9.7));
#367965=CARTESIAN_POINT('Origin',(0.,2.16840434497101E-16,-9.7));
#367966=CARTESIAN_POINT('Ctrl Pts',(2.43930167567386E-11,1.30188293868178,
-9.52311706131822));
#367967=CARTESIAN_POINT('Ctrl Pts',(0.0761076165708164,1.29920822421006,
-9.52579177578852));
#367968=CARTESIAN_POINT('Ctrl Pts',(0.159739133609348,1.28946730994931,
-9.52888182473693));
#367969=CARTESIAN_POINT('Ctrl Pts',(0.40287502943865,1.23198478745045,-9.53853482060624));
#367970=CARTESIAN_POINT('Ctrl Pts',(0.549010376213962,1.16703886874139,
-9.54503863078224));
#367971=CARTESIAN_POINT('Ctrl Pts',(0.818389915914693,0.981050906469348,
-9.55859771056026));
#367972=CARTESIAN_POINT('Ctrl Pts',(0.93687656106349,0.858483479453949,
-9.56552845851573));
#367973=CARTESIAN_POINT('Ctrl Pts',(1.116008365168,0.579288345692445,-9.57818164518354));
#367974=CARTESIAN_POINT('Ctrl Pts',(1.17614262990486,0.427743363043572,
-9.58411524905681));
#367975=CARTESIAN_POINT('Ctrl Pts',(1.23203342741208,0.114644612869533,
-9.59739583493339));
#367976=CARTESIAN_POINT('Ctrl Pts',(1.22994817565386,-0.0419119689212186,
-9.60414125823576));
#367977=CARTESIAN_POINT('Ctrl Pts',(1.161346903398,-0.374697918051623,-9.61872246149687));
#367978=CARTESIAN_POINT('Ctrl Pts',(1.08803701736073,-0.523098651946534,
-9.62519803010312));
#367979=CARTESIAN_POINT('Ctrl Pts',(0.926562190370942,-0.75996639628023,
-9.63638853623501));
#367980=CARTESIAN_POINT('Ctrl Pts',(0.816715032446504,-0.868035363199342,
-9.64294180913862));
#367981=CARTESIAN_POINT('Ctrl Pts',(0.689217670442766,-0.951929185124573,
-9.64975952641917));
#367982=CARTESIAN_POINT('Origin',(0.,2.16840434497101E-16,-9.7));
#367983=CARTESIAN_POINT('Ctrl Pts',(-2.99099185042107E-14,-1.5,-8.88750000000001));
#367984=CARTESIAN_POINT('Ctrl Pts',(-0.016764684548797,-1.5,-8.88830659126143));
#367985=CARTESIAN_POINT('Ctrl Pts',(-0.0335394535524549,-1.49971894682661,
-8.88912147474409));
#367986=CARTESIAN_POINT('Ctrl Pts',(-0.249045952375023,-1.49248573428552,
-8.89969095857362));
#367987=CARTESIAN_POINT('Ctrl Pts',(-0.444445184321647,-1.44636830249076,
-8.91037314827601));
#367988=CARTESIAN_POINT('Ctrl Pts',(-0.802322896738174,-1.28229148655965,
-8.93214923707415));
#367989=CARTESIAN_POINT('Ctrl Pts',(-0.961996620200093,-1.16728937111781,
-8.94302604588281));
#367990=CARTESIAN_POINT('Ctrl Pts',(-1.22557574019166,-0.885646162997747,
-8.96353092465391));
#367991=CARTESIAN_POINT('Ctrl Pts',(-1.32815830670805,-0.722770501492501,
-8.9723460832505));
#367992=CARTESIAN_POINT('Ctrl Pts',(-1.47027232381364,-0.358375675815785,
-8.99259024023253));
#367993=CARTESIAN_POINT('Ctrl Pts',(-1.50493256730985,-0.159048108768436,
-9.00366399395739));
#367994=CARTESIAN_POINT('Ctrl Pts',(-1.49414680166945,0.23375615123113,
-9.02548645284625));
#367995=CARTESIAN_POINT('Ctrl Pts',(-1.45180469463996,0.423553061262505,
-9.03603072562577));
#367996=CARTESIAN_POINT('Ctrl Pts',(-1.29656150195308,0.779148072440641,
-9.05578600402455));
#367997=CARTESIAN_POINT('Ctrl Pts',(-1.18422609999239,0.941149075529152,
-9.06500025840822));
#367998=CARTESIAN_POINT('Ctrl Pts',(-0.901907738019758,1.21478504099838,
-9.08618430597254));
#367999=CARTESIAN_POINT('Ctrl Pts',(-0.734004107147856,1.32301696951808,
-9.09726901563823));
#368000=CARTESIAN_POINT('Ctrl Pts',(-0.37267916446526,1.46540646275545,
-9.1186085337495));
#368001=CARTESIAN_POINT('Ctrl Pts',(-0.183777280373563,1.5008253247504,
-9.12863508578802));
#368002=CARTESIAN_POINT('Ctrl Pts',(0.205421062548106,1.49910838576655,
-9.14740809254207));
#368003=CARTESIAN_POINT('Ctrl Pts',(0.402044492391625,1.45871762005048,
-9.1579901074355));
#368004=CARTESIAN_POINT('Ctrl Pts',(0.765033707725997,1.30496455179117,
-9.17972535276377));
#368005=CARTESIAN_POINT('Ctrl Pts',(0.92840545307133,1.19426902615948,-9.19066045523852));
#368006=CARTESIAN_POINT('Ctrl Pts',(1.19982948118002,0.920120487096611,
-9.2113345870758));
#368007=CARTESIAN_POINT('Ctrl Pts',(1.30674059259681,0.760680194257607,
-9.22023998920799));
#368008=CARTESIAN_POINT('Ctrl Pts',(1.4594399044428,0.400508372435874,-9.24024953486476));
#368009=CARTESIAN_POINT('Ctrl Pts',(1.49989618200679,0.201656004166217,
-9.25129688865752));
#368010=CARTESIAN_POINT('Ctrl Pts',(1.50009944355299,-0.192401669391178,
-9.27318898163292));
#368011=CARTESIAN_POINT('Ctrl Pts',(1.46288142732614,-0.383810092514896,
-9.28382278291757));
#368012=CARTESIAN_POINT('Ctrl Pts',(1.35231292083348,-0.656914113380578,
-9.29899522852122));
#368013=CARTESIAN_POINT('Ctrl Pts',(1.30483483328299,-0.746784757003529,
-9.30379845917422));
#368014=CARTESIAN_POINT('Ctrl Pts',(1.19118218895726,-0.91751820480455,
-9.3140091703461));
#368015=CARTESIAN_POINT('Ctrl Pts',(1.12492471439177,-0.997644552077798,
-9.31942271644616));
#368016=CARTESIAN_POINT('Ctrl Pts',(1.05094390383308,-1.07028823734361,
-9.325));
#368017=CARTESIAN_POINT('Ctrl Pts',(1.5,2.08513761812412E-14,-9.325));
#368018=CARTESIAN_POINT('Ctrl Pts',(1.5,0.12960195655018,-9.31779989130277));
#368019=CARTESIAN_POINT('Ctrl Pts',(1.48320505460745,0.258655672138285,
-9.31063024043674));
#368020=CARTESIAN_POINT('Ctrl Pts',(1.41793481240152,0.505154131452618,
-9.29693588158595));
#368021=CARTESIAN_POINT('Ctrl Pts',(1.37076777116574,0.621871157175992,
-9.2904516023791));
#368022=CARTESIAN_POINT('Ctrl Pts',(1.21686069124155,0.897465020181764,
-9.27514083221211));
#368023=CARTESIAN_POINT('Ctrl Pts',(1.09331169914294,1.04446688461033,-9.26525568130039));
#368024=CARTESIAN_POINT('Ctrl Pts',(0.792105738691596,1.28903984869781,
-9.24397020932451));
#368025=CARTESIAN_POINT('Ctrl Pts',(0.615567738611666,1.38207633547858,
-9.23289217398046));
#368026=CARTESIAN_POINT('Ctrl Pts',(0.238269039661259,1.49385235718827,
-9.21163449237153));
#368027=CARTESIAN_POINT('Ctrl Pts',(0.0414182077513572,1.51216394019312,
-9.20233062167712));
#368028=CARTESIAN_POINT('Ctrl Pts',(-0.344911503806603,1.4724470676907,
-9.18264007830506));
#368029=CARTESIAN_POINT('Ctrl Pts',(-0.530828562312111,1.41607458027076,
-9.1721292372288));
#368030=CARTESIAN_POINT('Ctrl Pts',(-0.877887868290141,1.23261868646805,
-9.15033534153446));
#368031=CARTESIAN_POINT('Ctrl Pts',(-1.03431538205672,1.10464573789137,
-9.13925441514218));
#368032=CARTESIAN_POINT('Ctrl Pts',(-1.28197696314223,0.80188845513952,
-9.11892886724566));
#368033=CARTESIAN_POINT('Ctrl Pts',(-1.37356108825293,0.63231503049334,
-9.11012861280517));
#368034=CARTESIAN_POINT('Ctrl Pts',(-1.48931778815661,0.264311081277164,
-9.08968394895983));
#368035=CARTESIAN_POINT('Ctrl Pts',(-1.51101519260302,0.0689319743571016,
-9.07882955413094));
#368036=CARTESIAN_POINT('Ctrl Pts',(-1.47819153152631,-0.323214650039326,
-9.05704363055336));
#368037=CARTESIAN_POINT('Ctrl Pts',(-1.42239168475186,-0.516085078045942,
-9.04632860677521));
#368038=CARTESIAN_POINT('Ctrl Pts',(-1.24289975815323,-0.860977276769388,
-9.02716792906835));
#368039=CARTESIAN_POINT('Ctrl Pts',(-1.12398358187228,-1.01132277704982,
-9.01765205260071));
#368040=CARTESIAN_POINT('Ctrl Pts',(-0.830981507794516,-1.2642343798264,
-8.99652966143954));
#368041=CARTESIAN_POINT('Ctrl Pts',(-0.657919660216403,-1.36233668602944,
-8.98547815535453));
#368042=CARTESIAN_POINT('Ctrl Pts',(-0.318701383774487,-1.4744861624803,
-8.96604224518497));
#368043=CARTESIAN_POINT('Ctrl Pts',(-0.159749516444619,-1.5,-8.95768595219353));
#368044=CARTESIAN_POINT('Ctrl Pts',(2.07899853370503E-13,-1.5,-8.94999999999999));
#368045=CARTESIAN_POINT('Origin',(-1.04744440165294E-14,-1.5,-9.7));
#368046=CARTESIAN_POINT('Origin',(1.92031473636372E-14,-2.75,-1.7));
#368047=CARTESIAN_POINT('',(-0.823407874165093,-0.838564036615816,-1.7));
#368048=CARTESIAN_POINT('Ctrl Pts',(-0.823407874165095,-0.838564036615814,
-1.7));
#368049=CARTESIAN_POINT('Ctrl Pts',(-0.906488444224223,-0.774361328520471,
-1.7));
#368050=CARTESIAN_POINT('Ctrl Pts',(-0.980239661944283,-0.698929860052436,
-1.7));
#368051=CARTESIAN_POINT('Ctrl Pts',(-1.08659688413256,-0.554881140374752,
-1.7));
#368052=CARTESIAN_POINT('Ctrl Pts',(-1.14864632923241,-0.460352743585334,
-1.7));
#368053=CARTESIAN_POINT('Ctrl Pts',(-1.26100849448902,-0.179088137671936,
-1.7));
#368054=CARTESIAN_POINT('Ctrl Pts',(-1.29189652800491,-0.0173593023659969,
-1.7));
#368055=CARTESIAN_POINT('Ctrl Pts',(-1.29108984811542,0.29991757832034,
-1.7));
#368056=CARTESIAN_POINT('Ctrl Pts',(-1.26280816915346,0.452628510455921,
-1.7));
#368057=CARTESIAN_POINT('Ctrl Pts',(-1.15403315966975,0.739009298630757,
-1.7));
#368058=CARTESIAN_POINT('Ctrl Pts',(-1.06946215919407,0.88567669595877,
-1.70000000000001));
#368059=CARTESIAN_POINT('Ctrl Pts',(-0.838257759590746,1.15024353406291,
-1.70000000000001));
#368060=CARTESIAN_POINT('Ctrl Pts',(-0.70010011391448,1.25940600481097,
-1.7));
#368061=CARTESIAN_POINT('Ctrl Pts',(-0.464663729175284,1.38344883181634,
-1.7));
#368062=CARTESIAN_POINT('Ctrl Pts',(-0.379811168312268,1.41817558821392,
-1.69999999991096));
#368063=CARTESIAN_POINT('Ctrl Pts',(-0.197010229499014,1.47315843181175,
-1.69999999991096));
#368064=CARTESIAN_POINT('Ctrl Pts',(-0.0990730826998878,1.49174390977524,
-1.7));
#368065=CARTESIAN_POINT('Ctrl Pts',(3.29540263058496E-12,1.50000000000027,
-1.7));
#368066=CARTESIAN_POINT('',(-1.43925448419918E-16,-1.17524047358083,-1.7));
#368067=CARTESIAN_POINT('Origin',(4.23799807892358E-15,4.71844785465692E-15,
-1.7));
#368068=CARTESIAN_POINT('Ctrl Pts',(1.05094390383305,1.07028823734363,-1.7));
#368069=CARTESIAN_POINT('Ctrl Pts',(1.156452495554,0.945434066171969,-1.7));
#368070=CARTESIAN_POINT('Ctrl Pts',(1.2586537518754,0.783905914653593,-1.7));
#368071=CARTESIAN_POINT('Ctrl Pts',(1.37926337433591,0.431629318194347,
-1.7));
#368072=CARTESIAN_POINT('Ctrl Pts',(1.40434668153212,0.262454779629501,
-1.7));
#368073=CARTESIAN_POINT('Ctrl Pts',(1.39184448034083,-0.0842699563767622,
-1.7));
#368074=CARTESIAN_POINT('Ctrl Pts',(1.35148029165158,-0.258561181463102,
-1.69999999999998));
#368075=CARTESIAN_POINT('Ctrl Pts',(1.22264368235685,-0.547784646368696,
-1.69999999999998));
#368076=CARTESIAN_POINT('Ctrl Pts',(1.13071611052457,-0.704303236236527,
-1.69999999996066));
#368077=CARTESIAN_POINT('Ctrl Pts',(0.870776629029807,-0.949213555039079,
-1.69999999996066));
#368078=CARTESIAN_POINT('Ctrl Pts',(0.741388190020053,-1.03251050868711,
-1.7));
#368079=CARTESIAN_POINT('Ctrl Pts',(0.507415161659025,-1.12806794424744,
-1.7));
#368080=CARTESIAN_POINT('Ctrl Pts',(0.410499846437694,-1.15454479340249,
-1.7));
#368081=CARTESIAN_POINT('Ctrl Pts',(0.208295996222876,-1.18420961712132,
-1.7));
#368082=CARTESIAN_POINT('Ctrl Pts',(0.103670375869531,-1.18626698030435,
-1.7));
#368083=CARTESIAN_POINT('Ctrl Pts',(-1.38777878078145E-16,-1.17524047358083,
-1.7));
#368084=CARTESIAN_POINT('Origin',(0.,-6.07153216591882E-15,-1.275));
#368085=CARTESIAN_POINT('Origin',(1.04744440165294E-14,-1.5,0.));
#368086=CARTESIAN_POINT('',(-0.999999999999999,0.577350269189625,0.));
#368087=CARTESIAN_POINT('',(-0.999999999999999,-0.577350269189627,0.));
#368088=CARTESIAN_POINT('Origin',(0.,0.,0.));
#368089=CARTESIAN_POINT('',(3.25260651745651E-16,1.15470053837925,0.));
#368090=CARTESIAN_POINT('Origin',(0.,0.,0.));
#368091=CARTESIAN_POINT('Origin',(0.,0.,0.));
#368092=CARTESIAN_POINT('',(5.42101086242752E-16,-1.15470053837925,0.));
#368093=CARTESIAN_POINT('Origin',(0.,0.,0.));
#368094=CARTESIAN_POINT('Origin',(0.,0.,0.));
#368095=CARTESIAN_POINT('Origin',(0.,0.,0.));
#368096=CARTESIAN_POINT('Ctrl Pts',(0.999999999999951,0.577350269189654,
-2.7791564077117E-14));
#368097=CARTESIAN_POINT('Ctrl Pts',(0.500000000000001,0.866025403784438,
-0.28867513459479));
#368098=CARTESIAN_POINT('Ctrl Pts',(5.09575199449458E-14,1.15470053837922,
-2.90996254149895E-14));
#368099=CARTESIAN_POINT('Origin',(0.,0.,0.));
#368100=CARTESIAN_POINT('Ctrl Pts',(-4.99717345888679E-14,1.15470053837922,
-2.93650291647028E-14));
#368101=CARTESIAN_POINT('Ctrl Pts',(-0.5,0.866025403784438,-0.288675134594791));
#368102=CARTESIAN_POINT('Ctrl Pts',(-0.999999999999949,0.577350269189654,
-2.94219013967842E-14));
#368103=CARTESIAN_POINT('Origin',(0.,0.,0.));
#368104=CARTESIAN_POINT('Ctrl Pts',(-0.999999999999999,0.577350269189567,
-2.99337514855168E-14));
#368105=CARTESIAN_POINT('Ctrl Pts',(-0.999999999999999,-1.33226762955019E-15,
-0.288675134594791));
#368106=CARTESIAN_POINT('Ctrl Pts',(-0.999999999999999,-0.57735026918957,
-2.85119456834816E-14));
#368107=CARTESIAN_POINT('Origin',(0.,0.,0.));
#368108=CARTESIAN_POINT('Ctrl Pts',(-0.999999999999948,-0.577350269189654,
-2.99906237175983E-14));
#368109=CARTESIAN_POINT('Ctrl Pts',(-0.499999999999999,-0.866025403784438,
-0.288675134594791));
#368110=CARTESIAN_POINT('Ctrl Pts',(-4.92134381611157E-14,-1.15470053837922,
-2.91564976470709E-14));
#368111=CARTESIAN_POINT('Origin',(0.,0.,0.));
#368112=CARTESIAN_POINT('Ctrl Pts',(5.0350882802744E-14,-1.15470053837922,
-2.93650291647027E-14));
#368113=CARTESIAN_POINT('Ctrl Pts',(0.5,-0.866025403784437,-0.288675134594791));
#368114=CARTESIAN_POINT('Ctrl Pts',(0.99999999999995,-0.577350269189653,
-2.91944124684585E-14));
#368115=CARTESIAN_POINT('Origin',(1.,-0.577350269189624,-1.19));
#368116=CARTESIAN_POINT('',(1.9352544089507E-16,-1.15470053837925,-1.19));
#368117=CARTESIAN_POINT('',(1.,-0.577350269189624,-1.19));
#368118=CARTESIAN_POINT('',(1.9352544089507E-16,-1.15470053837925,-1.19));
#368119=CARTESIAN_POINT('',(1.,0.577350269189626,-1.19));
#368120=CARTESIAN_POINT('',(1.,-0.577350269189624,-1.19));
#368121=CARTESIAN_POINT('',(3.85779730129493E-16,1.15470053837925,-1.19));
#368122=CARTESIAN_POINT('',(1.,0.577350269189626,-1.19));
#368123=CARTESIAN_POINT('',(-0.999999999999999,0.577350269189625,-1.19));
#368124=CARTESIAN_POINT('',(3.85779730129493E-16,1.15470053837925,-1.19));
#368125=CARTESIAN_POINT('',(-0.999999999999999,-0.577350269189625,-1.19));
#368126=CARTESIAN_POINT('',(-0.999999999999999,0.577350269189625,-1.19));
#368127=CARTESIAN_POINT('',(-0.999999999999999,-0.577350269189625,-1.19));
#368128=CARTESIAN_POINT('Origin',(1.,-0.577350269189624,-1.19));
#368129=CARTESIAN_POINT('',(1.,-0.577350269189624,-1.19));
#368130=CARTESIAN_POINT('',(1.,0.577350269189626,-1.19));
#368131=CARTESIAN_POINT('Origin',(1.,0.577350269189626,-1.19));
#368132=CARTESIAN_POINT('',(3.85779730129493E-16,1.15470053837925,-1.19));
#368133=CARTESIAN_POINT('Origin',(3.85779730129493E-16,1.15470053837925,
-1.19));
#368134=CARTESIAN_POINT('',(-0.999999999999999,0.577350269189625,-1.19));
#368135=CARTESIAN_POINT('Origin',(-0.999999999999999,0.577350269189625,
-1.19));
#368136=CARTESIAN_POINT('',(-0.999999999999999,-0.577350269189625,-1.19));
#368137=CARTESIAN_POINT('Origin',(-0.999999999999999,-0.577350269189625,
-1.19));
#368138=CARTESIAN_POINT('',(1.9352544089507E-16,-1.15470053837925,-1.19));
#368139=CARTESIAN_POINT('Origin',(1.9352544089507E-16,-1.15470053837925,
-1.19));
#368140=CARTESIAN_POINT('Ctrl Pts',(0.,1.17524047358083,-9.95));
#368141=CARTESIAN_POINT('Ctrl Pts',(-0.678525403784435,1.17524047358083,
-9.90833333333333));
#368142=CARTESIAN_POINT('Ctrl Pts',(-1.01778810567665,0.58762023679042,
-9.86666666666667));
#368143=CARTESIAN_POINT('Ctrl Pts',(-1.35705080756887,5.0380876514183E-15,
-9.825));
#368144=CARTESIAN_POINT('Ctrl Pts',(-1.01778810567665,-0.58762023679041,
-9.78333333333333));
#368145=CARTESIAN_POINT('Ctrl Pts',(-0.678525403784435,-1.17524047358082,
-9.74166666666667));
#368146=CARTESIAN_POINT('Ctrl Pts',(-1.43925448419918E-16,-1.17524047358082,
-9.7));
#368147=CARTESIAN_POINT('Ctrl Pts',(0.678525403784435,-1.17524047358082,
-9.65833333333333));
#368148=CARTESIAN_POINT('Ctrl Pts',(1.01778810567665,-0.58762023679041,
-9.61666666666667));
#368149=CARTESIAN_POINT('Ctrl Pts',(1.35705080756887,4.59643214611782E-15,
-9.575));
#368150=CARTESIAN_POINT('Ctrl Pts',(1.01778810567665,0.587620236790419,
-9.53333333333333));
#368151=CARTESIAN_POINT('Ctrl Pts',(0.678525403784436,1.17524047358083,
-9.49166666666667));
#368152=CARTESIAN_POINT('Ctrl Pts',(0.,1.17524047358083,-9.45));
#368153=CARTESIAN_POINT('Ctrl Pts',(-0.678525403784435,1.17524047358083,
-9.40833333333333));
#368154=CARTESIAN_POINT('Ctrl Pts',(-1.01778810567665,0.58762023679042,
-9.36666666666667));
#368155=CARTESIAN_POINT('Ctrl Pts',(-1.35705080756887,4.81953981192516E-15,
-9.325));
#368156=CARTESIAN_POINT('Ctrl Pts',(-1.01778810567665,-0.58762023679041,
-9.28333333333333));
#368157=CARTESIAN_POINT('Ctrl Pts',(-0.678525403784435,-1.17524047358082,
-9.24166666666667));
#368158=CARTESIAN_POINT('Ctrl Pts',(-1.43925448419918E-16,-1.17524047358082,
-9.2));
#368159=CARTESIAN_POINT('Ctrl Pts',(0.678525403784435,-1.17524047358083,
-9.15833333333333));
#368160=CARTESIAN_POINT('Ctrl Pts',(1.01778810567665,-0.587620236790411,
-9.11666666666667));
#368161=CARTESIAN_POINT('Ctrl Pts',(1.35705080756887,4.37788430662468E-15,
-9.075));
#368162=CARTESIAN_POINT('Ctrl Pts',(1.01778810567665,0.587620236790418,
-9.03333333333333));
#368163=CARTESIAN_POINT('Ctrl Pts',(0.678525403784436,1.17524047358083,
-8.99166666666667));
#368164=CARTESIAN_POINT('Ctrl Pts',(0.,1.17524047358083,-8.95));
#368165=CARTESIAN_POINT('Ctrl Pts',(-0.678525403784435,1.17524047358083,
-8.90833333333333));
#368166=CARTESIAN_POINT('Ctrl Pts',(-1.01778810567665,0.587620236790419,
-8.86666666666667));
#368167=CARTESIAN_POINT('Ctrl Pts',(-1.35705080756887,4.60099197243202E-15,
-8.825));
#368168=CARTESIAN_POINT('Ctrl Pts',(-1.01778810567665,-0.58762023679041,
-8.78333333333333));
#368169=CARTESIAN_POINT('Ctrl Pts',(-0.678525403784435,-1.17524047358082,
-8.74166666666667));
#368170=CARTESIAN_POINT('Ctrl Pts',(-1.43925448419918E-16,-1.17524047358082,
-8.7));
#368171=CARTESIAN_POINT('Ctrl Pts',(0.678525403784435,-1.17524047358083,
-8.65833333333333));
#368172=CARTESIAN_POINT('Ctrl Pts',(1.01778810567665,-0.587620236790411,
-8.61666666666667));
#368173=CARTESIAN_POINT('Ctrl Pts',(1.35705080756887,4.15933646713154E-15,
-8.575));
#368174=CARTESIAN_POINT('Ctrl Pts',(1.01778810567665,0.587620236790418,
-8.53333333333333));
#368175=CARTESIAN_POINT('Ctrl Pts',(0.678525403784436,1.17524047358083,
-8.49166666666667));
#368176=CARTESIAN_POINT('Ctrl Pts',(0.,1.17524047358083,-8.45));
#368177=CARTESIAN_POINT('Ctrl Pts',(-0.678525403784435,1.17524047358083,
-8.40833333333333));
#368178=CARTESIAN_POINT('Ctrl Pts',(-1.01778810567665,0.587620236790419,
-8.36666666666667));
#368179=CARTESIAN_POINT('Ctrl Pts',(-1.35705080756887,4.38244413293887E-15,
-8.325));
#368180=CARTESIAN_POINT('Ctrl Pts',(-1.01778810567665,-0.58762023679041,
-8.28333333333333));
#368181=CARTESIAN_POINT('Ctrl Pts',(-0.678525403784435,-1.17524047358082,
-8.24166666666667));
#368182=CARTESIAN_POINT('Ctrl Pts',(-1.43925448419918E-16,-1.17524047358083,
-8.2));
#368183=CARTESIAN_POINT('Ctrl Pts',(0.678525403784435,-1.17524047358083,
-8.15833333333333));
#368184=CARTESIAN_POINT('Ctrl Pts',(1.01778810567665,-0.587620236790411,
-8.11666666666667));
#368185=CARTESIAN_POINT('Ctrl Pts',(1.35705080756887,3.94078862763839E-15,
-8.075));
#368186=CARTESIAN_POINT('Ctrl Pts',(1.01778810567665,0.587620236790418,
-8.03333333333333));
#368187=CARTESIAN_POINT('Ctrl Pts',(0.678525403784436,1.17524047358083,
-7.99166666666667));
#368188=CARTESIAN_POINT('Ctrl Pts',(0.,1.17524047358083,-7.95));
#368189=CARTESIAN_POINT('Ctrl Pts',(-0.678525403784435,1.17524047358083,
-7.90833333333333));
#368190=CARTESIAN_POINT('Ctrl Pts',(-1.01778810567665,0.587620236790419,
-7.86666666666667));
#368191=CARTESIAN_POINT('Ctrl Pts',(-1.35705080756887,4.16389629344573E-15,
-7.825));
#368192=CARTESIAN_POINT('Ctrl Pts',(-1.01778810567665,-0.58762023679041,
-7.78333333333333));
#368193=CARTESIAN_POINT('Ctrl Pts',(-0.678525403784435,-1.17524047358083,
-7.74166666666667));
#368194=CARTESIAN_POINT('Ctrl Pts',(-1.43925448419918E-16,-1.17524047358083,
-7.7));
#368195=CARTESIAN_POINT('Ctrl Pts',(0.678525403784435,-1.17524047358083,
-7.65833333333333));
#368196=CARTESIAN_POINT('Ctrl Pts',(1.01778810567665,-0.587620236790411,
-7.61666666666667));
#368197=CARTESIAN_POINT('Ctrl Pts',(1.35705080756887,3.72224078814525E-15,
-7.575));
#368198=CARTESIAN_POINT('Ctrl Pts',(1.01778810567665,0.587620236790418,
-7.53333333333333));
#368199=CARTESIAN_POINT('Ctrl Pts',(0.678525403784436,1.17524047358083,
-7.49166666666667));
#368200=CARTESIAN_POINT('Ctrl Pts',(0.,1.17524047358083,-7.45));
#368201=CARTESIAN_POINT('Ctrl Pts',(-0.678525403784435,1.17524047358083,
-7.40833333333333));
#368202=CARTESIAN_POINT('Ctrl Pts',(-1.01778810567665,0.587620236790419,
-7.36666666666667));
#368203=CARTESIAN_POINT('Ctrl Pts',(-1.35705080756887,3.94534845395259E-15,
-7.325));
#368204=CARTESIAN_POINT('Ctrl Pts',(-1.01778810567665,-0.587620236790411,
-7.28333333333333));
#368205=CARTESIAN_POINT('Ctrl Pts',(-0.678525403784435,-1.17524047358083,
-7.24166666666667));
#368206=CARTESIAN_POINT('Ctrl Pts',(-1.43925448419918E-16,-1.17524047358083,
-7.2));
#368207=CARTESIAN_POINT('Ctrl Pts',(0.678525403784435,-1.17524047358083,
-7.15833333333333));
#368208=CARTESIAN_POINT('Ctrl Pts',(1.01778810567665,-0.587620236790411,
-7.11666666666667));
#368209=CARTESIAN_POINT('Ctrl Pts',(1.35705080756887,3.50369294865211E-15,
-7.075));
#368210=CARTESIAN_POINT('Ctrl Pts',(1.01778810567665,0.587620236790417,
-7.03333333333333));
#368211=CARTESIAN_POINT('Ctrl Pts',(0.678525403784436,1.17524047358083,
-6.99166666666667));
#368212=CARTESIAN_POINT('Ctrl Pts',(0.,1.17524047358083,-6.95));
#368213=CARTESIAN_POINT('Ctrl Pts',(-0.678525403784435,1.17524047358083,
-6.90833333333333));
#368214=CARTESIAN_POINT('Ctrl Pts',(-1.01778810567665,0.587620236790418,
-6.86666666666667));
#368215=CARTESIAN_POINT('Ctrl Pts',(-1.35705080756887,3.72680061445945E-15,
-6.825));
#368216=CARTESIAN_POINT('Ctrl Pts',(-1.01778810567665,-0.587620236790411,
-6.78333333333333));
#368217=CARTESIAN_POINT('Ctrl Pts',(-0.678525403784435,-1.17524047358083,
-6.74166666666667));
#368218=CARTESIAN_POINT('Ctrl Pts',(-1.43925448419918E-16,-1.17524047358083,
-6.7));
#368219=CARTESIAN_POINT('Ctrl Pts',(0.678525403784435,-1.17524047358083,
-6.65833333333333));
#368220=CARTESIAN_POINT('Ctrl Pts',(1.01778810567665,-0.587620236790412,
-6.61666666666667));
#368221=CARTESIAN_POINT('Ctrl Pts',(1.35705080756887,3.28514510915897E-15,
-6.575));
#368222=CARTESIAN_POINT('Ctrl Pts',(1.01778810567665,0.587620236790417,
-6.53333333333333));
#368223=CARTESIAN_POINT('Ctrl Pts',(0.678525403784436,1.17524047358083,
-6.49166666666667));
#368224=CARTESIAN_POINT('Ctrl Pts',(0.,1.17524047358083,-6.45));
#368225=CARTESIAN_POINT('Ctrl Pts',(-0.678525403784435,1.17524047358083,
-6.40833333333334));
#368226=CARTESIAN_POINT('Ctrl Pts',(-1.01778810567665,0.587620236790418,
-6.36666666666667));
#368227=CARTESIAN_POINT('Ctrl Pts',(-1.35705080756887,3.50825277496631E-15,
-6.325));
#368228=CARTESIAN_POINT('Ctrl Pts',(-1.01778810567665,-0.587620236790411,
-6.28333333333333));
#368229=CARTESIAN_POINT('Ctrl Pts',(-0.678525403784435,-1.17524047358083,
-6.24166666666667));
#368230=CARTESIAN_POINT('Ctrl Pts',(-1.43925448419918E-16,-1.17524047358083,
-6.2));
#368231=CARTESIAN_POINT('Ctrl Pts',(0.678525403784435,-1.17524047358083,
-6.15833333333333));
#368232=CARTESIAN_POINT('Ctrl Pts',(1.01778810567665,-0.587620236790412,
-6.11666666666667));
#368233=CARTESIAN_POINT('Ctrl Pts',(1.35705080756887,3.06659726966583E-15,
-6.075));
#368234=CARTESIAN_POINT('Ctrl Pts',(1.01778810567665,0.587620236790417,
-6.03333333333333));
#368235=CARTESIAN_POINT('Ctrl Pts',(0.678525403784436,1.17524047358083,
-5.99166666666667));
#368236=CARTESIAN_POINT('Ctrl Pts',(0.,1.17524047358083,-5.95));
#368237=CARTESIAN_POINT('Ctrl Pts',(-0.678525403784435,1.17524047358083,
-5.90833333333333));
#368238=CARTESIAN_POINT('Ctrl Pts',(-1.01778810567665,0.587620236790418,
-5.86666666666667));
#368239=CARTESIAN_POINT('Ctrl Pts',(-1.35705080756887,3.28970493547317E-15,
-5.825));
#368240=CARTESIAN_POINT('Ctrl Pts',(-1.01778810567665,-0.587620236790411,
-5.78333333333333));
#368241=CARTESIAN_POINT('Ctrl Pts',(-0.678525403784435,-1.17524047358083,
-5.74166666666667));
#368242=CARTESIAN_POINT('Ctrl Pts',(-1.43925448419918E-16,-1.17524047358083,
-5.7));
#368243=CARTESIAN_POINT('Ctrl Pts',(0.678525403784435,-1.17524047358083,
-5.65833333333333));
#368244=CARTESIAN_POINT('Ctrl Pts',(1.01778810567665,-0.587620236790412,
-5.61666666666667));
#368245=CARTESIAN_POINT('Ctrl Pts',(1.35705080756887,2.84804943017269E-15,
-5.575));
#368246=CARTESIAN_POINT('Ctrl Pts',(1.01778810567665,0.587620236790417,
-5.53333333333333));
#368247=CARTESIAN_POINT('Ctrl Pts',(0.678525403784436,1.17524047358083,
-5.49166666666667));
#368248=CARTESIAN_POINT('Ctrl Pts',(0.,1.17524047358083,-5.45));
#368249=CARTESIAN_POINT('Ctrl Pts',(-0.678525403784435,1.17524047358083,
-5.40833333333333));
#368250=CARTESIAN_POINT('Ctrl Pts',(-1.01778810567665,0.587620236790418,
-5.36666666666667));
#368251=CARTESIAN_POINT('Ctrl Pts',(-1.35705080756887,3.07115709598003E-15,
-5.325));
#368252=CARTESIAN_POINT('Ctrl Pts',(-1.01778810567665,-0.587620236790411,
-5.28333333333333));
#368253=CARTESIAN_POINT('Ctrl Pts',(-0.678525403784435,-1.17524047358083,
-5.24166666666667));
#368254=CARTESIAN_POINT('Ctrl Pts',(-1.43925448419918E-16,-1.17524047358083,
-5.2));
#368255=CARTESIAN_POINT('Ctrl Pts',(0.678525403784435,-1.17524047358083,
-5.15833333333333));
#368256=CARTESIAN_POINT('Ctrl Pts',(1.01778810567665,-0.587620236790412,
-5.11666666666667));
#368257=CARTESIAN_POINT('Ctrl Pts',(1.35705080756887,2.62950159067955E-15,
-5.075));
#368258=CARTESIAN_POINT('Ctrl Pts',(1.01778810567665,0.587620236790417,
-5.03333333333333));
#368259=CARTESIAN_POINT('Ctrl Pts',(0.678525403784436,1.17524047358083,
-4.99166666666667));
#368260=CARTESIAN_POINT('Ctrl Pts',(0.,1.17524047358083,-4.95));
#368261=CARTESIAN_POINT('Ctrl Pts',(-0.678525403784435,1.17524047358083,
-4.90833333333333));
#368262=CARTESIAN_POINT('Ctrl Pts',(-1.01778810567665,0.587620236790418,
-4.86666666666667));
#368263=CARTESIAN_POINT('Ctrl Pts',(-1.35705080756887,2.85260925648689E-15,
-4.825));
#368264=CARTESIAN_POINT('Ctrl Pts',(-1.01778810567665,-0.587620236790412,
-4.78333333333333));
#368265=CARTESIAN_POINT('Ctrl Pts',(-0.678525403784435,-1.17524047358083,
-4.74166666666667));
#368266=CARTESIAN_POINT('Ctrl Pts',(-1.43925448419918E-16,-1.17524047358083,
-4.7));
#368267=CARTESIAN_POINT('Ctrl Pts',(0.678525403784435,-1.17524047358083,
-4.65833333333333));
#368268=CARTESIAN_POINT('Ctrl Pts',(1.01778810567665,-0.587620236790413,
-4.61666666666667));
#368269=CARTESIAN_POINT('Ctrl Pts',(1.35705080756887,2.41095375118641E-15,
-4.575));
#368270=CARTESIAN_POINT('Ctrl Pts',(1.01778810567665,0.587620236790416,
-4.53333333333333));
#368271=CARTESIAN_POINT('Ctrl Pts',(0.678525403784436,1.17524047358083,
-4.49166666666667));
#368272=CARTESIAN_POINT('Ctrl Pts',(0.,1.17524047358083,-4.45));
#368273=CARTESIAN_POINT('Ctrl Pts',(-0.678525403784435,1.17524047358083,
-4.40833333333333));
#368274=CARTESIAN_POINT('Ctrl Pts',(-1.01778810567665,0.587620236790417,
-4.36666666666667));
#368275=CARTESIAN_POINT('Ctrl Pts',(-1.35705080756887,2.63406141699374E-15,
-4.325));
#368276=CARTESIAN_POINT('Ctrl Pts',(-1.01778810567665,-0.587620236790412,
-4.28333333333333));
#368277=CARTESIAN_POINT('Ctrl Pts',(-0.678525403784435,-1.17524047358083,
-4.24166666666667));
#368278=CARTESIAN_POINT('Ctrl Pts',(-1.43925448419918E-16,-1.17524047358083,
-4.2));
#368279=CARTESIAN_POINT('Ctrl Pts',(0.678525403784435,-1.17524047358083,
-4.15833333333333));
#368280=CARTESIAN_POINT('Ctrl Pts',(1.01778810567665,-0.587620236790413,
-4.11666666666667));
#368281=CARTESIAN_POINT('Ctrl Pts',(1.35705080756887,2.19240591169327E-15,
-4.075));
#368282=CARTESIAN_POINT('Ctrl Pts',(1.01778810567665,0.587620236790416,
-4.03333333333333));
#368283=CARTESIAN_POINT('Ctrl Pts',(0.678525403784436,1.17524047358083,
-3.99166666666667));
#368284=CARTESIAN_POINT('Ctrl Pts',(0.,1.17524047358083,-3.95));
#368285=CARTESIAN_POINT('Ctrl Pts',(-0.678525403784435,1.17524047358083,
-3.90833333333333));
#368286=CARTESIAN_POINT('Ctrl Pts',(-1.01778810567665,0.587620236790417,
-3.86666666666667));
#368287=CARTESIAN_POINT('Ctrl Pts',(-1.35705080756887,2.4155135775006E-15,
-3.825));
#368288=CARTESIAN_POINT('Ctrl Pts',(-1.01778810567665,-0.587620236790412,
-3.78333333333333));
#368289=CARTESIAN_POINT('Ctrl Pts',(-0.678525403784435,-1.17524047358083,
-3.74166666666667));
#368290=CARTESIAN_POINT('Ctrl Pts',(-1.43925448419918E-16,-1.17524047358083,
-3.7));
#368291=CARTESIAN_POINT('Ctrl Pts',(0.678525403784435,-1.17524047358083,
-3.65833333333333));
#368292=CARTESIAN_POINT('Ctrl Pts',(1.01778810567665,-0.587620236790413,
-3.61666666666667));
#368293=CARTESIAN_POINT('Ctrl Pts',(1.35705080756887,1.97385807220012E-15,
-3.575));
#368294=CARTESIAN_POINT('Ctrl Pts',(1.01778810567665,0.587620236790416,
-3.53333333333333));
#368295=CARTESIAN_POINT('Ctrl Pts',(0.678525403784436,1.17524047358083,
-3.49166666666667));
#368296=CARTESIAN_POINT('Ctrl Pts',(0.,1.17524047358083,-3.45));
#368297=CARTESIAN_POINT('Ctrl Pts',(-0.678525403784435,1.17524047358083,
-3.40833333333333));
#368298=CARTESIAN_POINT('Ctrl Pts',(-1.01778810567665,0.587620236790417,
-3.36666666666667));
#368299=CARTESIAN_POINT('Ctrl Pts',(-1.35705080756887,2.19696573800746E-15,
-3.325));
#368300=CARTESIAN_POINT('Ctrl Pts',(-1.01778810567665,-0.587620236790412,
-3.28333333333333));
#368301=CARTESIAN_POINT('Ctrl Pts',(-0.678525403784435,-1.17524047358083,
-3.24166666666667));
#368302=CARTESIAN_POINT('Ctrl Pts',(-1.43925448419918E-16,-1.17524047358083,
-3.2));
#368303=CARTESIAN_POINT('Ctrl Pts',(0.678525403784435,-1.17524047358083,
-3.15833333333333));
#368304=CARTESIAN_POINT('Ctrl Pts',(1.01778810567665,-0.587620236790413,
-3.11666666666667));
#368305=CARTESIAN_POINT('Ctrl Pts',(1.35705080756887,1.75531023270698E-15,
-3.075));
#368306=CARTESIAN_POINT('Ctrl Pts',(1.01778810567665,0.587620236790416,
-3.03333333333333));
#368307=CARTESIAN_POINT('Ctrl Pts',(0.678525403784436,1.17524047358083,
-2.99166666666667));
#368308=CARTESIAN_POINT('Ctrl Pts',(0.,1.17524047358083,-2.95));
#368309=CARTESIAN_POINT('Ctrl Pts',(-0.678525403784435,1.17524047358083,
-2.90833333333333));
#368310=CARTESIAN_POINT('Ctrl Pts',(-1.01778810567665,0.587620236790417,
-2.86666666666667));
#368311=CARTESIAN_POINT('Ctrl Pts',(-1.35705080756887,1.97841789851432E-15,
-2.825));
#368312=CARTESIAN_POINT('Ctrl Pts',(-1.01778810567665,-0.587620236790413,
-2.78333333333333));
#368313=CARTESIAN_POINT('Ctrl Pts',(-0.678525403784435,-1.17524047358083,
-2.74166666666667));
#368314=CARTESIAN_POINT('Ctrl Pts',(-1.43925448419918E-16,-1.17524047358083,
-2.7));
#368315=CARTESIAN_POINT('Ctrl Pts',(0.678525403784435,-1.17524047358083,
-2.65833333333333));
#368316=CARTESIAN_POINT('Ctrl Pts',(1.01778810567665,-0.587620236790414,
-2.61666666666667));
#368317=CARTESIAN_POINT('Ctrl Pts',(1.35705080756887,1.53676239321384E-15,
-2.575));
#368318=CARTESIAN_POINT('Ctrl Pts',(1.01778810567665,0.587620236790415,
-2.53333333333333));
#368319=CARTESIAN_POINT('Ctrl Pts',(0.678525403784436,1.17524047358083,
-2.49166666666667));
#368320=CARTESIAN_POINT('Ctrl Pts',(0.,1.17524047358083,-2.45));
#368321=CARTESIAN_POINT('Ctrl Pts',(-0.678525403784435,1.17524047358083,
-2.40833333333333));
#368322=CARTESIAN_POINT('Ctrl Pts',(-1.01778810567665,0.587620236790416,
-2.36666666666667));
#368323=CARTESIAN_POINT('Ctrl Pts',(-1.35705080756887,1.75987005902118E-15,
-2.325));
#368324=CARTESIAN_POINT('Ctrl Pts',(-1.01778810567665,-0.587620236790413,
-2.28333333333333));
#368325=CARTESIAN_POINT('Ctrl Pts',(-0.678525403784435,-1.17524047358083,
-2.24166666666667));
#368326=CARTESIAN_POINT('Ctrl Pts',(-1.43925448419918E-16,-1.17524047358083,
-2.2));
#368327=CARTESIAN_POINT('Ctrl Pts',(0.678525403784435,-1.17524047358083,
-2.15833333333333));
#368328=CARTESIAN_POINT('Ctrl Pts',(1.01778810567665,-0.587620236790414,
-2.11666666666667));
#368329=CARTESIAN_POINT('Ctrl Pts',(1.35705080756887,1.3182145537207E-15,
-2.075));
#368330=CARTESIAN_POINT('Ctrl Pts',(1.01778810567665,0.587620236790415,
-2.03333333333333));
#368331=CARTESIAN_POINT('Ctrl Pts',(0.678525403784436,1.17524047358083,
-1.99166666666667));
#368332=CARTESIAN_POINT('Ctrl Pts',(0.,1.17524047358083,-1.95));
#368333=CARTESIAN_POINT('Ctrl Pts',(-0.678525403784435,1.17524047358083,
-1.90833333333333));
#368334=CARTESIAN_POINT('Ctrl Pts',(-1.01778810567665,0.587620236790416,
-1.86666666666667));
#368335=CARTESIAN_POINT('Ctrl Pts',(-1.35705080756887,1.54132221952804E-15,
-1.825));
#368336=CARTESIAN_POINT('Ctrl Pts',(-1.01778810567665,-0.587620236790413,
-1.78333333333333));
#368337=CARTESIAN_POINT('Ctrl Pts',(-0.678525403784435,-1.17524047358083,
-1.74166666666667));
#368338=CARTESIAN_POINT('Ctrl Pts',(-1.43925448419918E-16,-1.17524047358083,
-1.7));
#368339=CARTESIAN_POINT('Ctrl Pts',(0.678525403784435,-1.17524047358083,
-1.65833333333333));
#368340=CARTESIAN_POINT('Ctrl Pts',(1.01778810567665,-0.587620236790414,
-1.61666666666667));
#368341=CARTESIAN_POINT('Ctrl Pts',(1.35705080756887,1.09966671422756E-15,
-1.575));
#368342=CARTESIAN_POINT('Ctrl Pts',(1.01778810567665,0.587620236790415,
-1.53333333333333));
#368343=CARTESIAN_POINT('Ctrl Pts',(0.678525403784436,1.17524047358083,
-1.49166666666667));
#368344=CARTESIAN_POINT('Ctrl Pts',(0.,1.17524047358083,-1.45));
#368345=CARTESIAN_POINT('Ctrl Pts',(0.,1.5,-10.1375));
#368346=CARTESIAN_POINT('Ctrl Pts',(-0.866025403784437,1.5,-10.0958333333333));
#368347=CARTESIAN_POINT('Ctrl Pts',(-1.29903810567666,0.750000000000004,
-10.0541666666667));
#368348=CARTESIAN_POINT('Ctrl Pts',(-1.73205080756887,5.14300521871224E-15,
-10.0125));
#368349=CARTESIAN_POINT('Ctrl Pts',(-1.29903810567666,-0.749999999999993,
-9.97083333333333));
#368350=CARTESIAN_POINT('Ctrl Pts',(-0.866025403784437,-1.49999999999999,
-9.92916666666667));
#368351=CARTESIAN_POINT('Ctrl Pts',(-1.83697019872103E-16,-1.49999999999999,
-9.8875));
#368352=CARTESIAN_POINT('Ctrl Pts',(0.866025403784436,-1.49999999999999,
-9.84583333333333));
#368353=CARTESIAN_POINT('Ctrl Pts',(1.29903810567665,-0.749999999999994,
-9.80416666666667));
#368354=CARTESIAN_POINT('Ctrl Pts',(1.73205080756887,4.60950120347571E-15,
-9.7625));
#368355=CARTESIAN_POINT('Ctrl Pts',(1.29903810567666,0.750000000000002,
-9.72083333333333));
#368356=CARTESIAN_POINT('Ctrl Pts',(0.866025403784437,1.5,-9.67916666666667));
#368357=CARTESIAN_POINT('Ctrl Pts',(0.,1.5,-9.6375));
#368358=CARTESIAN_POINT('Ctrl Pts',(-0.866025403784437,1.5,-9.59583333333333));
#368359=CARTESIAN_POINT('Ctrl Pts',(-1.29903810567666,0.750000000000003,
-9.55416666666667));
#368360=CARTESIAN_POINT('Ctrl Pts',(-1.73205080756887,4.9244573792191E-15,
-9.5125));
#368361=CARTESIAN_POINT('Ctrl Pts',(-1.29903810567666,-0.749999999999993,
-9.47083333333333));
#368362=CARTESIAN_POINT('Ctrl Pts',(-0.866025403784437,-1.49999999999999,
-9.42916666666667));
#368363=CARTESIAN_POINT('Ctrl Pts',(-1.83697019872103E-16,-1.49999999999999,
-9.3875));
#368364=CARTESIAN_POINT('Ctrl Pts',(0.866025403784436,-1.49999999999999,
-9.34583333333333));
#368365=CARTESIAN_POINT('Ctrl Pts',(1.29903810567665,-0.749999999999994,
-9.30416666666667));
#368366=CARTESIAN_POINT('Ctrl Pts',(1.73205080756887,4.39095336398257E-15,
-9.2625));
#368367=CARTESIAN_POINT('Ctrl Pts',(1.29903810567666,0.750000000000002,
-9.22083333333333));
#368368=CARTESIAN_POINT('Ctrl Pts',(0.866025403784437,1.5,-9.17916666666667));
#368369=CARTESIAN_POINT('Ctrl Pts',(0.,1.5,-9.1375));
#368370=CARTESIAN_POINT('Ctrl Pts',(-0.866025403784437,1.5,-9.09583333333333));
#368371=CARTESIAN_POINT('Ctrl Pts',(-1.29903810567666,0.750000000000003,
-9.05416666666667));
#368372=CARTESIAN_POINT('Ctrl Pts',(-1.73205080756887,4.70590953972596E-15,
-9.0125));
#368373=CARTESIAN_POINT('Ctrl Pts',(-1.29903810567666,-0.749999999999993,
-8.97083333333333));
#368374=CARTESIAN_POINT('Ctrl Pts',(-0.866025403784437,-1.49999999999999,
-8.92916666666667));
#368375=CARTESIAN_POINT('Ctrl Pts',(-1.83697019872103E-16,-1.49999999999999,
-8.8875));
#368376=CARTESIAN_POINT('Ctrl Pts',(0.866025403784436,-1.49999999999999,
-8.84583333333333));
#368377=CARTESIAN_POINT('Ctrl Pts',(1.29903810567665,-0.749999999999994,
-8.80416666666667));
#368378=CARTESIAN_POINT('Ctrl Pts',(1.73205080756887,4.17240552448942E-15,
-8.7625));
#368379=CARTESIAN_POINT('Ctrl Pts',(1.29903810567666,0.750000000000002,
-8.72083333333333));
#368380=CARTESIAN_POINT('Ctrl Pts',(0.866025403784437,1.5,-8.67916666666667));
#368381=CARTESIAN_POINT('Ctrl Pts',(0.,1.5,-8.6375));
#368382=CARTESIAN_POINT('Ctrl Pts',(-0.866025403784437,1.5,-8.59583333333333));
#368383=CARTESIAN_POINT('Ctrl Pts',(-1.29903810567666,0.750000000000003,
-8.55416666666667));
#368384=CARTESIAN_POINT('Ctrl Pts',(-1.73205080756887,4.48736170023282E-15,
-8.5125));
#368385=CARTESIAN_POINT('Ctrl Pts',(-1.29903810567666,-0.749999999999994,
-8.47083333333333));
#368386=CARTESIAN_POINT('Ctrl Pts',(-0.866025403784437,-1.49999999999999,
-8.42916666666667));
#368387=CARTESIAN_POINT('Ctrl Pts',(-1.83697019872103E-16,-1.49999999999999,
-8.3875));
#368388=CARTESIAN_POINT('Ctrl Pts',(0.866025403784436,-1.49999999999999,
-8.34583333333333));
#368389=CARTESIAN_POINT('Ctrl Pts',(1.29903810567665,-0.749999999999995,
-8.30416666666667));
#368390=CARTESIAN_POINT('Ctrl Pts',(1.73205080756887,3.95385768499628E-15,
-8.2625));
#368391=CARTESIAN_POINT('Ctrl Pts',(1.29903810567666,0.750000000000002,
-8.22083333333333));
#368392=CARTESIAN_POINT('Ctrl Pts',(0.866025403784437,1.5,-8.17916666666667));
#368393=CARTESIAN_POINT('Ctrl Pts',(0.,1.5,-8.1375));
#368394=CARTESIAN_POINT('Ctrl Pts',(-0.866025403784437,1.5,-8.09583333333333));
#368395=CARTESIAN_POINT('Ctrl Pts',(-1.29903810567666,0.750000000000003,
-8.05416666666667));
#368396=CARTESIAN_POINT('Ctrl Pts',(-1.73205080756887,4.26881386073967E-15,
-8.0125));
#368397=CARTESIAN_POINT('Ctrl Pts',(-1.29903810567666,-0.749999999999994,
-7.97083333333333));
#368398=CARTESIAN_POINT('Ctrl Pts',(-0.866025403784437,-1.49999999999999,
-7.92916666666667));
#368399=CARTESIAN_POINT('Ctrl Pts',(-1.83697019872103E-16,-1.49999999999999,
-7.8875));
#368400=CARTESIAN_POINT('Ctrl Pts',(0.866025403784436,-1.49999999999999,
-7.84583333333333));
#368401=CARTESIAN_POINT('Ctrl Pts',(1.29903810567665,-0.749999999999995,
-7.80416666666667));
#368402=CARTESIAN_POINT('Ctrl Pts',(1.73205080756887,3.73530984550314E-15,
-7.7625));
#368403=CARTESIAN_POINT('Ctrl Pts',(1.29903810567666,0.750000000000001,
-7.72083333333333));
#368404=CARTESIAN_POINT('Ctrl Pts',(0.866025403784437,1.5,-7.67916666666667));
#368405=CARTESIAN_POINT('Ctrl Pts',(0.,1.5,-7.6375));
#368406=CARTESIAN_POINT('Ctrl Pts',(-0.866025403784437,1.5,-7.59583333333333));
#368407=CARTESIAN_POINT('Ctrl Pts',(-1.29903810567666,0.750000000000003,
-7.55416666666667));
#368408=CARTESIAN_POINT('Ctrl Pts',(-1.73205080756887,4.05026602124653E-15,
-7.5125));
#368409=CARTESIAN_POINT('Ctrl Pts',(-1.29903810567666,-0.749999999999994,
-7.47083333333333));
#368410=CARTESIAN_POINT('Ctrl Pts',(-0.866025403784437,-1.49999999999999,
-7.42916666666667));
#368411=CARTESIAN_POINT('Ctrl Pts',(-1.83697019872103E-16,-1.49999999999999,
-7.3875));
#368412=CARTESIAN_POINT('Ctrl Pts',(0.866025403784436,-1.49999999999999,
-7.34583333333334));
#368413=CARTESIAN_POINT('Ctrl Pts',(1.29903810567665,-0.749999999999995,
-7.30416666666667));
#368414=CARTESIAN_POINT('Ctrl Pts',(1.73205080756887,3.51676200601E-15,
-7.2625));
#368415=CARTESIAN_POINT('Ctrl Pts',(1.29903810567666,0.750000000000001,
-7.22083333333333));
#368416=CARTESIAN_POINT('Ctrl Pts',(0.866025403784437,1.5,-7.17916666666667));
#368417=CARTESIAN_POINT('Ctrl Pts',(0.,1.5,-7.1375));
#368418=CARTESIAN_POINT('Ctrl Pts',(-0.866025403784437,1.5,-7.09583333333333));
#368419=CARTESIAN_POINT('Ctrl Pts',(-1.29903810567666,0.750000000000002,
-7.05416666666667));
#368420=CARTESIAN_POINT('Ctrl Pts',(-1.73205080756887,3.83171818175339E-15,
-7.0125));
#368421=CARTESIAN_POINT('Ctrl Pts',(-1.29903810567666,-0.749999999999994,
-6.97083333333333));
#368422=CARTESIAN_POINT('Ctrl Pts',(-0.866025403784437,-1.49999999999999,
-6.92916666666667));
#368423=CARTESIAN_POINT('Ctrl Pts',(-1.83697019872103E-16,-1.49999999999999,
-6.8875));
#368424=CARTESIAN_POINT('Ctrl Pts',(0.866025403784436,-1.49999999999999,
-6.84583333333333));
#368425=CARTESIAN_POINT('Ctrl Pts',(1.29903810567665,-0.749999999999995,
-6.80416666666667));
#368426=CARTESIAN_POINT('Ctrl Pts',(1.73205080756887,3.29821416651686E-15,
-6.7625));
#368427=CARTESIAN_POINT('Ctrl Pts',(1.29903810567666,0.750000000000001,
-6.72083333333333));
#368428=CARTESIAN_POINT('Ctrl Pts',(0.866025403784437,1.5,-6.67916666666667));
#368429=CARTESIAN_POINT('Ctrl Pts',(0.,1.5,-6.6375));
#368430=CARTESIAN_POINT('Ctrl Pts',(-0.866025403784437,1.5,-6.59583333333333));
#368431=CARTESIAN_POINT('Ctrl Pts',(-1.29903810567666,0.750000000000002,
-6.55416666666667));
#368432=CARTESIAN_POINT('Ctrl Pts',(-1.73205080756887,3.61317034226025E-15,
-6.5125));
#368433=CARTESIAN_POINT('Ctrl Pts',(-1.29903810567666,-0.749999999999994,
-6.47083333333333));
#368434=CARTESIAN_POINT('Ctrl Pts',(-0.866025403784437,-1.49999999999999,
-6.42916666666667));
#368435=CARTESIAN_POINT('Ctrl Pts',(-1.83697019872103E-16,-1.49999999999999,
-6.3875));
#368436=CARTESIAN_POINT('Ctrl Pts',(0.866025403784436,-1.49999999999999,
-6.34583333333333));
#368437=CARTESIAN_POINT('Ctrl Pts',(1.29903810567665,-0.749999999999996,
-6.30416666666667));
#368438=CARTESIAN_POINT('Ctrl Pts',(1.73205080756887,3.07966632702372E-15,
-6.2625));
#368439=CARTESIAN_POINT('Ctrl Pts',(1.29903810567666,0.750000000000001,
-6.22083333333333));
#368440=CARTESIAN_POINT('Ctrl Pts',(0.866025403784437,1.5,-6.17916666666667));
#368441=CARTESIAN_POINT('Ctrl Pts',(0.,1.5,-6.1375));
#368442=CARTESIAN_POINT('Ctrl Pts',(-0.866025403784437,1.5,-6.09583333333334));
#368443=CARTESIAN_POINT('Ctrl Pts',(-1.29903810567666,0.750000000000002,
-6.05416666666667));
#368444=CARTESIAN_POINT('Ctrl Pts',(-1.73205080756887,3.39462250276711E-15,
-6.0125));
#368445=CARTESIAN_POINT('Ctrl Pts',(-1.29903810567666,-0.749999999999995,
-5.97083333333333));
#368446=CARTESIAN_POINT('Ctrl Pts',(-0.866025403784437,-1.49999999999999,
-5.92916666666667));
#368447=CARTESIAN_POINT('Ctrl Pts',(-1.83697019872103E-16,-1.49999999999999,
-5.8875));
#368448=CARTESIAN_POINT('Ctrl Pts',(0.866025403784436,-1.49999999999999,
-5.84583333333333));
#368449=CARTESIAN_POINT('Ctrl Pts',(1.29903810567665,-0.749999999999996,
-5.80416666666667));
#368450=CARTESIAN_POINT('Ctrl Pts',(1.73205080756887,2.86111848753058E-15,
-5.7625));
#368451=CARTESIAN_POINT('Ctrl Pts',(1.29903810567666,0.75,-5.72083333333333));
#368452=CARTESIAN_POINT('Ctrl Pts',(0.866025403784437,1.5,-5.67916666666667));
#368453=CARTESIAN_POINT('Ctrl Pts',(0.,1.5,-5.6375));
#368454=CARTESIAN_POINT('Ctrl Pts',(-0.866025403784437,1.5,-5.59583333333333));
#368455=CARTESIAN_POINT('Ctrl Pts',(-1.29903810567666,0.750000000000002,
-5.55416666666667));
#368456=CARTESIAN_POINT('Ctrl Pts',(-1.73205080756887,3.17607466327397E-15,
-5.5125));
#368457=CARTESIAN_POINT('Ctrl Pts',(-1.29903810567666,-0.749999999999995,
-5.47083333333333));
#368458=CARTESIAN_POINT('Ctrl Pts',(-0.866025403784437,-1.49999999999999,
-5.42916666666667));
#368459=CARTESIAN_POINT('Ctrl Pts',(-1.83697019872103E-16,-1.49999999999999,
-5.3875));
#368460=CARTESIAN_POINT('Ctrl Pts',(0.866025403784436,-1.49999999999999,
-5.34583333333333));
#368461=CARTESIAN_POINT('Ctrl Pts',(1.29903810567665,-0.749999999999996,
-5.30416666666667));
#368462=CARTESIAN_POINT('Ctrl Pts',(1.73205080756887,2.64257064803744E-15,
-5.2625));
#368463=CARTESIAN_POINT('Ctrl Pts',(1.29903810567666,0.75,-5.22083333333333));
#368464=CARTESIAN_POINT('Ctrl Pts',(0.866025403784437,1.5,-5.17916666666667));
#368465=CARTESIAN_POINT('Ctrl Pts',(0.,1.5,-5.1375));
#368466=CARTESIAN_POINT('Ctrl Pts',(-0.866025403784437,1.5,-5.09583333333333));
#368467=CARTESIAN_POINT('Ctrl Pts',(-1.29903810567666,0.750000000000002,
-5.05416666666667));
#368468=CARTESIAN_POINT('Ctrl Pts',(-1.73205080756887,2.95752682378083E-15,
-5.0125));
#368469=CARTESIAN_POINT('Ctrl Pts',(-1.29903810567666,-0.749999999999995,
-4.97083333333333));
#368470=CARTESIAN_POINT('Ctrl Pts',(-0.866025403784437,-1.49999999999999,
-4.92916666666667));
#368471=CARTESIAN_POINT('Ctrl Pts',(-1.83697019872103E-16,-1.49999999999999,
-4.8875));
#368472=CARTESIAN_POINT('Ctrl Pts',(0.866025403784436,-1.49999999999999,
-4.84583333333333));
#368473=CARTESIAN_POINT('Ctrl Pts',(1.29903810567665,-0.749999999999996,
-4.80416666666667));
#368474=CARTESIAN_POINT('Ctrl Pts',(1.73205080756887,2.4240228085443E-15,
-4.7625));
#368475=CARTESIAN_POINT('Ctrl Pts',(1.29903810567666,0.75,-4.72083333333333));
#368476=CARTESIAN_POINT('Ctrl Pts',(0.866025403784437,1.5,-4.67916666666667));
#368477=CARTESIAN_POINT('Ctrl Pts',(0.,1.5,-4.6375));
#368478=CARTESIAN_POINT('Ctrl Pts',(-0.866025403784437,1.5,-4.59583333333333));
#368479=CARTESIAN_POINT('Ctrl Pts',(-1.29903810567666,0.750000000000001,
-4.55416666666667));
#368480=CARTESIAN_POINT('Ctrl Pts',(-1.73205080756887,2.73897898428769E-15,
-4.5125));
#368481=CARTESIAN_POINT('Ctrl Pts',(-1.29903810567666,-0.749999999999995,
-4.47083333333333));
#368482=CARTESIAN_POINT('Ctrl Pts',(-0.866025403784437,-1.49999999999999,
-4.42916666666667));
#368483=CARTESIAN_POINT('Ctrl Pts',(-1.83697019872103E-16,-1.49999999999999,
-4.3875));
#368484=CARTESIAN_POINT('Ctrl Pts',(0.866025403784436,-1.49999999999999,
-4.34583333333333));
#368485=CARTESIAN_POINT('Ctrl Pts',(1.29903810567665,-0.749999999999996,
-4.30416666666667));
#368486=CARTESIAN_POINT('Ctrl Pts',(1.73205080756887,2.20547496905115E-15,
-4.2625));
#368487=CARTESIAN_POINT('Ctrl Pts',(1.29903810567666,0.75,-4.22083333333333));
#368488=CARTESIAN_POINT('Ctrl Pts',(0.866025403784437,1.5,-4.17916666666667));
#368489=CARTESIAN_POINT('Ctrl Pts',(0.,1.5,-4.1375));
#368490=CARTESIAN_POINT('Ctrl Pts',(-0.866025403784437,1.5,-4.09583333333333));
#368491=CARTESIAN_POINT('Ctrl Pts',(-1.29903810567666,0.750000000000001,
-4.05416666666667));
#368492=CARTESIAN_POINT('Ctrl Pts',(-1.73205080756887,2.52043114479455E-15,
-4.0125));
#368493=CARTESIAN_POINT('Ctrl Pts',(-1.29903810567666,-0.749999999999996,
-3.97083333333333));
#368494=CARTESIAN_POINT('Ctrl Pts',(-0.866025403784437,-1.49999999999999,
-3.92916666666667));
#368495=CARTESIAN_POINT('Ctrl Pts',(-1.83697019872103E-16,-1.49999999999999,
-3.8875));
#368496=CARTESIAN_POINT('Ctrl Pts',(0.866025403784436,-1.49999999999999,
-3.84583333333333));
#368497=CARTESIAN_POINT('Ctrl Pts',(1.29903810567665,-0.749999999999997,
-3.80416666666667));
#368498=CARTESIAN_POINT('Ctrl Pts',(1.73205080756887,1.98692712955801E-15,
-3.7625));
#368499=CARTESIAN_POINT('Ctrl Pts',(1.29903810567666,0.749999999999999,
-3.72083333333333));
#368500=CARTESIAN_POINT('Ctrl Pts',(0.866025403784437,1.5,-3.67916666666667));
#368501=CARTESIAN_POINT('Ctrl Pts',(0.,1.5,-3.6375));
#368502=CARTESIAN_POINT('Ctrl Pts',(-0.866025403784437,1.5,-3.59583333333333));
#368503=CARTESIAN_POINT('Ctrl Pts',(-1.29903810567666,0.750000000000001,
-3.55416666666667));
#368504=CARTESIAN_POINT('Ctrl Pts',(-1.73205080756887,2.3018833053014E-15,
-3.5125));
#368505=CARTESIAN_POINT('Ctrl Pts',(-1.29903810567666,-0.749999999999996,
-3.47083333333333));
#368506=CARTESIAN_POINT('Ctrl Pts',(-0.866025403784437,-1.49999999999999,
-3.42916666666667));
#368507=CARTESIAN_POINT('Ctrl Pts',(-1.83697019872103E-16,-1.49999999999999,
-3.3875));
#368508=CARTESIAN_POINT('Ctrl Pts',(0.866025403784436,-1.5,-3.34583333333333));
#368509=CARTESIAN_POINT('Ctrl Pts',(1.29903810567665,-0.749999999999997,
-3.30416666666667));
#368510=CARTESIAN_POINT('Ctrl Pts',(1.73205080756887,1.76837929006487E-15,
-3.2625));
#368511=CARTESIAN_POINT('Ctrl Pts',(1.29903810567666,0.749999999999999,
-3.22083333333333));
#368512=CARTESIAN_POINT('Ctrl Pts',(0.866025403784437,1.5,-3.17916666666667));
#368513=CARTESIAN_POINT('Ctrl Pts',(0.,1.5,-3.1375));
#368514=CARTESIAN_POINT('Ctrl Pts',(-0.866025403784437,1.5,-3.09583333333333));
#368515=CARTESIAN_POINT('Ctrl Pts',(-1.29903810567666,0.750000000000001,
-3.05416666666667));
#368516=CARTESIAN_POINT('Ctrl Pts',(-1.73205080756887,2.08333546580826E-15,
-3.0125));
#368517=CARTESIAN_POINT('Ctrl Pts',(-1.29903810567666,-0.749999999999996,
-2.97083333333333));
#368518=CARTESIAN_POINT('Ctrl Pts',(-0.866025403784437,-1.49999999999999,
-2.92916666666667));
#368519=CARTESIAN_POINT('Ctrl Pts',(-1.83697019872103E-16,-1.49999999999999,
-2.8875));
#368520=CARTESIAN_POINT('Ctrl Pts',(0.866025403784436,-1.5,-2.84583333333333));
#368521=CARTESIAN_POINT('Ctrl Pts',(1.29903810567665,-0.749999999999997,
-2.80416666666667));
#368522=CARTESIAN_POINT('Ctrl Pts',(1.73205080756887,1.54983145057173E-15,
-2.7625));
#368523=CARTESIAN_POINT('Ctrl Pts',(1.29903810567666,0.749999999999999,
-2.72083333333333));
#368524=CARTESIAN_POINT('Ctrl Pts',(0.866025403784437,1.5,-2.67916666666667));
#368525=CARTESIAN_POINT('Ctrl Pts',(0.,1.5,-2.6375));
#368526=CARTESIAN_POINT('Ctrl Pts',(-0.866025403784437,1.5,-2.59583333333333));
#368527=CARTESIAN_POINT('Ctrl Pts',(-1.29903810567666,0.75,-2.55416666666667));
#368528=CARTESIAN_POINT('Ctrl Pts',(-1.73205080756887,1.86478762631512E-15,
-2.5125));
#368529=CARTESIAN_POINT('Ctrl Pts',(-1.29903810567666,-0.749999999999996,
-2.47083333333333));
#368530=CARTESIAN_POINT('Ctrl Pts',(-0.866025403784437,-1.49999999999999,
-2.42916666666667));
#368531=CARTESIAN_POINT('Ctrl Pts',(-1.83697019872103E-16,-1.5,-2.3875));
#368532=CARTESIAN_POINT('Ctrl Pts',(0.866025403784436,-1.5,-2.34583333333333));
#368533=CARTESIAN_POINT('Ctrl Pts',(1.29903810567665,-0.749999999999997,
-2.30416666666667));
#368534=CARTESIAN_POINT('Ctrl Pts',(1.73205080756887,1.33128361107859E-15,
-2.2625));
#368535=CARTESIAN_POINT('Ctrl Pts',(1.29903810567666,0.749999999999999,
-2.22083333333333));
#368536=CARTESIAN_POINT('Ctrl Pts',(0.866025403784437,1.5,-2.17916666666667));
#368537=CARTESIAN_POINT('Ctrl Pts',(0.,1.5,-2.1375));
#368538=CARTESIAN_POINT('Ctrl Pts',(-0.866025403784437,1.5,-2.09583333333333));
#368539=CARTESIAN_POINT('Ctrl Pts',(-1.29903810567666,0.75,-2.05416666666667));
#368540=CARTESIAN_POINT('Ctrl Pts',(-1.73205080756887,1.64623978682198E-15,
-2.0125));
#368541=CARTESIAN_POINT('Ctrl Pts',(-1.29903810567666,-0.749999999999996,
-1.97083333333333));
#368542=CARTESIAN_POINT('Ctrl Pts',(-0.866025403784437,-1.49999999999999,
-1.92916666666667));
#368543=CARTESIAN_POINT('Ctrl Pts',(-1.83697019872103E-16,-1.5,-1.8875));
#368544=CARTESIAN_POINT('Ctrl Pts',(0.866025403784436,-1.5,-1.84583333333334));
#368545=CARTESIAN_POINT('Ctrl Pts',(1.29903810567665,-0.749999999999998,
-1.80416666666667));
#368546=CARTESIAN_POINT('Ctrl Pts',(1.73205080756887,1.11273577158545E-15,
-1.7625));
#368547=CARTESIAN_POINT('Ctrl Pts',(1.29903810567666,0.749999999999999,
-1.72083333333333));
#368548=CARTESIAN_POINT('Ctrl Pts',(0.866025403784437,1.5,-1.67916666666667));
#368549=CARTESIAN_POINT('Ctrl Pts',(0.,1.5,-1.6375));
#368550=CARTESIAN_POINT('Ctrl Pts',(-1.43925448419918E-16,-1.17524047358083,
-2.2));
#368551=CARTESIAN_POINT('Ctrl Pts',(0.678525403784435,-1.17524047358083,
-2.15833333333333));
#368552=CARTESIAN_POINT('Ctrl Pts',(1.01778810567665,-0.587620236790414,
-2.11666666666667));
#368553=CARTESIAN_POINT('Ctrl Pts',(1.35705080756887,1.3182145537207E-15,
-2.075));
#368554=CARTESIAN_POINT('Ctrl Pts',(1.01778810567665,0.587620236790415,
-2.03333333333333));
#368555=CARTESIAN_POINT('Ctrl Pts',(0.678525403784436,1.17524047358083,
-1.99166666666667));
#368556=CARTESIAN_POINT('Ctrl Pts',(0.,1.17524047358083,-1.95));
#368557=CARTESIAN_POINT('Ctrl Pts',(-0.678525403784435,1.17524047358083,
-1.90833333333333));
#368558=CARTESIAN_POINT('Ctrl Pts',(-1.01778810567665,0.587620236790416,
-1.86666666666667));
#368559=CARTESIAN_POINT('Ctrl Pts',(-1.35705080756887,1.54132221952804E-15,
-1.825));
#368560=CARTESIAN_POINT('Ctrl Pts',(-1.01778810567665,-0.587620236790413,
-1.78333333333333));
#368561=CARTESIAN_POINT('Ctrl Pts',(-0.678525403784426,-1.17524047358084,
-1.74166666666667));
#368562=CARTESIAN_POINT('Ctrl Pts',(-1.43925448419918E-16,-1.17524047358083,
-1.7));
#368563=CARTESIAN_POINT('Origin',(0.,-7.56339435525888E-14,-9.91875));
#368564=CARTESIAN_POINT('Ctrl Pts',(-1.43925448419918E-16,-1.17524047358083,
-2.1375));
#368565=CARTESIAN_POINT('Ctrl Pts',(0.678525403784435,-1.17524047358083,
-2.09583333333333));
#368566=CARTESIAN_POINT('Ctrl Pts',(1.01778810567665,-0.587620236790414,
-2.05416666666667));
#368567=CARTESIAN_POINT('Ctrl Pts',(1.35705080756887,1.29089607378406E-15,
-2.0125));
#368568=CARTESIAN_POINT('Ctrl Pts',(1.01778810567665,0.587620236790415,
-1.97083333333333));
#368569=CARTESIAN_POINT('Ctrl Pts',(0.678525403784436,1.17524047358083,
-1.92916666666667));
#368570=CARTESIAN_POINT('Ctrl Pts',(0.,1.17524047358083,-1.8875));
#368571=CARTESIAN_POINT('Ctrl Pts',(-0.678525403784435,1.17524047358083,
-1.84583333333333));
#368572=CARTESIAN_POINT('Ctrl Pts',(-1.01778810567665,0.587620236790416,
-1.80416666666667));
#368573=CARTESIAN_POINT('Ctrl Pts',(-1.35705080756887,1.5140037395914E-15,
-1.7625));
#368574=CARTESIAN_POINT('Ctrl Pts',(-1.01778810567665,-0.587620236790413,
-1.72083333333333));
#368575=CARTESIAN_POINT('Ctrl Pts',(-0.937699045799841,-0.726338557627476,
-1.71099716760418));
#368576=CARTESIAN_POINT('Ctrl Pts',(-0.823407874165093,-0.838564036615816,
-1.7));
#368577=CARTESIAN_POINT('Ctrl Pts',(0.,1.50000767573777,-9.69999556841073));
#368578=CARTESIAN_POINT('Ctrl Pts',(-0.866029835373706,1.50000767573777,
-9.65832890174406));
#368579=CARTESIAN_POINT('Ctrl Pts',(-1.29904475306056,0.75000383786889,
-9.6166622350774));
#368580=CARTESIAN_POINT('Ctrl Pts',(-1.73205967074741,4.95177446484038E-15,
-9.57499556841073));
#368581=CARTESIAN_POINT('Ctrl Pts',(-1.29904475306056,-0.75000383786888,
-9.53332890174407));
#368582=CARTESIAN_POINT('Ctrl Pts',(-0.866029835373706,-1.50000767573776,
-9.4916622350774));
#368583=CARTESIAN_POINT('Ctrl Pts',(-1.83697959878872E-16,-1.50000767573776,
-9.44999556841073));
#368584=CARTESIAN_POINT('Ctrl Pts',(0.866029835373705,-1.50000767573776,
-9.40832890174407));
#368585=CARTESIAN_POINT('Ctrl Pts',(1.29904475306056,-0.75000383786888,
-9.3666622350774));
#368586=CARTESIAN_POINT('Ctrl Pts',(1.73205967074741,4.4182682787512E-15,
-9.32499556841073));
#368587=CARTESIAN_POINT('Ctrl Pts',(1.29904475306056,0.750003837868888,
-9.28332890174407));
#368588=CARTESIAN_POINT('Ctrl Pts',(0.866029835373707,1.50000767573777,
-9.2416622350774));
#368589=CARTESIAN_POINT('Ctrl Pts',(0.,1.50000767573777,-9.19999556841073));
#368590=CARTESIAN_POINT('Ctrl Pts',(-0.866029835373706,1.50000767573777,
-9.15832890174407));
#368591=CARTESIAN_POINT('Ctrl Pts',(-1.29904475306056,0.750003837868889,
-9.1166622350774));
#368592=CARTESIAN_POINT('Ctrl Pts',(-1.73205967074741,4.73322662534724E-15,
-9.07499556841073));
#368593=CARTESIAN_POINT('Ctrl Pts',(-1.29904475306056,-0.75000383786888,
-9.03332890174407));
#368594=CARTESIAN_POINT('Ctrl Pts',(-0.866029835373706,-1.50000767573776,
-8.9916622350774));
#368595=CARTESIAN_POINT('Ctrl Pts',(-1.83697959878872E-16,-1.50000767573776,
-8.94999556841073));
#368596=CARTESIAN_POINT('Ctrl Pts',(0.866029835373705,-1.50000767573776,
-8.90832890174407));
#368597=CARTESIAN_POINT('Ctrl Pts',(1.29904475306056,-0.750003837868881,
-8.8666622350774));
#368598=CARTESIAN_POINT('Ctrl Pts',(1.73205967074741,4.19972043925806E-15,
-8.82499556841073));
#368599=CARTESIAN_POINT('Ctrl Pts',(1.29904475306056,0.750003837868888,
-8.78332890174407));
#368600=CARTESIAN_POINT('Ctrl Pts',(0.866029835373707,1.50000767573777,
-8.7416622350774));
#368601=CARTESIAN_POINT('Ctrl Pts',(0.,1.50000767573777,-8.69999556841073));
#368602=CARTESIAN_POINT('Ctrl Pts',(-0.866029835373706,1.50000767573777,
-8.65832890174407));
#368603=CARTESIAN_POINT('Ctrl Pts',(-1.29904475306056,0.750003837868889,
-8.6166622350774));
#368604=CARTESIAN_POINT('Ctrl Pts',(-1.73205967074741,4.5146787858541E-15,
-8.57499556841073));
#368605=CARTESIAN_POINT('Ctrl Pts',(-1.29904475306056,-0.75000383786888,
-8.53332890174406));
#368606=CARTESIAN_POINT('Ctrl Pts',(-0.866029835373706,-1.50000767573776,
-8.4916622350774));
#368607=CARTESIAN_POINT('Ctrl Pts',(-1.83697959878872E-16,-1.50000767573776,
-8.44999556841073));
#368608=CARTESIAN_POINT('Ctrl Pts',(0.866029835373705,-1.50000767573776,
-8.40832890174406));
#368609=CARTESIAN_POINT('Ctrl Pts',(1.29904475306056,-0.750003837868881,
-8.3666622350774));
#368610=CARTESIAN_POINT('Ctrl Pts',(1.73205967074741,3.98117259976492E-15,
-8.32499556841073));
#368611=CARTESIAN_POINT('Ctrl Pts',(1.29904475306056,0.750003837868888,
-8.28332890174407));
#368612=CARTESIAN_POINT('Ctrl Pts',(0.866029835373707,1.50000767573777,
-8.2416622350774));
#368613=CARTESIAN_POINT('Ctrl Pts',(0.,1.50000767573777,-8.19999556841073));
#368614=CARTESIAN_POINT('Ctrl Pts',(-0.866029835373706,1.50000767573777,
-8.15832890174407));
#368615=CARTESIAN_POINT('Ctrl Pts',(-1.29904475306056,0.750003837868889,
-8.1166622350774));
#368616=CARTESIAN_POINT('Ctrl Pts',(-1.73205967074741,4.29613094636096E-15,
-8.07499556841073));
#368617=CARTESIAN_POINT('Ctrl Pts',(-1.29904475306056,-0.75000383786888,
-8.03332890174407));
#368618=CARTESIAN_POINT('Ctrl Pts',(-0.866029835373706,-1.50000767573776,
-7.9916622350774));
#368619=CARTESIAN_POINT('Ctrl Pts',(-1.83697959878872E-16,-1.50000767573776,
-7.94999556841073));
#368620=CARTESIAN_POINT('Ctrl Pts',(0.866029835373705,-1.50000767573776,
-7.90832890174407));
#368621=CARTESIAN_POINT('Ctrl Pts',(1.29904475306056,-0.750003837868881,
-7.8666622350774));
#368622=CARTESIAN_POINT('Ctrl Pts',(1.73205967074741,3.76262476027178E-15,
-7.82499556841073));
#368623=CARTESIAN_POINT('Ctrl Pts',(1.29904475306056,0.750003837868888,
-7.78332890174406));
#368624=CARTESIAN_POINT('Ctrl Pts',(0.866029835373707,1.50000767573777,
-7.7416622350774));
#368625=CARTESIAN_POINT('Ctrl Pts',(0.,1.50000767573777,-7.69999556841073));
#368626=CARTESIAN_POINT('Ctrl Pts',(-0.866029835373706,1.50000767573777,
-7.65832890174406));
#368627=CARTESIAN_POINT('Ctrl Pts',(-1.29904475306056,0.750003837868889,
-7.6166622350774));
#368628=CARTESIAN_POINT('Ctrl Pts',(-1.73205967074741,4.07758310686782E-15,
-7.57499556841073));
#368629=CARTESIAN_POINT('Ctrl Pts',(-1.29904475306056,-0.75000383786888,
-7.53332890174407));
#368630=CARTESIAN_POINT('Ctrl Pts',(-0.866029835373706,-1.50000767573776,
-7.4916622350774));
#368631=CARTESIAN_POINT('Ctrl Pts',(-1.83697959878872E-16,-1.50000767573777,
-7.44999556841073));
#368632=CARTESIAN_POINT('Ctrl Pts',(0.866029835373705,-1.50000767573777,
-7.40832890174406));
#368633=CARTESIAN_POINT('Ctrl Pts',(1.29904475306056,-0.750003837868881,
-7.3666622350774));
#368634=CARTESIAN_POINT('Ctrl Pts',(1.73205967074741,3.54407692077864E-15,
-7.32499556841073));
#368635=CARTESIAN_POINT('Ctrl Pts',(1.29904475306056,0.750003837868887,
-7.28332890174406));
#368636=CARTESIAN_POINT('Ctrl Pts',(0.866029835373707,1.50000767573777,
-7.2416622350774));
#368637=CARTESIAN_POINT('Ctrl Pts',(0.,1.50000767573777,-7.19999556841073));
#368638=CARTESIAN_POINT('Ctrl Pts',(-0.866029835373706,1.50000767573777,
-7.15832890174407));
#368639=CARTESIAN_POINT('Ctrl Pts',(-1.29904475306056,0.750003837868889,
-7.1166622350774));
#368640=CARTESIAN_POINT('Ctrl Pts',(-1.73205967074741,3.85903526737468E-15,
-7.07499556841073));
#368641=CARTESIAN_POINT('Ctrl Pts',(-1.29904475306056,-0.750003837868881,
-7.03332890174407));
#368642=CARTESIAN_POINT('Ctrl Pts',(-0.866029835373706,-1.50000767573776,
-6.9916622350774));
#368643=CARTESIAN_POINT('Ctrl Pts',(-1.83697959878872E-16,-1.50000767573777,
-6.94999556841073));
#368644=CARTESIAN_POINT('Ctrl Pts',(0.866029835373705,-1.50000767573777,
-6.90832890174407));
#368645=CARTESIAN_POINT('Ctrl Pts',(1.29904475306056,-0.750003837868882,
-6.8666622350774));
#368646=CARTESIAN_POINT('Ctrl Pts',(1.73205967074741,3.3255290812855E-15,
-6.82499556841073));
#368647=CARTESIAN_POINT('Ctrl Pts',(1.29904475306056,0.750003837868887,
-6.78332890174407));
#368648=CARTESIAN_POINT('Ctrl Pts',(0.866029835373707,1.50000767573777,
-6.7416622350774));
#368649=CARTESIAN_POINT('Ctrl Pts',(0.,1.50000767573777,-6.69999556841073));
#368650=CARTESIAN_POINT('Ctrl Pts',(-0.866029835373706,1.50000767573777,
-6.65832890174406));
#368651=CARTESIAN_POINT('Ctrl Pts',(-1.29904475306056,0.750003837868888,
-6.6166622350774));
#368652=CARTESIAN_POINT('Ctrl Pts',(-1.73205967074741,3.64048742788154E-15,
-6.57499556841073));
#368653=CARTESIAN_POINT('Ctrl Pts',(-1.29904475306056,-0.750003837868881,
-6.53332890174406));
#368654=CARTESIAN_POINT('Ctrl Pts',(-0.866029835373706,-1.50000767573776,
-6.4916622350774));
#368655=CARTESIAN_POINT('Ctrl Pts',(-1.83697959878872E-16,-1.50000767573777,
-6.44999556841073));
#368656=CARTESIAN_POINT('Ctrl Pts',(0.866029835373705,-1.50000767573777,
-6.40832890174407));
#368657=CARTESIAN_POINT('Ctrl Pts',(1.29904475306056,-0.750003837868882,
-6.3666622350774));
#368658=CARTESIAN_POINT('Ctrl Pts',(1.73205967074741,3.10698124179236E-15,
-6.32499556841073));
#368659=CARTESIAN_POINT('Ctrl Pts',(1.29904475306056,0.750003837868887,
-6.28332890174407));
#368660=CARTESIAN_POINT('Ctrl Pts',(0.866029835373707,1.50000767573777,
-6.2416622350774));
#368661=CARTESIAN_POINT('Ctrl Pts',(0.,1.50000767573777,-6.19999556841073));
#368662=CARTESIAN_POINT('Ctrl Pts',(-0.866029835373706,1.50000767573777,
-6.15832890174407));
#368663=CARTESIAN_POINT('Ctrl Pts',(-1.29904475306056,0.750003837868888,
-6.1166622350774));
#368664=CARTESIAN_POINT('Ctrl Pts',(-1.73205967074741,3.42193958838839E-15,
-6.07499556841073));
#368665=CARTESIAN_POINT('Ctrl Pts',(-1.29904475306056,-0.750003837868881,
-6.03332890174406));
#368666=CARTESIAN_POINT('Ctrl Pts',(-0.866029835373706,-1.50000767573776,
-5.9916622350774));
#368667=CARTESIAN_POINT('Ctrl Pts',(-1.83697959878872E-16,-1.50000767573777,
-5.94999556841073));
#368668=CARTESIAN_POINT('Ctrl Pts',(0.866029835373705,-1.50000767573777,
-5.90832890174406));
#368669=CARTESIAN_POINT('Ctrl Pts',(1.29904475306056,-0.750003837868882,
-5.8666622350774));
#368670=CARTESIAN_POINT('Ctrl Pts',(1.73205967074741,2.88843340229921E-15,
-5.82499556841073));
#368671=CARTESIAN_POINT('Ctrl Pts',(1.29904475306056,0.750003837868887,
-5.78332890174407));
#368672=CARTESIAN_POINT('Ctrl Pts',(0.866029835373707,1.50000767573777,
-5.7416622350774));
#368673=CARTESIAN_POINT('Ctrl Pts',(0.,1.50000767573777,-5.69999556841073));
#368674=CARTESIAN_POINT('Ctrl Pts',(-0.866029835373706,1.50000767573777,
-5.65832890174406));
#368675=CARTESIAN_POINT('Ctrl Pts',(-1.29904475306056,0.750003837868888,
-5.6166622350774));
#368676=CARTESIAN_POINT('Ctrl Pts',(-1.73205967074741,3.20339174889525E-15,
-5.57499556841073));
#368677=CARTESIAN_POINT('Ctrl Pts',(-1.29904475306056,-0.750003837868881,
-5.53332890174407));
#368678=CARTESIAN_POINT('Ctrl Pts',(-0.866029835373706,-1.50000767573776,
-5.4916622350774));
#368679=CARTESIAN_POINT('Ctrl Pts',(-1.83697959878872E-16,-1.50000767573777,
-5.44999556841073));
#368680=CARTESIAN_POINT('Ctrl Pts',(0.866029835373705,-1.50000767573777,
-5.40832890174406));
#368681=CARTESIAN_POINT('Ctrl Pts',(1.29904475306056,-0.750003837868882,
-5.3666622350774));
#368682=CARTESIAN_POINT('Ctrl Pts',(1.73205967074741,2.66988556280607E-15,
-5.32499556841073));
#368683=CARTESIAN_POINT('Ctrl Pts',(1.29904475306056,0.750003837868886,
-5.28332890174406));
#368684=CARTESIAN_POINT('Ctrl Pts',(0.866029835373707,1.50000767573777,
-5.2416622350774));
#368685=CARTESIAN_POINT('Ctrl Pts',(0.,1.50000767573777,-5.19999556841073));
#368686=CARTESIAN_POINT('Ctrl Pts',(-0.866029835373706,1.50000767573777,
-5.15832890174406));
#368687=CARTESIAN_POINT('Ctrl Pts',(-1.29904475306056,0.750003837868888,
-5.1166622350774));
#368688=CARTESIAN_POINT('Ctrl Pts',(-1.73205967074741,2.98484390940211E-15,
-5.07499556841073));
#368689=CARTESIAN_POINT('Ctrl Pts',(-1.29904475306056,-0.750003837868881,
-5.03332890174407));
#368690=CARTESIAN_POINT('Ctrl Pts',(-0.866029835373706,-1.50000767573777,
-4.9916622350774));
#368691=CARTESIAN_POINT('Ctrl Pts',(-1.83697959878872E-16,-1.50000767573777,
-4.94999556841073));
#368692=CARTESIAN_POINT('Ctrl Pts',(0.866029835373705,-1.50000767573777,
-4.90832890174407));
#368693=CARTESIAN_POINT('Ctrl Pts',(1.29904475306056,-0.750003837868882,
-4.8666622350774));
#368694=CARTESIAN_POINT('Ctrl Pts',(1.73205967074741,2.45133772331293E-15,
-4.82499556841073));
#368695=CARTESIAN_POINT('Ctrl Pts',(1.29904475306056,0.750003837868886,
-4.78332890174407));
#368696=CARTESIAN_POINT('Ctrl Pts',(0.866029835373707,1.50000767573777,
-4.7416622350774));
#368697=CARTESIAN_POINT('Ctrl Pts',(0.,1.50000767573777,-4.69999556841073));
#368698=CARTESIAN_POINT('Ctrl Pts',(-0.866029835373706,1.50000767573777,
-4.65832890174406));
#368699=CARTESIAN_POINT('Ctrl Pts',(-1.29904475306056,0.750003837868888,
-4.6166622350774));
#368700=CARTESIAN_POINT('Ctrl Pts',(-1.73205967074741,2.76629606990897E-15,
-4.57499556841073));
#368701=CARTESIAN_POINT('Ctrl Pts',(-1.29904475306056,-0.750003837868882,
-4.53332890174406));
#368702=CARTESIAN_POINT('Ctrl Pts',(-0.866029835373706,-1.50000767573777,
-4.4916622350774));
#368703=CARTESIAN_POINT('Ctrl Pts',(-1.83697959878872E-16,-1.50000767573777,
-4.44999556841073));
#368704=CARTESIAN_POINT('Ctrl Pts',(0.866029835373705,-1.50000767573777,
-4.40832890174406));
#368705=CARTESIAN_POINT('Ctrl Pts',(1.29904475306056,-0.750003837868883,
-4.3666622350774));
#368706=CARTESIAN_POINT('Ctrl Pts',(1.73205967074741,2.23278988381979E-15,
-4.32499556841073));
#368707=CARTESIAN_POINT('Ctrl Pts',(1.29904475306056,0.750003837868886,
-4.28332890174406));
#368708=CARTESIAN_POINT('Ctrl Pts',(0.866029835373707,1.50000767573777,
-4.2416622350774));
#368709=CARTESIAN_POINT('Ctrl Pts',(0.,1.50000767573777,-4.19999556841073));
#368710=CARTESIAN_POINT('Ctrl Pts',(-0.866029835373706,1.50000767573777,
-4.15832890174406));
#368711=CARTESIAN_POINT('Ctrl Pts',(-1.29904475306056,0.750003837868887,
-4.1166622350774));
#368712=CARTESIAN_POINT('Ctrl Pts',(-1.73205967074741,2.54774823041583E-15,
-4.07499556841073));
#368713=CARTESIAN_POINT('Ctrl Pts',(-1.29904475306056,-0.750003837868882,
-4.03332890174407));
#368714=CARTESIAN_POINT('Ctrl Pts',(-0.866029835373706,-1.50000767573777,
-3.9916622350774));
#368715=CARTESIAN_POINT('Ctrl Pts',(-1.83697959878872E-16,-1.50000767573777,
-3.94999556841073));
#368716=CARTESIAN_POINT('Ctrl Pts',(0.866029835373705,-1.50000767573777,
-3.90832890174407));
#368717=CARTESIAN_POINT('Ctrl Pts',(1.29904475306056,-0.750003837868883,
-3.8666622350774));
#368718=CARTESIAN_POINT('Ctrl Pts',(1.73205967074741,2.01424204432665E-15,
-3.82499556841073));
#368719=CARTESIAN_POINT('Ctrl Pts',(1.29904475306056,0.750003837868886,
-3.78332890174407));
#368720=CARTESIAN_POINT('Ctrl Pts',(0.866029835373707,1.50000767573777,
-3.7416622350774));
#368721=CARTESIAN_POINT('Ctrl Pts',(0.,1.50000767573777,-3.69999556841073));
#368722=CARTESIAN_POINT('Ctrl Pts',(-0.866029835373706,1.50000767573777,
-3.65832890174407));
#368723=CARTESIAN_POINT('Ctrl Pts',(-1.29904475306056,0.750003837868887,
-3.6166622350774));
#368724=CARTESIAN_POINT('Ctrl Pts',(-1.73205967074741,2.32920039092269E-15,
-3.57499556841073));
#368725=CARTESIAN_POINT('Ctrl Pts',(-1.29904475306056,-0.750003837868882,
-3.53332890174406));
#368726=CARTESIAN_POINT('Ctrl Pts',(-0.866029835373706,-1.50000767573777,
-3.4916622350774));
#368727=CARTESIAN_POINT('Ctrl Pts',(-1.83697959878872E-16,-1.50000767573777,
-3.44999556841073));
#368728=CARTESIAN_POINT('Ctrl Pts',(0.866029835373705,-1.50000767573777,
-3.40832890174406));
#368729=CARTESIAN_POINT('Ctrl Pts',(1.29904475306056,-0.750003837868883,
-3.3666622350774));
#368730=CARTESIAN_POINT('Ctrl Pts',(1.73205967074741,1.79569420483351E-15,
-3.32499556841073));
#368731=CARTESIAN_POINT('Ctrl Pts',(1.29904475306056,0.750003837868886,
-3.28332890174406));
#368732=CARTESIAN_POINT('Ctrl Pts',(0.866029835373707,1.50000767573777,
-3.2416622350774));
#368733=CARTESIAN_POINT('Ctrl Pts',(0.,1.50000767573777,-3.19999556841073));
#368734=CARTESIAN_POINT('Ctrl Pts',(-0.866029835373706,1.50000767573777,
-3.15832890174406));
#368735=CARTESIAN_POINT('Ctrl Pts',(-1.29904475306056,0.750003837868887,
-3.1166622350774));
#368736=CARTESIAN_POINT('Ctrl Pts',(-1.73205967074741,2.11065255142955E-15,
-3.07499556841073));
#368737=CARTESIAN_POINT('Ctrl Pts',(-1.29904475306056,-0.750003837868882,
-3.03332890174407));
#368738=CARTESIAN_POINT('Ctrl Pts',(-0.866029835373706,-1.50000767573777,
-2.9916622350774));
#368739=CARTESIAN_POINT('Ctrl Pts',(-1.83697959878872E-16,-1.50000767573777,
-2.94999556841073));
#368740=CARTESIAN_POINT('Ctrl Pts',(0.866029835373705,-1.50000767573777,
-2.90832890174406));
#368741=CARTESIAN_POINT('Ctrl Pts',(1.29904475306056,-0.750003837868883,
-2.8666622350774));
#368742=CARTESIAN_POINT('Ctrl Pts',(1.73205967074741,1.57714636534037E-15,
-2.82499556841073));
#368743=CARTESIAN_POINT('Ctrl Pts',(1.29904475306056,0.750003837868885,
-2.78332890174406));
#368744=CARTESIAN_POINT('Ctrl Pts',(0.866029835373707,1.50000767573777,
-2.7416622350774));
#368745=CARTESIAN_POINT('Ctrl Pts',(0.,1.50000767573777,-2.69999556841073));
#368746=CARTESIAN_POINT('Ctrl Pts',(-0.866029835373706,1.50000767573777,
-2.65832890174406));
#368747=CARTESIAN_POINT('Ctrl Pts',(-1.29904475306056,0.750003837868887,
-2.6166622350774));
#368748=CARTESIAN_POINT('Ctrl Pts',(-1.73205967074741,1.89210471193641E-15,
-2.57499556841073));
#368749=CARTESIAN_POINT('Ctrl Pts',(-1.29904475306056,-0.750003837868882,
-2.53332890174406));
#368750=CARTESIAN_POINT('Ctrl Pts',(-0.866029835373706,-1.50000767573777,
-2.4916622350774));
#368751=CARTESIAN_POINT('Ctrl Pts',(-1.83697959878872E-16,-1.50000767573777,
-2.44999556841073));
#368752=CARTESIAN_POINT('Ctrl Pts',(0.866029835373705,-1.50000767573777,
-2.40832890174406));
#368753=CARTESIAN_POINT('Ctrl Pts',(1.29904475306056,-0.750003837868884,
-2.3666622350774));
#368754=CARTESIAN_POINT('Ctrl Pts',(1.73205967074741,1.35859852584723E-15,
-2.32499556841073));
#368755=CARTESIAN_POINT('Ctrl Pts',(1.29904475306056,0.750003837868885,
-2.28332890174407));
#368756=CARTESIAN_POINT('Ctrl Pts',(0.866029835373707,1.50000767573777,
-2.2416622350774));
#368757=CARTESIAN_POINT('Ctrl Pts',(0.,1.50000767573777,-2.19999556841073));
#368758=CARTESIAN_POINT('Ctrl Pts',(-0.866029835373706,1.50000767573777,
-2.15832890174407));
#368759=CARTESIAN_POINT('Ctrl Pts',(-1.29904475306056,0.750003837868886,
-2.1166622350774));
#368760=CARTESIAN_POINT('Ctrl Pts',(-1.73205967074741,1.67355687244326E-15,
-2.07499556841073));
#368761=CARTESIAN_POINT('Ctrl Pts',(-1.29904475306056,-0.750003837868883,
-2.03332890174407));
#368762=CARTESIAN_POINT('Ctrl Pts',(-0.866029835373706,-1.50000767573777,
-1.9916622350774));
#368763=CARTESIAN_POINT('Ctrl Pts',(-1.83697959878872E-16,-1.50000767573777,
-1.94999556841073));
#368764=CARTESIAN_POINT('Ctrl Pts',(0.866029835373705,-1.50000767573777,
-1.90832890174406));
#368765=CARTESIAN_POINT('Ctrl Pts',(1.29904475306056,-0.750003837868884,
-1.8666622350774));
#368766=CARTESIAN_POINT('Ctrl Pts',(1.73205967074741,1.14005068635409E-15,
-1.82499556841073));
#368767=CARTESIAN_POINT('Ctrl Pts',(1.29904475306056,0.750003837868885,
-1.78332890174407));
#368768=CARTESIAN_POINT('Ctrl Pts',(0.866029835373707,1.50000767573777,
-1.7416622350774));
#368769=CARTESIAN_POINT('Ctrl Pts',(0.,1.50000767573777,-1.69999556841073));
#368770=CARTESIAN_POINT('Ctrl Pts',(-0.866029835373706,1.50000767573777,
-1.65832890174407));
#368771=CARTESIAN_POINT('Ctrl Pts',(-1.29904475306056,0.750003837868886,
-1.6166622350774));
#368772=CARTESIAN_POINT('Ctrl Pts',(-1.73205967074741,1.45500903295012E-15,
-1.57499556841073));
#368773=CARTESIAN_POINT('Ctrl Pts',(-1.29904475306056,-0.750003837868883,
-1.53332890174407));
#368774=CARTESIAN_POINT('Ctrl Pts',(-0.866029835373706,-1.50000767573777,
-1.4916622350774));
#368775=CARTESIAN_POINT('Ctrl Pts',(-1.83697959878872E-16,-1.50000767573777,
-1.44999556841073));
#368776=CARTESIAN_POINT('Ctrl Pts',(0.866029835373705,-1.50000767573777,
-1.40832890174407));
#368777=CARTESIAN_POINT('Ctrl Pts',(1.29904475306056,-0.750003837868884,
-1.3666622350774));
#368778=CARTESIAN_POINT('Ctrl Pts',(1.73205967074741,9.21502846860943E-16,
-1.32499556841073));
#368779=CARTESIAN_POINT('Ctrl Pts',(1.29904475306056,0.750003837868885,
-1.28332890174407));
#368780=CARTESIAN_POINT('Ctrl Pts',(0.866029835373707,1.50000767573777,
-1.2416622350774));
#368781=CARTESIAN_POINT('Ctrl Pts',(0.,1.50000767573777,-1.19999556841073));
#368782=CARTESIAN_POINT('Ctrl Pts',(0.,1.17524047358083,-9.8875));
#368783=CARTESIAN_POINT('Ctrl Pts',(-0.678525403784435,1.17524047358083,
-9.84583333333333));
#368784=CARTESIAN_POINT('Ctrl Pts',(-1.01778810567665,0.58762023679042,
-9.80416666666667));
#368785=CARTESIAN_POINT('Ctrl Pts',(-1.35705080756887,5.01076917148166E-15,
-9.7625));
#368786=CARTESIAN_POINT('Ctrl Pts',(-1.01778810567665,-0.58762023679041,
-9.72083333333333));
#368787=CARTESIAN_POINT('Ctrl Pts',(-0.678525403784435,-1.17524047358082,
-9.67916666666667));
#368788=CARTESIAN_POINT('Ctrl Pts',(-1.43925448419918E-16,-1.17524047358082,
-9.6375));
#368789=CARTESIAN_POINT('Ctrl Pts',(0.678525403784435,-1.17524047358082,
-9.59583333333333));
#368790=CARTESIAN_POINT('Ctrl Pts',(1.01778810567665,-0.58762023679041,
-9.55416666666667));
#368791=CARTESIAN_POINT('Ctrl Pts',(1.35705080756887,4.56911366618118E-15,
-9.5125));
#368792=CARTESIAN_POINT('Ctrl Pts',(1.01778810567665,0.587620236790419,
-9.47083333333333));
#368793=CARTESIAN_POINT('Ctrl Pts',(0.678525403784436,1.17524047358083,
-9.42916666666667));
#368794=CARTESIAN_POINT('Ctrl Pts',(0.,1.17524047358083,-9.3875));
#368795=CARTESIAN_POINT('Ctrl Pts',(-0.678525403784435,1.17524047358083,
-9.34583333333333));
#368796=CARTESIAN_POINT('Ctrl Pts',(-1.01778810567665,0.58762023679042,
-9.30416666666667));
#368797=CARTESIAN_POINT('Ctrl Pts',(-1.35705080756887,4.79222133198851E-15,
-9.2625));
#368798=CARTESIAN_POINT('Ctrl Pts',(-1.01778810567665,-0.58762023679041,
-9.22083333333333));
#368799=CARTESIAN_POINT('Ctrl Pts',(-0.678525403784435,-1.17524047358082,
-9.17916666666667));
#368800=CARTESIAN_POINT('Ctrl Pts',(-1.43925448419918E-16,-1.17524047358082,
-9.1375));
#368801=CARTESIAN_POINT('Ctrl Pts',(0.678525403784435,-1.17524047358083,
-9.09583333333333));
#368802=CARTESIAN_POINT('Ctrl Pts',(1.01778810567665,-0.587620236790411,
-9.05416666666667));
#368803=CARTESIAN_POINT('Ctrl Pts',(1.35705080756887,4.35056582668803E-15,
-9.0125));
#368804=CARTESIAN_POINT('Ctrl Pts',(1.01778810567665,0.587620236790418,
-8.97083333333333));
#368805=CARTESIAN_POINT('Ctrl Pts',(0.678525403784436,1.17524047358083,
-8.92916666666667));
#368806=CARTESIAN_POINT('Ctrl Pts',(0.,1.17524047358083,-8.8875));
#368807=CARTESIAN_POINT('Ctrl Pts',(-0.678525403784435,1.17524047358083,
-8.84583333333333));
#368808=CARTESIAN_POINT('Ctrl Pts',(-1.01778810567665,0.587620236790419,
-8.80416666666667));
#368809=CARTESIAN_POINT('Ctrl Pts',(-1.35705080756887,4.57367349249537E-15,
-8.7625));
#368810=CARTESIAN_POINT('Ctrl Pts',(-1.01778810567665,-0.58762023679041,
-8.72083333333333));
#368811=CARTESIAN_POINT('Ctrl Pts',(-0.678525403784435,-1.17524047358082,
-8.67916666666667));
#368812=CARTESIAN_POINT('Ctrl Pts',(-1.43925448419918E-16,-1.17524047358082,
-8.6375));
#368813=CARTESIAN_POINT('Ctrl Pts',(0.678525403784435,-1.17524047358083,
-8.59583333333333));
#368814=CARTESIAN_POINT('Ctrl Pts',(1.01778810567665,-0.587620236790411,
-8.55416666666667));
#368815=CARTESIAN_POINT('Ctrl Pts',(1.35705080756887,4.13201798719489E-15,
-8.5125));
#368816=CARTESIAN_POINT('Ctrl Pts',(1.01778810567665,0.587620236790418,
-8.47083333333333));
#368817=CARTESIAN_POINT('Ctrl Pts',(0.678525403784436,1.17524047358083,
-8.42916666666667));
#368818=CARTESIAN_POINT('Ctrl Pts',(0.,1.17524047358083,-8.3875));
#368819=CARTESIAN_POINT('Ctrl Pts',(-0.678525403784435,1.17524047358083,
-8.34583333333333));
#368820=CARTESIAN_POINT('Ctrl Pts',(-1.01778810567665,0.587620236790419,
-8.30416666666667));
#368821=CARTESIAN_POINT('Ctrl Pts',(-1.35705080756887,4.35512565300223E-15,
-8.2625));
#368822=CARTESIAN_POINT('Ctrl Pts',(-1.01778810567665,-0.58762023679041,
-8.22083333333333));
#368823=CARTESIAN_POINT('Ctrl Pts',(-0.678525403784435,-1.17524047358082,
-8.17916666666667));
#368824=CARTESIAN_POINT('Ctrl Pts',(-1.43925448419918E-16,-1.17524047358083,
-8.1375));
#368825=CARTESIAN_POINT('Ctrl Pts',(0.678525403784435,-1.17524047358083,
-8.09583333333333));
#368826=CARTESIAN_POINT('Ctrl Pts',(1.01778810567665,-0.587620236790411,
-8.05416666666667));
#368827=CARTESIAN_POINT('Ctrl Pts',(1.35705080756887,3.91347014770175E-15,
-8.0125));
#368828=CARTESIAN_POINT('Ctrl Pts',(1.01778810567665,0.587620236790418,
-7.97083333333333));
#368829=CARTESIAN_POINT('Ctrl Pts',(0.678525403784436,1.17524047358083,
-7.92916666666667));
#368830=CARTESIAN_POINT('Ctrl Pts',(0.,1.17524047358083,-7.8875));
#368831=CARTESIAN_POINT('Ctrl Pts',(-0.678525403784435,1.17524047358083,
-7.84583333333333));
#368832=CARTESIAN_POINT('Ctrl Pts',(-1.01778810567665,0.587620236790419,
-7.80416666666667));
#368833=CARTESIAN_POINT('Ctrl Pts',(-1.35705080756887,4.13657781350909E-15,
-7.7625));
#368834=CARTESIAN_POINT('Ctrl Pts',(-1.01778810567665,-0.58762023679041,
-7.72083333333333));
#368835=CARTESIAN_POINT('Ctrl Pts',(-0.678525403784435,-1.17524047358083,
-7.67916666666667));
#368836=CARTESIAN_POINT('Ctrl Pts',(-1.43925448419918E-16,-1.17524047358083,
-7.6375));
#368837=CARTESIAN_POINT('Ctrl Pts',(0.678525403784435,-1.17524047358083,
-7.59583333333333));
#368838=CARTESIAN_POINT('Ctrl Pts',(1.01778810567665,-0.587620236790411,
-7.55416666666667));
#368839=CARTESIAN_POINT('Ctrl Pts',(1.35705080756887,3.69492230820861E-15,
-7.5125));
#368840=CARTESIAN_POINT('Ctrl Pts',(1.01778810567665,0.587620236790418,
-7.47083333333333));
#368841=CARTESIAN_POINT('Ctrl Pts',(0.678525403784436,1.17524047358083,
-7.42916666666667));
#368842=CARTESIAN_POINT('Ctrl Pts',(0.,1.17524047358083,-7.3875));
#368843=CARTESIAN_POINT('Ctrl Pts',(-0.678525403784435,1.17524047358083,
-7.34583333333334));
#368844=CARTESIAN_POINT('Ctrl Pts',(-1.01778810567665,0.587620236790419,
-7.30416666666667));
#368845=CARTESIAN_POINT('Ctrl Pts',(-1.35705080756887,3.91802997401595E-15,
-7.2625));
#368846=CARTESIAN_POINT('Ctrl Pts',(-1.01778810567665,-0.587620236790411,
-7.22083333333333));
#368847=CARTESIAN_POINT('Ctrl Pts',(-0.678525403784435,-1.17524047358083,
-7.17916666666667));
#368848=CARTESIAN_POINT('Ctrl Pts',(-1.43925448419918E-16,-1.17524047358083,
-7.1375));
#368849=CARTESIAN_POINT('Ctrl Pts',(0.678525403784435,-1.17524047358083,
-7.09583333333333));
#368850=CARTESIAN_POINT('Ctrl Pts',(1.01778810567665,-0.587620236790411,
-7.05416666666667));
#368851=CARTESIAN_POINT('Ctrl Pts',(1.35705080756887,3.47637446871547E-15,
-7.0125));
#368852=CARTESIAN_POINT('Ctrl Pts',(1.01778810567665,0.587620236790417,
-6.97083333333333));
#368853=CARTESIAN_POINT('Ctrl Pts',(0.678525403784436,1.17524047358083,
-6.92916666666667));
#368854=CARTESIAN_POINT('Ctrl Pts',(0.,1.17524047358083,-6.8875));
#368855=CARTESIAN_POINT('Ctrl Pts',(-0.678525403784435,1.17524047358083,
-6.84583333333333));
#368856=CARTESIAN_POINT('Ctrl Pts',(-1.01778810567665,0.587620236790418,
-6.80416666666667));
#368857=CARTESIAN_POINT('Ctrl Pts',(-1.35705080756887,3.69948213452281E-15,
-6.7625));
#368858=CARTESIAN_POINT('Ctrl Pts',(-1.01778810567665,-0.587620236790411,
-6.72083333333333));
#368859=CARTESIAN_POINT('Ctrl Pts',(-0.678525403784435,-1.17524047358083,
-6.67916666666667));
#368860=CARTESIAN_POINT('Ctrl Pts',(-1.43925448419918E-16,-1.17524047358083,
-6.6375));
#368861=CARTESIAN_POINT('Ctrl Pts',(0.678525403784435,-1.17524047358083,
-6.59583333333333));
#368862=CARTESIAN_POINT('Ctrl Pts',(1.01778810567665,-0.587620236790412,
-6.55416666666667));
#368863=CARTESIAN_POINT('Ctrl Pts',(1.35705080756887,3.25782662922233E-15,
-6.5125));
#368864=CARTESIAN_POINT('Ctrl Pts',(1.01778810567665,0.587620236790417,
-6.47083333333333));
#368865=CARTESIAN_POINT('Ctrl Pts',(0.678525403784436,1.17524047358083,
-6.42916666666667));
#368866=CARTESIAN_POINT('Ctrl Pts',(0.,1.17524047358083,-6.3875));
#368867=CARTESIAN_POINT('Ctrl Pts',(-0.678525403784435,1.17524047358083,
-6.34583333333333));
#368868=CARTESIAN_POINT('Ctrl Pts',(-1.01778810567665,0.587620236790418,
-6.30416666666667));
#368869=CARTESIAN_POINT('Ctrl Pts',(-1.35705080756887,3.48093429502967E-15,
-6.2625));
#368870=CARTESIAN_POINT('Ctrl Pts',(-1.01778810567665,-0.587620236790411,
-6.22083333333333));
#368871=CARTESIAN_POINT('Ctrl Pts',(-0.678525403784435,-1.17524047358083,
-6.17916666666667));
#368872=CARTESIAN_POINT('Ctrl Pts',(-1.43925448419918E-16,-1.17524047358083,
-6.1375));
#368873=CARTESIAN_POINT('Ctrl Pts',(0.678525403784435,-1.17524047358083,
-6.09583333333333));
#368874=CARTESIAN_POINT('Ctrl Pts',(1.01778810567665,-0.587620236790412,
-6.05416666666667));
#368875=CARTESIAN_POINT('Ctrl Pts',(1.35705080756887,3.03927878972919E-15,
-6.0125));
#368876=CARTESIAN_POINT('Ctrl Pts',(1.01778810567665,0.587620236790417,
-5.97083333333333));
#368877=CARTESIAN_POINT('Ctrl Pts',(0.678525403784436,1.17524047358083,
-5.92916666666667));
#368878=CARTESIAN_POINT('Ctrl Pts',(0.,1.17524047358083,-5.8875));
#368879=CARTESIAN_POINT('Ctrl Pts',(-0.678525403784435,1.17524047358083,
-5.84583333333333));
#368880=CARTESIAN_POINT('Ctrl Pts',(-1.01778810567665,0.587620236790418,
-5.80416666666667));
#368881=CARTESIAN_POINT('Ctrl Pts',(-1.35705080756887,3.26238645553653E-15,
-5.7625));
#368882=CARTESIAN_POINT('Ctrl Pts',(-1.01778810567665,-0.587620236790411,
-5.72083333333333));
#368883=CARTESIAN_POINT('Ctrl Pts',(-0.678525403784435,-1.17524047358083,
-5.67916666666667));
#368884=CARTESIAN_POINT('Ctrl Pts',(-1.43925448419918E-16,-1.17524047358083,
-5.6375));
#368885=CARTESIAN_POINT('Ctrl Pts',(0.678525403784435,-1.17524047358083,
-5.59583333333333));
#368886=CARTESIAN_POINT('Ctrl Pts',(1.01778810567665,-0.587620236790412,
-5.55416666666667));
#368887=CARTESIAN_POINT('Ctrl Pts',(1.35705080756887,2.82073095023605E-15,
-5.5125));
#368888=CARTESIAN_POINT('Ctrl Pts',(1.01778810567665,0.587620236790417,
-5.47083333333333));
#368889=CARTESIAN_POINT('Ctrl Pts',(0.678525403784436,1.17524047358083,
-5.42916666666667));
#368890=CARTESIAN_POINT('Ctrl Pts',(0.,1.17524047358083,-5.3875));
#368891=CARTESIAN_POINT('Ctrl Pts',(-0.678525403784435,1.17524047358083,
-5.34583333333333));
#368892=CARTESIAN_POINT('Ctrl Pts',(-1.01778810567665,0.587620236790418,
-5.30416666666667));
#368893=CARTESIAN_POINT('Ctrl Pts',(-1.35705080756887,3.04383861604338E-15,
-5.2625));
#368894=CARTESIAN_POINT('Ctrl Pts',(-1.01778810567665,-0.587620236790411,
-5.22083333333333));
#368895=CARTESIAN_POINT('Ctrl Pts',(-0.678525403784435,-1.17524047358083,
-5.17916666666667));
#368896=CARTESIAN_POINT('Ctrl Pts',(-1.43925448419918E-16,-1.17524047358083,
-5.1375));
#368897=CARTESIAN_POINT('Ctrl Pts',(0.678525403784435,-1.17524047358083,
-5.09583333333333));
#368898=CARTESIAN_POINT('Ctrl Pts',(1.01778810567665,-0.587620236790412,
-5.05416666666667));
#368899=CARTESIAN_POINT('Ctrl Pts',(1.35705080756887,2.6021831107429E-15,
-5.0125));
#368900=CARTESIAN_POINT('Ctrl Pts',(1.01778810567665,0.587620236790417,
-4.97083333333333));
#368901=CARTESIAN_POINT('Ctrl Pts',(0.678525403784436,1.17524047358083,
-4.92916666666667));
#368902=CARTESIAN_POINT('Ctrl Pts',(0.,1.17524047358083,-4.8875));
#368903=CARTESIAN_POINT('Ctrl Pts',(-0.678525403784435,1.17524047358083,
-4.84583333333333));
#368904=CARTESIAN_POINT('Ctrl Pts',(-1.01778810567665,0.587620236790418,
-4.80416666666667));
#368905=CARTESIAN_POINT('Ctrl Pts',(-1.35705080756887,2.82529077655024E-15,
-4.7625));
#368906=CARTESIAN_POINT('Ctrl Pts',(-1.01778810567665,-0.587620236790412,
-4.72083333333333));
#368907=CARTESIAN_POINT('Ctrl Pts',(-0.678525403784435,-1.17524047358083,
-4.67916666666667));
#368908=CARTESIAN_POINT('Ctrl Pts',(-1.43925448419918E-16,-1.17524047358083,
-4.6375));
#368909=CARTESIAN_POINT('Ctrl Pts',(0.678525403784435,-1.17524047358083,
-4.59583333333333));
#368910=CARTESIAN_POINT('Ctrl Pts',(1.01778810567665,-0.587620236790413,
-4.55416666666667));
#368911=CARTESIAN_POINT('Ctrl Pts',(1.35705080756887,2.38363527124976E-15,
-4.5125));
#368912=CARTESIAN_POINT('Ctrl Pts',(1.01778810567665,0.587620236790416,
-4.47083333333333));
#368913=CARTESIAN_POINT('Ctrl Pts',(0.678525403784436,1.17524047358083,
-4.42916666666667));
#368914=CARTESIAN_POINT('Ctrl Pts',(0.,1.17524047358083,-4.3875));
#368915=CARTESIAN_POINT('Ctrl Pts',(-0.678525403784435,1.17524047358083,
-4.34583333333333));
#368916=CARTESIAN_POINT('Ctrl Pts',(-1.01778810567665,0.587620236790417,
-4.30416666666667));
#368917=CARTESIAN_POINT('Ctrl Pts',(-1.35705080756887,2.6067429370571E-15,
-4.2625));
#368918=CARTESIAN_POINT('Ctrl Pts',(-1.01778810567665,-0.587620236790412,
-4.22083333333333));
#368919=CARTESIAN_POINT('Ctrl Pts',(-0.678525403784435,-1.17524047358083,
-4.17916666666667));
#368920=CARTESIAN_POINT('Ctrl Pts',(-1.43925448419918E-16,-1.17524047358083,
-4.1375));
#368921=CARTESIAN_POINT('Ctrl Pts',(0.678525403784435,-1.17524047358083,
-4.09583333333333));
#368922=CARTESIAN_POINT('Ctrl Pts',(1.01778810567665,-0.587620236790413,
-4.05416666666667));
#368923=CARTESIAN_POINT('Ctrl Pts',(1.35705080756887,2.16508743175662E-15,
-4.0125));
#368924=CARTESIAN_POINT('Ctrl Pts',(1.01778810567665,0.587620236790416,
-3.97083333333333));
#368925=CARTESIAN_POINT('Ctrl Pts',(0.678525403784436,1.17524047358083,
-3.92916666666667));
#368926=CARTESIAN_POINT('Ctrl Pts',(0.,1.17524047358083,-3.8875));
#368927=CARTESIAN_POINT('Ctrl Pts',(-0.678525403784435,1.17524047358083,
-3.84583333333333));
#368928=CARTESIAN_POINT('Ctrl Pts',(-1.01778810567665,0.587620236790417,
-3.80416666666667));
#368929=CARTESIAN_POINT('Ctrl Pts',(-1.35705080756887,2.38819509756396E-15,
-3.7625));
#368930=CARTESIAN_POINT('Ctrl Pts',(-1.01778810567665,-0.587620236790412,
-3.72083333333333));
#368931=CARTESIAN_POINT('Ctrl Pts',(-0.678525403784435,-1.17524047358083,
-3.67916666666667));
#368932=CARTESIAN_POINT('Ctrl Pts',(-1.43925448419918E-16,-1.17524047358083,
-3.6375));
#368933=CARTESIAN_POINT('Ctrl Pts',(0.678525403784435,-1.17524047358083,
-3.59583333333333));
#368934=CARTESIAN_POINT('Ctrl Pts',(1.01778810567665,-0.587620236790413,
-3.55416666666667));
#368935=CARTESIAN_POINT('Ctrl Pts',(1.35705080756887,1.94653959226348E-15,
-3.5125));
#368936=CARTESIAN_POINT('Ctrl Pts',(1.01778810567665,0.587620236790416,
-3.47083333333333));
#368937=CARTESIAN_POINT('Ctrl Pts',(0.678525403784436,1.17524047358083,
-3.42916666666667));
#368938=CARTESIAN_POINT('Ctrl Pts',(0.,1.17524047358083,-3.3875));
#368939=CARTESIAN_POINT('Ctrl Pts',(-0.678525403784435,1.17524047358083,
-3.34583333333333));
#368940=CARTESIAN_POINT('Ctrl Pts',(-1.01778810567665,0.587620236790417,
-3.30416666666667));
#368941=CARTESIAN_POINT('Ctrl Pts',(-1.35705080756887,2.16964725807082E-15,
-3.2625));
#368942=CARTESIAN_POINT('Ctrl Pts',(-1.01778810567665,-0.587620236790412,
-3.22083333333333));
#368943=CARTESIAN_POINT('Ctrl Pts',(-0.678525403784435,-1.17524047358083,
-3.17916666666667));
#368944=CARTESIAN_POINT('Ctrl Pts',(-1.43925448419918E-16,-1.17524047358083,
-3.1375));
#368945=CARTESIAN_POINT('Ctrl Pts',(0.678525403784435,-1.17524047358083,
-3.09583333333333));
#368946=CARTESIAN_POINT('Ctrl Pts',(1.01778810567665,-0.587620236790413,
-3.05416666666667));
#368947=CARTESIAN_POINT('Ctrl Pts',(1.35705080756887,1.72799175277034E-15,
-3.0125));
#368948=CARTESIAN_POINT('Ctrl Pts',(1.01778810567665,0.587620236790416,
-2.97083333333333));
#368949=CARTESIAN_POINT('Ctrl Pts',(0.678525403784436,1.17524047358083,
-2.92916666666667));
#368950=CARTESIAN_POINT('Ctrl Pts',(0.,1.17524047358083,-2.8875));
#368951=CARTESIAN_POINT('Ctrl Pts',(-0.678525403784435,1.17524047358083,
-2.84583333333333));
#368952=CARTESIAN_POINT('Ctrl Pts',(-1.01778810567665,0.587620236790417,
-2.80416666666667));
#368953=CARTESIAN_POINT('Ctrl Pts',(-1.35705080756887,1.95109941857768E-15,
-2.7625));
#368954=CARTESIAN_POINT('Ctrl Pts',(-1.01778810567665,-0.587620236790413,
-2.72083333333333));
#368955=CARTESIAN_POINT('Ctrl Pts',(-0.678525403784435,-1.17524047358083,
-2.67916666666667));
#368956=CARTESIAN_POINT('Ctrl Pts',(-1.43925448419918E-16,-1.17524047358083,
-2.6375));
#368957=CARTESIAN_POINT('Ctrl Pts',(0.678525403784435,-1.17524047358083,
-2.59583333333333));
#368958=CARTESIAN_POINT('Ctrl Pts',(1.01778810567665,-0.587620236790414,
-2.55416666666667));
#368959=CARTESIAN_POINT('Ctrl Pts',(1.35705080756887,1.5094439132772E-15,
-2.5125));
#368960=CARTESIAN_POINT('Ctrl Pts',(1.01778810567665,0.587620236790415,
-2.47083333333333));
#368961=CARTESIAN_POINT('Ctrl Pts',(0.678525403784436,1.17524047358083,
-2.42916666666667));
#368962=CARTESIAN_POINT('Ctrl Pts',(0.,1.17524047358083,-2.3875));
#368963=CARTESIAN_POINT('Ctrl Pts',(-0.678525403784435,1.17524047358083,
-2.34583333333333));
#368964=CARTESIAN_POINT('Ctrl Pts',(-1.01778810567665,0.587620236790416,
-2.30416666666667));
#368965=CARTESIAN_POINT('Ctrl Pts',(-1.35705080756887,1.73255157908454E-15,
-2.2625));
#368966=CARTESIAN_POINT('Ctrl Pts',(-1.01778810567665,-0.587620236790413,
-2.22083333333333));
#368967=CARTESIAN_POINT('Ctrl Pts',(-0.678525403784435,-1.17524047358083,
-2.17916666666667));
#368968=CARTESIAN_POINT('Ctrl Pts',(-1.43925448419918E-16,-1.17524047358083,
-2.1375));
#368969=CARTESIAN_POINT('Ctrl Pts',(0.678525403784435,-1.17524047358083,
-2.09583333333333));
#368970=CARTESIAN_POINT('Ctrl Pts',(1.01778810567665,-0.587620236790414,
-2.05416666666667));
#368971=CARTESIAN_POINT('Ctrl Pts',(1.35705080756887,1.29089607378406E-15,
-2.0125));
#368972=CARTESIAN_POINT('Ctrl Pts',(1.01778810567665,0.587620236790415,
-1.97083333333333));
#368973=CARTESIAN_POINT('Ctrl Pts',(0.678525403784436,1.17524047358083,
-1.92916666666667));
#368974=CARTESIAN_POINT('Ctrl Pts',(0.,1.17524047358083,-1.8875));
#368975=CARTESIAN_POINT('Ctrl Pts',(-0.678525403784435,1.17524047358083,
-1.84583333333334));
#368976=CARTESIAN_POINT('Ctrl Pts',(-1.01778810567665,0.587620236790416,
-1.80416666666667));
#368977=CARTESIAN_POINT('Ctrl Pts',(-1.35705080756887,1.5140037395914E-15,
-1.7625));
#368978=CARTESIAN_POINT('Ctrl Pts',(-1.01778810567665,-0.587620236790413,
-1.72083333333333));
#368979=CARTESIAN_POINT('Ctrl Pts',(-0.678525403784435,-1.17524047358083,
-1.67916666666667));
#368980=CARTESIAN_POINT('Ctrl Pts',(-1.43925448419918E-16,-1.17524047358083,
-1.6375));
#368981=CARTESIAN_POINT('Ctrl Pts',(0.678525403784435,-1.17524047358083,
-1.59583333333333));
#368982=CARTESIAN_POINT('Ctrl Pts',(1.01778810567665,-0.587620236790414,
-1.55416666666667));
#368983=CARTESIAN_POINT('Ctrl Pts',(1.35705080756887,1.07234823429092E-15,
-1.5125));
#368984=CARTESIAN_POINT('Ctrl Pts',(1.01778810567665,0.587620236790415,
-1.47083333333333));
#368985=CARTESIAN_POINT('Ctrl Pts',(0.678525403784436,1.17524047358083,
-1.42916666666667));
#368986=CARTESIAN_POINT('Ctrl Pts',(0.,1.17524047358083,-1.3875));
#368987=CARTESIAN_POINT('',(0.,0.,0.));
#368988=CARTESIAN_POINT('Origin',(1.38777878078145E-16,1.38777878078145E-16,
-4.19687500000002));
#368989=CARTESIAN_POINT('',(2.14917752421619E-17,-0.957716426222737,2.29999999999999));
#368990=CARTESIAN_POINT('',(2.14917781231183E-17,-0.957716426222737,2.35624999999998));
#368991=CARTESIAN_POINT('',(1.60269320569837E-16,-0.957716426222737,-4.19687500000002));
#368992=CARTESIAN_POINT('',(0.333926106471282,0.897615791123229,2.5));
#368993=CARTESIAN_POINT('Ctrl Pts',(-1.17286435586452E-16,-0.957716426222737,
2.29999999999999));
#368994=CARTESIAN_POINT('Ctrl Pts',(0.552937836487023,-0.957716426222737,
2.33749999999999));
#368995=CARTESIAN_POINT('Ctrl Pts',(0.829406754730535,-0.478858213111369,
2.37499999999999));
#368996=CARTESIAN_POINT('Ctrl Pts',(1.10587567297405,-3.31349931757196E-16,
2.41249999999999));
#368997=CARTESIAN_POINT('Ctrl Pts',(0.829406754730536,0.478858213111368,
2.44999999999999));
#368998=CARTESIAN_POINT('Ctrl Pts',(0.657035190041872,0.777414520932278,
2.47338032686238));
#368999=CARTESIAN_POINT('Ctrl Pts',(0.333926106471282,0.897615791123229,
2.5));
#369000=CARTESIAN_POINT('',(0.870621065093338,0.399048510926419,2.5));
#369001=CARTESIAN_POINT('Origin',(1.38778564065884E-16,1.38777878078145E-16,
2.5));
#369002=CARTESIAN_POINT('Ctrl Pts',(-1.17286435586452E-16,-0.957716426222737,
2.35624999999998));
#369003=CARTESIAN_POINT('Ctrl Pts',(0.552937836487023,-0.957716426222737,
2.39374999999998));
#369004=CARTESIAN_POINT('Ctrl Pts',(0.829406754730535,-0.478858213111369,
2.43124999999998));
#369005=CARTESIAN_POINT('Ctrl Pts',(1.07669261690991,-0.050546535823224,
2.46479163603864));
#369006=CARTESIAN_POINT('Ctrl Pts',(0.870621065093338,0.399048510926419,
2.5));
#369007=CARTESIAN_POINT('Origin',(1.38777878078145E-16,1.38777878078145E-16,
-4.19687500000002));
#369008=CARTESIAN_POINT('',(2.14917521945104E-17,-0.957716426222737,1.84999999999999));
#369009=CARTESIAN_POINT('',(2.14917550754668E-17,-0.957716426222737,1.90624999999998));
#369010=CARTESIAN_POINT('',(1.60269320569837E-16,-0.957716426222737,-4.19687500000002));
#369011=CARTESIAN_POINT('Ctrl Pts',(-1.17286435586452E-16,-0.957716426222737,
1.84999999999999));
#369012=CARTESIAN_POINT('Ctrl Pts',(0.552937836487023,-0.957716426222737,
1.88749999999999));
#369013=CARTESIAN_POINT('Ctrl Pts',(0.829406754730535,-0.478858213111369,
1.92499999999999));
#369014=CARTESIAN_POINT('Ctrl Pts',(1.10587567297405,-3.31752530400862E-16,
1.96249999999999));
#369015=CARTESIAN_POINT('Ctrl Pts',(0.829406754730536,0.478858213111368,
1.99999999999999));
#369016=CARTESIAN_POINT('Ctrl Pts',(0.552937836487024,0.957716426222737,
2.03749999999999));
#369017=CARTESIAN_POINT('Ctrl Pts',(0.,0.957716426222737,2.07499999999999));
#369018=CARTESIAN_POINT('Ctrl Pts',(-0.552937836487023,0.957716426222737,
2.11249999999999));
#369019=CARTESIAN_POINT('Ctrl Pts',(-0.829406754730535,0.478858213111368,
2.14999999999999));
#369020=CARTESIAN_POINT('Ctrl Pts',(-1.10587567297405,-6.06898104465106E-17,
2.18749999999999));
#369021=CARTESIAN_POINT('Ctrl Pts',(-0.829406754730535,-0.478858213111368,
2.22499999999999));
#369022=CARTESIAN_POINT('Ctrl Pts',(-0.552937836487024,-0.957716426222737,
2.26249999999999));
#369023=CARTESIAN_POINT('Ctrl Pts',(-1.17286435586452E-16,-0.957716426222737,
2.29999999999999));
#369024=CARTESIAN_POINT('Ctrl Pts',(-1.17286435586452E-16,-0.957716426222737,
1.90624999999998));
#369025=CARTESIAN_POINT('Ctrl Pts',(0.552937836487023,-0.957716426222737,
1.94374999999998));
#369026=CARTESIAN_POINT('Ctrl Pts',(0.829406754730535,-0.478858213111369,
1.98124999999998));
#369027=CARTESIAN_POINT('Ctrl Pts',(1.10587567297405,-3.31702205570404E-16,
2.01874999999998));
#369028=CARTESIAN_POINT('Ctrl Pts',(0.829406754730536,0.478858213111368,
2.05624999999998));
#369029=CARTESIAN_POINT('Ctrl Pts',(0.552937836487024,0.957716426222737,
2.09374999999998));
#369030=CARTESIAN_POINT('Ctrl Pts',(0.,0.957716426222737,2.13124999999998));
#369031=CARTESIAN_POINT('Ctrl Pts',(-0.552937836487023,0.957716426222737,
2.16874999999998));
#369032=CARTESIAN_POINT('Ctrl Pts',(-0.829406754730535,0.478858213111368,
2.20624999999998));
#369033=CARTESIAN_POINT('Ctrl Pts',(-1.10587567297405,-6.06394856160523E-17,
2.24374999999998));
#369034=CARTESIAN_POINT('Ctrl Pts',(-0.829406754730535,-0.478858213111368,
2.28124999999998));
#369035=CARTESIAN_POINT('Ctrl Pts',(-0.552937836487024,-0.957716426222737,
2.31874999999998));
#369036=CARTESIAN_POINT('Ctrl Pts',(-1.17286435586452E-16,-0.957716426222737,
2.35624999999998));
#369037=CARTESIAN_POINT('Origin',(1.38777878078145E-16,1.38777878078145E-16,
-4.19687500000002));
#369038=CARTESIAN_POINT('',(2.14917291468588E-17,-0.957716426222737,1.39999999999999));
#369039=CARTESIAN_POINT('',(2.14917320278152E-17,-0.957716426222737,1.45624999999998));
#369040=CARTESIAN_POINT('',(1.60269320569837E-16,-0.957716426222737,-4.19687500000002));
#369041=CARTESIAN_POINT('Ctrl Pts',(-1.17286435586452E-16,-0.957716426222737,
1.39999999999999));
#369042=CARTESIAN_POINT('Ctrl Pts',(0.552937836487023,-0.957716426222737,
1.43749999999999));
#369043=CARTESIAN_POINT('Ctrl Pts',(0.829406754730535,-0.478858213111369,
1.47499999999999));
#369044=CARTESIAN_POINT('Ctrl Pts',(1.10587567297405,-3.32155129044528E-16,
1.51249999999999));
#369045=CARTESIAN_POINT('Ctrl Pts',(0.829406754730536,0.478858213111368,
1.54999999999999));
#369046=CARTESIAN_POINT('Ctrl Pts',(0.552937836487024,0.957716426222737,
1.58749999999999));
#369047=CARTESIAN_POINT('Ctrl Pts',(0.,0.957716426222737,1.62499999999999));
#369048=CARTESIAN_POINT('Ctrl Pts',(-0.552937836487023,0.957716426222737,
1.66249999999999));
#369049=CARTESIAN_POINT('Ctrl Pts',(-0.829406754730535,0.478858213111368,
1.69999999999999));
#369050=CARTESIAN_POINT('Ctrl Pts',(-1.10587567297405,-6.10924090901767E-17,
1.73749999999999));
#369051=CARTESIAN_POINT('Ctrl Pts',(-0.829406754730535,-0.478858213111368,
1.77499999999999));
#369052=CARTESIAN_POINT('Ctrl Pts',(-0.552937836487024,-0.957716426222737,
1.81249999999999));
#369053=CARTESIAN_POINT('Ctrl Pts',(-1.17286435586452E-16,-0.957716426222737,
1.84999999999999));
#369054=CARTESIAN_POINT('Ctrl Pts',(-1.17286435586452E-16,-0.957716426222737,
1.45624999999998));
#369055=CARTESIAN_POINT('Ctrl Pts',(0.552937836487023,-0.957716426222737,
1.49374999999998));
#369056=CARTESIAN_POINT('Ctrl Pts',(0.829406754730535,-0.478858213111369,
1.53124999999998));
#369057=CARTESIAN_POINT('Ctrl Pts',(1.10587567297405,-3.3210480421407E-16,
1.56874999999998));
#369058=CARTESIAN_POINT('Ctrl Pts',(0.829406754730536,0.478858213111368,
1.60624999999998));
#369059=CARTESIAN_POINT('Ctrl Pts',(0.552937836487024,0.957716426222737,
1.64374999999998));
#369060=CARTESIAN_POINT('Ctrl Pts',(0.,0.957716426222737,1.68124999999998));
#369061=CARTESIAN_POINT('Ctrl Pts',(-0.552937836487023,0.957716426222737,
1.71874999999998));
#369062=CARTESIAN_POINT('Ctrl Pts',(-0.829406754730535,0.478858213111368,
1.75624999999998));
#369063=CARTESIAN_POINT('Ctrl Pts',(-1.10587567297405,-6.10420842597184E-17,
1.79374999999998));
#369064=CARTESIAN_POINT('Ctrl Pts',(-0.829406754730535,-0.478858213111368,
1.83124999999998));
#369065=CARTESIAN_POINT('Ctrl Pts',(-0.552937836487024,-0.957716426222737,
1.86874999999998));
#369066=CARTESIAN_POINT('Ctrl Pts',(-1.17286435586452E-16,-0.957716426222737,
1.90624999999998));
#369067=CARTESIAN_POINT('Origin',(1.38777878078145E-16,1.38777878078145E-16,
-4.19687500000002));
#369068=CARTESIAN_POINT('',(2.14917060992073E-17,-0.957716426222737,0.949999999999986));
#369069=CARTESIAN_POINT('',(2.14917089801637E-17,-0.957716426222737,1.00624999999998));
#369070=CARTESIAN_POINT('',(1.60269320569837E-16,-0.957716426222737,-4.19687500000002));
#369071=CARTESIAN_POINT('Ctrl Pts',(-1.17286435586452E-16,-0.957716426222737,
0.949999999999986));
#369072=CARTESIAN_POINT('Ctrl Pts',(0.552937836487023,-0.957716426222737,
0.987499999999986));
#369073=CARTESIAN_POINT('Ctrl Pts',(0.829406754730535,-0.478858213111369,
1.02499999999999));
#369074=CARTESIAN_POINT('Ctrl Pts',(1.10587567297405,-3.32557727688194E-16,
1.06249999999999));
#369075=CARTESIAN_POINT('Ctrl Pts',(0.829406754730536,0.478858213111368,
1.09999999999999));
#369076=CARTESIAN_POINT('Ctrl Pts',(0.552937836487024,0.957716426222737,
1.13749999999999));
#369077=CARTESIAN_POINT('Ctrl Pts',(0.,0.957716426222737,1.17499999999999));
#369078=CARTESIAN_POINT('Ctrl Pts',(-0.552937836487023,0.957716426222737,
1.21249999999999));
#369079=CARTESIAN_POINT('Ctrl Pts',(-0.829406754730535,0.478858213111368,
1.24999999999999));
#369080=CARTESIAN_POINT('Ctrl Pts',(-1.10587567297405,-6.14950077338427E-17,
1.28749999999999));
#369081=CARTESIAN_POINT('Ctrl Pts',(-0.829406754730535,-0.478858213111368,
1.32499999999999));
#369082=CARTESIAN_POINT('Ctrl Pts',(-0.552937836487024,-0.957716426222737,
1.36249999999999));
#369083=CARTESIAN_POINT('Ctrl Pts',(-1.17286435586452E-16,-0.957716426222737,
1.39999999999999));
#369084=CARTESIAN_POINT('Ctrl Pts',(-1.17286435586452E-16,-0.957716426222737,
1.00624999999998));
#369085=CARTESIAN_POINT('Ctrl Pts',(0.552937836487023,-0.957716426222737,
1.04374999999998));
#369086=CARTESIAN_POINT('Ctrl Pts',(0.829406754730535,-0.478858213111369,
1.08124999999998));
#369087=CARTESIAN_POINT('Ctrl Pts',(1.10587567297405,-3.32507402857736E-16,
1.11874999999998));
#369088=CARTESIAN_POINT('Ctrl Pts',(0.829406754730536,0.478858213111368,
1.15624999999998));
#369089=CARTESIAN_POINT('Ctrl Pts',(0.552937836487024,0.957716426222737,
1.19374999999998));
#369090=CARTESIAN_POINT('Ctrl Pts',(0.,0.957716426222737,1.23124999999998));
#369091=CARTESIAN_POINT('Ctrl Pts',(-0.552937836487023,0.957716426222737,
1.26874999999998));
#369092=CARTESIAN_POINT('Ctrl Pts',(-0.829406754730535,0.478858213111368,
1.30624999999998));
#369093=CARTESIAN_POINT('Ctrl Pts',(-1.10587567297405,-6.14446829033844E-17,
1.34374999999998));
#369094=CARTESIAN_POINT('Ctrl Pts',(-0.829406754730535,-0.478858213111368,
1.38124999999998));
#369095=CARTESIAN_POINT('Ctrl Pts',(-0.552937836487024,-0.957716426222737,
1.41874999999998));
#369096=CARTESIAN_POINT('Ctrl Pts',(-1.17286435586452E-16,-0.957716426222737,
1.45624999999998));
#369097=CARTESIAN_POINT('Origin',(1.38777878078145E-16,1.38777878078145E-16,
-4.19687500000002));
#369098=CARTESIAN_POINT('',(2.14916830515557E-17,-0.957716426222737,0.499999999999986));
#369099=CARTESIAN_POINT('',(2.14916859325122E-17,-0.957716426222737,0.556249999999979));
#369100=CARTESIAN_POINT('',(1.60269320569837E-16,-0.957716426222737,-4.19687500000002));
#369101=CARTESIAN_POINT('Ctrl Pts',(-1.17286435586452E-16,-0.957716426222737,
0.499999999999986));
#369102=CARTESIAN_POINT('Ctrl Pts',(0.552937836487023,-0.957716426222737,
0.537499999999986));
#369103=CARTESIAN_POINT('Ctrl Pts',(0.829406754730535,-0.478858213111369,
0.574999999999986));
#369104=CARTESIAN_POINT('Ctrl Pts',(1.10587567297405,-3.3296032633186E-16,
0.612499999999986));
#369105=CARTESIAN_POINT('Ctrl Pts',(0.829406754730536,0.478858213111368,
0.649999999999987));
#369106=CARTESIAN_POINT('Ctrl Pts',(0.552937836487024,0.957716426222737,
0.687499999999986));
#369107=CARTESIAN_POINT('Ctrl Pts',(0.,0.957716426222737,0.724999999999986));
#369108=CARTESIAN_POINT('Ctrl Pts',(-0.552937836487023,0.957716426222737,
0.762499999999986));
#369109=CARTESIAN_POINT('Ctrl Pts',(-0.829406754730535,0.478858213111368,
0.799999999999986));
#369110=CARTESIAN_POINT('Ctrl Pts',(-1.10587567297405,-6.18976063775088E-17,
0.837499999999986));
#369111=CARTESIAN_POINT('Ctrl Pts',(-0.829406754730535,-0.478858213111368,
0.874999999999986));
#369112=CARTESIAN_POINT('Ctrl Pts',(-0.552937836487024,-0.957716426222737,
0.912499999999986));
#369113=CARTESIAN_POINT('Ctrl Pts',(-1.17286435586452E-16,-0.957716426222737,
0.949999999999986));
#369114=CARTESIAN_POINT('Ctrl Pts',(-1.17286435586452E-16,-0.957716426222737,
0.556249999999979));
#369115=CARTESIAN_POINT('Ctrl Pts',(0.552937836487023,-0.957716426222737,
0.59374999999998));
#369116=CARTESIAN_POINT('Ctrl Pts',(0.829406754730535,-0.478858213111369,
0.63124999999998));
#369117=CARTESIAN_POINT('Ctrl Pts',(1.10587567297405,-3.32910001501402E-16,
0.66874999999998));
#369118=CARTESIAN_POINT('Ctrl Pts',(0.829406754730536,0.478858213111368,
0.70624999999998));
#369119=CARTESIAN_POINT('Ctrl Pts',(0.552937836487024,0.957716426222737,
0.74374999999998));
#369120=CARTESIAN_POINT('Ctrl Pts',(0.,0.957716426222737,0.78124999999998));
#369121=CARTESIAN_POINT('Ctrl Pts',(-0.552937836487023,0.957716426222737,
0.81874999999998));
#369122=CARTESIAN_POINT('Ctrl Pts',(-0.829406754730535,0.478858213111368,
0.85624999999998));
#369123=CARTESIAN_POINT('Ctrl Pts',(-1.10587567297405,-6.18472815470505E-17,
0.89374999999998));
#369124=CARTESIAN_POINT('Ctrl Pts',(-0.829406754730535,-0.478858213111368,
0.93124999999998));
#369125=CARTESIAN_POINT('Ctrl Pts',(-0.552937836487024,-0.957716426222737,
0.96874999999998));
#369126=CARTESIAN_POINT('Ctrl Pts',(-1.17286435586452E-16,-0.957716426222737,
1.00624999999998));
#369127=CARTESIAN_POINT('Origin',(1.38777878078145E-16,1.38777878078145E-16,
-4.19687500000002));
#369128=CARTESIAN_POINT('',(2.14916600039042E-17,-0.957716426222737,0.0499999999999858));
#369129=CARTESIAN_POINT('',(2.14916628848607E-17,-0.957716426222737,0.10624999999998));
#369130=CARTESIAN_POINT('',(1.60269320569837E-16,-0.957716426222737,-4.19687500000002));
#369131=CARTESIAN_POINT('Ctrl Pts',(-1.17286435586452E-16,-0.957716426222737,
0.0499999999999858));
#369132=CARTESIAN_POINT('Ctrl Pts',(0.552937836487023,-0.957716426222737,
0.087499999999986));
#369133=CARTESIAN_POINT('Ctrl Pts',(0.829406754730535,-0.478858213111369,
0.124999999999986));
#369134=CARTESIAN_POINT('Ctrl Pts',(1.10587567297405,-3.33362924975526E-16,
0.162499999999987));
#369135=CARTESIAN_POINT('Ctrl Pts',(0.829406754730536,0.478858213111368,
0.199999999999986));
#369136=CARTESIAN_POINT('Ctrl Pts',(0.552937836487024,0.957716426222737,
0.237499999999986));
#369137=CARTESIAN_POINT('Ctrl Pts',(0.,0.957716426222737,0.274999999999986));
#369138=CARTESIAN_POINT('Ctrl Pts',(-0.552937836487023,0.957716426222737,
0.312499999999986));
#369139=CARTESIAN_POINT('Ctrl Pts',(-0.829406754730535,0.478858213111368,
0.349999999999986));
#369140=CARTESIAN_POINT('Ctrl Pts',(-1.10587567297405,-6.23002050211748E-17,
0.387499999999986));
#369141=CARTESIAN_POINT('Ctrl Pts',(-0.829406754730535,-0.478858213111368,
0.424999999999986));
#369142=CARTESIAN_POINT('Ctrl Pts',(-0.552937836487024,-0.957716426222737,
0.462499999999986));
#369143=CARTESIAN_POINT('Ctrl Pts',(-1.17286435586452E-16,-0.957716426222737,
0.499999999999986));
#369144=CARTESIAN_POINT('Ctrl Pts',(-1.17286435586452E-16,-0.957716426222737,
0.10624999999998));
#369145=CARTESIAN_POINT('Ctrl Pts',(0.552937836487023,-0.957716426222737,
0.14374999999998));
#369146=CARTESIAN_POINT('Ctrl Pts',(0.829406754730535,-0.478858213111369,
0.18124999999998));
#369147=CARTESIAN_POINT('Ctrl Pts',(1.10587567297405,-3.33312600145068E-16,
0.21874999999998));
#369148=CARTESIAN_POINT('Ctrl Pts',(0.829406754730536,0.478858213111368,
0.25624999999998));
#369149=CARTESIAN_POINT('Ctrl Pts',(0.552937836487024,0.957716426222737,
0.29374999999998));
#369150=CARTESIAN_POINT('Ctrl Pts',(0.,0.957716426222737,0.33124999999998));
#369151=CARTESIAN_POINT('Ctrl Pts',(-0.552937836487023,0.957716426222737,
0.36874999999998));
#369152=CARTESIAN_POINT('Ctrl Pts',(-0.829406754730535,0.478858213111368,
0.40624999999998));
#369153=CARTESIAN_POINT('Ctrl Pts',(-1.10587567297405,-6.22498801907165E-17,
0.44374999999998));
#369154=CARTESIAN_POINT('Ctrl Pts',(-0.829406754730535,-0.478858213111368,
0.48124999999998));
#369155=CARTESIAN_POINT('Ctrl Pts',(-0.552937836487024,-0.957716426222737,
0.51874999999998));
#369156=CARTESIAN_POINT('Ctrl Pts',(-1.17286435586452E-16,-0.957716426222737,
0.556249999999979));
#369157=CARTESIAN_POINT('Origin',(1.38777878078145E-16,1.38777878078145E-16,
-4.19687500000002));
#369158=CARTESIAN_POINT('',(2.14916369562527E-17,-0.957716426222737,-0.400000000000014));
#369159=CARTESIAN_POINT('',(2.14916398372091E-17,-0.957716426222737,-0.34375000000002));
#369160=CARTESIAN_POINT('',(1.60269320569837E-16,-0.957716426222737,-4.19687500000002));
#369161=CARTESIAN_POINT('Ctrl Pts',(-1.17286435586452E-16,-0.957716426222737,
-0.400000000000014));
#369162=CARTESIAN_POINT('Ctrl Pts',(0.552937836487023,-0.957716426222737,
-0.362500000000014));
#369163=CARTESIAN_POINT('Ctrl Pts',(0.829406754730535,-0.478858213111369,
-0.325000000000014));
#369164=CARTESIAN_POINT('Ctrl Pts',(1.10587567297405,-3.33765523619192E-16,
-0.287500000000013));
#369165=CARTESIAN_POINT('Ctrl Pts',(0.829406754730536,0.478858213111368,
-0.250000000000014));
#369166=CARTESIAN_POINT('Ctrl Pts',(0.552937836487024,0.957716426222737,
-0.212500000000014));
#369167=CARTESIAN_POINT('Ctrl Pts',(0.,0.957716426222737,-0.175000000000014));
#369168=CARTESIAN_POINT('Ctrl Pts',(-0.552937836487023,0.957716426222737,
-0.137500000000013));
#369169=CARTESIAN_POINT('Ctrl Pts',(-0.829406754730535,0.478858213111368,
-0.100000000000014));
#369170=CARTESIAN_POINT('Ctrl Pts',(-1.10587567297405,-6.27028036648408E-17,
-0.0625000000000139));
#369171=CARTESIAN_POINT('Ctrl Pts',(-0.829406754730535,-0.478858213111368,
-0.0250000000000137));
#369172=CARTESIAN_POINT('Ctrl Pts',(-0.552937836487024,-0.957716426222737,
0.0124999999999865));
#369173=CARTESIAN_POINT('Ctrl Pts',(-1.17286435586452E-16,-0.957716426222737,
0.0499999999999858));
#369174=CARTESIAN_POINT('Ctrl Pts',(-1.17286435586452E-16,-0.957716426222737,
-0.34375000000002));
#369175=CARTESIAN_POINT('Ctrl Pts',(0.552937836487023,-0.957716426222737,
-0.30625000000002));
#369176=CARTESIAN_POINT('Ctrl Pts',(0.829406754730535,-0.478858213111369,
-0.26875000000002));
#369177=CARTESIAN_POINT('Ctrl Pts',(1.10587567297405,-3.33715198788734E-16,
-0.23125000000002));
#369178=CARTESIAN_POINT('Ctrl Pts',(0.829406754730536,0.478858213111368,
-0.19375000000002));
#369179=CARTESIAN_POINT('Ctrl Pts',(0.552937836487024,0.957716426222737,
-0.15625000000002));
#369180=CARTESIAN_POINT('Ctrl Pts',(0.,0.957716426222737,-0.11875000000002));
#369181=CARTESIAN_POINT('Ctrl Pts',(-0.552937836487023,0.957716426222737,
-0.0812500000000197));
#369182=CARTESIAN_POINT('Ctrl Pts',(-0.829406754730535,0.478858213111368,
-0.0437500000000203));
#369183=CARTESIAN_POINT('Ctrl Pts',(-1.10587567297405,-6.26524788343826E-17,
-0.00625000000002013));
#369184=CARTESIAN_POINT('Ctrl Pts',(-0.829406754730535,-0.478858213111368,
0.0312499999999801));
#369185=CARTESIAN_POINT('Ctrl Pts',(-0.552937836487024,-0.957716426222737,
0.0687499999999803));
#369186=CARTESIAN_POINT('Ctrl Pts',(-1.17286435586452E-16,-0.957716426222737,
0.10624999999998));
#369187=CARTESIAN_POINT('Origin',(1.38777878078145E-16,1.38777878078145E-16,
-4.19687500000002));
#369188=CARTESIAN_POINT('',(2.14916139086011E-17,-0.957716426222737,-0.850000000000014));
#369189=CARTESIAN_POINT('',(2.14916167895576E-17,-0.957716426222737,-0.79375000000002));
#369190=CARTESIAN_POINT('',(1.60269320569837E-16,-0.957716426222737,-4.19687500000002));
#369191=CARTESIAN_POINT('Ctrl Pts',(-1.17286435586452E-16,-0.957716426222737,
-0.850000000000014));
#369192=CARTESIAN_POINT('Ctrl Pts',(0.552937836487023,-0.957716426222737,
-0.812500000000014));
#369193=CARTESIAN_POINT('Ctrl Pts',(0.829406754730535,-0.478858213111369,
-0.775000000000014));
#369194=CARTESIAN_POINT('Ctrl Pts',(1.10587567297405,-3.34168122262858E-16,
-0.737500000000014));
#369195=CARTESIAN_POINT('Ctrl Pts',(0.829406754730536,0.478858213111368,
-0.700000000000014));
#369196=CARTESIAN_POINT('Ctrl Pts',(0.552937836487024,0.957716426222737,
-0.662500000000014));
#369197=CARTESIAN_POINT('Ctrl Pts',(0.,0.957716426222737,-0.625000000000014));
#369198=CARTESIAN_POINT('Ctrl Pts',(-0.552937836487023,0.957716426222737,
-0.587500000000014));
#369199=CARTESIAN_POINT('Ctrl Pts',(-0.829406754730535,0.478858213111368,
-0.550000000000014));
#369200=CARTESIAN_POINT('Ctrl Pts',(-1.10587567297405,-6.31054023085069E-17,
-0.512500000000014));
#369201=CARTESIAN_POINT('Ctrl Pts',(-0.829406754730535,-0.478858213111368,
-0.475000000000014));
#369202=CARTESIAN_POINT('Ctrl Pts',(-0.552937836487024,-0.957716426222737,
-0.437500000000014));
#369203=CARTESIAN_POINT('Ctrl Pts',(-1.17286435586452E-16,-0.957716426222737,
-0.400000000000014));
#369204=CARTESIAN_POINT('Ctrl Pts',(-1.17286435586452E-16,-0.957716426222737,
-0.79375000000002));
#369205=CARTESIAN_POINT('Ctrl Pts',(0.552937836487023,-0.957716426222737,
-0.75625000000002));
#369206=CARTESIAN_POINT('Ctrl Pts',(0.829406754730535,-0.478858213111369,
-0.71875000000002));
#369207=CARTESIAN_POINT('Ctrl Pts',(1.10587567297405,-3.341177974324E-16,
-0.68125000000002));
#369208=CARTESIAN_POINT('Ctrl Pts',(0.829406754730536,0.478858213111368,
-0.64375000000002));
#369209=CARTESIAN_POINT('Ctrl Pts',(0.552937836487024,0.957716426222737,
-0.60625000000002));
#369210=CARTESIAN_POINT('Ctrl Pts',(0.,0.957716426222737,-0.56875000000002));
#369211=CARTESIAN_POINT('Ctrl Pts',(-0.552937836487023,0.957716426222737,
-0.53125000000002));
#369212=CARTESIAN_POINT('Ctrl Pts',(-0.829406754730535,0.478858213111368,
-0.49375000000002));
#369213=CARTESIAN_POINT('Ctrl Pts',(-1.10587567297405,-6.30550774780486E-17,
-0.45625000000002));
#369214=CARTESIAN_POINT('Ctrl Pts',(-0.829406754730535,-0.478858213111368,
-0.41875000000002));
#369215=CARTESIAN_POINT('Ctrl Pts',(-0.552937836487024,-0.957716426222737,
-0.38125000000002));
#369216=CARTESIAN_POINT('Ctrl Pts',(-1.17286435586452E-16,-0.957716426222737,
-0.34375000000002));
#369217=CARTESIAN_POINT('Origin',(1.38777878078145E-16,1.38777878078145E-16,
-4.19687500000002));
#369218=CARTESIAN_POINT('',(2.14915908609496E-17,-0.957716426222737,-1.30000000000001));
#369219=CARTESIAN_POINT('',(2.14915937419061E-17,-0.957716426222737,-1.24375000000002));
#369220=CARTESIAN_POINT('',(1.60269320569837E-16,-0.957716426222737,-4.19687500000002));
#369221=CARTESIAN_POINT('Ctrl Pts',(-1.17286435586452E-16,-0.957716426222737,
-1.30000000000001));
#369222=CARTESIAN_POINT('Ctrl Pts',(0.552937836487023,-0.957716426222737,
-1.26250000000001));
#369223=CARTESIAN_POINT('Ctrl Pts',(0.829406754730535,-0.478858213111369,
-1.22500000000001));
#369224=CARTESIAN_POINT('Ctrl Pts',(1.10587567297405,-3.34570720906524E-16,
-1.18750000000001));
#369225=CARTESIAN_POINT('Ctrl Pts',(0.829406754730536,0.478858213111368,
-1.15000000000001));
#369226=CARTESIAN_POINT('Ctrl Pts',(0.552937836487024,0.957716426222737,
-1.11250000000001));
#369227=CARTESIAN_POINT('Ctrl Pts',(0.,0.957716426222737,-1.07500000000001));
#369228=CARTESIAN_POINT('Ctrl Pts',(-0.552937836487023,0.957716426222737,
-1.03750000000001));
#369229=CARTESIAN_POINT('Ctrl Pts',(-0.829406754730535,0.478858213111368,
-1.00000000000001));
#369230=CARTESIAN_POINT('Ctrl Pts',(-1.10587567297405,-6.35080009521729E-17,
-0.962500000000014));
#369231=CARTESIAN_POINT('Ctrl Pts',(-0.829406754730535,-0.478858213111368,
-0.925000000000014));
#369232=CARTESIAN_POINT('Ctrl Pts',(-0.552937836487024,-0.957716426222737,
-0.887500000000014));
#369233=CARTESIAN_POINT('Ctrl Pts',(-1.17286435586452E-16,-0.957716426222737,
-0.850000000000014));
#369234=CARTESIAN_POINT('Ctrl Pts',(-1.17286435586452E-16,-0.957716426222737,
-1.24375000000002));
#369235=CARTESIAN_POINT('Ctrl Pts',(0.552937836487023,-0.957716426222737,
-1.20625000000002));
#369236=CARTESIAN_POINT('Ctrl Pts',(0.829406754730535,-0.478858213111369,
-1.16875000000002));
#369237=CARTESIAN_POINT('Ctrl Pts',(1.10587567297405,-3.34520396076066E-16,
-1.13125000000002));
#369238=CARTESIAN_POINT('Ctrl Pts',(0.829406754730536,0.478858213111368,
-1.09375000000002));
#369239=CARTESIAN_POINT('Ctrl Pts',(0.552937836487024,0.957716426222737,
-1.05625000000002));
#369240=CARTESIAN_POINT('Ctrl Pts',(0.,0.957716426222737,-1.01875000000002));
#369241=CARTESIAN_POINT('Ctrl Pts',(-0.552937836487023,0.957716426222737,
-0.98125000000002));
#369242=CARTESIAN_POINT('Ctrl Pts',(-0.829406754730535,0.478858213111368,
-0.94375000000002));
#369243=CARTESIAN_POINT('Ctrl Pts',(-1.10587567297405,-6.34576761217147E-17,
-0.90625000000002));
#369244=CARTESIAN_POINT('Ctrl Pts',(-0.829406754730535,-0.478858213111368,
-0.86875000000002));
#369245=CARTESIAN_POINT('Ctrl Pts',(-0.552937836487024,-0.957716426222737,
-0.83125000000002));
#369246=CARTESIAN_POINT('Ctrl Pts',(-1.17286435586452E-16,-0.957716426222737,
-0.79375000000002));
#369247=CARTESIAN_POINT('Origin',(1.38777878078145E-16,1.38777878078145E-16,
-4.19687500000002));
#369248=CARTESIAN_POINT('',(2.14915678132981E-17,-0.957716426222737,-1.75000000000001));
#369249=CARTESIAN_POINT('',(2.14915706942545E-17,-0.957716426222737,-1.69375000000002));
#369250=CARTESIAN_POINT('',(1.60269320569837E-16,-0.957716426222737,-4.19687500000002));
#369251=CARTESIAN_POINT('Ctrl Pts',(-1.17286435586452E-16,-0.957716426222737,
-1.75000000000001));
#369252=CARTESIAN_POINT('Ctrl Pts',(0.552937836487023,-0.957716426222737,
-1.71250000000001));
#369253=CARTESIAN_POINT('Ctrl Pts',(0.829406754730535,-0.478858213111369,
-1.67500000000001));
#369254=CARTESIAN_POINT('Ctrl Pts',(1.10587567297405,-3.3497331955019E-16,
-1.63750000000001));
#369255=CARTESIAN_POINT('Ctrl Pts',(0.829406754730536,0.478858213111368,
-1.60000000000001));
#369256=CARTESIAN_POINT('Ctrl Pts',(0.552937836487024,0.957716426222737,
-1.56250000000001));
#369257=CARTESIAN_POINT('Ctrl Pts',(0.,0.957716426222737,-1.52500000000001));
#369258=CARTESIAN_POINT('Ctrl Pts',(-0.552937836487023,0.957716426222737,
-1.48750000000001));
#369259=CARTESIAN_POINT('Ctrl Pts',(-0.829406754730535,0.478858213111368,
-1.45000000000001));
#369260=CARTESIAN_POINT('Ctrl Pts',(-1.10587567297405,-6.3910599595839E-17,
-1.41250000000001));
#369261=CARTESIAN_POINT('Ctrl Pts',(-0.829406754730535,-0.478858213111368,
-1.37500000000001));
#369262=CARTESIAN_POINT('Ctrl Pts',(-0.552937836487024,-0.957716426222737,
-1.33750000000001));
#369263=CARTESIAN_POINT('Ctrl Pts',(-1.17286435586452E-16,-0.957716426222737,
-1.30000000000001));
#369264=CARTESIAN_POINT('Ctrl Pts',(-1.17286435586452E-16,-0.957716426222737,
-1.69375000000002));
#369265=CARTESIAN_POINT('Ctrl Pts',(0.552937836487023,-0.957716426222737,
-1.65625000000002));
#369266=CARTESIAN_POINT('Ctrl Pts',(0.829406754730535,-0.478858213111369,
-1.61875000000002));
#369267=CARTESIAN_POINT('Ctrl Pts',(1.10587567297405,-3.34922994719732E-16,
-1.58125000000002));
#369268=CARTESIAN_POINT('Ctrl Pts',(0.829406754730536,0.478858213111368,
-1.54375000000002));
#369269=CARTESIAN_POINT('Ctrl Pts',(0.552937836487024,0.957716426222737,
-1.50625000000002));
#369270=CARTESIAN_POINT('Ctrl Pts',(0.,0.957716426222737,-1.46875000000002));
#369271=CARTESIAN_POINT('Ctrl Pts',(-0.552937836487023,0.957716426222737,
-1.43125000000002));
#369272=CARTESIAN_POINT('Ctrl Pts',(-0.829406754730535,0.478858213111368,
-1.39375000000002));
#369273=CARTESIAN_POINT('Ctrl Pts',(-1.10587567297405,-6.38602747653807E-17,
-1.35625000000002));
#369274=CARTESIAN_POINT('Ctrl Pts',(-0.829406754730535,-0.478858213111368,
-1.31875000000002));
#369275=CARTESIAN_POINT('Ctrl Pts',(-0.552937836487024,-0.957716426222737,
-1.28125000000002));
#369276=CARTESIAN_POINT('Ctrl Pts',(-1.17286435586452E-16,-0.957716426222737,
-1.24375000000002));
#369277=CARTESIAN_POINT('Origin',(1.38777878078145E-16,1.38777878078145E-16,
-4.19687500000002));
#369278=CARTESIAN_POINT('',(2.14915447656466E-17,-0.957716426222737,-2.20000000000001));
#369279=CARTESIAN_POINT('',(2.1491547646603E-17,-0.957716426222737,-2.14375000000002));
#369280=CARTESIAN_POINT('',(1.60269320569837E-16,-0.957716426222737,-4.19687500000002));
#369281=CARTESIAN_POINT('Ctrl Pts',(-1.17286435586452E-16,-0.957716426222737,
-2.20000000000001));
#369282=CARTESIAN_POINT('Ctrl Pts',(0.552937836487023,-0.957716426222737,
-2.16250000000001));
#369283=CARTESIAN_POINT('Ctrl Pts',(0.829406754730535,-0.478858213111369,
-2.12500000000001));
#369284=CARTESIAN_POINT('Ctrl Pts',(1.10587567297405,-3.35375918193856E-16,
-2.08750000000001));
#369285=CARTESIAN_POINT('Ctrl Pts',(0.829406754730536,0.478858213111368,
-2.05000000000001));
#369286=CARTESIAN_POINT('Ctrl Pts',(0.552937836487024,0.957716426222737,
-2.01250000000001));
#369287=CARTESIAN_POINT('Ctrl Pts',(0.,0.957716426222737,-1.97500000000001));
#369288=CARTESIAN_POINT('Ctrl Pts',(-0.552937836487023,0.957716426222737,
-1.93750000000001));
#369289=CARTESIAN_POINT('Ctrl Pts',(-0.829406754730535,0.478858213111368,
-1.90000000000001));
#369290=CARTESIAN_POINT('Ctrl Pts',(-1.10587567297405,-6.4313198239505E-17,
-1.86250000000001));
#369291=CARTESIAN_POINT('Ctrl Pts',(-0.829406754730535,-0.478858213111368,
-1.82500000000001));
#369292=CARTESIAN_POINT('Ctrl Pts',(-0.552937836487024,-0.957716426222737,
-1.78750000000001));
#369293=CARTESIAN_POINT('Ctrl Pts',(-1.17286435586452E-16,-0.957716426222737,
-1.75000000000001));
#369294=CARTESIAN_POINT('Ctrl Pts',(-1.17286435586452E-16,-0.957716426222737,
-2.14375000000002));
#369295=CARTESIAN_POINT('Ctrl Pts',(0.552937836487023,-0.957716426222737,
-2.10625000000002));
#369296=CARTESIAN_POINT('Ctrl Pts',(0.829406754730535,-0.478858213111369,
-2.06875000000002));
#369297=CARTESIAN_POINT('Ctrl Pts',(1.10587567297405,-3.35325593363398E-16,
-2.03125000000002));
#369298=CARTESIAN_POINT('Ctrl Pts',(0.829406754730536,0.478858213111368,
-1.99375000000002));
#369299=CARTESIAN_POINT('Ctrl Pts',(0.552937836487024,0.957716426222737,
-1.95625000000002));
#369300=CARTESIAN_POINT('Ctrl Pts',(0.,0.957716426222737,-1.91875000000002));
#369301=CARTESIAN_POINT('Ctrl Pts',(-0.552937836487023,0.957716426222737,
-1.88125000000002));
#369302=CARTESIAN_POINT('Ctrl Pts',(-0.829406754730535,0.478858213111368,
-1.84375000000002));
#369303=CARTESIAN_POINT('Ctrl Pts',(-1.10587567297405,-6.42628734090468E-17,
-1.80625000000002));
#369304=CARTESIAN_POINT('Ctrl Pts',(-0.829406754730535,-0.478858213111368,
-1.76875000000002));
#369305=CARTESIAN_POINT('Ctrl Pts',(-0.552937836487024,-0.957716426222737,
-1.73125000000002));
#369306=CARTESIAN_POINT('Ctrl Pts',(-1.17286435586452E-16,-0.957716426222737,
-1.69375000000002));
#369307=CARTESIAN_POINT('Origin',(1.38777878078145E-16,1.38777878078145E-16,
-4.19687500000002));
#369308=CARTESIAN_POINT('',(2.1491521717995E-17,-0.957716426222737,-2.65000000000001));
#369309=CARTESIAN_POINT('',(2.14915245989515E-17,-0.957716426222737,-2.59375000000002));
#369310=CARTESIAN_POINT('',(1.60269320569837E-16,-0.957716426222737,-4.19687500000002));
#369311=CARTESIAN_POINT('Ctrl Pts',(-1.17286435586452E-16,-0.957716426222737,
-2.65000000000001));
#369312=CARTESIAN_POINT('Ctrl Pts',(0.552937836487023,-0.957716426222737,
-2.61250000000001));
#369313=CARTESIAN_POINT('Ctrl Pts',(0.829406754730535,-0.478858213111369,
-2.57500000000001));
#369314=CARTESIAN_POINT('Ctrl Pts',(1.10587567297405,-3.35778516837522E-16,
-2.53750000000001));
#369315=CARTESIAN_POINT('Ctrl Pts',(0.829406754730536,0.478858213111368,
-2.50000000000001));
#369316=CARTESIAN_POINT('Ctrl Pts',(0.552937836487024,0.957716426222737,
-2.46250000000001));
#369317=CARTESIAN_POINT('Ctrl Pts',(0.,0.957716426222737,-2.42500000000001));
#369318=CARTESIAN_POINT('Ctrl Pts',(-0.552937836487023,0.957716426222737,
-2.38750000000001));
#369319=CARTESIAN_POINT('Ctrl Pts',(-0.829406754730535,0.478858213111368,
-2.35000000000001));
#369320=CARTESIAN_POINT('Ctrl Pts',(-1.10587567297405,-6.47157968831711E-17,
-2.31250000000001));
#369321=CARTESIAN_POINT('Ctrl Pts',(-0.829406754730535,-0.478858213111368,
-2.27500000000001));
#369322=CARTESIAN_POINT('Ctrl Pts',(-0.552937836487024,-0.957716426222737,
-2.23750000000001));
#369323=CARTESIAN_POINT('Ctrl Pts',(-1.17286435586452E-16,-0.957716426222737,
-2.20000000000001));
#369324=CARTESIAN_POINT('Ctrl Pts',(-1.17286435586452E-16,-0.957716426222737,
-2.59375000000002));
#369325=CARTESIAN_POINT('Ctrl Pts',(0.552937836487023,-0.957716426222737,
-2.55625000000002));
#369326=CARTESIAN_POINT('Ctrl Pts',(0.829406754730535,-0.478858213111369,
-2.51875000000002));
#369327=CARTESIAN_POINT('Ctrl Pts',(1.10587567297405,-3.35728192007064E-16,
-2.48125000000002));
#369328=CARTESIAN_POINT('Ctrl Pts',(0.829406754730536,0.478858213111368,
-2.44375000000002));
#369329=CARTESIAN_POINT('Ctrl Pts',(0.552937836487024,0.957716426222737,
-2.40625000000002));
#369330=CARTESIAN_POINT('Ctrl Pts',(0.,0.957716426222737,-2.36875000000002));
#369331=CARTESIAN_POINT('Ctrl Pts',(-0.552937836487023,0.957716426222737,
-2.33125000000002));
#369332=CARTESIAN_POINT('Ctrl Pts',(-0.829406754730535,0.478858213111368,
-2.29375000000002));
#369333=CARTESIAN_POINT('Ctrl Pts',(-1.10587567297405,-6.46654720527128E-17,
-2.25625000000002));
#369334=CARTESIAN_POINT('Ctrl Pts',(-0.829406754730535,-0.478858213111368,
-2.21875000000002));
#369335=CARTESIAN_POINT('Ctrl Pts',(-0.552937836487024,-0.957716426222737,
-2.18125000000002));
#369336=CARTESIAN_POINT('Ctrl Pts',(-1.17286435586452E-16,-0.957716426222737,
-2.14375000000002));
#369337=CARTESIAN_POINT('Origin',(1.38777878078145E-16,1.38777878078145E-16,
-4.19687500000002));
#369338=CARTESIAN_POINT('',(2.14914986703435E-17,-0.957716426222737,-3.10000000000001));
#369339=CARTESIAN_POINT('',(2.14915015512999E-17,-0.957716426222737,-3.04375000000002));
#369340=CARTESIAN_POINT('',(1.60269320569837E-16,-0.957716426222737,-4.19687500000002));
#369341=CARTESIAN_POINT('Ctrl Pts',(-1.17286435586452E-16,-0.957716426222737,
-3.10000000000001));
#369342=CARTESIAN_POINT('Ctrl Pts',(0.552937836487023,-0.957716426222737,
-3.06250000000001));
#369343=CARTESIAN_POINT('Ctrl Pts',(0.829406754730535,-0.478858213111369,
-3.02500000000001));
#369344=CARTESIAN_POINT('Ctrl Pts',(1.10587567297405,-3.36181115481189E-16,
-2.98750000000001));
#369345=CARTESIAN_POINT('Ctrl Pts',(0.829406754730536,0.478858213111368,
-2.95000000000001));
#369346=CARTESIAN_POINT('Ctrl Pts',(0.552937836487024,0.957716426222737,
-2.91250000000001));
#369347=CARTESIAN_POINT('Ctrl Pts',(0.,0.957716426222737,-2.87500000000001));
#369348=CARTESIAN_POINT('Ctrl Pts',(-0.552937836487023,0.957716426222737,
-2.83750000000001));
#369349=CARTESIAN_POINT('Ctrl Pts',(-0.829406754730535,0.478858213111368,
-2.80000000000001));
#369350=CARTESIAN_POINT('Ctrl Pts',(-1.10587567297405,-6.51183955268371E-17,
-2.76250000000001));
#369351=CARTESIAN_POINT('Ctrl Pts',(-0.829406754730535,-0.478858213111368,
-2.72500000000001));
#369352=CARTESIAN_POINT('Ctrl Pts',(-0.552937836487024,-0.957716426222737,
-2.68750000000001));
#369353=CARTESIAN_POINT('Ctrl Pts',(-1.17286435586452E-16,-0.957716426222737,
-2.65000000000001));
#369354=CARTESIAN_POINT('Ctrl Pts',(-1.17286435586452E-16,-0.957716426222737,
-3.04375000000002));
#369355=CARTESIAN_POINT('Ctrl Pts',(0.552937836487023,-0.957716426222737,
-3.00625000000002));
#369356=CARTESIAN_POINT('Ctrl Pts',(0.829406754730535,-0.478858213111369,
-2.96875000000002));
#369357=CARTESIAN_POINT('Ctrl Pts',(1.10587567297405,-3.3613079065073E-16,
-2.93125000000002));
#369358=CARTESIAN_POINT('Ctrl Pts',(0.829406754730536,0.478858213111368,
-2.89375000000002));
#369359=CARTESIAN_POINT('Ctrl Pts',(0.552937836487024,0.957716426222737,
-2.85625000000002));
#369360=CARTESIAN_POINT('Ctrl Pts',(0.,0.957716426222737,-2.81875000000002));
#369361=CARTESIAN_POINT('Ctrl Pts',(-0.552937836487023,0.957716426222737,
-2.78125000000002));
#369362=CARTESIAN_POINT('Ctrl Pts',(-0.829406754730535,0.478858213111368,
-2.74375000000002));
#369363=CARTESIAN_POINT('Ctrl Pts',(-1.10587567297405,-6.50680706963789E-17,
-2.70625000000002));
#369364=CARTESIAN_POINT('Ctrl Pts',(-0.829406754730535,-0.478858213111368,
-2.66875000000002));
#369365=CARTESIAN_POINT('Ctrl Pts',(-0.552937836487024,-0.957716426222737,
-2.63125000000002));
#369366=CARTESIAN_POINT('Ctrl Pts',(-1.17286435586452E-16,-0.957716426222737,
-2.59375000000002));
#369367=CARTESIAN_POINT('Origin',(1.38777878078145E-16,1.38777878078145E-16,
-4.19687500000002));
#369368=CARTESIAN_POINT('',(2.1491475622692E-17,-0.957716426222737,-3.55000000000001));
#369369=CARTESIAN_POINT('',(2.14914785036484E-17,-0.957716426222737,-3.49375000000002));
#369370=CARTESIAN_POINT('',(1.60269320569837E-16,-0.957716426222737,-4.19687500000002));
#369371=CARTESIAN_POINT('Ctrl Pts',(-1.17286435586452E-16,-0.957716426222737,
-3.55000000000001));
#369372=CARTESIAN_POINT('Ctrl Pts',(0.552937836487023,-0.957716426222737,
-3.51250000000001));
#369373=CARTESIAN_POINT('Ctrl Pts',(0.829406754730535,-0.478858213111369,
-3.47500000000001));
#369374=CARTESIAN_POINT('Ctrl Pts',(1.10587567297405,-3.36583714124855E-16,
-3.43750000000001));
#369375=CARTESIAN_POINT('Ctrl Pts',(0.829406754730536,0.478858213111368,
-3.40000000000001));
#369376=CARTESIAN_POINT('Ctrl Pts',(0.552937836487024,0.957716426222737,
-3.36250000000001));
#369377=CARTESIAN_POINT('Ctrl Pts',(0.,0.957716426222737,-3.32500000000001));
#369378=CARTESIAN_POINT('Ctrl Pts',(-0.552937836487023,0.957716426222737,
-3.28750000000001));
#369379=CARTESIAN_POINT('Ctrl Pts',(-0.829406754730535,0.478858213111368,
-3.25000000000001));
#369380=CARTESIAN_POINT('Ctrl Pts',(-1.10587567297405,-6.55209941705032E-17,
-3.21250000000001));
#369381=CARTESIAN_POINT('Ctrl Pts',(-0.829406754730535,-0.478858213111368,
-3.17500000000001));
#369382=CARTESIAN_POINT('Ctrl Pts',(-0.552937836487024,-0.957716426222737,
-3.13750000000001));
#369383=CARTESIAN_POINT('Ctrl Pts',(-1.17286435586452E-16,-0.957716426222737,
-3.10000000000001));
#369384=CARTESIAN_POINT('Ctrl Pts',(-1.17286435586452E-16,-0.957716426222737,
-3.49375000000002));
#369385=CARTESIAN_POINT('Ctrl Pts',(0.552937836487023,-0.957716426222737,
-3.45625000000002));
#369386=CARTESIAN_POINT('Ctrl Pts',(0.829406754730535,-0.478858213111369,
-3.41875000000002));
#369387=CARTESIAN_POINT('Ctrl Pts',(1.10587567297405,-3.36533389294396E-16,
-3.38125000000002));
#369388=CARTESIAN_POINT('Ctrl Pts',(0.829406754730536,0.478858213111368,
-3.34375000000002));
#369389=CARTESIAN_POINT('Ctrl Pts',(0.552937836487024,0.957716426222737,
-3.30625000000002));
#369390=CARTESIAN_POINT('Ctrl Pts',(0.,0.957716426222737,-3.26875000000002));
#369391=CARTESIAN_POINT('Ctrl Pts',(-0.552937836487023,0.957716426222737,
-3.23125000000002));
#369392=CARTESIAN_POINT('Ctrl Pts',(-0.829406754730535,0.478858213111368,
-3.19375000000002));
#369393=CARTESIAN_POINT('Ctrl Pts',(-1.10587567297405,-6.54706693400449E-17,
-3.15625000000002));
#369394=CARTESIAN_POINT('Ctrl Pts',(-0.829406754730535,-0.478858213111368,
-3.11875000000002));
#369395=CARTESIAN_POINT('Ctrl Pts',(-0.552937836487024,-0.957716426222737,
-3.08125000000002));
#369396=CARTESIAN_POINT('Ctrl Pts',(-1.17286435586452E-16,-0.957716426222737,
-3.04375000000002));
#369397=CARTESIAN_POINT('Origin',(1.38777878078145E-16,1.38777878078145E-16,
-4.19687500000002));
#369398=CARTESIAN_POINT('',(1.60269345368232E-16,-0.957716426222737,-3.95478357377733));
#369399=CARTESIAN_POINT('',(2.14914554559969E-17,-0.957716426222737,-3.94375000000002));
#369400=CARTESIAN_POINT('',(1.60269320569837E-16,-0.957716426222737,-4.19687500000002));
#369401=CARTESIAN_POINT('',(0.561651082536657,-0.775737593869378,-3.95478357377714));
#369402=CARTESIAN_POINT('Origin',(-4.58730275987307E-13,1.7608137170555E-12,
-3.95478357377551));
#369403=CARTESIAN_POINT('Ctrl Pts',(0.561651082536657,-0.775737593869378,
-3.95478357377714));
#369404=CARTESIAN_POINT('Ctrl Pts',(0.727208897839709,-0.655870093670933,
-3.93886202708702));
#369405=CARTESIAN_POINT('Ctrl Pts',(0.829406754730535,-0.478858213111369,
-3.92500000000001));
#369406=CARTESIAN_POINT('Ctrl Pts',(1.10587567297405,-3.36986312768521E-16,
-3.88750000000001));
#369407=CARTESIAN_POINT('Ctrl Pts',(0.829406754730536,0.478858213111368,
-3.85000000000001));
#369408=CARTESIAN_POINT('Ctrl Pts',(0.552937836487024,0.957716426222737,
-3.81250000000001));
#369409=CARTESIAN_POINT('Ctrl Pts',(0.,0.957716426222737,-3.77500000000001));
#369410=CARTESIAN_POINT('Ctrl Pts',(-0.552937836487023,0.957716426222737,
-3.73750000000001));
#369411=CARTESIAN_POINT('Ctrl Pts',(-0.829406754730535,0.478858213111368,
-3.70000000000001));
#369412=CARTESIAN_POINT('Ctrl Pts',(-1.10587567297405,-6.59235928141692E-17,
-3.66250000000001));
#369413=CARTESIAN_POINT('Ctrl Pts',(-0.829406754730535,-0.478858213111368,
-3.62500000000001));
#369414=CARTESIAN_POINT('Ctrl Pts',(-0.552937836487024,-0.957716426222737,
-3.58750000000001));
#369415=CARTESIAN_POINT('Ctrl Pts',(-1.17286435586452E-16,-0.957716426222737,
-3.55000000000001));
#369416=CARTESIAN_POINT('Ctrl Pts',(-1.17286435586452E-16,-0.957716426222737,
-3.94375000000002));
#369417=CARTESIAN_POINT('Ctrl Pts',(0.552937836487023,-0.957716426222737,
-3.90625000000002));
#369418=CARTESIAN_POINT('Ctrl Pts',(0.829406754730535,-0.478858213111369,
-3.86875000000002));
#369419=CARTESIAN_POINT('Ctrl Pts',(1.10587567297405,-3.36935987938062E-16,
-3.83125000000002));
#369420=CARTESIAN_POINT('Ctrl Pts',(0.829406754730536,0.478858213111368,
-3.79375000000002));
#369421=CARTESIAN_POINT('Ctrl Pts',(0.552937836487024,0.957716426222737,
-3.75625000000002));
#369422=CARTESIAN_POINT('Ctrl Pts',(0.,0.957716426222737,-3.71875000000002));
#369423=CARTESIAN_POINT('Ctrl Pts',(-0.552937836487023,0.957716426222737,
-3.68125000000002));
#369424=CARTESIAN_POINT('Ctrl Pts',(-0.829406754730535,0.478858213111368,
-3.64375000000002));
#369425=CARTESIAN_POINT('Ctrl Pts',(-1.10587567297405,-6.58732679837109E-17,
-3.60625000000002));
#369426=CARTESIAN_POINT('Ctrl Pts',(-0.829406754730535,-0.478858213111368,
-3.56875000000002));
#369427=CARTESIAN_POINT('Ctrl Pts',(-0.552937836487024,-0.957716426222737,
-3.53125000000002));
#369428=CARTESIAN_POINT('Ctrl Pts',(-1.17286435586452E-16,-0.957716426222737,
-3.49375000000002));
#369429=CARTESIAN_POINT('Origin',(0.,0.,2.95));
#369430=CARTESIAN_POINT('',(5.80020015507564E-14,1.25000000000001,-3.49375000000003));
#369431=CARTESIAN_POINT('',(7.48635137372505E-14,1.25000000000001,-3.55000000000002));
#369432=CARTESIAN_POINT('',(-1.5308084989342E-16,1.25000000000001,2.95));
#369433=CARTESIAN_POINT('',(0.875786586618201,-0.891906864366224,-3.66249999999728));
#369434=CARTESIAN_POINT('Ctrl Pts',(1.16157083951406E-13,1.25000000000001,
-3.49375000000003));
#369435=CARTESIAN_POINT('Ctrl Pts',(0.0558262619039152,1.25000000000001,
-3.49665081766045));
#369436=CARTESIAN_POINT('Ctrl Pts',(0.111699054709194,1.24626059886401,
-3.49966623517157));
#369437=CARTESIAN_POINT('Ctrl Pts',(0.333022130666348,1.2163788867422,-3.51206297090858));
#369438=CARTESIAN_POINT('Ctrl Pts',(0.492605203231851,1.16095117575365,
-3.52201798192958));
#369439=CARTESIAN_POINT('Ctrl Pts',(0.774960304797056,0.993884904164799,
-3.54170157152786));
#369440=CARTESIAN_POINT('Ctrl Pts',(0.896304252028742,0.886014998629642,
-3.5512428851478));
#369441=CARTESIAN_POINT('Ctrl Pts',(1.09217035418525,0.62923090622271,-3.56912390913247));
#369442=CARTESIAN_POINT('Ctrl Pts',(1.16446017056606,0.482499223607466,
-3.57730004658363));
#369443=CARTESIAN_POINT('Ctrl Pts',(1.2498202949631,0.166545811296484,-3.59625725132228));
#369444=CARTESIAN_POINT('Ctrl Pts',(1.26086616979021,0.000109175634494391,
-3.606243449462));
#369445=CARTESIAN_POINT('Ctrl Pts',(1.22094386548057,-0.302209608995765,
-3.62438257653982));
#369446=CARTESIAN_POINT('Ctrl Pts',(1.17953231039141,-0.436750102582941,
-3.63245500615505));
#369447=CARTESIAN_POINT('Ctrl Pts',(1.05507856256371,-0.684196471505689,
-3.64730178829041));
#369448=CARTESIAN_POINT('Ctrl Pts',(0.973700164305609,-0.795762971529037,
-3.65452794446843));
#369449=CARTESIAN_POINT('Ctrl Pts',(0.875786586616994,-0.891906864365204,
-3.66249999999274));
#369450=CARTESIAN_POINT('',(1.25000000000001,1.00721982129472E-13,-3.6625));
#369451=CARTESIAN_POINT('Origin',(0.,-9.76875228502569E-17,-3.6625));
#369452=CARTESIAN_POINT('Ctrl Pts',(1.25000000000001,-1.72868663828041E-12,
-3.66250000000011));
#369453=CARTESIAN_POINT('Ctrl Pts',(1.25000000000022,0.154429265794931,
-3.65323424405232));
#369454=CARTESIAN_POINT('Ctrl Pts',(1.22138437816133,0.307537553418373,
-3.64404774679489));
#369455=CARTESIAN_POINT('Ctrl Pts',(1.11179970332925,0.590395200419514,
-3.62707628797482));
#369456=CARTESIAN_POINT('Ctrl Pts',(1.03366513337583,0.718472897613953,
-3.61965662894215));
#369457=CARTESIAN_POINT('Ctrl Pts',(0.827234960889385,0.951025440084063,
-3.6019536262592));
#369458=CARTESIAN_POINT('Ctrl Pts',(0.697099868255548,1.05014772137054,
-3.59221794005192));
#369459=CARTESIAN_POINT('Ctrl Pts',(0.402996178943989,1.19480263661878,
-3.57259621661704));
#369460=CARTESIAN_POINT('Ctrl Pts',(0.241205989437471,1.23765799933533,
-3.5629036908838));
#369461=CARTESIAN_POINT('Ctrl Pts',(0.0504979547264238,1.2492356898471,
-3.55264688000252));
#369462=CARTESIAN_POINT('Ctrl Pts',(0.0252376533412523,1.25000000000001,
-3.55131138693554));
#369463=CARTESIAN_POINT('Ctrl Pts',(1.49880108324394E-13,1.25000000000001,
-3.55000000000002));
#369464=CARTESIAN_POINT('Origin',(0.,0.,2.95));
#369465=CARTESIAN_POINT('',(-7.654042494671E-17,1.25000000000001,-3.04375000000002));
#369466=CARTESIAN_POINT('',(1.01092532694019E-13,1.25000000000001,-3.10000000000002));
#369467=CARTESIAN_POINT('',(-1.5308084989342E-16,1.25000000000001,2.95));
#369468=CARTESIAN_POINT('Ctrl Pts',(0.,1.25000000000001,-3.04375000000002));
#369469=CARTESIAN_POINT('Ctrl Pts',(0.0801005201788763,1.25000000000001,
-3.0479121451199));
#369470=CARTESIAN_POINT('Ctrl Pts',(0.160186539952716,1.24230243878038,
-3.05230446361325));
#369471=CARTESIAN_POINT('Ctrl Pts',(0.40239322377935,1.19508772134168,-3.06630633360603));
#369472=CARTESIAN_POINT('Ctrl Pts',(0.557624581099529,1.13101732560779,
-3.07629450341224));
#369473=CARTESIAN_POINT('Ctrl Pts',(0.828663890971705,0.949425856712451,
-3.09582586314551));
#369474=CARTESIAN_POINT('Ctrl Pts',(0.943270166994007,0.83567394848635,
-3.1051935371804));
#369475=CARTESIAN_POINT('Ctrl Pts',(1.12600178305657,0.567228567228114,
-3.12274191191323));
#369476=CARTESIAN_POINT('Ctrl Pts',(1.19087205499603,0.414087629904788,
-3.13140474220578));
#369477=CARTESIAN_POINT('Ctrl Pts',(1.25738607605826,0.0919088285462163,
-3.15073547028729));
#369478=CARTESIAN_POINT('Ctrl Pts',(1.25857313222639,-0.0738927601021803,
-3.16068356560619));
#369479=CARTESIAN_POINT('Ctrl Pts',(1.19787636075818,-0.390746558040131,
-3.17969479348247));
#369480=CARTESIAN_POINT('Ctrl Pts',(1.13878777518423,-0.539192113889463,
-3.18825261484703));
#369481=CARTESIAN_POINT('Ctrl Pts',(0.964401571050862,-0.812343959042414,
-3.20550854317256));
#369482=CARTESIAN_POINT('Ctrl Pts',(0.84832420071093,-0.932898580437442,
-3.21515673890554));
#369483=CARTESIAN_POINT('Ctrl Pts',(0.578771305933263,-1.11976065620169,
-3.23476898045094));
#369484=CARTESIAN_POINT('Ctrl Pts',(0.428640235704609,-1.1853755909506,
-3.24453846773632));
#369485=CARTESIAN_POINT('Ctrl Pts',(0.114671973971978,-1.25487465779539,
-3.26293770918022));
#369486=CARTESIAN_POINT('Ctrl Pts',(-0.0459245874231769,-1.2592653387857,
-3.27085835139851));
#369487=CARTESIAN_POINT('Ctrl Pts',(-0.367625069297885,-1.20630429357242,
-3.2891632301377));
#369488=CARTESIAN_POINT('Ctrl Pts',(-0.525104066239286,-1.1465479638438,
-3.29913876874438));
#369489=CARTESIAN_POINT('Ctrl Pts',(-0.801932878622589,-0.972181167374948,
-3.31875421967985));
#369490=CARTESIAN_POINT('Ctrl Pts',(-0.919967305363899,-0.861340512618317,
-3.32821268804729));
#369491=CARTESIAN_POINT('Ctrl Pts',(-1.10934819693316,-0.598757638681498,
-3.34593069405082));
#369492=CARTESIAN_POINT('Ctrl Pts',(-1.17799385288076,-0.44889238620976,
-3.35431645682749));
#369493=CARTESIAN_POINT('Ctrl Pts',(-1.25410425134268,-0.129813702317056,
-3.37346117786105));
#369494=CARTESIAN_POINT('Ctrl Pts',(-1.2602788701469,0.0363811147974186,
-3.38343286688791));
#369495=CARTESIAN_POINT('Ctrl Pts',(-1.20880266299188,0.355630032051346,
-3.40258780192315));
#369496=CARTESIAN_POINT('Ctrl Pts',(-1.15395901910286,0.505981224656806,
-3.41146796721162));
#369497=CARTESIAN_POINT('Ctrl Pts',(-0.987406810821905,0.784214035498693,
-3.42846925814254));
#369498=CARTESIAN_POINT('Ctrl Pts',(-0.874873756978497,0.908041106904038,
-3.43803145928833));
#369499=CARTESIAN_POINT('Ctrl Pts',(-0.610488461751786,1.10285608983475,
-3.45761377169945));
#369500=CARTESIAN_POINT('Ctrl Pts',(-0.461856329770814,1.17289478537514,
-3.46743808469252));
#369501=CARTESIAN_POINT('Ctrl Pts',(-0.204354382331899,1.23745189198145,
-3.48275499157107));
#369502=CARTESIAN_POINT('Ctrl Pts',(-0.102275013815502,1.25000000000001,
-3.48843563439182));
#369503=CARTESIAN_POINT('Ctrl Pts',(1.16209125655686E-13,1.25000000000001,
-3.49375000000003));
#369504=CARTESIAN_POINT('Ctrl Pts',(1.49984191732955E-13,1.25000000000001,
-3.55000000000002));
#369505=CARTESIAN_POINT('Ctrl Pts',(-0.132674294559962,1.25000000000001,
-3.54310604142893));
#369506=CARTESIAN_POINT('Ctrl Pts',(-0.26465747431644,1.228882811502,-3.53561447858149));
#369507=CARTESIAN_POINT('Ctrl Pts',(-0.546731051132629,1.13598604793516,
-3.51817060267893));
#369508=CARTESIAN_POINT('Ctrl Pts',(-0.690850975295588,1.05456313893759,
-3.50823922447801));
#369509=CARTESIAN_POINT('Ctrl Pts',(-0.940700856621858,0.839649471497178,
-3.48880923379313));
#369510=CARTESIAN_POINT('Ctrl Pts',(-1.04351636963,0.707800398739344,-3.47996802392435));
#369511=CARTESIAN_POINT('Ctrl Pts',(-1.18921447801218,0.416897828238739,
-3.46251386969432));
#369512=CARTESIAN_POINT('Ctrl Pts',(-1.23270515879014,0.261640644464715,
-3.45319843866788));
#369513=CARTESIAN_POINT('Ctrl Pts',(-1.25939974289888,-0.0630143527908859,
-3.43371913883254));
#369514=CARTESIAN_POINT('Ctrl Pts',(-1.23991046724957,-0.229540855795417,
-3.42372754865227));
#369515=CARTESIAN_POINT('Ctrl Pts',(-1.13875725577918,-0.539856394523013,
-3.40510861632861));
#369516=CARTESIAN_POINT('Ctrl Pts',(-1.06020700578772,-0.681302486930842,
-3.39715089740901));
#369517=CARTESIAN_POINT('Ctrl Pts',(-0.85308723432579,-0.927829827179376,
-3.37899281817883));
#369518=CARTESIAN_POINT('Ctrl Pts',(-0.726101406925719,-1.03023901135182,
-3.36932216550672));
#369519=CARTESIAN_POINT('Ctrl Pts',(-0.436568842699685,-1.18295211451495,
-3.34969621906127));
#369520=CARTESIAN_POINT('Ctrl Pts',(-0.276028747136534,-1.23036286746581,
-3.33993198840772));
#369521=CARTESIAN_POINT('Ctrl Pts',(0.0467989359121036,-1.25911687906126,
-3.32229474958596));
#369522=CARTESIAN_POINT('Ctrl Pts',(0.205727709267049,-1.2430821436253,
-3.3141025389595));
#369523=CARTESIAN_POINT('Ctrl Pts',(0.51413235956892,-1.15104145573479,
-3.29531614261438));
#369524=CARTESIAN_POINT('Ctrl Pts',(0.66010527760148,-1.07400506479895,
-3.28542007556946));
#369525=CARTESIAN_POINT('Ctrl Pts',(0.917020015673747,-0.865760355830752,
-3.26582305291378));
#369526=CARTESIAN_POINT('Ctrl Pts',(1.02444705071578,-0.73548782844564,
-3.25662926970673));
#369527=CARTESIAN_POINT('Ctrl Pts',(1.1780467288341,-0.44733973729301,-3.23934038423758));
#369528=CARTESIAN_POINT('Ctrl Pts',(1.22542020036252,-0.293656149941834,
-3.23011936899651));
#369529=CARTESIAN_POINT('Ctrl Pts',(1.26057525901858,0.0293356889581505,
-3.21073985866251));
#369530=CARTESIAN_POINT('Ctrl Pts',(1.24561377045063,0.195865703788074,
-3.20074805777271));
#369531=CARTESIAN_POINT('Ctrl Pts',(1.15289542449753,0.509239004921235,
-3.18194565970473));
#369532=CARTESIAN_POINT('Ctrl Pts',(1.07769691096265,0.653497200184776,
-3.17389385814288));
#369533=CARTESIAN_POINT('Ctrl Pts',(0.876616464365373,0.905559960847434,
-3.15588352882554));
#369534=CARTESIAN_POINT('Ctrl Pts',(0.752640825960971,1.01094764575026,
-3.14627993513994));
#369535=CARTESIAN_POINT('Ctrl Pts',(0.46757179903791,1.17104730599246,-3.12666432418383));
#369536=CARTESIAN_POINT('Ctrl Pts',(0.308316758016824,1.22267363848955,
-3.11684039953662));
#369537=CARTESIAN_POINT('Ctrl Pts',(0.0958504907300428,1.24724676713127,
-3.10506313458231));
#369538=CARTESIAN_POINT('Ctrl Pts',(0.0479017666976706,1.25000000000001,
-3.10248904881079));
#369539=CARTESIAN_POINT('Ctrl Pts',(2.02338146237931E-13,1.25000000000001,
-3.10000000000002));
#369540=CARTESIAN_POINT('Origin',(0.,0.,2.95));
#369541=CARTESIAN_POINT('',(-7.12695918790362E-14,1.25000000000001,-2.59375000000002));
#369542=CARTESIAN_POINT('',(1.79696092910825E-15,1.25000000000001,-2.65000000000001));
#369543=CARTESIAN_POINT('',(-1.5308084989342E-16,1.25000000000001,2.95));
#369544=CARTESIAN_POINT('Ctrl Pts',(-1.42386102908176E-13,1.25000000000001,
-2.59375000000002));
#369545=CARTESIAN_POINT('Ctrl Pts',(0.105342329382033,1.25000000000002,
-2.59922374800034));
#369546=CARTESIAN_POINT('Ctrl Pts',(0.210464993290618,1.23668796757782,
-2.60508544282054));
#369547=CARTESIAN_POINT('Ctrl Pts',(0.472931271974733,1.16882871805381,
-2.62075936820489));
#369548=CARTESIAN_POINT('Ctrl Pts',(0.623176125175293,1.09611624799401,
-2.63074769388626));
#369549=CARTESIAN_POINT('Ctrl Pts',(0.881712267495814,0.900217730807902,
-2.6500585814246));
#369550=CARTESIAN_POINT('Ctrl Pts',(0.989034488987936,0.78079342394926,
-2.65921793684252));
#369551=CARTESIAN_POINT('Ctrl Pts',(1.15647945686897,0.502488376758182,
-2.67626778401351));
#369552=CARTESIAN_POINT('Ctrl Pts',(1.21284945899906,0.344928507153231,
-2.68555428957086));
#369553=CARTESIAN_POINT('Ctrl Pts',(1.2604713269282,0.019338514041045,-2.70508968915759));
#369554=CARTESIAN_POINT('Ctrl Pts',(1.2522183870622,-0.145308449334908,
-2.71496850696015));
#369555=CARTESIAN_POINT('Ctrl Pts',(1.17405124976896,-0.457385009487385,
-2.73369310056929));
#369556=CARTESIAN_POINT('Ctrl Pts',(1.10671349811452,-0.602306727205998,
-2.74181268157154));
#369557=CARTESIAN_POINT('Ctrl Pts',(0.917179620939207,-0.86531427570947,
-2.75955137717734));
#369558=CARTESIAN_POINT('Ctrl Pts',(0.794466491816304,-0.979180490624983,
-2.7693437248567));
#369559=CARTESIAN_POINT('Ctrl Pts',(0.515519595225215,-1.15012812765669,
-2.78896665989293));
#369560=CARTESIAN_POINT('Ctrl Pts',(0.362833793640631,-1.20702852828054,
-2.79860745888981));
#369561=CARTESIAN_POINT('Ctrl Pts',(0.0449590270720812,-1.25948835649622,
-2.81669851112051));
#369562=CARTESIAN_POINT('Ctrl Pts',(-0.117152741739399,-1.25483438374123,
-2.82469240351598));
#369563=CARTESIAN_POINT('Ctrl Pts',(-0.435769191696286,-1.18325981368898,
-2.84339543700112));
#369564=CARTESIAN_POINT('Ctrl Pts',(-0.588713704895264,-1.1150817006434,
-2.85338801042048));
#369565=CARTESIAN_POINT('Ctrl Pts',(-0.853965955173471,-0.926661281286531,
-2.8728235342303));
#369566=CARTESIAN_POINT('Ctrl Pts',(-0.965181724295405,-0.810185693519208,
-2.88209674274498));
#369567=CARTESIAN_POINT('Ctrl Pts',(-1.1413894115652,-0.536069156456338,
-2.89947625886793));
#369568=CARTESIAN_POINT('Ctrl Pts',(-1.20250854929645,-0.379656750626062,
-2.9084705949625));
#369569=CARTESIAN_POINT('Ctrl Pts',(-1.25949740328438,-0.0545476131985929,
-2.92797714320814));
#369570=CARTESIAN_POINT('Ctrl Pts',(-1.25580678653293,0.110725047297354,
-2.9378935028379));
#369571=CARTESIAN_POINT('Ctrl Pts',(-1.18609130510389,0.425150928291168,
-2.95675905569753));
#369572=CARTESIAN_POINT('Ctrl Pts',(-1.12278089789272,0.571763500175269,
-2.96506149817778));
#369573=CARTESIAN_POINT('Ctrl Pts',(-0.94062407355898,0.839766230910028,
-2.98256672634057));
#369574=CARTESIAN_POINT('Ctrl Pts',(-0.821104779434934,0.956948443351132,
-2.99229259741103));
#369575=CARTESIAN_POINT('Ctrl Pts',(-0.546631107919309,1.13573250749033,
-3.01191818966735));
#369576=CARTESIAN_POINT('Ctrl Pts',(-0.39513175643769,1.19690191271148,
-3.02162540904638));
#369577=CARTESIAN_POINT('Ctrl Pts',(-0.158157705063089,1.242496613601,-3.03530678298476));
#369578=CARTESIAN_POINT('Ctrl Pts',(-0.0790836106868099,1.25000000000001,
-3.03964069504736));
#369579=CARTESIAN_POINT('Ctrl Pts',(0.,1.25000000000001,-3.04375000000002));
#369580=CARTESIAN_POINT('Ctrl Pts',(1.98504407356026E-13,1.25000000000001,
-3.10000000000002));
#369581=CARTESIAN_POINT('Ctrl Pts',(-0.110023330863273,1.25000000000001,
-3.09428302002783));
#369582=CARTESIAN_POINT('Ctrl Pts',(-0.219753373684046,1.23547878878256,
-3.08814564341281));
#369583=CARTESIAN_POINT('Ctrl Pts',(-0.483784337213042,1.16406351081363,
-3.07228373376564));
#369584=CARTESIAN_POINT('Ctrl Pts',(-0.631346657530357,1.09109489844724,
-3.06242711231248));
#369585=CARTESIAN_POINT('Ctrl Pts',(-0.892250491426103,0.890989610552251,
-3.04286699278972));
#369586=CARTESIAN_POINT('Ctrl Pts',(-1.00234506247223,0.76500253803068,
-3.03340015228184));
#369587=CARTESIAN_POINT('Ctrl Pts',(-1.1636454044465,0.483408458576927,
-3.01650450751462));
#369588=CARTESIAN_POINT('Ctrl Pts',(-1.21560102978879,0.331735897822884,
-3.00740415386937));
#369589=CARTESIAN_POINT('Ctrl Pts',(-1.26079895223703,0.0110195436563138,
-2.98816117261938));
#369590=CARTESIAN_POINT('Ctrl Pts',(-1.25124075256951,-0.155358063370983,
-2.97817851619774));
#369591=CARTESIAN_POINT('Ctrl Pts',(-1.16869360067347,-0.472275959171684,
-2.9591634424497));
#369592=CARTESIAN_POINT('Ctrl Pts',(-1.09751310445712,-0.619957886750929,
-2.95092971716425));
#369593=CARTESIAN_POINT('Ctrl Pts',(-0.903627337233052,-0.878521253299362,
-2.9330982161769));
#369594=CARTESIAN_POINT('Ctrl Pts',(-0.783289989381195,-0.987312035831273,
-2.92358158068511));
#369595=CARTESIAN_POINT('Ctrl Pts',(-0.502608934507082,-1.15663399822554,
-2.90391730638037));
#369596=CARTESIAN_POINT('Ctrl Pts',(-0.343658713220788,-1.2133959834479,
-2.89395515104943));
#369597=CARTESIAN_POINT('Ctrl Pts',(-0.0209816289176561,-1.25988228237505,
-2.87579376894808));
#369598=CARTESIAN_POINT('Ctrl Pts',(0.13913046002791,-1.25235370103634,
-2.86784118026163));
#369599=CARTESIAN_POINT('Ctrl Pts',(0.451659987362524,-1.17683970593185,
-2.84933624980222));
#369600=CARTESIAN_POINT('Ctrl Pts',(0.600767646557596,-1.10816080217134,
-2.8395280214437));
#369601=CARTESIAN_POINT('Ctrl Pts',(0.866770480060013,-0.915781193785182,
-2.81993472051462));
#369602=CARTESIAN_POINT('Ctrl Pts',(0.980405780280576,-0.792951045382059,
-2.81034515265706));
#369603=CARTESIAN_POINT('Ctrl Pts',(1.14937757073535,-0.516276107469031,
-2.79326487273626));
#369604=CARTESIAN_POINT('Ctrl Pts',(1.20553169019293,-0.366519856087064,
-2.78449119136523));
#369605=CARTESIAN_POINT('Ctrl Pts',(1.25986993086269,-0.0480047442141254,
-2.76538028465285));
#369606=CARTESIAN_POINT('Ctrl Pts',(1.25524295575607,0.118083896291753,
-2.7554149662225));
#369607=CARTESIAN_POINT('Ctrl Pts',(1.18209588403663,0.438135514494601,
-2.73621186913033));
#369608=CARTESIAN_POINT('Ctrl Pts',(1.11461619357743,0.589009815920291,
-2.72774686186885));
#369609=CARTESIAN_POINT('Ctrl Pts',(0.927297001734213,0.853419375895082,
-2.71008118434445));
#369610=CARTESIAN_POINT('Ctrl Pts',(0.810322094209521,0.965177306505159,
-2.70065025193484));
#369611=CARTESIAN_POINT('Ctrl Pts',(0.535275736301416,1.14181259951419,
-2.68105936515457));
#369612=CARTESIAN_POINT('Ctrl Pts',(0.378484215519997,1.20292015139326,
-2.67107901219251));
#369613=CARTESIAN_POINT('Ctrl Pts',(0.14337927547669,1.24383556877028,-2.65763513863324));
#369614=CARTESIAN_POINT('Ctrl Pts',(0.0716801446618524,1.25000000000001,
-2.65372460957346));
#369615=CARTESIAN_POINT('Ctrl Pts',(3.74700270810992E-15,1.25000000000001,
-2.65000000000001));
#369616=CARTESIAN_POINT('Origin',(0.,0.,2.95));
#369617=CARTESIAN_POINT('',(-1.34968637916908E-13,1.25000000000001,-2.14375000000001));
#369618=CARTESIAN_POINT('',(-2.06850553195514E-14,1.25000000000001,-2.20000000000001));
#369619=CARTESIAN_POINT('',(-1.5308084989342E-16,1.25000000000001,2.95));
#369620=CARTESIAN_POINT('Ctrl Pts',(-2.70200528618147E-13,1.25000000000001,
-2.14375000000001));
#369621=CARTESIAN_POINT('Ctrl Pts',(0.130400599680054,1.25000000000003,
-2.15052581391952));
#369622=CARTESIAN_POINT('Ctrl Pts',(0.260188488106204,1.22960103321381,
-2.15788175943196));
#369623=CARTESIAN_POINT('Ctrl Pts',(0.541027657753502,1.13876865933085,
-2.17519956196599));
#369624=CARTESIAN_POINT('Ctrl Pts',(0.6858869727539,1.0578577579882,-2.18515399981218));
#369625=CARTESIAN_POINT('Ctrl Pts',(0.931518979784196,0.848456115260838,
-2.20419946257825));
#369626=CARTESIAN_POINT('Ctrl Pts',(1.03141898990211,0.723707518137767,
-2.21282754891178));
#369627=CARTESIAN_POINT('Ctrl Pts',(1.18275495824577,0.437106100705102,
-2.23002363395774));
#369628=CARTESIAN_POINT('Ctrl Pts',(1.23021426454136,0.276629885961306,
-2.23965220684237));
#369629=CARTESIAN_POINT('Ctrl Pts',(1.25950792098496,-0.0501476581208609,
-2.2592588594873));
#369630=CARTESIAN_POINT('Ctrl Pts',(1.24234770403752,-0.21320020716703,
-2.26904201243007));
#369631=CARTESIAN_POINT('Ctrl Pts',(1.14757966301889,-0.520460564018815,
-2.28747763384117));
#369632=CARTESIAN_POINT('Ctrl Pts',(1.07210138549065,-0.662128816518621,
-2.29540584237956));
#369633=CARTESIAN_POINT('Ctrl Pts',(0.867140045341389,-0.91565552203857,
-2.31366174718694));
#369634=CARTESIAN_POINT('Ctrl Pts',(0.737281518839768,-1.02311320506751,
-2.32363312464871));
#369635=CARTESIAN_POINT('Ctrl Pts',(0.448686870271631,-1.1776864945793,
-2.34326614115744));
#369636=CARTESIAN_POINT('Ctrl Pts',(0.293886489933415,-1.22552458722037,
-2.35274494764997));
#369637=CARTESIAN_POINT('Ctrl Pts',(-0.0277882329935411,-1.26027459942359,
-2.37050215692467));
#369638=CARTESIAN_POINT('Ctrl Pts',(-0.191681604333076,-1.24592573976443,
-2.37883229613455));
#369639=CARTESIAN_POINT('Ctrl Pts',(-0.50653836891461,-1.15459340299165,
-2.39793270363859));
#369640=CARTESIAN_POINT('Ctrl Pts',(-0.654198020566734,-1.07781669916157,
-2.40790862532018));
#369641=CARTESIAN_POINT('Ctrl Pts',(-0.906488342174939,-0.875205244858828,
-2.42709635860776));
#369642=CARTESIAN_POINT('Ctrl Pts',(-1.01015543604116,-0.753159657325788,
-2.4360604205605));
#369643=CARTESIAN_POINT('Ctrl Pts',(-1.16974926270548,-0.470795286726956,
-2.45300228279643));
#369644=CARTESIAN_POINT('Ctrl Pts',(-1.22177589738895,-0.311775055933201,
-2.46254349664406));
#369645=CARTESIAN_POINT('Ctrl Pts',(-1.2604813845259,0.014442586313074,
-2.48211655517883));
#369646=CARTESIAN_POINT('Ctrl Pts',(-1.24788218824376,0.178373896895093,
-2.49195243381375));
#369647=CARTESIAN_POINT('Ctrl Pts',(-1.16163592241478,0.488139475969799,
-2.51053836855824));
#369648=CARTESIAN_POINT('Ctrl Pts',(-1.09037690212478,0.63146750447024,
-2.51853637931777));
#369649=CARTESIAN_POINT('Ctrl Pts',(-0.892749692734237,0.890795644436746,
-2.53658523454544));
#369650=CARTESIAN_POINT('Ctrl Pts',(-0.765588978650082,1.00218666747823,
-2.54653442976229));
#369651=CARTESIAN_POINT('Ctrl Pts',(-0.480574618493332,1.16509672348177,
-2.56623151202275));
#369652=CARTESIAN_POINT('Ctrl Pts',(-0.326711235242754,1.21724071537535,
-2.57579080769599));
#369653=CARTESIAN_POINT('Ctrl Pts',(-0.111645874219062,1.24626437544745,
-2.58783664146539));
#369654=CARTESIAN_POINT('Ctrl Pts',(-0.0557979962155551,1.25,-2.59085065106785));
#369655=CARTESIAN_POINT('Ctrl Pts',(-1.42386102908179E-13,1.25000000000001,
-2.59375000000002));
#369656=CARTESIAN_POINT('Ctrl Pts',(3.74700270810992E-15,1.25000000000001,
-2.65000000000001));
#369657=CARTESIAN_POINT('Ctrl Pts',(-0.0870368365289856,1.25000000000001,
-2.64547743331006));
#369658=CARTESIAN_POINT('Ctrl Pts',(-0.174017038472817,1.24091191735034,
-2.64068516695999));
#369659=CARTESIAN_POINT('Ctrl Pts',(-0.418189121696728,1.18908380191606,
-2.62644276987895));
#369660=CARTESIAN_POINT('Ctrl Pts',(-0.56876222727317,1.12485723352674,
-2.61669196475391));
#369661=CARTESIAN_POINT('Ctrl Pts',(-0.839880964929171,0.940508819212412,
-2.59707376946936));
#369662=CARTESIAN_POINT('Ctrl Pts',(-0.957046079674429,0.820998481605603,
-2.58740038139275));
#369663=CARTESIAN_POINT('Ctrl Pts',(-1.1338694789778,0.54944959773603,-2.57006590152985));
#369664=CARTESIAN_POINT('Ctrl Pts',(-1.19428053340036,0.401584919981543,
-2.5615950951989));
#369665=CARTESIAN_POINT('Ctrl Pts',(-1.25781923999118,0.0854872513799908,
-2.5426292350828));
#369666=CARTESIAN_POINT('Ctrl Pts',(-1.25816971613052,-0.0801631234019533,
-2.53269021259589));
#369667=CARTESIAN_POINT('Ctrl Pts',(-1.19464241373935,-0.403276661186595,
-2.51330340032881));
#369668=CARTESIAN_POINT('Ctrl Pts',(-1.130947533088,-0.557441487641628,
-2.50454251301085));
#369669=CARTESIAN_POINT('Ctrl Pts',(-0.950269536212173,-0.827680662772613,
-2.48704703364496));
#369670=CARTESIAN_POINT('Ctrl Pts',(-0.836727996672834,-0.942304107899593,
-2.4777085388336));
#369671=CARTESIAN_POINT('Ctrl Pts',(-0.567499653063559,-1.1260730553892,
-2.45820595530984));
#369672=CARTESIAN_POINT('Ctrl Pts',(-0.412979789708039,-1.19144996938435,
-2.44821556026668));
#369673=CARTESIAN_POINT('Ctrl Pts',(-0.0932791076376549,-1.25676118364574,
-2.42964408910203));
#369674=CARTESIAN_POINT('Ctrl Pts',(0.0683051291320635,-1.25836539260636,
-2.42170172315597));
#369675=CARTESIAN_POINT('Ctrl Pts',(0.384901361116856,-1.20021273172363,
-2.40350632055101));
#369676=CARTESIAN_POINT('Ctrl Pts',(0.536790394902123,-1.14039721052624,
-2.39381946920623));
#369677=CARTESIAN_POINT('Ctrl Pts',(0.812709266568332,-0.964090096418552,
-2.37419309064821));
#369678=CARTESIAN_POINT('Ctrl Pts',(0.933253212969323,-0.847951376294141,
-2.36444528185314));
#369679=CARTESIAN_POINT('Ctrl Pts',(1.11775814554646,-0.581527009011775,
-2.34686539331055));
#369680=CARTESIAN_POINT('Ctrl Pts',(1.1823479907869,-0.435457656484337,
-2.33862745938907));
#369681=CARTESIAN_POINT('Ctrl Pts',(1.25476494009658,-0.121775017149212,
-2.31980650102896));
#369682=CARTESIAN_POINT('Ctrl Pts',(1.25991513645705,0.0433113316044855,
-2.30990132010374));
#369683=CARTESIAN_POINT('Ctrl Pts',(1.20580612045286,0.369277092449537,
-2.29034337445304));
#369684=CARTESIAN_POINT('Ctrl Pts',(1.1458231285194,0.526681754001067,-2.28123826363247));
#369685=CARTESIAN_POINT('Ctrl Pts',(0.97157355437601,0.802484878243874,
-2.26390989643678));
#369686=CARTESIAN_POINT('Ctrl Pts',(0.861379553736349,0.919752348254905,
-2.25466602410253));
#369687=CARTESIAN_POINT('Ctrl Pts',(0.5978826770635,1.11017193361377,-2.23526173720077));
#369688=CARTESIAN_POINT('Ctrl Pts',(0.445639208929776,1.17955841433044,
-2.22526934012143));
#369689=CARTESIAN_POINT('Ctrl Pts',(0.190878358124393,1.23905928514506,
-2.21024655187576));
#369690=CARTESIAN_POINT('Ctrl Pts',(0.0954986701827122,1.25000000000001,
-2.20496225646436));
#369691=CARTESIAN_POINT('Ctrl Pts',(-4.12170297892093E-14,1.25000000000001,
-2.20000000000001));
#369692=CARTESIAN_POINT('Origin',(0.,0.,2.95));
#369693=CARTESIAN_POINT('',(-7.57054584116654E-15,1.25000000000001,-1.69375000000002));
#369694=CARTESIAN_POINT('',(-1.42462643333128E-13,1.25000000000001,-1.75));
#369695=CARTESIAN_POINT('',(-1.5308084989342E-16,1.25000000000001,2.95));
#369696=CARTESIAN_POINT('Ctrl Pts',(-1.45369827286856E-14,1.25000000000001,
-1.69375000000002));
#369697=CARTESIAN_POINT('Ctrl Pts',(0.155286777933764,1.25000000000001,
-1.70181893767377));
#369698=CARTESIAN_POINT('Ctrl Pts',(0.309345025886403,1.22106605206648,
-1.71069205749516));
#369699=CARTESIAN_POINT('Ctrl Pts',(0.606478691077016,1.10516013999761,
-1.72960875299971));
#369700=CARTESIAN_POINT('Ctrl Pts',(0.74559126023823,1.01650974762323,-1.7394967659037));
#369701=CARTESIAN_POINT('Ctrl Pts',(0.978202071192304,0.794170145224384,
-1.75825376626453));
#369702=CARTESIAN_POINT('Ctrl Pts',(1.07083083826407,0.664000290496938,
-1.76640998257022));
#369703=CARTESIAN_POINT('Ctrl Pts',(1.20567341556416,0.369239130681009,
-1.78409565215918));
#369704=CARTESIAN_POINT('Ctrl Pts',(1.24395338002485,0.206275750069565,
-1.79387345499587));
#369705=CARTESIAN_POINT('Ctrl Pts',(1.25458873064323,-0.120805419414252,
-1.81349832516489));
#369706=CARTESIAN_POINT('Ctrl Pts',(1.22850120747155,-0.281748656109735,
-1.82315491936662));
#369707=CARTESIAN_POINT('Ctrl Pts',(1.11686342852972,-0.583852736797541,
-1.84128116420789));
#369708=CARTESIAN_POINT('Ctrl Pts',(1.03275646151661,-0.722276572455576,
-1.84925469727795));
#369709=CARTESIAN_POINT('Ctrl Pts',(0.813102736283407,-0.963793726505868,
-1.86791375426473));
#369710=CARTESIAN_POINT('Ctrl Pts',(0.678131628412114,-1.0630916610204,
-1.87790599679178));
#369711=CARTESIAN_POINT('Ctrl Pts',(0.383002849197226,-1.20054098376891,
-1.89736481768551));
#369712=CARTESIAN_POINT('Ctrl Pts',(0.22666646407795,-1.23960859735568,
-1.90666032295606));
#369713=CARTESIAN_POINT('Ctrl Pts',(-0.0984540233871174,-1.25710918060458,
-1.92407909653966));
#369714=CARTESIAN_POINT('Ctrl Pts',(-0.26424740528379,-1.23296943282957,
-1.93299161496675));
#369715=CARTESIAN_POINT('Ctrl Pts',(-0.574822733720398,-1.12201798537666,
-1.95245812584322));
#369716=CARTESIAN_POINT('Ctrl Pts',(-0.716787539462754,-1.03709317355258,
-1.96238257789092));
#369717=CARTESIAN_POINT('Ctrl Pts',(-0.955764002205384,-0.821024658166677,
-1.98128221461099));
#369718=CARTESIAN_POINT('Ctrl Pts',(-1.05193413271564,-0.693529768620369,
-1.98963821388282));
#369719=CARTESIAN_POINT('Ctrl Pts',(-1.19489887339543,-0.402735570372728,
-2.00708586577768));
#369720=CARTESIAN_POINT('Ctrl Pts',(-1.23770575764424,-0.240926756812164,
-2.01679439459131));
#369721=CARTESIAN_POINT('Ctrl Pts',(-1.25750064517564,0.086139235517628,
-2.0364183541311));
#369722=CARTESIAN_POINT('Ctrl Pts',(-1.23577670752401,0.248178869789145,
-2.04614073218739));
#369723=CARTESIAN_POINT('Ctrl Pts',(-1.13242189057427,0.552845721494632,
-2.06442074328972));
#369724=CARTESIAN_POINT('Ctrl Pts',(-1.05259819111681,0.692859611668211,
-2.07234118194101));
#369725=CARTESIAN_POINT('Ctrl Pts',(-0.840186016140514,0.940361879897444,
-2.09080351036404));
#369726=CARTESIAN_POINT('Ctrl Pts',(-0.70768418083934,1.04372697881743,
-2.10078946065677));
#369727=CARTESIAN_POINT('Ctrl Pts',(-0.415666351516008,1.18968370559345,
-2.12034185397317));
#369728=CARTESIAN_POINT('Ctrl Pts',(-0.260028950008825,1.23309638342485,
-2.12973139091717));
#369729=CARTESIAN_POINT('Ctrl Pts',(-0.0669608855494323,1.24865638160365,
-2.14023030177141));
#369730=CARTESIAN_POINT('Ctrl Pts',(-0.0334623557046908,1.25,-2.14201124499338));
#369731=CARTESIAN_POINT('Ctrl Pts',(-2.69784194983923E-13,1.25000000000001,
-2.14375000000001));
#369732=CARTESIAN_POINT('Ctrl Pts',(-4.12170297892093E-14,1.25000000000001,
-2.20000000000001));
#369733=CARTESIAN_POINT('Ctrl Pts',(-0.0647810486097229,1.25,-2.19663387797322));
#369734=CARTESIAN_POINT('Ctrl Pts',(-0.129600986562227,1.24496494293533,
-2.19311468348496));
#369735=CARTESIAN_POINT('Ctrl Pts',(-0.353256875456652,1.20984938920675,
-2.18043971598379));
#369736=CARTESIAN_POINT('Ctrl Pts',(-0.506270063531051,1.15421186913492,
-2.17081979190245));
#369737=CARTESIAN_POINT('Ctrl Pts',(-0.786493493807059,0.985597069104727,
-2.15120051134026));
#369738=CARTESIAN_POINT('Ctrl Pts',(-0.910130720092299,0.872726159978944,
-2.1413900053375));
#369739=CARTESIAN_POINT('Ctrl Pts',(-1.10183240546497,0.61120721254002,
-2.12358332514547));
#369740=CARTESIAN_POINT('Ctrl Pts',(-1.17035845423982,0.466773829291593,
-2.1155064297575));
#369741=CARTESIAN_POINT('Ctrl Pts',(-1.250989790789,0.155395450473429,-2.09682372702841));
#369742=CARTESIAN_POINT('Ctrl Pts',(-1.2605702438239,-0.00904539410554187,
-2.08695727635368));
#369743=CARTESIAN_POINT('Ctrl Pts',(-1.21566154919393,-0.334877404994928,
-2.06740735570031));
#369744=CARTESIAN_POINT('Ctrl Pts',(-1.16060197035058,-0.492883303139761,
-2.05802014830617));
#369745=CARTESIAN_POINT('Ctrl Pts',(-0.995554734047103,-0.772435597087128,
-2.04105747351995));
#369746=CARTESIAN_POINT('Ctrl Pts',(-0.889336587800216,-0.892662821719336,
-2.03193140000143));
#369747=CARTESIAN_POINT('Ctrl Pts',(-0.632717987694954,-1.09061430116893,
-2.01265856201145));
#369748=CARTESIAN_POINT('Ctrl Pts',(-0.48325231240284,-1.16457864282161,
-2.00267316745407));
#369749=CARTESIAN_POINT('Ctrl Pts',(-0.167088712669152,-1.24935288526733,
-1.98370159763342));
#369750=CARTESIAN_POINT('Ctrl Pts',(-0.00380441567397249,-1.26046862460645,
-1.97551174197542));
#369751=CARTESIAN_POINT('Ctrl Pts',(0.316647040092291,-1.21988038313864,
-1.95764294864898));
#369752=CARTESIAN_POINT('Ctrl Pts',(0.470811021249917,-1.16905823065059,
-1.94810768863248));
#369753=CARTESIAN_POINT('Ctrl Pts',(0.756950846378177,-1.00870245239308,
-1.92842875382902));
#369754=CARTESIAN_POINT('Ctrl Pts',(0.884953056591838,-0.898513754696194,
-1.91847190295098));
#369755=CARTESIAN_POINT('Ctrl Pts',(1.08484115950618,-0.64096092588016,
-1.90035882758421));
#369756=CARTESIAN_POINT('Ctrl Pts',(1.15739523816577,-0.498148242707441,
-1.89238889456246));
#369757=CARTESIAN_POINT('Ctrl Pts',(1.24627629073527,-0.189149877313387,
-1.87384899263881));
#369758=CARTESIAN_POINT('Ctrl Pts',(1.26028859049331,-0.0254767233671498,
-1.86402860340204));
#369759=CARTESIAN_POINT('Ctrl Pts',(1.22449047099654,0.300943039848027,
-1.84444341760913));
#369760=CARTESIAN_POINT('Ctrl Pts',(1.17387017787683,0.460427435436986,
-1.83487435387379));
#369761=CARTESIAN_POINT('Ctrl Pts',(1.01682426480175,0.744109680436825,
-1.8178534191738));
#369762=CARTESIAN_POINT('Ctrl Pts',(0.914329258508945,0.866988940796929,
-1.80900027369363));
#369763=CARTESIAN_POINT('Ctrl Pts',(0.66410303533597,1.07171880692443,-1.78985624175215));
#369764=CARTESIAN_POINT('Ctrl Pts',(0.517300972152133,1.14978964816988,
-1.77988605755208));
#369765=CARTESIAN_POINT('Ctrl Pts',(0.24271468140597,1.23226703832922,-1.76314381364827));
#369766=CARTESIAN_POINT('Ctrl Pts',(0.121582743043821,1.25000000000003,
-1.75631762464827));
#369767=CARTESIAN_POINT('Ctrl Pts',(-2.84286483243079E-13,1.25000000000001,
-1.75));
#369768=CARTESIAN_POINT('Origin',(0.,0.,2.95));
#369769=CARTESIAN_POINT('',(1.1164467699383E-14,1.25000000000001,-1.24375000000002));
#369770=CARTESIAN_POINT('',(-4.8787575630376E-14,1.25000000000001,-1.30000000000001));
#369771=CARTESIAN_POINT('',(-1.5308084989342E-16,1.25000000000001,2.95));
#369772=CARTESIAN_POINT('Ctrl Pts',(2.24820162486595E-14,1.25000000000001,
-1.24375000000002));
#369773=CARTESIAN_POINT('Ctrl Pts',(0.0127281062361425,1.25000000000001,
-1.24441137180058));
#369774=CARTESIAN_POINT('Ctrl Pts',(0.0254632122145805,1.24980559517503,
-1.24507893946317));
#369775=CARTESIAN_POINT('Ctrl Pts',(0.203860559145116,1.24435109304023,
-1.25451237259179));
#369776=CARTESIAN_POINT('Ctrl Pts',(0.366837339527073,1.20639085544612,
-1.26411970164188));
#369777=CARTESIAN_POINT('Ctrl Pts',(0.665567426987489,1.07048208238334,
-1.28371943551069));
#369778=CARTESIAN_POINT('Ctrl Pts',(0.79896948154755,0.974969921241595,
-1.29351657443491));
#369779=CARTESIAN_POINT('Ctrl Pts',(1.01930482958355,0.74080719754203,-1.31199041667094));
#369780=CARTESIAN_POINT('Ctrl Pts',(1.10514936595059,0.605326011347319,
-1.3199304393192));
#369781=CARTESIAN_POINT('Ctrl Pts',(1.2244338282566,0.301926367291954,-1.33813441796252));
#369782=CARTESIAN_POINT('Ctrl Pts',(1.25376969848511,0.135817983777003,
-1.34810092097341));
#369783=CARTESIAN_POINT('Ctrl Pts',(1.2456139393707,-0.191692248813633,
-1.36775153492885));
#369784=CARTESIAN_POINT('Ctrl Pts',(1.21070154737509,-0.350022539283802,
-1.37725135235706));
#369785=CARTESIAN_POINT('Ctrl Pts',(1.0820322245629,-0.646659895859928,
-1.39504959375163));
#369786=CARTESIAN_POINT('Ctrl Pts',(0.988800838246133,-0.781820332299102,
-1.40332501125674));
#369787=CARTESIAN_POINT('Ctrl Pts',(0.754117042098744,-1.01045261579018,
-1.42237850752068));
#369788=CARTESIAN_POINT('Ctrl Pts',(0.614351745382173,-1.10103371717197,
-1.43235835841358));
#369789=CARTESIAN_POINT('Ctrl Pts',(0.313379499428504,-1.220463975613,-1.4515802428166));
#369790=CARTESIAN_POINT('Ctrl Pts',(0.155954832647281,-1.2503484056177,
-1.46063589701658));
#369791=CARTESIAN_POINT('Ctrl Pts',(-0.168475210398195,-1.24962999895112,
-1.47751532875827));
#369792=CARTESIAN_POINT('Ctrl Pts',(-0.332431325582248,-1.21631678881768,
-1.48703413471358));
#369793=CARTESIAN_POINT('Ctrl Pts',(-0.635284907096783,-1.08879328545755,
-1.50659657352751));
#369794=CARTESIAN_POINT('Ctrl Pts',(-0.771678355994766,-0.996782364114874,
-1.51644411266711));
#369795=CARTESIAN_POINT('Ctrl Pts',(-0.998373503197278,-0.768702169358859,
-1.53506594389332));
#369796=CARTESIAN_POINT('Ctrl Pts',(-1.08772771993399,-0.635999235042484,
-1.54309004589749));
#369797=CARTESIAN_POINT('Ctrl Pts',(-1.2155835215503,-0.336028052942537,
-1.56108831682348));
#369798=CARTESIAN_POINT('Ctrl Pts',(-1.24961419220872,-0.170316563301853,
-1.57103100620193));
#369799=CARTESIAN_POINT('Ctrl Pts',(-1.25036462615099,0.158188737307977,
-1.59074132423851));
#369800=CARTESIAN_POINT('Ctrl Pts',(-1.21960674659214,0.317816345497064,
-1.60031898072986));
#369801=CARTESIAN_POINT('Ctrl Pts',(-1.09900788393657,0.617077459222631,
-1.61827464755339));
#369802=CARTESIAN_POINT('Ctrl Pts',(-1.01015551600508,0.753785553840078,
-1.62637434629724));
#369803=CARTESIAN_POINT('Ctrl Pts',(-0.782614867327652,0.988623438011208,
-1.64524284175127));
#369804=CARTESIAN_POINT('Ctrl Pts',(-0.645070837698452,1.08339291048551,
-1.65523292335336));
#369805=CARTESIAN_POINT('Ctrl Pts',(-0.346804125794038,1.21143226967225,
-1.67457249710571));
#369806=CARTESIAN_POINT('Ctrl Pts',(-0.189838231421895,1.24572127088795,
-1.68375735426542));
#369807=CARTESIAN_POINT('Ctrl Pts',(-0.0204217310817705,1.24987494654477,
-1.69268510412202));
#369808=CARTESIAN_POINT('Ctrl Pts',(-0.0102084025352138,1.25000000000001,
-1.69321955584437));
#369809=CARTESIAN_POINT('Ctrl Pts',(-1.49880108324397E-14,1.25000000000001,
-1.69375000000002));
#369810=CARTESIAN_POINT('Ctrl Pts',(-2.84772205816363E-13,1.25000000000001,
-1.75));
#369811=CARTESIAN_POINT('Ctrl Pts',(-0.0412379402322696,1.25,-1.74785721376956));
#369812=CARTESIAN_POINT('Ctrl Pts',(-0.082521366394907,1.2479594563662,
-1.74565084771182));
#369813=CARTESIAN_POINT('Ctrl Pts',(-0.283340441980625,1.2279881156091,
-1.7346168422278));
#369814=CARTESIAN_POINT('Ctrl Pts',(-0.4384154967692,1.18153019181367,-1.72516516829753));
#369815=CARTESIAN_POINT('Ctrl Pts',(-0.72810549192602,1.02963893727432,
-1.70555569695967));
#369816=CARTESIAN_POINT('Ctrl Pts',(-0.858802387945824,0.923452201779286,
-1.69557888496588));
#369817=CARTESIAN_POINT('Ctrl Pts',(-1.06609644115566,0.671797047142976,
-1.6772579153588));
#369818=CARTESIAN_POINT('Ctrl Pts',(-1.14292836215908,0.530649881919136,
-1.66933899291516));
#369819=CARTESIAN_POINT('Ctrl Pts',(-1.24039206079692,0.224196266994979,
-1.65095177601971));
#369820=CARTESIAN_POINT('Ctrl Pts',(-1.25898881622381,0.0614480007142603,
-1.64118688004287));
#369821=CARTESIAN_POINT('Ctrl Pts',(-1.23267628598684,-0.265449968273263,
-1.62157300190361));
#369822=CARTESIAN_POINT('Ctrl Pts',(-1.18667248152148,-0.4263592175113,
-1.61191844694933));
#369823=CARTESIAN_POINT('Ctrl Pts',(-1.03795902411092,-0.714285349565246,
-1.5946428790261));
#369824=CARTESIAN_POINT('Ctrl Pts',(-0.939236737582259,-0.839893385026882,
-1.58610737094403));
#369825=CARTESIAN_POINT('Ctrl Pts',(-0.695700049671344,-1.05140649200394,
-1.56710744022566));
#369826=CARTESIAN_POINT('Ctrl Pts',(-0.551741958562074,-1.13359398593297,
-1.55716153356893));
#369827=CARTESIAN_POINT('Ctrl Pts',(-0.239639453135485,-1.23784354146212,
-1.53781672500601));
#369828=CARTESIAN_POINT('Ctrl Pts',(-0.0745058670337822,-1.25861645548798,
-1.52912993207958));
#369829=CARTESIAN_POINT('Ctrl Pts',(0.249472744485028,-1.23525801597555,
-1.51159475642273));
#369830=CARTESIAN_POINT('Ctrl Pts',(0.405344692418652,-1.19322182775177,
-1.50223432677714));
#369831=CARTESIAN_POINT('Ctrl Pts',(0.698374746362645,-1.04995514196101,
-1.48271003795615));
#369832=CARTESIAN_POINT('Ctrl Pts',(0.831672281641646,-0.947873274054076,
-1.47272123881013));
#369833=CARTESIAN_POINT('Ctrl Pts',(1.04638590509879,-0.702259138485739,
-1.45419596759593));
#369834=CARTESIAN_POINT('Ctrl Pts',(1.12756444492058,-0.562751786731794,
-1.44626510720392));
#369835=CARTESIAN_POINT('Ctrl Pts',(1.23355811931842,-0.258895173107009,
-1.42803371038643));
#369836=CARTESIAN_POINT('Ctrl Pts',(1.25667676143754,-0.0971922309217783,
-1.41833153385532));
#369837=CARTESIAN_POINT('Ctrl Pts',(1.23980119532603,0.229906637539728,
-1.39870560174763));
#369838=CARTESIAN_POINT('Ctrl Pts',(1.19843279992721,0.392097358863673,
-1.38897415846819));
#369839=CARTESIAN_POINT('Ctrl Pts',(1.05805073920253,0.684163885447196,
-1.37145016687318));
#369840=CARTESIAN_POINT('Ctrl Pts',(0.96301458371052,0.812508070063661,
-1.36316446352059));
#369841=CARTESIAN_POINT('Ctrl Pts',(0.726072104313078,1.03059125088679,
-1.34431007571227));
#369842=CARTESIAN_POINT('Ctrl Pts',(0.58501002378196,1.11671866359526,-1.33439645261598));
#369843=CARTESIAN_POINT('Ctrl Pts',(0.293050512555949,1.22406674226904,
-1.31600534903987));
#369844=CARTESIAN_POINT('Ctrl Pts',(0.147021398436324,1.25000000000002,
-1.30763945595676));
#369845=CARTESIAN_POINT('Ctrl Pts',(-9.75608482889356E-14,1.25000000000001,
-1.30000000000001));
#369846=CARTESIAN_POINT('Origin',(0.,0.,2.95));
#369847=CARTESIAN_POINT('',(1.19827546234567E-13,1.25000000000001,-0.793750000000035));
#369848=CARTESIAN_POINT('',(1.12041877347729E-15,1.25000000000001,-0.850000000000011));
#369849=CARTESIAN_POINT('',(-1.5308084989342E-16,1.25000000000001,2.95));
#369850=CARTESIAN_POINT('Ctrl Pts',(2.39808173319028E-13,1.25000000000001,
-0.793750000000035));
#369851=CARTESIAN_POINT('Ctrl Pts',(0.0365173478034769,1.25000000000001,
-0.795647497052625));
#369852=CARTESIAN_POINT('Ctrl Pts',(0.0730723172239904,1.24839986395991,
-0.797594953062993));
#369853=CARTESIAN_POINT('Ctrl Pts',(0.274707902745124,1.23065835222477,
-0.808604490777142));
#369854=CARTESIAN_POINT('Ctrl Pts',(0.435297972263029,1.18342022225767,
-0.818366139464036));
#369855=CARTESIAN_POINT('Ctrl Pts',(0.725008495213411,1.03101104211775,
-0.837992215225356));
#369856=CARTESIAN_POINT('Ctrl Pts',(0.852115607178022,0.928725125068446,
-0.847665472014617));
#369857=CARTESIAN_POINT('Ctrl Pts',(1.05948058715358,0.682424082896479,
-0.865829503710621));
#369858=CARTESIAN_POINT('Ctrl Pts',(1.13816663450739,0.541090959828185,
-0.873784542410338));
#369859=CARTESIAN_POINT('Ctrl Pts',(1.23966034531577,0.230901071017197,
-0.892395935738997));
#369860=CARTESIAN_POINT('Ctrl Pts',(1.25933320407108,0.0643772244945477,
-0.902387366530356));
#369861=CARTESIAN_POINT('Ctrl Pts',(1.23298251531999,-0.260340540740618,
-0.921870432444466));
#369862=CARTESIAN_POINT('Ctrl Pts',(1.18965009002461,-0.415659389709601,
-0.931189563382605));
#369863=CARTESIAN_POINT('Ctrl Pts',(1.04427124475132,-0.706671991977973,
-0.948650319518707));
#369864=CARTESIAN_POINT('Ctrl Pts',(0.9416398402894,-0.838584097320959,
-0.95747848154529));
#369865=CARTESIAN_POINT('Ctrl Pts',(0.692075161884984,-1.05376307551937,
-0.976901611974373));
#369866=CARTESIAN_POINT('Ctrl Pts',(0.5480324326052,-1.1353614754684,-0.986834243740048));
#369867=CARTESIAN_POINT('Ctrl Pts',(0.242017662625025,-1.23652649733511,
-1.00577018828021));
#369868=CARTESIAN_POINT('Ctrl Pts',(0.0836508584413915,-1.25720057094587,
-1.01418735676414));
#369869=CARTESIAN_POINT('Ctrl Pts',(-0.239812722176032,-1.23792859452494,
-1.03157317673759));
#369870=CARTESIAN_POINT('Ctrl Pts',(-0.401650028505976,-1.19525567937202,
-1.04126267730588));
#369871=CARTESIAN_POINT('Ctrl Pts',(-0.695931420421101,-1.05092513450937,
-1.06088390332734));
#369872=CARTESIAN_POINT('Ctrl Pts',(-0.826190438255108,-0.951935961435196,
-1.07062203563054));
#369873=CARTESIAN_POINT('Ctrl Pts',(-1.03998665229848,-0.711611274437244,
-1.08894095339615));
#369874=CARTESIAN_POINT('Ctrl Pts',(-1.12222627208494,-0.57321047632536,
-1.09685737142051));
#369875=CARTESIAN_POINT('Ctrl Pts',(-1.23259475698515,-0.2663527696126,
-1.11526883382328));
#369876=CARTESIAN_POINT('Ctrl Pts',(-1.25707176408953,-0.0999679092363408,
-1.12525192544585));
#369877=CARTESIAN_POINT('Ctrl Pts',(-1.2397440633541,0.226263518164349,
-1.14482581108989));
#369878=CARTESIAN_POINT('Ctrl Pts',(-1.20057573536714,0.383137006547994,
-1.15423822039291));
#369879=CARTESIAN_POINT('Ctrl Pts',(-1.06352535481532,0.676985820908605,
-1.17186914925455));
#369880=CARTESIAN_POINT('Ctrl Pts',(-0.96563652366167,0.810527613814236,
-1.18038988279567));
#369881=CARTESIAN_POINT('Ctrl Pts',(-0.723501631277279,1.03251673351281,
-1.19963125446348));
#369882=CARTESIAN_POINT('Ctrl Pts',(-0.581534058121792,1.11864293190939,
-1.20959189190736));
#369883=CARTESIAN_POINT('Ctrl Pts',(-0.289985603189499,1.22460330790096,
-1.22792000529143));
#369884=CARTESIAN_POINT('Ctrl Pts',(-0.145489013964085,1.25000000000001,
-1.23619016907615));
#369885=CARTESIAN_POINT('Ctrl Pts',(2.29677388219329E-14,1.25000000000001,
-1.24375000000002));
#369886=CARTESIAN_POINT('Ctrl Pts',(-9.74220704108586E-14,1.25000000000001,
-1.30000000000001));
#369887=CARTESIAN_POINT('Ctrl Pts',(-0.0190409872021563,1.25000000000001,
-1.2990106012822));
#369888=CARTESIAN_POINT('Ctrl Pts',(-0.0380972829579135,1.24956493390915,
-1.29800735512603));
#369889=CARTESIAN_POINT('Ctrl Pts',(-0.222731980051923,1.24111397627159,
-1.28815992611069));
#369890=CARTESIAN_POINT('Ctrl Pts',(-0.385128926343269,1.20067890393287,
-1.2785084810814));
#369891=CARTESIAN_POINT('Ctrl Pts',(-0.681556641099898,1.06033714157496,
-1.25889539232875));
#369892=CARTESIAN_POINT('Ctrl Pts',(-0.813322019598976,0.962989753698685,
-1.2491282407853));
#369893=CARTESIAN_POINT('Ctrl Pts',(-1.0302354240953,0.725591051741989,
-1.23073512860368));
#369894=CARTESIAN_POINT('Ctrl Pts',(-1.11419355189862,0.588590187634581,
-1.22281541125822));
#369895=CARTESIAN_POINT('Ctrl Pts',(-1.22882546163461,0.283372076139634,
-1.20450232456852));
#369896=CARTESIAN_POINT('Ctrl Pts',(-1.25562223077578,0.117102176125761,
-1.19452613056768));
#369897=CARTESIAN_POINT('Ctrl Pts',(-1.24266769967108,-0.209771385660699,
-1.17491371686049));
#369898=CARTESIAN_POINT('Ctrl Pts',(-1.20552571858969,-0.367354877423882,
-1.1654587073547));
#369899=CARTESIAN_POINT('Ctrl Pts',(-1.07248116616986,-0.662544656832272,
-1.14774732059019));
#369900=CARTESIAN_POINT('Ctrl Pts',(-0.976832623185124,-0.796862145498132,
-1.13935184765062));
#369901=CARTESIAN_POINT('Ctrl Pts',(-0.738262791311813,-1.02205221437746,
-1.1201996934855));
#369902=CARTESIAN_POINT('Ctrl Pts',(-0.59733404065815,-1.11032074290285,
-1.11022876493836));
#369903=CARTESIAN_POINT('Ctrl Pts',(-0.295016969221521,-1.22500492444781,
-1.0910793836603));
#369904=CARTESIAN_POINT('Ctrl Pts',(-0.137369759755668,-1.25250311107604,
-1.08221303543204));
#369905=CARTESIAN_POINT('Ctrl Pts',(0.186845868943726,-1.24701759014455,
-1.06520173155863));
#369906=CARTESIAN_POINT('Ctrl Pts',(0.350311044841314,-1.21129078502437,
-1.05563602770734));
#369907=CARTESIAN_POINT('Ctrl Pts',(0.651055283763593,-1.07940213285225,
-1.03605223908526));
#369908=CARTESIAN_POINT('Ctrl Pts',(0.785908291001378,-0.985563751667752,
-1.02622991984705));
#369909=CARTESIAN_POINT('Ctrl Pts',(1.00931044594874,-0.754322872482359,
-1.00768437698481));
#369910=CARTESIAN_POINT('Ctrl Pts',(1.0968464808068,-0.620188757326572,
-0.999711325439738));
#369911=CARTESIAN_POINT('Ctrl Pts',(1.22027633890838,-0.318434680606061,
-0.981606080836504));
#369912=CARTESIAN_POINT('Ctrl Pts',(1.25188032904612,-0.152502113655608,
-0.971650126819475));
#369913=CARTESIAN_POINT('Ctrl Pts',(1.24802188377458,0.17551837181343,-0.951968897691329));
#369914=CARTESIAN_POINT('Ctrl Pts',(1.21511140908213,0.334488951887869,
-0.942430662886862));
#369915=CARTESIAN_POINT('Ctrl Pts',(1.09034364386156,0.632402229996957,
-0.924555866200313));
#369916=CARTESIAN_POINT('Ctrl Pts',(0.999241971903155,0.768311677217683,
-0.916372785615359));
#369917=CARTESIAN_POINT('Ctrl Pts',(0.768015762081745,0.999966960031412,
-0.897408260827375));
#369918=CARTESIAN_POINT('Ctrl Pts',(0.629312446831229,1.09258559884888,
-0.887422465987086));
#369919=CARTESIAN_POINT('Ctrl Pts',(0.329671299273571,1.21617780828834,
-0.868144888955655));
#369920=CARTESIAN_POINT('Ctrl Pts',(0.172459340124662,1.24821827234065,
-0.859014702009984));
#369921=CARTESIAN_POINT('Ctrl Pts',(0.00895700522214871,1.24997593707043,
-0.85046614153187));
#369922=CARTESIAN_POINT('Ctrl Pts',(0.004477996082354,1.25000000000001,
-0.850232683501933));
#369923=CARTESIAN_POINT('Ctrl Pts',(0.,1.25000000000001,-0.850000000000011));
#369924=CARTESIAN_POINT('Origin',(0.,0.,2.95));
#369925=CARTESIAN_POINT('',(3.73401184355099E-14,1.25000000000001,-0.343750000000027));
#369926=CARTESIAN_POINT('',(1.04839535402128E-13,1.25000000000001,-0.400000000000021));
#369927=CARTESIAN_POINT('',(-1.5308084989342E-16,1.25000000000001,2.95));
#369928=CARTESIAN_POINT('Ctrl Pts',(7.48333177209133E-14,1.25000000000001,
-0.343750000000027));
#369929=CARTESIAN_POINT('Ctrl Pts',(0.0590798183387906,1.25000000000001,
-0.346819877411967));
#369930=CARTESIAN_POINT('Ctrl Pts',(0.118203739862037,1.24581209387059,
-0.350017683676478));
#369931=CARTESIAN_POINT('Ctrl Pts',(0.342396087495437,1.2137553293898,-0.362628762713977));
#369932=CARTESIAN_POINT('Ctrl Pts',(0.501422074682511,1.15715155894079,
-0.372590108513402));
#369933=CARTESIAN_POINT('Ctrl Pts',(0.782302987972495,0.988096824696519,
-0.392256750921568));
#369934=CARTESIAN_POINT('Ctrl Pts',(0.902760319636144,0.879414999889457,
-0.401776352223348));
#369935=CARTESIAN_POINT('Ctrl Pts',(1.09688175758355,0.621062980984667,
-0.41961375859139));
#369936=CARTESIAN_POINT('Ctrl Pts',(1.16819441836778,0.473494446690105,
-0.427840333198619));
#369937=CARTESIAN_POINT('Ctrl Pts',(1.25107686146537,0.156690871643344,
-0.446848547701424));
#369938=CARTESIAN_POINT('Ctrl Pts',(1.26081210456799,-0.00969444195940881,
-0.45683166651759));
#369939=CARTESIAN_POINT('Ctrl Pts',(1.21594231605393,-0.330490392139359,
-0.476079423528387));
#369940=CARTESIAN_POINT('Ctrl Pts',(1.16413593700529,-0.482231152694698,
-0.485183869161707));
#369941=CARTESIAN_POINT('Ctrl Pts',(1.00310790144222,-0.764002651354767,
-0.502090159081311));
#369942=CARTESIAN_POINT('Ctrl Pts',(0.893137586098338,-0.890100582752752,
-0.511544227164456));
#369943=CARTESIAN_POINT('Ctrl Pts',(0.632419645583964,-1.09047567866554,
-0.531102781624308));
#369944=CARTESIAN_POINT('Ctrl Pts',(0.484914215223203,-1.16359546852985,
-0.540960982313552));
#369945=CARTESIAN_POINT('Ctrl Pts',(0.174538128288854,-1.24786536409498,
-0.559616693741247));
#369946=CARTESIAN_POINT('Ctrl Pts',(0.0150798860017847,-1.25991949277691,
-0.567668841354896));
#369947=CARTESIAN_POINT('Ctrl Pts',(-0.307116863691302,-1.22297551077751,
-0.585518995029937));
#369948=CARTESIAN_POINT('Ctrl Pts',(-0.466421854092992,-1.17150569243725,
-0.595340819698395));
#369949=CARTESIAN_POINT('Ctrl Pts',(-0.751660673322387,-1.01167905245061,
-0.614957062713882));
#369950=CARTESIAN_POINT('Ctrl Pts',(-0.875749745986111,-0.906400855472546,
-0.624563265978754));
#369951=CARTESIAN_POINT('Ctrl Pts',(-1.07705624390254,-0.654543977177846,
-0.642579164796146));
#369952=CARTESIAN_POINT('Ctrl Pts',(-1.15238050450015,-0.510392064237707,
-0.650626476145764));
#369953=CARTESIAN_POINT('Ctrl Pts',(-1.24541625508687,-0.197131903492209,
-0.669422085790494));
#369954=CARTESIAN_POINT('Ctrl Pts',(-1.26054739582606,-0.0305998677198683,
-0.679414007936835));
#369955=CARTESIAN_POINT('Ctrl Pts',(-1.22570860841471,0.292458283934986,
-0.698797497036126));
#369956=CARTESIAN_POINT('Ctrl Pts',(-1.17847991536056,0.446202662816261,
-0.708022159769002));
#369957=CARTESIAN_POINT('Ctrl Pts',(-1.02517732108211,0.734455413406625,
-0.725317324804424));
#369958=CARTESIAN_POINT('Ctrl Pts',(-0.917925590338391,0.864787847910805,
-0.734496822636339));
#369959=CARTESIAN_POINT('Ctrl Pts',(-0.661276644980384,1.07328691194847,
-0.75408766494954));
#369960=CARTESIAN_POINT('Ctrl Pts',(-0.515371358678158,1.15048969731129,
-0.763985209579475));
#369961=CARTESIAN_POINT('Ctrl Pts',(-0.242149779611746,1.23234648324921,
-0.780637922857629));
#369962=CARTESIAN_POINT('Ctrl Pts',(-0.121309990693237,1.25000000000001,
-0.787446547979619));
#369963=CARTESIAN_POINT('Ctrl Pts',(2.40345937596587E-13,1.25000000000001,
-0.793750000000035));
#369964=CARTESIAN_POINT('Ctrl Pts',(6.93889390390723E-16,1.25000000000001,
-0.850000000000011));
#369965=CARTESIAN_POINT('Ctrl Pts',(-0.161070456295141,1.25000000000001,
-0.841630533582966));
#369966=CARTESIAN_POINT('Ctrl Pts',(-0.320734334238032,1.21886810249861,
-0.832400198196137));
#369967=CARTESIAN_POINT('Ctrl Pts',(-0.621354677061918,1.09683306156792,
-0.813118455741421));
#369968=CARTESIAN_POINT('Ctrl Pts',(-0.759078094490395,1.00644365084719,
-0.803250454728453));
#369969=CARTESIAN_POINT('Ctrl Pts',(-0.988649420329641,0.781144304134001,
-0.784562598317619));
#369970=CARTESIAN_POINT('Ctrl Pts',(-1.07959412169325,0.649678886643446,
-0.776480733198751));
#369971=CARTESIAN_POINT('Ctrl Pts',(-1.21051709652743,0.353039718571868,
-0.758682383114453));
#369972=CARTESIAN_POINT('Ctrl Pts',(-1.24661034872577,0.189567869179206,
-0.748874072150891));
#369973=CARTESIAN_POINT('Ctrl Pts',(-1.2528498488519,-0.137428795599859,
-0.729254272264144));
#369974=CARTESIAN_POINT('Ctrl Pts',(-1.22468102346119,-0.297804126963716,
-0.719631752382311));
#369975=CARTESIAN_POINT('Ctrl Pts',(-1.10906314316296,-0.598654633471895,
-0.701580721991817));
#369976=CARTESIAN_POINT('Ctrl Pts',(-1.02286331264974,-0.736316148380509,
-0.693560052349953));
#369977=CARTESIAN_POINT('Ctrl Pts',(-0.79971284996578,-0.974893530087458,
-0.674807492725708));
#369978=CARTESIAN_POINT('Ctrl Pts',(-0.663585751690908,-1.07219633131756,
-0.664815037173834));
#369979=CARTESIAN_POINT('Ctrl Pts',(-0.367033046470049,-1.20549191785441,
-0.645406839000789));
#369980=CARTESIAN_POINT('Ctrl Pts',(-0.210400404408204,-1.24244664919953,
-0.636159326235188));
#369981=CARTESIAN_POINT('Ctrl Pts',(0.115517861008065,-1.2557624780115,
-0.618824641526355));
#369982=CARTESIAN_POINT('Ctrl Pts',(0.281789808952139,-1.22918976875112,
-0.609733465077867));
#369983=CARTESIAN_POINT('Ctrl Pts',(0.591225776742806,-1.11342710022432,
-0.59018182048498));
#369984=CARTESIAN_POINT('Ctrl Pts',(0.731730043175942,-1.02656762164794,
-0.580275220283415));
#369985=CARTESIAN_POINT('Ctrl Pts',(0.967424821284296,-0.807253702477117,
-0.561448742785417));
#369986=CARTESIAN_POINT('Ctrl Pts',(1.06176654932889,-0.678386061936249,
-0.553203163716318));
#369987=CARTESIAN_POINT('Ctrl Pts',(1.20055853238085,-0.385541243379893,
-0.535632474602934));
#369988=CARTESIAN_POINT('Ctrl Pts',(1.24104077393615,-0.223122249194351,
-0.5258873349518));
#369989=CARTESIAN_POINT('Ctrl Pts',(1.25612202631843,0.103983811598946,
-0.506260971304199));
#369990=CARTESIAN_POINT('Ctrl Pts',(1.23214798552696,0.26547389174927,-0.496571566495178));
#369991=CARTESIAN_POINT('Ctrl Pts',(1.12453189915568,0.568829763456653,
-0.478370214192732));
#369992=CARTESIAN_POINT('Ctrl Pts',(1.04251622806055,0.70802524800795,-0.470429974801382));
#369993=CARTESIAN_POINT('Ctrl Pts',(0.826384873996718,0.95247021514956,
-0.451866111196714));
#369994=CARTESIAN_POINT('Ctrl Pts',(0.692602275545821,1.05375733649945,
-0.441875949825649));
#369995=CARTESIAN_POINT('Ctrl Pts',(0.398959608144391,1.19536072578793,
-0.422369727570711));
#369996=CARTESIAN_POINT('Ctrl Pts',(0.242948921825937,1.23654700648412,
-0.413027586093006));
#369997=CARTESIAN_POINT('Ctrl Pts',(0.0555960823497595,1.24907368203338,
-0.402916646719076));
#369998=CARTESIAN_POINT('Ctrl Pts',(0.0277840398287292,1.25000000000001,
-0.401443701058694));
#369999=CARTESIAN_POINT('Ctrl Pts',(2.0983215165415E-13,1.25000000000001,
-0.400000000000021));
#370000=CARTESIAN_POINT('Origin',(0.,0.,2.95));
#370001=CARTESIAN_POINT('',(-7.654042494671E-17,1.25000000000001,0.106249999999977));
#370002=CARTESIAN_POINT('',(1.04876898677003E-13,1.25000000000001,0.0499999999999784));
#370003=CARTESIAN_POINT('',(-1.5308084989342E-16,1.25000000000001,2.95));
#370004=CARTESIAN_POINT('Ctrl Pts',(0.,1.25000000000001,0.106249999999977));
#370005=CARTESIAN_POINT('Ctrl Pts',(0.0834088693143275,1.25000000000001,
0.101915948016348));
#370006=CARTESIAN_POINT('Ctrl Pts',(0.166785812227005,1.24165359687058,
0.0973331628833295));
#370007=CARTESIAN_POINT('Ctrl Pts',(0.411738826024968,1.1918818279468,0.0831118778546601));
#370008=CARTESIAN_POINT('Ctrl Pts',(0.566342753569499,1.12665789301637,
0.0731217040800425));
#370009=CARTESIAN_POINT('Ctrl Pts',(0.835784555992207,0.943143645940193,
0.0536156699233854));
#370010=CARTESIAN_POINT('Ctrl Pts',(0.949451415498427,0.828621999182428,
0.0442737172466055));
#370011=CARTESIAN_POINT('Ctrl Pts',(1.13037087400892,0.558593324922486,
0.0267720061922665));
#370012=CARTESIAN_POINT('Ctrl Pts',(1.19420420310689,0.404549174140306,
0.018022950448395));
#370013=CARTESIAN_POINT('Ctrl Pts',(1.2580832363353,0.0815449674168411,
-0.00135730195501261));
#370014=CARTESIAN_POINT('Ctrl Pts',(1.25791345087848,-0.0841239198618764,
-0.0112974351917356));
#370015=CARTESIAN_POINT('Ctrl Pts',(1.19470875237361,-0.400310883510322,
-0.0302686530106424));
#370016=CARTESIAN_POINT('Ctrl Pts',(1.13445349055922,-0.548243673418319,
-0.0387493776684003));
#370017=CARTESIAN_POINT('Ctrl Pts',(0.957917079583416,-0.819981873941055,
-0.0560746246799611));
#370018=CARTESIAN_POINT('Ctrl Pts',(0.840879668656194,-0.939615820839286,
-0.0657450853502759));
#370019=CARTESIAN_POINT('Ctrl Pts',(0.569944260123193,-1.12426118399076,
-0.0853626630392777));
#370020=CARTESIAN_POINT('Ctrl Pts',(0.419422598591749,-1.18865152536158,
-0.0951157082427667));
#370021=CARTESIAN_POINT('Ctrl Pts',(0.104889477891838,-1.25575118075505,
-0.113472318276034));
#370022=CARTESIAN_POINT('Ctrl Pts',(-0.0559083233995013,-1.25888277588398,
-0.121388598424323));
#370023=CARTESIAN_POINT('Ctrl Pts',(-0.377203291411351,-1.2033249302256,
-0.139750310058456));
#370024=CARTESIAN_POINT('Ctrl Pts',(-0.534076587870779,-1.14237658644158,
-0.149730135966533));
#370025=CARTESIAN_POINT('Ctrl Pts',(-0.809334411153535,-0.966008315914971,
-0.169324000135528));
#370026=CARTESIAN_POINT('Ctrl Pts',(-0.926434823137354,-0.854358209189572,
-0.178758219231586));
#370027=CARTESIAN_POINT('Ctrl Pts',(-1.11399790116324,-0.590164314846684,
-0.196430099484818));
#370028=CARTESIAN_POINT('Ctrl Pts',(-1.18161572487833,-0.439409693334734,
-0.20488541839994));
#370029=CARTESIAN_POINT('Ctrl Pts',(-1.25511391105904,-0.119472629925005,
-0.224081642204524));
#370030=CARTESIAN_POINT('Ctrl Pts',(-1.25992391885208,0.0466293087341037,
-0.234047758524071));
#370031=CARTESIAN_POINT('Ctrl Pts',(-1.20592409544673,0.365231644649184,
-0.253163898678975));
#370032=CARTESIAN_POINT('Ctrl Pts',(-1.14992525470469,0.515058082995038,
-0.261949873508223));
#370033=CARTESIAN_POINT('Ctrl Pts',(-0.981240132165863,0.791918120465329,
-0.279020810713878));
#370034=CARTESIAN_POINT('Ctrl Pts',(-0.867735079639031,0.914867029055821,
-0.288607173508361));
#370035=CARTESIAN_POINT('Ctrl Pts',(-0.601922899937307,1.10753616276619,
-0.308199253535092));
#370036=CARTESIAN_POINT('Ctrl Pts',(-0.452870998658559,1.17637648246142,
-0.318009427105334));
#370037=CARTESIAN_POINT('Ctrl Pts',(-0.198077417543586,1.23821417476648,
-0.333104020712493));
#370038=CARTESIAN_POINT('Ctrl Pts',(-0.0991193281752952,1.25000000000001,
-0.338599608627669));
#370039=CARTESIAN_POINT('Ctrl Pts',(7.48333177209133E-14,1.25000000000001,
-0.343750000000027));
#370040=CARTESIAN_POINT('Ctrl Pts',(2.09485206958959E-13,1.25000000000001,
-0.400000000000021));
#370041=CARTESIAN_POINT('Ctrl Pts',(-0.136903696688647,1.25000000000001,
-0.392886275247762));
#370042=CARTESIAN_POINT('Ctrl Pts',(-0.273058001040094,1.22751495154707,
-0.385136938610113));
#370043=CARTESIAN_POINT('Ctrl Pts',(-0.558353812348898,1.13033815795081,
-0.367397229591019));
#370044=CARTESIAN_POINT('Ctrl Pts',(-0.70174819474871,1.04736472661969,
-0.357457035975991));
#370045=CARTESIAN_POINT('Ctrl Pts',(-0.943985141713251,0.834547743205648,
-0.338485525485178));
#370046=CARTESIAN_POINT('Ctrl Pts',(-1.041978547034,0.708404271325426,-0.330004256279668));
#370047=CARTESIAN_POINT('Ctrl Pts',(-1.18905932418912,0.419658566023798,
-0.312679513961568));
#370048=CARTESIAN_POINT('Ctrl Pts',(-1.23415599260509,0.258486892859228,
-0.303009213571692));
#370049=CARTESIAN_POINT('Ctrl Pts',(-1.25861492432823,-0.0684721620563943,
-0.283391670276752));
#370050=CARTESIAN_POINT('Ctrl Pts',(-1.23912692196633,-0.231024950580754,
-0.273638502965289));
#370051=CARTESIAN_POINT('Ctrl Pts',(-1.139987597103,-0.536973656436101,
-0.255281580613964));
#370052=CARTESIAN_POINT('Ctrl Pts',(-1.0623094578172,-0.677797753505098,
-0.247365286023998));
#370053=CARTESIAN_POINT('Ctrl Pts',(-0.853562419787044,-0.928280526100581,
-0.229003988572199));
#370054=CARTESIAN_POINT('Ctrl Pts',(-0.722348260470575,-1.03367082872141,
-0.219024191775315));
#370055=CARTESIAN_POINT('Ctrl Pts',(-0.431986812182885,-1.18388425517077,
-0.199430165552024));
#370056=CARTESIAN_POINT('Ctrl Pts',(-0.276746455241951,-1.22948001514874,
-0.189995767184479));
#370057=CARTESIAN_POINT('Ctrl Pts',(0.0458301644706234,-1.25983488406571,
-0.172323548276687));
#370058=CARTESIAN_POINT('Ctrl Pts',(0.210194521093855,-1.24302612505785,
-0.163868756051661));
#370059=CARTESIAN_POINT('Ctrl Pts',(0.524021402602072,-1.14672862259996,
-0.144672907871327));
#370060=CARTESIAN_POINT('Ctrl Pts',(0.670280527211671,-1.06785153907181,
-0.134706748318649));
#370061=CARTESIAN_POINT('Ctrl Pts',(0.919211696323998,-0.861798778988717,
-0.115590322541451));
#370062=CARTESIAN_POINT('Ctrl Pts',(1.02097333773227,-0.738394566236283,
-0.10680367397432));
#370063=CARTESIAN_POINT('Ctrl Pts',(1.17641517753716,-0.453887450265798,
-0.0897332470160875));
#370064=CARTESIAN_POINT('Ctrl Pts',(1.22614869806113,-0.29411765853171,
-0.0801470595120406));
#370065=CARTESIAN_POINT('Ctrl Pts',(1.26011786530385,0.032415887063119,
-0.0605550467763477));
#370066=CARTESIAN_POINT('Ctrl Pts',(1.24521853548645,0.195920544983718,
-0.0507447673011102));
#370067=CARTESIAN_POINT('Ctrl Pts',(1.1546812098639,0.504433246136558,-0.032234005231937));
#370068=CARTESIAN_POINT('Ctrl Pts',(1.0813087608889,0.646923000665087,-0.024278761356057));
#370069=CARTESIAN_POINT('Ctrl Pts',(0.879996318837545,0.903351473327351,
-0.00612540584132411));
#370070=CARTESIAN_POINT('Ctrl Pts',(0.75146843718215,1.01277802912597,0.00383589546912666));
#370071=CARTESIAN_POINT('Ctrl Pts',(0.464629472064984,1.17151740429263,
0.0235026665593323));
#370072=CARTESIAN_POINT('Ctrl Pts',(0.310281465381834,1.22150424509551,
0.0330224294720864));
#370073=CARTESIAN_POINT('Ctrl Pts',(0.100584043353169,1.24696823739944,
0.0446825469163021));
#370074=CARTESIAN_POINT('Ctrl Pts',(0.0502665808276812,1.25000000000001,
0.0473880718425048));
#370075=CARTESIAN_POINT('Ctrl Pts',(2.099068782039E-13,1.25000000000001,
0.0499999999999786));
#370076=CARTESIAN_POINT('Origin',(0.,0.,2.95));
#370077=CARTESIAN_POINT('',(-9.75093065587137E-14,1.25000000000001,0.556249999999987));
#370078=CARTESIAN_POINT('',(-7.654042494671E-17,1.25000000000001,0.499999999999989));
#370079=CARTESIAN_POINT('',(-1.5308084989342E-16,1.25000000000001,2.95));
#370080=CARTESIAN_POINT('Ctrl Pts',(-1.95538030212106E-13,1.25000000000001,
0.556249999999987));
#370081=CARTESIAN_POINT('Ctrl Pts',(0.110095727452467,1.25000000000002,
0.550529258190659));
#370082=CARTESIAN_POINT('Ctrl Pts',(0.219897164527631,1.23545967302211,
0.544387598348574));
#370083=CARTESIAN_POINT('Ctrl Pts',(0.483988304843397,1.16397911390651,
0.528520603389435));
#370084=CARTESIAN_POINT('Ctrl Pts',(0.631540368194716,1.09098321222581,
0.518663696224431));
#370085=CARTESIAN_POINT('Ctrl Pts',(0.892410668998942,0.890829214599118,
0.49910385784027));
#370086=CARTESIAN_POINT('Ctrl Pts',(1.00248282092227,0.7648221248362,0.489639327490149));
#370087=CARTESIAN_POINT('Ctrl Pts',(1.16373402854627,0.483196003908649,
0.472741760234496));
#370088=CARTESIAN_POINT('Ctrl Pts',(1.21566272275007,0.331511123020428,
0.463640667381203));
#370089=CARTESIAN_POINT('Ctrl Pts',(1.26080142902313,0.0107803782299532,
0.444396822693775));
#370090=CARTESIAN_POINT('Ctrl Pts',(1.25121127696836,-0.155598633295204,
0.434414082002265));
#370091=CARTESIAN_POINT('Ctrl Pts',(1.16860360178229,-0.472495905952001,
0.415400245642857));
#370092=CARTESIAN_POINT('Ctrl Pts',(1.09739924970882,-0.620157362400895,
0.407167816828459));
#370093=CARTESIAN_POINT('Ctrl Pts',(0.903470949119029,-0.878682593259535,
0.38933524981329));
#370094=CARTESIAN_POINT('Ctrl Pts',(0.783111943046633,-0.987453723955263,
0.379818078483398));
#370095=CARTESIAN_POINT('Ctrl Pts',(0.507349053267152,-1.1537400470651,
0.360500428711867));
#370096=CARTESIAN_POINT('Ctrl Pts',(0.354373467382822,-1.20952473987467,
0.350878043314579));
#370097=CARTESIAN_POINT('Ctrl Pts',(0.0360168821165519,-1.25980624593843,
0.332827304714507));
#370098=CARTESIAN_POINT('Ctrl Pts',(-0.126302915894441,-1.25397726122806,
0.32480642581262));
#370099=CARTESIAN_POINT('Ctrl Pts',(-0.44448908312833,-1.17999457526421,
0.306053506996264));
#370100=CARTESIAN_POINT('Ctrl Pts',(-0.596814831391358,-1.11074875148646,
0.296061054224156));
#370101=CARTESIAN_POINT('Ctrl Pts',(-0.860517304112876,-0.920561641676312,
0.276653058504795));
#370102=CARTESIAN_POINT('Ctrl Pts',(-0.970830823621374,-0.803386125286054,
0.267405734396574));
#370103=CARTESIAN_POINT('Ctrl Pts',(-1.14530928127823,-0.527779774932947,
0.250071377281343));
#370104=CARTESIAN_POINT('Ctrl Pts',(-1.20542533674739,-0.370491333408049,
0.24097948000446));
#370105=CARTESIAN_POINT('Ctrl Pts',(-1.25987147061771,-0.0446251390695866,
0.221427508344152));
#370106=CARTESIAN_POINT('Ctrl Pts',(-1.25489176136244,0.120483642117867,
0.211520981472905));
#370107=CARTESIAN_POINT('Ctrl Pts',(-1.18279045668018,0.434253498461013,
0.192694790092316));
#370108=CARTESIAN_POINT('Ctrl Pts',(-1.1183504744051,0.580386185888755,
0.184449609693465));
#370109=CARTESIAN_POINT('Ctrl Pts',(-0.934120381403464,0.846995847917418,
0.166878443391746));
#370110=CARTESIAN_POINT('Ctrl Pts',(-0.813695985431435,0.963257286950447,
0.157133165051925));
#370111=CARTESIAN_POINT('Ctrl Pts',(-0.537945249268492,1.13985516804468,
0.137506800061336));
#370112=CARTESIAN_POINT('Ctrl Pts',(-0.386101249454913,1.19982940090801,
0.127817527400389));
#370113=CARTESIAN_POINT('Ctrl Pts',(-0.15197324095669,1.24307314195488,
0.114354566983167));
#370114=CARTESIAN_POINT('Ctrl Pts',(-0.0759842892410821,1.25000000000001,
0.110198259486254));
#370115=CARTESIAN_POINT('Ctrl Pts',(0.,1.25000000000001,0.106249999999977));
#370116=CARTESIAN_POINT('Ctrl Pts',(2.11150541495897E-13,1.25000000000001,
0.0499999999999785));
#370117=CARTESIAN_POINT('Ctrl Pts',(-0.111470455421133,1.25000000000001,
0.0557921747699455));
#370118=CARTESIAN_POINT('Ctrl Pts',(-0.222643888038024,1.23509422747958,
0.0620160889577699));
#370119=CARTESIAN_POINT('Ctrl Pts',(-0.489772689440863,1.16183835855839,
0.078094184711249));
#370120=CARTESIAN_POINT('Ctrl Pts',(-0.638739409342658,1.08708482841797,
0.0880773284406671));
#370121=CARTESIAN_POINT('Ctrl Pts',(-0.894134663808368,0.88784181787852,
0.107325345459251));
#370122=CARTESIAN_POINT('Ctrl Pts',(-0.99965011951641,0.767110993144499,
0.116430014109376));
#370123=CARTESIAN_POINT('Ctrl Pts',(-1.16317318624406,0.486778909701346,
0.133336884406127));
#370124=CARTESIAN_POINT('Ctrl Pts',(-1.21740066739827,0.328495708506877,
0.14279025748945));
#370125=CARTESIAN_POINT('Ctrl Pts',(-1.26058944048159,0.00252123275269689,
0.162348726034704));
#370126=CARTESIAN_POINT('Ctrl Pts',(-1.25016901739024,-0.161783543797773,
0.172207012627734));
#370127=CARTESIAN_POINT('Ctrl Pts',(-1.16797700891844,-0.472716691392178,
0.190863001483401));
#370128=CARTESIAN_POINT('Ctrl Pts',(-1.09869491440265,-0.616841832868966,
0.198915392573041));
#370129=CARTESIAN_POINT('Ctrl Pts',(-0.90561638891264,-0.877410288353267,
0.216765100717548));
#370130=CARTESIAN_POINT('Ctrl Pts',(-0.781395758288791,-0.98964417282974,
0.226586810559507));
#370131=CARTESIAN_POINT('Ctrl Pts',(-0.500370692919775,-1.15677037951647,
0.246203087502697));
#370132=CARTESIAN_POINT('Ctrl Pts',(-0.347154646230893,-1.21160391429263,
0.255809432867983));
#370133=CARTESIAN_POINT('Ctrl Pts',(-0.0283905049197947,-1.26002830846002,
0.273825635344463));
#370134=CARTESIAN_POINT('Ctrl Pts',(0.134109254753663,-1.25319391071158,
0.281872703968469));
#370135=CARTESIAN_POINT('Ctrl Pts',(0.451921694253178,-1.17715322848757,
0.30066794320991));
#370136=CARTESIAN_POINT('Ctrl Pts',(0.603712955450508,-1.10699912270918,
0.310659871679425));
#370137=CARTESIAN_POINT('Ctrl Pts',(0.866081876952995,-0.915311906885435,
0.330043577225222));
#370138=CARTESIAN_POINT('Ctrl Pts',(0.975620884385336,-0.797543653015307,
0.339268438629833));
#370139=CARTESIAN_POINT('Ctrl Pts',(1.148616831659,-0.520664513371695,0.356563945924589));
#370140=CARTESIAN_POINT('Ctrl Pts',(1.20786977038538,-0.362622214666592,
0.365742667119868));
#370141=CARTESIAN_POINT('Ctrl Pts',(1.26013003425235,-0.0361137966221107,
0.38533317220254));
#370142=CARTESIAN_POINT('Ctrl Pts',(1.25404666538466,0.128846617713408,
0.395230797062673));
#370143=CARTESIAN_POINT('Ctrl Pts',(1.17990149401884,0.44204997373243,0.414022998423818));
#370144=CARTESIAN_POINT('Ctrl Pts',(1.11448934346675,0.587773184588203,
0.422222630516152));
#370145=CARTESIAN_POINT('Ctrl Pts',(0.928477354831601,0.853178879245708,
0.439850267809871));
#370146=CARTESIAN_POINT('Ctrl Pts',(0.807279689485484,0.968641952923779,
0.449611775444361));
#370147=CARTESIAN_POINT('Ctrl Pts',(0.530443711573877,1.14335071217548,
0.469237857595093));
#370148=CARTESIAN_POINT('Ctrl Pts',(0.378310471213608,1.20229482442116,
0.478911256017188));
#370149=CARTESIAN_POINT('Ctrl Pts',(0.146649687795479,1.24355080550249,
0.492186382859672));
#370150=CARTESIAN_POINT('Ctrl Pts',(0.0733172695478839,1.25000000000001,
0.496190322922115));
#370151=CARTESIAN_POINT('Ctrl Pts',(0.,1.25000000000001,0.499999999999989));
#370152=CARTESIAN_POINT('Origin',(0.,0.,2.95));
#370153=CARTESIAN_POINT('',(-8.24839292940005E-14,1.25000000000001,1.00624999999999));
#370154=CARTESIAN_POINT('',(-3.00232052310016E-14,1.25000000000001,0.949999999999992));
#370155=CARTESIAN_POINT('',(-1.5308084989342E-16,1.25000000000001,2.95));
#370156=CARTESIAN_POINT('Ctrl Pts',(-1.64070146357886E-13,1.25000000000001,
1.00624999999999));
#370157=CARTESIAN_POINT('Ctrl Pts',(0.132760180009687,1.25000000000002,
0.999351578690014));
#370158=CARTESIAN_POINT('Ctrl Pts',(0.264827410352974,1.22885544962755,
0.991854827589753));
#370159=CARTESIAN_POINT('Ctrl Pts',(0.546966301958247,1.13587327957377,
0.974404995636595));
#370160=CARTESIAN_POINT('Ctrl Pts',(0.691072290179626,1.05441864922568,
0.964473389927922));
#370161=CARTESIAN_POINT('Ctrl Pts',(0.940870633762533,0.839457016764246,
0.945044638272116));
#370162=CARTESIAN_POINT('Ctrl Pts',(1.04365286579185,0.707596550603973,
0.936205793036214));
#370163=CARTESIAN_POINT('Ctrl Pts',(1.18929328356091,0.416674090237899,
0.91875044541425));
#370164=CARTESIAN_POINT('Ctrl Pts',(1.23275537538807,0.261405752446612,
0.909434345146773));
#370165=CARTESIAN_POINT('Ctrl Pts',(1.25938782921475,-0.0632606126396011,
0.8899543632416));
#370166=CARTESIAN_POINT('Ctrl Pts',(1.23986538365966,-0.229786650150815,
0.879962800990927));
#370167=CARTESIAN_POINT('Ctrl Pts',(1.1386506424248,-0.540079495994821,
0.861345230240287));
#370168=CARTESIAN_POINT('Ctrl Pts',(1.06007585639613,-0.681505171105023,
0.85338800216148));
#370169=CARTESIAN_POINT('Ctrl Pts',(0.852911782822347,-0.927991634854894,
0.835228847221003));
#370170=CARTESIAN_POINT('Ctrl Pts',(0.725904037164835,-1.030378561644,0.825557723364322));
#370171=CARTESIAN_POINT('Ctrl Pts',(0.436339301598169,-1.18303677761975,
0.805931751862598));
#370172=CARTESIAN_POINT('Ctrl Pts',(0.275790164279255,-1.23041635082661,
0.796167986777961));
#370173=CARTESIAN_POINT('Ctrl Pts',(-0.047042049554638,-1.25910770535608,
0.77853239224167));
#370174=CARTESIAN_POINT('Ctrl Pts',(-0.205966929131309,-1.2430424311163,
0.770338917355434));
#370175=CARTESIAN_POINT('Ctrl Pts',(-0.514356173324183,-1.15094190380244,
0.751551526352524));
#370176=CARTESIAN_POINT('Ctrl Pts',(-0.660316890432176,-1.07387545713724,
0.741655191614361));
#370177=CARTESIAN_POINT('Ctrl Pts',(-0.917183631103573,-0.865584795699296,
0.722059284402699));
#370178=CARTESIAN_POINT('Ctrl Pts',(-1.02457899863437,-0.735301446329246,
0.712868086779731));
#370179=CARTESIAN_POINT('Ctrl Pts',(-1.17812502949243,-0.447134449431192,
0.695578066965848));
#370180=CARTESIAN_POINT('Ctrl Pts',(-1.22547236411816,-0.293439875093998,
0.686356392505617));
#370181=CARTESIAN_POINT('Ctrl Pts',(-1.260570321567,0.0295639601923402,
0.666976162388436));
#370182=CARTESIAN_POINT('Ctrl Pts',(-1.24557820086212,0.196094352339869,
0.656984338859585));
#370183=CARTESIAN_POINT('Ctrl Pts',(-1.15280253655963,0.509447233287784,
0.63818316600271));
#370184=CARTESIAN_POINT('Ctrl Pts',(-1.07758131698412,0.653686233007904,
0.630132180718844));
#370185=CARTESIAN_POINT('Ctrl Pts',(-0.876460055967045,0.905711828286041,
0.612120845583583));
#370186=CARTESIAN_POINT('Ctrl Pts',(-0.752463932383305,1.01107975625542,
0.602516780164843));
#370187=CARTESIAN_POINT('Ctrl Pts',(-0.467364233531721,1.17113014174595,
0.582901053691121));
#370188=CARTESIAN_POINT('Ctrl Pts',(-0.30810016347818,1.22272822250969,
0.573077507433621));
#370189=CARTESIAN_POINT('Ctrl Pts',(-0.0957032265067624,1.24725522245179,
0.561305228849163));
#370190=CARTESIAN_POINT('Ctrl Pts',(-0.0478281484139007,1.25,0.558735223492522));
#370191=CARTESIAN_POINT('Ctrl Pts',(-1.94865532267534E-13,1.25000000000001,
0.556249999999987));
#370192=CARTESIAN_POINT('Ctrl Pts',(0.,1.25000000000001,0.499999999999989));
#370193=CARTESIAN_POINT('Ctrl Pts',(-0.0862682746159715,1.25000000000001,
0.504482631041474));
#370194=CARTESIAN_POINT('Ctrl Pts',(-0.172487434489133,1.24107165734585,
0.50923056028556));
#370195=CARTESIAN_POINT('Ctrl Pts',(-0.419792968061261,1.18905309932987,
0.523641489500238));
#370196=CARTESIAN_POINT('Ctrl Pts',(-0.57384815019037,1.12283710963577,
0.53363291126957));
#370197=CARTESIAN_POINT('Ctrl Pts',(-0.841898962499962,0.937672385738494,
0.553116181764401));
#370198=CARTESIAN_POINT('Ctrl Pts',(-0.954750036912509,0.822491771888897,
0.562435514017028));
#370199=CARTESIAN_POINT('Ctrl Pts',(-1.13409880660983,0.551095765076556,
0.579896629663123));
#370200=CARTESIAN_POINT('Ctrl Pts',(-1.19703032424223,0.396265274860239,
0.588724083508252));
#370201=CARTESIAN_POINT('Ctrl Pts',(-1.25861872515985,0.0725526675554756,
0.608146839946541));
#370202=CARTESIAN_POINT('Ctrl Pts',(-1.25727402968328,-0.0929923270629792,
0.61807953962365));
#370203=CARTESIAN_POINT('Ctrl Pts',(-1.19189731845674,-0.408596573876534,
0.637015794432467));
#370204=CARTESIAN_POINT('Ctrl Pts',(-1.13062717708045,-0.556087186048838,
0.645433504127685));
#370205=CARTESIAN_POINT('Ctrl Pts',(-0.952221908809357,-0.826589841779339,
0.662818793469107));
#370206=CARTESIAN_POINT('Ctrl Pts',(-0.834354752304146,-0.945415787489115,
0.672508128948723));
#370207=CARTESIAN_POINT('Ctrl Pts',(-0.56223060675814,-1.12812288180903,
0.692129327159882));
#370208=CARTESIAN_POINT('Ctrl Pts',(-0.411376867902615,-1.19144538062551,
0.701867592330662));
#370209=CARTESIAN_POINT('Ctrl Pts',(-0.0963557838829768,-1.25645451633575,
0.720186842091296));
#370210=CARTESIAN_POINT('Ctrl Pts',(0.064621031364767,-1.25848548666364,
0.728103242686795));
#370211=CARTESIAN_POINT('Ctrl Pts',(0.385555073851676,-1.20065867985365,
0.746514268915072));
#370212=CARTESIAN_POINT('Ctrl Pts',(0.541891884231855,-1.13867314532483,
0.75649733391109));
#370213=CARTESIAN_POINT('Ctrl Pts',(0.815765074426867,-0.960566583942252,
0.776071399160033));
#370214=CARTESIAN_POINT('Ctrl Pts',(0.932044640374465,-0.848215269769055,
0.78548400206833));
#370215=CARTESIAN_POINT('Ctrl Pts',(1.11801415160888,-0.582614236382718,
0.803115292333425));
#370216=CARTESIAN_POINT('Ctrl Pts',(1.18472836351054,-0.431076105084149,
0.81163543369482));
#370217=CARTESIAN_POINT('Ctrl Pts',(1.25592957878956,-0.110393178259806,
0.830876409304284));
#370218=CARTESIAN_POINT('Ctrl Pts',(1.25954389228496,0.0556182878332724,
0.84083709726987));
#370219=CARTESIAN_POINT('Ctrl Pts',(1.20333352798253,0.37364868035265,0.859918920821036));
#370220=CARTESIAN_POINT('Ctrl Pts',(1.14631880003878,0.523017439510358,
0.868626051085022));
#370221=CARTESIAN_POINT('Ctrl Pts',(0.975758416920615,0.798664048580137,
0.88575802683669));
#370222=CARTESIAN_POINT('Ctrl Pts',(0.861403046258177,0.920832937256386,
0.89536517286015));
#370223=CARTESIAN_POINT('Ctrl Pts',(0.594348557227779,1.11160334448386,
0.914964843378677));
#370224=CARTESIAN_POINT('Ctrl Pts',(0.444934762586208,1.17938625870543,
0.924762099315452));
#370225=CARTESIAN_POINT('Ctrl Pts',(0.19254863413642,1.23886551112042,0.939660844815923));
#370226=CARTESIAN_POINT('Ctrl Pts',(0.0963410370308149,1.25000000000001,
0.944993972870252));
#370227=CARTESIAN_POINT('Ctrl Pts',(-5.98933296121097E-14,1.25000000000001,
0.949999999999993));
#370228=CARTESIAN_POINT('Origin',(0.,0.,2.95));
#370229=CARTESIAN_POINT('',(9.03658428620226E-9,1.25000000000001,1.45624999906087));
#370230=CARTESIAN_POINT('',(-1.20004646332587E-13,1.25000000000001,1.4));
#370231=CARTESIAN_POINT('',(-1.5308084989342E-16,1.25000000000001,2.95));
#370232=CARTESIAN_POINT('Ctrl Pts',(1.80731740684337E-8,1.25000000000001,
1.45624999906087));
#370233=CARTESIAN_POINT('Ctrl Pts',(0.157398679770193,1.24999999772425,
1.44807132461952));
#370234=CARTESIAN_POINT('Ctrl Pts',(0.313475064425583,1.22026998729107,
1.43906945746397));
#370235=CARTESIAN_POINT('Ctrl Pts',(0.613327249792887,1.10160244908175,
1.41992865472319));
#370236=CARTESIAN_POINT('Ctrl Pts',(0.753163918005052,1.01116072139918,
1.40994927646958));
#370237=CARTESIAN_POINT('Ctrl Pts',(0.988083053645535,0.782735539991384,
1.39088976466936));
#370238=CARTESIAN_POINT('Ctrl Pts',(1.08146010550208,0.64762610461839,1.38260756627708));
#370239=CARTESIAN_POINT('Ctrl Pts',(1.21039467654472,0.351076002414244,
1.36481456014483));
#370240=CARTESIAN_POINT('Ctrl Pts',(1.24544270847957,0.192790124873009,
1.35531740749235));
#370241=CARTESIAN_POINT('Ctrl Pts',(1.2538900214955,-0.134683444613013,
1.33566899332319));
#370242=CARTESIAN_POINT('Ctrl Pts',(1.22470822614229,-0.300802691914751,
1.32570183848509));
#370243=CARTESIAN_POINT('Ctrl Pts',(1.10570570688357,-0.604313394287262,
1.30749119634274));
#370244=CARTESIAN_POINT('Ctrl Pts',(1.01997583690477,-0.739886435954298,
1.29955290608169));
#370245=CARTESIAN_POINT('Ctrl Pts',(0.799848460765771,-0.974246553231572,
1.28108394857509));
#370246=CARTESIAN_POINT('Ctrl Pts',(0.666545352774837,-1.06987122986475,
1.27128857560068));
#370247=CARTESIAN_POINT('Ctrl Pts',(0.367953555362538,-1.20605101944918,
1.2516878969979));
#370248=CARTESIAN_POINT('Ctrl Pts',(0.205010971191739,-1.2441621947968,
1.24207781670246));
#370249=CARTESIAN_POINT('Ctrl Pts',(-0.118969573749707,-1.25436750783854,
1.22493713437614));
#370250=CARTESIAN_POINT('Ctrl Pts',(-0.276850276553407,-1.22921762208352,
1.21624096631008));
#370251=CARTESIAN_POINT('Ctrl Pts',(-0.580464475410518,-1.11919602198872,
1.19716406175764));
#370252=CARTESIAN_POINT('Ctrl Pts',(-0.72250095688813,-1.03321468577995,
1.18720418959795));
#370253=CARTESIAN_POINT('Ctrl Pts',(-0.964875735814266,-0.811442469879943,
1.16795686017375));
#370254=CARTESIAN_POINT('Ctrl Pts',(-1.06291611579921,-0.677952986670806,
1.15942717920022));
#370255=CARTESIAN_POINT('Ctrl Pts',(-1.20023579293853,-0.384194857888461,
1.14180169147328));
#370256=CARTESIAN_POINT('Ctrl Pts',(-1.23953981270102,-0.227369990182164,
1.1323921994109));
#370257=CARTESIAN_POINT('Ctrl Pts',(-1.25716076480177,0.0988162526587568,
1.11282102484045));
#370258=CARTESIAN_POINT('Ctrl Pts',(-1.23283951488155,0.265207716207856,
1.1028375370275));
#370259=CARTESIAN_POINT('Ctrl Pts',(-1.12275777229388,0.572174767427489,
1.08441951395433));
#370260=CARTESIAN_POINT('Ctrl Pts',(-1.04063341076924,0.710669974097316,
1.07650279896224));
#370261=CARTESIAN_POINT('Ctrl Pts',(-0.827046213520172,0.951190122724477,
1.05818887817897));
#370262=CARTESIAN_POINT('Ctrl Pts',(-0.696888708734302,1.05028835281727,
1.04845274893792));
#370263=CARTESIAN_POINT('Ctrl Pts',(-0.402752868975319,1.19488464689099,
1.02883111355203));
#370264=CARTESIAN_POINT('Ctrl Pts',(-0.240954146332926,1.23770703193248,
1.01913913375429));
#370265=CARTESIAN_POINT('Ctrl Pts',(-0.0503287006321313,1.24924080334692,
1.00888793189678));
#370266=CARTESIAN_POINT('Ctrl Pts',(-0.0251530851071151,1.25,1.00755699264116));
#370267=CARTESIAN_POINT('Ctrl Pts',(-1.64814777738108E-13,1.25000000000001,
1.00624999999999));
#370268=CARTESIAN_POINT('Ctrl Pts',(-5.98933296121097E-14,1.25000000000001,
0.949999999999993));
#370269=CARTESIAN_POINT('Ctrl Pts',(-0.0619569747754295,1.25,0.953219378845819));
#370270=CARTESIAN_POINT('Ctrl Pts',(-0.123954635380717,1.24539432313515,
0.956579042095208));
#370271=CARTESIAN_POINT('Ctrl Pts',(-0.350667273950477,1.21137547504059,
0.969379941799671));
#370272=CARTESIAN_POINT('Ctrl Pts',(-0.509193775382237,1.15373611528708,
0.979346401237057));
#370273=CARTESIAN_POINT('Ctrl Pts',(-0.788759858261056,0.982933458839484,
0.998997160719062));
#370274=CARTESIAN_POINT('Ctrl Pts',(-0.908428770459634,0.873539624078199,
1.00849715484233));
#370275=CARTESIAN_POINT('Ctrl Pts',(-1.10100341662785,0.613802400120149,
1.02629574370347));
#370276=CARTESIAN_POINT('Ctrl Pts',(-1.17144786116564,0.465488112493403,
1.03457071325027));
#370277=CARTESIAN_POINT('Ctrl Pts',(-1.25212704344905,0.147936500855631,
1.05362380994854));
#370278=CARTESIAN_POINT('Ctrl Pts',(-1.26070031217406,-0.018394865215165,
1.06360369191278));
#370279=CARTESIAN_POINT('Ctrl Pts',(-1.21366305072875,-0.338764412054756,
1.08282586472316));
#370280=CARTESIAN_POINT('Ctrl Pts',(-1.1608401142715,-0.490044425954557,
1.09188231105704));
#370281=CARTESIAN_POINT('Ctrl Pts',(-0.998019036056536,-0.770660115022403,
1.10876121312942));
#370282=CARTESIAN_POINT('Ctrl Pts',(-0.887198313757397,-0.896000136205884,
1.11827982741153));
#370283=CARTESIAN_POINT('Ctrl Pts',(-0.625343945649038,-1.09453322689978,
1.13784217222478));
#370284=CARTESIAN_POINT('Ctrl Pts',(-0.477466739633206,-1.1666569241532,
1.1476898081654));
#370285=CARTESIAN_POINT('Ctrl Pts',(-0.166600317335141,-1.2489582898092,
1.16631194226871));
#370286=CARTESIAN_POINT('Ctrl Pts',(-0.00700038512510649,-1.25999897012053,
1.17433628021498));
#370287=CARTESIAN_POINT('Ctrl Pts',(0.316712794779445,-1.22075857074284,
1.19233412243654));
#370288=CARTESIAN_POINT('Ctrl Pts',(0.477242499509596,-1.16738309297785,
1.20227675491099));
#370289=CARTESIAN_POINT('Ctrl Pts',(0.762122401229375,-1.00379534756186,
1.22198718118849));
#370290=CARTESIAN_POINT('Ctrl Pts',(0.884991537089302,-0.897350601019584,
1.23156499116451));
#370291=CARTESIAN_POINT('Ctrl Pts',(1.08387274485231,-0.643290066836535,
1.24952097788549));
#370292=CARTESIAN_POINT('Ctrl Pts',(1.15784644294826,-0.497993728927597,
1.25762037626422));
#370293=CARTESIAN_POINT('Ctrl Pts',(1.24746989975567,-0.183525205164368,
1.27648848769002));
#370294=CARTESIAN_POINT('Ctrl Pts',(1.26078035155956,-0.0170236310731421,
1.28647858213549));
#370295=CARTESIAN_POINT('Ctrl Pts',(1.22255037515762,0.305306571018055,
1.30581839426096));
#370296=CARTESIAN_POINT('Ctrl Pts',(1.17377081609769,0.458391081837177,
1.31500346491011));
#370297=CARTESIAN_POINT('Ctrl Pts',(1.01827339415832,0.743683533882543,
1.33212101203284));
#370298=CARTESIAN_POINT('Ctrl Pts',(0.910830807860765,0.871991864572587,
1.34133159884764));
#370299=CARTESIAN_POINT('Ctrl Pts',(0.653915268472853,1.07777105236075,
1.3608546975055));
#370300=CARTESIAN_POINT('Ctrl Pts',(0.507588766855547,1.15392907768717,
1.37074278632415));
#370301=CARTESIAN_POINT('Ctrl Pts',(0.236607028428954,1.23315076943472,
1.38720006124292));
#370302=CARTESIAN_POINT('Ctrl Pts',(0.118514754763226,1.25000000000003,
1.3938417926991));
#370303=CARTESIAN_POINT('Ctrl Pts',(-2.40987785282698E-13,1.25000000000001,
1.4));
#370304=CARTESIAN_POINT('Origin',(0.,0.,2.95));
#370305=CARTESIAN_POINT('',(6.739087296494E-14,1.25000000000001,1.90624999999997));
#370306=CARTESIAN_POINT('',(-2.25372062308248E-14,1.25000000000001,1.84999999999999));
#370307=CARTESIAN_POINT('',(-1.5308084989342E-16,1.25000000000001,2.95));
#370308=CARTESIAN_POINT('Ctrl Pts',(1.34934826779773E-13,1.25000000000001,
1.90624999999997));
#370309=CARTESIAN_POINT('Ctrl Pts',(0.0220641490125112,1.25000000000001,
1.90510351318651));
#370310=CARTESIAN_POINT('Ctrl Pts',(0.0441478634863414,1.2494158173731,
1.90393848424304));
#370311=CARTESIAN_POINT('Ctrl Pts',(0.225701489980945,1.23978309581366,
1.89421569943465));
#370312=CARTESIAN_POINT('Ctrl Pts',(0.382056259725138,1.20084092933029,
1.88492300228407));
#370313=CARTESIAN_POINT('Ctrl Pts',(0.67727119970412,1.06363791754484,1.86546709367459));
#370314=CARTESIAN_POINT('Ctrl Pts',(0.812311756712525,0.964458122179201,
1.855474786639));
#370315=CARTESIAN_POINT('Ctrl Pts',(1.03217352987493,0.723114940154323,
1.83681013832547));
#370316=CARTESIAN_POINT('Ctrl Pts',(1.11640454143149,0.584736554500829,
1.82883419327002));
#370317=CARTESIAN_POINT('Ctrl Pts',(1.22827946254893,0.282706754242194,
1.8107124052545));
#370318=CARTESIAN_POINT('Ctrl Pts',(1.25449128915545,0.121796612551182,
1.80105779675304));
#370319=CARTESIAN_POINT('Ctrl Pts',(1.24411798257265,-0.205281189536293,
1.78143312862779));
#370320=CARTESIAN_POINT('Ctrl Pts',(1.20596811453433,-0.368275711837578,
1.77165345728971));
#370321=CARTESIAN_POINT('Ctrl Pts',(1.0713587670456,-0.663149287941581,
1.75396104272347));
#370322=CARTESIAN_POINT('Ctrl Pts',(0.978830643778726,-0.793396141507814,
1.74580964796564));
#370323=CARTESIAN_POINT('Ctrl Pts',(0.746401283578218,-1.01591304971401,
1.72705675688831));
#370324=CARTESIAN_POINT('Ctrl Pts',(0.607371161633192,-1.1046679867251,
1.71716989172824));
#370325=CARTESIAN_POINT('Ctrl Pts',(0.300822031326495,-1.22453593311983,
1.69764509327518));
#370326=CARTESIAN_POINT('Ctrl Pts',(0.136009461171029,-1.25357347005352,
1.68842446301332));
#370327=CARTESIAN_POINT('Ctrl Pts',(-0.188800153321568,-1.24587736713163,
1.67131597727303));
#370328=CARTESIAN_POINT('Ctrl Pts',(-0.345781658244665,-1.21172279151361,
1.66213434173322));
#370329=CARTESIAN_POINT('Ctrl Pts',(-0.644132371049383,-1.08394895107769,
1.64279836872858));
#370330=CARTESIAN_POINT('Ctrl Pts',(-0.781746628810574,-0.98930770402191,
1.63280848472826));
#370331=CARTESIAN_POINT('Ctrl Pts',(-1.00950805411895,-0.754659338831184,
1.61393420295339));
#370332=CARTESIAN_POINT('Ctrl Pts',(-1.09849457327402,-0.617999115840741,
1.60582994695041));
#370333=CARTESIAN_POINT('Ctrl Pts',(-1.21934347855459,-0.318818391258399,
1.58787910347547));
#370334=CARTESIAN_POINT('Ctrl Pts',(-1.25023084516112,-0.159229393009295,
1.57830376358053));
#370335=CARTESIAN_POINT('Ctrl Pts',(-1.24975730886918,0.169248596871773,
1.55859508418767));
#370336=CARTESIAN_POINT('Ctrl Pts',(-1.21587226015212,0.33497431489362,
1.54865154110635));
#370337=CARTESIAN_POINT('Ctrl Pts',(-1.08828181784335,0.635053139877062,
1.53064681160735));
#370338=CARTESIAN_POINT('Ctrl Pts',(-0.999036985526338,0.767841680002532,
1.52262623412706));
#370339=CARTESIAN_POINT('Ctrl Pts',(-0.772539813423395,0.996112588657923,
1.50400896857181));
#370340=CARTESIAN_POINT('Ctrl Pts',(-0.636238448456786,1.08823425591884,
1.49416289187609));
#370341=CARTESIAN_POINT('Ctrl Pts',(-0.333510092793093,1.21602159134482,
1.47459904502627));
#370342=CARTESIAN_POINT('Ctrl Pts',(-0.169582503259977,1.24948034391829,
1.46507735503405));
#370343=CARTESIAN_POINT('Ctrl Pts',(-0.00258301669098132,1.24999799854518,
1.45638427752798));
#370344=CARTESIAN_POINT('Ctrl Pts',(-0.0012914578997066,1.25000000001868,
1.45631710612148));
#370345=CARTESIAN_POINT('Ctrl Pts',(1.80731730328256E-8,1.25000000000001,
1.45624999906087));
#370346=CARTESIAN_POINT('Ctrl Pts',(-2.39856211815281E-13,1.25000000000001,
1.4));
#370347=CARTESIAN_POINT('Ctrl Pts',(-0.0393195961679156,1.25,1.40204310614887));
#370348=CARTESIAN_POINT('Ctrl Pts',(-0.0786799031302476,1.24814487831034,
1.40414398134325));
#370349=CARTESIAN_POINT('Ctrl Pts',(-0.28300112969979,1.22877836477191,
1.4153418191139));
#370350=CARTESIAN_POINT('Ctrl Pts',(-0.443274061016728,1.18045660176147,
1.42511949780779));
#370351=CARTESIAN_POINT('Ctrl Pts',(-0.731861214538178,1.02614144341748,
1.44474438092743));
#370352=CARTESIAN_POINT('Ctrl Pts',(-0.858204404807066,0.923083411825348,
1.45440110661728));
#370353=CARTESIAN_POINT('Ctrl Pts',(-1.06402745181118,0.675361376603991,
1.47252764691732));
#370354=CARTESIAN_POINT('Ctrl Pts',(-1.14185924872533,0.533316303320672,
1.48050102180064));
#370355=CARTESIAN_POINT('Ctrl Pts',(-1.241209262208,0.222338201800774,1.49915970789184));
#370356=CARTESIAN_POINT('Ctrl Pts',(-1.25972732850135,0.0558009014966325,
1.50915194591009));
#370357=CARTESIAN_POINT('Ctrl Pts',(-1.23121454592064,-0.268515991300665,
1.52861095947793));
#370358=CARTESIAN_POINT('Ctrl Pts',(-1.18688771354205,-0.423444179144705,
1.53790665074857));
#370359=CARTESIAN_POINT('Ctrl Pts',(-1.03949924511053,-0.713762554541242,
1.55532575327237));
#370360=CARTESIAN_POINT('Ctrl Pts',(-0.93570609504241,-0.845277099607941,
1.56423759806116));
#370361=CARTESIAN_POINT('Ctrl Pts',(-0.684345802550768,-1.05878074353627,
1.58370377130704));
#370362=CARTESIAN_POINT('Ctrl Pts',(-0.539820130271814,-1.139272204496,
1.59362828935739));
#370363=CARTESIAN_POINT('Ctrl Pts',(-0.233215705057647,-1.23821515466295,
1.61252821113129));
#370364=CARTESIAN_POINT('Ctrl Pts',(-0.0747178744562011,-1.25776237786808,
1.62088467402009));
#370365=CARTESIAN_POINT('Ctrl Pts',(0.248600826170604,-1.23619451214554,
1.63833184248745));
#370366=CARTESIAN_POINT('Ctrl Pts',(0.410137222062212,-1.19237103518111,
1.64804022414506));
#370367=CARTESIAN_POINT('Ctrl Pts',(0.703291087901194,-1.04599702234766,
1.66766416623212));
#370368=CARTESIAN_POINT('Ctrl Pts',(0.832765775709602,-0.946170315616422,
1.6773866695614));
#370369=CARTESIAN_POINT('Ctrl Pts',(1.04495034516535,-0.704340870465485,
1.69566698656232));
#370370=CARTESIAN_POINT('Ctrl Pts',(1.12630111160027,-0.565210360485072,
1.70358737837078));
#370371=CARTESIAN_POINT('Ctrl Pts',(1.23445580820926,-0.257511520102835,
1.72204930879372));
#370372=CARTESIAN_POINT('Ctrl Pts',(1.25773119996678,-0.09107935617977,
1.7320352386291));
#370373=CARTESIAN_POINT('Ctrl Pts',(1.2381423983534,0.234796739196575,1.75158780435168));
#370374=CARTESIAN_POINT('Ctrl Pts',(1.19792844216626,0.391292042360348,
1.76097752254151));
#370375=CARTESIAN_POINT('Ctrl Pts',(1.05879936094225,0.684439091728722,
1.77856634550362));
#370376=CARTESIAN_POINT('Ctrl Pts',(0.959737623783481,0.817576508230252,
1.78715786545694));
#370377=CARTESIAN_POINT('Ctrl Pts',(0.715750379695562,1.03788568616187,
1.80644508988966));
#370378=CARTESIAN_POINT('Ctrl Pts',(0.573253984920157,1.12289098212861,
1.81639957863806));
#370379=CARTESIAN_POINT('Ctrl Pts',(0.28392458895852,1.22566437795554,1.83451677693073));
#370380=CARTESIAN_POINT('Ctrl Pts',(0.142419898735792,1.25000000000001,
1.84259964498141));
#370381=CARTESIAN_POINT('Ctrl Pts',(-4.44783099240453E-14,1.25000000000001,
1.84999999999999));
#370382=CARTESIAN_POINT('Origin',(0.,0.,2.95));
#370383=CARTESIAN_POINT('',(1.34858286354831E-13,1.25000000000001,2.35624999999996));
#370384=CARTESIAN_POINT('',(-7.654042494671E-17,1.25000000000001,2.29999999999999));
#370385=CARTESIAN_POINT('',(-1.5308084989342E-16,1.25000000000001,2.95));
#370386=CARTESIAN_POINT('Ctrl Pts',(2.69869653559555E-13,1.25000000000001,
2.35624999999996));
#370387=CARTESIAN_POINT('Ctrl Pts',(0.044433163138449,1.25000000000001,
2.35394118511707));
#370388=CARTESIAN_POINT('Ctrl Pts',(0.0889145499349906,1.24763102082333,
2.35155879508408));
#370389=CARTESIAN_POINT('Ctrl Pts',(0.292891387862558,1.2257611260194,2.34030375083423));
#370390=CARTESIAN_POINT('Ctrl Pts',(0.44771822940789,1.17805333018664,2.33082747828129));
#370391=CARTESIAN_POINT('Ctrl Pts',(0.736417365076694,1.02373303828326,
2.3111966223918));
#370392=CARTESIAN_POINT('Ctrl Pts',(0.866355583473318,0.916395130127912,
2.3012246972639));
#370393=CARTESIAN_POINT('Ctrl Pts',(1.07153750812881,0.663044844477098,
2.28296262314544));
#370394=CARTESIAN_POINT('Ctrl Pts',(1.14714353414279,0.521425998584306,
2.27503555991502));
#370395=CARTESIAN_POINT('Ctrl Pts',(1.24216677553308,0.214241724025496,
2.2566045034415));
#370396=CARTESIAN_POINT('Ctrl Pts',(1.25946313075807,0.0512174419276202,
2.24682304651562));
#370397=CARTESIAN_POINT('Ctrl Pts',(1.23045164409321,-0.275572672931196,
2.2272156396241));
#370398=CARTESIAN_POINT('Ctrl Pts',(1.18312992230814,-0.436090455363154,
2.21758457267818));
#370399=CARTESIAN_POINT('Ctrl Pts',(1.0320420154748,-0.72281761118703,2.20038094332875));
#370400=CARTESIAN_POINT('Ctrl Pts',(0.932253777922101,-0.847647473052605,
2.19176190307566));
#370401=CARTESIAN_POINT('Ctrl Pts',(0.686820365306802,-1.05724974831533,
2.17272074060204));
#370402=CARTESIAN_POINT('Ctrl Pts',(0.542046066061274,-1.13828215032821,
2.16276707528395));
#370403=CARTESIAN_POINT('Ctrl Pts',(0.22932722660143,-1.23973872013907,
2.14347403063677));
#370404=CARTESIAN_POINT('Ctrl Pts',(0.0644657010172478,-1.25911568572811,
2.13487320665703));
#370405=CARTESIAN_POINT('Ctrl Pts',(-0.259026376116058,-1.23330572766472,
2.1172897665119));
#370406=CARTESIAN_POINT('Ctrl Pts',(-0.414686589460496,-1.1900238484095,
2.10790296818736));
#370407=CARTESIAN_POINT('Ctrl Pts',(-0.706801671398365,-1.04432253623698,
2.08835318391498));
#370408=CARTESIAN_POINT('Ctrl Pts',(-0.839379654808393,-0.941079165393031,
2.07836692869273));
#370409=CARTESIAN_POINT('Ctrl Pts',(-1.05201080633447,-0.69375603870744,
2.05989859616071));
#370410=CARTESIAN_POINT('Ctrl Pts',(-1.13196320875619,-0.553790353984001,
2.05197742123901));
#370411=CARTESIAN_POINT('Ctrl Pts',(-1.23556938761572,-0.249200461310902,
2.03370202767862));
#370412=CARTESIAN_POINT('Ctrl Pts',(-1.25742635352416,-0.0871923884049848,
2.02398154330427));
#370413=CARTESIAN_POINT('Ctrl Pts',(-1.23790957988289,0.239877866056647,
2.00435732803657));
#370414=CARTESIAN_POINT('Ctrl Pts',(-1.19523956098039,0.401723623453222,
1.99464658259278));
#370415=CARTESIAN_POINT('Ctrl Pts',(-1.05252064112392,0.692639357327156,
1.97719163856034));
#370416=CARTESIAN_POINT('Ctrl Pts',(-0.956458771175397,0.820215036291892,
1.96884260452183));
#370417=CARTESIAN_POINT('Ctrl Pts',(-0.717676298548484,1.03647614944333,
1.94994726989089));
#370418=CARTESIAN_POINT('Ctrl Pts',(-0.575797232204222,1.12151614880628,
1.94002381736684));
#370419=CARTESIAN_POINT('Ctrl Pts',(-0.286113450961956,1.22529191614851,
1.92185813352936));
#370420=CARTESIAN_POINT('Ctrl Pts',(-0.143508577417465,1.25000000000001,
1.91370692442225));
#370421=CARTESIAN_POINT('Ctrl Pts',(1.34441069388203E-13,1.25000000000001,
1.90624999999997));
#370422=CARTESIAN_POINT('Ctrl Pts',(-4.49213316117562E-14,1.25000000000001,
1.84999999999999));
#370423=CARTESIAN_POINT('Ctrl Pts',(-0.0157044861541279,1.25000000000001,
1.85081602903776));
#370424=CARTESIAN_POINT('Ctrl Pts',(-0.0314191927020232,1.24970404498241,
1.8516414677932));
#370425=CARTESIAN_POINT('Ctrl Pts',(-0.212761819155421,1.2428609839098,
1.86126959890323));
#370426=CARTESIAN_POINT('Ctrl Pts',(-0.375470118394336,1.20373310983395,
1.87089800635836));
#370427=CARTESIAN_POINT('Ctrl Pts',(-0.6731232162385,1.06572999251169,1.89050460853292));
#370428=CARTESIAN_POINT('Ctrl Pts',(-0.805756883777148,0.969349409244335,
1.90028787356008));
#370429=CARTESIAN_POINT('Ctrl Pts',(-1.02448095042294,0.733659818577383,
1.91872379716814));
#370430=CARTESIAN_POINT('Ctrl Pts',(-1.10943718024133,0.597465274702968,
1.92665208351771));
#370431=CARTESIAN_POINT('Ctrl Pts',(-1.22653449491264,0.293207005417949,
1.94490757967481));
#370432=CARTESIAN_POINT('Ctrl Pts',(-1.25467582129209,0.127017989629909,
1.9548789206221));
#370433=CARTESIAN_POINT('Ctrl Pts',(-1.24426086020019,-0.200201328686394,
1.97451207972108));
#370434=CARTESIAN_POINT('Ctrl Pts',(-1.20829802228421,-0.358184229595967,
1.98399105377565));
#370435=CARTESIAN_POINT('Ctrl Pts',(-1.07757143364063,-0.65414313490744,
2.00174858809434));
#370436=CARTESIAN_POINT('Ctrl Pts',(-0.983207316756803,-0.788907683287219,
2.01007827968862));
#370437=CARTESIAN_POINT('Ctrl Pts',(-0.746697357985156,-1.01592835213342,
2.02917831770666));
#370438=CARTESIAN_POINT('Ctrl Pts',(-0.60638131509394,-1.10542566430186,
2.03915427253386));
#370439=CARTESIAN_POINT('Ctrl Pts',(-0.304774524172768,-1.2226275299057,
2.05834227707547));
#370440=CARTESIAN_POINT('Ctrl Pts',(-0.147247229315901,-1.2513920043842,
2.0673070493949));
#370441=CARTESIAN_POINT('Ctrl Pts',(0.177085201866623,-1.24843996704571,
2.08424841799557));
#370442=CARTESIAN_POINT('Ctrl Pts',(0.340815911920561,-1.21399527196157,
2.09378945610528));
#370443=CARTESIAN_POINT('Ctrl Pts',(0.642689307430307,-1.08442272513257,
2.11336243426444));
#370444=CARTESIAN_POINT('Ctrl Pts',(0.778364150743864,-0.991552687290698,
2.12319840705753));
#370445=CARTESIAN_POINT('Ctrl Pts',(1.0035182001428,-0.761990269780845,
2.1417846271755));
#370446=CARTESIAN_POINT('Ctrl Pts',(1.09202120709043,-0.628619487024861,
2.1497828307784));
#370447=CARTESIAN_POINT('Ctrl Pts',(1.2178089173922,-0.327811906339744,
2.16783128561951));
#370448=CARTESIAN_POINT('Ctrl Pts',(1.25070509520255,-0.161992817094826,
2.17778043097421));
#370449=CARTESIAN_POINT('Ctrl Pts',(1.24929940706568,0.166293693894003,
2.19747762163354));
#370450=CARTESIAN_POINT('Ctrl Pts',(1.21753379203214,0.325617743326955,
2.20703706459952));
#370451=CARTESIAN_POINT('Ctrl Pts',(1.09498652619744,0.624250917867314,
2.22495505507194));
#370452=CARTESIAN_POINT('Ctrl Pts',(1.00508626477818,0.760585901245542,
2.2330917627397));
#370453=CARTESIAN_POINT('Ctrl Pts',(0.775824314847745,0.993942399079391,
2.25200525804037));
#370454=CARTESIAN_POINT('Ctrl Pts',(0.637735382131881,1.08771006731678,
2.2619935995103));
#370455=CARTESIAN_POINT('Ctrl Pts',(0.338819367231804,1.21367630871059,
2.2813047185022));
#370456=CARTESIAN_POINT('Ctrl Pts',(0.181734697085463,1.24691633605466,
2.29046427821604));
#370457=CARTESIAN_POINT('Ctrl Pts',(0.0150734947248369,1.24993186207365,
2.29921471410078));
#370458=CARTESIAN_POINT('Ctrl Pts',(0.00753536179884883,1.25000000000001,
2.29960845111532));
#370459=CARTESIAN_POINT('Ctrl Pts',(0.,1.25000000000001,2.29999999999999));
#370460=CARTESIAN_POINT('Origin',(0.,-9.76875228502569E-17,-3.6625));
#370461=CARTESIAN_POINT('',(-0.155365792422873,-0.945030276552907,-3.95478357377727));
#370462=CARTESIAN_POINT('Origin',(-4.58730275987307E-13,1.7608137170555E-12,
-3.95478357377551));
#370463=CARTESIAN_POINT('Ctrl Pts',(-0.155365792422871,-0.945030276552904,
-3.95478357377728));
#370464=CARTESIAN_POINT('Ctrl Pts',(-0.0279053867386288,-0.989345562927712,
-3.93173259563576));
#370465=CARTESIAN_POINT('Ctrl Pts',(0.0908406055947738,-0.997960828573256,
-3.91446248497396));
#370466=CARTESIAN_POINT('Ctrl Pts',(0.2939266609703,-0.994471102906672,
-3.88139632958021));
#370467=CARTESIAN_POINT('Ctrl Pts',(0.404737306683732,-0.974830092903115,
-3.86277453676972));
#370468=CARTESIAN_POINT('Ctrl Pts',(0.634402236959834,-0.895212934293821,
-3.82294769474439));
#370469=CARTESIAN_POINT('Ctrl Pts',(0.749402513368721,-0.829536503600064,
-3.80217950070126));
#370470=CARTESIAN_POINT('Ctrl Pts',(0.984142487761137,-0.630335856567594,
-3.75689034668222));
#370471=CARTESIAN_POINT('Ctrl Pts',(1.06926532203318,-0.500451973862013,
-3.73786753572628));
#370472=CARTESIAN_POINT('Ctrl Pts',(1.18794310478873,-0.270780370964604,
-3.7018818371992));
#370473=CARTESIAN_POINT('Ctrl Pts',(1.23047313162925,-0.137550427674414,
-3.68202686837076));
#370474=CARTESIAN_POINT('Ctrl Pts',(1.24999999999999,-1.42247325030098E-15,
-3.66250000000002));
#370475=CARTESIAN_POINT('',(-2.5977107395931E-13,1.07169464481439,-3.84080535518562));
#370476=CARTESIAN_POINT('Ctrl Pts',(0.875786586620195,-0.891906864368513,
-3.6624999999954));
#370477=CARTESIAN_POINT('Ctrl Pts',(0.803162978577988,-0.958147518332696,
-3.66611783025492));
#370478=CARTESIAN_POINT('Ctrl Pts',(0.7229160327686,-1.01549113836917,-3.66984833805803));
#370479=CARTESIAN_POINT('Ctrl Pts',(0.551640702174221,-1.10937740583169,
-3.67733818712611));
#370480=CARTESIAN_POINT('Ctrl Pts',(0.46136363988503,-1.14584661025103,
-3.68107032221587));
#370481=CARTESIAN_POINT('Ctrl Pts',(0.220775486284481,-1.21150525514029,
-3.69049017126946));
#370482=CARTESIAN_POINT('Ctrl Pts',(0.0667413551172497,-1.22437521577925,
-3.69573027211842));
#370483=CARTESIAN_POINT('Ctrl Pts',(-0.240687585667333,-1.19202036778278,
-3.70662761066056));
#370484=CARTESIAN_POINT('Ctrl Pts',(-0.392307468273431,-1.14470527425269,
-3.71268458241303));
#370485=CARTESIAN_POINT('Ctrl Pts',(-0.662432154086964,-0.997083129168331,
-3.72491348355897));
#370486=CARTESIAN_POINT('Ctrl Pts',(-0.779641139378463,-0.900461687408625,
-3.73095969955023));
#370487=CARTESIAN_POINT('Ctrl Pts',(-0.945919539367262,-0.699864947625556,
-3.74096526360374));
#370488=CARTESIAN_POINT('Ctrl Pts',(-1.03886893322305,-0.56454169648239,
-3.74641423599297));
#370489=CARTESIAN_POINT('Ctrl Pts',(-1.13927032774389,-0.231646122171666,
-3.75989697957764));
#370490=CARTESIAN_POINT('Ctrl Pts',(-1.15366319118036,-0.0787124006907397,
-3.76618339589642));
#370491=CARTESIAN_POINT('Ctrl Pts',(-1.12285379978883,0.212860456164627,
-3.77837702194193));
#370492=CARTESIAN_POINT('Ctrl Pts',(-1.0821482238887,0.349228633959777,
-3.78417389022775));
#370493=CARTESIAN_POINT('Ctrl Pts',(-0.950436071606793,0.60543400761943,
-3.79522025808186));
#370494=CARTESIAN_POINT('Ctrl Pts',(-0.859180942083836,0.720913828422761,
-3.80059269283917));
#370495=CARTESIAN_POINT('Ctrl Pts',(-0.64028655446859,0.905058775893708,
-3.81259207988882));
#370496=CARTESIAN_POINT('Ctrl Pts',(-0.517800650893318,0.973476873865921,
-3.81866376976776));
#370497=CARTESIAN_POINT('Ctrl Pts',(-0.24560153936023,1.06350276870297,
-3.83102133314356));
#370498=CARTESIAN_POINT('Ctrl Pts',(-0.112468620062744,1.07601604072728,
-3.83648395927268));
#370499=CARTESIAN_POINT('Ctrl Pts',(-5.19688458933132E-13,1.07169464481439,
-3.84080535518562));
#370500=CARTESIAN_POINT('',(-1.11749020422196E-16,0.912499999999999,-4.00000000000001));
#370501=CARTESIAN_POINT('',(-1.5308084989342E-16,1.25000000000001,-3.6625));
#370502=CARTESIAN_POINT('Origin',(0.,-1.02673464470213E-16,-4.00000000000001));
#370503=CARTESIAN_POINT('Ctrl Pts',(-5.19624170088432E-13,1.07169464481439,
-3.84080535518562));
#370504=CARTESIAN_POINT('Ctrl Pts',(0.0132807037919846,1.07118435866472,
-3.84131564133529));
#370505=CARTESIAN_POINT('Ctrl Pts',(0.0262725682478854,1.07043200166311,
-3.84182103819358));
#370506=CARTESIAN_POINT('Ctrl Pts',(0.164982451660776,1.05991889326409,
-3.84727828766257));
#370507=CARTESIAN_POINT('Ctrl Pts',(0.288230522434384,1.02763979747026,
-3.85269578885312));
#370508=CARTESIAN_POINT('Ctrl Pts',(0.525243537044531,0.917015259508444,
-3.864379774694));
#370509=CARTESIAN_POINT('Ctrl Pts',(0.635518934908194,0.836644670589503,
-3.87057106866854));
#370510=CARTESIAN_POINT('Ctrl Pts',(0.811012773854783,0.64746200723685,
-3.88202106240099));
#370511=CARTESIAN_POINT('Ctrl Pts',(0.889005880992891,0.531601381546978,
-3.88742893998826));
#370512=CARTESIAN_POINT('Ctrl Pts',(0.982611668862114,0.276475013801935,
-3.89912755433172));
#370513=CARTESIAN_POINT('Ctrl Pts',(1.00330564083417,0.154442537046033,
-3.90480655630969));
#370514=CARTESIAN_POINT('Ctrl Pts',(0.999305789144461,-0.0998950462085405,
-3.91685903687869));
#370515=CARTESIAN_POINT('Ctrl Pts',(0.971246564415423,-0.229819589385441,
-3.92313678730786));
#370516=CARTESIAN_POINT('Ctrl Pts',(0.886252493360822,-0.425561051651668,
-3.93276679919375));
#370517=CARTESIAN_POINT('Ctrl Pts',(0.837759723201096,-0.51280233158914,
-3.93678750846591));
#370518=CARTESIAN_POINT('Ctrl Pts',(0.70522478018958,-0.666965853173508,
-3.94601792006284));
#370519=CARTESIAN_POINT('Ctrl Pts',(0.637118232403117,-0.726582133647196,
-3.95034126928747));
#370520=CARTESIAN_POINT('Ctrl Pts',(0.561651082536775,-0.775737593869401,
-3.95478357377719));
#370521=CARTESIAN_POINT('Origin',(0.,0.,2.95));
#370522=CARTESIAN_POINT('',(1.08253175473061,0.625000000000032,2.67500000000004));
#370523=CARTESIAN_POINT('Ctrl Pts',(5.20417042793042E-16,1.25000000000001,
2.29999999999999));
#370524=CARTESIAN_POINT('Ctrl Pts',(-0.15798414204464,1.25000000000001,
2.30820909682433));
#370525=CARTESIAN_POINT('Ctrl Pts',(-0.314658277380827,1.22005106146879,
2.3172485918592));
#370526=CARTESIAN_POINT('Ctrl Pts',(-0.613432363236355,1.10130056988825,
2.33633586350722));
#370527=CARTESIAN_POINT('Ctrl Pts',(-0.751899539744469,1.01183633973303,
2.34621475595866));
#370528=CARTESIAN_POINT('Ctrl Pts',(-0.983093567839997,0.788114405040584,
2.36493960809148));
#370529=CARTESIAN_POINT('Ctrl Pts',(-1.07493687987653,0.657342186486791,
2.37305946881069));
#370530=CARTESIAN_POINT('Ctrl Pts',(-1.20795581572139,0.361704284892804,
2.39079774290633));
#370531=CARTESIAN_POINT('Ctrl Pts',(-1.24521846245067,0.198500395363415,
2.40058997627809));
#370532=CARTESIAN_POINT('Ctrl Pts',(-1.25380644971248,-0.12854883069771,
2.42021292984176));
#370533=CARTESIAN_POINT('Ctrl Pts',(-1.22674852580128,-0.289230934492819,
2.42985385606947));
#370534=CARTESIAN_POINT('Ctrl Pts',(-1.11325757004244,-0.590753157646939,
2.44794518945872));
#370535=CARTESIAN_POINT('Ctrl Pts',(-1.02817905034803,-0.728821931999858,
2.45593890732547));
#370536=CARTESIAN_POINT('Ctrl Pts',(-0.806898504343732,-0.968975574709854,
2.47464159105895));
#370537=CARTESIAN_POINT('Ctrl Pts',(-0.671386595342725,-1.06734780968674,
2.48463416345087));
#370538=CARTESIAN_POINT('Ctrl Pts',(-0.375588931227746,-1.20286831517439,
2.50406987610572));
#370539=CARTESIAN_POINT('Ctrl Pts',(-0.219111339884313,-1.24095410198731,
2.5133432638637));
#370540=CARTESIAN_POINT('Ctrl Pts',(0.106381404288763,-1.25651181033803,
2.53072309422631));
#370541=CARTESIAN_POINT('Ctrl Pts',(0.272396301628041,-1.23124542513271,
2.53971676427232));
#370542=CARTESIAN_POINT('Ctrl Pts',(0.582447754407332,-1.11806263459385,
2.55922299406372));
#370543=CARTESIAN_POINT('Ctrl Pts',(0.723738224576676,-1.03223737104514,
2.56913942015894));
#370544=CARTESIAN_POINT('Ctrl Pts',(0.961193549459415,-0.814661185400381,
2.58800524634503));
#370545=CARTESIAN_POINT('Ctrl Pts',(1.05651539179714,-0.686531607242866,
2.59630810356532));
#370546=CARTESIAN_POINT('Ctrl Pts',(1.19754974404801,-0.394785470141088,
2.61381287179143));
#370547=CARTESIAN_POINT('Ctrl Pts',(1.23928155555513,-0.232689903651711,
2.6235386057808));
#370548=CARTESIAN_POINT('Ctrl Pts',(1.25478281639912,0.0551969019069727,
2.64081181411432));
#370549=CARTESIAN_POINT('Ctrl Pts',(1.24333250688269,0.17791489555393,2.64817489373322));
#370550=CARTESIAN_POINT('Ctrl Pts',(1.18605566680237,0.412076722424357,
2.66222460334545));
#370551=CARTESIAN_POINT('Ctrl Pts',(1.14170784117889,0.522504011678397,
2.66885024070069));
#370552=CARTESIAN_POINT('Ctrl Pts',(1.08253175473058,0.624999999999965,
2.67499999999999));
#370553=CARTESIAN_POINT('',(1.21030729568997,-0.312499999999427,2.67500000000001));
#370554=CARTESIAN_POINT('Origin',(0.,1.19785708548589E-17,2.67500000000001));
#370555=CARTESIAN_POINT('Ctrl Pts',(1.21030729568997,-0.312499999999433,
2.67500000000001));
#370556=CARTESIAN_POINT('Ctrl Pts',(1.175718981605,-0.446459964424188,2.66696240213453));
#370557=CARTESIAN_POINT('Ctrl Pts',(1.11915142536756,-0.573695925916809,
2.65969193612545));
#370558=CARTESIAN_POINT('Ctrl Pts',(0.965151072782271,-0.806771638479094,
2.64469757169674));
#370559=CARTESIAN_POINT('Ctrl Pts',(0.868041694629622,-0.910432845154661,
2.63654178419092));
#370560=CARTESIAN_POINT('Ctrl Pts',(0.624071847967031,-1.09560447505936,
2.61830959019575));
#370561=CARTESIAN_POINT('Ctrl Pts',(0.473899543568118,-1.16843452864645,
2.60832150675488));
#370562=CARTESIAN_POINT('Ctrl Pts',(0.157230972575195,-1.25059130591894,
2.58940222181311));
#370563=CARTESIAN_POINT('Ctrl Pts',(-0.00581482137773669,-1.26042122838038,
2.58126048986948));
#370564=CARTESIAN_POINT('Ctrl Pts',(-0.325767666610162,-1.21749197202904,
2.56334737465988));
#370565=CARTESIAN_POINT('Ctrl Pts',(-0.479659736469491,-1.16547197089985,
2.55379030810965));
#370566=CARTESIAN_POINT('Ctrl Pts',(-0.7647806647957,-1.00280132258151,
2.53409487063524));
#370567=CARTESIAN_POINT('Ctrl Pts',(-0.892020816335206,-0.891522885192972,
2.5241449252967));
#370568=CARTESIAN_POINT('Ctrl Pts',(-1.08986046956139,-0.632361074998956,
2.5060900210567));
#370569=CARTESIAN_POINT('Ctrl Pts',(-1.16124097803301,-0.489081617941554,
2.49809489707646));
#370570=CARTESIAN_POINT('Ctrl Pts',(-1.24773512440905,-0.179387936090198,
2.47951327616538));
#370571=CARTESIAN_POINT('Ctrl Pts',(-1.26046736614005,-0.0154803948659127,
2.46967882369192));
#370572=CARTESIAN_POINT('Ctrl Pts',(-1.22203528254611,0.310757366402179,
2.45010455801583));
#370573=CARTESIAN_POINT('Ctrl Pts',(-1.170140724678,0.469821795044816,2.44056069229728));
#370574=CARTESIAN_POINT('Ctrl Pts',(-1.0107864054522,0.752310445892212,
2.42361137324643));
#370575=CARTESIAN_POINT('Ctrl Pts',(-0.907229871159249,0.874434395171338,
2.41465801507458));
#370576=CARTESIAN_POINT('Ctrl Pts',(-0.655133943368811,1.07724588582535,
2.39547438169554));
#370577=CARTESIAN_POINT('Ctrl Pts',(-0.50755464776196,1.15414494620869,
2.38549896473995));
#370578=CARTESIAN_POINT('Ctrl Pts',(-0.235584599701466,1.23330008226491,
2.36899233241693));
#370579=CARTESIAN_POINT('Ctrl Pts',(-0.117988461920189,1.25000000000001,
2.36238086032257));
#370580=CARTESIAN_POINT('Ctrl Pts',(2.69541333697276E-13,1.25000000000001,
2.35624999999996));
#370581=CARTESIAN_POINT('Origin',(0.,2.73795905253904E-16,4.));
#370582=CARTESIAN_POINT('',(-0.750000000000001,-0.433012701892221,4.));
#370583=CARTESIAN_POINT('',(-0.750000000000004,0.433012701892217,4.));
#370584=CARTESIAN_POINT('Ctrl Pts',(-0.750000000000001,-0.433012701891379,
3.99999999999958));
#370585=CARTESIAN_POINT('Ctrl Pts',(-0.750000000000001,-2.44249065417534E-15,
3.78349364905421));
#370586=CARTESIAN_POINT('Ctrl Pts',(-0.750000000000001,0.433012701891373,
3.99999999999958));
#370587=CARTESIAN_POINT('Origin',(0.,2.73795905253904E-16,4.));
#370588=CARTESIAN_POINT('Origin',(0.,1.02673464470214E-16,4.));
#370589=CARTESIAN_POINT('',(-3.06161699786838E-16,2.5,4.));
#370590=CARTESIAN_POINT('Origin',(0.,1.02673464470214E-16,4.));
#370591=CARTESIAN_POINT('',(-3.06161699786838E-16,2.5,3.92500000000001));
#370592=CARTESIAN_POINT('',(-3.06161699786838E-16,2.5,4.));
#370593=CARTESIAN_POINT('Origin',(0.,9.75397912467035E-17,3.92500000000001));
#370594=CARTESIAN_POINT('Origin',(0.,9.75397912467035E-17,3.92500000000001));
#370595=CARTESIAN_POINT('',(-1.31649530908145E-16,1.0749999999984,2.49999999999841));
#370596=CARTESIAN_POINT('',(-3.06161699786838E-16,2.5,3.92500000000001));
#370597=CARTESIAN_POINT('',(-0.600917552801184,0.891360249694494,2.5));
#370598=CARTESIAN_POINT('Origin',(0.,0.,2.5));
#370599=CARTESIAN_POINT('Ctrl Pts',(1.21030729569027,-0.312499999998426,
2.67500000000005));
#370600=CARTESIAN_POINT('Ctrl Pts',(1.18496462782676,-0.397581898517953,
2.67173254198385));
#370601=CARTESIAN_POINT('Ctrl Pts',(1.15071194387983,-0.479744379279913,
2.66855106458315));
#370602=CARTESIAN_POINT('Ctrl Pts',(1.06411233511274,-0.63809170895112,
2.66237530137405));
#370603=CARTESIAN_POINT('Ctrl Pts',(1.01158452541921,-0.713299582901373,
2.6593557985417));
#370604=CARTESIAN_POINT('Ctrl Pts',(0.84399258075297,-0.902574391318878,
2.65021838828378));
#370605=CARTESIAN_POINT('Ctrl Pts',(0.71459255327479,-1.00055120699789,
2.643996728307));
#370606=CARTESIAN_POINT('Ctrl Pts',(0.434173163941591,-1.1360209702507,
2.63180275510934));
#370607=CARTESIAN_POINT('Ctrl Pts',(0.287439235068762,-1.17572689937217,
2.62594495039157));
#370608=CARTESIAN_POINT('Ctrl Pts',(-0.00405856185293136,-1.19866379085335,
2.61527944790127));
#370609=CARTESIAN_POINT('Ctrl Pts',(-0.161827341071919,-1.18631210777794,
2.61000562432497));
#370610=CARTESIAN_POINT('Ctrl Pts',(-0.469523736948815,-1.08498293735393,
2.59733204263689));
#370611=CARTESIAN_POINT('Ctrl Pts',(-0.603757024458315,-1.00920269685259,
2.59107878785054));
#370612=CARTESIAN_POINT('Ctrl Pts',(-0.861528187143977,-0.78774923249859,
2.57730651982981));
#370613=CARTESIAN_POINT('Ctrl Pts',(-0.949059710520787,-0.653224258938384,
2.57135243097231));
#370614=CARTESIAN_POINT('Ctrl Pts',(-1.06141710896073,-0.429890511860025,
2.56223771836896));
#370615=CARTESIAN_POINT('Ctrl Pts',(-1.09971742194718,-0.299695292969128,
2.55686044362927));
#370616=CARTESIAN_POINT('Ctrl Pts',(-1.12921272728689,-0.0226329958877538,
2.54523562102516));
#370617=CARTESIAN_POINT('Ctrl Pts',(-1.11665106720043,0.122177185089892,
2.53906054867293));
#370618=CARTESIAN_POINT('Ctrl Pts',(-1.03868521105767,0.394217153047777,
2.5272679762311));
#370619=CARTESIAN_POINT('Ctrl Pts',(-0.975394129424348,0.521041945584162,
2.52204255166252));
#370620=CARTESIAN_POINT('Ctrl Pts',(-0.810562892434841,0.735010845992019,
2.51135815914312));
#370621=CARTESIAN_POINT('Ctrl Pts',(-0.712460791732769,0.823114275812464,
2.50576422497663));
#370622=CARTESIAN_POINT('Ctrl Pts',(-0.600917552799552,0.891360249695952,
2.5000000000003));
#370623=CARTESIAN_POINT('',(0.93939647226611,-0.522646408087846,2.5));
#370624=CARTESIAN_POINT('Ctrl Pts',(0.939396472267503,-0.522646408088621,
2.49999999999841));
#370625=CARTESIAN_POINT('Ctrl Pts',(0.961378560063887,-0.493788939776118,
2.50517920331836));
#370626=CARTESIAN_POINT('Ctrl Pts',(0.981820055297906,-0.464129314934742,
2.51041697946993));
#370627=CARTESIAN_POINT('Ctrl Pts',(1.0007700635912,-0.433707147497555,
2.51570738971129));
#370628=CARTESIAN_POINT('Ctrl Pts',(1.01994614712023,-0.40292204097513,
2.52106091500378));
#370629=CARTESIAN_POINT('Ctrl Pts',(1.03759557945029,-0.37135536873159,
2.5264683377358));
#370630=CARTESIAN_POINT('Ctrl Pts',(1.05373251191938,-0.339009494244571,
2.53192350407058));
#370631=CARTESIAN_POINT('Ctrl Pts',(1.06650581336374,-0.313405891695234,
2.53624157903042));
#370632=CARTESIAN_POINT('Ctrl Pts',(1.07833079358038,-0.287313159438676,
2.54058956833869));
#370633=CARTESIAN_POINT('Ctrl Pts',(1.08919476231099,-0.260720293963244,
2.5449644199393));
#370634=CARTESIAN_POINT('Ctrl Pts',(1.10300386884231,-0.226918308571939,
2.55052525993339));
#370635=CARTESIAN_POINT('Ctrl Pts',(1.11523473813783,-0.192359407629985,
2.55612338880833));
#370636=CARTESIAN_POINT('Ctrl Pts',(1.12578644196984,-0.157280562137357,
2.56171996909941));
#370637=CARTESIAN_POINT('Ctrl Pts',(1.13631796415245,-0.122268809976041,
2.5673058451267));
#370638=CARTESIAN_POINT('Ctrl Pts',(1.14517642535264,-0.0867397266179055,
2.57289017848826));
#370639=CARTESIAN_POINT('Ctrl Pts',(1.15230846923948,-0.0509509669151141,
2.57843435414011));
#370640=CARTESIAN_POINT('Ctrl Pts',(1.15777287478455,-0.0235304546364063,
2.58268217210865));
#370641=CARTESIAN_POINT('Ctrl Pts',(1.16222477420995,0.00404196088120024,
2.58690641643057));
#370642=CARTESIAN_POINT('Ctrl Pts',(1.16566024779681,0.0316452258566077,
2.59108971936693));
#370643=CARTESIAN_POINT('Ctrl Pts',(1.16979235853104,0.0648458151264462,
2.59612130250411));
#370644=CARTESIAN_POINT('Ctrl Pts',(1.17249164294556,0.0984124738475194,
2.60114190384908));
#370645=CARTESIAN_POINT('Ctrl Pts',(1.17370841641877,0.132104984926701,
2.60611945789355));
#370646=CARTESIAN_POINT('Ctrl Pts',(1.17492748242562,0.16586097636351,2.61110639019154));
#370647=CARTESIAN_POINT('Ctrl Pts',(1.17465826041775,0.199742639149629,
2.61605011282462));
#370648=CARTESIAN_POINT('Ctrl Pts',(1.17290223392284,0.233497576361194,
2.62091837869804));
#370649=CARTESIAN_POINT('Ctrl Pts',(1.17114620742794,0.26725251357276,2.62578664457147));
#370650=CARTESIAN_POINT('Ctrl Pts',(1.16790337302496,0.300880045545673,
2.63057945368526));
#370651=CARTESIAN_POINT('Ctrl Pts',(1.16322801875488,0.334127040242341,
2.63526455894467));
#370652=CARTESIAN_POINT('Ctrl Pts',(1.1579563645548,0.371614393950363,2.6405472077862));
#370653=CARTESIAN_POINT('Ctrl Pts',(1.15086291017788,0.408718986722986,
2.64571065172927));
#370654=CARTESIAN_POINT('Ctrl Pts',(1.14196088119301,0.445439796657672,
2.65076150478858));
#370655=CARTESIAN_POINT('Ctrl Pts',(1.13310236418022,0.48198111999896,2.65578766992812));
#370656=CARTESIAN_POINT('Ctrl Pts',(1.12245275596893,0.518143424683796,
2.66070234215347));
#370657=CARTESIAN_POINT('Ctrl Pts',(1.10997435913185,0.553919706178163,
2.66551203896725));
#370658=CARTESIAN_POINT('Ctrl Pts',(1.1016495495542,0.577787414083731,2.66872076927321));
#370659=CARTESIAN_POINT('Ctrl Pts',(1.09250974434973,0.601483170784815,
2.67188277788132));
#370660=CARTESIAN_POINT('Ctrl Pts',(1.08253175473059,0.625000000000025,
2.67500000000006));
#370661=CARTESIAN_POINT('Origin',(0.,0.,2.5));
#370662=CARTESIAN_POINT('Origin',(-1.91190658769134E-30,5.47591810507809E-16,
4.));
#370663=CARTESIAN_POINT('',(-3.57786716920216E-15,0.866025403784441,4.));
#370664=CARTESIAN_POINT('Origin',(0.,2.73795905253904E-16,4.));
#370665=CARTESIAN_POINT('',(0.750000000000002,0.433012701892219,4.));
#370666=CARTESIAN_POINT('Origin',(0.,2.73795905253904E-16,4.));
#370667=CARTESIAN_POINT('',(0.750000000000002,-0.433012701892219,4.));
#370668=CARTESIAN_POINT('Origin',(0.,2.73795905253904E-16,4.));
#370669=CARTESIAN_POINT('',(-4.28259858131774E-15,-0.86602540378444,4.));
#370670=CARTESIAN_POINT('Origin',(0.,2.73795905253904E-16,4.));
#370671=CARTESIAN_POINT('Origin',(0.,2.73795905253904E-16,4.));
#370672=CARTESIAN_POINT('Origin',(-1.19494161730709E-30,3.4224488156738E-16,
2.5));
#370673=CARTESIAN_POINT('Ctrl Pts',(-0.600917552801664,0.891360249695444,
2.5));
#370674=CARTESIAN_POINT('Ctrl Pts',(-0.52912367055064,0.928118712066169,
2.5));
#370675=CARTESIAN_POINT('Ctrl Pts',(-0.45338281650616,0.956546033855086,
2.5));
#370676=CARTESIAN_POINT('Ctrl Pts',(-0.296173149603253,0.995821882185393,
2.5));
#370677=CARTESIAN_POINT('Ctrl Pts',(-0.215216702988762,1.00636894049577,
2.50000000001075));
#370678=CARTESIAN_POINT('Ctrl Pts',(-0.0605603584965276,1.00860738826189,
2.50000000001075));
#370679=CARTESIAN_POINT('Ctrl Pts',(0.0255986159637691,1.00270295342094,
2.5));
#370680=CARTESIAN_POINT('Ctrl Pts',(0.193358226390499,0.96153036876019,
2.5));
#370681=CARTESIAN_POINT('Ctrl Pts',(0.26576695744227,0.93389263995366,2.5));
#370682=CARTESIAN_POINT('Ctrl Pts',(0.333926106471282,0.897615791123228,
2.5));
#370683=CARTESIAN_POINT('Ctrl Pts',(0.870621065093339,0.39904851092642,
2.5));
#370684=CARTESIAN_POINT('Ctrl Pts',(0.912954540737191,0.330380547800277,
2.5));
#370685=CARTESIAN_POINT('Ctrl Pts',(0.946864699817239,0.256884680432555,
2.5));
#370686=CARTESIAN_POINT('Ctrl Pts',(0.996003967301862,0.104444769787427,
2.5));
#370687=CARTESIAN_POINT('Ctrl Pts',(1.01131329268253,0.0261625419559724,
2.5));
#370688=CARTESIAN_POINT('Ctrl Pts',(1.02292765596175,-0.129431544988595,
2.5));
#370689=CARTESIAN_POINT('Ctrl Pts',(1.01988149559102,-0.206142778785646,
2.5));
#370690=CARTESIAN_POINT('Ctrl Pts',(0.995349857534893,-0.364613759944385,
2.5));
#370691=CARTESIAN_POINT('Ctrl Pts',(0.972235069110387,-0.445515811209248,
2.5));
#370692=CARTESIAN_POINT('Ctrl Pts',(0.939396472266109,-0.522646408087845,
2.5));
#370693=CARTESIAN_POINT('Origin',(0.,2.73795905253904E-16,4.));
#370694=CARTESIAN_POINT('Ctrl Pts',(0.750000000000002,0.433012701891376,
3.99999999999958));
#370695=CARTESIAN_POINT('Ctrl Pts',(0.750000000000002,-4.71844785465692E-16,
3.78349364905421));
#370696=CARTESIAN_POINT('Ctrl Pts',(0.750000000000002,-0.433012701891378,
3.99999999999958));
#370697=CARTESIAN_POINT('Origin',(0.,2.73795905253904E-16,4.));
#370698=CARTESIAN_POINT('Ctrl Pts',(7.26431099148093E-13,0.866025403784019,
3.99999999999958));
#370699=CARTESIAN_POINT('Ctrl Pts',(0.375,0.649519052838329,3.78349364905421));
#370700=CARTESIAN_POINT('Ctrl Pts',(0.749999999999273,0.43301270189264,
3.99999999999958));
#370701=CARTESIAN_POINT('Origin',(0.,2.73795905253904E-16,4.));
#370702=CARTESIAN_POINT('Ctrl Pts',(-0.749999999999275,0.433012701892637,
3.99999999999958));
#370703=CARTESIAN_POINT('Ctrl Pts',(-0.375000000000002,0.649519052838327,
3.78349364905421));
#370704=CARTESIAN_POINT('Ctrl Pts',(-7.29620208486308E-13,0.866025403784017,
3.99999999999958));
#370705=CARTESIAN_POINT('Origin',(0.,2.73795905253904E-16,4.));
#370706=CARTESIAN_POINT('Ctrl Pts',(-7.33598022284514E-13,-0.866025403784019,
3.99999999999958));
#370707=CARTESIAN_POINT('Ctrl Pts',(-0.375000000000003,-0.649519052838331,
3.78349364905421));
#370708=CARTESIAN_POINT('Ctrl Pts',(-0.749999999999272,-0.433012701892644,
3.99999999999958));
#370709=CARTESIAN_POINT('Origin',(0.,2.73795905253904E-16,4.));
#370710=CARTESIAN_POINT('Ctrl Pts',(0.749999999999273,-0.433012701892642,
3.99999999999958));
#370711=CARTESIAN_POINT('Ctrl Pts',(0.375000000000001,-0.649519052838331,
3.78349364905421));
#370712=CARTESIAN_POINT('Ctrl Pts',(7.28385714548936E-13,-0.866025403784021,
3.99999999999958));
#370713=CARTESIAN_POINT('Origin',(0.750000000000002,-0.433012701892221,
2.95));
#370714=CARTESIAN_POINT('',(-8.98696932731E-16,-0.866025403784442,2.95));
#370715=CARTESIAN_POINT('',(0.750000000000002,-0.433012701892221,2.95));
#370716=CARTESIAN_POINT('',(-8.98696932731E-16,-0.866025403784442,2.95));
#370717=CARTESIAN_POINT('',(0.750000000000002,0.433012701892219,2.95));
#370718=CARTESIAN_POINT('',(0.750000000000002,-0.433012701892221,2.95));
#370719=CARTESIAN_POINT('',(6.5096847437113E-16,0.866025403784438,2.95));
#370720=CARTESIAN_POINT('',(0.750000000000002,0.433012701892219,2.95));
#370721=CARTESIAN_POINT('',(-0.750000000000001,0.433012701892218,2.95));
#370722=CARTESIAN_POINT('',(6.5096847437113E-16,0.866025403784438,2.95));
#370723=CARTESIAN_POINT('',(-0.750000000000001,-0.433012701892223,2.95));
#370724=CARTESIAN_POINT('',(-0.750000000000001,0.433012701892218,2.95));
#370725=CARTESIAN_POINT('',(-0.750000000000001,-0.433012701892223,2.95));
#370726=CARTESIAN_POINT('Origin',(0.750000000000002,-0.433012701892221,
2.95));
#370727=CARTESIAN_POINT('',(0.750000000000002,0.433012701892219,2.95));
#370728=CARTESIAN_POINT('',(0.750000000000002,-0.433012701892221,2.95));
#370729=CARTESIAN_POINT('Origin',(0.750000000000002,0.433012701892219,2.95));
#370730=CARTESIAN_POINT('',(6.5096847437113E-16,0.866025403784438,2.95));
#370731=CARTESIAN_POINT('Origin',(6.5096847437113E-16,0.866025403784438,
2.95));
#370732=CARTESIAN_POINT('',(-0.750000000000001,0.433012701892218,2.95));
#370733=CARTESIAN_POINT('Origin',(-0.750000000000001,0.433012701892218,
2.95));
#370734=CARTESIAN_POINT('',(-0.750000000000001,-0.433012701892223,2.95));
#370735=CARTESIAN_POINT('Origin',(-0.750000000000001,-0.433012701892223,
2.95));
#370736=CARTESIAN_POINT('',(-8.98696932731E-16,-0.866025403784442,2.95));
#370737=CARTESIAN_POINT('Origin',(-8.98696932731E-16,-0.866025403784442,
2.95));
#370738=CARTESIAN_POINT('Origin',(8.72870334710784E-15,-1.25,-4.00000000000001));
#370739=CARTESIAN_POINT('Ctrl Pts',(0.,0.957713005082983,-4.22499802480406));
#370740=CARTESIAN_POINT('Ctrl Pts',(-0.552935861291066,0.957713005082983,
-4.18749802480406));
#370741=CARTESIAN_POINT('Ctrl Pts',(-0.829403791936599,0.478856502541492,
-4.14999802480405));
#370742=CARTESIAN_POINT('Ctrl Pts',(-1.10587172258213,-6.632643158244E-17,
-4.11249802480406));
#370743=CARTESIAN_POINT('Ctrl Pts',(-0.829403791936599,-0.478856502541491,
-4.07499802480406));
#370744=CARTESIAN_POINT('Ctrl Pts',(-0.552935861291066,-0.957713005082983,
-4.03749802480406));
#370745=CARTESIAN_POINT('Ctrl Pts',(-1.17286016617667E-16,-0.957713005082983,
-3.99999802480406));
#370746=CARTESIAN_POINT('Ctrl Pts',(0.552935861291066,-0.957713005082984,
-3.96249802480406));
#370747=CARTESIAN_POINT('Ctrl Pts',(0.829403791936598,-0.478856502541492,
-3.92499802480406));
#370748=CARTESIAN_POINT('Ctrl Pts',(1.10587172258213,-3.36985585326162E-16,
-3.88749802480406));
#370749=CARTESIAN_POINT('Ctrl Pts',(0.829403791936599,0.478856502541491,
-3.84999802480406));
#370750=CARTESIAN_POINT('Ctrl Pts',(0.552935861291066,0.957713005082983,
-3.81249802480406));
#370751=CARTESIAN_POINT('Ctrl Pts',(0.,0.957713005082983,-3.77499802480406));
#370752=CARTESIAN_POINT('Ctrl Pts',(-0.552935861291066,0.957713005082983,
-3.73749802480406));
#370753=CARTESIAN_POINT('Ctrl Pts',(-0.829403791936599,0.478856502541492,
-3.69999802480406));
#370754=CARTESIAN_POINT('Ctrl Pts',(-1.10587172258213,-6.59238329387739E-17,
-3.66249802480405));
#370755=CARTESIAN_POINT('Ctrl Pts',(-0.829403791936599,-0.478856502541491,
-3.62499802480406));
#370756=CARTESIAN_POINT('Ctrl Pts',(-0.552935861291066,-0.957713005082983,
-3.58749802480406));
#370757=CARTESIAN_POINT('Ctrl Pts',(-1.17286016617667E-16,-0.957713005082983,
-3.54999802480406));
#370758=CARTESIAN_POINT('Ctrl Pts',(0.552935861291066,-0.957713005082984,
-3.51249802480406));
#370759=CARTESIAN_POINT('Ctrl Pts',(0.829403791936598,-0.478856502541492,
-3.47499802480406));
#370760=CARTESIAN_POINT('Ctrl Pts',(1.10587172258213,-3.36582986682496E-16,
-3.43749802480405));
#370761=CARTESIAN_POINT('Ctrl Pts',(0.829403791936599,0.478856502541491,
-3.39999802480406));
#370762=CARTESIAN_POINT('Ctrl Pts',(0.552935861291066,0.957713005082983,
-3.36249802480406));
#370763=CARTESIAN_POINT('Ctrl Pts',(0.,0.957713005082983,-3.32499802480406));
#370764=CARTESIAN_POINT('Ctrl Pts',(-0.552935861291066,0.957713005082983,
-3.28749802480406));
#370765=CARTESIAN_POINT('Ctrl Pts',(-0.829403791936599,0.478856502541492,
-3.24999802480406));
#370766=CARTESIAN_POINT('Ctrl Pts',(-1.10587172258213,-6.55212342951079E-17,
-3.21249802480406));
#370767=CARTESIAN_POINT('Ctrl Pts',(-0.829403791936599,-0.478856502541491,
-3.17499802480406));
#370768=CARTESIAN_POINT('Ctrl Pts',(-0.552935861291066,-0.957713005082983,
-3.13749802480406));
#370769=CARTESIAN_POINT('Ctrl Pts',(-1.17286016617667E-16,-0.957713005082983,
-3.09999802480406));
#370770=CARTESIAN_POINT('Ctrl Pts',(0.552935861291066,-0.957713005082984,
-3.06249802480406));
#370771=CARTESIAN_POINT('Ctrl Pts',(0.829403791936598,-0.478856502541492,
-3.02499802480406));
#370772=CARTESIAN_POINT('Ctrl Pts',(1.10587172258213,-3.3618038803883E-16,
-2.98749802480406));
#370773=CARTESIAN_POINT('Ctrl Pts',(0.829403791936599,0.478856502541491,
-2.94999802480406));
#370774=CARTESIAN_POINT('Ctrl Pts',(0.552935861291066,0.957713005082983,
-2.91249802480406));
#370775=CARTESIAN_POINT('Ctrl Pts',(0.,0.957713005082983,-2.87499802480406));
#370776=CARTESIAN_POINT('Ctrl Pts',(-0.552935861291066,0.957713005082983,
-2.83749802480406));
#370777=CARTESIAN_POINT('Ctrl Pts',(-0.829403791936599,0.478856502541492,
-2.79999802480406));
#370778=CARTESIAN_POINT('Ctrl Pts',(-1.10587172258213,-6.51186356514418E-17,
-2.76249802480406));
#370779=CARTESIAN_POINT('Ctrl Pts',(-0.829403791936599,-0.478856502541491,
-2.72499802480406));
#370780=CARTESIAN_POINT('Ctrl Pts',(-0.552935861291066,-0.957713005082983,
-2.68749802480406));
#370781=CARTESIAN_POINT('Ctrl Pts',(-1.17286016617667E-16,-0.957713005082983,
-2.64999802480406));
#370782=CARTESIAN_POINT('Ctrl Pts',(0.552935861291066,-0.957713005082984,
-2.61249802480406));
#370783=CARTESIAN_POINT('Ctrl Pts',(0.829403791936598,-0.478856502541492,
-2.57499802480406));
#370784=CARTESIAN_POINT('Ctrl Pts',(1.10587172258213,-3.35777789395164E-16,
-2.53749802480406));
#370785=CARTESIAN_POINT('Ctrl Pts',(0.829403791936599,0.478856502541491,
-2.49999802480406));
#370786=CARTESIAN_POINT('Ctrl Pts',(0.552935861291066,0.957713005082983,
-2.46249802480406));
#370787=CARTESIAN_POINT('Ctrl Pts',(0.,0.957713005082983,-2.42499802480406));
#370788=CARTESIAN_POINT('Ctrl Pts',(-0.552935861291066,0.957713005082983,
-2.38749802480406));
#370789=CARTESIAN_POINT('Ctrl Pts',(-0.829403791936599,0.478856502541492,
-2.34999802480406));
#370790=CARTESIAN_POINT('Ctrl Pts',(-1.10587172258213,-6.47160370077758E-17,
-2.31249802480406));
#370791=CARTESIAN_POINT('Ctrl Pts',(-0.829403791936599,-0.478856502541491,
-2.27499802480406));
#370792=CARTESIAN_POINT('Ctrl Pts',(-0.552935861291066,-0.957713005082983,
-2.23749802480406));
#370793=CARTESIAN_POINT('Ctrl Pts',(-1.17286016617667E-16,-0.957713005082983,
-2.19999802480406));
#370794=CARTESIAN_POINT('Ctrl Pts',(0.552935861291066,-0.957713005082984,
-2.16249802480406));
#370795=CARTESIAN_POINT('Ctrl Pts',(0.829403791936598,-0.478856502541492,
-2.12499802480406));
#370796=CARTESIAN_POINT('Ctrl Pts',(1.10587172258213,-3.35375190751498E-16,
-2.08749802480406));
#370797=CARTESIAN_POINT('Ctrl Pts',(0.829403791936599,0.478856502541491,
-2.04999802480406));
#370798=CARTESIAN_POINT('Ctrl Pts',(0.552935861291066,0.957713005082983,
-2.01249802480406));
#370799=CARTESIAN_POINT('Ctrl Pts',(0.,0.957713005082983,-1.97499802480406));
#370800=CARTESIAN_POINT('Ctrl Pts',(-0.552935861291066,0.957713005082983,
-1.93749802480406));
#370801=CARTESIAN_POINT('Ctrl Pts',(-0.829403791936599,0.478856502541492,
-1.89999802480406));
#370802=CARTESIAN_POINT('Ctrl Pts',(-1.10587172258213,-6.43134383641097E-17,
-1.86249802480406));
#370803=CARTESIAN_POINT('Ctrl Pts',(-0.829403791936599,-0.478856502541491,
-1.82499802480406));
#370804=CARTESIAN_POINT('Ctrl Pts',(-0.552935861291066,-0.957713005082983,
-1.78749802480406));
#370805=CARTESIAN_POINT('Ctrl Pts',(-1.17286016617667E-16,-0.957713005082983,
-1.74999802480406));
#370806=CARTESIAN_POINT('Ctrl Pts',(0.552935861291066,-0.957713005082984,
-1.71249802480406));
#370807=CARTESIAN_POINT('Ctrl Pts',(0.829403791936598,-0.478856502541492,
-1.67499802480406));
#370808=CARTESIAN_POINT('Ctrl Pts',(1.10587172258213,-3.34972592107832E-16,
-1.63749802480406));
#370809=CARTESIAN_POINT('Ctrl Pts',(0.829403791936599,0.478856502541491,
-1.59999802480406));
#370810=CARTESIAN_POINT('Ctrl Pts',(0.552935861291066,0.957713005082983,
-1.56249802480406));
#370811=CARTESIAN_POINT('Ctrl Pts',(0.,0.957713005082983,-1.52499802480406));
#370812=CARTESIAN_POINT('Ctrl Pts',(-0.552935861291066,0.957713005082983,
-1.48749802480406));
#370813=CARTESIAN_POINT('Ctrl Pts',(-0.829403791936599,0.478856502541492,
-1.44999802480406));
#370814=CARTESIAN_POINT('Ctrl Pts',(-1.10587172258213,-6.39108397204437E-17,
-1.41249802480406));
#370815=CARTESIAN_POINT('Ctrl Pts',(-0.829403791936599,-0.478856502541491,
-1.37499802480406));
#370816=CARTESIAN_POINT('Ctrl Pts',(-0.552935861291066,-0.957713005082983,
-1.33749802480406));
#370817=CARTESIAN_POINT('Ctrl Pts',(-1.17286016617667E-16,-0.957713005082983,
-1.29999802480406));
#370818=CARTESIAN_POINT('Ctrl Pts',(0.552935861291066,-0.957713005082984,
-1.26249802480406));
#370819=CARTESIAN_POINT('Ctrl Pts',(0.829403791936598,-0.478856502541492,
-1.22499802480406));
#370820=CARTESIAN_POINT('Ctrl Pts',(1.10587172258213,-3.34569993464166E-16,
-1.18749802480406));
#370821=CARTESIAN_POINT('Ctrl Pts',(0.829403791936599,0.478856502541491,
-1.14999802480406));
#370822=CARTESIAN_POINT('Ctrl Pts',(0.552935861291066,0.957713005082983,
-1.11249802480406));
#370823=CARTESIAN_POINT('Ctrl Pts',(0.,0.957713005082983,-1.07499802480406));
#370824=CARTESIAN_POINT('Ctrl Pts',(-0.552935861291066,0.957713005082983,
-1.03749802480406));
#370825=CARTESIAN_POINT('Ctrl Pts',(-0.829403791936599,0.478856502541492,
-0.999998024804056));
#370826=CARTESIAN_POINT('Ctrl Pts',(-1.10587172258213,-6.35082410767776E-17,
-0.962498024804056));
#370827=CARTESIAN_POINT('Ctrl Pts',(-0.829403791936599,-0.478856502541491,
-0.924998024804056));
#370828=CARTESIAN_POINT('Ctrl Pts',(-0.552935861291066,-0.957713005082983,
-0.887498024804056));
#370829=CARTESIAN_POINT('Ctrl Pts',(-1.17286016617667E-16,-0.957713005082983,
-0.849998024804056));
#370830=CARTESIAN_POINT('Ctrl Pts',(0.552935861291066,-0.957713005082984,
-0.812498024804056));
#370831=CARTESIAN_POINT('Ctrl Pts',(0.829403791936598,-0.478856502541492,
-0.774998024804056));
#370832=CARTESIAN_POINT('Ctrl Pts',(1.10587172258213,-3.341673948205E-16,
-0.737498024804056));
#370833=CARTESIAN_POINT('Ctrl Pts',(0.829403791936599,0.478856502541491,
-0.699998024804056));
#370834=CARTESIAN_POINT('Ctrl Pts',(0.552935861291066,0.957713005082983,
-0.662498024804056));
#370835=CARTESIAN_POINT('Ctrl Pts',(0.,0.957713005082983,-0.624998024804056));
#370836=CARTESIAN_POINT('Ctrl Pts',(-0.552935861291066,0.957713005082983,
-0.587498024804056));
#370837=CARTESIAN_POINT('Ctrl Pts',(-0.829403791936599,0.478856502541492,
-0.549998024804056));
#370838=CARTESIAN_POINT('Ctrl Pts',(-1.10587172258213,-6.31056424331116E-17,
-0.512498024804056));
#370839=CARTESIAN_POINT('Ctrl Pts',(-0.829403791936599,-0.478856502541491,
-0.474998024804056));
#370840=CARTESIAN_POINT('Ctrl Pts',(-0.552935861291066,-0.957713005082983,
-0.437498024804056));
#370841=CARTESIAN_POINT('Ctrl Pts',(-1.17286016617667E-16,-0.957713005082983,
-0.399998024804056));
#370842=CARTESIAN_POINT('Ctrl Pts',(0.552935861291066,-0.957713005082984,
-0.362498024804056));
#370843=CARTESIAN_POINT('Ctrl Pts',(0.829403791936598,-0.478856502541492,
-0.324998024804056));
#370844=CARTESIAN_POINT('Ctrl Pts',(1.10587172258213,-3.33764796176834E-16,
-0.287498024804056));
#370845=CARTESIAN_POINT('Ctrl Pts',(0.829403791936599,0.478856502541491,
-0.249998024804056));
#370846=CARTESIAN_POINT('Ctrl Pts',(0.552935861291066,0.957713005082983,
-0.212498024804056));
#370847=CARTESIAN_POINT('Ctrl Pts',(0.,0.957713005082983,-0.174998024804056));
#370848=CARTESIAN_POINT('Ctrl Pts',(-0.552935861291066,0.957713005082983,
-0.137498024804056));
#370849=CARTESIAN_POINT('Ctrl Pts',(-0.829403791936599,0.478856502541492,
-0.0999980248040564));
#370850=CARTESIAN_POINT('Ctrl Pts',(-1.10587172258213,-6.27030437894455E-17,
-0.0624980248040562));
#370851=CARTESIAN_POINT('Ctrl Pts',(-0.829403791936599,-0.478856502541491,
-0.024998024804056));
#370852=CARTESIAN_POINT('Ctrl Pts',(-0.552935861291066,-0.957713005082983,
0.0125019751959442));
#370853=CARTESIAN_POINT('Ctrl Pts',(-1.17286016617667E-16,-0.957713005082983,
0.0500019751959436));
#370854=CARTESIAN_POINT('Ctrl Pts',(0.552935861291066,-0.957713005082984,
0.0875019751959438));
#370855=CARTESIAN_POINT('Ctrl Pts',(0.829403791936598,-0.478856502541492,
0.125001975195944));
#370856=CARTESIAN_POINT('Ctrl Pts',(1.10587172258213,-3.33362197533168E-16,
0.162501975195944));
#370857=CARTESIAN_POINT('Ctrl Pts',(0.829403791936599,0.478856502541491,
0.200001975195944));
#370858=CARTESIAN_POINT('Ctrl Pts',(0.552935861291066,0.957713005082983,
0.237501975195944));
#370859=CARTESIAN_POINT('Ctrl Pts',(0.,0.957713005082983,0.275001975195944));
#370860=CARTESIAN_POINT('Ctrl Pts',(-0.552935861291066,0.957713005082983,
0.312501975195944));
#370861=CARTESIAN_POINT('Ctrl Pts',(-0.829403791936599,0.478856502541492,
0.350001975195944));
#370862=CARTESIAN_POINT('Ctrl Pts',(-1.10587172258213,-6.23004451457795E-17,
0.387501975195944));
#370863=CARTESIAN_POINT('Ctrl Pts',(-0.829403791936599,-0.478856502541491,
0.425001975195944));
#370864=CARTESIAN_POINT('Ctrl Pts',(-0.552935861291066,-0.957713005082983,
0.462501975195944));
#370865=CARTESIAN_POINT('Ctrl Pts',(-1.17286016617667E-16,-0.957713005082983,
0.500001975195943));
#370866=CARTESIAN_POINT('Ctrl Pts',(0.552935861291066,-0.957713005082984,
0.537501975195944));
#370867=CARTESIAN_POINT('Ctrl Pts',(0.829403791936598,-0.478856502541492,
0.575001975195944));
#370868=CARTESIAN_POINT('Ctrl Pts',(1.10587172258213,-3.32959598889502E-16,
0.612501975195944));
#370869=CARTESIAN_POINT('Ctrl Pts',(0.829403791936599,0.478856502541491,
0.650001975195944));
#370870=CARTESIAN_POINT('Ctrl Pts',(0.552935861291066,0.957713005082983,
0.687501975195943));
#370871=CARTESIAN_POINT('Ctrl Pts',(0.,0.957713005082983,0.725001975195944));
#370872=CARTESIAN_POINT('Ctrl Pts',(-0.552935861291066,0.957713005082983,
0.762501975195944));
#370873=CARTESIAN_POINT('Ctrl Pts',(-0.829403791936599,0.478856502541492,
0.800001975195944));
#370874=CARTESIAN_POINT('Ctrl Pts',(-1.10587172258213,-6.18978465021134E-17,
0.837501975195944));
#370875=CARTESIAN_POINT('Ctrl Pts',(-0.829403791936599,-0.478856502541491,
0.875001975195944));
#370876=CARTESIAN_POINT('Ctrl Pts',(-0.552935861291066,-0.957713005082983,
0.912501975195944));
#370877=CARTESIAN_POINT('Ctrl Pts',(-1.17286016617667E-16,-0.957713005082983,
0.950001975195944));
#370878=CARTESIAN_POINT('Ctrl Pts',(0.552935861291066,-0.957713005082984,
0.987501975195944));
#370879=CARTESIAN_POINT('Ctrl Pts',(0.829403791936598,-0.478856502541492,
1.02500197519594));
#370880=CARTESIAN_POINT('Ctrl Pts',(1.10587172258213,-3.32557000245836E-16,
1.06250197519594));
#370881=CARTESIAN_POINT('Ctrl Pts',(0.829403791936599,0.478856502541491,
1.10000197519594));
#370882=CARTESIAN_POINT('Ctrl Pts',(0.552935861291066,0.957713005082983,
1.13750197519594));
#370883=CARTESIAN_POINT('Ctrl Pts',(0.,0.957713005082983,1.17500197519594));
#370884=CARTESIAN_POINT('Ctrl Pts',(-0.552935861291066,0.957713005082983,
1.21250197519594));
#370885=CARTESIAN_POINT('Ctrl Pts',(-0.829403791936599,0.478856502541492,
1.25000197519594));
#370886=CARTESIAN_POINT('Ctrl Pts',(-1.10587172258213,-6.14952478584474E-17,
1.28750197519594));
#370887=CARTESIAN_POINT('Ctrl Pts',(-0.829403791936599,-0.478856502541491,
1.32500197519594));
#370888=CARTESIAN_POINT('Ctrl Pts',(-0.552935861291066,-0.957713005082983,
1.36250197519594));
#370889=CARTESIAN_POINT('Ctrl Pts',(-1.17286016617667E-16,-0.957713005082983,
1.40000197519594));
#370890=CARTESIAN_POINT('Ctrl Pts',(0.552935861291066,-0.957713005082984,
1.43750197519594));
#370891=CARTESIAN_POINT('Ctrl Pts',(0.829403791936598,-0.478856502541492,
1.47500197519594));
#370892=CARTESIAN_POINT('Ctrl Pts',(1.10587172258213,-3.3215440160217E-16,
1.51250197519594));
#370893=CARTESIAN_POINT('Ctrl Pts',(0.829403791936599,0.478856502541491,
1.55000197519594));
#370894=CARTESIAN_POINT('Ctrl Pts',(0.552935861291066,0.957713005082983,
1.58750197519594));
#370895=CARTESIAN_POINT('Ctrl Pts',(0.,0.957713005082983,1.62500197519594));
#370896=CARTESIAN_POINT('Ctrl Pts',(-0.552935861291066,0.957713005082983,
1.66250197519594));
#370897=CARTESIAN_POINT('Ctrl Pts',(-0.829403791936599,0.478856502541492,
1.70000197519594));
#370898=CARTESIAN_POINT('Ctrl Pts',(-1.10587172258213,-6.10926492147814E-17,
1.73750197519594));
#370899=CARTESIAN_POINT('Ctrl Pts',(-0.829403791936599,-0.478856502541491,
1.77500197519594));
#370900=CARTESIAN_POINT('Ctrl Pts',(-0.552935861291066,-0.957713005082983,
1.81250197519594));
#370901=CARTESIAN_POINT('Ctrl Pts',(-1.17286016617667E-16,-0.957713005082983,
1.85000197519594));
#370902=CARTESIAN_POINT('Ctrl Pts',(0.552935861291066,-0.957713005082984,
1.88750197519594));
#370903=CARTESIAN_POINT('Ctrl Pts',(0.829403791936598,-0.478856502541492,
1.92500197519594));
#370904=CARTESIAN_POINT('Ctrl Pts',(1.10587172258213,-3.31751802958504E-16,
1.96250197519594));
#370905=CARTESIAN_POINT('Ctrl Pts',(0.829403791936599,0.478856502541491,
2.00000197519594));
#370906=CARTESIAN_POINT('Ctrl Pts',(0.552935861291066,0.957713005082983,
2.03750197519594));
#370907=CARTESIAN_POINT('Ctrl Pts',(0.,0.957713005082983,2.07500197519594));
#370908=CARTESIAN_POINT('Ctrl Pts',(-0.552935861291066,0.957713005082983,
2.11250197519594));
#370909=CARTESIAN_POINT('Ctrl Pts',(-0.829403791936599,0.478856502541492,
2.15000197519594));
#370910=CARTESIAN_POINT('Ctrl Pts',(-1.10587172258213,-6.06900505711153E-17,
2.18750197519594));
#370911=CARTESIAN_POINT('Ctrl Pts',(-0.829403791936599,-0.478856502541491,
2.22500197519594));
#370912=CARTESIAN_POINT('Ctrl Pts',(-0.552935861291066,-0.957713005082983,
2.26250197519594));
#370913=CARTESIAN_POINT('Ctrl Pts',(-1.17286016617667E-16,-0.957713005082983,
2.30000197519594));
#370914=CARTESIAN_POINT('Ctrl Pts',(0.552935861291066,-0.957713005082984,
2.33750197519594));
#370915=CARTESIAN_POINT('Ctrl Pts',(0.829403791936598,-0.478856502541492,
2.37500197519594));
#370916=CARTESIAN_POINT('Ctrl Pts',(1.10587172258213,-3.31349204314838E-16,
2.41250197519594));
#370917=CARTESIAN_POINT('Ctrl Pts',(0.829403791936599,0.478856502541491,
2.45000197519594));
#370918=CARTESIAN_POINT('Ctrl Pts',(0.552935861291066,0.957713005082983,
2.48750197519594));
#370919=CARTESIAN_POINT('Ctrl Pts',(0.,0.957713005082983,2.52500197519594));
#370920=CARTESIAN_POINT('Ctrl Pts',(-0.552935861291066,0.957713005082983,
2.56250197519594));
#370921=CARTESIAN_POINT('Ctrl Pts',(-0.829403791936599,0.478856502541492,
2.60000197519594));
#370922=CARTESIAN_POINT('Ctrl Pts',(-1.10587172258213,-6.02874519274493E-17,
2.63750197519594));
#370923=CARTESIAN_POINT('Ctrl Pts',(-0.829403791936599,-0.478856502541491,
2.67500197519594));
#370924=CARTESIAN_POINT('Ctrl Pts',(-0.552935861291066,-0.957713005082983,
2.71250197519594));
#370925=CARTESIAN_POINT('Ctrl Pts',(-1.17286016617667E-16,-0.957713005082983,
2.75000197519594));
#370926=CARTESIAN_POINT('Ctrl Pts',(0.552935861291066,-0.957713005082984,
2.78750197519594));
#370927=CARTESIAN_POINT('Ctrl Pts',(0.829403791936598,-0.478856502541492,
2.82500197519594));
#370928=CARTESIAN_POINT('Ctrl Pts',(1.10587172258213,-3.30946605671172E-16,
2.86250197519594));
#370929=CARTESIAN_POINT('Ctrl Pts',(0.829403791936599,0.478856502541491,
2.90000197519594));
#370930=CARTESIAN_POINT('Ctrl Pts',(0.552935861291066,0.957713005082983,
2.93750197519594));
#370931=CARTESIAN_POINT('Ctrl Pts',(0.,0.957713005082983,2.97500197519594));
#370932=CARTESIAN_POINT('Ctrl Pts',(-0.552935861291066,0.957713005082983,
3.01250197519594));
#370933=CARTESIAN_POINT('Ctrl Pts',(-0.829403791936599,0.478856502541492,
3.05000197519594));
#370934=CARTESIAN_POINT('Ctrl Pts',(-1.10587172258213,-5.98848532837832E-17,
3.08750197519594));
#370935=CARTESIAN_POINT('Ctrl Pts',(-0.829403791936599,-0.478856502541491,
3.12500197519594));
#370936=CARTESIAN_POINT('Ctrl Pts',(-0.552935861291066,-0.957713005082983,
3.16250197519594));
#370937=CARTESIAN_POINT('Ctrl Pts',(-1.17286016617667E-16,-0.957713005082983,
3.20000197519594));
#370938=CARTESIAN_POINT('Ctrl Pts',(0.552935861291066,-0.957713005082984,
3.23750197519594));
#370939=CARTESIAN_POINT('Ctrl Pts',(0.829403791936598,-0.478856502541492,
3.27500197519594));
#370940=CARTESIAN_POINT('Ctrl Pts',(1.10587172258213,-3.30544007027506E-16,
3.31250197519594));
#370941=CARTESIAN_POINT('Ctrl Pts',(0.829403791936599,0.478856502541491,
3.35000197519594));
#370942=CARTESIAN_POINT('Ctrl Pts',(0.552935861291066,0.957713005082983,
3.38750197519594));
#370943=CARTESIAN_POINT('Ctrl Pts',(0.,0.957713005082983,3.42500197519594));
#370944=CARTESIAN_POINT('Ctrl Pts',(-0.552935861291066,0.957713005082983,
3.46250197519594));
#370945=CARTESIAN_POINT('Ctrl Pts',(-0.829403791936599,0.478856502541492,
3.50000197519594));
#370946=CARTESIAN_POINT('Ctrl Pts',(-1.10587172258213,-5.94822546401172E-17,
3.53750197519594));
#370947=CARTESIAN_POINT('Ctrl Pts',(-0.829403791936599,-0.478856502541491,
3.57500197519594));
#370948=CARTESIAN_POINT('Ctrl Pts',(-0.552935861291066,-0.957713005082983,
3.61250197519594));
#370949=CARTESIAN_POINT('Ctrl Pts',(-1.17286016617667E-16,-0.957713005082983,
3.65000197519594));
#370950=CARTESIAN_POINT('Ctrl Pts',(0.552935861291066,-0.957713005082984,
3.68750197519594));
#370951=CARTESIAN_POINT('Ctrl Pts',(0.829403791936598,-0.478856502541492,
3.72500197519594));
#370952=CARTESIAN_POINT('Ctrl Pts',(1.0036847708126,-0.176992992335418,
3.74864137775736));
#370953=CARTESIAN_POINT('Ctrl Pts',(0.943168426706962,0.166275431041969,
3.77552326368421));
#370954=CARTESIAN_POINT('Ctrl Pts',(0.848846015356109,0.701302883742039,
3.81742209844946));
#370955=CARTESIAN_POINT('Ctrl Pts',(0.754523604005256,1.23633033644211,
3.85932093321471));
#370956=CARTESIAN_POINT('Ctrl Pts',(0.,1.27435696448144,-4.40781250000002));
#370957=CARTESIAN_POINT('Ctrl Pts',(-0.735750336487031,1.27435696448144,
-4.37031250000002));
#370958=CARTESIAN_POINT('Ctrl Pts',(-1.10362550473055,0.637178482240718,
-4.33281250000002));
#370959=CARTESIAN_POINT('Ctrl Pts',(-1.47150067297406,-4.41016728599111E-17,
-4.29531250000002));
#370960=CARTESIAN_POINT('Ctrl Pts',(-1.10362550473055,-0.637178482240718,
-4.25781250000002));
#370961=CARTESIAN_POINT('Ctrl Pts',(-0.735750336487032,-1.27435696448144,
-4.22031250000002));
#370962=CARTESIAN_POINT('Ctrl Pts',(-1.56063717752333E-16,-1.27435696448144,
-4.18281250000002));
#370963=CARTESIAN_POINT('Ctrl Pts',(0.735750336487031,-1.27435696448144,
-4.14531250000002));
#370964=CARTESIAN_POINT('Ctrl Pts',(1.10362550473055,-0.637178482240719,
-4.10781250000002));
#370965=CARTESIAN_POINT('Ctrl Pts',(1.47150067297406,-4.0431409135825E-16,
-4.07031250000002));
#370966=CARTESIAN_POINT('Ctrl Pts',(1.10362550473055,0.637178482240717,
-4.03281250000002));
#370967=CARTESIAN_POINT('Ctrl Pts',(0.735750336487032,1.27435696448144,
-3.99531250000002));
#370968=CARTESIAN_POINT('Ctrl Pts',(0.,1.27435696448144,-3.95781250000002));
#370969=CARTESIAN_POINT('Ctrl Pts',(-0.735750336487031,1.27435696448144,
-3.92031250000002));
#370970=CARTESIAN_POINT('Ctrl Pts',(-1.10362550473055,0.637178482240718,
-3.88281250000002));
#370971=CARTESIAN_POINT('Ctrl Pts',(-1.47150067297406,-4.3699074216245E-17,
-3.84531250000002));
#370972=CARTESIAN_POINT('Ctrl Pts',(-1.10362550473055,-0.637178482240718,
-3.80781250000002));
#370973=CARTESIAN_POINT('Ctrl Pts',(-0.735750336487032,-1.27435696448144,
-3.77031250000002));
#370974=CARTESIAN_POINT('Ctrl Pts',(-1.56063717752333E-16,-1.27435696448144,
-3.73281250000002));
#370975=CARTESIAN_POINT('Ctrl Pts',(0.735750336487031,-1.27435696448144,
-3.69531250000002));
#370976=CARTESIAN_POINT('Ctrl Pts',(1.10362550473055,-0.637178482240719,
-3.65781250000002));
#370977=CARTESIAN_POINT('Ctrl Pts',(1.47150067297406,-4.03911492714584E-16,
-3.62031250000002));
#370978=CARTESIAN_POINT('Ctrl Pts',(1.10362550473055,0.637178482240717,
-3.58281250000002));
#370979=CARTESIAN_POINT('Ctrl Pts',(0.735750336487032,1.27435696448144,
-3.54531250000002));
#370980=CARTESIAN_POINT('Ctrl Pts',(0.,1.27435696448144,-3.50781250000002));
#370981=CARTESIAN_POINT('Ctrl Pts',(-0.735750336487031,1.27435696448144,
-3.47031250000002));
#370982=CARTESIAN_POINT('Ctrl Pts',(-1.10362550473055,0.637178482240718,
-3.43281250000002));
#370983=CARTESIAN_POINT('Ctrl Pts',(-1.47150067297406,-4.3296475572579E-17,
-3.39531250000002));
#370984=CARTESIAN_POINT('Ctrl Pts',(-1.10362550473055,-0.637178482240718,
-3.35781250000002));
#370985=CARTESIAN_POINT('Ctrl Pts',(-0.735750336487032,-1.27435696448144,
-3.32031250000002));
#370986=CARTESIAN_POINT('Ctrl Pts',(-1.56063717752333E-16,-1.27435696448144,
-3.28281250000002));
#370987=CARTESIAN_POINT('Ctrl Pts',(0.735750336487031,-1.27435696448144,
-3.24531250000002));
#370988=CARTESIAN_POINT('Ctrl Pts',(1.10362550473055,-0.637178482240719,
-3.20781250000002));
#370989=CARTESIAN_POINT('Ctrl Pts',(1.47150067297406,-4.03508894070918E-16,
-3.17031250000002));
#370990=CARTESIAN_POINT('Ctrl Pts',(1.10362550473055,0.637178482240717,
-3.13281250000002));
#370991=CARTESIAN_POINT('Ctrl Pts',(0.735750336487032,1.27435696448144,
-3.09531250000002));
#370992=CARTESIAN_POINT('Ctrl Pts',(0.,1.27435696448144,-3.05781250000002));
#370993=CARTESIAN_POINT('Ctrl Pts',(-0.735750336487031,1.27435696448144,
-3.02031250000002));
#370994=CARTESIAN_POINT('Ctrl Pts',(-1.10362550473055,0.637178482240718,
-2.98281250000002));
#370995=CARTESIAN_POINT('Ctrl Pts',(-1.47150067297406,-4.28938769289129E-17,
-2.94531250000002));
#370996=CARTESIAN_POINT('Ctrl Pts',(-1.10362550473055,-0.637178482240718,
-2.90781250000002));
#370997=CARTESIAN_POINT('Ctrl Pts',(-0.735750336487032,-1.27435696448144,
-2.87031250000002));
#370998=CARTESIAN_POINT('Ctrl Pts',(-1.56063717752333E-16,-1.27435696448144,
-2.83281250000002));
#370999=CARTESIAN_POINT('Ctrl Pts',(0.735750336487031,-1.27435696448144,
-2.79531250000002));
#371000=CARTESIAN_POINT('Ctrl Pts',(1.10362550473055,-0.637178482240719,
-2.75781250000002));
#371001=CARTESIAN_POINT('Ctrl Pts',(1.47150067297406,-4.03106295427252E-16,
-2.72031250000002));
#371002=CARTESIAN_POINT('Ctrl Pts',(1.10362550473055,0.637178482240717,
-2.68281250000002));
#371003=CARTESIAN_POINT('Ctrl Pts',(0.735750336487032,1.27435696448144,
-2.64531250000002));
#371004=CARTESIAN_POINT('Ctrl Pts',(0.,1.27435696448144,-2.60781250000002));
#371005=CARTESIAN_POINT('Ctrl Pts',(-0.735750336487031,1.27435696448144,
-2.57031250000002));
#371006=CARTESIAN_POINT('Ctrl Pts',(-1.10362550473055,0.637178482240718,
-2.53281250000002));
#371007=CARTESIAN_POINT('Ctrl Pts',(-1.47150067297406,-4.24912782852469E-17,
-2.49531250000002));
#371008=CARTESIAN_POINT('Ctrl Pts',(-1.10362550473055,-0.637178482240718,
-2.45781250000002));
#371009=CARTESIAN_POINT('Ctrl Pts',(-0.735750336487032,-1.27435696448144,
-2.42031250000002));
#371010=CARTESIAN_POINT('Ctrl Pts',(-1.56063717752333E-16,-1.27435696448144,
-2.38281250000002));
#371011=CARTESIAN_POINT('Ctrl Pts',(0.735750336487031,-1.27435696448144,
-2.34531250000002));
#371012=CARTESIAN_POINT('Ctrl Pts',(1.10362550473055,-0.637178482240719,
-2.30781250000002));
#371013=CARTESIAN_POINT('Ctrl Pts',(1.47150067297406,-4.02703696783586E-16,
-2.27031250000002));
#371014=CARTESIAN_POINT('Ctrl Pts',(1.10362550473055,0.637178482240717,
-2.23281250000002));
#371015=CARTESIAN_POINT('Ctrl Pts',(0.735750336487032,1.27435696448144,
-2.19531250000002));
#371016=CARTESIAN_POINT('Ctrl Pts',(0.,1.27435696448144,-2.15781250000002));
#371017=CARTESIAN_POINT('Ctrl Pts',(-0.735750336487031,1.27435696448144,
-2.12031250000002));
#371018=CARTESIAN_POINT('Ctrl Pts',(-1.10362550473055,0.637178482240718,
-2.08281250000002));
#371019=CARTESIAN_POINT('Ctrl Pts',(-1.47150067297406,-4.20886796415808E-17,
-2.04531250000002));
#371020=CARTESIAN_POINT('Ctrl Pts',(-1.10362550473055,-0.637178482240718,
-2.00781250000002));
#371021=CARTESIAN_POINT('Ctrl Pts',(-0.735750336487032,-1.27435696448144,
-1.97031250000002));
#371022=CARTESIAN_POINT('Ctrl Pts',(-1.56063717752333E-16,-1.27435696448144,
-1.93281250000002));
#371023=CARTESIAN_POINT('Ctrl Pts',(0.735750336487031,-1.27435696448144,
-1.89531250000002));
#371024=CARTESIAN_POINT('Ctrl Pts',(1.10362550473055,-0.637178482240719,
-1.85781250000002));
#371025=CARTESIAN_POINT('Ctrl Pts',(1.47150067297406,-4.0230109813992E-16,
-1.82031250000002));
#371026=CARTESIAN_POINT('Ctrl Pts',(1.10362550473055,0.637178482240717,
-1.78281250000002));
#371027=CARTESIAN_POINT('Ctrl Pts',(0.735750336487032,1.27435696448144,
-1.74531250000002));
#371028=CARTESIAN_POINT('Ctrl Pts',(0.,1.27435696448144,-1.70781250000002));
#371029=CARTESIAN_POINT('Ctrl Pts',(-0.735750336487031,1.27435696448144,
-1.67031250000002));
#371030=CARTESIAN_POINT('Ctrl Pts',(-1.10362550473055,0.637178482240718,
-1.63281250000002));
#371031=CARTESIAN_POINT('Ctrl Pts',(-1.47150067297406,-4.16860809979148E-17,
-1.59531250000002));
#371032=CARTESIAN_POINT('Ctrl Pts',(-1.10362550473055,-0.637178482240718,
-1.55781250000002));
#371033=CARTESIAN_POINT('Ctrl Pts',(-0.735750336487032,-1.27435696448144,
-1.52031250000002));
#371034=CARTESIAN_POINT('Ctrl Pts',(-1.56063717752333E-16,-1.27435696448144,
-1.48281250000002));
#371035=CARTESIAN_POINT('Ctrl Pts',(0.735750336487031,-1.27435696448144,
-1.44531250000002));
#371036=CARTESIAN_POINT('Ctrl Pts',(1.10362550473055,-0.637178482240719,
-1.40781250000002));
#371037=CARTESIAN_POINT('Ctrl Pts',(1.47150067297406,-4.01898499496254E-16,
-1.37031250000002));
#371038=CARTESIAN_POINT('Ctrl Pts',(1.10362550473055,0.637178482240717,
-1.33281250000002));
#371039=CARTESIAN_POINT('Ctrl Pts',(0.735750336487032,1.27435696448144,
-1.29531250000002));
#371040=CARTESIAN_POINT('Ctrl Pts',(0.,1.27435696448144,-1.25781250000002));
#371041=CARTESIAN_POINT('Ctrl Pts',(-0.735750336487031,1.27435696448144,
-1.22031250000002));
#371042=CARTESIAN_POINT('Ctrl Pts',(-1.10362550473055,0.637178482240718,
-1.18281250000002));
#371043=CARTESIAN_POINT('Ctrl Pts',(-1.47150067297406,-4.12834823542487E-17,
-1.14531250000002));
#371044=CARTESIAN_POINT('Ctrl Pts',(-1.10362550473055,-0.637178482240718,
-1.10781250000002));
#371045=CARTESIAN_POINT('Ctrl Pts',(-0.735750336487032,-1.27435696448144,
-1.07031250000002));
#371046=CARTESIAN_POINT('Ctrl Pts',(-1.56063717752333E-16,-1.27435696448144,
-1.03281250000002));
#371047=CARTESIAN_POINT('Ctrl Pts',(0.735750336487031,-1.27435696448144,
-0.995312500000018));
#371048=CARTESIAN_POINT('Ctrl Pts',(1.10362550473055,-0.637178482240719,
-0.957812500000018));
#371049=CARTESIAN_POINT('Ctrl Pts',(1.47150067297406,-4.01495900852588E-16,
-0.920312500000018));
#371050=CARTESIAN_POINT('Ctrl Pts',(1.10362550473055,0.637178482240717,
-0.882812500000018));
#371051=CARTESIAN_POINT('Ctrl Pts',(0.735750336487032,1.27435696448144,
-0.845312500000018));
#371052=CARTESIAN_POINT('Ctrl Pts',(0.,1.27435696448144,-0.807812500000018));
#371053=CARTESIAN_POINT('Ctrl Pts',(-0.735750336487031,1.27435696448144,
-0.770312500000018));
#371054=CARTESIAN_POINT('Ctrl Pts',(-1.10362550473055,0.637178482240718,
-0.732812500000018));
#371055=CARTESIAN_POINT('Ctrl Pts',(-1.47150067297406,-4.08808837105827E-17,
-0.695312500000018));
#371056=CARTESIAN_POINT('Ctrl Pts',(-1.10362550473055,-0.637178482240718,
-0.657812500000018));
#371057=CARTESIAN_POINT('Ctrl Pts',(-0.735750336487032,-1.27435696448144,
-0.620312500000018));
#371058=CARTESIAN_POINT('Ctrl Pts',(-1.56063717752333E-16,-1.27435696448144,
-0.582812500000018));
#371059=CARTESIAN_POINT('Ctrl Pts',(0.735750336487031,-1.27435696448144,
-0.545312500000018));
#371060=CARTESIAN_POINT('Ctrl Pts',(1.10362550473055,-0.637178482240719,
-0.507812500000018));
#371061=CARTESIAN_POINT('Ctrl Pts',(1.47150067297406,-4.01093302208922E-16,
-0.470312500000018));
#371062=CARTESIAN_POINT('Ctrl Pts',(1.10362550473055,0.637178482240717,
-0.432812500000018));
#371063=CARTESIAN_POINT('Ctrl Pts',(0.735750336487032,1.27435696448144,
-0.395312500000018));
#371064=CARTESIAN_POINT('Ctrl Pts',(0.,1.27435696448144,-0.357812500000018));
#371065=CARTESIAN_POINT('Ctrl Pts',(-0.735750336487031,1.27435696448144,
-0.320312500000018));
#371066=CARTESIAN_POINT('Ctrl Pts',(-1.10362550473055,0.637178482240718,
-0.282812500000018));
#371067=CARTESIAN_POINT('Ctrl Pts',(-1.47150067297406,-4.04782850669166E-17,
-0.245312500000018));
#371068=CARTESIAN_POINT('Ctrl Pts',(-1.10362550473055,-0.637178482240718,
-0.207812500000018));
#371069=CARTESIAN_POINT('Ctrl Pts',(-0.735750336487032,-1.27435696448144,
-0.170312500000018));
#371070=CARTESIAN_POINT('Ctrl Pts',(-1.56063717752333E-16,-1.27435696448144,
-0.132812500000018));
#371071=CARTESIAN_POINT('Ctrl Pts',(0.735750336487031,-1.27435696448144,
-0.0953125000000181));
#371072=CARTESIAN_POINT('Ctrl Pts',(1.10362550473055,-0.637178482240719,
-0.0578125000000179));
#371073=CARTESIAN_POINT('Ctrl Pts',(1.47150067297406,-4.00690703565256E-16,
-0.0203125000000177));
#371074=CARTESIAN_POINT('Ctrl Pts',(1.10362550473055,0.637178482240717,
0.0171874999999816));
#371075=CARTESIAN_POINT('Ctrl Pts',(0.735750336487032,1.27435696448144,
0.0546874999999818));
#371076=CARTESIAN_POINT('Ctrl Pts',(0.,1.27435696448144,0.0921874999999821));
#371077=CARTESIAN_POINT('Ctrl Pts',(-0.735750336487031,1.27435696448144,
0.129687499999982));
#371078=CARTESIAN_POINT('Ctrl Pts',(-1.10362550473055,0.637178482240718,
0.167187499999982));
#371079=CARTESIAN_POINT('Ctrl Pts',(-1.47150067297406,-4.00756864232506E-17,
0.204687499999982));
#371080=CARTESIAN_POINT('Ctrl Pts',(-1.10362550473055,-0.637178482240718,
0.242187499999982));
#371081=CARTESIAN_POINT('Ctrl Pts',(-0.735750336487032,-1.27435696448144,
0.279687499999982));
#371082=CARTESIAN_POINT('Ctrl Pts',(-1.56063717752333E-16,-1.27435696448144,
0.317187499999982));
#371083=CARTESIAN_POINT('Ctrl Pts',(0.735750336487031,-1.27435696448144,
0.354687499999982));
#371084=CARTESIAN_POINT('Ctrl Pts',(1.10362550473055,-0.637178482240719,
0.392187499999982));
#371085=CARTESIAN_POINT('Ctrl Pts',(1.47150067297406,-4.0028810492159E-16,
0.429687499999982));
#371086=CARTESIAN_POINT('Ctrl Pts',(1.10362550473055,0.637178482240717,
0.467187499999982));
#371087=CARTESIAN_POINT('Ctrl Pts',(0.735750336487032,1.27435696448144,
0.504687499999982));
#371088=CARTESIAN_POINT('Ctrl Pts',(0.,1.27435696448144,0.542187499999982));
#371089=CARTESIAN_POINT('Ctrl Pts',(-0.735750336487031,1.27435696448144,
0.579687499999982));
#371090=CARTESIAN_POINT('Ctrl Pts',(-1.10362550473055,0.637178482240718,
0.617187499999982));
#371091=CARTESIAN_POINT('Ctrl Pts',(-1.47150067297406,-3.96730877795845E-17,
0.654687499999982));
#371092=CARTESIAN_POINT('Ctrl Pts',(-1.10362550473055,-0.637178482240718,
0.692187499999982));
#371093=CARTESIAN_POINT('Ctrl Pts',(-0.735750336487032,-1.27435696448144,
0.729687499999982));
#371094=CARTESIAN_POINT('Ctrl Pts',(-1.56063717752333E-16,-1.27435696448144,
0.767187499999982));
#371095=CARTESIAN_POINT('Ctrl Pts',(0.735750336487031,-1.27435696448144,
0.804687499999982));
#371096=CARTESIAN_POINT('Ctrl Pts',(1.10362550473055,-0.637178482240719,
0.842187499999982));
#371097=CARTESIAN_POINT('Ctrl Pts',(1.47150067297406,-3.99885506277924E-16,
0.879687499999982));
#371098=CARTESIAN_POINT('Ctrl Pts',(1.10362550473055,0.637178482240717,
0.917187499999982));
#371099=CARTESIAN_POINT('Ctrl Pts',(0.735750336487032,1.27435696448144,
0.954687499999982));
#371100=CARTESIAN_POINT('Ctrl Pts',(0.,1.27435696448144,0.992187499999982));
#371101=CARTESIAN_POINT('Ctrl Pts',(-0.735750336487031,1.27435696448144,
1.02968749999998));
#371102=CARTESIAN_POINT('Ctrl Pts',(-1.10362550473055,0.637178482240718,
1.06718749999998));
#371103=CARTESIAN_POINT('Ctrl Pts',(-1.47150067297406,-3.92704891359185E-17,
1.10468749999998));
#371104=CARTESIAN_POINT('Ctrl Pts',(-1.10362550473055,-0.637178482240718,
1.14218749999998));
#371105=CARTESIAN_POINT('Ctrl Pts',(-0.735750336487032,-1.27435696448144,
1.17968749999998));
#371106=CARTESIAN_POINT('Ctrl Pts',(-1.56063717752333E-16,-1.27435696448144,
1.21718749999998));
#371107=CARTESIAN_POINT('Ctrl Pts',(0.735750336487031,-1.27435696448144,
1.25468749999998));
#371108=CARTESIAN_POINT('Ctrl Pts',(1.10362550473055,-0.637178482240719,
1.29218749999998));
#371109=CARTESIAN_POINT('Ctrl Pts',(1.47150067297406,-3.99482907634258E-16,
1.32968749999998));
#371110=CARTESIAN_POINT('Ctrl Pts',(1.10362550473055,0.637178482240717,
1.36718749999998));
#371111=CARTESIAN_POINT('Ctrl Pts',(0.735750336487032,1.27435696448144,
1.40468749999998));
#371112=CARTESIAN_POINT('Ctrl Pts',(0.,1.27435696448144,1.44218749999998));
#371113=CARTESIAN_POINT('Ctrl Pts',(-0.735750336487031,1.27435696448144,
1.47968749999998));
#371114=CARTESIAN_POINT('Ctrl Pts',(-1.10362550473055,0.637178482240718,
1.51718749999998));
#371115=CARTESIAN_POINT('Ctrl Pts',(-1.47150067297406,-3.88678904922525E-17,
1.55468749999998));
#371116=CARTESIAN_POINT('Ctrl Pts',(-1.10362550473055,-0.637178482240718,
1.59218749999998));
#371117=CARTESIAN_POINT('Ctrl Pts',(-0.735750336487032,-1.27435696448144,
1.62968749999998));
#371118=CARTESIAN_POINT('Ctrl Pts',(-1.56063717752333E-16,-1.27435696448144,
1.66718749999998));
#371119=CARTESIAN_POINT('Ctrl Pts',(0.735750336487031,-1.27435696448144,
1.70468749999998));
#371120=CARTESIAN_POINT('Ctrl Pts',(1.10362550473055,-0.637178482240719,
1.74218749999998));
#371121=CARTESIAN_POINT('Ctrl Pts',(1.47150067297406,-3.99080308990592E-16,
1.77968749999998));
#371122=CARTESIAN_POINT('Ctrl Pts',(1.10362550473055,0.637178482240717,
1.81718749999998));
#371123=CARTESIAN_POINT('Ctrl Pts',(0.735750336487032,1.27435696448144,
1.85468749999998));
#371124=CARTESIAN_POINT('Ctrl Pts',(0.,1.27435696448144,1.89218749999998));
#371125=CARTESIAN_POINT('Ctrl Pts',(-0.735750336487031,1.27435696448144,
1.92968749999998));
#371126=CARTESIAN_POINT('Ctrl Pts',(-1.10362550473055,0.637178482240718,
1.96718749999998));
#371127=CARTESIAN_POINT('Ctrl Pts',(-1.47150067297406,-3.84652918485864E-17,
2.00468749999998));
#371128=CARTESIAN_POINT('Ctrl Pts',(-1.10362550473055,-0.637178482240718,
2.04218749999998));
#371129=CARTESIAN_POINT('Ctrl Pts',(-0.735750336487032,-1.27435696448144,
2.07968749999998));
#371130=CARTESIAN_POINT('Ctrl Pts',(-1.56063717752333E-16,-1.27435696448144,
2.11718749999998));
#371131=CARTESIAN_POINT('Ctrl Pts',(0.735750336487031,-1.27435696448144,
2.15468749999998));
#371132=CARTESIAN_POINT('Ctrl Pts',(1.10362550473055,-0.637178482240719,
2.19218749999998));
#371133=CARTESIAN_POINT('Ctrl Pts',(1.47150067297406,-3.98677710346926E-16,
2.22968749999998));
#371134=CARTESIAN_POINT('Ctrl Pts',(1.10362550473055,0.637178482240717,
2.26718749999998));
#371135=CARTESIAN_POINT('Ctrl Pts',(0.735750336487032,1.27435696448144,
2.30468749999998));
#371136=CARTESIAN_POINT('Ctrl Pts',(0.,1.27435696448144,2.34218749999998));
#371137=CARTESIAN_POINT('Ctrl Pts',(-0.735750336487031,1.27435696448144,
2.37968749999998));
#371138=CARTESIAN_POINT('Ctrl Pts',(-1.10362550473055,0.637178482240718,
2.41718749999998));
#371139=CARTESIAN_POINT('Ctrl Pts',(-1.47150067297406,-3.80626932049204E-17,
2.45468749999998));
#371140=CARTESIAN_POINT('Ctrl Pts',(-1.10362550473055,-0.637178482240718,
2.49218749999998));
#371141=CARTESIAN_POINT('Ctrl Pts',(-0.735750336487032,-1.27435696448144,
2.52968749999998));
#371142=CARTESIAN_POINT('Ctrl Pts',(-1.56063717752333E-16,-1.27435696448144,
2.56718749999998));
#371143=CARTESIAN_POINT('Ctrl Pts',(0.735750336487031,-1.27435696448144,
2.60468749999998));
#371144=CARTESIAN_POINT('Ctrl Pts',(1.10362550473055,-0.637178482240719,
2.64218749999998));
#371145=CARTESIAN_POINT('Ctrl Pts',(1.47150067297406,-3.9827511170326E-16,
2.67968749999998));
#371146=CARTESIAN_POINT('Ctrl Pts',(1.10362550473055,0.637178482240717,
2.71718749999998));
#371147=CARTESIAN_POINT('Ctrl Pts',(0.735750336487032,1.27435696448144,
2.75468749999998));
#371148=CARTESIAN_POINT('Ctrl Pts',(0.,1.27435696448144,2.79218749999998));
#371149=CARTESIAN_POINT('Ctrl Pts',(-0.735750336487031,1.27435696448144,
2.82968749999998));
#371150=CARTESIAN_POINT('Ctrl Pts',(-1.10362550473055,0.637178482240718,
2.86718749999998));
#371151=CARTESIAN_POINT('Ctrl Pts',(-1.47150067297406,-3.76600945612543E-17,
2.90468749999998));
#371152=CARTESIAN_POINT('Ctrl Pts',(-1.10362550473055,-0.637178482240718,
2.94218749999998));
#371153=CARTESIAN_POINT('Ctrl Pts',(-0.735750336487032,-1.27435696448144,
2.97968749999998));
#371154=CARTESIAN_POINT('Ctrl Pts',(-1.56063717752333E-16,-1.27435696448144,
3.01718749999998));
#371155=CARTESIAN_POINT('Ctrl Pts',(0.735750336487031,-1.27435696448144,
3.05468749999998));
#371156=CARTESIAN_POINT('Ctrl Pts',(1.10362550473055,-0.637178482240719,
3.09218749999998));
#371157=CARTESIAN_POINT('Ctrl Pts',(1.47150067297406,-3.97872513059594E-16,
3.12968749999998));
#371158=CARTESIAN_POINT('Ctrl Pts',(1.10362550473055,0.637178482240717,
3.16718749999998));
#371159=CARTESIAN_POINT('Ctrl Pts',(0.735750336487032,1.27435696448144,
3.20468749999998));
#371160=CARTESIAN_POINT('Ctrl Pts',(0.,1.27435696448144,3.24218749999998));
#371161=CARTESIAN_POINT('Ctrl Pts',(-0.735750336487031,1.27435696448144,
3.27968749999998));
#371162=CARTESIAN_POINT('Ctrl Pts',(-1.10362550473055,0.637178482240718,
3.31718749999998));
#371163=CARTESIAN_POINT('Ctrl Pts',(-1.47150067297406,-3.72574959175883E-17,
3.35468749999998));
#371164=CARTESIAN_POINT('Ctrl Pts',(-1.10362550473055,-0.637178482240718,
3.39218749999998));
#371165=CARTESIAN_POINT('Ctrl Pts',(-0.735750336487032,-1.27435696448144,
3.42968749999998));
#371166=CARTESIAN_POINT('Ctrl Pts',(-1.56063717752333E-16,-1.27435696448144,
3.46718749999998));
#371167=CARTESIAN_POINT('Ctrl Pts',(0.735750336487031,-1.27435696448144,
3.50468749999998));
#371168=CARTESIAN_POINT('Ctrl Pts',(1.10362550473055,-0.637178482240719,
3.54218749999998));
#371169=CARTESIAN_POINT('Ctrl Pts',(1.33552814991602,-0.235511318369856,
3.56582690256139));
#371170=CARTESIAN_POINT('Ctrl Pts',(1.25500358340531,0.221250262287215,
3.59270878848825));
#371171=CARTESIAN_POINT('Ctrl Pts',(1.12949581523918,0.933171220777297,
3.6346076232535));
#371172=CARTESIAN_POINT('Ctrl Pts',(1.00398804707305,1.64509217926738,3.67650645801875));
#371173=CARTESIAN_POINT('Origin',(1.38777878078145E-16,1.38777878078145E-16,
-4.19687500000002));
#371174=CARTESIAN_POINT('Ctrl Pts',(-0.155365792422873,-0.945030276552907,
-3.95478357377727));
#371175=CARTESIAN_POINT('Ctrl Pts',(-0.0782008300208539,-0.957716426222737,
-3.94905354577365));
#371176=CARTESIAN_POINT('Ctrl Pts',(-1.17286435586452E-16,-0.957716426222737,
-3.94375000000002));
#371177=CARTESIAN_POINT('Ctrl Pts',(0.,1.27435696448144,-3.98593750000002));
#371178=CARTESIAN_POINT('Ctrl Pts',(-0.735750336487031,1.27435696448144,
-3.94843750000002));
#371179=CARTESIAN_POINT('Ctrl Pts',(-1.10362550473055,0.637178482240718,
-3.91093750000002));
#371180=CARTESIAN_POINT('Ctrl Pts',(-1.47150067297406,-4.37242366314742E-17,
-3.87343750000002));
#371181=CARTESIAN_POINT('Ctrl Pts',(-1.10362550473055,-0.637178482240718,
-3.83593750000002));
#371182=CARTESIAN_POINT('Ctrl Pts',(-0.735750336487032,-1.27435696448144,
-3.79843750000002));
#371183=CARTESIAN_POINT('Ctrl Pts',(-1.56063717752333E-16,-1.27435696448144,
-3.76093750000002));
#371184=CARTESIAN_POINT('Ctrl Pts',(0.735750336487031,-1.27435696448144,
-3.72343750000002));
#371185=CARTESIAN_POINT('Ctrl Pts',(1.10362550473055,-0.637178482240719,
-3.68593750000002));
#371186=CARTESIAN_POINT('Ctrl Pts',(1.47150067297406,-4.03936655129813E-16,
-3.64843750000002));
#371187=CARTESIAN_POINT('Ctrl Pts',(1.10362550473055,0.637178482240717,
-3.61093750000002));
#371188=CARTESIAN_POINT('Ctrl Pts',(0.735750336487032,1.27435696448144,
-3.57343750000002));
#371189=CARTESIAN_POINT('Ctrl Pts',(0.,1.27435696448144,-3.53593750000002));
#371190=CARTESIAN_POINT('Ctrl Pts',(-0.735750336487031,1.27435696448144,
-3.49843750000002));
#371191=CARTESIAN_POINT('Ctrl Pts',(-1.10362550473055,0.637178482240718,
-3.46093750000002));
#371192=CARTESIAN_POINT('Ctrl Pts',(-1.47150067297406,-4.33216379878081E-17,
-3.42343750000002));
#371193=CARTESIAN_POINT('Ctrl Pts',(-1.10362550473055,-0.637178482240718,
-3.38593750000002));
#371194=CARTESIAN_POINT('Ctrl Pts',(-0.735750336487032,-1.27435696448144,
-3.34843750000002));
#371195=CARTESIAN_POINT('Ctrl Pts',(-1.56063717752333E-16,-1.27435696448144,
-3.31093750000002));
#371196=CARTESIAN_POINT('Ctrl Pts',(0.735750336487031,-1.27435696448144,
-3.27343750000002));
#371197=CARTESIAN_POINT('Ctrl Pts',(1.10362550473055,-0.637178482240719,
-3.23593750000002));
#371198=CARTESIAN_POINT('Ctrl Pts',(1.47150067297406,-4.03534056486148E-16,
-3.19843750000002));
#371199=CARTESIAN_POINT('Ctrl Pts',(1.10362550473055,0.637178482240717,
-3.16093750000002));
#371200=CARTESIAN_POINT('Ctrl Pts',(0.735750336487032,1.27435696448144,
-3.12343750000002));
#371201=CARTESIAN_POINT('Ctrl Pts',(0.,1.27435696448144,-3.08593750000002));
#371202=CARTESIAN_POINT('Ctrl Pts',(-0.735750336487031,1.27435696448144,
-3.04843750000002));
#371203=CARTESIAN_POINT('Ctrl Pts',(-1.10362550473055,0.637178482240718,
-3.01093750000002));
#371204=CARTESIAN_POINT('Ctrl Pts',(-1.47150067297406,-4.29190393441421E-17,
-2.97343750000002));
#371205=CARTESIAN_POINT('Ctrl Pts',(-1.10362550473055,-0.637178482240718,
-2.93593750000002));
#371206=CARTESIAN_POINT('Ctrl Pts',(-0.735750336487032,-1.27435696448144,
-2.89843750000002));
#371207=CARTESIAN_POINT('Ctrl Pts',(-1.56063717752333E-16,-1.27435696448144,
-2.86093750000002));
#371208=CARTESIAN_POINT('Ctrl Pts',(0.735750336487031,-1.27435696448144,
-2.82343750000002));
#371209=CARTESIAN_POINT('Ctrl Pts',(1.10362550473055,-0.637178482240719,
-2.78593750000002));
#371210=CARTESIAN_POINT('Ctrl Pts',(1.47150067297406,-4.03131457842481E-16,
-2.74843750000002));
#371211=CARTESIAN_POINT('Ctrl Pts',(1.10362550473055,0.637178482240717,
-2.71093750000002));
#371212=CARTESIAN_POINT('Ctrl Pts',(0.735750336487032,1.27435696448144,
-2.67343750000002));
#371213=CARTESIAN_POINT('Ctrl Pts',(0.,1.27435696448144,-2.63593750000002));
#371214=CARTESIAN_POINT('Ctrl Pts',(-0.735750336487031,1.27435696448144,
-2.59843750000002));
#371215=CARTESIAN_POINT('Ctrl Pts',(-1.10362550473055,0.637178482240718,
-2.56093750000002));
#371216=CARTESIAN_POINT('Ctrl Pts',(-1.47150067297406,-4.2516440700476E-17,
-2.52343750000002));
#371217=CARTESIAN_POINT('Ctrl Pts',(-1.10362550473055,-0.637178482240718,
-2.48593750000002));
#371218=CARTESIAN_POINT('Ctrl Pts',(-0.735750336487032,-1.27435696448144,
-2.44843750000002));
#371219=CARTESIAN_POINT('Ctrl Pts',(-1.56063717752333E-16,-1.27435696448144,
-2.41093750000002));
#371220=CARTESIAN_POINT('Ctrl Pts',(0.735750336487031,-1.27435696448144,
-2.37343750000002));
#371221=CARTESIAN_POINT('Ctrl Pts',(1.10362550473055,-0.637178482240719,
-2.33593750000002));
#371222=CARTESIAN_POINT('Ctrl Pts',(1.47150067297406,-4.02728859198815E-16,
-2.29843750000002));
#371223=CARTESIAN_POINT('Ctrl Pts',(1.10362550473055,0.637178482240717,
-2.26093750000002));
#371224=CARTESIAN_POINT('Ctrl Pts',(0.735750336487032,1.27435696448144,
-2.22343750000002));
#371225=CARTESIAN_POINT('Ctrl Pts',(0.,1.27435696448144,-2.18593750000002));
#371226=CARTESIAN_POINT('Ctrl Pts',(-0.735750336487031,1.27435696448144,
-2.14843750000002));
#371227=CARTESIAN_POINT('Ctrl Pts',(-1.10362550473055,0.637178482240718,
-2.11093750000002));
#371228=CARTESIAN_POINT('Ctrl Pts',(-1.47150067297406,-4.211384205681E-17,
-2.07343750000002));
#371229=CARTESIAN_POINT('Ctrl Pts',(-1.10362550473055,-0.637178482240718,
-2.03593750000002));
#371230=CARTESIAN_POINT('Ctrl Pts',(-0.735750336487032,-1.27435696448144,
-1.99843750000002));
#371231=CARTESIAN_POINT('Ctrl Pts',(-1.56063717752333E-16,-1.27435696448144,
-1.96093750000002));
#371232=CARTESIAN_POINT('Ctrl Pts',(0.735750336487031,-1.27435696448144,
-1.92343750000002));
#371233=CARTESIAN_POINT('Ctrl Pts',(1.10362550473055,-0.637178482240719,
-1.88593750000002));
#371234=CARTESIAN_POINT('Ctrl Pts',(1.47150067297406,-4.02326260555149E-16,
-1.84843750000002));
#371235=CARTESIAN_POINT('Ctrl Pts',(1.10362550473055,0.637178482240717,
-1.81093750000002));
#371236=CARTESIAN_POINT('Ctrl Pts',(0.735750336487032,1.27435696448144,
-1.77343750000002));
#371237=CARTESIAN_POINT('Ctrl Pts',(0.,1.27435696448144,-1.73593750000002));
#371238=CARTESIAN_POINT('Ctrl Pts',(-0.735750336487031,1.27435696448144,
-1.69843750000002));
#371239=CARTESIAN_POINT('Ctrl Pts',(-1.10362550473055,0.637178482240718,
-1.66093750000002));
#371240=CARTESIAN_POINT('Ctrl Pts',(-1.47150067297406,-4.17112434131439E-17,
-1.62343750000002));
#371241=CARTESIAN_POINT('Ctrl Pts',(-1.10362550473055,-0.637178482240718,
-1.58593750000002));
#371242=CARTESIAN_POINT('Ctrl Pts',(-0.735750336487032,-1.27435696448144,
-1.54843750000002));
#371243=CARTESIAN_POINT('Ctrl Pts',(-1.56063717752333E-16,-1.27435696448144,
-1.51093750000002));
#371244=CARTESIAN_POINT('Ctrl Pts',(0.735750336487031,-1.27435696448144,
-1.47343750000002));
#371245=CARTESIAN_POINT('Ctrl Pts',(1.10362550473055,-0.637178482240719,
-1.43593750000002));
#371246=CARTESIAN_POINT('Ctrl Pts',(1.47150067297406,-4.01923661911483E-16,
-1.39843750000002));
#371247=CARTESIAN_POINT('Ctrl Pts',(1.10362550473055,0.637178482240717,
-1.36093750000002));
#371248=CARTESIAN_POINT('Ctrl Pts',(0.735750336487032,1.27435696448144,
-1.32343750000002));
#371249=CARTESIAN_POINT('Ctrl Pts',(0.,1.27435696448144,-1.28593750000002));
#371250=CARTESIAN_POINT('Ctrl Pts',(-0.735750336487031,1.27435696448144,
-1.24843750000002));
#371251=CARTESIAN_POINT('Ctrl Pts',(-1.10362550473055,0.637178482240718,
-1.21093750000002));
#371252=CARTESIAN_POINT('Ctrl Pts',(-1.47150067297406,-4.13086447694779E-17,
-1.17343750000002));
#371253=CARTESIAN_POINT('Ctrl Pts',(-1.10362550473055,-0.637178482240718,
-1.13593750000002));
#371254=CARTESIAN_POINT('Ctrl Pts',(-0.735750336487032,-1.27435696448144,
-1.09843750000002));
#371255=CARTESIAN_POINT('Ctrl Pts',(-1.56063717752333E-16,-1.27435696448144,
-1.06093750000002));
#371256=CARTESIAN_POINT('Ctrl Pts',(0.735750336487031,-1.27435696448144,
-1.02343750000002));
#371257=CARTESIAN_POINT('Ctrl Pts',(1.10362550473055,-0.637178482240719,
-0.985937500000016));
#371258=CARTESIAN_POINT('Ctrl Pts',(1.47150067297406,-4.01521063267817E-16,
-0.948437500000016));
#371259=CARTESIAN_POINT('Ctrl Pts',(1.10362550473055,0.637178482240717,
-0.910937500000016));
#371260=CARTESIAN_POINT('Ctrl Pts',(0.735750336487032,1.27435696448144,
-0.873437500000016));
#371261=CARTESIAN_POINT('Ctrl Pts',(0.,1.27435696448144,-0.835937500000016));
#371262=CARTESIAN_POINT('Ctrl Pts',(-0.735750336487031,1.27435696448144,
-0.798437500000016));
#371263=CARTESIAN_POINT('Ctrl Pts',(-1.10362550473055,0.637178482240718,
-0.760937500000016));
#371264=CARTESIAN_POINT('Ctrl Pts',(-1.47150067297406,-4.09060461258118E-17,
-0.723437500000016));
#371265=CARTESIAN_POINT('Ctrl Pts',(-1.10362550473055,-0.637178482240718,
-0.685937500000016));
#371266=CARTESIAN_POINT('Ctrl Pts',(-0.735750336487032,-1.27435696448144,
-0.648437500000016));
#371267=CARTESIAN_POINT('Ctrl Pts',(-1.56063717752333E-16,-1.27435696448144,
-0.610937500000016));
#371268=CARTESIAN_POINT('Ctrl Pts',(0.735750336487031,-1.27435696448144,
-0.573437500000016));
#371269=CARTESIAN_POINT('Ctrl Pts',(1.10362550473055,-0.637178482240719,
-0.535937500000016));
#371270=CARTESIAN_POINT('Ctrl Pts',(1.47150067297406,-4.01118464624151E-16,
-0.498437500000016));
#371271=CARTESIAN_POINT('Ctrl Pts',(1.10362550473055,0.637178482240717,
-0.460937500000016));
#371272=CARTESIAN_POINT('Ctrl Pts',(0.735750336487032,1.27435696448144,
-0.423437500000016));
#371273=CARTESIAN_POINT('Ctrl Pts',(0.,1.27435696448144,-0.385937500000016));
#371274=CARTESIAN_POINT('Ctrl Pts',(-0.735750336487031,1.27435696448144,
-0.348437500000016));
#371275=CARTESIAN_POINT('Ctrl Pts',(-1.10362550473055,0.637178482240718,
-0.310937500000016));
#371276=CARTESIAN_POINT('Ctrl Pts',(-1.47150067297406,-4.05034474821458E-17,
-0.273437500000016));
#371277=CARTESIAN_POINT('Ctrl Pts',(-1.10362550473055,-0.637178482240718,
-0.235937500000016));
#371278=CARTESIAN_POINT('Ctrl Pts',(-0.735750336487032,-1.27435696448144,
-0.198437500000016));
#371279=CARTESIAN_POINT('Ctrl Pts',(-1.56063717752333E-16,-1.27435696448144,
-0.160937500000016));
#371280=CARTESIAN_POINT('Ctrl Pts',(0.735750336487031,-1.27435696448144,
-0.123437500000016));
#371281=CARTESIAN_POINT('Ctrl Pts',(1.10362550473055,-0.637178482240719,
-0.0859375000000157));
#371282=CARTESIAN_POINT('Ctrl Pts',(1.47150067297406,-4.00715865980485E-16,
-0.0484375000000155));
#371283=CARTESIAN_POINT('Ctrl Pts',(1.10362550473055,0.637178482240717,
-0.0109375000000161));
#371284=CARTESIAN_POINT('Ctrl Pts',(0.735750336487032,1.27435696448144,
0.0265624999999841));
#371285=CARTESIAN_POINT('Ctrl Pts',(0.,1.27435696448144,0.0640624999999843));
#371286=CARTESIAN_POINT('Ctrl Pts',(-0.735750336487031,1.27435696448144,
0.101562499999984));
#371287=CARTESIAN_POINT('Ctrl Pts',(-1.10362550473055,0.637178482240718,
0.139062499999984));
#371288=CARTESIAN_POINT('Ctrl Pts',(-1.47150067297406,-4.01008488384797E-17,
0.176562499999984));
#371289=CARTESIAN_POINT('Ctrl Pts',(-1.10362550473055,-0.637178482240718,
0.214062499999984));
#371290=CARTESIAN_POINT('Ctrl Pts',(-0.735750336487032,-1.27435696448144,
0.251562499999984));
#371291=CARTESIAN_POINT('Ctrl Pts',(-1.56063717752333E-16,-1.27435696448144,
0.289062499999984));
#371292=CARTESIAN_POINT('Ctrl Pts',(0.735750336487031,-1.27435696448144,
0.326562499999984));
#371293=CARTESIAN_POINT('Ctrl Pts',(1.10362550473055,-0.637178482240719,
0.364062499999984));
#371294=CARTESIAN_POINT('Ctrl Pts',(1.47150067297406,-4.00313267336819E-16,
0.401562499999984));
#371295=CARTESIAN_POINT('Ctrl Pts',(1.10362550473055,0.637178482240717,
0.439062499999984));
#371296=CARTESIAN_POINT('Ctrl Pts',(0.735750336487032,1.27435696448144,
0.476562499999984));
#371297=CARTESIAN_POINT('Ctrl Pts',(0.,1.27435696448144,0.514062499999984));
#371298=CARTESIAN_POINT('Ctrl Pts',(-0.735750336487031,1.27435696448144,
0.551562499999984));
#371299=CARTESIAN_POINT('Ctrl Pts',(-1.10362550473055,0.637178482240718,
0.589062499999984));
#371300=CARTESIAN_POINT('Ctrl Pts',(-1.47150067297406,-3.96982501948137E-17,
0.626562499999984));
#371301=CARTESIAN_POINT('Ctrl Pts',(-1.10362550473055,-0.637178482240718,
0.664062499999984));
#371302=CARTESIAN_POINT('Ctrl Pts',(-0.735750336487032,-1.27435696448144,
0.701562499999984));
#371303=CARTESIAN_POINT('Ctrl Pts',(-1.56063717752333E-16,-1.27435696448144,
0.739062499999984));
#371304=CARTESIAN_POINT('Ctrl Pts',(0.735750336487031,-1.27435696448144,
0.776562499999984));
#371305=CARTESIAN_POINT('Ctrl Pts',(1.10362550473055,-0.637178482240719,
0.814062499999984));
#371306=CARTESIAN_POINT('Ctrl Pts',(1.47150067297406,-3.99910668693153E-16,
0.851562499999984));
#371307=CARTESIAN_POINT('Ctrl Pts',(1.10362550473055,0.637178482240717,
0.889062499999985));
#371308=CARTESIAN_POINT('Ctrl Pts',(0.735750336487032,1.27435696448144,
0.926562499999984));
#371309=CARTESIAN_POINT('Ctrl Pts',(0.,1.27435696448144,0.964062499999984));
#371310=CARTESIAN_POINT('Ctrl Pts',(-0.735750336487031,1.27435696448144,
1.00156249999998));
#371311=CARTESIAN_POINT('Ctrl Pts',(-1.10362550473055,0.637178482240718,
1.03906249999998));
#371312=CARTESIAN_POINT('Ctrl Pts',(-1.47150067297406,-3.92956515511476E-17,
1.07656249999998));
#371313=CARTESIAN_POINT('Ctrl Pts',(-1.10362550473055,-0.637178482240718,
1.11406249999998));
#371314=CARTESIAN_POINT('Ctrl Pts',(-0.735750336487032,-1.27435696448144,
1.15156249999998));
#371315=CARTESIAN_POINT('Ctrl Pts',(-1.56063717752333E-16,-1.27435696448144,
1.18906249999998));
#371316=CARTESIAN_POINT('Ctrl Pts',(0.735750336487031,-1.27435696448144,
1.22656249999998));
#371317=CARTESIAN_POINT('Ctrl Pts',(1.10362550473055,-0.637178482240719,
1.26406249999998));
#371318=CARTESIAN_POINT('Ctrl Pts',(1.47150067297406,-3.99508070049487E-16,
1.30156249999998));
#371319=CARTESIAN_POINT('Ctrl Pts',(1.10362550473055,0.637178482240717,
1.33906249999998));
#371320=CARTESIAN_POINT('Ctrl Pts',(0.735750336487032,1.27435696448144,
1.37656249999998));
#371321=CARTESIAN_POINT('Ctrl Pts',(0.,1.27435696448144,1.41406249999998));
#371322=CARTESIAN_POINT('Ctrl Pts',(-0.735750336487031,1.27435696448144,
1.45156249999998));
#371323=CARTESIAN_POINT('Ctrl Pts',(-1.10362550473055,0.637178482240718,
1.48906249999998));
#371324=CARTESIAN_POINT('Ctrl Pts',(-1.47150067297406,-3.88930529074816E-17,
1.52656249999998));
#371325=CARTESIAN_POINT('Ctrl Pts',(-1.10362550473055,-0.637178482240718,
1.56406249999998));
#371326=CARTESIAN_POINT('Ctrl Pts',(-0.735750336487032,-1.27435696448144,
1.60156249999998));
#371327=CARTESIAN_POINT('Ctrl Pts',(-1.56063717752333E-16,-1.27435696448144,
1.63906249999998));
#371328=CARTESIAN_POINT('Ctrl Pts',(0.735750336487031,-1.27435696448144,
1.67656249999998));
#371329=CARTESIAN_POINT('Ctrl Pts',(1.10362550473055,-0.637178482240719,
1.71406249999998));
#371330=CARTESIAN_POINT('Ctrl Pts',(1.47150067297406,-3.99105471405821E-16,
1.75156249999998));
#371331=CARTESIAN_POINT('Ctrl Pts',(1.10362550473055,0.637178482240717,
1.78906249999998));
#371332=CARTESIAN_POINT('Ctrl Pts',(0.735750336487032,1.27435696448144,
1.82656249999998));
#371333=CARTESIAN_POINT('Ctrl Pts',(0.,1.27435696448144,1.86406249999998));
#371334=CARTESIAN_POINT('Ctrl Pts',(-0.735750336487031,1.27435696448144,
1.90156249999998));
#371335=CARTESIAN_POINT('Ctrl Pts',(-1.10362550473055,0.637178482240718,
1.93906249999998));
#371336=CARTESIAN_POINT('Ctrl Pts',(-1.47150067297406,-3.84904542638155E-17,
1.97656249999998));
#371337=CARTESIAN_POINT('Ctrl Pts',(-1.10362550473055,-0.637178482240718,
2.01406249999998));
#371338=CARTESIAN_POINT('Ctrl Pts',(-0.735750336487032,-1.27435696448144,
2.05156249999998));
#371339=CARTESIAN_POINT('Ctrl Pts',(-1.56063717752333E-16,-1.27435696448144,
2.08906249999998));
#371340=CARTESIAN_POINT('Ctrl Pts',(0.735750336487031,-1.27435696448144,
2.12656249999998));
#371341=CARTESIAN_POINT('Ctrl Pts',(1.10362550473055,-0.637178482240719,
2.16406249999998));
#371342=CARTESIAN_POINT('Ctrl Pts',(1.47150067297406,-3.98702872762155E-16,
2.20156249999998));
#371343=CARTESIAN_POINT('Ctrl Pts',(1.10362550473055,0.637178482240717,
2.23906249999998));
#371344=CARTESIAN_POINT('Ctrl Pts',(0.735750336487032,1.27435696448144,
2.27656249999998));
#371345=CARTESIAN_POINT('Ctrl Pts',(0.,1.27435696448144,2.31406249999998));
#371346=CARTESIAN_POINT('Ctrl Pts',(-0.735750336487031,1.27435696448144,
2.35156249999998));
#371347=CARTESIAN_POINT('Ctrl Pts',(-1.10362550473055,0.637178482240718,
2.38906249999998));
#371348=CARTESIAN_POINT('Ctrl Pts',(-1.47150067297406,-3.80878556201495E-17,
2.42656249999998));
#371349=CARTESIAN_POINT('Ctrl Pts',(-1.10362550473055,-0.637178482240718,
2.46406249999998));
#371350=CARTESIAN_POINT('Ctrl Pts',(-0.735750336487032,-1.27435696448144,
2.50156249999998));
#371351=CARTESIAN_POINT('Ctrl Pts',(-1.56063717752333E-16,-1.27435696448144,
2.53906249999998));
#371352=CARTESIAN_POINT('Ctrl Pts',(0.735750336487031,-1.27435696448144,
2.57656249999998));
#371353=CARTESIAN_POINT('Ctrl Pts',(1.10362550473055,-0.637178482240719,
2.61406249999998));
#371354=CARTESIAN_POINT('Ctrl Pts',(1.47150067297406,-3.98300274118489E-16,
2.65156249999998));
#371355=CARTESIAN_POINT('Ctrl Pts',(1.10362550473055,0.637178482240717,
2.68906249999998));
#371356=CARTESIAN_POINT('Ctrl Pts',(0.735750336487032,1.27435696448144,
2.72656249999998));
#371357=CARTESIAN_POINT('Ctrl Pts',(0.,1.27435696448144,2.76406249999998));
#371358=CARTESIAN_POINT('Ctrl Pts',(-0.735750336487031,1.27435696448144,
2.80156249999998));
#371359=CARTESIAN_POINT('Ctrl Pts',(-1.10362550473055,0.637178482240718,
2.83906249999998));
#371360=CARTESIAN_POINT('Ctrl Pts',(-1.47150067297406,-3.76852569764834E-17,
2.87656249999998));
#371361=CARTESIAN_POINT('Ctrl Pts',(-1.10362550473055,-0.637178482240718,
2.91406249999998));
#371362=CARTESIAN_POINT('Ctrl Pts',(-0.735750336487032,-1.27435696448144,
2.95156249999998));
#371363=CARTESIAN_POINT('Ctrl Pts',(-1.56063717752333E-16,-1.27435696448144,
2.98906249999998));
#371364=CARTESIAN_POINT('Ctrl Pts',(0.735750336487031,-1.27435696448144,
3.02656249999998));
#371365=CARTESIAN_POINT('Ctrl Pts',(1.10362550473055,-0.637178482240719,
3.06406249999998));
#371366=CARTESIAN_POINT('Ctrl Pts',(1.47150067297406,-3.97897675474823E-16,
3.10156249999998));
#371367=CARTESIAN_POINT('Ctrl Pts',(1.10362550473055,0.637178482240717,
3.13906249999998));
#371368=CARTESIAN_POINT('Ctrl Pts',(0.735750336487032,1.27435696448144,
3.17656249999998));
#371369=CARTESIAN_POINT('Ctrl Pts',(0.,1.27435696448144,3.21406249999998));
#371370=CARTESIAN_POINT('Ctrl Pts',(-0.735750336487031,1.27435696448144,
3.25156249999998));
#371371=CARTESIAN_POINT('Ctrl Pts',(-1.10362550473055,0.637178482240718,
3.28906249999998));
#371372=CARTESIAN_POINT('Ctrl Pts',(-1.47150067297406,-3.72826583328174E-17,
3.32656249999998));
#371373=CARTESIAN_POINT('Ctrl Pts',(-1.10362550473055,-0.637178482240718,
3.36406249999998));
#371374=CARTESIAN_POINT('Ctrl Pts',(-0.735750336487032,-1.27435696448144,
3.40156249999998));
#371375=CARTESIAN_POINT('Ctrl Pts',(-1.56063717752333E-16,-1.27435696448144,
3.43906249999998));
#371376=CARTESIAN_POINT('Ctrl Pts',(0.735750336487031,-1.27435696448144,
3.47656249999998));
#371377=CARTESIAN_POINT('Ctrl Pts',(1.10362550473055,-0.637178482240719,
3.51406249999998));
#371378=CARTESIAN_POINT('Ctrl Pts',(1.47150067297406,-3.97495076831157E-16,
3.55156249999998));
#371379=CARTESIAN_POINT('Ctrl Pts',(1.10362550473055,0.637178482240717,
3.58906249999998));
#371380=CARTESIAN_POINT('Ctrl Pts',(0.735750336487032,1.27435696448144,
3.62656249999998));
#371381=CARTESIAN_POINT('Ctrl Pts',(0.,1.27435696448144,3.66406249999998));
#371382=CARTESIAN_POINT('Ctrl Pts',(-0.735750336487031,1.27435696448144,
3.70156249999998));
#371383=CARTESIAN_POINT('Ctrl Pts',(-1.10362550473055,0.637178482240718,
3.73906249999998));
#371384=CARTESIAN_POINT('Ctrl Pts',(-1.47150067297406,-3.68800596891513E-17,
3.77656249999998));
#371385=CARTESIAN_POINT('Ctrl Pts',(-1.10362550473055,-0.637178482240718,
3.81406249999998));
#371386=CARTESIAN_POINT('Ctrl Pts',(-0.735750336487032,-1.27435696448144,
3.85156249999998));
#371387=CARTESIAN_POINT('Ctrl Pts',(-1.56063717752333E-16,-1.27435696448144,
3.88906249999998));
#371388=CARTESIAN_POINT('Ctrl Pts',(0.735750336487031,-1.27435696448144,
3.92656249999998));
#371389=CARTESIAN_POINT('Ctrl Pts',(1.10362550473055,-0.637178482240719,
3.96406249999998));
#371390=CARTESIAN_POINT('Ctrl Pts',(1.33553307714466,-0.235502784159521,
3.98770240482708));
#371391=CARTESIAN_POINT('Ctrl Pts',(1.2550005617303,0.22126740152805,4.01458479718761));
#371392=CARTESIAN_POINT('Ctrl Pts',(0.,0.957716426222737,-4.16875000000002));
#371393=CARTESIAN_POINT('Ctrl Pts',(-0.552937836487023,0.957716426222737,
-4.13125000000002));
#371394=CARTESIAN_POINT('Ctrl Pts',(-0.829406754730535,0.478858213111368,
-4.09375000000002));
#371395=CARTESIAN_POINT('Ctrl Pts',(-1.10587567297405,-6.6275866627377E-17,
-4.05625000000002));
#371396=CARTESIAN_POINT('Ctrl Pts',(-0.829406754730535,-0.478858213111368,
-4.01875000000002));
#371397=CARTESIAN_POINT('Ctrl Pts',(-0.552937836487024,-0.957716426222737,
-3.98125000000002));
#371398=CARTESIAN_POINT('Ctrl Pts',(-1.17286435586452E-16,-0.957716426222737,
-3.94375000000002));
#371399=CARTESIAN_POINT('Ctrl Pts',(0.552937836487023,-0.957716426222737,
-3.90625000000002));
#371400=CARTESIAN_POINT('Ctrl Pts',(0.829406754730535,-0.478858213111369,
-3.86875000000002));
#371401=CARTESIAN_POINT('Ctrl Pts',(1.10587567297405,-3.36935987938062E-16,
-3.83125000000002));
#371402=CARTESIAN_POINT('Ctrl Pts',(0.829406754730536,0.478858213111368,
-3.79375000000002));
#371403=CARTESIAN_POINT('Ctrl Pts',(0.552937836487024,0.957716426222737,
-3.75625000000002));
#371404=CARTESIAN_POINT('Ctrl Pts',(0.,0.957716426222737,-3.71875000000002));
#371405=CARTESIAN_POINT('Ctrl Pts',(-0.552937836487023,0.957716426222737,
-3.68125000000002));
#371406=CARTESIAN_POINT('Ctrl Pts',(-0.829406754730535,0.478858213111368,
-3.64375000000002));
#371407=CARTESIAN_POINT('Ctrl Pts',(-1.10587567297405,-6.5873267983711E-17,
-3.60625000000002));
#371408=CARTESIAN_POINT('Ctrl Pts',(-0.829406754730535,-0.478858213111368,
-3.56875000000002));
#371409=CARTESIAN_POINT('Ctrl Pts',(-0.552937836487024,-0.957716426222737,
-3.53125000000002));
#371410=CARTESIAN_POINT('Ctrl Pts',(-1.17286435586452E-16,-0.957716426222737,
-3.49375000000002));
#371411=CARTESIAN_POINT('Ctrl Pts',(0.552937836487023,-0.957716426222737,
-3.45625000000002));
#371412=CARTESIAN_POINT('Ctrl Pts',(0.829406754730535,-0.478858213111369,
-3.41875000000002));
#371413=CARTESIAN_POINT('Ctrl Pts',(1.10587567297405,-3.36533389294396E-16,
-3.38125000000002));
#371414=CARTESIAN_POINT('Ctrl Pts',(0.829406754730536,0.478858213111368,
-3.34375000000002));
#371415=CARTESIAN_POINT('Ctrl Pts',(0.552937836487024,0.957716426222737,
-3.30625000000002));
#371416=CARTESIAN_POINT('Ctrl Pts',(0.,0.957716426222737,-3.26875000000002));
#371417=CARTESIAN_POINT('Ctrl Pts',(-0.552937836487023,0.957716426222737,
-3.23125000000002));
#371418=CARTESIAN_POINT('Ctrl Pts',(-0.829406754730535,0.478858213111368,
-3.19375000000002));
#371419=CARTESIAN_POINT('Ctrl Pts',(-1.10587567297405,-6.54706693400449E-17,
-3.15625000000002));
#371420=CARTESIAN_POINT('Ctrl Pts',(-0.829406754730535,-0.478858213111368,
-3.11875000000002));
#371421=CARTESIAN_POINT('Ctrl Pts',(-0.552937836487024,-0.957716426222737,
-3.08125000000002));
#371422=CARTESIAN_POINT('Ctrl Pts',(-1.17286435586452E-16,-0.957716426222737,
-3.04375000000002));
#371423=CARTESIAN_POINT('Ctrl Pts',(0.552937836487023,-0.957716426222737,
-3.00625000000002));
#371424=CARTESIAN_POINT('Ctrl Pts',(0.829406754730535,-0.478858213111369,
-2.96875000000002));
#371425=CARTESIAN_POINT('Ctrl Pts',(1.10587567297405,-3.3613079065073E-16,
-2.93125000000002));
#371426=CARTESIAN_POINT('Ctrl Pts',(0.829406754730536,0.478858213111368,
-2.89375000000002));
#371427=CARTESIAN_POINT('Ctrl Pts',(0.552937836487024,0.957716426222737,
-2.85625000000002));
#371428=CARTESIAN_POINT('Ctrl Pts',(0.,0.957716426222737,-2.81875000000002));
#371429=CARTESIAN_POINT('Ctrl Pts',(-0.552937836487023,0.957716426222737,
-2.78125000000002));
#371430=CARTESIAN_POINT('Ctrl Pts',(-0.829406754730535,0.478858213111368,
-2.74375000000002));
#371431=CARTESIAN_POINT('Ctrl Pts',(-1.10587567297405,-6.50680706963789E-17,
-2.70625000000002));
#371432=CARTESIAN_POINT('Ctrl Pts',(-0.829406754730535,-0.478858213111368,
-2.66875000000002));
#371433=CARTESIAN_POINT('Ctrl Pts',(-0.552937836487024,-0.957716426222737,
-2.63125000000002));
#371434=CARTESIAN_POINT('Ctrl Pts',(-1.17286435586452E-16,-0.957716426222737,
-2.59375000000002));
#371435=CARTESIAN_POINT('Ctrl Pts',(0.552937836487023,-0.957716426222737,
-2.55625000000002));
#371436=CARTESIAN_POINT('Ctrl Pts',(0.829406754730535,-0.478858213111369,
-2.51875000000002));
#371437=CARTESIAN_POINT('Ctrl Pts',(1.10587567297405,-3.35728192007064E-16,
-2.48125000000002));
#371438=CARTESIAN_POINT('Ctrl Pts',(0.829406754730536,0.478858213111368,
-2.44375000000002));
#371439=CARTESIAN_POINT('Ctrl Pts',(0.552937836487024,0.957716426222737,
-2.40625000000002));
#371440=CARTESIAN_POINT('Ctrl Pts',(0.,0.957716426222737,-2.36875000000002));
#371441=CARTESIAN_POINT('Ctrl Pts',(-0.552937836487023,0.957716426222737,
-2.33125000000002));
#371442=CARTESIAN_POINT('Ctrl Pts',(-0.829406754730535,0.478858213111368,
-2.29375000000002));
#371443=CARTESIAN_POINT('Ctrl Pts',(-1.10587567297405,-6.46654720527128E-17,
-2.25625000000002));
#371444=CARTESIAN_POINT('Ctrl Pts',(-0.829406754730535,-0.478858213111368,
-2.21875000000002));
#371445=CARTESIAN_POINT('Ctrl Pts',(-0.552937836487024,-0.957716426222737,
-2.18125000000002));
#371446=CARTESIAN_POINT('Ctrl Pts',(-1.17286435586452E-16,-0.957716426222737,
-2.14375000000002));
#371447=CARTESIAN_POINT('Ctrl Pts',(0.552937836487023,-0.957716426222737,
-2.10625000000002));
#371448=CARTESIAN_POINT('Ctrl Pts',(0.829406754730535,-0.478858213111369,
-2.06875000000002));
#371449=CARTESIAN_POINT('Ctrl Pts',(1.10587567297405,-3.35325593363398E-16,
-2.03125000000002));
#371450=CARTESIAN_POINT('Ctrl Pts',(0.829406754730536,0.478858213111368,
-1.99375000000002));
#371451=CARTESIAN_POINT('Ctrl Pts',(0.552937836487024,0.957716426222737,
-1.95625000000002));
#371452=CARTESIAN_POINT('Ctrl Pts',(0.,0.957716426222737,-1.91875000000002));
#371453=CARTESIAN_POINT('Ctrl Pts',(-0.552937836487023,0.957716426222737,
-1.88125000000002));
#371454=CARTESIAN_POINT('Ctrl Pts',(-0.829406754730535,0.478858213111368,
-1.84375000000002));
#371455=CARTESIAN_POINT('Ctrl Pts',(-1.10587567297405,-6.42628734090468E-17,
-1.80625000000002));
#371456=CARTESIAN_POINT('Ctrl Pts',(-0.829406754730535,-0.478858213111368,
-1.76875000000002));
#371457=CARTESIAN_POINT('Ctrl Pts',(-0.552937836487024,-0.957716426222737,
-1.73125000000002));
#371458=CARTESIAN_POINT('Ctrl Pts',(-1.17286435586452E-16,-0.957716426222737,
-1.69375000000002));
#371459=CARTESIAN_POINT('Ctrl Pts',(0.552937836487023,-0.957716426222737,
-1.65625000000002));
#371460=CARTESIAN_POINT('Ctrl Pts',(0.829406754730535,-0.478858213111369,
-1.61875000000002));
#371461=CARTESIAN_POINT('Ctrl Pts',(1.10587567297405,-3.34922994719732E-16,
-1.58125000000002));
#371462=CARTESIAN_POINT('Ctrl Pts',(0.829406754730536,0.478858213111368,
-1.54375000000002));
#371463=CARTESIAN_POINT('Ctrl Pts',(0.552937836487024,0.957716426222737,
-1.50625000000002));
#371464=CARTESIAN_POINT('Ctrl Pts',(0.,0.957716426222737,-1.46875000000002));
#371465=CARTESIAN_POINT('Ctrl Pts',(-0.552937836487023,0.957716426222737,
-1.43125000000002));
#371466=CARTESIAN_POINT('Ctrl Pts',(-0.829406754730535,0.478858213111368,
-1.39375000000002));
#371467=CARTESIAN_POINT('Ctrl Pts',(-1.10587567297405,-6.38602747653807E-17,
-1.35625000000002));
#371468=CARTESIAN_POINT('Ctrl Pts',(-0.829406754730535,-0.478858213111368,
-1.31875000000002));
#371469=CARTESIAN_POINT('Ctrl Pts',(-0.552937836487024,-0.957716426222737,
-1.28125000000002));
#371470=CARTESIAN_POINT('Ctrl Pts',(-1.17286435586452E-16,-0.957716426222737,
-1.24375000000002));
#371471=CARTESIAN_POINT('Ctrl Pts',(0.552937836487023,-0.957716426222737,
-1.20625000000002));
#371472=CARTESIAN_POINT('Ctrl Pts',(0.829406754730535,-0.478858213111369,
-1.16875000000002));
#371473=CARTESIAN_POINT('Ctrl Pts',(1.10587567297405,-3.34520396076066E-16,
-1.13125000000002));
#371474=CARTESIAN_POINT('Ctrl Pts',(0.829406754730536,0.478858213111368,
-1.09375000000002));
#371475=CARTESIAN_POINT('Ctrl Pts',(0.552937836487024,0.957716426222737,
-1.05625000000002));
#371476=CARTESIAN_POINT('Ctrl Pts',(0.,0.957716426222737,-1.01875000000002));
#371477=CARTESIAN_POINT('Ctrl Pts',(-0.552937836487023,0.957716426222737,
-0.98125000000002));
#371478=CARTESIAN_POINT('Ctrl Pts',(-0.829406754730535,0.478858213111368,
-0.94375000000002));
#371479=CARTESIAN_POINT('Ctrl Pts',(-1.10587567297405,-6.34576761217147E-17,
-0.90625000000002));
#371480=CARTESIAN_POINT('Ctrl Pts',(-0.829406754730535,-0.478858213111368,
-0.86875000000002));
#371481=CARTESIAN_POINT('Ctrl Pts',(-0.552937836487024,-0.957716426222737,
-0.83125000000002));
#371482=CARTESIAN_POINT('Ctrl Pts',(-1.17286435586452E-16,-0.957716426222737,
-0.79375000000002));
#371483=CARTESIAN_POINT('Ctrl Pts',(0.552937836487023,-0.957716426222737,
-0.75625000000002));
#371484=CARTESIAN_POINT('Ctrl Pts',(0.829406754730535,-0.478858213111369,
-0.71875000000002));
#371485=CARTESIAN_POINT('Ctrl Pts',(1.10587567297405,-3.341177974324E-16,
-0.68125000000002));
#371486=CARTESIAN_POINT('Ctrl Pts',(0.829406754730536,0.478858213111368,
-0.64375000000002));
#371487=CARTESIAN_POINT('Ctrl Pts',(0.552937836487024,0.957716426222737,
-0.60625000000002));
#371488=CARTESIAN_POINT('Ctrl Pts',(0.,0.957716426222737,-0.56875000000002));
#371489=CARTESIAN_POINT('Ctrl Pts',(-0.552937836487023,0.957716426222737,
-0.53125000000002));
#371490=CARTESIAN_POINT('Ctrl Pts',(-0.829406754730535,0.478858213111368,
-0.49375000000002));
#371491=CARTESIAN_POINT('Ctrl Pts',(-1.10587567297405,-6.30550774780486E-17,
-0.45625000000002));
#371492=CARTESIAN_POINT('Ctrl Pts',(-0.829406754730535,-0.478858213111368,
-0.41875000000002));
#371493=CARTESIAN_POINT('Ctrl Pts',(-0.552937836487024,-0.957716426222737,
-0.38125000000002));
#371494=CARTESIAN_POINT('Ctrl Pts',(-1.17286435586452E-16,-0.957716426222737,
-0.34375000000002));
#371495=CARTESIAN_POINT('Ctrl Pts',(0.552937836487023,-0.957716426222737,
-0.30625000000002));
#371496=CARTESIAN_POINT('Ctrl Pts',(0.829406754730535,-0.478858213111369,
-0.26875000000002));
#371497=CARTESIAN_POINT('Ctrl Pts',(1.10587567297405,-3.33715198788734E-16,
-0.23125000000002));
#371498=CARTESIAN_POINT('Ctrl Pts',(0.829406754730536,0.478858213111368,
-0.19375000000002));
#371499=CARTESIAN_POINT('Ctrl Pts',(0.552937836487024,0.957716426222737,
-0.15625000000002));
#371500=CARTESIAN_POINT('Ctrl Pts',(0.,0.957716426222737,-0.11875000000002));
#371501=CARTESIAN_POINT('Ctrl Pts',(-0.552937836487023,0.957716426222737,
-0.0812500000000197));
#371502=CARTESIAN_POINT('Ctrl Pts',(-0.829406754730535,0.478858213111368,
-0.0437500000000203));
#371503=CARTESIAN_POINT('Ctrl Pts',(-1.10587567297405,-6.26524788343826E-17,
-0.00625000000002013));
#371504=CARTESIAN_POINT('Ctrl Pts',(-0.829406754730535,-0.478858213111368,
0.0312499999999801));
#371505=CARTESIAN_POINT('Ctrl Pts',(-0.552937836487024,-0.957716426222737,
0.0687499999999803));
#371506=CARTESIAN_POINT('Ctrl Pts',(-1.17286435586452E-16,-0.957716426222737,
0.10624999999998));
#371507=CARTESIAN_POINT('Ctrl Pts',(0.552937836487023,-0.957716426222737,
0.14374999999998));
#371508=CARTESIAN_POINT('Ctrl Pts',(0.829406754730535,-0.478858213111369,
0.18124999999998));
#371509=CARTESIAN_POINT('Ctrl Pts',(1.10587567297405,-3.33312600145068E-16,
0.21874999999998));
#371510=CARTESIAN_POINT('Ctrl Pts',(0.829406754730536,0.478858213111368,
0.25624999999998));
#371511=CARTESIAN_POINT('Ctrl Pts',(0.552937836487024,0.957716426222737,
0.29374999999998));
#371512=CARTESIAN_POINT('Ctrl Pts',(0.,0.957716426222737,0.33124999999998));
#371513=CARTESIAN_POINT('Ctrl Pts',(-0.552937836487023,0.957716426222737,
0.36874999999998));
#371514=CARTESIAN_POINT('Ctrl Pts',(-0.829406754730535,0.478858213111368,
0.40624999999998));
#371515=CARTESIAN_POINT('Ctrl Pts',(-1.10587567297405,-6.22498801907165E-17,
0.44374999999998));
#371516=CARTESIAN_POINT('Ctrl Pts',(-0.829406754730535,-0.478858213111368,
0.48124999999998));
#371517=CARTESIAN_POINT('Ctrl Pts',(-0.552937836487024,-0.957716426222737,
0.51874999999998));
#371518=CARTESIAN_POINT('Ctrl Pts',(-1.17286435586452E-16,-0.957716426222737,
0.556249999999979));
#371519=CARTESIAN_POINT('Ctrl Pts',(0.552937836487023,-0.957716426222737,
0.59374999999998));
#371520=CARTESIAN_POINT('Ctrl Pts',(0.829406754730535,-0.478858213111369,
0.63124999999998));
#371521=CARTESIAN_POINT('Ctrl Pts',(1.10587567297405,-3.32910001501402E-16,
0.66874999999998));
#371522=CARTESIAN_POINT('Ctrl Pts',(0.829406754730536,0.478858213111368,
0.70624999999998));
#371523=CARTESIAN_POINT('Ctrl Pts',(0.552937836487024,0.957716426222737,
0.74374999999998));
#371524=CARTESIAN_POINT('Ctrl Pts',(0.,0.957716426222737,0.78124999999998));
#371525=CARTESIAN_POINT('Ctrl Pts',(-0.552937836487023,0.957716426222737,
0.81874999999998));
#371526=CARTESIAN_POINT('Ctrl Pts',(-0.829406754730535,0.478858213111368,
0.85624999999998));
#371527=CARTESIAN_POINT('Ctrl Pts',(-1.10587567297405,-6.18472815470505E-17,
0.89374999999998));
#371528=CARTESIAN_POINT('Ctrl Pts',(-0.829406754730535,-0.478858213111368,
0.93124999999998));
#371529=CARTESIAN_POINT('Ctrl Pts',(-0.552937836487024,-0.957716426222737,
0.96874999999998));
#371530=CARTESIAN_POINT('Ctrl Pts',(-1.17286435586452E-16,-0.957716426222737,
1.00624999999998));
#371531=CARTESIAN_POINT('Ctrl Pts',(0.552937836487023,-0.957716426222737,
1.04374999999998));
#371532=CARTESIAN_POINT('Ctrl Pts',(0.829406754730535,-0.478858213111369,
1.08124999999998));
#371533=CARTESIAN_POINT('Ctrl Pts',(1.10587567297405,-3.32507402857736E-16,
1.11874999999998));
#371534=CARTESIAN_POINT('Ctrl Pts',(0.829406754730536,0.478858213111368,
1.15624999999998));
#371535=CARTESIAN_POINT('Ctrl Pts',(0.552937836487024,0.957716426222737,
1.19374999999998));
#371536=CARTESIAN_POINT('Ctrl Pts',(0.,0.957716426222737,1.23124999999998));
#371537=CARTESIAN_POINT('Ctrl Pts',(-0.552937836487023,0.957716426222737,
1.26874999999998));
#371538=CARTESIAN_POINT('Ctrl Pts',(-0.829406754730535,0.478858213111368,
1.30624999999998));
#371539=CARTESIAN_POINT('Ctrl Pts',(-1.10587567297405,-6.14446829033844E-17,
1.34374999999998));
#371540=CARTESIAN_POINT('Ctrl Pts',(-0.829406754730535,-0.478858213111368,
1.38124999999998));
#371541=CARTESIAN_POINT('Ctrl Pts',(-0.552937836487024,-0.957716426222737,
1.41874999999998));
#371542=CARTESIAN_POINT('Ctrl Pts',(-1.17286435586452E-16,-0.957716426222737,
1.45624999999998));
#371543=CARTESIAN_POINT('Ctrl Pts',(0.552937836487023,-0.957716426222737,
1.49374999999998));
#371544=CARTESIAN_POINT('Ctrl Pts',(0.829406754730535,-0.478858213111369,
1.53124999999998));
#371545=CARTESIAN_POINT('Ctrl Pts',(1.10587567297405,-3.3210480421407E-16,
1.56874999999998));
#371546=CARTESIAN_POINT('Ctrl Pts',(0.829406754730536,0.478858213111368,
1.60624999999998));
#371547=CARTESIAN_POINT('Ctrl Pts',(0.552937836487024,0.957716426222737,
1.64374999999998));
#371548=CARTESIAN_POINT('Ctrl Pts',(0.,0.957716426222737,1.68124999999998));
#371549=CARTESIAN_POINT('Ctrl Pts',(-0.552937836487023,0.957716426222737,
1.71874999999998));
#371550=CARTESIAN_POINT('Ctrl Pts',(-0.829406754730535,0.478858213111368,
1.75624999999998));
#371551=CARTESIAN_POINT('Ctrl Pts',(-1.10587567297405,-6.10420842597184E-17,
1.79374999999998));
#371552=CARTESIAN_POINT('Ctrl Pts',(-0.829406754730535,-0.478858213111368,
1.83124999999998));
#371553=CARTESIAN_POINT('Ctrl Pts',(-0.552937836487024,-0.957716426222737,
1.86874999999998));
#371554=CARTESIAN_POINT('Ctrl Pts',(-1.17286435586452E-16,-0.957716426222737,
1.90624999999998));
#371555=CARTESIAN_POINT('Ctrl Pts',(0.552937836487023,-0.957716426222737,
1.94374999999998));
#371556=CARTESIAN_POINT('Ctrl Pts',(0.829406754730535,-0.478858213111369,
1.98124999999998));
#371557=CARTESIAN_POINT('Ctrl Pts',(1.10587567297405,-3.31702205570404E-16,
2.01874999999998));
#371558=CARTESIAN_POINT('Ctrl Pts',(0.829406754730536,0.478858213111368,
2.05624999999998));
#371559=CARTESIAN_POINT('Ctrl Pts',(0.552937836487024,0.957716426222737,
2.09374999999998));
#371560=CARTESIAN_POINT('Ctrl Pts',(0.,0.957716426222737,2.13124999999998));
#371561=CARTESIAN_POINT('Ctrl Pts',(-0.552937836487023,0.957716426222737,
2.16874999999998));
#371562=CARTESIAN_POINT('Ctrl Pts',(-0.829406754730535,0.478858213111368,
2.20624999999998));
#371563=CARTESIAN_POINT('Ctrl Pts',(-1.10587567297405,-6.06394856160523E-17,
2.24374999999998));
#371564=CARTESIAN_POINT('Ctrl Pts',(-0.829406754730535,-0.478858213111368,
2.28124999999998));
#371565=CARTESIAN_POINT('Ctrl Pts',(-0.552937836487024,-0.957716426222737,
2.31874999999998));
#371566=CARTESIAN_POINT('Ctrl Pts',(-1.17286435586452E-16,-0.957716426222737,
2.35624999999998));
#371567=CARTESIAN_POINT('Ctrl Pts',(0.552937836487023,-0.957716426222737,
2.39374999999998));
#371568=CARTESIAN_POINT('Ctrl Pts',(0.829406754730535,-0.478858213111369,
2.43124999999998));
#371569=CARTESIAN_POINT('Ctrl Pts',(1.10587567297405,-3.31299606926738E-16,
2.46874999999998));
#371570=CARTESIAN_POINT('Ctrl Pts',(0.829406754730536,0.478858213111368,
2.50624999999998));
#371571=CARTESIAN_POINT('Ctrl Pts',(0.552937836487024,0.957716426222737,
2.54374999999998));
#371572=CARTESIAN_POINT('Ctrl Pts',(0.,0.957716426222737,2.58124999999998));
#371573=CARTESIAN_POINT('Ctrl Pts',(-0.552937836487023,0.957716426222737,
2.61874999999998));
#371574=CARTESIAN_POINT('Ctrl Pts',(-0.829406754730535,0.478858213111368,
2.65624999999998));
#371575=CARTESIAN_POINT('Ctrl Pts',(-1.10587567297405,-6.02368869723863E-17,
2.69374999999998));
#371576=CARTESIAN_POINT('Ctrl Pts',(-0.829406754730535,-0.478858213111368,
2.73124999999998));
#371577=CARTESIAN_POINT('Ctrl Pts',(-0.552937836487024,-0.957716426222737,
2.76874999999998));
#371578=CARTESIAN_POINT('Ctrl Pts',(-1.17286435586452E-16,-0.957716426222737,
2.80624999999998));
#371579=CARTESIAN_POINT('Ctrl Pts',(0.552937836487023,-0.957716426222737,
2.84374999999998));
#371580=CARTESIAN_POINT('Ctrl Pts',(0.829406754730535,-0.478858213111369,
2.88124999999998));
#371581=CARTESIAN_POINT('Ctrl Pts',(1.10587567297405,-3.30897008283072E-16,
2.91874999999998));
#371582=CARTESIAN_POINT('Ctrl Pts',(0.829406754730536,0.478858213111368,
2.95624999999998));
#371583=CARTESIAN_POINT('Ctrl Pts',(0.552937836487024,0.957716426222737,
2.99374999999998));
#371584=CARTESIAN_POINT('Ctrl Pts',(0.,0.957716426222737,3.03124999999998));
#371585=CARTESIAN_POINT('Ctrl Pts',(-0.552937836487023,0.957716426222737,
3.06874999999998));
#371586=CARTESIAN_POINT('Ctrl Pts',(-0.829406754730535,0.478858213111368,
3.10624999999998));
#371587=CARTESIAN_POINT('Ctrl Pts',(-1.10587567297405,-5.98342883287202E-17,
3.14374999999998));
#371588=CARTESIAN_POINT('Ctrl Pts',(-0.829406754730535,-0.478858213111368,
3.18124999999998));
#371589=CARTESIAN_POINT('Ctrl Pts',(-0.552937836487024,-0.957716426222737,
3.21874999999998));
#371590=CARTESIAN_POINT('Ctrl Pts',(-1.17286435586452E-16,-0.957716426222737,
3.25624999999998));
#371591=CARTESIAN_POINT('Ctrl Pts',(0.552937836487023,-0.957716426222737,
3.29374999999998));
#371592=CARTESIAN_POINT('Ctrl Pts',(0.829406754730535,-0.478858213111369,
3.33124999999998));
#371593=CARTESIAN_POINT('Ctrl Pts',(1.10587567297405,-3.30494409639406E-16,
3.36874999999998));
#371594=CARTESIAN_POINT('Ctrl Pts',(0.829406754730536,0.478858213111368,
3.40624999999998));
#371595=CARTESIAN_POINT('Ctrl Pts',(0.552937836487024,0.957716426222737,
3.44374999999998));
#371596=CARTESIAN_POINT('Ctrl Pts',(0.,0.957716426222737,3.48124999999998));
#371597=CARTESIAN_POINT('Ctrl Pts',(-0.552937836487023,0.957716426222737,
3.51874999999998));
#371598=CARTESIAN_POINT('Ctrl Pts',(-0.829406754730535,0.478858213111368,
3.55624999999998));
#371599=CARTESIAN_POINT('Ctrl Pts',(-1.10587567297405,-5.94316896850542E-17,
3.59374999999998));
#371600=CARTESIAN_POINT('Ctrl Pts',(-0.829406754730535,-0.478858213111368,
3.63124999999998));
#371601=CARTESIAN_POINT('Ctrl Pts',(-0.552937836487024,-0.957716426222737,
3.66874999999998));
#371602=CARTESIAN_POINT('Ctrl Pts',(-1.17286435586452E-16,-0.957716426222737,
3.70624999999998));
#371603=CARTESIAN_POINT('Ctrl Pts',(0.552937836487023,-0.957716426222737,
3.74374999999998));
#371604=CARTESIAN_POINT('Ctrl Pts',(0.829406754730535,-0.478858213111369,
3.78124999999998));
#371605=CARTESIAN_POINT('Ctrl Pts',(1.00369205912859,-0.176987210881325,
3.80488990482708));
#371606=CARTESIAN_POINT('Ctrl Pts',(0.94316952501371,0.16628890564997,3.83177229718761));
#371607=CARTESIAN_POINT('',(0.,0.,0.));
#371608=CARTESIAN_POINT('Origin',(6.93889390390723E-17,9.71445146547012E-16,
-9.21875));
#371609=CARTESIAN_POINT('',(6.93889390390724E-17,-1.17524047358083,-8.9375));
#371610=CARTESIAN_POINT('',(-1.43925448419919E-16,-1.17524047358083,-9.));
#371611=CARTESIAN_POINT('',(2.82703326498063E-16,-1.17524047358083,-9.21875));
#371612=CARTESIAN_POINT('',(-0.823407874165055,-0.838564036615861,-9.));
#371613=CARTESIAN_POINT('Ctrl Pts',(-0.823407874165055,-0.838564036615862,
-9.));
#371614=CARTESIAN_POINT('Ctrl Pts',(-0.480534359260824,-1.17524047358083,
-8.96700849718747));
#371615=CARTESIAN_POINT('Ctrl Pts',(-1.43925448419919E-16,-1.17524047358083,
-8.9375));
#371616=CARTESIAN_POINT('Origin',(0.,1.84795814293585E-15,-9.));
#371617=CARTESIAN_POINT('Origin',(6.93889390390723E-17,9.71445146547012E-16,
-9.21875));
#371618=CARTESIAN_POINT('',(6.93889390390724E-17,-1.17524047358083,-8.4375));
#371619=CARTESIAN_POINT('',(6.93889390390724E-17,-1.17524047358083,-8.5));
#371620=CARTESIAN_POINT('',(2.82703326498063E-16,-1.17524047358083,-9.21875));
#371621=CARTESIAN_POINT('Ctrl Pts',(-1.43925448419919E-16,-1.17524047358083,
-8.9375));
#371622=CARTESIAN_POINT('Ctrl Pts',(0.678525403784437,-1.17524047358083,
-8.89583333333333));
#371623=CARTESIAN_POINT('Ctrl Pts',(1.01778810567666,-0.587620236790417,
-8.85416666666667));
#371624=CARTESIAN_POINT('Ctrl Pts',(1.35705080756888,2.70659426667139E-16,
-8.8125));
#371625=CARTESIAN_POINT('Ctrl Pts',(1.01778810567666,0.587620236790417,
-8.77083333333333));
#371626=CARTESIAN_POINT('Ctrl Pts',(0.678525403784439,1.17524047358083,
-8.72916666666667));
#371627=CARTESIAN_POINT('Ctrl Pts',(0.,1.17524047358083,-8.6875));
#371628=CARTESIAN_POINT('Ctrl Pts',(-0.678525403784438,1.17524047358083,
-8.64583333333334));
#371629=CARTESIAN_POINT('Ctrl Pts',(-1.01778810567666,0.587620236790418,
-8.60416666666667));
#371630=CARTESIAN_POINT('Ctrl Pts',(-1.35705080756888,6.0304101222105E-16,
-8.5625));
#371631=CARTESIAN_POINT('Ctrl Pts',(-1.01778810567666,-0.587620236790416,
-8.52083333333333));
#371632=CARTESIAN_POINT('Ctrl Pts',(-0.678525403784438,-1.17524047358083,
-8.47916666666667));
#371633=CARTESIAN_POINT('Ctrl Pts',(-1.43925448419919E-16,-1.17524047358083,
-8.4375));
#371634=CARTESIAN_POINT('Ctrl Pts',(-1.43925448419919E-16,-1.17524047358083,
-9.));
#371635=CARTESIAN_POINT('Ctrl Pts',(0.678525403784438,-1.17524047358083,
-8.95833333333334));
#371636=CARTESIAN_POINT('Ctrl Pts',(1.01778810567666,-0.587620236790417,
-8.91666666666667));
#371637=CARTESIAN_POINT('Ctrl Pts',(1.35705080756888,2.70659426667139E-16,
-8.875));
#371638=CARTESIAN_POINT('Ctrl Pts',(1.01778810567666,0.587620236790417,
-8.83333333333333));
#371639=CARTESIAN_POINT('Ctrl Pts',(0.678525403784439,1.17524047358083,
-8.79166666666667));
#371640=CARTESIAN_POINT('Ctrl Pts',(0.,1.17524047358083,-8.75));
#371641=CARTESIAN_POINT('Ctrl Pts',(-0.678525403784438,1.17524047358083,
-8.70833333333333));
#371642=CARTESIAN_POINT('Ctrl Pts',(-1.01778810567666,0.587620236790418,
-8.66666666666667));
#371643=CARTESIAN_POINT('Ctrl Pts',(-1.35705080756888,6.0304101222105E-16,
-8.625));
#371644=CARTESIAN_POINT('Ctrl Pts',(-1.01778810567666,-0.587620236790416,
-8.58333333333333));
#371645=CARTESIAN_POINT('Ctrl Pts',(-0.678525403784438,-1.17524047358083,
-8.54166666666667));
#371646=CARTESIAN_POINT('Ctrl Pts',(-1.43925448419919E-16,-1.17524047358083,
-8.5));
#371647=CARTESIAN_POINT('Origin',(6.93889390390723E-17,9.71445146547012E-16,
-9.21875));
#371648=CARTESIAN_POINT('',(6.93889390390724E-17,-1.17524047358083,-7.9375));
#371649=CARTESIAN_POINT('',(6.93889390390724E-17,-1.17524047358083,-8.));
#371650=CARTESIAN_POINT('',(2.82703326498063E-16,-1.17524047358083,-9.21875));
#371651=CARTESIAN_POINT('Ctrl Pts',(-1.43925448419919E-16,-1.17524047358083,
-8.4375));
#371652=CARTESIAN_POINT('Ctrl Pts',(0.678525403784437,-1.17524047358083,
-8.39583333333333));
#371653=CARTESIAN_POINT('Ctrl Pts',(1.01778810567666,-0.587620236790417,
-8.35416666666667));
#371654=CARTESIAN_POINT('Ctrl Pts',(1.35705080756888,2.70659426667139E-16,
-8.3125));
#371655=CARTESIAN_POINT('Ctrl Pts',(1.01778810567666,0.587620236790417,
-8.27083333333333));
#371656=CARTESIAN_POINT('Ctrl Pts',(0.678525403784439,1.17524047358083,
-8.22916666666667));
#371657=CARTESIAN_POINT('Ctrl Pts',(0.,1.17524047358083,-8.1875));
#371658=CARTESIAN_POINT('Ctrl Pts',(-0.678525403784438,1.17524047358083,
-8.14583333333333));
#371659=CARTESIAN_POINT('Ctrl Pts',(-1.01778810567666,0.587620236790418,
-8.10416666666667));
#371660=CARTESIAN_POINT('Ctrl Pts',(-1.35705080756888,6.0304101222105E-16,
-8.0625));
#371661=CARTESIAN_POINT('Ctrl Pts',(-1.01778810567666,-0.587620236790416,
-8.02083333333333));
#371662=CARTESIAN_POINT('Ctrl Pts',(-0.678525403784438,-1.17524047358083,
-7.97916666666667));
#371663=CARTESIAN_POINT('Ctrl Pts',(-1.43925448419919E-16,-1.17524047358083,
-7.9375));
#371664=CARTESIAN_POINT('Ctrl Pts',(-1.43925448419919E-16,-1.17524047358083,
-8.5));
#371665=CARTESIAN_POINT('Ctrl Pts',(0.678525403784437,-1.17524047358083,
-8.45833333333333));
#371666=CARTESIAN_POINT('Ctrl Pts',(1.01778810567666,-0.587620236790417,
-8.41666666666667));
#371667=CARTESIAN_POINT('Ctrl Pts',(1.35705080756888,2.70659426667139E-16,
-8.375));
#371668=CARTESIAN_POINT('Ctrl Pts',(1.01778810567666,0.587620236790417,
-8.33333333333334));
#371669=CARTESIAN_POINT('Ctrl Pts',(0.678525403784439,1.17524047358083,
-8.29166666666667));
#371670=CARTESIAN_POINT('Ctrl Pts',(0.,1.17524047358083,-8.25));
#371671=CARTESIAN_POINT('Ctrl Pts',(-0.678525403784438,1.17524047358083,
-8.20833333333333));
#371672=CARTESIAN_POINT('Ctrl Pts',(-1.01778810567666,0.587620236790418,
-8.16666666666667));
#371673=CARTESIAN_POINT('Ctrl Pts',(-1.35705080756888,6.0304101222105E-16,
-8.125));
#371674=CARTESIAN_POINT('Ctrl Pts',(-1.01778810567666,-0.587620236790416,
-8.08333333333333));
#371675=CARTESIAN_POINT('Ctrl Pts',(-0.678525403784438,-1.17524047358083,
-8.04166666666667));
#371676=CARTESIAN_POINT('Ctrl Pts',(-1.43925448419919E-16,-1.17524047358083,
-8.));
#371677=CARTESIAN_POINT('Origin',(6.93889390390723E-17,9.71445146547012E-16,
-9.21875));
#371678=CARTESIAN_POINT('',(6.93889390390724E-17,-1.17524047358083,-7.4375));
#371679=CARTESIAN_POINT('',(6.93889390390724E-17,-1.17524047358083,-7.5));
#371680=CARTESIAN_POINT('',(2.82703326498063E-16,-1.17524047358083,-9.21875));
#371681=CARTESIAN_POINT('Ctrl Pts',(-1.43925448419919E-16,-1.17524047358083,
-7.9375));
#371682=CARTESIAN_POINT('Ctrl Pts',(0.678525403784437,-1.17524047358083,
-7.89583333333333));
#371683=CARTESIAN_POINT('Ctrl Pts',(1.01778810567666,-0.587620236790417,
-7.85416666666667));
#371684=CARTESIAN_POINT('Ctrl Pts',(1.35705080756888,2.7065942666714E-16,
-7.8125));
#371685=CARTESIAN_POINT('Ctrl Pts',(1.01778810567666,0.587620236790417,
-7.77083333333333));
#371686=CARTESIAN_POINT('Ctrl Pts',(0.678525403784439,1.17524047358083,
-7.72916666666667));
#371687=CARTESIAN_POINT('Ctrl Pts',(0.,1.17524047358083,-7.6875));
#371688=CARTESIAN_POINT('Ctrl Pts',(-0.678525403784438,1.17524047358083,
-7.64583333333333));
#371689=CARTESIAN_POINT('Ctrl Pts',(-1.01778810567666,0.587620236790418,
-7.60416666666667));
#371690=CARTESIAN_POINT('Ctrl Pts',(-1.35705080756888,6.0304101222105E-16,
-7.5625));
#371691=CARTESIAN_POINT('Ctrl Pts',(-1.01778810567666,-0.587620236790416,
-7.52083333333333));
#371692=CARTESIAN_POINT('Ctrl Pts',(-0.678525403784438,-1.17524047358083,
-7.47916666666667));
#371693=CARTESIAN_POINT('Ctrl Pts',(-1.43925448419919E-16,-1.17524047358083,
-7.4375));
#371694=CARTESIAN_POINT('Ctrl Pts',(-1.43925448419919E-16,-1.17524047358083,
-8.));
#371695=CARTESIAN_POINT('Ctrl Pts',(0.678525403784437,-1.17524047358083,
-7.95833333333333));
#371696=CARTESIAN_POINT('Ctrl Pts',(1.01778810567666,-0.587620236790417,
-7.91666666666667));
#371697=CARTESIAN_POINT('Ctrl Pts',(1.35705080756888,2.7065942666714E-16,
-7.875));
#371698=CARTESIAN_POINT('Ctrl Pts',(1.01778810567666,0.587620236790417,
-7.83333333333333));
#371699=CARTESIAN_POINT('Ctrl Pts',(0.678525403784439,1.17524047358083,
-7.79166666666666));
#371700=CARTESIAN_POINT('Ctrl Pts',(0.,1.17524047358083,-7.75));
#371701=CARTESIAN_POINT('Ctrl Pts',(-0.678525403784438,1.17524047358083,
-7.70833333333333));
#371702=CARTESIAN_POINT('Ctrl Pts',(-1.01778810567666,0.587620236790418,
-7.66666666666667));
#371703=CARTESIAN_POINT('Ctrl Pts',(-1.35705080756888,6.0304101222105E-16,
-7.625));
#371704=CARTESIAN_POINT('Ctrl Pts',(-1.01778810567666,-0.587620236790416,
-7.58333333333333));
#371705=CARTESIAN_POINT('Ctrl Pts',(-0.678525403784438,-1.17524047358083,
-7.54166666666667));
#371706=CARTESIAN_POINT('Ctrl Pts',(-1.43925448419919E-16,-1.17524047358083,
-7.5));
#371707=CARTESIAN_POINT('Origin',(6.93889390390723E-17,9.71445146547012E-16,
-9.21875));
#371708=CARTESIAN_POINT('',(6.93889390390724E-17,-1.17524047358083,-6.9375));
#371709=CARTESIAN_POINT('',(6.93889390390724E-17,-1.17524047358083,-7.));
#371710=CARTESIAN_POINT('',(2.82703326498063E-16,-1.17524047358083,-9.21875));
#371711=CARTESIAN_POINT('Ctrl Pts',(-1.43925448419919E-16,-1.17524047358083,
-7.4375));
#371712=CARTESIAN_POINT('Ctrl Pts',(0.678525403784437,-1.17524047358083,
-7.39583333333333));
#371713=CARTESIAN_POINT('Ctrl Pts',(1.01778810567666,-0.587620236790417,
-7.35416666666667));
#371714=CARTESIAN_POINT('Ctrl Pts',(1.35705080756888,2.7065942666714E-16,
-7.3125));
#371715=CARTESIAN_POINT('Ctrl Pts',(1.01778810567666,0.587620236790417,
-7.27083333333333));
#371716=CARTESIAN_POINT('Ctrl Pts',(0.678525403784439,1.17524047358083,
-7.22916666666667));
#371717=CARTESIAN_POINT('Ctrl Pts',(0.,1.17524047358083,-7.1875));
#371718=CARTESIAN_POINT('Ctrl Pts',(-0.678525403784438,1.17524047358083,
-7.14583333333333));
#371719=CARTESIAN_POINT('Ctrl Pts',(-1.01778810567666,0.587620236790418,
-7.10416666666667));
#371720=CARTESIAN_POINT('Ctrl Pts',(-1.35705080756888,6.0304101222105E-16,
-7.0625));
#371721=CARTESIAN_POINT('Ctrl Pts',(-1.01778810567666,-0.587620236790416,
-7.02083333333333));
#371722=CARTESIAN_POINT('Ctrl Pts',(-0.678525403784438,-1.17524047358083,
-6.97916666666667));
#371723=CARTESIAN_POINT('Ctrl Pts',(-1.43925448419919E-16,-1.17524047358083,
-6.9375));
#371724=CARTESIAN_POINT('Ctrl Pts',(-1.43925448419919E-16,-1.17524047358083,
-7.5));
#371725=CARTESIAN_POINT('Ctrl Pts',(0.678525403784437,-1.17524047358083,
-7.45833333333333));
#371726=CARTESIAN_POINT('Ctrl Pts',(1.01778810567666,-0.587620236790417,
-7.41666666666667));
#371727=CARTESIAN_POINT('Ctrl Pts',(1.35705080756888,2.7065942666714E-16,
-7.375));
#371728=CARTESIAN_POINT('Ctrl Pts',(1.01778810567666,0.587620236790417,
-7.33333333333333));
#371729=CARTESIAN_POINT('Ctrl Pts',(0.678525403784439,1.17524047358083,
-7.29166666666667));
#371730=CARTESIAN_POINT('Ctrl Pts',(0.,1.17524047358083,-7.25));
#371731=CARTESIAN_POINT('Ctrl Pts',(-0.678525403784438,1.17524047358083,
-7.20833333333333));
#371732=CARTESIAN_POINT('Ctrl Pts',(-1.01778810567666,0.587620236790418,
-7.16666666666667));
#371733=CARTESIAN_POINT('Ctrl Pts',(-1.35705080756888,6.0304101222105E-16,
-7.125));
#371734=CARTESIAN_POINT('Ctrl Pts',(-1.01778810567666,-0.587620236790416,
-7.08333333333333));
#371735=CARTESIAN_POINT('Ctrl Pts',(-0.678525403784438,-1.17524047358083,
-7.04166666666667));
#371736=CARTESIAN_POINT('Ctrl Pts',(-1.43925448419919E-16,-1.17524047358083,
-7.));
#371737=CARTESIAN_POINT('Origin',(6.93889390390723E-17,9.71445146547012E-16,
-9.21875));
#371738=CARTESIAN_POINT('',(6.93889390390724E-17,-1.17524047358083,-6.4375));
#371739=CARTESIAN_POINT('',(6.93889390390724E-17,-1.17524047358083,-6.5));
#371740=CARTESIAN_POINT('',(2.82703326498063E-16,-1.17524047358083,-9.21875));
#371741=CARTESIAN_POINT('Ctrl Pts',(-1.43925448419919E-16,-1.17524047358083,
-6.9375));
#371742=CARTESIAN_POINT('Ctrl Pts',(0.678525403784437,-1.17524047358083,
-6.89583333333333));
#371743=CARTESIAN_POINT('Ctrl Pts',(1.01778810567666,-0.587620236790417,
-6.85416666666667));
#371744=CARTESIAN_POINT('Ctrl Pts',(1.35705080756888,2.7065942666714E-16,
-6.8125));
#371745=CARTESIAN_POINT('Ctrl Pts',(1.01778810567666,0.587620236790417,
-6.77083333333333));
#371746=CARTESIAN_POINT('Ctrl Pts',(0.678525403784439,1.17524047358083,
-6.72916666666667));
#371747=CARTESIAN_POINT('Ctrl Pts',(0.,1.17524047358083,-6.6875));
#371748=CARTESIAN_POINT('Ctrl Pts',(-0.678525403784438,1.17524047358083,
-6.64583333333333));
#371749=CARTESIAN_POINT('Ctrl Pts',(-1.01778810567666,0.587620236790418,
-6.60416666666667));
#371750=CARTESIAN_POINT('Ctrl Pts',(-1.35705080756888,6.0304101222105E-16,
-6.5625));
#371751=CARTESIAN_POINT('Ctrl Pts',(-1.01778810567666,-0.587620236790416,
-6.52083333333333));
#371752=CARTESIAN_POINT('Ctrl Pts',(-0.678525403784438,-1.17524047358083,
-6.47916666666667));
#371753=CARTESIAN_POINT('Ctrl Pts',(-1.43925448419919E-16,-1.17524047358083,
-6.4375));
#371754=CARTESIAN_POINT('Ctrl Pts',(-1.43925448419919E-16,-1.17524047358083,
-7.));
#371755=CARTESIAN_POINT('Ctrl Pts',(0.678525403784437,-1.17524047358083,
-6.95833333333333));
#371756=CARTESIAN_POINT('Ctrl Pts',(1.01778810567666,-0.587620236790417,
-6.91666666666667));
#371757=CARTESIAN_POINT('Ctrl Pts',(1.35705080756888,2.7065942666714E-16,
-6.875));
#371758=CARTESIAN_POINT('Ctrl Pts',(1.01778810567666,0.587620236790417,
-6.83333333333333));
#371759=CARTESIAN_POINT('Ctrl Pts',(0.678525403784439,1.17524047358083,
-6.79166666666667));
#371760=CARTESIAN_POINT('Ctrl Pts',(0.,1.17524047358083,-6.75));
#371761=CARTESIAN_POINT('Ctrl Pts',(-0.678525403784438,1.17524047358083,
-6.70833333333333));
#371762=CARTESIAN_POINT('Ctrl Pts',(-1.01778810567666,0.587620236790418,
-6.66666666666667));
#371763=CARTESIAN_POINT('Ctrl Pts',(-1.35705080756888,6.0304101222105E-16,
-6.625));
#371764=CARTESIAN_POINT('Ctrl Pts',(-1.01778810567666,-0.587620236790416,
-6.58333333333333));
#371765=CARTESIAN_POINT('Ctrl Pts',(-0.678525403784438,-1.17524047358083,
-6.54166666666667));
#371766=CARTESIAN_POINT('Ctrl Pts',(-1.43925448419919E-16,-1.17524047358083,
-6.5));
#371767=CARTESIAN_POINT('Origin',(6.93889390390723E-17,9.71445146547012E-16,
-9.21875));
#371768=CARTESIAN_POINT('',(6.93889390390724E-17,-1.17524047358083,-5.9375));
#371769=CARTESIAN_POINT('',(6.93889390390724E-17,-1.17524047358083,-6.));
#371770=CARTESIAN_POINT('',(2.82703326498063E-16,-1.17524047358083,-9.21875));
#371771=CARTESIAN_POINT('Ctrl Pts',(-1.43925448419919E-16,-1.17524047358083,
-6.4375));
#371772=CARTESIAN_POINT('Ctrl Pts',(0.678525403784437,-1.17524047358083,
-6.39583333333333));
#371773=CARTESIAN_POINT('Ctrl Pts',(1.01778810567666,-0.587620236790417,
-6.35416666666667));
#371774=CARTESIAN_POINT('Ctrl Pts',(1.35705080756888,2.7065942666714E-16,
-6.3125));
#371775=CARTESIAN_POINT('Ctrl Pts',(1.01778810567666,0.587620236790417,
-6.27083333333333));
#371776=CARTESIAN_POINT('Ctrl Pts',(0.678525403784439,1.17524047358083,
-6.22916666666667));
#371777=CARTESIAN_POINT('Ctrl Pts',(0.,1.17524047358083,-6.1875));
#371778=CARTESIAN_POINT('Ctrl Pts',(-0.678525403784438,1.17524047358083,
-6.14583333333333));
#371779=CARTESIAN_POINT('Ctrl Pts',(-1.01778810567666,0.587620236790418,
-6.10416666666667));
#371780=CARTESIAN_POINT('Ctrl Pts',(-1.35705080756888,6.0304101222105E-16,
-6.0625));
#371781=CARTESIAN_POINT('Ctrl Pts',(-1.01778810567666,-0.587620236790416,
-6.02083333333333));
#371782=CARTESIAN_POINT('Ctrl Pts',(-0.678525403784438,-1.17524047358083,
-5.97916666666667));
#371783=CARTESIAN_POINT('Ctrl Pts',(-1.43925448419919E-16,-1.17524047358083,
-5.9375));
#371784=CARTESIAN_POINT('Ctrl Pts',(-1.43925448419919E-16,-1.17524047358083,
-6.5));
#371785=CARTESIAN_POINT('Ctrl Pts',(0.678525403784437,-1.17524047358083,
-6.45833333333333));
#371786=CARTESIAN_POINT('Ctrl Pts',(1.01778810567666,-0.587620236790417,
-6.41666666666667));
#371787=CARTESIAN_POINT('Ctrl Pts',(1.35705080756888,2.7065942666714E-16,
-6.375));
#371788=CARTESIAN_POINT('Ctrl Pts',(1.01778810567666,0.587620236790417,
-6.33333333333333));
#371789=CARTESIAN_POINT('Ctrl Pts',(0.678525403784439,1.17524047358083,
-6.29166666666667));
#371790=CARTESIAN_POINT('Ctrl Pts',(0.,1.17524047358083,-6.25));
#371791=CARTESIAN_POINT('Ctrl Pts',(-0.678525403784438,1.17524047358083,
-6.20833333333333));
#371792=CARTESIAN_POINT('Ctrl Pts',(-1.01778810567666,0.587620236790418,
-6.16666666666667));
#371793=CARTESIAN_POINT('Ctrl Pts',(-1.35705080756888,6.0304101222105E-16,
-6.125));
#371794=CARTESIAN_POINT('Ctrl Pts',(-1.01778810567666,-0.587620236790416,
-6.08333333333333));
#371795=CARTESIAN_POINT('Ctrl Pts',(-0.678525403784438,-1.17524047358083,
-6.04166666666667));
#371796=CARTESIAN_POINT('Ctrl Pts',(-1.43925448419919E-16,-1.17524047358083,
-6.));
#371797=CARTESIAN_POINT('Origin',(6.93889390390723E-17,9.71445146547012E-16,
-9.21875));
#371798=CARTESIAN_POINT('',(6.93889390390724E-17,-1.17524047358083,-5.4375));
#371799=CARTESIAN_POINT('',(6.93889390390724E-17,-1.17524047358083,-5.5));
#371800=CARTESIAN_POINT('',(2.82703326498063E-16,-1.17524047358083,-9.21875));
#371801=CARTESIAN_POINT('Ctrl Pts',(-1.43925448419919E-16,-1.17524047358083,
-5.9375));
#371802=CARTESIAN_POINT('Ctrl Pts',(0.678525403784437,-1.17524047358083,
-5.89583333333333));
#371803=CARTESIAN_POINT('Ctrl Pts',(1.01778810567666,-0.587620236790417,
-5.85416666666667));
#371804=CARTESIAN_POINT('Ctrl Pts',(1.35705080756888,2.7065942666714E-16,
-5.8125));
#371805=CARTESIAN_POINT('Ctrl Pts',(1.01778810567666,0.587620236790417,
-5.77083333333333));
#371806=CARTESIAN_POINT('Ctrl Pts',(0.678525403784439,1.17524047358083,
-5.72916666666667));
#371807=CARTESIAN_POINT('Ctrl Pts',(0.,1.17524047358083,-5.6875));
#371808=CARTESIAN_POINT('Ctrl Pts',(-0.678525403784438,1.17524047358083,
-5.64583333333333));
#371809=CARTESIAN_POINT('Ctrl Pts',(-1.01778810567666,0.587620236790418,
-5.60416666666667));
#371810=CARTESIAN_POINT('Ctrl Pts',(-1.35705080756888,6.0304101222105E-16,
-5.5625));
#371811=CARTESIAN_POINT('Ctrl Pts',(-1.01778810567666,-0.587620236790416,
-5.52083333333333));
#371812=CARTESIAN_POINT('Ctrl Pts',(-0.678525403784438,-1.17524047358083,
-5.47916666666667));
#371813=CARTESIAN_POINT('Ctrl Pts',(-1.43925448419919E-16,-1.17524047358083,
-5.4375));
#371814=CARTESIAN_POINT('Ctrl Pts',(-1.43925448419919E-16,-1.17524047358083,
-6.));
#371815=CARTESIAN_POINT('Ctrl Pts',(0.678525403784437,-1.17524047358083,
-5.95833333333333));
#371816=CARTESIAN_POINT('Ctrl Pts',(1.01778810567666,-0.587620236790417,
-5.91666666666667));
#371817=CARTESIAN_POINT('Ctrl Pts',(1.35705080756888,2.7065942666714E-16,
-5.875));
#371818=CARTESIAN_POINT('Ctrl Pts',(1.01778810567666,0.587620236790417,
-5.83333333333333));
#371819=CARTESIAN_POINT('Ctrl Pts',(0.678525403784439,1.17524047358083,
-5.79166666666667));
#371820=CARTESIAN_POINT('Ctrl Pts',(0.,1.17524047358083,-5.75));
#371821=CARTESIAN_POINT('Ctrl Pts',(-0.678525403784438,1.17524047358083,
-5.70833333333333));
#371822=CARTESIAN_POINT('Ctrl Pts',(-1.01778810567666,0.587620236790418,
-5.66666666666667));
#371823=CARTESIAN_POINT('Ctrl Pts',(-1.35705080756888,6.0304101222105E-16,
-5.625));
#371824=CARTESIAN_POINT('Ctrl Pts',(-1.01778810567666,-0.587620236790416,
-5.58333333333333));
#371825=CARTESIAN_POINT('Ctrl Pts',(-0.678525403784438,-1.17524047358083,
-5.54166666666667));
#371826=CARTESIAN_POINT('Ctrl Pts',(-1.43925448419919E-16,-1.17524047358083,
-5.5));
#371827=CARTESIAN_POINT('Origin',(6.93889390390723E-17,9.71445146547012E-16,
-9.21875));
#371828=CARTESIAN_POINT('',(6.93889390390724E-17,-1.17524047358083,-4.9375));
#371829=CARTESIAN_POINT('',(6.93889390390724E-17,-1.17524047358083,-5.));
#371830=CARTESIAN_POINT('',(2.82703326498063E-16,-1.17524047358083,-9.21875));
#371831=CARTESIAN_POINT('Ctrl Pts',(-1.43925448419919E-16,-1.17524047358083,
-5.4375));
#371832=CARTESIAN_POINT('Ctrl Pts',(0.678525403784437,-1.17524047358083,
-5.39583333333333));
#371833=CARTESIAN_POINT('Ctrl Pts',(1.01778810567666,-0.587620236790417,
-5.35416666666667));
#371834=CARTESIAN_POINT('Ctrl Pts',(1.35705080756888,2.7065942666714E-16,
-5.3125));
#371835=CARTESIAN_POINT('Ctrl Pts',(1.01778810567666,0.587620236790417,
-5.27083333333333));
#371836=CARTESIAN_POINT('Ctrl Pts',(0.678525403784439,1.17524047358083,
-5.22916666666667));
#371837=CARTESIAN_POINT('Ctrl Pts',(0.,1.17524047358083,-5.1875));
#371838=CARTESIAN_POINT('Ctrl Pts',(-0.678525403784438,1.17524047358083,
-5.14583333333333));
#371839=CARTESIAN_POINT('Ctrl Pts',(-1.01778810567666,0.587620236790418,
-5.10416666666667));
#371840=CARTESIAN_POINT('Ctrl Pts',(-1.35705080756888,6.0304101222105E-16,
-5.0625));
#371841=CARTESIAN_POINT('Ctrl Pts',(-1.01778810567666,-0.587620236790416,
-5.02083333333333));
#371842=CARTESIAN_POINT('Ctrl Pts',(-0.678525403784438,-1.17524047358083,
-4.97916666666667));
#371843=CARTESIAN_POINT('Ctrl Pts',(-1.43925448419919E-16,-1.17524047358083,
-4.9375));
#371844=CARTESIAN_POINT('Ctrl Pts',(-1.43925448419919E-16,-1.17524047358083,
-5.5));
#371845=CARTESIAN_POINT('Ctrl Pts',(0.678525403784437,-1.17524047358083,
-5.45833333333333));
#371846=CARTESIAN_POINT('Ctrl Pts',(1.01778810567666,-0.587620236790417,
-5.41666666666667));
#371847=CARTESIAN_POINT('Ctrl Pts',(1.35705080756888,2.7065942666714E-16,
-5.375));
#371848=CARTESIAN_POINT('Ctrl Pts',(1.01778810567666,0.587620236790417,
-5.33333333333333));
#371849=CARTESIAN_POINT('Ctrl Pts',(0.678525403784439,1.17524047358083,
-5.29166666666667));
#371850=CARTESIAN_POINT('Ctrl Pts',(0.,1.17524047358083,-5.25));
#371851=CARTESIAN_POINT('Ctrl Pts',(-0.678525403784438,1.17524047358083,
-5.20833333333333));
#371852=CARTESIAN_POINT('Ctrl Pts',(-1.01778810567666,0.587620236790418,
-5.16666666666667));
#371853=CARTESIAN_POINT('Ctrl Pts',(-1.35705080756888,6.0304101222105E-16,
-5.125));
#371854=CARTESIAN_POINT('Ctrl Pts',(-1.01778810567666,-0.587620236790416,
-5.08333333333333));
#371855=CARTESIAN_POINT('Ctrl Pts',(-0.678525403784438,-1.17524047358083,
-5.04166666666667));
#371856=CARTESIAN_POINT('Ctrl Pts',(-1.43925448419919E-16,-1.17524047358083,
-5.));
#371857=CARTESIAN_POINT('Origin',(6.93889390390723E-17,9.71445146547012E-16,
-9.21875));
#371858=CARTESIAN_POINT('',(6.93889390390724E-17,-1.17524047358083,-4.4375));
#371859=CARTESIAN_POINT('',(6.93889390390724E-17,-1.17524047358083,-4.5));
#371860=CARTESIAN_POINT('',(2.82703326498063E-16,-1.17524047358083,-9.21875));
#371861=CARTESIAN_POINT('Ctrl Pts',(-1.43925448419919E-16,-1.17524047358083,
-4.9375));
#371862=CARTESIAN_POINT('Ctrl Pts',(0.678525403784437,-1.17524047358083,
-4.89583333333333));
#371863=CARTESIAN_POINT('Ctrl Pts',(1.01778810567666,-0.587620236790417,
-4.85416666666667));
#371864=CARTESIAN_POINT('Ctrl Pts',(1.35705080756888,2.7065942666714E-16,
-4.8125));
#371865=CARTESIAN_POINT('Ctrl Pts',(1.01778810567666,0.587620236790417,
-4.77083333333333));
#371866=CARTESIAN_POINT('Ctrl Pts',(0.678525403784439,1.17524047358083,
-4.72916666666667));
#371867=CARTESIAN_POINT('Ctrl Pts',(0.,1.17524047358083,-4.6875));
#371868=CARTESIAN_POINT('Ctrl Pts',(-0.678525403784438,1.17524047358083,
-4.64583333333333));
#371869=CARTESIAN_POINT('Ctrl Pts',(-1.01778810567666,0.587620236790418,
-4.60416666666667));
#371870=CARTESIAN_POINT('Ctrl Pts',(-1.35705080756888,6.0304101222105E-16,
-4.5625));
#371871=CARTESIAN_POINT('Ctrl Pts',(-1.01778810567666,-0.587620236790416,
-4.52083333333333));
#371872=CARTESIAN_POINT('Ctrl Pts',(-0.678525403784438,-1.17524047358083,
-4.47916666666667));
#371873=CARTESIAN_POINT('Ctrl Pts',(-1.43925448419919E-16,-1.17524047358083,
-4.4375));
#371874=CARTESIAN_POINT('Ctrl Pts',(-1.43925448419919E-16,-1.17524047358083,
-5.));
#371875=CARTESIAN_POINT('Ctrl Pts',(0.678525403784437,-1.17524047358083,
-4.95833333333333));
#371876=CARTESIAN_POINT('Ctrl Pts',(1.01778810567666,-0.587620236790417,
-4.91666666666667));
#371877=CARTESIAN_POINT('Ctrl Pts',(1.35705080756888,2.7065942666714E-16,
-4.875));
#371878=CARTESIAN_POINT('Ctrl Pts',(1.01778810567666,0.587620236790417,
-4.83333333333333));
#371879=CARTESIAN_POINT('Ctrl Pts',(0.678525403784439,1.17524047358083,
-4.79166666666667));
#371880=CARTESIAN_POINT('Ctrl Pts',(0.,1.17524047358083,-4.75));
#371881=CARTESIAN_POINT('Ctrl Pts',(-0.678525403784438,1.17524047358083,
-4.70833333333333));
#371882=CARTESIAN_POINT('Ctrl Pts',(-1.01778810567666,0.587620236790418,
-4.66666666666667));
#371883=CARTESIAN_POINT('Ctrl Pts',(-1.35705080756888,6.0304101222105E-16,
-4.625));
#371884=CARTESIAN_POINT('Ctrl Pts',(-1.01778810567666,-0.587620236790416,
-4.58333333333333));
#371885=CARTESIAN_POINT('Ctrl Pts',(-0.678525403784438,-1.17524047358083,
-4.54166666666667));
#371886=CARTESIAN_POINT('Ctrl Pts',(-1.43925448419919E-16,-1.17524047358083,
-4.5));
#371887=CARTESIAN_POINT('Origin',(6.93889390390723E-17,9.71445146547012E-16,
-9.21875));
#371888=CARTESIAN_POINT('',(6.93889390390724E-17,-1.17524047358083,-3.9375));
#371889=CARTESIAN_POINT('',(6.93889390390724E-17,-1.17524047358083,-4.));
#371890=CARTESIAN_POINT('',(2.82703326498063E-16,-1.17524047358083,-9.21875));
#371891=CARTESIAN_POINT('Ctrl Pts',(-1.43925448419919E-16,-1.17524047358083,
-4.4375));
#371892=CARTESIAN_POINT('Ctrl Pts',(0.678525403784437,-1.17524047358083,
-4.39583333333333));
#371893=CARTESIAN_POINT('Ctrl Pts',(1.01778810567666,-0.587620236790417,
-4.35416666666667));
#371894=CARTESIAN_POINT('Ctrl Pts',(1.35705080756888,2.7065942666714E-16,
-4.3125));
#371895=CARTESIAN_POINT('Ctrl Pts',(1.01778810567666,0.587620236790417,
-4.27083333333333));
#371896=CARTESIAN_POINT('Ctrl Pts',(0.678525403784439,1.17524047358083,
-4.22916666666667));
#371897=CARTESIAN_POINT('Ctrl Pts',(0.,1.17524047358083,-4.1875));
#371898=CARTESIAN_POINT('Ctrl Pts',(-0.678525403784438,1.17524047358083,
-4.14583333333333));
#371899=CARTESIAN_POINT('Ctrl Pts',(-1.01778810567666,0.587620236790418,
-4.10416666666667));
#371900=CARTESIAN_POINT('Ctrl Pts',(-1.35705080756888,6.0304101222105E-16,
-4.0625));
#371901=CARTESIAN_POINT('Ctrl Pts',(-1.01778810567666,-0.587620236790416,
-4.02083333333333));
#371902=CARTESIAN_POINT('Ctrl Pts',(-0.678525403784438,-1.17524047358083,
-3.97916666666667));
#371903=CARTESIAN_POINT('Ctrl Pts',(-1.43925448419919E-16,-1.17524047358083,
-3.9375));
#371904=CARTESIAN_POINT('Ctrl Pts',(-1.43925448419919E-16,-1.17524047358083,
-4.5));
#371905=CARTESIAN_POINT('Ctrl Pts',(0.678525403784437,-1.17524047358083,
-4.45833333333333));
#371906=CARTESIAN_POINT('Ctrl Pts',(1.01778810567666,-0.587620236790417,
-4.41666666666667));
#371907=CARTESIAN_POINT('Ctrl Pts',(1.35705080756888,2.7065942666714E-16,
-4.375));
#371908=CARTESIAN_POINT('Ctrl Pts',(1.01778810567666,0.587620236790417,
-4.33333333333333));
#371909=CARTESIAN_POINT('Ctrl Pts',(0.678525403784439,1.17524047358083,
-4.29166666666667));
#371910=CARTESIAN_POINT('Ctrl Pts',(0.,1.17524047358083,-4.25));
#371911=CARTESIAN_POINT('Ctrl Pts',(-0.678525403784438,1.17524047358083,
-4.20833333333333));
#371912=CARTESIAN_POINT('Ctrl Pts',(-1.01778810567666,0.587620236790418,
-4.16666666666667));
#371913=CARTESIAN_POINT('Ctrl Pts',(-1.35705080756888,6.0304101222105E-16,
-4.125));
#371914=CARTESIAN_POINT('Ctrl Pts',(-1.01778810567666,-0.587620236790416,
-4.08333333333333));
#371915=CARTESIAN_POINT('Ctrl Pts',(-0.678525403784438,-1.17524047358083,
-4.04166666666667));
#371916=CARTESIAN_POINT('Ctrl Pts',(-1.43925448419919E-16,-1.17524047358083,
-4.));
#371917=CARTESIAN_POINT('Origin',(6.93889390390723E-17,9.71445146547012E-16,
-9.21875));
#371918=CARTESIAN_POINT('',(6.93889390390724E-17,-1.17524047358083,-3.4375));
#371919=CARTESIAN_POINT('',(6.93889390390724E-17,-1.17524047358083,-3.5));
#371920=CARTESIAN_POINT('',(2.82703326498063E-16,-1.17524047358083,-9.21875));
#371921=CARTESIAN_POINT('Ctrl Pts',(-1.43925448419919E-16,-1.17524047358083,
-3.9375));
#371922=CARTESIAN_POINT('Ctrl Pts',(0.678525403784437,-1.17524047358083,
-3.89583333333333));
#371923=CARTESIAN_POINT('Ctrl Pts',(1.01778810567666,-0.587620236790417,
-3.85416666666667));
#371924=CARTESIAN_POINT('Ctrl Pts',(1.35705080756888,2.7065942666714E-16,
-3.8125));
#371925=CARTESIAN_POINT('Ctrl Pts',(1.01778810567666,0.587620236790417,
-3.77083333333333));
#371926=CARTESIAN_POINT('Ctrl Pts',(0.678525403784439,1.17524047358083,
-3.72916666666667));
#371927=CARTESIAN_POINT('Ctrl Pts',(0.,1.17524047358083,-3.6875));
#371928=CARTESIAN_POINT('Ctrl Pts',(-0.678525403784438,1.17524047358083,
-3.64583333333333));
#371929=CARTESIAN_POINT('Ctrl Pts',(-1.01778810567666,0.587620236790418,
-3.60416666666667));
#371930=CARTESIAN_POINT('Ctrl Pts',(-1.35705080756888,6.0304101222105E-16,
-3.5625));
#371931=CARTESIAN_POINT('Ctrl Pts',(-1.01778810567666,-0.587620236790416,
-3.52083333333333));
#371932=CARTESIAN_POINT('Ctrl Pts',(-0.678525403784438,-1.17524047358083,
-3.47916666666667));
#371933=CARTESIAN_POINT('Ctrl Pts',(-1.43925448419919E-16,-1.17524047358083,
-3.4375));
#371934=CARTESIAN_POINT('Ctrl Pts',(-1.43925448419919E-16,-1.17524047358083,
-4.));
#371935=CARTESIAN_POINT('Ctrl Pts',(0.678525403784437,-1.17524047358083,
-3.95833333333333));
#371936=CARTESIAN_POINT('Ctrl Pts',(1.01778810567666,-0.587620236790417,
-3.91666666666667));
#371937=CARTESIAN_POINT('Ctrl Pts',(1.35705080756888,2.7065942666714E-16,
-3.875));
#371938=CARTESIAN_POINT('Ctrl Pts',(1.01778810567666,0.587620236790417,
-3.83333333333333));
#371939=CARTESIAN_POINT('Ctrl Pts',(0.678525403784439,1.17524047358083,
-3.79166666666667));
#371940=CARTESIAN_POINT('Ctrl Pts',(0.,1.17524047358083,-3.75));
#371941=CARTESIAN_POINT('Ctrl Pts',(-0.678525403784438,1.17524047358083,
-3.70833333333333));
#371942=CARTESIAN_POINT('Ctrl Pts',(-1.01778810567666,0.587620236790418,
-3.66666666666667));
#371943=CARTESIAN_POINT('Ctrl Pts',(-1.35705080756888,6.0304101222105E-16,
-3.625));
#371944=CARTESIAN_POINT('Ctrl Pts',(-1.01778810567666,-0.587620236790416,
-3.58333333333333));
#371945=CARTESIAN_POINT('Ctrl Pts',(-0.678525403784438,-1.17524047358083,
-3.54166666666667));
#371946=CARTESIAN_POINT('Ctrl Pts',(-1.43925448419919E-16,-1.17524047358083,
-3.5));
#371947=CARTESIAN_POINT('Origin',(6.93889390390723E-17,9.71445146547012E-16,
-9.21875));
#371948=CARTESIAN_POINT('',(6.93889390390724E-17,-1.17524047358083,-2.9375));
#371949=CARTESIAN_POINT('',(6.93889390390724E-17,-1.17524047358083,-3.));
#371950=CARTESIAN_POINT('',(2.82703326498063E-16,-1.17524047358083,-9.21875));
#371951=CARTESIAN_POINT('Ctrl Pts',(-1.43925448419919E-16,-1.17524047358083,
-3.4375));
#371952=CARTESIAN_POINT('Ctrl Pts',(0.678525403784437,-1.17524047358083,
-3.39583333333333));
#371953=CARTESIAN_POINT('Ctrl Pts',(1.01778810567666,-0.587620236790417,
-3.35416666666667));
#371954=CARTESIAN_POINT('Ctrl Pts',(1.35705080756888,2.7065942666714E-16,
-3.3125));
#371955=CARTESIAN_POINT('Ctrl Pts',(1.01778810567666,0.587620236790417,
-3.27083333333333));
#371956=CARTESIAN_POINT('Ctrl Pts',(0.678525403784439,1.17524047358083,
-3.22916666666667));
#371957=CARTESIAN_POINT('Ctrl Pts',(0.,1.17524047358083,-3.1875));
#371958=CARTESIAN_POINT('Ctrl Pts',(-0.678525403784438,1.17524047358083,
-3.14583333333333));
#371959=CARTESIAN_POINT('Ctrl Pts',(-1.01778810567666,0.587620236790418,
-3.10416666666667));
#371960=CARTESIAN_POINT('Ctrl Pts',(-1.35705080756888,6.0304101222105E-16,
-3.0625));
#371961=CARTESIAN_POINT('Ctrl Pts',(-1.01778810567666,-0.587620236790416,
-3.02083333333333));
#371962=CARTESIAN_POINT('Ctrl Pts',(-0.678525403784438,-1.17524047358083,
-2.97916666666667));
#371963=CARTESIAN_POINT('Ctrl Pts',(-1.43925448419919E-16,-1.17524047358083,
-2.9375));
#371964=CARTESIAN_POINT('Ctrl Pts',(-1.43925448419919E-16,-1.17524047358083,
-3.5));
#371965=CARTESIAN_POINT('Ctrl Pts',(0.678525403784437,-1.17524047358083,
-3.45833333333333));
#371966=CARTESIAN_POINT('Ctrl Pts',(1.01778810567666,-0.587620236790417,
-3.41666666666667));
#371967=CARTESIAN_POINT('Ctrl Pts',(1.35705080756888,2.7065942666714E-16,
-3.375));
#371968=CARTESIAN_POINT('Ctrl Pts',(1.01778810567666,0.587620236790417,
-3.33333333333333));
#371969=CARTESIAN_POINT('Ctrl Pts',(0.678525403784439,1.17524047358083,
-3.29166666666667));
#371970=CARTESIAN_POINT('Ctrl Pts',(0.,1.17524047358083,-3.25));
#371971=CARTESIAN_POINT('Ctrl Pts',(-0.678525403784438,1.17524047358083,
-3.20833333333333));
#371972=CARTESIAN_POINT('Ctrl Pts',(-1.01778810567666,0.587620236790418,
-3.16666666666667));
#371973=CARTESIAN_POINT('Ctrl Pts',(-1.35705080756888,6.0304101222105E-16,
-3.125));
#371974=CARTESIAN_POINT('Ctrl Pts',(-1.01778810567666,-0.587620236790416,
-3.08333333333333));
#371975=CARTESIAN_POINT('Ctrl Pts',(-0.678525403784438,-1.17524047358083,
-3.04166666666667));
#371976=CARTESIAN_POINT('Ctrl Pts',(-1.43925448419919E-16,-1.17524047358083,
-3.));
#371977=CARTESIAN_POINT('Origin',(6.93889390390723E-17,9.71445146547012E-16,
-9.21875));
#371978=CARTESIAN_POINT('',(6.93889390390724E-17,-1.17524047358083,-2.4375));
#371979=CARTESIAN_POINT('',(6.93889390390724E-17,-1.17524047358083,-2.5));
#371980=CARTESIAN_POINT('',(2.82703326498063E-16,-1.17524047358083,-9.21875));
#371981=CARTESIAN_POINT('Ctrl Pts',(-1.43925448419919E-16,-1.17524047358083,
-2.9375));
#371982=CARTESIAN_POINT('Ctrl Pts',(0.678525403784437,-1.17524047358083,
-2.89583333333333));
#371983=CARTESIAN_POINT('Ctrl Pts',(1.01778810567666,-0.587620236790417,
-2.85416666666667));
#371984=CARTESIAN_POINT('Ctrl Pts',(1.35705080756888,2.7065942666714E-16,
-2.8125));
#371985=CARTESIAN_POINT('Ctrl Pts',(1.01778810567666,0.587620236790417,
-2.77083333333333));
#371986=CARTESIAN_POINT('Ctrl Pts',(0.678525403784439,1.17524047358083,
-2.72916666666667));
#371987=CARTESIAN_POINT('Ctrl Pts',(0.,1.17524047358083,-2.6875));
#371988=CARTESIAN_POINT('Ctrl Pts',(-0.678525403784438,1.17524047358083,
-2.64583333333333));
#371989=CARTESIAN_POINT('Ctrl Pts',(-1.01778810567666,0.587620236790418,
-2.60416666666667));
#371990=CARTESIAN_POINT('Ctrl Pts',(-1.35705080756888,6.03041012221051E-16,
-2.5625));
#371991=CARTESIAN_POINT('Ctrl Pts',(-1.01778810567666,-0.587620236790416,
-2.52083333333333));
#371992=CARTESIAN_POINT('Ctrl Pts',(-0.678525403784438,-1.17524047358083,
-2.47916666666667));
#371993=CARTESIAN_POINT('Ctrl Pts',(-1.43925448419919E-16,-1.17524047358083,
-2.4375));
#371994=CARTESIAN_POINT('Ctrl Pts',(-1.43925448419919E-16,-1.17524047358083,
-3.));
#371995=CARTESIAN_POINT('Ctrl Pts',(0.678525403784437,-1.17524047358083,
-2.95833333333333));
#371996=CARTESIAN_POINT('Ctrl Pts',(1.01778810567666,-0.587620236790417,
-2.91666666666667));
#371997=CARTESIAN_POINT('Ctrl Pts',(1.35705080756888,2.7065942666714E-16,
-2.875));
#371998=CARTESIAN_POINT('Ctrl Pts',(1.01778810567666,0.587620236790417,
-2.83333333333333));
#371999=CARTESIAN_POINT('Ctrl Pts',(0.678525403784439,1.17524047358083,
-2.79166666666667));
#372000=CARTESIAN_POINT('Ctrl Pts',(0.,1.17524047358083,-2.75));
#372001=CARTESIAN_POINT('Ctrl Pts',(-0.678525403784438,1.17524047358083,
-2.70833333333333));
#372002=CARTESIAN_POINT('Ctrl Pts',(-1.01778810567666,0.587620236790418,
-2.66666666666667));
#372003=CARTESIAN_POINT('Ctrl Pts',(-1.35705080756888,6.03041012221051E-16,
-2.625));
#372004=CARTESIAN_POINT('Ctrl Pts',(-1.01778810567666,-0.587620236790416,
-2.58333333333333));
#372005=CARTESIAN_POINT('Ctrl Pts',(-0.678525403784438,-1.17524047358083,
-2.54166666666667));
#372006=CARTESIAN_POINT('Ctrl Pts',(-1.43925448419919E-16,-1.17524047358083,
-2.5));
#372007=CARTESIAN_POINT('Origin',(6.93889390390723E-17,9.71445146547012E-16,
-9.21875));
#372008=CARTESIAN_POINT('',(6.93889390390724E-17,-1.17524047358083,-1.9375));
#372009=CARTESIAN_POINT('',(6.93889390390724E-17,-1.17524047358083,-2.));
#372010=CARTESIAN_POINT('',(2.82703326498063E-16,-1.17524047358083,-9.21875));
#372011=CARTESIAN_POINT('Ctrl Pts',(-1.43925448419919E-16,-1.17524047358083,
-2.4375));
#372012=CARTESIAN_POINT('Ctrl Pts',(0.678525403784437,-1.17524047358083,
-2.39583333333333));
#372013=CARTESIAN_POINT('Ctrl Pts',(1.01778810567666,-0.587620236790417,
-2.35416666666667));
#372014=CARTESIAN_POINT('Ctrl Pts',(1.35705080756888,2.7065942666714E-16,
-2.3125));
#372015=CARTESIAN_POINT('Ctrl Pts',(1.01778810567666,0.587620236790417,
-2.27083333333333));
#372016=CARTESIAN_POINT('Ctrl Pts',(0.678525403784439,1.17524047358083,
-2.22916666666667));
#372017=CARTESIAN_POINT('Ctrl Pts',(0.,1.17524047358083,-2.1875));
#372018=CARTESIAN_POINT('Ctrl Pts',(-0.678525403784438,1.17524047358083,
-2.14583333333333));
#372019=CARTESIAN_POINT('Ctrl Pts',(-1.01778810567666,0.587620236790418,
-2.10416666666667));
#372020=CARTESIAN_POINT('Ctrl Pts',(-1.35705080756888,6.03041012221051E-16,
-2.0625));
#372021=CARTESIAN_POINT('Ctrl Pts',(-1.01778810567666,-0.587620236790416,
-2.02083333333333));
#372022=CARTESIAN_POINT('Ctrl Pts',(-0.678525403784438,-1.17524047358083,
-1.97916666666667));
#372023=CARTESIAN_POINT('Ctrl Pts',(-1.43925448419919E-16,-1.17524047358083,
-1.9375));
#372024=CARTESIAN_POINT('Ctrl Pts',(-1.43925448419919E-16,-1.17524047358083,
-2.5));
#372025=CARTESIAN_POINT('Ctrl Pts',(0.678525403784437,-1.17524047358083,
-2.45833333333333));
#372026=CARTESIAN_POINT('Ctrl Pts',(1.01778810567666,-0.587620236790417,
-2.41666666666667));
#372027=CARTESIAN_POINT('Ctrl Pts',(1.35705080756888,2.7065942666714E-16,
-2.375));
#372028=CARTESIAN_POINT('Ctrl Pts',(1.01778810567666,0.587620236790417,
-2.33333333333333));
#372029=CARTESIAN_POINT('Ctrl Pts',(0.678525403784439,1.17524047358083,
-2.29166666666667));
#372030=CARTESIAN_POINT('Ctrl Pts',(0.,1.17524047358083,-2.25));
#372031=CARTESIAN_POINT('Ctrl Pts',(-0.678525403784438,1.17524047358083,
-2.20833333333333));
#372032=CARTESIAN_POINT('Ctrl Pts',(-1.01778810567666,0.587620236790418,
-2.16666666666667));
#372033=CARTESIAN_POINT('Ctrl Pts',(-1.35705080756888,6.03041012221051E-16,
-2.125));
#372034=CARTESIAN_POINT('Ctrl Pts',(-1.01778810567666,-0.587620236790416,
-2.08333333333333));
#372035=CARTESIAN_POINT('Ctrl Pts',(-0.678525403784438,-1.17524047358083,
-2.04166666666667));
#372036=CARTESIAN_POINT('Ctrl Pts',(-1.43925448419919E-16,-1.17524047358083,
-2.));
#372037=CARTESIAN_POINT('Origin',(6.93889390390723E-17,9.71445146547012E-16,
-9.21875));
#372038=CARTESIAN_POINT('',(6.93889390390724E-17,-1.17524047358083,-1.4375));
#372039=CARTESIAN_POINT('',(6.93889390390724E-17,-1.17524047358083,-1.5));
#372040=CARTESIAN_POINT('',(2.82703326498063E-16,-1.17524047358083,-9.21875));
#372041=CARTESIAN_POINT('Ctrl Pts',(-1.43925448419919E-16,-1.17524047358083,
-1.9375));
#372042=CARTESIAN_POINT('Ctrl Pts',(0.678525403784437,-1.17524047358083,
-1.89583333333333));
#372043=CARTESIAN_POINT('Ctrl Pts',(1.01778810567666,-0.587620236790417,
-1.85416666666667));
#372044=CARTESIAN_POINT('Ctrl Pts',(1.35705080756888,2.7065942666714E-16,
-1.8125));
#372045=CARTESIAN_POINT('Ctrl Pts',(1.01778810567666,0.587620236790417,
-1.77083333333333));
#372046=CARTESIAN_POINT('Ctrl Pts',(0.678525403784439,1.17524047358083,
-1.72916666666667));
#372047=CARTESIAN_POINT('Ctrl Pts',(0.,1.17524047358083,-1.6875));
#372048=CARTESIAN_POINT('Ctrl Pts',(-0.678525403784438,1.17524047358083,
-1.64583333333333));
#372049=CARTESIAN_POINT('Ctrl Pts',(-1.01778810567666,0.587620236790418,
-1.60416666666667));
#372050=CARTESIAN_POINT('Ctrl Pts',(-1.35705080756888,6.03041012221051E-16,
-1.5625));
#372051=CARTESIAN_POINT('Ctrl Pts',(-1.01778810567666,-0.587620236790416,
-1.52083333333333));
#372052=CARTESIAN_POINT('Ctrl Pts',(-0.678525403784438,-1.17524047358083,
-1.47916666666667));
#372053=CARTESIAN_POINT('Ctrl Pts',(-1.43925448419919E-16,-1.17524047358083,
-1.4375));
#372054=CARTESIAN_POINT('Ctrl Pts',(-1.43925448419919E-16,-1.17524047358083,
-2.));
#372055=CARTESIAN_POINT('Ctrl Pts',(0.678525403784437,-1.17524047358083,
-1.95833333333333));
#372056=CARTESIAN_POINT('Ctrl Pts',(1.01778810567666,-0.587620236790417,
-1.91666666666667));
#372057=CARTESIAN_POINT('Ctrl Pts',(1.35705080756888,2.7065942666714E-16,
-1.875));
#372058=CARTESIAN_POINT('Ctrl Pts',(1.01778810567666,0.587620236790417,
-1.83333333333333));
#372059=CARTESIAN_POINT('Ctrl Pts',(0.678525403784439,1.17524047358083,
-1.79166666666667));
#372060=CARTESIAN_POINT('Ctrl Pts',(0.,1.17524047358083,-1.75));
#372061=CARTESIAN_POINT('Ctrl Pts',(-0.678525403784438,1.17524047358083,
-1.70833333333333));
#372062=CARTESIAN_POINT('Ctrl Pts',(-1.01778810567666,0.587620236790418,
-1.66666666666667));
#372063=CARTESIAN_POINT('Ctrl Pts',(-1.35705080756888,6.03041012221051E-16,
-1.625));
#372064=CARTESIAN_POINT('Ctrl Pts',(-1.01778810567666,-0.587620236790416,
-1.58333333333333));
#372065=CARTESIAN_POINT('Ctrl Pts',(-0.678525403784438,-1.17524047358083,
-1.54166666666667));
#372066=CARTESIAN_POINT('Ctrl Pts',(-1.43925448419919E-16,-1.17524047358083,
-1.5));
#372067=CARTESIAN_POINT('Origin',(6.93889390390723E-17,9.71445146547012E-16,
-9.21875));
#372068=CARTESIAN_POINT('',(6.93889390390724E-17,-1.17524047358083,-0.937499999999999));
#372069=CARTESIAN_POINT('',(6.93889390390724E-17,-1.17524047358083,-0.999999999999999));
#372070=CARTESIAN_POINT('',(2.82703326498063E-16,-1.17524047358083,-9.21875));
#372071=CARTESIAN_POINT('Ctrl Pts',(-1.43925448419919E-16,-1.17524047358083,
-1.4375));
#372072=CARTESIAN_POINT('Ctrl Pts',(0.678525403784437,-1.17524047358083,
-1.39583333333333));
#372073=CARTESIAN_POINT('Ctrl Pts',(1.01778810567666,-0.587620236790417,
-1.35416666666667));
#372074=CARTESIAN_POINT('Ctrl Pts',(1.35705080756888,2.7065942666714E-16,
-1.3125));
#372075=CARTESIAN_POINT('Ctrl Pts',(1.01778810567666,0.587620236790417,
-1.27083333333333));
#372076=CARTESIAN_POINT('Ctrl Pts',(0.678525403784439,1.17524047358083,
-1.22916666666667));
#372077=CARTESIAN_POINT('Ctrl Pts',(0.,1.17524047358083,-1.1875));
#372078=CARTESIAN_POINT('Ctrl Pts',(-0.678525403784438,1.17524047358083,
-1.14583333333333));
#372079=CARTESIAN_POINT('Ctrl Pts',(-1.01778810567666,0.587620236790418,
-1.10416666666667));
#372080=CARTESIAN_POINT('Ctrl Pts',(-1.35705080756888,6.03041012221051E-16,
-1.0625));
#372081=CARTESIAN_POINT('Ctrl Pts',(-1.01778810567666,-0.587620236790416,
-1.02083333333333));
#372082=CARTESIAN_POINT('Ctrl Pts',(-0.678525403784438,-1.17524047358083,
-0.979166666666667));
#372083=CARTESIAN_POINT('Ctrl Pts',(-1.43925448419919E-16,-1.17524047358083,
-0.937499999999999));
#372084=CARTESIAN_POINT('Ctrl Pts',(-1.43925448419919E-16,-1.17524047358083,
-1.5));
#372085=CARTESIAN_POINT('Ctrl Pts',(0.678525403784437,-1.17524047358083,
-1.45833333333333));
#372086=CARTESIAN_POINT('Ctrl Pts',(1.01778810567666,-0.587620236790417,
-1.41666666666667));
#372087=CARTESIAN_POINT('Ctrl Pts',(1.35705080756888,2.7065942666714E-16,
-1.375));
#372088=CARTESIAN_POINT('Ctrl Pts',(1.01778810567666,0.587620236790417,
-1.33333333333333));
#372089=CARTESIAN_POINT('Ctrl Pts',(0.678525403784439,1.17524047358083,
-1.29166666666667));
#372090=CARTESIAN_POINT('Ctrl Pts',(0.,1.17524047358083,-1.25));
#372091=CARTESIAN_POINT('Ctrl Pts',(-0.678525403784438,1.17524047358083,
-1.20833333333333));
#372092=CARTESIAN_POINT('Ctrl Pts',(-1.01778810567666,0.587620236790418,
-1.16666666666667));
#372093=CARTESIAN_POINT('Ctrl Pts',(-1.35705080756888,6.03041012221051E-16,
-1.125));
#372094=CARTESIAN_POINT('Ctrl Pts',(-1.01778810567666,-0.587620236790416,
-1.08333333333333));
#372095=CARTESIAN_POINT('Ctrl Pts',(-0.678525403784438,-1.17524047358083,
-1.04166666666667));
#372096=CARTESIAN_POINT('Ctrl Pts',(-1.43925448419919E-16,-1.17524047358083,
-0.999999999999999));
#372097=CARTESIAN_POINT('Origin',(6.93889390390723E-17,9.71445146547012E-16,
-9.21875));
#372098=CARTESIAN_POINT('',(6.93889390390724E-17,-1.17524047358083,-0.4375));
#372099=CARTESIAN_POINT('',(6.93889390390724E-17,-1.17524047358083,-0.5));
#372100=CARTESIAN_POINT('',(2.82703326498063E-16,-1.17524047358083,-9.21875));
#372101=CARTESIAN_POINT('Ctrl Pts',(-1.43925448419919E-16,-1.17524047358083,
-0.937499999999999));
#372102=CARTESIAN_POINT('Ctrl Pts',(0.678525403784437,-1.17524047358083,
-0.895833333333333));
#372103=CARTESIAN_POINT('Ctrl Pts',(1.01778810567666,-0.587620236790417,
-0.854166666666666));
#372104=CARTESIAN_POINT('Ctrl Pts',(1.35705080756888,2.7065942666714E-16,
-0.812499999999999));
#372105=CARTESIAN_POINT('Ctrl Pts',(1.01778810567666,0.587620236790417,
-0.770833333333333));
#372106=CARTESIAN_POINT('Ctrl Pts',(0.678525403784439,1.17524047358083,
-0.729166666666666));
#372107=CARTESIAN_POINT('Ctrl Pts',(0.,1.17524047358083,-0.687500000000001));
#372108=CARTESIAN_POINT('Ctrl Pts',(-0.678525403784438,1.17524047358083,
-0.645833333333333));
#372109=CARTESIAN_POINT('Ctrl Pts',(-1.01778810567666,0.587620236790418,
-0.604166666666666));
#372110=CARTESIAN_POINT('Ctrl Pts',(-1.35705080756888,6.03041012221051E-16,
-0.5625));
#372111=CARTESIAN_POINT('Ctrl Pts',(-1.01778810567666,-0.587620236790416,
-0.520833333333333));
#372112=CARTESIAN_POINT('Ctrl Pts',(-0.678525403784438,-1.17524047358083,
-0.479166666666666));
#372113=CARTESIAN_POINT('Ctrl Pts',(-1.43925448419919E-16,-1.17524047358083,
-0.4375));
#372114=CARTESIAN_POINT('Ctrl Pts',(-1.43925448419919E-16,-1.17524047358083,
-0.999999999999999));
#372115=CARTESIAN_POINT('Ctrl Pts',(0.678525403784437,-1.17524047358083,
-0.958333333333334));
#372116=CARTESIAN_POINT('Ctrl Pts',(1.01778810567666,-0.587620236790417,
-0.916666666666666));
#372117=CARTESIAN_POINT('Ctrl Pts',(1.35705080756888,2.7065942666714E-16,
-0.874999999999999));
#372118=CARTESIAN_POINT('Ctrl Pts',(1.01778810567666,0.587620236790417,
-0.833333333333334));
#372119=CARTESIAN_POINT('Ctrl Pts',(0.678525403784439,1.17524047358083,
-0.791666666666666));
#372120=CARTESIAN_POINT('Ctrl Pts',(0.,1.17524047358083,-0.750000000000001));
#372121=CARTESIAN_POINT('Ctrl Pts',(-0.678525403784438,1.17524047358083,
-0.708333333333333));
#372122=CARTESIAN_POINT('Ctrl Pts',(-1.01778810567666,0.587620236790418,
-0.666666666666666));
#372123=CARTESIAN_POINT('Ctrl Pts',(-1.35705080756888,6.03041012221051E-16,
-0.625000000000001));
#372124=CARTESIAN_POINT('Ctrl Pts',(-1.01778810567666,-0.587620236790416,
-0.583333333333333));
#372125=CARTESIAN_POINT('Ctrl Pts',(-0.678525403784438,-1.17524047358083,
-0.541666666666666));
#372126=CARTESIAN_POINT('Ctrl Pts',(-1.43925448419919E-16,-1.17524047358083,
-0.5));
#372127=CARTESIAN_POINT('Origin',(6.93889390390723E-17,9.71445146547012E-16,
-9.21875));
#372128=CARTESIAN_POINT('',(6.93889390390724E-17,-1.17524047358083,0.0625000000000001));
#372129=CARTESIAN_POINT('',(6.93889390390724E-17,-1.17524047358083,0.));
#372130=CARTESIAN_POINT('',(2.82703326498063E-16,-1.17524047358083,-9.21875));
#372131=CARTESIAN_POINT('Ctrl Pts',(-1.43925448419919E-16,-1.17524047358083,
-0.4375));
#372132=CARTESIAN_POINT('Ctrl Pts',(0.678525403784437,-1.17524047358083,
-0.395833333333333));
#372133=CARTESIAN_POINT('Ctrl Pts',(1.01778810567666,-0.587620236790417,
-0.354166666666666));
#372134=CARTESIAN_POINT('Ctrl Pts',(1.35705080756888,2.7065942666714E-16,
-0.3125));
#372135=CARTESIAN_POINT('Ctrl Pts',(1.01778810567666,0.587620236790417,
-0.270833333333333));
#372136=CARTESIAN_POINT('Ctrl Pts',(0.678525403784439,1.17524047358083,
-0.229166666666666));
#372137=CARTESIAN_POINT('Ctrl Pts',(0.,1.17524047358083,-0.1875));
#372138=CARTESIAN_POINT('Ctrl Pts',(-0.678525403784438,1.17524047358083,
-0.145833333333333));
#372139=CARTESIAN_POINT('Ctrl Pts',(-1.01778810567666,0.587620236790418,
-0.104166666666666));
#372140=CARTESIAN_POINT('Ctrl Pts',(-1.35705080756888,6.03041012221051E-16,
-0.0625000000000001));
#372141=CARTESIAN_POINT('Ctrl Pts',(-1.01778810567666,-0.587620236790416,
-0.0208333333333328));
#372142=CARTESIAN_POINT('Ctrl Pts',(-0.678525403784438,-1.17524047358083,
0.0208333333333328));
#372143=CARTESIAN_POINT('Ctrl Pts',(-1.43925448419919E-16,-1.17524047358083,
0.0625000000000001));
#372144=CARTESIAN_POINT('Ctrl Pts',(-1.43925448419919E-16,-1.17524047358083,
-0.5));
#372145=CARTESIAN_POINT('Ctrl Pts',(0.678525403784437,-1.17524047358083,
-0.458333333333333));
#372146=CARTESIAN_POINT('Ctrl Pts',(1.01778810567666,-0.587620236790417,
-0.416666666666666));
#372147=CARTESIAN_POINT('Ctrl Pts',(1.35705080756888,2.7065942666714E-16,
-0.375));
#372148=CARTESIAN_POINT('Ctrl Pts',(1.01778810567666,0.587620236790417,
-0.333333333333333));
#372149=CARTESIAN_POINT('Ctrl Pts',(0.678525403784439,1.17524047358083,
-0.291666666666666));
#372150=CARTESIAN_POINT('Ctrl Pts',(0.,1.17524047358083,-0.25));
#372151=CARTESIAN_POINT('Ctrl Pts',(-0.678525403784438,1.17524047358083,
-0.208333333333333));
#372152=CARTESIAN_POINT('Ctrl Pts',(-1.01778810567666,0.587620236790418,
-0.166666666666666));
#372153=CARTESIAN_POINT('Ctrl Pts',(-1.35705080756888,6.03041012221051E-16,
-0.125));
#372154=CARTESIAN_POINT('Ctrl Pts',(-1.01778810567666,-0.587620236790416,
-0.0833333333333328));
#372155=CARTESIAN_POINT('Ctrl Pts',(-0.678525403784438,-1.17524047358083,
-0.0416666666666673));
#372156=CARTESIAN_POINT('Ctrl Pts',(-1.43925448419919E-16,-1.17524047358083,
0.));
#372157=CARTESIAN_POINT('Origin',(6.93889390390723E-17,9.71445146547012E-16,
-9.21875));
#372158=CARTESIAN_POINT('',(6.93889390390724E-17,-1.17524047358083,0.5625));
#372159=CARTESIAN_POINT('',(6.93889390390724E-17,-1.17524047358083,0.5));
#372160=CARTESIAN_POINT('',(2.82703326498063E-16,-1.17524047358083,-9.21875));
#372161=CARTESIAN_POINT('Ctrl Pts',(-1.43925448419919E-16,-1.17524047358083,
0.0625000000000001));
#372162=CARTESIAN_POINT('Ctrl Pts',(0.678525403784437,-1.17524047358083,
0.104166666666667));
#372163=CARTESIAN_POINT('Ctrl Pts',(1.01778810567666,-0.587620236790417,
0.145833333333333));
#372164=CARTESIAN_POINT('Ctrl Pts',(1.35705080756888,2.7065942666714E-16,
0.1875));
#372165=CARTESIAN_POINT('Ctrl Pts',(1.01778810567666,0.587620236790417,
0.229166666666667));
#372166=CARTESIAN_POINT('Ctrl Pts',(0.678525403784439,1.17524047358083,
0.270833333333333));
#372167=CARTESIAN_POINT('Ctrl Pts',(0.,1.17524047358083,0.3125));
#372168=CARTESIAN_POINT('Ctrl Pts',(-0.678525403784438,1.17524047358083,
0.354166666666668));
#372169=CARTESIAN_POINT('Ctrl Pts',(-1.01778810567666,0.587620236790418,
0.395833333333333));
#372170=CARTESIAN_POINT('Ctrl Pts',(-1.35705080756888,6.03041012221051E-16,
0.4375));
#372171=CARTESIAN_POINT('Ctrl Pts',(-1.01778810567666,-0.587620236790416,
0.479166666666668));
#372172=CARTESIAN_POINT('Ctrl Pts',(-0.678525403784438,-1.17524047358083,
0.520833333333333));
#372173=CARTESIAN_POINT('Ctrl Pts',(-1.43925448419919E-16,-1.17524047358083,
0.5625));
#372174=CARTESIAN_POINT('Ctrl Pts',(-1.43925448419919E-16,-1.17524047358083,
0.));
#372175=CARTESIAN_POINT('Ctrl Pts',(0.678525403784437,-1.17524047358083,
0.0416666666666673));
#372176=CARTESIAN_POINT('Ctrl Pts',(1.01778810567666,-0.587620236790417,
0.0833333333333328));
#372177=CARTESIAN_POINT('Ctrl Pts',(1.35705080756888,2.7065942666714E-16,
0.125));
#372178=CARTESIAN_POINT('Ctrl Pts',(1.01778810567666,0.587620236790417,
0.166666666666667));
#372179=CARTESIAN_POINT('Ctrl Pts',(0.678525403784439,1.17524047358083,
0.208333333333333));
#372180=CARTESIAN_POINT('Ctrl Pts',(0.,1.17524047358083,0.25));
#372181=CARTESIAN_POINT('Ctrl Pts',(-0.678525403784438,1.17524047358083,
0.291666666666668));
#372182=CARTESIAN_POINT('Ctrl Pts',(-1.01778810567666,0.587620236790418,
0.333333333333333));
#372183=CARTESIAN_POINT('Ctrl Pts',(-1.35705080756888,6.03041012221051E-16,
0.375));
#372184=CARTESIAN_POINT('Ctrl Pts',(-1.01778810567666,-0.587620236790416,
0.416666666666668));
#372185=CARTESIAN_POINT('Ctrl Pts',(-0.678525403784438,-1.17524047358083,
0.458333333333333));
#372186=CARTESIAN_POINT('Ctrl Pts',(-1.43925448419919E-16,-1.17524047358083,
0.5));
#372187=CARTESIAN_POINT('Origin',(6.93889390390723E-17,9.71445146547012E-16,
-9.21875));
#372188=CARTESIAN_POINT('',(6.93889390390724E-17,-1.17524047358083,1.0625));
#372189=CARTESIAN_POINT('',(6.93889390390724E-17,-1.17524047358083,1.));
#372190=CARTESIAN_POINT('',(2.82703326498063E-16,-1.17524047358083,-9.21875));
#372191=CARTESIAN_POINT('Ctrl Pts',(-1.43925448419919E-16,-1.17524047358083,
0.5625));
#372192=CARTESIAN_POINT('Ctrl Pts',(0.678525403784437,-1.17524047358083,
0.604166666666666));
#372193=CARTESIAN_POINT('Ctrl Pts',(1.01778810567666,-0.587620236790417,
0.645833333333333));
#372194=CARTESIAN_POINT('Ctrl Pts',(1.35705080756888,2.7065942666714E-16,
0.687500000000001));
#372195=CARTESIAN_POINT('Ctrl Pts',(1.01778810567666,0.587620236790417,
0.729166666666666));
#372196=CARTESIAN_POINT('Ctrl Pts',(0.678525403784439,1.17524047358083,
0.770833333333333));
#372197=CARTESIAN_POINT('Ctrl Pts',(0.,1.17524047358083,0.812500000000001));
#372198=CARTESIAN_POINT('Ctrl Pts',(-0.678525403784438,1.17524047358083,
0.854166666666666));
#372199=CARTESIAN_POINT('Ctrl Pts',(-1.01778810567666,0.587620236790418,
0.895833333333334));
#372200=CARTESIAN_POINT('Ctrl Pts',(-1.35705080756888,6.03041012221051E-16,
0.937500000000001));
#372201=CARTESIAN_POINT('Ctrl Pts',(-1.01778810567666,-0.587620236790416,
0.979166666666667));
#372202=CARTESIAN_POINT('Ctrl Pts',(-0.678525403784438,-1.17524047358083,
1.02083333333333));
#372203=CARTESIAN_POINT('Ctrl Pts',(-1.43925448419919E-16,-1.17524047358083,
1.0625));
#372204=CARTESIAN_POINT('Ctrl Pts',(-1.43925448419919E-16,-1.17524047358083,
0.5));
#372205=CARTESIAN_POINT('Ctrl Pts',(0.678525403784437,-1.17524047358083,
0.541666666666666));
#372206=CARTESIAN_POINT('Ctrl Pts',(1.01778810567666,-0.587620236790417,
0.583333333333333));
#372207=CARTESIAN_POINT('Ctrl Pts',(1.35705080756888,2.7065942666714E-16,
0.625000000000001));
#372208=CARTESIAN_POINT('Ctrl Pts',(1.01778810567666,0.587620236790417,
0.666666666666666));
#372209=CARTESIAN_POINT('Ctrl Pts',(0.678525403784439,1.17524047358083,
0.708333333333333));
#372210=CARTESIAN_POINT('Ctrl Pts',(0.,1.17524047358083,0.750000000000001));
#372211=CARTESIAN_POINT('Ctrl Pts',(-0.678525403784438,1.17524047358083,
0.791666666666666));
#372212=CARTESIAN_POINT('Ctrl Pts',(-1.01778810567666,0.587620236790418,
0.833333333333334));
#372213=CARTESIAN_POINT('Ctrl Pts',(-1.35705080756888,6.03041012221051E-16,
0.875000000000001));
#372214=CARTESIAN_POINT('Ctrl Pts',(-1.01778810567666,-0.587620236790416,
0.916666666666666));
#372215=CARTESIAN_POINT('Ctrl Pts',(-0.678525403784438,-1.17524047358083,
0.958333333333334));
#372216=CARTESIAN_POINT('Ctrl Pts',(-1.43925448419919E-16,-1.17524047358083,
1.));
#372217=CARTESIAN_POINT('Origin',(6.93889390390723E-17,9.71445146547012E-16,
-9.21875));
#372218=CARTESIAN_POINT('',(6.93889390390724E-17,-1.17524047358083,1.5625));
#372219=CARTESIAN_POINT('',(6.93889390390724E-17,-1.17524047358083,1.5));
#372220=CARTESIAN_POINT('',(2.82703326498063E-16,-1.17524047358083,-9.21875));
#372221=CARTESIAN_POINT('Ctrl Pts',(-1.43925448419919E-16,-1.17524047358083,
1.0625));
#372222=CARTESIAN_POINT('Ctrl Pts',(0.678525403784437,-1.17524047358083,
1.10416666666667));
#372223=CARTESIAN_POINT('Ctrl Pts',(1.01778810567666,-0.587620236790417,
1.14583333333333));
#372224=CARTESIAN_POINT('Ctrl Pts',(1.35705080756888,2.7065942666714E-16,
1.1875));
#372225=CARTESIAN_POINT('Ctrl Pts',(1.01778810567666,0.587620236790417,
1.22916666666667));
#372226=CARTESIAN_POINT('Ctrl Pts',(0.678525403784439,1.17524047358083,
1.27083333333333));
#372227=CARTESIAN_POINT('Ctrl Pts',(0.,1.17524047358083,1.3125));
#372228=CARTESIAN_POINT('Ctrl Pts',(-0.678525403784438,1.17524047358083,
1.35416666666667));
#372229=CARTESIAN_POINT('Ctrl Pts',(-1.01778810567666,0.587620236790418,
1.39583333333333));
